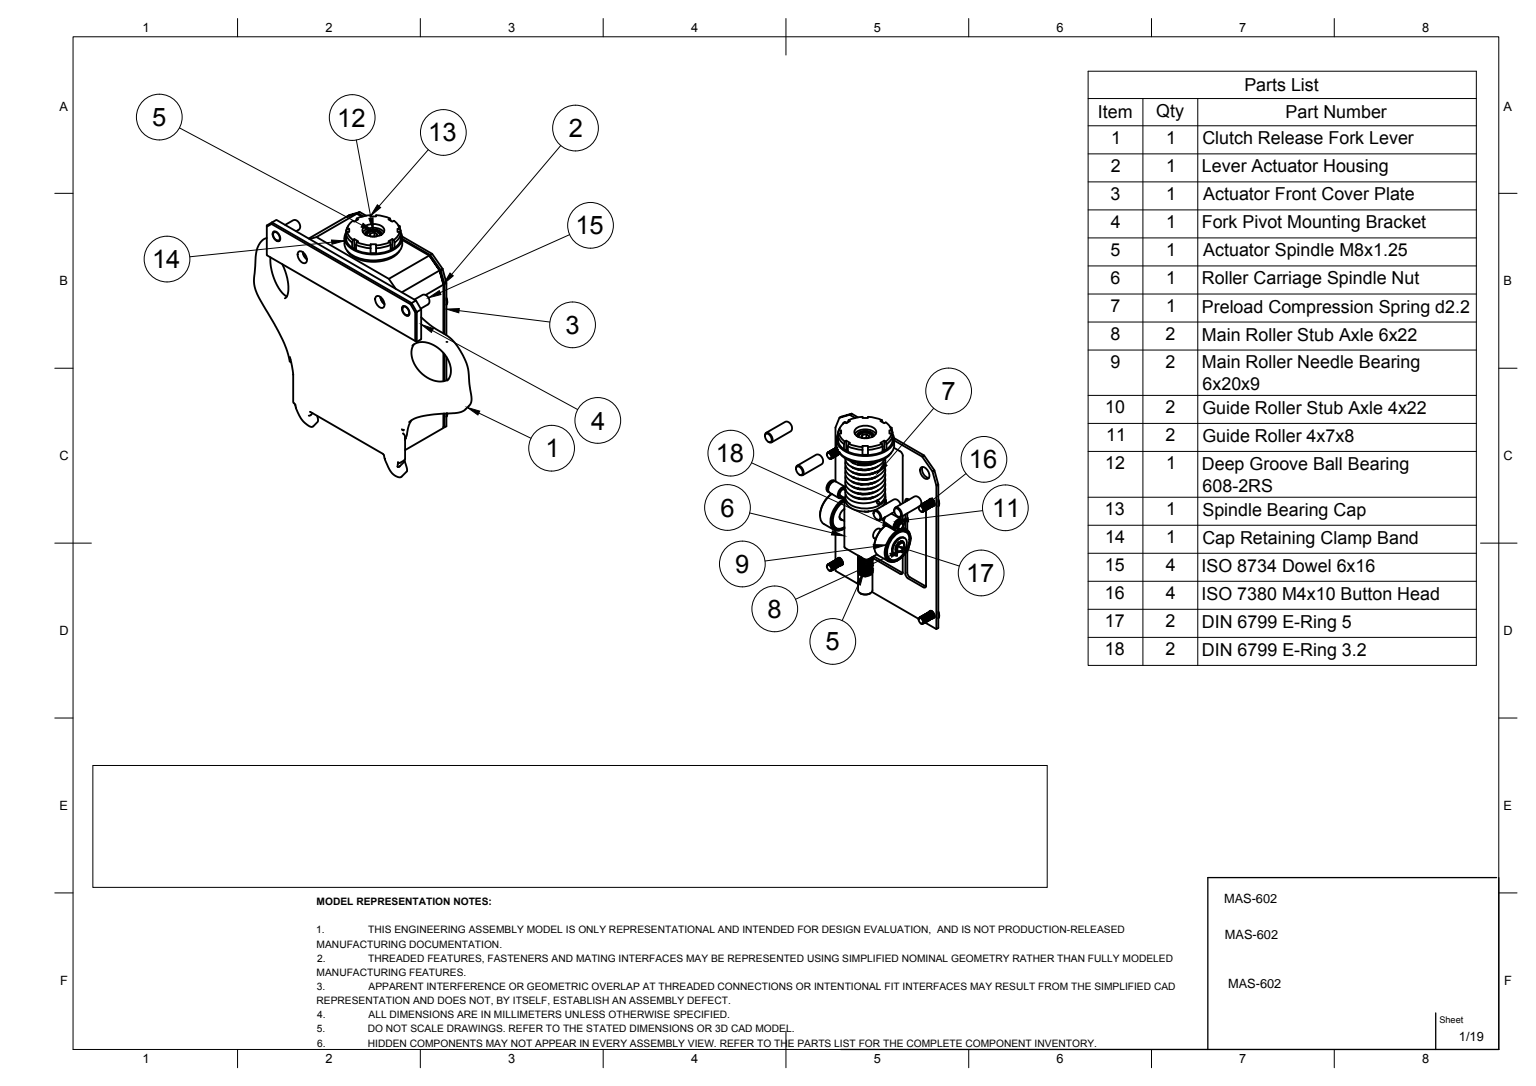
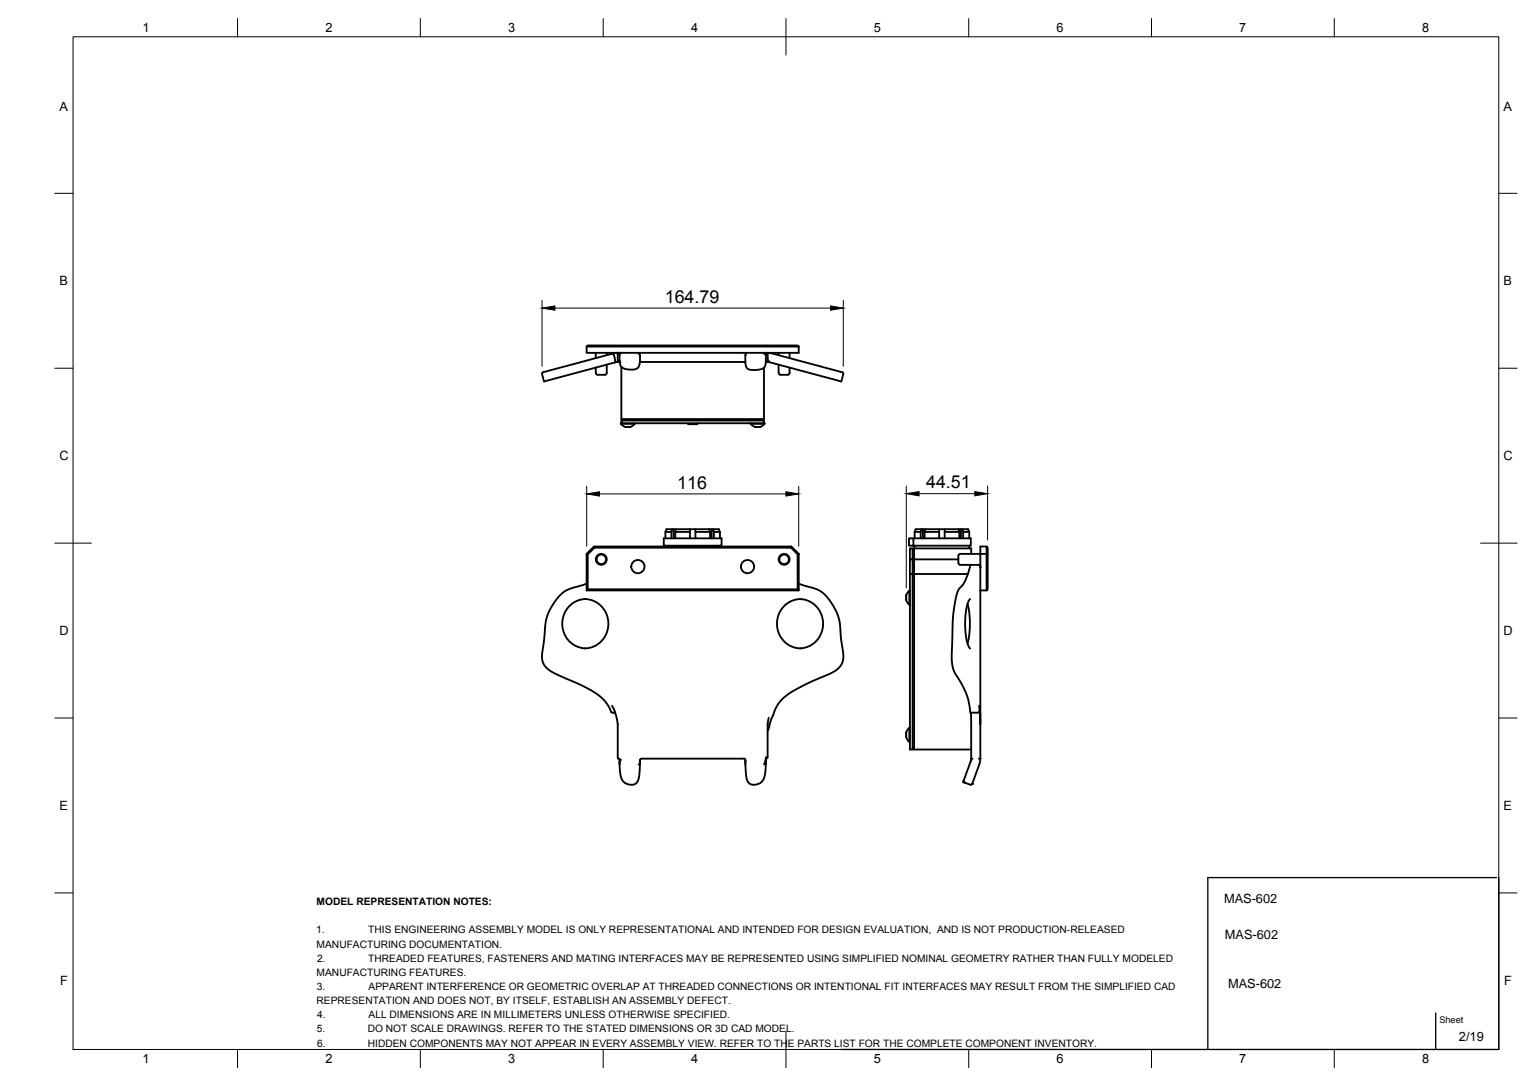
ISO-10303-21;
HEADER;
/* Generated by software containing ST-Developer
 * from STEP Tools, Inc. (www.steptools.com) 
 */

FILE_DESCRIPTION(
/* description */ (''),
/* implementation_level */ '2;1');

FILE_NAME(
/* name */ 'MAS-602',
/* time_stamp */ '2026-10-15T14:42:47-07:00',
/* author */ (''),
/* organization */ (''),
/* preprocessor_version */ 'ST-DEVELOPER v20.2',
/* originating_system */ 'Autodesk Translation Framework v15.15.0.0',
/* authorisation */ '');

FILE_SCHEMA (('AUTOMOTIVE_DESIGN { 1 0 10303 214 3 1 1 }'));
ENDSEC;

DATA;
#10=MECHANICAL_DESIGN_GEOMETRIC_PRESENTATION_REPRESENTATION('',(#234,#235,
#236,#237,#238,#239,#240,#241,#242,#243,#244,#245,#246,#247,#248,#249,#250,
#251),#85789);
#11=ITEM_DEFINED_TRANSFORMATION($,$,#10099,#10929);
#12=ITEM_DEFINED_TRANSFORMATION($,$,#10303,#10930);
#13=ITEM_DEFINED_TRANSFORMATION($,$,#10376,#10931);
#14=ITEM_DEFINED_TRANSFORMATION($,$,#10453,#10932);
#15=ITEM_DEFINED_TRANSFORMATION($,$,#10480,#10933);
#16=ITEM_DEFINED_TRANSFORMATION($,$,#10504,#10934);
#17=ITEM_DEFINED_TRANSFORMATION($,$,#10562,#10935);
#18=ITEM_DEFINED_TRANSFORMATION($,$,#10741,#10936);
#19=ITEM_DEFINED_TRANSFORMATION($,$,#10691,#10937);
#20=ITEM_DEFINED_TRANSFORMATION($,$,#10759,#10938);
#21=ITEM_DEFINED_TRANSFORMATION($,$,#10724,#10939);
#22=ITEM_DEFINED_TRANSFORMATION($,$,#10565,#10940);
#23=ITEM_DEFINED_TRANSFORMATION($,$,#10598,#10941);
#24=ITEM_DEFINED_TRANSFORMATION($,$,#10679,#10942);
#25=ITEM_DEFINED_TRANSFORMATION($,$,#10777,#10943);
#26=ITEM_DEFINED_TRANSFORMATION($,$,#10788,#10944);
#27=ITEM_DEFINED_TRANSFORMATION($,$,#10855,#10945);
#28=ITEM_DEFINED_TRANSFORMATION($,$,#10892,#10946);
#29=ITEM_DEFINED_TRANSFORMATION($,$,#10691,#10947);
#30=ITEM_DEFINED_TRANSFORMATION($,$,#10724,#10948);
#31=ITEM_DEFINED_TRANSFORMATION($,$,#10741,#10949);
#32=ITEM_DEFINED_TRANSFORMATION($,$,#10759,#10950);
#33=ITEM_DEFINED_TRANSFORMATION($,$,#10777,#10951);
#34=ITEM_DEFINED_TRANSFORMATION($,$,#10777,#10952);
#35=ITEM_DEFINED_TRANSFORMATION($,$,#10777,#10953);
#36=ITEM_DEFINED_TRANSFORMATION($,$,#10788,#10954);
#37=ITEM_DEFINED_TRANSFORMATION($,$,#10788,#10955);
#38=ITEM_DEFINED_TRANSFORMATION($,$,#10788,#10956);
#39=ITEM_DEFINED_TRANSFORMATION($,$,#10855,#10957);
#40=ITEM_DEFINED_TRANSFORMATION($,$,#10892,#10958);
#41=(
REPRESENTATION_RELATIONSHIP($,$,#85863,#85862)
REPRESENTATION_RELATIONSHIP_WITH_TRANSFORMATION(#11)
SHAPE_REPRESENTATION_RELATIONSHIP()
);
#42=(
REPRESENTATION_RELATIONSHIP($,$,#85864,#85862)
REPRESENTATION_RELATIONSHIP_WITH_TRANSFORMATION(#12)
SHAPE_REPRESENTATION_RELATIONSHIP()
);
#43=(
REPRESENTATION_RELATIONSHIP($,$,#85865,#85862)
REPRESENTATION_RELATIONSHIP_WITH_TRANSFORMATION(#13)
SHAPE_REPRESENTATION_RELATIONSHIP()
);
#44=(
REPRESENTATION_RELATIONSHIP($,$,#85866,#85862)
REPRESENTATION_RELATIONSHIP_WITH_TRANSFORMATION(#14)
SHAPE_REPRESENTATION_RELATIONSHIP()
);
#45=(
REPRESENTATION_RELATIONSHIP($,$,#85867,#85862)
REPRESENTATION_RELATIONSHIP_WITH_TRANSFORMATION(#15)
SHAPE_REPRESENTATION_RELATIONSHIP()
);
#46=(
REPRESENTATION_RELATIONSHIP($,$,#85868,#85862)
REPRESENTATION_RELATIONSHIP_WITH_TRANSFORMATION(#16)
SHAPE_REPRESENTATION_RELATIONSHIP()
);
#47=(
REPRESENTATION_RELATIONSHIP($,$,#85869,#85862)
REPRESENTATION_RELATIONSHIP_WITH_TRANSFORMATION(#17)
SHAPE_REPRESENTATION_RELATIONSHIP()
);
#48=(
REPRESENTATION_RELATIONSHIP($,$,#85875,#85862)
REPRESENTATION_RELATIONSHIP_WITH_TRANSFORMATION(#18)
SHAPE_REPRESENTATION_RELATIONSHIP()
);
#49=(
REPRESENTATION_RELATIONSHIP($,$,#85873,#85862)
REPRESENTATION_RELATIONSHIP_WITH_TRANSFORMATION(#19)
SHAPE_REPRESENTATION_RELATIONSHIP()
);
#50=(
REPRESENTATION_RELATIONSHIP($,$,#85876,#85862)
REPRESENTATION_RELATIONSHIP_WITH_TRANSFORMATION(#20)
SHAPE_REPRESENTATION_RELATIONSHIP()
);
#51=(
REPRESENTATION_RELATIONSHIP($,$,#85874,#85862)
REPRESENTATION_RELATIONSHIP_WITH_TRANSFORMATION(#21)
SHAPE_REPRESENTATION_RELATIONSHIP()
);
#52=(
REPRESENTATION_RELATIONSHIP($,$,#85870,#85862)
REPRESENTATION_RELATIONSHIP_WITH_TRANSFORMATION(#22)
SHAPE_REPRESENTATION_RELATIONSHIP()
);
#53=(
REPRESENTATION_RELATIONSHIP($,$,#85871,#85862)
REPRESENTATION_RELATIONSHIP_WITH_TRANSFORMATION(#23)
SHAPE_REPRESENTATION_RELATIONSHIP()
);
#54=(
REPRESENTATION_RELATIONSHIP($,$,#85872,#85862)
REPRESENTATION_RELATIONSHIP_WITH_TRANSFORMATION(#24)
SHAPE_REPRESENTATION_RELATIONSHIP()
);
#55=(
REPRESENTATION_RELATIONSHIP($,$,#85877,#85862)
REPRESENTATION_RELATIONSHIP_WITH_TRANSFORMATION(#25)
SHAPE_REPRESENTATION_RELATIONSHIP()
);
#56=(
REPRESENTATION_RELATIONSHIP($,$,#85878,#85862)
REPRESENTATION_RELATIONSHIP_WITH_TRANSFORMATION(#26)
SHAPE_REPRESENTATION_RELATIONSHIP()
);
#57=(
REPRESENTATION_RELATIONSHIP($,$,#85879,#85862)
REPRESENTATION_RELATIONSHIP_WITH_TRANSFORMATION(#27)
SHAPE_REPRESENTATION_RELATIONSHIP()
);
#58=(
REPRESENTATION_RELATIONSHIP($,$,#85880,#85862)
REPRESENTATION_RELATIONSHIP_WITH_TRANSFORMATION(#28)
SHAPE_REPRESENTATION_RELATIONSHIP()
);
#59=(
REPRESENTATION_RELATIONSHIP($,$,#85873,#85862)
REPRESENTATION_RELATIONSHIP_WITH_TRANSFORMATION(#29)
SHAPE_REPRESENTATION_RELATIONSHIP()
);
#60=(
REPRESENTATION_RELATIONSHIP($,$,#85874,#85862)
REPRESENTATION_RELATIONSHIP_WITH_TRANSFORMATION(#30)
SHAPE_REPRESENTATION_RELATIONSHIP()
);
#61=(
REPRESENTATION_RELATIONSHIP($,$,#85875,#85862)
REPRESENTATION_RELATIONSHIP_WITH_TRANSFORMATION(#31)
SHAPE_REPRESENTATION_RELATIONSHIP()
);
#62=(
REPRESENTATION_RELATIONSHIP($,$,#85876,#85862)
REPRESENTATION_RELATIONSHIP_WITH_TRANSFORMATION(#32)
SHAPE_REPRESENTATION_RELATIONSHIP()
);
#63=(
REPRESENTATION_RELATIONSHIP($,$,#85877,#85862)
REPRESENTATION_RELATIONSHIP_WITH_TRANSFORMATION(#33)
SHAPE_REPRESENTATION_RELATIONSHIP()
);
#64=(
REPRESENTATION_RELATIONSHIP($,$,#85877,#85862)
REPRESENTATION_RELATIONSHIP_WITH_TRANSFORMATION(#34)
SHAPE_REPRESENTATION_RELATIONSHIP()
);
#65=(
REPRESENTATION_RELATIONSHIP($,$,#85877,#85862)
REPRESENTATION_RELATIONSHIP_WITH_TRANSFORMATION(#35)
SHAPE_REPRESENTATION_RELATIONSHIP()
);
#66=(
REPRESENTATION_RELATIONSHIP($,$,#85878,#85862)
REPRESENTATION_RELATIONSHIP_WITH_TRANSFORMATION(#36)
SHAPE_REPRESENTATION_RELATIONSHIP()
);
#67=(
REPRESENTATION_RELATIONSHIP($,$,#85878,#85862)
REPRESENTATION_RELATIONSHIP_WITH_TRANSFORMATION(#37)
SHAPE_REPRESENTATION_RELATIONSHIP()
);
#68=(
REPRESENTATION_RELATIONSHIP($,$,#85878,#85862)
REPRESENTATION_RELATIONSHIP_WITH_TRANSFORMATION(#38)
SHAPE_REPRESENTATION_RELATIONSHIP()
);
#69=(
REPRESENTATION_RELATIONSHIP($,$,#85879,#85862)
REPRESENTATION_RELATIONSHIP_WITH_TRANSFORMATION(#39)
SHAPE_REPRESENTATION_RELATIONSHIP()
);
#70=(
REPRESENTATION_RELATIONSHIP($,$,#85880,#85862)
REPRESENTATION_RELATIONSHIP_WITH_TRANSFORMATION(#40)
SHAPE_REPRESENTATION_RELATIONSHIP()
);
#71=CONTEXT_DEPENDENT_SHAPE_REPRESENTATION(#41,#85832);
#72=CONTEXT_DEPENDENT_SHAPE_REPRESENTATION(#42,#85833);
#73=CONTEXT_DEPENDENT_SHAPE_REPRESENTATION(#43,#85834);
#74=CONTEXT_DEPENDENT_SHAPE_REPRESENTATION(#44,#85835);
#75=CONTEXT_DEPENDENT_SHAPE_REPRESENTATION(#45,#85836);
#76=CONTEXT_DEPENDENT_SHAPE_REPRESENTATION(#46,#85837);
#77=CONTEXT_DEPENDENT_SHAPE_REPRESENTATION(#47,#85838);
#78=CONTEXT_DEPENDENT_SHAPE_REPRESENTATION(#48,#85839);
#79=CONTEXT_DEPENDENT_SHAPE_REPRESENTATION(#49,#85840);
#80=CONTEXT_DEPENDENT_SHAPE_REPRESENTATION(#50,#85841);
#81=CONTEXT_DEPENDENT_SHAPE_REPRESENTATION(#51,#85842);
#82=CONTEXT_DEPENDENT_SHAPE_REPRESENTATION(#52,#85843);
#83=CONTEXT_DEPENDENT_SHAPE_REPRESENTATION(#53,#85844);
#84=CONTEXT_DEPENDENT_SHAPE_REPRESENTATION(#54,#85845);
#85=CONTEXT_DEPENDENT_SHAPE_REPRESENTATION(#55,#85846);
#86=CONTEXT_DEPENDENT_SHAPE_REPRESENTATION(#56,#85847);
#87=CONTEXT_DEPENDENT_SHAPE_REPRESENTATION(#57,#85848);
#88=CONTEXT_DEPENDENT_SHAPE_REPRESENTATION(#58,#85849);
#89=CONTEXT_DEPENDENT_SHAPE_REPRESENTATION(#59,#85850);
#90=CONTEXT_DEPENDENT_SHAPE_REPRESENTATION(#60,#85851);
#91=CONTEXT_DEPENDENT_SHAPE_REPRESENTATION(#61,#85852);
#92=CONTEXT_DEPENDENT_SHAPE_REPRESENTATION(#62,#85853);
#93=CONTEXT_DEPENDENT_SHAPE_REPRESENTATION(#63,#85854);
#94=CONTEXT_DEPENDENT_SHAPE_REPRESENTATION(#64,#85855);
#95=CONTEXT_DEPENDENT_SHAPE_REPRESENTATION(#65,#85856);
#96=CONTEXT_DEPENDENT_SHAPE_REPRESENTATION(#66,#85857);
#97=CONTEXT_DEPENDENT_SHAPE_REPRESENTATION(#67,#85858);
#98=CONTEXT_DEPENDENT_SHAPE_REPRESENTATION(#68,#85859);
#99=CONTEXT_DEPENDENT_SHAPE_REPRESENTATION(#69,#85860);
#100=CONTEXT_DEPENDENT_SHAPE_REPRESENTATION(#70,#85861);
#101=NEXT_ASSEMBLY_USAGE_OCCURRENCE('Clutch Release Fork Lever:1',
'Clutch Release Fork Lever:1','Clutch Release Fork Lever:1',#85882,#85883,
'Clutch Release Fork Lever:1');
#102=NEXT_ASSEMBLY_USAGE_OCCURRENCE('Lever Actuator Housing:1',
'Lever Actuator Housing:1','Lever Actuator Housing:1',#85882,#85884,
'Lever Actuator Housing:1');
#103=NEXT_ASSEMBLY_USAGE_OCCURRENCE('Actuator Front Cover Plate:1',
'Actuator Front Cover Plate:1','Actuator Front Cover Plate:1',#85882,#85885,
'Actuator Front Cover Plate:1');
#104=NEXT_ASSEMBLY_USAGE_OCCURRENCE('Fork Pivot Mounting Bracket:1',
'Fork Pivot Mounting Bracket:1','Fork Pivot Mounting Bracket:1',#85882,
#85886,'Fork Pivot Mounting Bracket:1');
#105=NEXT_ASSEMBLY_USAGE_OCCURRENCE('Actuator Spindle M8x1.25:1',
'Actuator Spindle M8x1.25:1','Actuator Spindle M8x1.25:1',#85882,#85887,
'Actuator Spindle M8x1.25:1');
#106=NEXT_ASSEMBLY_USAGE_OCCURRENCE('Roller Carriage Spindle Nut:1',
'Roller Carriage Spindle Nut:1','Roller Carriage Spindle Nut:1',#85882,
#85888,'Roller Carriage Spindle Nut:1');
#107=NEXT_ASSEMBLY_USAGE_OCCURRENCE('Preload Compression Spring d2.2:1',
'Preload Compression Spring d2.2:1','Preload Compression Spring d2.2:1',
#85882,#85889,'Preload Compression Spring d2.2:1');
#108=NEXT_ASSEMBLY_USAGE_OCCURRENCE('Main Roller Stub Axle 6x22:1',
'Main Roller Stub Axle 6x22:1','Main Roller Stub Axle 6x22:1',#85882,#85895,
'Main Roller Stub Axle 6x22:1');
#109=NEXT_ASSEMBLY_USAGE_OCCURRENCE(
'Main Roller Needle Bearing 6x20x9:1',
'Main Roller Needle Bearing 6x20x9:1',
'Main Roller Needle Bearing 6x20x9:1',#85882,#85893,
'Main Roller Needle Bearing 6x20x9:1');
#110=NEXT_ASSEMBLY_USAGE_OCCURRENCE('Guide Roller Stub Axle 4x22:1',
'Guide Roller Stub Axle 4x22:1','Guide Roller Stub Axle 4x22:1',#85882,
#85896,'Guide Roller Stub Axle 4x22:1');
#111=NEXT_ASSEMBLY_USAGE_OCCURRENCE('Guide Roller 4x7x8:1',
'Guide Roller 4x7x8:1','Guide Roller 4x7x8:1',#85882,#85894,
'Guide Roller 4x7x8:1');
#112=NEXT_ASSEMBLY_USAGE_OCCURRENCE(
'Deep Groove Ball Bearing 608-2RS:1',
'Deep Groove Ball Bearing 608-2RS:1',
'Deep Groove Ball Bearing 608-2RS:1',#85882,#85890,
'Deep Groove Ball Bearing 608-2RS:1');
#113=NEXT_ASSEMBLY_USAGE_OCCURRENCE('Spindle Bearing Cap:1',
'Spindle Bearing Cap:1','Spindle Bearing Cap:1',#85882,#85891,
'Spindle Bearing Cap:1');
#114=NEXT_ASSEMBLY_USAGE_OCCURRENCE('Cap Retaining Clamp Band:1',
'Cap Retaining Clamp Band:1','Cap Retaining Clamp Band:1',#85882,#85892,
'Cap Retaining Clamp Band:1');
#115=NEXT_ASSEMBLY_USAGE_OCCURRENCE('ISO 8734 Dowel 6x16:1',
'ISO 8734 Dowel 6x16:1','ISO 8734 Dowel 6x16:1',#85882,#85897,
'ISO 8734 Dowel 6x16:1');
#116=NEXT_ASSEMBLY_USAGE_OCCURRENCE('ISO 7380 M4x10 Button Head:1',
'ISO 7380 M4x10 Button Head:1','ISO 7380 M4x10 Button Head:1',#85882,#85898,
'ISO 7380 M4x10 Button Head:1');
#117=NEXT_ASSEMBLY_USAGE_OCCURRENCE('DIN 6799 E-Ring 5:1',
'DIN 6799 E-Ring 5:1','DIN 6799 E-Ring 5:1',#85882,#85899,
'DIN 6799 E-Ring 5:1');
#118=NEXT_ASSEMBLY_USAGE_OCCURRENCE('DIN 6799 E-Ring 3.2:1',
'DIN 6799 E-Ring 3.2:1','DIN 6799 E-Ring 3.2:1',#85882,#85900,
'DIN 6799 E-Ring 3.2:1');
#119=NEXT_ASSEMBLY_USAGE_OCCURRENCE(
'Main Roller Needle Bearing 6x20x9:2',
'Main Roller Needle Bearing 6x20x9:2',
'Main Roller Needle Bearing 6x20x9:2',#85882,#85893,
'Main Roller Needle Bearing 6x20x9:2');
#120=NEXT_ASSEMBLY_USAGE_OCCURRENCE('Guide Roller 4x7x8:2',
'Guide Roller 4x7x8:2','Guide Roller 4x7x8:2',#85882,#85894,
'Guide Roller 4x7x8:2');
#121=NEXT_ASSEMBLY_USAGE_OCCURRENCE('Main Roller Stub Axle 6x22:2',
'Main Roller Stub Axle 6x22:2','Main Roller Stub Axle 6x22:2',#85882,#85895,
'Main Roller Stub Axle 6x22:2');
#122=NEXT_ASSEMBLY_USAGE_OCCURRENCE('Guide Roller Stub Axle 4x22:2',
'Guide Roller Stub Axle 4x22:2','Guide Roller Stub Axle 4x22:2',#85882,
#85896,'Guide Roller Stub Axle 4x22:2');
#123=NEXT_ASSEMBLY_USAGE_OCCURRENCE('ISO 8734 Dowel 6x16:2',
'ISO 8734 Dowel 6x16:2','ISO 8734 Dowel 6x16:2',#85882,#85897,
'ISO 8734 Dowel 6x16:2');
#124=NEXT_ASSEMBLY_USAGE_OCCURRENCE('ISO 8734 Dowel 6x16:3',
'ISO 8734 Dowel 6x16:3','ISO 8734 Dowel 6x16:3',#85882,#85897,
'ISO 8734 Dowel 6x16:3');
#125=NEXT_ASSEMBLY_USAGE_OCCURRENCE('ISO 8734 Dowel 6x16:4',
'ISO 8734 Dowel 6x16:4','ISO 8734 Dowel 6x16:4',#85882,#85897,
'ISO 8734 Dowel 6x16:4');
#126=NEXT_ASSEMBLY_USAGE_OCCURRENCE('ISO 7380 M4x10 Button Head:2',
'ISO 7380 M4x10 Button Head:2','ISO 7380 M4x10 Button Head:2',#85882,#85898,
'ISO 7380 M4x10 Button Head:2');
#127=NEXT_ASSEMBLY_USAGE_OCCURRENCE('ISO 7380 M4x10 Button Head:3',
'ISO 7380 M4x10 Button Head:3','ISO 7380 M4x10 Button Head:3',#85882,#85898,
'ISO 7380 M4x10 Button Head:3');
#128=NEXT_ASSEMBLY_USAGE_OCCURRENCE('ISO 7380 M4x10 Button Head:4',
'ISO 7380 M4x10 Button Head:4','ISO 7380 M4x10 Button Head:4',#85882,#85898,
'ISO 7380 M4x10 Button Head:4');
#129=NEXT_ASSEMBLY_USAGE_OCCURRENCE('DIN 6799 E-Ring 5:2',
'DIN 6799 E-Ring 5:2','DIN 6799 E-Ring 5:2',#85882,#85899,
'DIN 6799 E-Ring 5:2');
#130=NEXT_ASSEMBLY_USAGE_OCCURRENCE('DIN 6799 E-Ring 3.2:2',
'DIN 6799 E-Ring 3.2:2','DIN 6799 E-Ring 3.2:2',#85882,#85900,
'DIN 6799 E-Ring 3.2:2');
#131=(
BOUNDED_CURVE()
B_SPLINE_CURVE(2,(#77398,#77399,#77400),.UNSPECIFIED.,.F.,.F.)
B_SPLINE_CURVE_WITH_KNOTS((3,3),(0.,0.161672183572005),.UNSPECIFIED.)
CURVE()
GEOMETRIC_REPRESENTATION_ITEM()
RATIONAL_B_SPLINE_CURVE((1.,1.00021050527521,1.))
REPRESENTATION_ITEM('')
);
#132=(
BOUNDED_CURVE()
B_SPLINE_CURVE(2,(#77406,#77407,#77408),.UNSPECIFIED.,.F.,.F.)
B_SPLINE_CURVE_WITH_KNOTS((3,3),(0.,0.161672183572005),.UNSPECIFIED.)
CURVE()
GEOMETRIC_REPRESENTATION_ITEM()
RATIONAL_B_SPLINE_CURVE((1.,1.00021050550154,1.))
REPRESENTATION_ITEM('')
);
#133=(
BOUNDED_CURVE()
B_SPLINE_CURVE(2,(#77482,#77483,#77484),.UNSPECIFIED.,.F.,.F.)
B_SPLINE_CURVE_WITH_KNOTS((3,3),(0.,0.161672183572003),.UNSPECIFIED.)
CURVE()
GEOMETRIC_REPRESENTATION_ITEM()
RATIONAL_B_SPLINE_CURVE((1.,1.00021050513902,1.))
REPRESENTATION_ITEM('')
);
#134=(
BOUNDED_CURVE()
B_SPLINE_CURVE(2,(#77487,#77488,#77489),.UNSPECIFIED.,.F.,.F.)
B_SPLINE_CURVE_WITH_KNOTS((3,3),(0.,0.161672183572005),.UNSPECIFIED.)
CURVE()
GEOMETRIC_REPRESENTATION_ITEM()
RATIONAL_B_SPLINE_CURVE((1.,1.00021050510688,1.))
REPRESENTATION_ITEM('')
);
#135=(
BOUNDED_CURVE()
B_SPLINE_CURVE(2,(#77498,#77499,#77500),.UNSPECIFIED.,.F.,.F.)
B_SPLINE_CURVE_WITH_KNOTS((3,3),(0.,0.161672183572005),.UNSPECIFIED.)
CURVE()
GEOMETRIC_REPRESENTATION_ITEM()
RATIONAL_B_SPLINE_CURVE((1.,1.00021050528206,1.))
REPRESENTATION_ITEM('')
);
#136=(
BOUNDED_CURVE()
B_SPLINE_CURVE(2,(#77513,#77514,#77515),.UNSPECIFIED.,.F.,.F.)
B_SPLINE_CURVE_WITH_KNOTS((3,3),(0.,0.161672183572005),.UNSPECIFIED.)
CURVE()
GEOMETRIC_REPRESENTATION_ITEM()
RATIONAL_B_SPLINE_CURVE((1.,1.00021050523753,1.))
REPRESENTATION_ITEM('')
);
#137=(
BOUNDED_CURVE()
B_SPLINE_CURVE(2,(#77524,#77525,#77526),.UNSPECIFIED.,.F.,.F.)
B_SPLINE_CURVE_WITH_KNOTS((3,3),(0.,0.161672183572005),.UNSPECIFIED.)
CURVE()
GEOMETRIC_REPRESENTATION_ITEM()
RATIONAL_B_SPLINE_CURVE((1.,1.00021050533942,1.))
REPRESENTATION_ITEM('')
);
#138=(
BOUNDED_CURVE()
B_SPLINE_CURVE(2,(#77539,#77540,#77541),.UNSPECIFIED.,.F.,.F.)
B_SPLINE_CURVE_WITH_KNOTS((3,3),(0.,0.161672183572005),.UNSPECIFIED.)
CURVE()
GEOMETRIC_REPRESENTATION_ITEM()
RATIONAL_B_SPLINE_CURVE((1.,1.00021050540546,1.))
REPRESENTATION_ITEM('')
);
#139=(
BOUNDED_CURVE()
B_SPLINE_CURVE(2,(#77550,#77551,#77552),.UNSPECIFIED.,.F.,.F.)
B_SPLINE_CURVE_WITH_KNOTS((3,3),(0.,0.161672183572005),.UNSPECIFIED.)
CURVE()
GEOMETRIC_REPRESENTATION_ITEM()
RATIONAL_B_SPLINE_CURVE((1.,1.00021050533233,1.))
REPRESENTATION_ITEM('')
);
#140=(
BOUNDED_CURVE()
B_SPLINE_CURVE(2,(#77567,#77568,#77569),.UNSPECIFIED.,.F.,.F.)
B_SPLINE_CURVE_WITH_KNOTS((3,3),(0.,0.161672183572005),.UNSPECIFIED.)
CURVE()
GEOMETRIC_REPRESENTATION_ITEM()
RATIONAL_B_SPLINE_CURVE((1.,1.00021050531619,1.))
REPRESENTATION_ITEM('')
);
#141=(
BOUNDED_CURVE()
B_SPLINE_CURVE(2,(#77578,#77579,#77580),.UNSPECIFIED.,.F.,.F.)
B_SPLINE_CURVE_WITH_KNOTS((3,3),(0.,0.161672183572005),.UNSPECIFIED.)
CURVE()
GEOMETRIC_REPRESENTATION_ITEM()
RATIONAL_B_SPLINE_CURVE((1.,1.00021050600963,1.))
REPRESENTATION_ITEM('')
);
#142=(
BOUNDED_CURVE()
B_SPLINE_CURVE(2,(#77593,#77594,#77595),.UNSPECIFIED.,.F.,.F.)
B_SPLINE_CURVE_WITH_KNOTS((3,3),(0.,0.161672183572005),.UNSPECIFIED.)
CURVE()
GEOMETRIC_REPRESENTATION_ITEM()
RATIONAL_B_SPLINE_CURVE((1.,1.00021050495933,1.))
REPRESENTATION_ITEM('')
);
#143=(
BOUNDED_CURVE()
B_SPLINE_CURVE(2,(#77604,#77605,#77606),.UNSPECIFIED.,.F.,.F.)
B_SPLINE_CURVE_WITH_KNOTS((3,3),(0.,0.161672183572005),.UNSPECIFIED.)
CURVE()
GEOMETRIC_REPRESENTATION_ITEM()
RATIONAL_B_SPLINE_CURVE((1.,1.00021050494585,1.))
REPRESENTATION_ITEM('')
);
#144=(
BOUNDED_CURVE()
B_SPLINE_CURVE(2,(#77619,#77620,#77621),.UNSPECIFIED.,.F.,.F.)
B_SPLINE_CURVE_WITH_KNOTS((3,3),(0.,0.161672183572003),.UNSPECIFIED.)
CURVE()
GEOMETRIC_REPRESENTATION_ITEM()
RATIONAL_B_SPLINE_CURVE((1.,1.00021050534925,1.))
REPRESENTATION_ITEM('')
);
#145=(
BOUNDED_CURVE()
B_SPLINE_CURVE(2,(#77631,#77632,#77633),.UNSPECIFIED.,.F.,.F.)
B_SPLINE_CURVE_WITH_KNOTS((3,3),(0.,0.161672183572003),.UNSPECIFIED.)
CURVE()
GEOMETRIC_REPRESENTATION_ITEM()
RATIONAL_B_SPLINE_CURVE((1.,1.00021050497678,1.))
REPRESENTATION_ITEM('')
);
#146=(
BOUNDED_CURVE()
B_SPLINE_CURVE(2,(#77645,#77646,#77647),.UNSPECIFIED.,.F.,.F.)
B_SPLINE_CURVE_WITH_KNOTS((3,3),(0.,0.161672183572003),.UNSPECIFIED.)
CURVE()
GEOMETRIC_REPRESENTATION_ITEM()
RATIONAL_B_SPLINE_CURVE((1.,1.00021050515309,1.))
REPRESENTATION_ITEM('')
);
#147=(
BOUNDED_CURVE()
B_SPLINE_CURVE(2,(#85443,#85444,#85445),.UNSPECIFIED.,.F.,.F.)
B_SPLINE_CURVE_WITH_KNOTS((3,3),(0.00911071066679689,0.0953350369275265),
 .UNSPECIFIED.)
CURVE()
GEOMETRIC_REPRESENTATION_ITEM()
RATIONAL_B_SPLINE_CURVE((1.01317087172823,1.0695397444443,1.01317087172823))
REPRESENTATION_ITEM('')
);
#148=(
BOUNDED_CURVE()
B_SPLINE_CURVE(2,(#85450,#85451,#85452),.UNSPECIFIED.,.F.,.F.)
B_SPLINE_CURVE_WITH_KNOTS((3,3),(0.00911071066679641,0.0953350369275264),
 .UNSPECIFIED.)
CURVE()
GEOMETRIC_REPRESENTATION_ITEM()
RATIONAL_B_SPLINE_CURVE((1.01317087172823,1.06953974444431,1.01317087172823))
REPRESENTATION_ITEM('')
);
#149=(
BOUNDED_CURVE()
B_SPLINE_CURVE(2,(#85457,#85458,#85459),.UNSPECIFIED.,.F.,.F.)
B_SPLINE_CURVE_WITH_KNOTS((3,3),(0.00911071066679675,0.0953350369275265),
 .UNSPECIFIED.)
CURVE()
GEOMETRIC_REPRESENTATION_ITEM()
RATIONAL_B_SPLINE_CURVE((1.01317087172823,1.0695397444443,1.01317087172823))
REPRESENTATION_ITEM('')
);
#150=(
BOUNDED_CURVE()
B_SPLINE_CURVE(2,(#85464,#85465,#85466),.UNSPECIFIED.,.F.,.F.)
B_SPLINE_CURVE_WITH_KNOTS((3,3),(0.00911071066679614,0.0953350369275257),
 .UNSPECIFIED.)
CURVE()
GEOMETRIC_REPRESENTATION_ITEM()
RATIONAL_B_SPLINE_CURVE((1.01317087172823,1.0695397444443,1.01317087172823))
REPRESENTATION_ITEM('')
);
#151=(
BOUNDED_CURVE()
B_SPLINE_CURVE(2,(#85471,#85472,#85473),.UNSPECIFIED.,.F.,.F.)
B_SPLINE_CURVE_WITH_KNOTS((3,3),(0.0091107106667967,0.0953350369275265),
 .UNSPECIFIED.)
CURVE()
GEOMETRIC_REPRESENTATION_ITEM()
RATIONAL_B_SPLINE_CURVE((1.01317087172823,1.0695397444443,1.01317087172823))
REPRESENTATION_ITEM('')
);
#152=(
BOUNDED_CURVE()
B_SPLINE_CURVE(2,(#85480,#85481,#85482),.UNSPECIFIED.,.F.,.F.)
B_SPLINE_CURVE_WITH_KNOTS((3,3),(0.00911071066679617,0.0953350369275259),
 .UNSPECIFIED.)
CURVE()
GEOMETRIC_REPRESENTATION_ITEM()
RATIONAL_B_SPLINE_CURVE((1.01317087172823,1.0695397444443,1.01317087172823))
REPRESENTATION_ITEM('')
);
#153=CONICAL_SURFACE('',#10323,0.1025,1.02974425867665);
#154=CONICAL_SURFACE('',#10327,0.255,0.785398163397446);
#155=CONICAL_SURFACE('',#10328,0.1025,1.02974425867665);
#156=CONICAL_SURFACE('',#10332,0.255,0.785398163397448);
#157=CONICAL_SURFACE('',#10333,0.1025,1.02974425867665);
#158=CONICAL_SURFACE('',#10337,0.255,0.785398163397446);
#159=CONICAL_SURFACE('',#10338,0.1025,1.02974425867665);
#160=CONICAL_SURFACE('',#10342,0.255,0.785398163397448);
#161=CONICAL_SURFACE('',#10343,0.15,1.02974425867665);
#162=CONICAL_SURFACE('',#10347,0.15,1.02974425867665);
#163=CONICAL_SURFACE('',#10500,0.375,0.785398163397451);
#164=CONICAL_SURFACE('',#10501,0.38,0.785398163397437);
#165=CONICAL_SURFACE('',#10569,0.415,0.785398163397448);
#166=CONICAL_SURFACE('',#10581,1.085,0.785398163397452);
#167=CONICAL_SURFACE('',#10585,1.085,0.785398163397454);
#168=CONICAL_SURFACE('',#10597,0.415,0.785398163397449);
#169=CONICAL_SURFACE('',#10614,1.47,0.380506377112364);
#170=CONICAL_SURFACE('',#10616,1.47,0.380506377112364);
#171=CONICAL_SURFACE('',#10623,1.47,0.380506377112364);
#172=CONICAL_SURFACE('',#10630,1.47,0.380506377112364);
#173=CONICAL_SURFACE('',#10638,1.47,0.380506377112364);
#174=CONICAL_SURFACE('',#10645,1.47,0.380506377112364);
#175=CONICAL_SURFACE('',#10652,1.47,0.380506377112364);
#176=CONICAL_SURFACE('',#10659,1.47,0.380506377112364);
#177=CONICAL_SURFACE('',#10695,0.322,0.785398163397448);
#178=CONICAL_SURFACE('',#10707,0.975,0.785398163397449);
#179=CONICAL_SURFACE('',#10711,0.975,0.785398163397448);
#180=CONICAL_SURFACE('',#10723,0.322,0.785398163397448);
#181=CONICAL_SURFACE('',#10728,0.217,0.785398163397448);
#182=CONICAL_SURFACE('',#10732,0.335,0.785398163397448);
#183=CONICAL_SURFACE('',#10736,0.335,0.785398163397447);
#184=CONICAL_SURFACE('',#10740,0.217,0.785398163397447);
#185=CONICAL_SURFACE('',#10744,0.285,0.785398163397449);
#186=CONICAL_SURFACE('',#10756,0.285,0.785398163397444);
#187=CONICAL_SURFACE('',#10762,0.185,0.78539816339745);
#188=CONICAL_SURFACE('',#10774,0.185,0.785398163397445);
#189=CONICAL_SURFACE('',#10787,0.28,0.785398163397448);
#190=CONICAL_SURFACE('',#10812,0.185470053837925,1.0471975511966);
#191=CONICAL_SURFACE('',#10814,0.185470053837925,1.0471975511966);
#192=CONICAL_SURFACE('',#10816,0.185470053837925,1.0471975511966);
#193=CONICAL_SURFACE('',#10818,0.185470053837925,1.0471975511966);
#194=CONICAL_SURFACE('',#10820,0.185470053837925,1.0471975511966);
#195=CONICAL_SURFACE('',#10823,0.185470053837925,1.0471975511966);
#196=CONICAL_SURFACE('',#10840,0.06125,1.02376802452586);
#197=CONICAL_SURFACE('',#10851,0.185,0.785398163397448);
#198=SHAPE_REPRESENTATION_RELATIONSHIP('SRR','None',#85863,#216);
#199=SHAPE_REPRESENTATION_RELATIONSHIP('SRR','None',#85864,#217);
#200=SHAPE_REPRESENTATION_RELATIONSHIP('SRR','None',#85865,#218);
#201=SHAPE_REPRESENTATION_RELATIONSHIP('SRR','None',#85866,#219);
#202=SHAPE_REPRESENTATION_RELATIONSHIP('SRR','None',#85867,#220);
#203=SHAPE_REPRESENTATION_RELATIONSHIP('SRR','None',#85868,#221);
#204=SHAPE_REPRESENTATION_RELATIONSHIP('SRR','None',#85869,#222);
#205=SHAPE_REPRESENTATION_RELATIONSHIP('SRR','None',#85870,#223);
#206=SHAPE_REPRESENTATION_RELATIONSHIP('SRR','None',#85871,#224);
#207=SHAPE_REPRESENTATION_RELATIONSHIP('SRR','None',#85872,#225);
#208=SHAPE_REPRESENTATION_RELATIONSHIP('SRR','None',#85873,#226);
#209=SHAPE_REPRESENTATION_RELATIONSHIP('SRR','None',#85874,#227);
#210=SHAPE_REPRESENTATION_RELATIONSHIP('SRR','None',#85875,#228);
#211=SHAPE_REPRESENTATION_RELATIONSHIP('SRR','None',#85876,#229);
#212=SHAPE_REPRESENTATION_RELATIONSHIP('SRR','None',#85877,#230);
#213=SHAPE_REPRESENTATION_RELATIONSHIP('SRR','None',#85878,#231);
#214=SHAPE_REPRESENTATION_RELATIONSHIP('SRR','None',#85879,#232);
#215=SHAPE_REPRESENTATION_RELATIONSHIP('SRR','None',#85880,#233);
#216=ADVANCED_BREP_SHAPE_REPRESENTATION('',(#252),#85771);
#217=ADVANCED_BREP_SHAPE_REPRESENTATION('',(#253),#85772);
#218=ADVANCED_BREP_SHAPE_REPRESENTATION('',(#254),#85773);
#219=ADVANCED_BREP_SHAPE_REPRESENTATION('',(#255),#85774);
#220=ADVANCED_BREP_SHAPE_REPRESENTATION('',(#256),#85775);
#221=ADVANCED_BREP_SHAPE_REPRESENTATION('',(#257),#85776);
#222=ADVANCED_BREP_SHAPE_REPRESENTATION('',(#258),#85777);
#223=ADVANCED_BREP_SHAPE_REPRESENTATION('',(#259),#85778);
#224=ADVANCED_BREP_SHAPE_REPRESENTATION('',(#260),#85779);
#225=ADVANCED_BREP_SHAPE_REPRESENTATION('',(#261),#85780);
#226=ADVANCED_BREP_SHAPE_REPRESENTATION('',(#262),#85781);
#227=ADVANCED_BREP_SHAPE_REPRESENTATION('',(#263),#85782);
#228=ADVANCED_BREP_SHAPE_REPRESENTATION('',(#264),#85783);
#229=ADVANCED_BREP_SHAPE_REPRESENTATION('',(#265),#85784);
#230=ADVANCED_BREP_SHAPE_REPRESENTATION('',(#266),#85785);
#231=ADVANCED_BREP_SHAPE_REPRESENTATION('',(#267),#85786);
#232=ADVANCED_BREP_SHAPE_REPRESENTATION('',(#268),#85787);
#233=ADVANCED_BREP_SHAPE_REPRESENTATION('',(#269),#85788);
#234=STYLED_ITEM('',(#85962),#252);
#235=STYLED_ITEM('',(#85963),#253);
#236=STYLED_ITEM('',(#85964),#254);
#237=STYLED_ITEM('',(#85965),#255);
#238=STYLED_ITEM('',(#85966),#256);
#239=STYLED_ITEM('',(#85967),#257);
#240=STYLED_ITEM('',(#85968),#258);
#241=STYLED_ITEM('',(#85969),#259);
#242=STYLED_ITEM('',(#85970),#260);
#243=STYLED_ITEM('',(#85971),#261);
#244=STYLED_ITEM('',(#85972),#262);
#245=STYLED_ITEM('',(#85973),#263);
#246=STYLED_ITEM('',(#85974),#264);
#247=STYLED_ITEM('',(#85975),#265);
#248=STYLED_ITEM('',(#85976),#266);
#249=STYLED_ITEM('',(#85977),#267);
#250=STYLED_ITEM('',(#85978),#268);
#251=STYLED_ITEM('',(#85978),#269);
#252=MANIFOLD_SOLID_BREP('Body1',#9881);
#253=MANIFOLD_SOLID_BREP('Body1',#9882);
#254=MANIFOLD_SOLID_BREP('Body1',#9883);
#255=MANIFOLD_SOLID_BREP('Body1',#9884);
#256=MANIFOLD_SOLID_BREP('Body1',#9885);
#257=MANIFOLD_SOLID_BREP('Body1',#9886);
#258=MANIFOLD_SOLID_BREP('Body1',#9887);
#259=MANIFOLD_SOLID_BREP('Body1',#9888);
#260=MANIFOLD_SOLID_BREP('Body1',#9889);
#261=MANIFOLD_SOLID_BREP('Body1',#9890);
#262=MANIFOLD_SOLID_BREP('Body1',#9891);
#263=MANIFOLD_SOLID_BREP('Body1',#9892);
#264=MANIFOLD_SOLID_BREP('Body1',#9893);
#265=MANIFOLD_SOLID_BREP('Body1',#9894);
#266=MANIFOLD_SOLID_BREP('Body1',#9895);
#267=MANIFOLD_SOLID_BREP('Body1',#9896);
#268=MANIFOLD_SOLID_BREP('Body1',#9897);
#269=MANIFOLD_SOLID_BREP('Body1',#9898);
#270=SPHERICAL_SURFACE('',#10130,0.08);
#271=SPHERICAL_SURFACE('',#10138,0.08);
#272=SPHERICAL_SURFACE('',#10178,0.08);
#273=SPHERICAL_SURFACE('',#10200,0.08);
#274=SPHERICAL_SURFACE('',#10239,0.08);
#275=SPHERICAL_SURFACE('',#10241,0.08);
#276=SPHERICAL_SURFACE('',#10260,0.08);
#277=SPHERICAL_SURFACE('',#10282,0.08);
#278=SPHERICAL_SURFACE('',#10292,0.08);
#279=SPHERICAL_SURFACE('',#10825,0.475);
#280=B_SPLINE_SURFACE_WITH_KNOTS('',3,1,((#13627,#13628),(#13629,#13630),
(#13631,#13632),(#13633,#13634),(#13635,#13636),(#13637,#13638),(#13639,
#13640)),.UNSPECIFIED.,.F.,.F.,.F.,(4,1,1,1,4),(2,2),(0.,0.285714285714286,
0.571428571428571,0.785714285714286,1.),(0.,0.504000000000458),
 .UNSPECIFIED.);
#281=B_SPLINE_SURFACE_WITH_KNOTS('',5,1,((#13700,#13701),(#13702,#13703),
(#13704,#13705),(#13706,#13707),(#13708,#13709),(#13710,#13711),(#13712,
#13713),(#13714,#13715),(#13716,#13717),(#13718,#13719),(#13720,#13721),
(#13722,#13723),(#13724,#13725),(#13726,#13727),(#13728,#13729),(#13730,
#13731),(#13732,#13733),(#13734,#13735),(#13736,#13737),(#13738,#13739),
(#13740,#13741),(#13742,#13743),(#13744,#13745),(#13746,#13747),(#13748,
#13749),(#13750,#13751),(#13752,#13753),(#13754,#13755),(#13756,#13757),
(#13758,#13759),(#13760,#13761),(#13762,#13763),(#13764,#13765),(#13766,
#13767),(#13768,#13769),(#13770,#13771),(#13772,#13773),(#13774,#13775),
(#13776,#13777),(#13778,#13779),(#13780,#13781),(#13782,#13783),(#13784,
#13785),(#13786,#13787),(#13788,#13789),(#13790,#13791),(#13792,#13793),
(#13794,#13795),(#13796,#13797),(#13798,#13799),(#13800,#13801),(#13802,
#13803),(#13804,#13805),(#13806,#13807),(#13808,#13809),(#13810,#13811),
(#13812,#13813),(#13814,#13815),(#13816,#13817),(#13818,#13819),(#13820,
#13821),(#13822,#13823),(#13824,#13825),(#13826,#13827),(#13828,#13829),
(#13830,#13831),(#13832,#13833),(#13834,#13835),(#13836,#13837),(#13838,
#13839),(#13840,#13841),(#13842,#13843),(#13844,#13845),(#13846,#13847),
(#13848,#13849),(#13850,#13851),(#13852,#13853),(#13854,#13855),(#13856,
#13857),(#13858,#13859),(#13860,#13861),(#13862,#13863),(#13864,#13865),
(#13866,#13867),(#13868,#13869),(#13870,#13871),(#13872,#13873),(#13874,
#13875),(#13876,#13877),(#13878,#13879),(#13880,#13881),(#13882,#13883),
(#13884,#13885),(#13886,#13887),(#13888,#13889),(#13890,#13891),(#13892,
#13893),(#13894,#13895),(#13896,#13897),(#13898,#13899),(#13900,#13901),
(#13902,#13903),(#13904,#13905),(#13906,#13907),(#13908,#13909),(#13910,
#13911),(#13912,#13913),(#13914,#13915),(#13916,#13917),(#13918,#13919),
(#13920,#13921),(#13922,#13923),(#13924,#13925),(#13926,#13927),(#13928,
#13929),(#13930,#13931),(#13932,#13933),(#13934,#13935),(#13936,#13937),
(#13938,#13939),(#13940,#13941),(#13942,#13943),(#13944,#13945),(#13946,
#13947),(#13948,#13949),(#13950,#13951),(#13952,#13953),(#13954,#13955),
(#13956,#13957),(#13958,#13959),(#13960,#13961),(#13962,#13963),(#13964,
#13965),(#13966,#13967),(#13968,#13969),(#13970,#13971),(#13972,#13973),
(#13974,#13975),(#13976,#13977),(#13978,#13979),(#13980,#13981),(#13982,
#13983),(#13984,#13985),(#13986,#13987),(#13988,#13989),(#13990,#13991),
(#13992,#13993),(#13994,#13995),(#13996,#13997),(#13998,#13999),(#14000,
#14001),(#14002,#14003),(#14004,#14005),(#14006,#14007),(#14008,#14009),
(#14010,#14011),(#14012,#14013),(#14014,#14015),(#14016,#14017),(#14018,
#14019),(#14020,#14021),(#14022,#14023),(#14024,#14025),(#14026,#14027),
(#14028,#14029),(#14030,#14031),(#14032,#14033),(#14034,#14035),(#14036,
#14037),(#14038,#14039),(#14040,#14041),(#14042,#14043),(#14044,#14045),
(#14046,#14047),(#14048,#14049),(#14050,#14051),(#14052,#14053),(#14054,
#14055),(#14056,#14057),(#14058,#14059),(#14060,#14061),(#14062,#14063),
(#14064,#14065),(#14066,#14067),(#14068,#14069),(#14070,#14071),(#14072,
#14073),(#14074,#14075),(#14076,#14077),(#14078,#14079),(#14080,#14081),
(#14082,#14083),(#14084,#14085),(#14086,#14087),(#14088,#14089),(#14090,
#14091),(#14092,#14093),(#14094,#14095),(#14096,#14097),(#14098,#14099),
(#14100,#14101),(#14102,#14103),(#14104,#14105),(#14106,#14107),(#14108,
#14109),(#14110,#14111),(#14112,#14113),(#14114,#14115),(#14116,#14117),
(#14118,#14119),(#14120,#14121),(#14122,#14123),(#14124,#14125),(#14126,
#14127),(#14128,#14129),(#14130,#14131),(#14132,#14133),(#14134,#14135),
(#14136,#14137),(#14138,#14139),(#14140,#14141),(#14142,#14143),(#14144,
#14145),(#14146,#14147),(#14148,#14149),(#14150,#14151),(#14152,#14153),
(#14154,#14155),(#14156,#14157),(#14158,#14159),(#14160,#14161),(#14162,
#14163),(#14164,#14165),(#14166,#14167),(#14168,#14169),(#14170,#14171),
(#14172,#14173),(#14174,#14175),(#14176,#14177),(#14178,#14179),(#14180,
#14181),(#14182,#14183),(#14184,#14185),(#14186,#14187),(#14188,#14189),
(#14190,#14191),(#14192,#14193),(#14194,#14195),(#14196,#14197),(#14198,
#14199),(#14200,#14201),(#14202,#14203),(#14204,#14205),(#14206,#14207),
(#14208,#14209),(#14210,#14211),(#14212,#14213),(#14214,#14215),(#14216,
#14217),(#14218,#14219)),.UNSPECIFIED.,.T.,.F.,.F.,(6,1,1,1,1,1,1,1,1,1,
1,1,1,1,1,1,1,1,1,1,1,1,1,1,1,1,1,1,1,1,1,1,1,1,1,1,1,1,1,1,1,1,1,1,1,1,
1,1,1,1,1,1,1,1,1,1,1,1,1,1,1,1,1,1,1,1,1,1,1,1,1,1,1,1,1,1,1,1,1,1,5,1,
1,1,1,1,1,1,1,1,1,1,1,1,1,1,1,1,1,1,1,1,1,1,1,1,1,1,1,1,1,1,1,1,1,1,1,1,
1,1,1,1,1,1,1,1,1,1,1,1,1,1,1,1,1,1,1,1,1,1,1,1,1,1,1,1,1,1,1,1,1,1,1,1,
1,1,1,1,1,1,1,1,1,1,1,1,1,1,1,1,1,1,1,1,1,1,1,1,1,1,1,1,1,1,1,1,1,1,1,1,
1,1,1,1,1,1,1,1,1,1,1,1,1,1,1,1,1,1,1,1,1,1,1,1,1,1,1,1,1,1,1,1,1,1,1,1,
1,1,1,1,1,1,1,1,1,1,1,1,1,1,1,1,1,1,1,1,1,1,1,1,1,6),(2,2),(-0.318438690804418,
-0.316,-0.312,-0.308,-0.304,-0.3,-0.296,-0.292,-0.288,-0.284,-0.28,-0.276,
-0.272,-0.268,-0.264,-0.26,-0.256,-0.252,-0.248,-0.244,-0.24,-0.236,-0.232,
-0.228,-0.224,-0.22,-0.216,-0.212,-0.208,-0.204,-0.2,-0.196,-0.192,-0.188,
-0.184,-0.18,-0.176,-0.172,-0.168,-0.164,-0.16,-0.156,-0.152,-0.148,-0.144,
-0.14,-0.136,-0.132,-0.128,-0.124,-0.12,-0.116,-0.112,-0.108,-0.104,-0.1,
-0.0960000000000001,-0.0920000000000001,-0.0880000000000001,-0.084,-0.08,
-0.076,-0.072,-0.068,-0.064,-0.06,-0.056,-0.052,-0.048,-0.044,-0.04,-0.036,
-0.032,-0.028,-0.024,-0.02,-0.016,-0.012,-0.008,-0.004,0.,0.00399999999999923,
0.00799999999999923,0.0119999999999992,0.0159999999999992,0.0199999999999992,
0.0239999999999992,0.0279999999999992,0.0319999999999993,0.0359999999999993,
0.0399999999999993,0.0439999999999993,0.0479999999999993,0.0519999999999993,
0.0559999999999993,0.0599999999999993,0.0639999999999993,0.0679999999999993,
0.0719999999999993,0.0759999999999993,0.0799999999999993,0.0839999999999993,
0.0879999999999993,0.0919999999999993,0.0959999999999993,0.0999999999999993,
0.103999999999999,0.107999999999999,0.111999999999999,0.115999999999999,
0.119999999999999,0.123999999999999,0.127999999999999,0.131999999999999,
0.135999999999999,0.139999999999999,0.143999999999999,0.147999999999999,
0.151999999999999,0.155999999999999,0.159999999999999,0.163999999999999,
0.167999999999999,0.171999999999999,0.175999999999999,0.179999999999999,
0.183999999999999,0.187999999999999,0.191999999999999,0.195999999999999,
0.199999999999999,0.203999999999999,0.207999999999999,0.211999999999999,
0.215999999999999,0.219999999999999,0.223999999999999,0.227999999999999,
0.231999999999999,0.235999999999999,0.239999999999999,0.243999999999999,
0.247999999999999,0.251999999999999,0.255999999999999,0.259999999999999,
0.263999999999999,0.267999999999999,0.271999999999999,0.275999999999999,
0.279999999999999,0.283999999999999,0.287999999999999,0.291999999999999,
0.295999999999999,0.299999999999999,0.303999999999999,0.307999999999999,
0.311999999999999,0.316,0.32,0.324,0.328,0.332,0.336,0.34,0.344,0.348,0.352,
0.356,0.36,0.364,0.368,0.372,0.376,0.38,0.384,0.388,0.392,0.396,0.4,0.404,
0.408,0.412,0.416,0.42,0.424,0.428,0.432,0.436,0.44,0.444,0.448,0.452,0.456,
0.46,0.464,0.468,0.472,0.476,0.48,0.484,0.488,0.492,0.496,0.5,0.504,0.508,
0.512,0.516,0.52,0.524,0.528,0.532,0.536,0.54,0.544,0.548,0.552,0.556,0.56,
0.564,0.568,0.572,0.576,0.58,0.584,0.588,0.592,0.596,0.6,0.604,0.608,0.612,
0.616,0.62,0.624,0.628,0.632,0.636,0.64,0.644,0.648,0.652,0.656,0.66,0.664,
0.668,0.672,0.676,0.68,0.681561309195582),(0.,2.17767906516806),
 .UNSPECIFIED.);
#282=B_SPLINE_SURFACE_WITH_KNOTS('',3,3,((#14275,#14276,#14277,#14278,#14279,
#14280,#14281,#14282,#14283,#14284,#14285,#14286,#14287,#14288,#14289,#14290,
#14291,#14292,#14293,#14294,#14295,#14296,#14297,#14298,#14299,#14300,#14301,
#14302,#14303,#14304,#14305,#14306,#14307,#14308,#14309),(#14310,#14311,
#14312,#14313,#14314,#14315,#14316,#14317,#14318,#14319,#14320,#14321,#14322,
#14323,#14324,#14325,#14326,#14327,#14328,#14329,#14330,#14331,#14332,#14333,
#14334,#14335,#14336,#14337,#14338,#14339,#14340,#14341,#14342,#14343,#14344),
(#14345,#14346,#14347,#14348,#14349,#14350,#14351,#14352,#14353,#14354,
#14355,#14356,#14357,#14358,#14359,#14360,#14361,#14362,#14363,#14364,#14365,
#14366,#14367,#14368,#14369,#14370,#14371,#14372,#14373,#14374,#14375,#14376,
#14377,#14378,#14379),(#14380,#14381,#14382,#14383,#14384,#14385,#14386,
#14387,#14388,#14389,#14390,#14391,#14392,#14393,#14394,#14395,#14396,#14397,
#14398,#14399,#14400,#14401,#14402,#14403,#14404,#14405,#14406,#14407,#14408,
#14409,#14410,#14411,#14412,#14413,#14414),(#14415,#14416,#14417,#14418,
#14419,#14420,#14421,#14422,#14423,#14424,#14425,#14426,#14427,#14428,#14429,
#14430,#14431,#14432,#14433,#14434,#14435,#14436,#14437,#14438,#14439,#14440,
#14441,#14442,#14443,#14444,#14445,#14446,#14447,#14448,#14449)),
 .UNSPECIFIED.,.F.,.F.,.F.,(4,1,4),(4,1,1,1,1,1,1,1,1,1,1,1,1,1,1,1,1,1,
1,1,1,1,1,1,1,1,1,1,1,1,1,1,4),(0.,0.571428571428571,1.),(0.,0.433353360299055,
0.866706720598111,1.30006008089717,1.73341344119622,2.16676680149528,2.49178182171957,
2.60012016179433,3.03347352209339,3.25015020224292,3.46682688239244,4.04463136279118,
4.62243584318992,4.91133808338929,5.20024032358866,5.77804480398741,6.06694704418677,
6.35584928438614,6.64475152458552,6.93365376478489,7.22255600498426,7.36700712508394,
7.51145824518363,7.65590936528331,7.800360485383,8.08926272558237,8.66706720598111,
9.24487168637985,9.82267616677859,10.4004806471773,11.2671873677754,11.7005407280745,
12.1338940883735),.UNSPECIFIED.);
#283=B_SPLINE_SURFACE_WITH_KNOTS('',3,3,((#14451,#14452,#14453,#14454,#14455,
#14456),(#14457,#14458,#14459,#14460,#14461,#14462),(#14463,#14464,#14465,
#14466,#14467,#14468),(#14469,#14470,#14471,#14472,#14473,#14474)),
 .UNSPECIFIED.,.F.,.F.,.F.,(4,4),(4,2,4),(-0.0537574666271907,1.),(-0.15340523472588,
-0.152867184867239,-0.0444303035234761),.UNSPECIFIED.);
#284=B_SPLINE_SURFACE_WITH_KNOTS('',3,3,((#14503,#14504,#14505,#14506),
(#14507,#14508,#14509,#14510),(#14511,#14512,#14513,#14514),(#14515,#14516,
#14517,#14518),(#14519,#14520,#14521,#14522)),.UNSPECIFIED.,.F.,.F.,.F.,
(4,1,4),(4,4),(0.,0.571428571428571,1.),(0.,0.0543233651499556),
 .UNSPECIFIED.);
#285=B_SPLINE_SURFACE_WITH_KNOTS('',3,3,((#14540,#14541,#14542,#14543,#14544,
#14545,#14546,#14547),(#14548,#14549,#14550,#14551,#14552,#14553,#14554,
#14555),(#14556,#14557,#14558,#14559,#14560,#14561,#14562,#14563),(#14564,
#14565,#14566,#14567,#14568,#14569,#14570,#14571),(#14572,#14573,#14574,
#14575,#14576,#14577,#14578,#14579),(#14580,#14581,#14582,#14583,#14584,
#14585,#14586,#14587)),.UNSPECIFIED.,.F.,.F.,.F.,(4,1,1,4),(4,1,1,1,1,4),
(0.,0.285714285714286,0.571428571428571,1.),(0.0937174606900304,0.104785099917186,
0.112163526068624,0.115852739144342,0.117697345682202,0.119541952220061),
 .UNSPECIFIED.);
#286=B_SPLINE_SURFACE_WITH_KNOTS('',3,3,((#14598,#14599,#14600,#14601,#14602,
#14603),(#14604,#14605,#14606,#14607,#14608,#14609),(#14610,#14611,#14612,
#14613,#14614,#14615),(#14616,#14617,#14618,#14619,#14620,#14621),(#14622,
#14623,#14624,#14625,#14626,#14627)),.UNSPECIFIED.,.F.,.F.,.F.,(4,1,4),
(4,1,1,4),(0.362133804475251,0.635505031128715,1.),(1.65498255800438E-15,
0.129082836972258,0.215138061620429,0.3011932862686),.UNSPECIFIED.);
#287=B_SPLINE_SURFACE_WITH_KNOTS('',3,3,((#14636,#14637,#14638,#14639),
(#14640,#14641,#14642,#14643),(#14644,#14645,#14646,#14647),(#14648,#14649,
#14650,#14651),(#14652,#14653,#14654,#14655)),.UNSPECIFIED.,.F.,.F.,.F.,
(4,1,4),(4,4),(-3.21642455285252E-5,0.5,1.),(-3.21642455285252E-5,0.22768259721804),
 .UNSPECIFIED.);
#288=B_SPLINE_SURFACE_WITH_KNOTS('',3,3,((#14667,#14668,#14669,#14670),
(#14671,#14672,#14673,#14674),(#14675,#14676,#14677,#14678),(#14679,#14680,
#14681,#14682),(#14683,#14684,#14685,#14686)),.UNSPECIFIED.,.F.,.F.,.F.,
(4,1,4),(4,4),(0.,0.5,1.),(6.03465648009666E-14,0.0429068684110201),
 .UNSPECIFIED.);
#289=B_SPLINE_SURFACE_WITH_KNOTS('',3,3,((#14693,#14694,#14695,#14696),
(#14697,#14698,#14699,#14700),(#14701,#14702,#14703,#14704),(#14705,#14706,
#14707,#14708),(#14709,#14710,#14711,#14712)),.UNSPECIFIED.,.F.,.F.,.F.,
(4,1,4),(4,4),(0.,0.571428571428571,1.),(0.,0.0979595230969147),
 .UNSPECIFIED.);
#290=B_SPLINE_SURFACE_WITH_KNOTS('',3,3,((#14714,#14715,#14716,#14717),
(#14718,#14719,#14720,#14721),(#14722,#14723,#14724,#14725),(#14726,#14727,
#14728,#14729),(#14730,#14731,#14732,#14733)),.UNSPECIFIED.,.F.,.F.,.F.,
(4,1,4),(4,4),(0.,0.5,1.),(0.101309492239901,0.150948832556605),
 .UNSPECIFIED.);
#291=B_SPLINE_SURFACE_WITH_KNOTS('',3,3,((#14774,#14775,#14776,#14777),
(#14778,#14779,#14780,#14781),(#14782,#14783,#14784,#14785),(#14786,#14787,
#14788,#14789),(#14790,#14791,#14792,#14793)),.UNSPECIFIED.,.F.,.F.,.F.,
(4,1,4),(4,4),(0.362133804475334,0.726628773346571,1.),(0.,0.0965340005117894),
 .UNSPECIFIED.);
#292=B_SPLINE_SURFACE_WITH_KNOTS('',3,3,((#14829,#14830,#14831,#14832),
(#14833,#14834,#14835,#14836),(#14837,#14838,#14839,#14840),(#14841,#14842,
#14843,#14844),(#14845,#14846,#14847,#14848)),.UNSPECIFIED.,.F.,.F.,.F.,
(4,1,4),(4,4),(0.40963181845835,0.704815909229175,1.),(0.,0.224615521635083),
 .UNSPECIFIED.);
#293=B_SPLINE_SURFACE_WITH_KNOTS('',3,3,((#14855,#14856,#14857,#14858),
(#14859,#14860,#14861,#14862),(#14863,#14864,#14865,#14866),(#14867,#14868,
#14869,#14870),(#14871,#14872,#14873,#14874)),.UNSPECIFIED.,.F.,.F.,.F.,
(4,1,4),(4,4),(0.,0.23767239441161,0.47534478882322),(0.0854459382956349,
0.127798241063314),.UNSPECIFIED.);
#294=B_SPLINE_SURFACE_WITH_KNOTS('',3,3,((#14881,#14882,#14883,#14884,#14885,
#14886,#14887),(#14888,#14889,#14890,#14891,#14892,#14893,#14894),(#14895,
#14896,#14897,#14898,#14899,#14900,#14901),(#14902,#14903,#14904,#14905,
#14906,#14907,#14908),(#14909,#14910,#14911,#14912,#14913,#14914,#14915),
(#14916,#14917,#14918,#14919,#14920,#14921,#14922)),.UNSPECIFIED.,.F.,.F.,
 .F.,(4,1,1,4),(4,1,1,1,4),(0.283162399774082,0.590378514156618,0.795189257078309,
1.),(0.,0.0328013253035665,0.065602650607133,0.109337751011888,0.153072851416644),
 .UNSPECIFIED.);
#295=B_SPLINE_SURFACE_WITH_KNOTS('',3,3,((#14931,#14932,#14933,#14934),
(#14935,#14936,#14937,#14938),(#14939,#14940,#14941,#14942),(#14943,#14944,
#14945,#14946),(#14947,#14948,#14949,#14950)),.UNSPECIFIED.,.F.,.F.,.F.,
(4,1,4),(4,4),(0.44925085787876,0.702584769501779,0.955918681124799),(0.,
0.0419417607304844),.UNSPECIFIED.);
#296=B_SPLINE_SURFACE_WITH_KNOTS('',3,3,((#14951,#14952,#14953,#14954),
(#14955,#14956,#14957,#14958),(#14959,#14960,#14961,#14962),(#14963,#14964,
#14965,#14966)),.UNSPECIFIED.,.F.,.F.,.F.,(4,4),(4,4),(0.,0.279727981322212),
(0.,0.17884239607127),.UNSPECIFIED.);
#297=B_SPLINE_SURFACE_WITH_KNOTS('',3,3,((#14973,#14974,#14975,#14976),
(#14977,#14978,#14979,#14980),(#14981,#14982,#14983,#14984),(#14985,#14986,
#14987,#14988)),.UNSPECIFIED.,.F.,.F.,.F.,(4,4),(4,4),(0.547578918945948,
1.),(0.,0.0801298062963358),.UNSPECIFIED.);
#298=B_SPLINE_SURFACE_WITH_KNOTS('',3,3,((#14995,#14996,#14997,#14998,#14999,
#15000,#15001,#15002,#15003,#15004,#15005,#15006,#15007,#15008,#15009,#15010,
#15011,#15012,#15013,#15014,#15015),(#15016,#15017,#15018,#15019,#15020,
#15021,#15022,#15023,#15024,#15025,#15026,#15027,#15028,#15029,#15030,#15031,
#15032,#15033,#15034,#15035,#15036),(#15037,#15038,#15039,#15040,#15041,
#15042,#15043,#15044,#15045,#15046,#15047,#15048,#15049,#15050,#15051,#15052,
#15053,#15054,#15055,#15056,#15057),(#15058,#15059,#15060,#15061,#15062,
#15063,#15064,#15065,#15066,#15067,#15068,#15069,#15070,#15071,#15072,#15073,
#15074,#15075,#15076,#15077,#15078),(#15079,#15080,#15081,#15082,#15083,
#15084,#15085,#15086,#15087,#15088,#15089,#15090,#15091,#15092,#15093,#15094,
#15095,#15096,#15097,#15098,#15099)),.UNSPECIFIED.,.F.,.F.,.F.,(4,1,4),
(4,1,1,1,1,1,1,1,1,1,1,1,1,1,1,1,1,1,4),(0.,0.571428571428571,1.),(0.,0.148302061038192,
0.296604122076384,0.444906183114576,0.593208244152767,0.889812366229151,
1.18641648830553,1.7796247324583,2.37283297661107,4.74566595322214,5.93208244152767,
6.52529068568044,7.11849892983321,7.41510305190959,7.71170717398598,7.86000923502417,
8.00831129606236,8.15661335710055,8.30491541813874),.UNSPECIFIED.);
#299=B_SPLINE_SURFACE_WITH_KNOTS('',5,1,((#15347,#15348),(#15349,#15350),
(#15351,#15352),(#15353,#15354),(#15355,#15356),(#15357,#15358),(#15359,
#15360),(#15361,#15362),(#15363,#15364),(#15365,#15366),(#15367,#15368),
(#15369,#15370),(#15371,#15372),(#15373,#15374),(#15375,#15376),(#15377,
#15378),(#15379,#15380),(#15381,#15382),(#15383,#15384),(#15385,#15386),
(#15387,#15388),(#15389,#15390),(#15391,#15392),(#15393,#15394),(#15395,
#15396),(#15397,#15398),(#15399,#15400),(#15401,#15402),(#15403,#15404),
(#15405,#15406),(#15407,#15408),(#15409,#15410),(#15411,#15412),(#15413,
#15414),(#15415,#15416),(#15417,#15418),(#15419,#15420),(#15421,#15422),
(#15423,#15424),(#15425,#15426),(#15427,#15428)),.UNSPECIFIED.,.F.,.F.,
 .F.,(6,1,1,1,1,1,1,1,1,1,1,1,1,1,1,1,5,1,1,1,1,1,1,1,1,1,1,1,1,1,1,1,6),
(2,2),(-1.06140995878253,-1.06,-1.056,-1.052,-1.048,-1.044,-1.04,-1.036,
-1.032,-1.028,-1.024,-1.02,-1.016,-1.012,-1.008,-1.004,-1.,-0.996000000000001,
-0.992000000000001,-0.988000000000001,-0.984000000000001,-0.980000000000001,
-0.976000000000001,-0.972000000000001,-0.968000000000001,-0.964000000000001,
-0.960000000000001,-0.956000000000001,-0.952000000000001,-0.948000000000001,
-0.944000000000001,-0.940000000000001,-0.938590041217474),(0.,0.6),
 .UNSPECIFIED.);
#300=B_SPLINE_SURFACE_WITH_KNOTS('',5,1,((#15656,#15657),(#15658,#15659),
(#15660,#15661),(#15662,#15663),(#15664,#15665),(#15666,#15667),(#15668,
#15669),(#15670,#15671),(#15672,#15673),(#15674,#15675),(#15676,#15677),
(#15678,#15679),(#15680,#15681),(#15682,#15683),(#15684,#15685),(#15686,
#15687),(#15688,#15689),(#15690,#15691),(#15692,#15693),(#15694,#15695),
(#15696,#15697),(#15698,#15699),(#15700,#15701),(#15702,#15703),(#15704,
#15705),(#15706,#15707),(#15708,#15709),(#15710,#15711),(#15712,#15713),
(#15714,#15715),(#15716,#15717),(#15718,#15719),(#15720,#15721),(#15722,
#15723),(#15724,#15725),(#15726,#15727),(#15728,#15729),(#15730,#15731),
(#15732,#15733),(#15734,#15735),(#15736,#15737),(#15738,#15739),(#15740,
#15741),(#15742,#15743),(#15744,#15745),(#15746,#15747),(#15748,#15749),
(#15750,#15751),(#15752,#15753),(#15754,#15755),(#15756,#15757),(#15758,
#15759),(#15760,#15761),(#15762,#15763),(#15764,#15765),(#15766,#15767),
(#15768,#15769),(#15770,#15771),(#15772,#15773),(#15774,#15775),(#15776,
#15777),(#15778,#15779),(#15780,#15781),(#15782,#15783),(#15784,#15785),
(#15786,#15787),(#15788,#15789),(#15790,#15791),(#15792,#15793),(#15794,
#15795)),.UNSPECIFIED.,.F.,.F.,.F.,(6,1,1,1,1,1,1,1,1,1,1,1,1,1,1,1,1,1,
1,1,1,1,1,1,1,1,1,1,1,1,1,1,1,1,1,1,1,1,1,1,1,1,1,1,1,1,1,1,1,1,1,1,1,1,
1,1,1,1,1,1,1,1,1,1,1,6),(2,2),(-0.318438690804418,-0.316,-0.312,-0.308,
-0.304,-0.3,-0.296,-0.292,-0.288,-0.284,-0.28,-0.276,-0.272,-0.268,-0.264,
-0.26,-0.256,-0.252,-0.248,-0.244,-0.24,-0.236,-0.232,-0.228,-0.224,-0.22,
-0.216,-0.212,-0.208,-0.204,-0.2,-0.196,-0.192,-0.188,-0.184,-0.18,-0.176,
-0.172,-0.168,-0.164,-0.16,-0.156,-0.152,-0.148,-0.144,-0.14,-0.136,-0.132,
-0.128,-0.124,-0.12,-0.116,-0.112,-0.108,-0.104,-0.1,-0.0960000000000001,
-0.0920000000000001,-0.0880000000000001,-0.084,-0.08,-0.076,-0.072,-0.068,
-0.064,-0.0614099587825327),(0.,7.2),.UNSPECIFIED.);
#301=B_SPLINE_SURFACE_WITH_KNOTS('',3,3,((#15802,#15803,#15804,#15805,#15806,
#15807),(#15808,#15809,#15810,#15811,#15812,#15813),(#15814,#15815,#15816,
#15817,#15818,#15819),(#15820,#15821,#15822,#15823,#15824,#15825)),
 .UNSPECIFIED.,.F.,.F.,.F.,(4,4),(4,1,1,4),(-4.4838175058205E-5,1.),(-0.140841580089521,
-0.0804552810939789,-0.0402276405469894,4.34253766641143E-5),
 .UNSPECIFIED.);
#302=B_SPLINE_SURFACE_WITH_KNOTS('',3,3,((#15860,#15861,#15862,#15863),
(#15864,#15865,#15866,#15867),(#15868,#15869,#15870,#15871),(#15872,#15873,
#15874,#15875)),.UNSPECIFIED.,.F.,.F.,.F.,(4,4),(4,4),(0.,1.),(-0.0800719510115295,
0.),.UNSPECIFIED.);
#303=B_SPLINE_SURFACE_WITH_KNOTS('',3,3,((#15884,#15885,#15886,#15887,#15888,
#15889),(#15890,#15891,#15892,#15893,#15894,#15895),(#15896,#15897,#15898,
#15899,#15900,#15901),(#15902,#15903,#15904,#15905,#15906,#15907)),
 .UNSPECIFIED.,.F.,.F.,.F.,(4,4),(4,2,4),(0.,1.),(0.148045073228805,0.168188087897107,
0.168704904027193),.UNSPECIFIED.);
#304=B_SPLINE_SURFACE_WITH_KNOTS('',3,3,((#15911,#15912,#15913,#15914),
(#15915,#15916,#15917,#15918),(#15919,#15920,#15921,#15922),(#15923,#15924,
#15925,#15926)),.UNSPECIFIED.,.F.,.F.,.F.,(4,4),(4,4),(0.,1.),(-0.0911290973321825,
-0.0858168351305703),.UNSPECIFIED.);
#305=B_SPLINE_SURFACE_WITH_KNOTS('',3,3,((#15932,#15933,#15934,#15935),
(#15936,#15937,#15938,#15939),(#15940,#15941,#15942,#15943),(#15944,#15945,
#15946,#15947)),.UNSPECIFIED.,.F.,.F.,.F.,(4,4),(4,4),(0.,1.),(0.00872869968615488,
0.428984955288124),.UNSPECIFIED.);
#306=B_SPLINE_SURFACE_WITH_KNOTS('',3,3,((#15962,#15963,#15964,#15965,#15966,
#15967,#15968,#15969),(#15970,#15971,#15972,#15973,#15974,#15975,#15976,
#15977),(#15978,#15979,#15980,#15981,#15982,#15983,#15984,#15985),(#15986,
#15987,#15988,#15989,#15990,#15991,#15992,#15993),(#15994,#15995,#15996,
#15997,#15998,#15999,#16000,#16001)),.UNSPECIFIED.,.F.,.F.,.F.,(4,1,4),
(4,1,1,1,1,4),(0.,0.5,1.),(-0.288406861392734,-0.268681894462045,-0.248956927531355,
-0.209506993669976,-0.170057059808597,-0.01225732436308),.UNSPECIFIED.);
#307=B_SPLINE_SURFACE_WITH_KNOTS('',5,1,((#16074,#16075),(#16076,#16077),
(#16078,#16079),(#16080,#16081),(#16082,#16083),(#16084,#16085),(#16086,
#16087),(#16088,#16089),(#16090,#16091),(#16092,#16093),(#16094,#16095),
(#16096,#16097),(#16098,#16099),(#16100,#16101),(#16102,#16103),(#16104,
#16105),(#16106,#16107),(#16108,#16109),(#16110,#16111),(#16112,#16113),
(#16114,#16115),(#16116,#16117),(#16118,#16119),(#16120,#16121),(#16122,
#16123),(#16124,#16125),(#16126,#16127),(#16128,#16129),(#16130,#16131),
(#16132,#16133),(#16134,#16135),(#16136,#16137),(#16138,#16139),(#16140,
#16141),(#16142,#16143),(#16144,#16145),(#16146,#16147),(#16148,#16149),
(#16150,#16151),(#16152,#16153),(#16154,#16155),(#16156,#16157),(#16158,
#16159),(#16160,#16161),(#16162,#16163),(#16164,#16165),(#16166,#16167),
(#16168,#16169),(#16170,#16171),(#16172,#16173),(#16174,#16175),(#16176,
#16177),(#16178,#16179),(#16180,#16181),(#16182,#16183),(#16184,#16185),
(#16186,#16187),(#16188,#16189),(#16190,#16191),(#16192,#16193),(#16194,
#16195),(#16196,#16197),(#16198,#16199),(#16200,#16201),(#16202,#16203),
(#16204,#16205),(#16206,#16207),(#16208,#16209),(#16210,#16211),(#16212,
#16213),(#16214,#16215),(#16216,#16217),(#16218,#16219),(#16220,#16221),
(#16222,#16223),(#16224,#16225),(#16226,#16227),(#16228,#16229),(#16230,
#16231),(#16232,#16233),(#16234,#16235),(#16236,#16237),(#16238,#16239),
(#16240,#16241),(#16242,#16243),(#16244,#16245),(#16246,#16247),(#16248,
#16249),(#16250,#16251),(#16252,#16253),(#16254,#16255),(#16256,#16257),
(#16258,#16259),(#16260,#16261),(#16262,#16263),(#16264,#16265),(#16266,
#16267),(#16268,#16269),(#16270,#16271),(#16272,#16273),(#16274,#16275),
(#16276,#16277),(#16278,#16279),(#16280,#16281),(#16282,#16283),(#16284,
#16285),(#16286,#16287),(#16288,#16289),(#16290,#16291),(#16292,#16293),
(#16294,#16295),(#16296,#16297),(#16298,#16299),(#16300,#16301),(#16302,
#16303),(#16304,#16305),(#16306,#16307),(#16308,#16309),(#16310,#16311),
(#16312,#16313),(#16314,#16315),(#16316,#16317),(#16318,#16319),(#16320,
#16321),(#16322,#16323),(#16324,#16325),(#16326,#16327),(#16328,#16329),
(#16330,#16331),(#16332,#16333),(#16334,#16335),(#16336,#16337),(#16338,
#16339),(#16340,#16341),(#16342,#16343),(#16344,#16345),(#16346,#16347),
(#16348,#16349),(#16350,#16351),(#16352,#16353),(#16354,#16355),(#16356,
#16357),(#16358,#16359),(#16360,#16361),(#16362,#16363),(#16364,#16365),
(#16366,#16367),(#16368,#16369),(#16370,#16371),(#16372,#16373),(#16374,
#16375),(#16376,#16377),(#16378,#16379),(#16380,#16381),(#16382,#16383),
(#16384,#16385),(#16386,#16387),(#16388,#16389),(#16390,#16391),(#16392,
#16393),(#16394,#16395),(#16396,#16397),(#16398,#16399),(#16400,#16401),
(#16402,#16403),(#16404,#16405),(#16406,#16407),(#16408,#16409),(#16410,
#16411),(#16412,#16413),(#16414,#16415),(#16416,#16417),(#16418,#16419),
(#16420,#16421),(#16422,#16423),(#16424,#16425),(#16426,#16427),(#16428,
#16429),(#16430,#16431),(#16432,#16433),(#16434,#16435),(#16436,#16437),
(#16438,#16439),(#16440,#16441),(#16442,#16443),(#16444,#16445),(#16446,
#16447),(#16448,#16449),(#16450,#16451),(#16452,#16453),(#16454,#16455),
(#16456,#16457),(#16458,#16459),(#16460,#16461),(#16462,#16463),(#16464,
#16465),(#16466,#16467),(#16468,#16469),(#16470,#16471),(#16472,#16473),
(#16474,#16475),(#16476,#16477),(#16478,#16479),(#16480,#16481),(#16482,
#16483),(#16484,#16485),(#16486,#16487),(#16488,#16489),(#16490,#16491),
(#16492,#16493),(#16494,#16495),(#16496,#16497),(#16498,#16499),(#16500,
#16501),(#16502,#16503),(#16504,#16505),(#16506,#16507),(#16508,#16509),
(#16510,#16511),(#16512,#16513),(#16514,#16515),(#16516,#16517),(#16518,
#16519),(#16520,#16521),(#16522,#16523),(#16524,#16525),(#16526,#16527),
(#16528,#16529),(#16530,#16531),(#16532,#16533),(#16534,#16535),(#16536,
#16537),(#16538,#16539),(#16540,#16541),(#16542,#16543),(#16544,#16545),
(#16546,#16547),(#16548,#16549),(#16550,#16551),(#16552,#16553),(#16554,
#16555),(#16556,#16557),(#16558,#16559),(#16560,#16561),(#16562,#16563),
(#16564,#16565),(#16566,#16567),(#16568,#16569),(#16570,#16571),(#16572,
#16573),(#16574,#16575),(#16576,#16577),(#16578,#16579),(#16580,#16581),
(#16582,#16583),(#16584,#16585),(#16586,#16587),(#16588,#16589),(#16590,
#16591),(#16592,#16593)),.UNSPECIFIED.,.T.,.F.,.F.,(6,1,1,1,1,1,1,1,1,1,
1,1,1,1,1,1,1,1,1,1,1,1,1,1,1,1,1,1,1,1,1,1,1,1,1,1,1,1,1,1,1,1,1,1,1,1,
1,1,1,1,1,1,1,1,1,1,1,1,1,1,1,1,1,1,1,1,1,1,1,1,1,1,1,1,1,1,1,1,1,1,1,1,
1,1,1,1,1,1,1,1,1,1,1,1,1,1,1,1,1,1,1,1,1,1,1,1,1,1,1,1,1,1,1,1,1,1,1,1,
1,1,1,1,1,1,1,1,1,1,1,1,1,1,1,1,1,1,1,1,1,1,1,1,1,1,1,1,1,1,1,1,1,1,1,1,
1,1,1,1,1,1,1,1,1,1,5,1,1,1,1,1,1,1,1,1,1,1,1,1,1,1,1,1,1,1,1,1,1,1,1,1,
1,1,1,1,1,1,1,1,1,1,1,1,1,1,1,1,1,1,1,1,1,1,1,1,1,1,1,1,1,1,1,1,1,1,1,1,
1,1,1,1,1,1,1,1,1,1,1,1,1,1,1,1,1,1,1,1,1,1,1,1,1,6),(2,2),(-0.652913544304935,
-0.652,-0.648,-0.644,-0.64,-0.636,-0.632,-0.628,-0.624,-0.62,-0.616,-0.612,
-0.608,-0.604,-0.6,-0.596,-0.592,-0.588,-0.584,-0.58,-0.576,-0.572,-0.568,
-0.564,-0.56,-0.556,-0.552,-0.548,-0.544,-0.54,-0.536,-0.532,-0.528,-0.524,
-0.52,-0.516,-0.512,-0.508,-0.504,-0.5,-0.496,-0.492,-0.488,-0.484,-0.48,
-0.476,-0.472,-0.468,-0.464,-0.46,-0.456,-0.452,-0.448,-0.444,-0.44,-0.436,
-0.432,-0.428,-0.424,-0.42,-0.416,-0.412,-0.408,-0.404,-0.4,-0.396,-0.392,
-0.388,-0.384,-0.38,-0.376,-0.372,-0.368,-0.364,-0.36,-0.356,-0.352,-0.348,
-0.344,-0.34,-0.336,-0.332,-0.328,-0.324,-0.32,-0.316,-0.312,-0.308,-0.304,
-0.3,-0.296,-0.292,-0.288,-0.284,-0.28,-0.276,-0.272,-0.268,-0.264,-0.26,
-0.256,-0.252,-0.248,-0.244,-0.24,-0.236,-0.232,-0.228,-0.224,-0.22,-0.216,
-0.212,-0.208,-0.204,-0.2,-0.196,-0.192,-0.188,-0.184,-0.18,-0.176,-0.172,
-0.168,-0.164,-0.16,-0.156,-0.152,-0.148,-0.144,-0.14,-0.136,-0.132,-0.128,
-0.124,-0.12,-0.116,-0.112,-0.108,-0.104,-0.1,-0.0960000000000001,-0.0920000000000001,
-0.0880000000000001,-0.084,-0.08,-0.076,-0.072,-0.068,-0.064,-0.06,-0.056,
-0.052,-0.048,-0.044,-0.04,-0.036,-0.032,-0.028,-0.024,-0.02,-0.016,-0.012,
-0.008,-0.004,0.,0.00399999999999923,0.00799999999999923,0.0119999999999992,
0.0159999999999992,0.0199999999999992,0.0239999999999992,0.0279999999999992,
0.0319999999999993,0.0359999999999993,0.0399999999999993,0.0439999999999993,
0.0479999999999993,0.0519999999999993,0.0559999999999993,0.0599999999999993,
0.0639999999999993,0.0679999999999993,0.0719999999999993,0.0759999999999993,
0.0799999999999993,0.0839999999999993,0.0879999999999993,0.0919999999999993,
0.0959999999999993,0.0999999999999993,0.103999999999999,0.107999999999999,
0.111999999999999,0.115999999999999,0.119999999999999,0.123999999999999,
0.127999999999999,0.131999999999999,0.135999999999999,0.139999999999999,
0.143999999999999,0.147999999999999,0.151999999999999,0.155999999999999,
0.159999999999999,0.163999999999999,0.167999999999999,0.171999999999999,
0.175999999999999,0.179999999999999,0.183999999999999,0.187999999999999,
0.191999999999999,0.195999999999999,0.199999999999999,0.203999999999999,
0.207999999999999,0.211999999999999,0.215999999999999,0.219999999999999,
0.223999999999999,0.227999999999999,0.231999999999999,0.235999999999999,
0.239999999999999,0.243999999999999,0.247999999999999,0.251999999999999,
0.255999999999999,0.259999999999999,0.263999999999999,0.267999999999999,
0.271999999999999,0.275999999999999,0.279999999999999,0.283999999999999,
0.287999999999999,0.291999999999999,0.295999999999999,0.299999999999999,
0.303999999999999,0.307999999999999,0.311999999999999,0.316,0.32,0.324,
0.328,0.332,0.336,0.34,0.344,0.347086455695065),(0.,1.0992),
 .UNSPECIFIED.);
#308=B_SPLINE_SURFACE_WITH_KNOTS('',3,3,((#16651,#16652,#16653,#16654,#16655,
#16656,#16657,#16658,#16659,#16660,#16661,#16662,#16663,#16664,#16665,#16666,
#16667,#16668,#16669),(#16670,#16671,#16672,#16673,#16674,#16675,#16676,
#16677,#16678,#16679,#16680,#16681,#16682,#16683,#16684,#16685,#16686,#16687,
#16688),(#16689,#16690,#16691,#16692,#16693,#16694,#16695,#16696,#16697,
#16698,#16699,#16700,#16701,#16702,#16703,#16704,#16705,#16706,#16707),
(#16708,#16709,#16710,#16711,#16712,#16713,#16714,#16715,#16716,#16717,
#16718,#16719,#16720,#16721,#16722,#16723,#16724,#16725,#16726),(#16727,
#16728,#16729,#16730,#16731,#16732,#16733,#16734,#16735,#16736,#16737,#16738,
#16739,#16740,#16741,#16742,#16743,#16744,#16745)),.UNSPECIFIED.,.F.,.F.,
 .F.,(4,1,4),(4,1,1,1,1,1,1,1,1,1,1,1,1,1,1,1,4),(0.,0.571428571428571,
1.),(0.,0.393620506063259,0.787241012126518,0.918447847480938,1.01685297399675,
1.04965468283536,1.11525810051257,1.18086151818978,1.3120683535442,1.44327518889862,
1.57448202425304,1.67288715076885,1.77129227728467,1.96810253031629,2.16491278334792,
2.36172303637955,2.75534354244281),.UNSPECIFIED.);
#309=B_SPLINE_SURFACE_WITH_KNOTS('',3,3,((#16940,#16941,#16942,#16943,#16944),
(#16945,#16946,#16947,#16948,#16949),(#16950,#16951,#16952,#16953,#16954),
(#16955,#16956,#16957,#16958,#16959),(#16960,#16961,#16962,#16963,#16964)),
 .UNSPECIFIED.,.F.,.F.,.F.,(4,1,4),(4,1,4),(0.,0.571428571428571,1.),(-0.166725339205234,
-0.0833626696026172,0.),.UNSPECIFIED.);
#310=B_SPLINE_SURFACE_WITH_KNOTS('',3,3,((#16977,#16978,#16979,#16980),
(#16981,#16982,#16983,#16984),(#16985,#16986,#16987,#16988),(#16989,#16990,
#16991,#16992),(#16993,#16994,#16995,#16996)),.UNSPECIFIED.,.F.,.F.,.F.,
(4,1,4),(4,4),(0.,0.571428571428571,1.),(0.,0.164730944371734),
 .UNSPECIFIED.);
#311=B_SPLINE_SURFACE_WITH_KNOTS('',3,3,((#17011,#17012,#17013,#17014),
(#17015,#17016,#17017,#17018),(#17019,#17020,#17021,#17022),(#17023,#17024,
#17025,#17026),(#17027,#17028,#17029,#17030)),.UNSPECIFIED.,.F.,.F.,.F.,
(4,1,4),(4,4),(0.,0.571428571428571,1.),(0.,0.0505769327849995),
 .UNSPECIFIED.);
#312=B_SPLINE_SURFACE_WITH_KNOTS('',3,3,((#17042,#17043,#17044,#17045),
(#17046,#17047,#17048,#17049),(#17050,#17051,#17052,#17053),(#17054,#17055,
#17056,#17057),(#17058,#17059,#17060,#17061)),.UNSPECIFIED.,.F.,.F.,.F.,
(4,1,4),(4,4),(0.,0.571428571428571,1.),(0.,0.075415368178403),
 .UNSPECIFIED.);
#313=B_SPLINE_SURFACE_WITH_KNOTS('',3,3,((#17070,#17071,#17072,#17073),
(#17074,#17075,#17076,#17077),(#17078,#17079,#17080,#17081),(#17082,#17083,
#17084,#17085),(#17086,#17087,#17088,#17089)),.UNSPECIFIED.,.F.,.F.,.F.,
(4,1,4),(4,4),(0.,0.571428571428571,1.),(0.,0.0172305871960441),
 .UNSPECIFIED.);
#314=B_SPLINE_SURFACE_WITH_KNOTS('',5,1,((#17098,#17099),(#17100,#17101),
(#17102,#17103),(#17104,#17105),(#17106,#17107),(#17108,#17109),(#17110,
#17111),(#17112,#17113),(#17114,#17115),(#17116,#17117),(#17118,#17119),
(#17120,#17121),(#17122,#17123),(#17124,#17125),(#17126,#17127),(#17128,
#17129),(#17130,#17131),(#17132,#17133),(#17134,#17135),(#17136,#17137),
(#17138,#17139),(#17140,#17141),(#17142,#17143),(#17144,#17145)),
 .UNSPECIFIED.,.F.,.F.,.F.,(6,1,1,1,1,1,1,1,1,1,1,1,1,1,1,1,1,1,1,6),(2,
2),(-0.648016352593037,-0.648,-0.644,-0.64,-0.636,-0.632,-0.628,-0.624,
-0.62,-0.616,-0.612,-0.608,-0.604,-0.6,-0.596,-0.592,-0.588,-0.584,-0.58,
-0.578213301303361),(0.,0.600000000000007),.UNSPECIFIED.);
#315=B_SPLINE_SURFACE_WITH_KNOTS('',3,3,((#17175,#17176,#17177,#17178),
(#17179,#17180,#17181,#17182),(#17183,#17184,#17185,#17186),(#17187,#17188,
#17189,#17190)),.UNSPECIFIED.,.F.,.F.,.F.,(4,4),(4,4),(0.,1.),(0.0795665830105256,
0.50017173665434),.UNSPECIFIED.);
#316=B_SPLINE_SURFACE_WITH_KNOTS('',3,3,((#17204,#17205,#17206,#17207),
(#17208,#17209,#17210,#17211),(#17212,#17213,#17214,#17215),(#17216,#17217,
#17218,#17219)),.UNSPECIFIED.,.F.,.F.,.F.,(4,4),(4,4),(0.301693544058951,
1.00002749346625),(0.119480684281991,0.541502145499565),.UNSPECIFIED.);
#317=B_SPLINE_SURFACE_WITH_KNOTS('',5,1,((#17232,#17233),(#17234,#17235),
(#17236,#17237),(#17238,#17239),(#17240,#17241),(#17242,#17243),(#17244,
#17245),(#17246,#17247),(#17248,#17249),(#17250,#17251),(#17252,#17253),
(#17254,#17255),(#17256,#17257),(#17258,#17259),(#17260,#17261),(#17262,
#17263),(#17264,#17265),(#17266,#17267),(#17268,#17269),(#17270,#17271),
(#17272,#17273),(#17274,#17275),(#17276,#17277),(#17278,#17279),(#17280,
#17281),(#17282,#17283),(#17284,#17285),(#17286,#17287),(#17288,#17289),
(#17290,#17291),(#17292,#17293),(#17294,#17295),(#17296,#17297),(#17298,
#17299),(#17300,#17301),(#17302,#17303),(#17304,#17305),(#17306,#17307),
(#17308,#17309),(#17310,#17311),(#17312,#17313),(#17314,#17315),(#17316,
#17317),(#17318,#17319),(#17320,#17321),(#17322,#17323),(#17324,#17325),
(#17326,#17327),(#17328,#17329),(#17330,#17331),(#17332,#17333),(#17334,
#17335),(#17336,#17337),(#17338,#17339),(#17340,#17341),(#17342,#17343),
(#17344,#17345),(#17346,#17347),(#17348,#17349),(#17350,#17351),(#17352,
#17353),(#17354,#17355),(#17356,#17357),(#17358,#17359),(#17360,#17361),
(#17362,#17363),(#17364,#17365),(#17366,#17367),(#17368,#17369),(#17370,
#17371),(#17372,#17373),(#17374,#17375),(#17376,#17377),(#17378,#17379),
(#17380,#17381),(#17382,#17383),(#17384,#17385),(#17386,#17387),(#17388,
#17389),(#17390,#17391),(#17392,#17393),(#17394,#17395),(#17396,#17397),
(#17398,#17399),(#17400,#17401),(#17402,#17403),(#17404,#17405),(#17406,
#17407),(#17408,#17409),(#17410,#17411),(#17412,#17413),(#17414,#17415),
(#17416,#17417),(#17418,#17419),(#17420,#17421),(#17422,#17423),(#17424,
#17425),(#17426,#17427),(#17428,#17429),(#17430,#17431),(#17432,#17433),
(#17434,#17435),(#17436,#17437),(#17438,#17439),(#17440,#17441),(#17442,
#17443),(#17444,#17445),(#17446,#17447),(#17448,#17449),(#17450,#17451),
(#17452,#17453),(#17454,#17455),(#17456,#17457),(#17458,#17459),(#17460,
#17461),(#17462,#17463),(#17464,#17465),(#17466,#17467),(#17468,#17469),
(#17470,#17471),(#17472,#17473),(#17474,#17475),(#17476,#17477),(#17478,
#17479),(#17480,#17481),(#17482,#17483),(#17484,#17485),(#17486,#17487),
(#17488,#17489),(#17490,#17491),(#17492,#17493),(#17494,#17495),(#17496,
#17497),(#17498,#17499),(#17500,#17501),(#17502,#17503),(#17504,#17505),
(#17506,#17507),(#17508,#17509),(#17510,#17511),(#17512,#17513),(#17514,
#17515),(#17516,#17517),(#17518,#17519),(#17520,#17521),(#17522,#17523),
(#17524,#17525),(#17526,#17527),(#17528,#17529),(#17530,#17531),(#17532,
#17533),(#17534,#17535),(#17536,#17537),(#17538,#17539),(#17540,#17541),
(#17542,#17543),(#17544,#17545),(#17546,#17547),(#17548,#17549),(#17550,
#17551),(#17552,#17553),(#17554,#17555),(#17556,#17557),(#17558,#17559),
(#17560,#17561),(#17562,#17563),(#17564,#17565),(#17566,#17567),(#17568,
#17569),(#17570,#17571),(#17572,#17573),(#17574,#17575),(#17576,#17577),
(#17578,#17579),(#17580,#17581),(#17582,#17583),(#17584,#17585),(#17586,
#17587),(#17588,#17589),(#17590,#17591),(#17592,#17593),(#17594,#17595),
(#17596,#17597),(#17598,#17599),(#17600,#17601),(#17602,#17603),(#17604,
#17605),(#17606,#17607),(#17608,#17609),(#17610,#17611),(#17612,#17613),
(#17614,#17615),(#17616,#17617),(#17618,#17619),(#17620,#17621),(#17622,
#17623),(#17624,#17625),(#17626,#17627),(#17628,#17629),(#17630,#17631),
(#17632,#17633),(#17634,#17635),(#17636,#17637),(#17638,#17639),(#17640,
#17641),(#17642,#17643),(#17644,#17645),(#17646,#17647),(#17648,#17649),
(#17650,#17651),(#17652,#17653),(#17654,#17655),(#17656,#17657),(#17658,
#17659),(#17660,#17661),(#17662,#17663),(#17664,#17665),(#17666,#17667),
(#17668,#17669),(#17670,#17671),(#17672,#17673),(#17674,#17675),(#17676,
#17677),(#17678,#17679),(#17680,#17681),(#17682,#17683),(#17684,#17685),
(#17686,#17687),(#17688,#17689),(#17690,#17691),(#17692,#17693),(#17694,
#17695),(#17696,#17697),(#17698,#17699),(#17700,#17701),(#17702,#17703),
(#17704,#17705),(#17706,#17707),(#17708,#17709),(#17710,#17711),(#17712,
#17713),(#17714,#17715),(#17716,#17717),(#17718,#17719),(#17720,#17721),
(#17722,#17723),(#17724,#17725),(#17726,#17727),(#17728,#17729),(#17730,
#17731),(#17732,#17733),(#17734,#17735),(#17736,#17737),(#17738,#17739),
(#17740,#17741),(#17742,#17743),(#17744,#17745),(#17746,#17747),(#17748,
#17749),(#17750,#17751)),.UNSPECIFIED.,.T.,.F.,.F.,(6,1,1,1,1,1,1,1,1,1,
1,1,1,1,1,1,1,1,1,1,1,1,1,1,1,1,1,1,1,1,1,1,1,1,1,1,1,1,1,1,1,1,1,1,1,1,
1,1,1,1,1,1,1,1,1,1,1,1,1,1,1,1,1,1,1,1,1,1,1,1,1,1,1,1,1,1,1,1,1,1,1,1,
1,1,1,1,1,1,1,1,1,1,1,1,1,1,1,1,1,1,1,1,1,1,1,1,1,1,1,1,1,1,1,1,1,1,1,1,
1,1,1,1,1,1,1,1,1,1,1,1,1,1,1,1,1,1,1,1,1,1,1,1,1,1,1,1,1,1,1,1,1,1,1,1,
1,1,1,1,1,1,1,1,1,5,1,1,1,1,1,1,1,1,1,1,1,1,1,1,1,1,1,1,1,1,1,1,1,1,1,1,
1,1,1,1,1,1,1,1,1,1,1,1,1,1,1,1,1,1,1,1,1,1,1,1,1,1,1,1,1,1,1,1,1,1,1,1,
1,1,1,1,1,1,1,1,1,1,1,1,1,1,1,1,1,1,1,1,1,1,1,1,1,6),(2,2),(-0.648016352593037,
-0.648,-0.644,-0.64,-0.636,-0.632,-0.628,-0.624,-0.62,-0.616,-0.612,-0.608,
-0.604,-0.6,-0.596,-0.592,-0.588,-0.584,-0.58,-0.576,-0.572,-0.568,-0.564,
-0.56,-0.556,-0.552,-0.548,-0.544,-0.54,-0.536,-0.532,-0.528,-0.524,-0.52,
-0.516,-0.512,-0.508,-0.504,-0.5,-0.496,-0.492,-0.488,-0.484,-0.48,-0.476,
-0.472,-0.468,-0.464,-0.46,-0.456,-0.452,-0.448,-0.444,-0.44,-0.436,-0.432,
-0.428,-0.424,-0.42,-0.416,-0.412,-0.408,-0.404,-0.4,-0.396,-0.392,-0.388,
-0.384,-0.38,-0.376,-0.372,-0.368,-0.364,-0.36,-0.356,-0.352,-0.348,-0.344,
-0.34,-0.336,-0.332,-0.328,-0.324,-0.32,-0.316,-0.312,-0.308,-0.304,-0.3,
-0.296,-0.292,-0.288,-0.284,-0.28,-0.276,-0.272,-0.268,-0.264,-0.26,-0.256,
-0.252,-0.248,-0.244,-0.24,-0.236,-0.232,-0.228,-0.224,-0.22,-0.216,-0.212,
-0.208,-0.204,-0.2,-0.196,-0.192,-0.188,-0.184,-0.18,-0.176,-0.172,-0.168,
-0.164,-0.16,-0.156,-0.152,-0.148,-0.144,-0.14,-0.136,-0.132,-0.128,-0.124,
-0.12,-0.116,-0.112,-0.108,-0.104,-0.1,-0.0960000000000001,-0.0920000000000001,
-0.0880000000000001,-0.084,-0.08,-0.076,-0.072,-0.068,-0.064,-0.06,-0.056,
-0.052,-0.048,-0.044,-0.04,-0.036,-0.032,-0.028,-0.024,-0.02,-0.016,-0.012,
-0.008,-0.004,0.,0.00399999999999923,0.00799999999999923,0.0119999999999992,
0.0159999999999992,0.0199999999999992,0.0239999999999992,0.0279999999999992,
0.0319999999999993,0.0359999999999993,0.0399999999999993,0.0439999999999993,
0.0479999999999993,0.0519999999999993,0.0559999999999993,0.0599999999999993,
0.0639999999999993,0.0679999999999993,0.0719999999999993,0.0759999999999993,
0.0799999999999993,0.0839999999999993,0.0879999999999993,0.0919999999999993,
0.0959999999999993,0.0999999999999993,0.103999999999999,0.107999999999999,
0.111999999999999,0.115999999999999,0.119999999999999,0.123999999999999,
0.127999999999999,0.131999999999999,0.135999999999999,0.139999999999999,
0.143999999999999,0.147999999999999,0.151999999999999,0.155999999999999,
0.159999999999999,0.163999999999999,0.167999999999999,0.171999999999999,
0.175999999999999,0.179999999999999,0.183999999999999,0.187999999999999,
0.191999999999999,0.195999999999999,0.199999999999999,0.203999999999999,
0.207999999999999,0.211999999999999,0.215999999999999,0.219999999999999,
0.223999999999999,0.227999999999999,0.231999999999999,0.235999999999999,
0.239999999999999,0.243999999999999,0.247999999999999,0.251999999999999,
0.255999999999999,0.259999999999999,0.263999999999999,0.267999999999999,
0.271999999999999,0.275999999999999,0.279999999999999,0.283999999999999,
0.287999999999999,0.291999999999999,0.295999999999999,0.299999999999999,
0.303999999999999,0.307999999999999,0.311999999999999,0.316,0.32,0.324,
0.328,0.332,0.336,0.34,0.344,0.348,0.351983647406963),(0.,0.878547542022766),
 .UNSPECIFIED.);
#318=B_SPLINE_SURFACE_WITH_KNOTS('',3,1,((#17757,#17758),(#17759,#17760),
(#17761,#17762),(#17763,#17764),(#17765,#17766)),.UNSPECIFIED.,.F.,.F.,
 .F.,(4,1,4),(2,2),(0.,0.571428571428571,1.),(0.,0.51269230976995),
 .UNSPECIFIED.);
#319=B_SPLINE_SURFACE_WITH_KNOTS('',5,1,((#17785,#17786),(#17787,#17788),
(#17789,#17790),(#17791,#17792),(#17793,#17794),(#17795,#17796),(#17797,
#17798),(#17799,#17800),(#17801,#17802),(#17803,#17804),(#17805,#17806),
(#17807,#17808),(#17809,#17810),(#17811,#17812),(#17813,#17814),(#17815,
#17816),(#17817,#17818),(#17819,#17820),(#17821,#17822),(#17823,#17824),
(#17825,#17826),(#17827,#17828),(#17829,#17830),(#17831,#17832),(#17833,
#17834),(#17835,#17836),(#17837,#17838),(#17839,#17840),(#17841,#17842),
(#17843,#17844),(#17845,#17846),(#17847,#17848),(#17849,#17850),(#17851,
#17852),(#17853,#17854),(#17855,#17856),(#17857,#17858),(#17859,#17860),
(#17861,#17862),(#17863,#17864),(#17865,#17866),(#17867,#17868),(#17869,
#17870),(#17871,#17872),(#17873,#17874),(#17875,#17876),(#17877,#17878),
(#17879,#17880),(#17881,#17882),(#17883,#17884),(#17885,#17886),(#17887,
#17888),(#17889,#17890),(#17891,#17892),(#17893,#17894),(#17895,#17896),
(#17897,#17898),(#17899,#17900),(#17901,#17902),(#17903,#17904),(#17905,
#17906),(#17907,#17908),(#17909,#17910),(#17911,#17912),(#17913,#17914),
(#17915,#17916),(#17917,#17918),(#17919,#17920),(#17921,#17922),(#17923,
#17924),(#17925,#17926),(#17927,#17928),(#17929,#17930),(#17931,#17932),
(#17933,#17934),(#17935,#17936),(#17937,#17938),(#17939,#17940),(#17941,
#17942),(#17943,#17944),(#17945,#17946),(#17947,#17948),(#17949,#17950),
(#17951,#17952),(#17953,#17954),(#17955,#17956),(#17957,#17958),(#17959,
#17960),(#17961,#17962),(#17963,#17964),(#17965,#17966),(#17967,#17968),
(#17969,#17970),(#17971,#17972),(#17973,#17974),(#17975,#17976),(#17977,
#17978),(#17979,#17980),(#17981,#17982),(#17983,#17984),(#17985,#17986),
(#17987,#17988),(#17989,#17990),(#17991,#17992),(#17993,#17994),(#17995,
#17996),(#17997,#17998),(#17999,#18000),(#18001,#18002),(#18003,#18004),
(#18005,#18006),(#18007,#18008),(#18009,#18010),(#18011,#18012),(#18013,
#18014),(#18015,#18016),(#18017,#18018),(#18019,#18020),(#18021,#18022),
(#18023,#18024),(#18025,#18026),(#18027,#18028),(#18029,#18030),(#18031,
#18032),(#18033,#18034),(#18035,#18036),(#18037,#18038),(#18039,#18040),
(#18041,#18042),(#18043,#18044),(#18045,#18046),(#18047,#18048),(#18049,
#18050),(#18051,#18052),(#18053,#18054),(#18055,#18056),(#18057,#18058),
(#18059,#18060),(#18061,#18062),(#18063,#18064),(#18065,#18066),(#18067,
#18068),(#18069,#18070),(#18071,#18072),(#18073,#18074),(#18075,#18076),
(#18077,#18078),(#18079,#18080),(#18081,#18082),(#18083,#18084),(#18085,
#18086),(#18087,#18088),(#18089,#18090),(#18091,#18092),(#18093,#18094),
(#18095,#18096),(#18097,#18098),(#18099,#18100),(#18101,#18102),(#18103,
#18104),(#18105,#18106),(#18107,#18108),(#18109,#18110),(#18111,#18112),
(#18113,#18114),(#18115,#18116),(#18117,#18118),(#18119,#18120),(#18121,
#18122),(#18123,#18124),(#18125,#18126),(#18127,#18128),(#18129,#18130),
(#18131,#18132),(#18133,#18134),(#18135,#18136),(#18137,#18138),(#18139,
#18140),(#18141,#18142),(#18143,#18144),(#18145,#18146),(#18147,#18148),
(#18149,#18150),(#18151,#18152),(#18153,#18154),(#18155,#18156),(#18157,
#18158),(#18159,#18160),(#18161,#18162),(#18163,#18164),(#18165,#18166),
(#18167,#18168),(#18169,#18170),(#18171,#18172),(#18173,#18174),(#18175,
#18176),(#18177,#18178),(#18179,#18180),(#18181,#18182),(#18183,#18184),
(#18185,#18186),(#18187,#18188),(#18189,#18190),(#18191,#18192),(#18193,
#18194),(#18195,#18196),(#18197,#18198),(#18199,#18200),(#18201,#18202),
(#18203,#18204),(#18205,#18206),(#18207,#18208),(#18209,#18210),(#18211,
#18212),(#18213,#18214),(#18215,#18216),(#18217,#18218),(#18219,#18220),
(#18221,#18222),(#18223,#18224),(#18225,#18226),(#18227,#18228),(#18229,
#18230),(#18231,#18232),(#18233,#18234),(#18235,#18236),(#18237,#18238),
(#18239,#18240),(#18241,#18242),(#18243,#18244),(#18245,#18246),(#18247,
#18248),(#18249,#18250),(#18251,#18252),(#18253,#18254),(#18255,#18256),
(#18257,#18258),(#18259,#18260),(#18261,#18262),(#18263,#18264),(#18265,
#18266),(#18267,#18268),(#18269,#18270),(#18271,#18272),(#18273,#18274),
(#18275,#18276),(#18277,#18278),(#18279,#18280),(#18281,#18282),(#18283,
#18284),(#18285,#18286),(#18287,#18288),(#18289,#18290),(#18291,#18292),
(#18293,#18294),(#18295,#18296),(#18297,#18298),(#18299,#18300),(#18301,
#18302),(#18303,#18304)),.UNSPECIFIED.,.T.,.F.,.F.,(6,1,1,1,1,1,1,1,1,1,
1,1,1,1,1,1,1,1,1,1,1,1,1,1,1,1,1,1,1,1,1,1,1,1,1,1,1,1,1,1,1,1,1,1,1,1,
1,1,1,1,1,1,1,1,1,1,1,1,1,1,1,1,1,1,1,1,1,1,1,1,1,1,1,1,1,1,1,1,1,1,1,5,
1,1,1,1,1,1,1,1,1,1,1,1,1,1,1,1,1,1,1,1,1,1,1,1,1,1,1,1,1,1,1,1,1,1,1,1,
1,1,1,1,1,1,1,1,1,1,1,1,1,1,1,1,1,1,1,1,1,1,1,1,1,1,1,1,1,1,1,1,1,1,1,1,
1,1,1,1,1,1,1,1,1,1,1,1,1,1,1,1,1,1,1,1,1,1,1,1,1,1,1,1,1,1,1,1,1,1,1,1,
1,1,1,1,1,1,1,1,1,1,1,1,1,1,1,1,1,1,1,1,1,1,1,1,1,1,1,1,1,1,1,1,1,1,1,1,
1,1,1,1,1,1,1,1,1,1,1,1,1,1,1,1,1,1,1,1,1,1,1,1,1,6),(2,2),(-0.322416215027029,
-0.32,-0.316,-0.312,-0.308,-0.304,-0.3,-0.296,-0.292,-0.288,-0.284,-0.28,
-0.276,-0.272,-0.268,-0.264,-0.26,-0.256,-0.252,-0.248,-0.244,-0.24,-0.236,
-0.232,-0.228,-0.224,-0.22,-0.216,-0.212,-0.208,-0.204,-0.2,-0.196,-0.192,
-0.188,-0.184,-0.18,-0.176,-0.172,-0.168,-0.164,-0.16,-0.156,-0.152,-0.148,
-0.144,-0.14,-0.136,-0.132,-0.128,-0.124,-0.12,-0.116,-0.112,-0.108,-0.104,
-0.1,-0.0960000000000001,-0.0920000000000001,-0.0880000000000001,-0.084,
-0.08,-0.076,-0.072,-0.068,-0.064,-0.06,-0.056,-0.052,-0.048,-0.044,-0.04,
-0.036,-0.032,-0.028,-0.024,-0.02,-0.016,-0.012,-0.008,-0.004,0.,0.00399999999999923,
0.00799999999999923,0.0119999999999992,0.0159999999999992,0.0199999999999992,
0.0239999999999992,0.0279999999999992,0.0319999999999993,0.0359999999999993,
0.0399999999999993,0.0439999999999993,0.0479999999999993,0.0519999999999993,
0.0559999999999993,0.0599999999999993,0.0639999999999993,0.0679999999999993,
0.0719999999999993,0.0759999999999993,0.0799999999999993,0.0839999999999993,
0.0879999999999993,0.0919999999999993,0.0959999999999993,0.0999999999999993,
0.103999999999999,0.107999999999999,0.111999999999999,0.115999999999999,
0.119999999999999,0.123999999999999,0.127999999999999,0.131999999999999,
0.135999999999999,0.139999999999999,0.143999999999999,0.147999999999999,
0.151999999999999,0.155999999999999,0.159999999999999,0.163999999999999,
0.167999999999999,0.171999999999999,0.175999999999999,0.179999999999999,
0.183999999999999,0.187999999999999,0.191999999999999,0.195999999999999,
0.199999999999999,0.203999999999999,0.207999999999999,0.211999999999999,
0.215999999999999,0.219999999999999,0.223999999999999,0.227999999999999,
0.231999999999999,0.235999999999999,0.239999999999999,0.243999999999999,
0.247999999999999,0.251999999999999,0.255999999999999,0.259999999999999,
0.263999999999999,0.267999999999999,0.271999999999999,0.275999999999999,
0.279999999999999,0.283999999999999,0.287999999999999,0.291999999999999,
0.295999999999999,0.299999999999999,0.303999999999999,0.307999999999999,
0.311999999999999,0.316,0.32,0.324,0.328,0.332,0.336,0.34,0.344,0.348,0.352,
0.356,0.36,0.364,0.368,0.372,0.376,0.38,0.384,0.388,0.392,0.396,0.4,0.404,
0.408,0.412,0.416,0.42,0.424,0.428,0.432,0.436,0.44,0.444,0.448,0.452,0.456,
0.46,0.464,0.468,0.472,0.476,0.48,0.484,0.488,0.492,0.496,0.5,0.504,0.508,
0.512,0.516,0.52,0.524,0.528,0.532,0.536,0.54,0.544,0.548,0.552,0.556,0.56,
0.564,0.568,0.572,0.576,0.58,0.584,0.588,0.592,0.596,0.6,0.604,0.608,0.612,
0.616,0.62,0.624,0.628,0.632,0.636,0.64,0.644,0.648,0.652,0.656,0.66,0.664,
0.668,0.672,0.676,0.677583784972971),(0.,7.2),.UNSPECIFIED.);
#320=B_SPLINE_SURFACE_WITH_KNOTS('',3,3,((#18315,#18316,#18317,#18318),
(#18319,#18320,#18321,#18322),(#18323,#18324,#18325,#18326),(#18327,#18328,
#18329,#18330)),.UNSPECIFIED.,.F.,.F.,.F.,(4,4),(4,4),(0.,1.),(0.214918350132049,
0.48911828449592),.UNSPECIFIED.);
#321=B_SPLINE_SURFACE_WITH_KNOTS('',3,3,((#18350,#18351,#18352,#18353),
(#18354,#18355,#18356,#18357),(#18358,#18359,#18360,#18361),(#18362,#18363,
#18364,#18365)),.UNSPECIFIED.,.F.,.F.,.F.,(4,4),(4,4),(0.,1.),(0.,0.197269104818139),
 .UNSPECIFIED.);
#322=B_SPLINE_SURFACE_WITH_KNOTS('',3,3,((#18377,#18378,#18379,#18380),
(#18381,#18382,#18383,#18384),(#18385,#18386,#18387,#18388),(#18389,#18390,
#18391,#18392)),.UNSPECIFIED.,.F.,.F.,.F.,(4,4),(4,4),(-0.0471135960368116,
1.),(-0.237658380445436,7.56806292790953E-5),.UNSPECIFIED.);
#323=B_SPLINE_SURFACE_WITH_KNOTS('',3,3,((#18408,#18409,#18410,#18411,#18412,
#18413),(#18414,#18415,#18416,#18417,#18418,#18419),(#18420,#18421,#18422,
#18423,#18424,#18425),(#18426,#18427,#18428,#18429,#18430,#18431)),
 .UNSPECIFIED.,.F.,.F.,.F.,(4,4),(4,2,4),(0.,1.),(0.,0.471468502883735,
0.473994966708672),.UNSPECIFIED.);
#324=B_SPLINE_SURFACE_WITH_KNOTS('',3,3,((#18452,#18453,#18454,#18455),
(#18456,#18457,#18458,#18459),(#18460,#18461,#18462,#18463),(#18464,#18465,
#18466,#18467)),.UNSPECIFIED.,.F.,.F.,.F.,(4,4),(4,4),(0.,1.),(1.89854339553983E-15,
0.0666641979607186),.UNSPECIFIED.);
#325=B_SPLINE_SURFACE_WITH_KNOTS('',3,3,((#18476,#18477,#18478,#18479),
(#18480,#18481,#18482,#18483),(#18484,#18485,#18486,#18487),(#18488,#18489,
#18490,#18491)),.UNSPECIFIED.,.F.,.F.,.F.,(4,4),(4,4),(0.186511816400127,
1.),(-1.01772858153936,-0.745004297261558),.UNSPECIFIED.);
#326=B_SPLINE_SURFACE_WITH_KNOTS('',3,3,((#18506,#18507,#18508,#18509),
(#18510,#18511,#18512,#18513),(#18514,#18515,#18516,#18517),(#18518,#18519,
#18520,#18521)),.UNSPECIFIED.,.F.,.F.,.F.,(4,4),(4,4),(0.165314557349038,
1.),(-0.195956842698031,-5.68173586430139E-15),.UNSPECIFIED.);
#327=B_SPLINE_SURFACE_WITH_KNOTS('',3,3,((#18523,#18524,#18525,#18526,#18527,
#18528),(#18529,#18530,#18531,#18532,#18533,#18534),(#18535,#18536,#18537,
#18538,#18539,#18540),(#18541,#18542,#18543,#18544,#18545,#18546)),
 .UNSPECIFIED.,.F.,.F.,.F.,(4,4),(4,2,4),(0.144606210418872,1.),(-0.531787427886525,
-0.530925715886322,0.),.UNSPECIFIED.);
#328=B_SPLINE_SURFACE_WITH_KNOTS('',3,3,((#18547,#18548,#18549,#18550,#18551,
#18552),(#18553,#18554,#18555,#18556,#18557,#18558),(#18559,#18560,#18561,
#18562,#18563,#18564),(#18565,#18566,#18567,#18568,#18569,#18570)),
 .UNSPECIFIED.,.F.,.F.,.F.,(4,4),(4,2,4),(0.,1.02106399261821),(-0.880320663133757,
0.,0.00551932282830541),.UNSPECIFIED.);
#329=B_SPLINE_SURFACE_WITH_KNOTS('',3,3,((#18652,#18653,#18654,#18655),
(#18656,#18657,#18658,#18659),(#18660,#18661,#18662,#18663),(#18664,#18665,
#18666,#18667),(#18668,#18669,#18670,#18671)),.UNSPECIFIED.,.F.,.F.,.F.,
(4,1,4),(4,4),(0.,0.571428571428571,1.00011302068706),(-0.000113020687060352,
0.32384869792086),.UNSPECIFIED.);
#330=B_SPLINE_SURFACE_WITH_KNOTS('',3,3,((#18692,#18693,#18694,#18695),
(#18696,#18697,#18698,#18699),(#18700,#18701,#18702,#18703),(#18704,#18705,
#18706,#18707),(#18708,#18709,#18710,#18711)),.UNSPECIFIED.,.F.,.F.,.F.,
(4,1,4),(4,4),(0.,0.5,1.),(0.,0.105411804182902),.UNSPECIFIED.);
#331=B_SPLINE_SURFACE_WITH_KNOTS('',3,3,((#18722,#18723,#18724,#18725),
(#18726,#18727,#18728,#18729),(#18730,#18731,#18732,#18733),(#18734,#18735,
#18736,#18737),(#18738,#18739,#18740,#18741)),.UNSPECIFIED.,.F.,.F.,.F.,
(4,1,4),(4,4),(0.,0.571428571428571,1.),(0.0597111975742865,0.0778887211231013),
 .UNSPECIFIED.);
#332=B_SPLINE_SURFACE_WITH_KNOTS('',3,3,((#18747,#18748,#18749,#18750,#18751,
#18752,#18753),(#18754,#18755,#18756,#18757,#18758,#18759,#18760),(#18761,
#18762,#18763,#18764,#18765,#18766,#18767),(#18768,#18769,#18770,#18771,
#18772,#18773,#18774),(#18775,#18776,#18777,#18778,#18779,#18780,#18781),
(#18782,#18783,#18784,#18785,#18786,#18787,#18788)),.UNSPECIFIED.,.F.,.F.,
 .F.,(4,1,1,4),(4,1,1,1,4),(0.,0.285714285714286,0.571428571428571,1.),
(-1.84302877518546E-14,0.0336059064221182,0.0672118128442549,0.11201968807377,
0.156827563303286),.UNSPECIFIED.);
#333=B_SPLINE_SURFACE_WITH_KNOTS('',3,3,((#18807,#18808,#18809,#18810,#18811),
(#18812,#18813,#18814,#18815,#18816),(#18817,#18818,#18819,#18820,#18821),
(#18822,#18823,#18824,#18825,#18826),(#18827,#18828,#18829,#18830,#18831)),
 .UNSPECIFIED.,.F.,.F.,.F.,(4,1,4),(4,1,4),(0.,0.571428571428571,1.),(4.07518504807266E-15,
0.0864360398355901,0.172872079671176),.UNSPECIFIED.);
#334=B_SPLINE_SURFACE_WITH_KNOTS('',3,3,((#18845,#18846,#18847,#18848),
(#18849,#18850,#18851,#18852),(#18853,#18854,#18855,#18856),(#18857,#18858,
#18859,#18860),(#18861,#18862,#18863,#18864)),.UNSPECIFIED.,.F.,.F.,.F.,
(4,1,4),(4,4),(0.,0.571428571428571,1.),(0.00704588444375797,0.110567549348147),
 .UNSPECIFIED.);
#335=B_SPLINE_SURFACE_WITH_KNOTS('',3,1,((#18892,#18893),(#18894,#18895),
(#18896,#18897),(#18898,#18899),(#18900,#18901)),.UNSPECIFIED.,.F.,.F.,
 .F.,(4,1,4),(2,2),(0.,0.367757184420533,0.643575072735933),(0.,0.504000000000047),
 .UNSPECIFIED.);
#336=B_SPLINE_SURFACE_WITH_KNOTS('',5,1,((#18910,#18911),(#18912,#18913),
(#18914,#18915),(#18916,#18917),(#18918,#18919),(#18920,#18921),(#18922,
#18923),(#18924,#18925),(#18926,#18927),(#18928,#18929),(#18930,#18931),
(#18932,#18933),(#18934,#18935),(#18936,#18937),(#18938,#18939),(#18940,
#18941),(#18942,#18943),(#18944,#18945),(#18946,#18947),(#18948,#18949),
(#18950,#18951),(#18952,#18953),(#18954,#18955),(#18956,#18957),(#18958,
#18959),(#18960,#18961),(#18962,#18963),(#18964,#18965),(#18966,#18967),
(#18968,#18969),(#18970,#18971),(#18972,#18973),(#18974,#18975),(#18976,
#18977),(#18978,#18979),(#18980,#18981),(#18982,#18983),(#18984,#18985),
(#18986,#18987),(#18988,#18989),(#18990,#18991),(#18992,#18993),(#18994,
#18995),(#18996,#18997),(#18998,#18999),(#19000,#19001),(#19002,#19003),
(#19004,#19005),(#19006,#19007),(#19008,#19009),(#19010,#19011),(#19012,
#19013),(#19014,#19015),(#19016,#19017),(#19018,#19019),(#19020,#19021),
(#19022,#19023),(#19024,#19025),(#19026,#19027),(#19028,#19029),(#19030,
#19031),(#19032,#19033),(#19034,#19035),(#19036,#19037),(#19038,#19039),
(#19040,#19041),(#19042,#19043),(#19044,#19045),(#19046,#19047),(#19048,
#19049),(#19050,#19051),(#19052,#19053),(#19054,#19055),(#19056,#19057),
(#19058,#19059),(#19060,#19061),(#19062,#19063),(#19064,#19065),(#19066,
#19067),(#19068,#19069),(#19070,#19071),(#19072,#19073),(#19074,#19075),
(#19076,#19077),(#19078,#19079),(#19080,#19081),(#19082,#19083),(#19084,
#19085),(#19086,#19087),(#19088,#19089),(#19090,#19091),(#19092,#19093),
(#19094,#19095),(#19096,#19097),(#19098,#19099),(#19100,#19101),(#19102,
#19103),(#19104,#19105),(#19106,#19107),(#19108,#19109),(#19110,#19111),
(#19112,#19113),(#19114,#19115),(#19116,#19117),(#19118,#19119),(#19120,
#19121),(#19122,#19123),(#19124,#19125),(#19126,#19127),(#19128,#19129),
(#19130,#19131),(#19132,#19133),(#19134,#19135),(#19136,#19137),(#19138,
#19139),(#19140,#19141),(#19142,#19143),(#19144,#19145),(#19146,#19147),
(#19148,#19149),(#19150,#19151),(#19152,#19153),(#19154,#19155),(#19156,
#19157),(#19158,#19159),(#19160,#19161),(#19162,#19163),(#19164,#19165),
(#19166,#19167),(#19168,#19169),(#19170,#19171),(#19172,#19173),(#19174,
#19175),(#19176,#19177),(#19178,#19179),(#19180,#19181),(#19182,#19183),
(#19184,#19185),(#19186,#19187),(#19188,#19189),(#19190,#19191),(#19192,
#19193),(#19194,#19195),(#19196,#19197),(#19198,#19199),(#19200,#19201),
(#19202,#19203),(#19204,#19205),(#19206,#19207),(#19208,#19209),(#19210,
#19211),(#19212,#19213),(#19214,#19215),(#19216,#19217),(#19218,#19219),
(#19220,#19221),(#19222,#19223),(#19224,#19225),(#19226,#19227),(#19228,
#19229),(#19230,#19231),(#19232,#19233),(#19234,#19235),(#19236,#19237),
(#19238,#19239),(#19240,#19241),(#19242,#19243),(#19244,#19245),(#19246,
#19247),(#19248,#19249),(#19250,#19251),(#19252,#19253),(#19254,#19255),
(#19256,#19257),(#19258,#19259),(#19260,#19261),(#19262,#19263),(#19264,
#19265),(#19266,#19267),(#19268,#19269),(#19270,#19271),(#19272,#19273),
(#19274,#19275),(#19276,#19277),(#19278,#19279),(#19280,#19281),(#19282,
#19283),(#19284,#19285),(#19286,#19287),(#19288,#19289),(#19290,#19291),
(#19292,#19293),(#19294,#19295),(#19296,#19297),(#19298,#19299),(#19300,
#19301),(#19302,#19303),(#19304,#19305),(#19306,#19307),(#19308,#19309),
(#19310,#19311),(#19312,#19313),(#19314,#19315),(#19316,#19317),(#19318,
#19319),(#19320,#19321),(#19322,#19323),(#19324,#19325),(#19326,#19327),
(#19328,#19329),(#19330,#19331),(#19332,#19333),(#19334,#19335),(#19336,
#19337),(#19338,#19339),(#19340,#19341),(#19342,#19343),(#19344,#19345),
(#19346,#19347),(#19348,#19349),(#19350,#19351),(#19352,#19353),(#19354,
#19355),(#19356,#19357),(#19358,#19359),(#19360,#19361),(#19362,#19363),
(#19364,#19365),(#19366,#19367),(#19368,#19369),(#19370,#19371),(#19372,
#19373),(#19374,#19375),(#19376,#19377),(#19378,#19379),(#19380,#19381),
(#19382,#19383),(#19384,#19385),(#19386,#19387),(#19388,#19389),(#19390,
#19391),(#19392,#19393),(#19394,#19395),(#19396,#19397),(#19398,#19399),
(#19400,#19401),(#19402,#19403),(#19404,#19405),(#19406,#19407),(#19408,
#19409),(#19410,#19411),(#19412,#19413),(#19414,#19415),(#19416,#19417),
(#19418,#19419),(#19420,#19421),(#19422,#19423),(#19424,#19425),(#19426,
#19427),(#19428,#19429)),.UNSPECIFIED.,.T.,.F.,.F.,(6,1,1,1,1,1,1,1,1,1,
1,1,1,1,1,1,1,1,1,1,1,1,1,1,1,1,1,1,1,1,1,1,1,1,1,1,1,1,1,1,1,1,1,1,1,1,
1,1,1,1,1,1,1,1,1,1,1,1,1,1,1,1,1,1,1,1,1,1,1,1,1,1,1,1,1,1,1,1,1,1,1,1,
1,1,1,1,1,1,1,1,1,1,1,1,1,1,1,1,1,1,1,1,1,1,1,1,1,1,1,1,1,1,1,1,1,1,1,1,
1,1,1,1,1,1,1,1,1,1,1,1,1,1,1,1,1,1,1,1,1,1,1,1,1,1,1,1,1,1,1,1,1,1,1,1,
1,1,1,1,1,1,1,1,1,1,1,1,1,1,1,1,1,1,1,1,1,1,1,1,1,1,1,1,1,1,1,1,1,1,1,1,
1,1,1,1,1,1,1,1,1,1,1,1,1,1,1,1,1,1,1,1,1,1,1,1,1,1,1,1,1,1,1,1,1,1,1,1,
1,1,1,1,1,1,1,1,1,5,1,1,1,1,1,1,1,1,1,1,1,1,1,1,1,6),(2,2),(-0.939015270874982,
-0.936000000000001,-0.932000000000001,-0.928000000000001,-0.924000000000001,
-0.920000000000001,-0.916000000000001,-0.912000000000001,-0.908000000000001,
-0.904000000000001,-0.900000000000001,-0.896000000000001,-0.892000000000001,
-0.888000000000001,-0.884000000000001,-0.880000000000001,-0.876000000000001,
-0.872000000000001,-0.868000000000001,-0.864000000000001,-0.860000000000001,
-0.856000000000001,-0.852000000000001,-0.848000000000001,-0.844000000000001,
-0.840000000000001,-0.836000000000001,-0.832000000000001,-0.828000000000001,
-0.824000000000001,-0.820000000000001,-0.816000000000001,-0.812000000000001,
-0.808000000000001,-0.804000000000001,-0.800000000000001,-0.796000000000001,
-0.792000000000001,-0.788000000000001,-0.784000000000001,-0.780000000000001,
-0.776000000000001,-0.772000000000001,-0.768000000000001,-0.764000000000001,
-0.760000000000001,-0.756000000000001,-0.752000000000001,-0.748000000000001,
-0.744000000000001,-0.740000000000001,-0.736000000000001,-0.732000000000001,
-0.728000000000001,-0.724000000000001,-0.720000000000001,-0.716000000000001,
-0.712000000000001,-0.708000000000001,-0.704000000000001,-0.700000000000001,
-0.696000000000001,-0.692000000000001,-0.688000000000001,-0.684,-0.68,-0.676,
-0.672,-0.668,-0.664,-0.66,-0.656,-0.652,-0.648,-0.644,-0.64,-0.636,-0.632,
-0.628,-0.624,-0.62,-0.616,-0.612,-0.608,-0.604,-0.6,-0.596,-0.592,-0.588,
-0.584,-0.58,-0.576,-0.572,-0.568,-0.564,-0.56,-0.556,-0.552,-0.548,-0.544,
-0.54,-0.536,-0.532,-0.528,-0.524,-0.52,-0.516,-0.512,-0.508,-0.504,-0.5,
-0.496,-0.492,-0.488,-0.484,-0.48,-0.476,-0.472,-0.468,-0.464,-0.46,-0.456,
-0.452,-0.448,-0.444,-0.44,-0.436,-0.432,-0.428,-0.424,-0.42,-0.416,-0.412,
-0.408,-0.404,-0.4,-0.396,-0.392,-0.388,-0.384,-0.38,-0.376,-0.372,-0.368,
-0.364,-0.36,-0.356,-0.352,-0.348,-0.344,-0.34,-0.336,-0.332,-0.328,-0.324,
-0.32,-0.316,-0.312,-0.308,-0.304,-0.3,-0.296,-0.292,-0.288,-0.284,-0.28,
-0.276,-0.272,-0.268,-0.264,-0.26,-0.256,-0.252,-0.248,-0.244,-0.24,-0.236,
-0.232,-0.228,-0.224,-0.22,-0.216,-0.212,-0.208,-0.204,-0.2,-0.196,-0.192,
-0.188,-0.184,-0.18,-0.176,-0.172,-0.168,-0.164,-0.16,-0.156,-0.152,-0.148,
-0.144,-0.14,-0.136,-0.132,-0.128,-0.124,-0.12,-0.116,-0.112,-0.108,-0.104,
-0.1,-0.0960000000000001,-0.0920000000000001,-0.0880000000000001,-0.084,
-0.08,-0.076,-0.072,-0.068,-0.064,-0.06,-0.056,-0.052,-0.048,-0.044,-0.04,
-0.036,-0.032,-0.028,-0.024,-0.02,-0.016,-0.012,-0.008,-0.004,0.,0.00399999999999923,
0.00799999999999923,0.0119999999999992,0.0159999999999992,0.0199999999999992,
0.0239999999999992,0.0279999999999992,0.0319999999999993,0.0359999999999993,
0.0399999999999993,0.0439999999999993,0.0479999999999993,0.0519999999999993,
0.0559999999999993,0.0599999999999993,0.0609847291250184),(0.,2.16728151094469),
 .UNSPECIFIED.);
#337=B_SPLINE_SURFACE_WITH_KNOTS('',5,1,((#19434,#19435),(#19436,#19437),
(#19438,#19439),(#19440,#19441),(#19442,#19443),(#19444,#19445),(#19446,
#19447),(#19448,#19449),(#19450,#19451),(#19452,#19453),(#19454,#19455),
(#19456,#19457),(#19458,#19459),(#19460,#19461),(#19462,#19463),(#19464,
#19465),(#19466,#19467),(#19468,#19469),(#19470,#19471),(#19472,#19473),
(#19474,#19475),(#19476,#19477),(#19478,#19479),(#19480,#19481),(#19482,
#19483),(#19484,#19485),(#19486,#19487),(#19488,#19489),(#19490,#19491),
(#19492,#19493),(#19494,#19495),(#19496,#19497),(#19498,#19499),(#19500,
#19501),(#19502,#19503),(#19504,#19505),(#19506,#19507),(#19508,#19509),
(#19510,#19511),(#19512,#19513),(#19514,#19515),(#19516,#19517),(#19518,
#19519),(#19520,#19521),(#19522,#19523),(#19524,#19525),(#19526,#19527),
(#19528,#19529),(#19530,#19531),(#19532,#19533),(#19534,#19535),(#19536,
#19537),(#19538,#19539),(#19540,#19541),(#19542,#19543),(#19544,#19545),
(#19546,#19547),(#19548,#19549),(#19550,#19551),(#19552,#19553),(#19554,
#19555),(#19556,#19557),(#19558,#19559),(#19560,#19561),(#19562,#19563),
(#19564,#19565),(#19566,#19567),(#19568,#19569),(#19570,#19571),(#19572,
#19573),(#19574,#19575),(#19576,#19577),(#19578,#19579),(#19580,#19581),
(#19582,#19583),(#19584,#19585),(#19586,#19587),(#19588,#19589),(#19590,
#19591),(#19592,#19593),(#19594,#19595),(#19596,#19597),(#19598,#19599),
(#19600,#19601),(#19602,#19603),(#19604,#19605),(#19606,#19607),(#19608,
#19609),(#19610,#19611),(#19612,#19613),(#19614,#19615),(#19616,#19617),
(#19618,#19619),(#19620,#19621),(#19622,#19623),(#19624,#19625),(#19626,
#19627),(#19628,#19629),(#19630,#19631),(#19632,#19633),(#19634,#19635),
(#19636,#19637),(#19638,#19639),(#19640,#19641),(#19642,#19643),(#19644,
#19645),(#19646,#19647),(#19648,#19649),(#19650,#19651),(#19652,#19653),
(#19654,#19655),(#19656,#19657),(#19658,#19659),(#19660,#19661),(#19662,
#19663),(#19664,#19665),(#19666,#19667),(#19668,#19669),(#19670,#19671),
(#19672,#19673),(#19674,#19675),(#19676,#19677),(#19678,#19679),(#19680,
#19681),(#19682,#19683),(#19684,#19685),(#19686,#19687),(#19688,#19689),
(#19690,#19691),(#19692,#19693),(#19694,#19695),(#19696,#19697),(#19698,
#19699),(#19700,#19701),(#19702,#19703),(#19704,#19705),(#19706,#19707),
(#19708,#19709),(#19710,#19711),(#19712,#19713),(#19714,#19715),(#19716,
#19717),(#19718,#19719),(#19720,#19721),(#19722,#19723),(#19724,#19725),
(#19726,#19727),(#19728,#19729),(#19730,#19731),(#19732,#19733),(#19734,
#19735),(#19736,#19737),(#19738,#19739),(#19740,#19741),(#19742,#19743),
(#19744,#19745),(#19746,#19747),(#19748,#19749),(#19750,#19751),(#19752,
#19753),(#19754,#19755),(#19756,#19757),(#19758,#19759),(#19760,#19761),
(#19762,#19763),(#19764,#19765),(#19766,#19767),(#19768,#19769),(#19770,
#19771),(#19772,#19773),(#19774,#19775),(#19776,#19777),(#19778,#19779),
(#19780,#19781),(#19782,#19783),(#19784,#19785),(#19786,#19787),(#19788,
#19789),(#19790,#19791),(#19792,#19793),(#19794,#19795),(#19796,#19797),
(#19798,#19799),(#19800,#19801),(#19802,#19803),(#19804,#19805),(#19806,
#19807),(#19808,#19809),(#19810,#19811),(#19812,#19813),(#19814,#19815),
(#19816,#19817),(#19818,#19819),(#19820,#19821),(#19822,#19823),(#19824,
#19825),(#19826,#19827),(#19828,#19829),(#19830,#19831),(#19832,#19833),
(#19834,#19835),(#19836,#19837),(#19838,#19839),(#19840,#19841),(#19842,
#19843),(#19844,#19845),(#19846,#19847),(#19848,#19849),(#19850,#19851),
(#19852,#19853),(#19854,#19855),(#19856,#19857),(#19858,#19859),(#19860,
#19861),(#19862,#19863),(#19864,#19865),(#19866,#19867),(#19868,#19869),
(#19870,#19871),(#19872,#19873),(#19874,#19875),(#19876,#19877),(#19878,
#19879),(#19880,#19881),(#19882,#19883),(#19884,#19885),(#19886,#19887),
(#19888,#19889),(#19890,#19891),(#19892,#19893),(#19894,#19895),(#19896,
#19897),(#19898,#19899),(#19900,#19901),(#19902,#19903),(#19904,#19905),
(#19906,#19907),(#19908,#19909),(#19910,#19911),(#19912,#19913),(#19914,
#19915),(#19916,#19917),(#19918,#19919),(#19920,#19921),(#19922,#19923),
(#19924,#19925),(#19926,#19927),(#19928,#19929),(#19930,#19931),(#19932,
#19933),(#19934,#19935),(#19936,#19937),(#19938,#19939),(#19940,#19941),
(#19942,#19943),(#19944,#19945),(#19946,#19947),(#19948,#19949),(#19950,
#19951),(#19952,#19953)),.UNSPECIFIED.,.T.,.F.,.F.,(6,1,1,1,1,1,1,1,1,1,
1,1,1,1,1,1,1,1,1,1,1,1,1,1,1,1,1,1,1,1,1,1,1,1,1,1,1,1,1,1,1,1,1,1,1,1,
1,1,1,1,1,1,1,1,1,1,1,1,1,1,1,1,1,1,1,1,1,1,1,1,1,1,1,1,1,1,1,1,1,1,1,1,
1,1,1,1,1,1,1,1,1,1,1,1,1,1,1,1,1,1,1,1,1,1,1,1,1,1,1,1,1,1,1,1,1,1,1,1,
1,1,1,1,1,1,1,1,1,1,1,1,1,1,1,1,1,1,1,1,1,1,1,1,1,1,1,1,1,1,1,1,1,1,1,1,
1,1,1,1,1,1,1,1,1,1,1,1,1,1,1,1,1,1,1,1,1,1,1,1,1,1,1,1,1,1,1,1,1,1,1,1,
1,1,1,1,1,1,1,1,1,1,1,1,1,1,1,1,1,1,1,1,1,1,1,1,1,1,1,1,1,1,1,1,1,1,1,1,
1,1,1,1,1,1,1,1,1,5,1,1,1,1,1,1,1,1,1,1,1,1,1,1,1,6),(2,2),(-0.938590041217468,
-0.936000000000001,-0.932000000000001,-0.928000000000001,-0.924000000000001,
-0.920000000000001,-0.916000000000001,-0.912000000000001,-0.908000000000001,
-0.904000000000001,-0.900000000000001,-0.896000000000001,-0.892000000000001,
-0.888000000000001,-0.884000000000001,-0.880000000000001,-0.876000000000001,
-0.872000000000001,-0.868000000000001,-0.864000000000001,-0.860000000000001,
-0.856000000000001,-0.852000000000001,-0.848000000000001,-0.844000000000001,
-0.840000000000001,-0.836000000000001,-0.832000000000001,-0.828000000000001,
-0.824000000000001,-0.820000000000001,-0.816000000000001,-0.812000000000001,
-0.808000000000001,-0.804000000000001,-0.800000000000001,-0.796000000000001,
-0.792000000000001,-0.788000000000001,-0.784000000000001,-0.780000000000001,
-0.776000000000001,-0.772000000000001,-0.768000000000001,-0.764000000000001,
-0.760000000000001,-0.756000000000001,-0.752000000000001,-0.748000000000001,
-0.744000000000001,-0.740000000000001,-0.736000000000001,-0.732000000000001,
-0.728000000000001,-0.724000000000001,-0.720000000000001,-0.716000000000001,
-0.712000000000001,-0.708000000000001,-0.704000000000001,-0.700000000000001,
-0.696000000000001,-0.692000000000001,-0.688000000000001,-0.684,-0.68,-0.676,
-0.672,-0.668,-0.664,-0.66,-0.656,-0.652,-0.648,-0.644,-0.64,-0.636,-0.632,
-0.628,-0.624,-0.62,-0.616,-0.612,-0.608,-0.604,-0.6,-0.596,-0.592,-0.588,
-0.584,-0.58,-0.576,-0.572,-0.568,-0.564,-0.56,-0.556,-0.552,-0.548,-0.544,
-0.54,-0.536,-0.532,-0.528,-0.524,-0.52,-0.516,-0.512,-0.508,-0.504,-0.5,
-0.496,-0.492,-0.488,-0.484,-0.48,-0.476,-0.472,-0.468,-0.464,-0.46,-0.456,
-0.452,-0.448,-0.444,-0.44,-0.436,-0.432,-0.428,-0.424,-0.42,-0.416,-0.412,
-0.408,-0.404,-0.4,-0.396,-0.392,-0.388,-0.384,-0.38,-0.376,-0.372,-0.368,
-0.364,-0.36,-0.356,-0.352,-0.348,-0.344,-0.34,-0.336,-0.332,-0.328,-0.324,
-0.32,-0.316,-0.312,-0.308,-0.304,-0.3,-0.296,-0.292,-0.288,-0.284,-0.28,
-0.276,-0.272,-0.268,-0.264,-0.26,-0.256,-0.252,-0.248,-0.244,-0.24,-0.236,
-0.232,-0.228,-0.224,-0.22,-0.216,-0.212,-0.208,-0.204,-0.2,-0.196,-0.192,
-0.188,-0.184,-0.18,-0.176,-0.172,-0.168,-0.164,-0.16,-0.156,-0.152,-0.148,
-0.144,-0.14,-0.136,-0.132,-0.128,-0.124,-0.12,-0.116,-0.112,-0.108,-0.104,
-0.1,-0.0960000000000001,-0.0920000000000001,-0.0880000000000001,-0.084,
-0.08,-0.076,-0.072,-0.068,-0.064,-0.06,-0.056,-0.052,-0.048,-0.044,-0.04,
-0.036,-0.032,-0.028,-0.024,-0.02,-0.016,-0.012,-0.008,-0.004,0.,0.00399999999999923,
0.00799999999999923,0.0119999999999992,0.0159999999999992,0.0199999999999992,
0.0239999999999992,0.0279999999999992,0.0319999999999993,0.0359999999999993,
0.0399999999999993,0.0439999999999993,0.0479999999999993,0.0519999999999993,
0.0559999999999993,0.0599999999999993,0.0614099587825321),(0.,0.936109769296308),
 .UNSPECIFIED.);
#338=B_SPLINE_SURFACE_WITH_KNOTS('',3,3,((#19994,#19995,#19996,#19997,#19998,
#19999,#20000,#20001,#20002,#20003,#20004,#20005,#20006,#20007,#20008,#20009,
#20010,#20011,#20012,#20013,#20014,#20015,#20016,#20017,#20018,#20019,#20020,
#20021,#20022,#20023,#20024,#20025,#20026,#20027),(#20028,#20029,#20030,
#20031,#20032,#20033,#20034,#20035,#20036,#20037,#20038,#20039,#20040,#20041,
#20042,#20043,#20044,#20045,#20046,#20047,#20048,#20049,#20050,#20051,#20052,
#20053,#20054,#20055,#20056,#20057,#20058,#20059,#20060,#20061),(#20062,
#20063,#20064,#20065,#20066,#20067,#20068,#20069,#20070,#20071,#20072,#20073,
#20074,#20075,#20076,#20077,#20078,#20079,#20080,#20081,#20082,#20083,#20084,
#20085,#20086,#20087,#20088,#20089,#20090,#20091,#20092,#20093,#20094,#20095),
(#20096,#20097,#20098,#20099,#20100,#20101,#20102,#20103,#20104,#20105,
#20106,#20107,#20108,#20109,#20110,#20111,#20112,#20113,#20114,#20115,#20116,
#20117,#20118,#20119,#20120,#20121,#20122,#20123,#20124,#20125,#20126,#20127,
#20128,#20129),(#20130,#20131,#20132,#20133,#20134,#20135,#20136,#20137,
#20138,#20139,#20140,#20141,#20142,#20143,#20144,#20145,#20146,#20147,#20148,
#20149,#20150,#20151,#20152,#20153,#20154,#20155,#20156,#20157,#20158,#20159,
#20160,#20161,#20162,#20163)),.UNSPECIFIED.,.F.,.F.,.F.,(4,1,4),(4,1,1,
1,1,1,1,1,1,1,1,1,1,1,1,1,1,1,1,1,1,1,1,1,1,1,1,1,1,1,1,4),(0.,0.571428571428571,
1.),(0.,0.438300757907035,0.876601515814069,1.3149022737211,1.75320303162814,
2.19150378953517,2.62980454744221,3.50640606325628,4.01775694748115,4.09080707379899,
4.6752080843417,4.96740858961306,5.11350884224874,5.25960909488442,5.55180960015577,
5.84401010542713,6.42841111596984,7.01281212651256,7.30501263178391,7.59721313705527,
8.18161414759798,8.76601515814069,9.05821566341205,9.35041616868341,9.64261667395476,
9.93481717922612,10.5192181897688,10.6287933792456,10.9575189476759,11.3958197055829,
11.8341204634899,12.272421221397),.UNSPECIFIED.);
#339=B_SPLINE_SURFACE_WITH_KNOTS('',3,3,((#20178,#20179,#20180,#20181),
(#20182,#20183,#20184,#20185),(#20186,#20187,#20188,#20189),(#20190,#20191,
#20192,#20193),(#20194,#20195,#20196,#20197)),.UNSPECIFIED.,.F.,.F.,.F.,
(4,1,4),(4,4),(0.,0.571428571428571,1.),(0.,0.164738445253465),
 .UNSPECIFIED.);
#340=B_SPLINE_SURFACE_WITH_KNOTS('',3,3,((#20212,#20213,#20214,#20215),
(#20216,#20217,#20218,#20219),(#20220,#20221,#20222,#20223),(#20224,#20225,
#20226,#20227),(#20228,#20229,#20230,#20231)),.UNSPECIFIED.,.F.,.F.,.F.,
(4,1,4),(4,4),(0.,0.571428571428571,1.),(0.,0.0754181362626584),
 .UNSPECIFIED.);
#341=B_SPLINE_SURFACE_WITH_KNOTS('',3,3,((#20243,#20244,#20245,#20246),
(#20247,#20248,#20249,#20250),(#20251,#20252,#20253,#20254),(#20255,#20256,
#20257,#20258),(#20259,#20260,#20261,#20262)),.UNSPECIFIED.,.F.,.F.,.F.,
(4,1,4),(4,4),(0.,0.571428571428571,1.),(0.,0.0505696713863416),
 .UNSPECIFIED.);
#342=B_SPLINE_SURFACE_WITH_KNOTS('',3,3,((#20274,#20275,#20276,#20277,#20278),
(#20279,#20280,#20281,#20282,#20283),(#20284,#20285,#20286,#20287,#20288),
(#20289,#20290,#20291,#20292,#20293),(#20294,#20295,#20296,#20297,#20298)),
 .UNSPECIFIED.,.F.,.F.,.F.,(4,1,4),(4,1,4),(0.,0.571428571428571,1.),(0.,
0.0837730396707311,0.167546079341462),.UNSPECIFIED.);
#343=B_SPLINE_SURFACE_WITH_KNOTS('',3,3,((#20309,#20310,#20311,#20312,#20313),
(#20314,#20315,#20316,#20317,#20318),(#20319,#20320,#20321,#20322,#20323),
(#20324,#20325,#20326,#20327,#20328),(#20329,#20330,#20331,#20332,#20333)),
 .UNSPECIFIED.,.F.,.F.,.F.,(4,1,4),(4,1,4),(-2.33603068056626E-9,0.571428571428571,
1.00000203313126),(-0.0971295855432269,-0.0737466502954258,-0.0503637127115938),
 .UNSPECIFIED.);
#344=B_SPLINE_SURFACE_WITH_KNOTS('',5,1,((#20382,#20383),(#20384,#20385),
(#20386,#20387),(#20388,#20389),(#20390,#20391),(#20392,#20393),(#20394,
#20395),(#20396,#20397),(#20398,#20399),(#20400,#20401),(#20402,#20403),
(#20404,#20405),(#20406,#20407),(#20408,#20409),(#20410,#20411),(#20412,
#20413),(#20414,#20415),(#20416,#20417),(#20418,#20419),(#20420,#20421),
(#20422,#20423),(#20424,#20425),(#20426,#20427),(#20428,#20429)),
 .UNSPECIFIED.,.F.,.F.,.F.,(6,1,1,1,1,1,1,1,1,1,1,1,1,1,1,1,1,1,1,6),(2,
2),(-0.421786698696643,-0.42,-0.416,-0.412,-0.408,-0.404,-0.4,-0.396,-0.392,
-0.388,-0.384,-0.38,-0.376,-0.372,-0.368,-0.364,-0.36,-0.356,-0.352,-0.351983647406963),
(0.,7.2),.UNSPECIFIED.);
#345=B_SPLINE_SURFACE_WITH_KNOTS('',3,3,((#20446,#20447,#20448,#20449),
(#20450,#20451,#20452,#20453),(#20454,#20455,#20456,#20457),(#20458,#20459,
#20460,#20461)),.UNSPECIFIED.,.F.,.F.,.F.,(4,4),(4,4),(-2.28168025676385E-5,
1.),(-0.0965691449411131,-0.0938109728066715),.UNSPECIFIED.);
#346=B_SPLINE_SURFACE_WITH_KNOTS('',3,3,((#20463,#20464,#20465,#20466,#20467,
#20468,#20469,#20470,#20471,#20472,#20473,#20474,#20475,#20476,#20477,#20478,
#20479,#20480,#20481,#20482),(#20483,#20484,#20485,#20486,#20487,#20488,
#20489,#20490,#20491,#20492,#20493,#20494,#20495,#20496,#20497,#20498,#20499,
#20500,#20501,#20502),(#20503,#20504,#20505,#20506,#20507,#20508,#20509,
#20510,#20511,#20512,#20513,#20514,#20515,#20516,#20517,#20518,#20519,#20520,
#20521,#20522),(#20523,#20524,#20525,#20526,#20527,#20528,#20529,#20530,
#20531,#20532,#20533,#20534,#20535,#20536,#20537,#20538,#20539,#20540,#20541,
#20542),(#20543,#20544,#20545,#20546,#20547,#20548,#20549,#20550,#20551,
#20552,#20553,#20554,#20555,#20556,#20557,#20558,#20559,#20560,#20561,#20562)),
 .UNSPECIFIED.,.F.,.F.,.F.,(4,1,4),(4,1,1,1,1,1,1,1,1,1,1,1,1,1,1,1,1,4),
(0.,0.571428571428571,1.),(0.,0.197097619692083,0.394195239384165,0.689841668922289,
0.78839047876833,0.886939288614372,0.985488098460413,1.08403690830645,1.1825857181525,
1.37968333784458,1.47823214769062,1.57678095753666,1.62605536245968,1.6753297673827,
1.77387857722874,1.97097619692083,2.36517143630499,2.75936667568916),
 .UNSPECIFIED.);
#347=B_SPLINE_SURFACE_WITH_KNOTS('',3,3,((#20785,#20786,#20787,#20788),
(#20789,#20790,#20791,#20792),(#20793,#20794,#20795,#20796),(#20797,#20798,
#20799,#20800),(#20801,#20802,#20803,#20804)),.UNSPECIFIED.,.F.,.F.,.F.,
(4,1,4),(4,4),(0.,0.571428571428571,1.),(0.,0.304037814733278),
 .UNSPECIFIED.);
#348=B_SPLINE_SURFACE_WITH_KNOTS('',3,3,((#20816,#20817,#20818,#20819,#20820,
#20821,#20822,#20823,#20824,#20825,#20826,#20827,#20828,#20829,#20830,#20831,
#20832,#20833,#20834,#20835,#20836),(#20837,#20838,#20839,#20840,#20841,
#20842,#20843,#20844,#20845,#20846,#20847,#20848,#20849,#20850,#20851,#20852,
#20853,#20854,#20855,#20856,#20857),(#20858,#20859,#20860,#20861,#20862,
#20863,#20864,#20865,#20866,#20867,#20868,#20869,#20870,#20871,#20872,#20873,
#20874,#20875,#20876,#20877,#20878),(#20879,#20880,#20881,#20882,#20883,
#20884,#20885,#20886,#20887,#20888,#20889,#20890,#20891,#20892,#20893,#20894,
#20895,#20896,#20897,#20898,#20899),(#20900,#20901,#20902,#20903,#20904,
#20905,#20906,#20907,#20908,#20909,#20910,#20911,#20912,#20913,#20914,#20915,
#20916,#20917,#20918,#20919,#20920)),.UNSPECIFIED.,.F.,.F.,.F.,(4,1,4),
(4,1,1,1,1,1,1,1,1,1,1,1,1,1,1,1,1,1,4),(0.,0.571428571428571,1.),(0.,0.148302061038192,
0.296604122076384,0.444906183114576,0.593208244152768,0.889812366229152,
1.18641648830554,1.7796247324583,2.37283297661107,4.74566595322215,5.93208244152768,
6.52529068568045,7.11849892983322,7.4151030519096,7.71170717398599,7.86000923502418,
8.00831129606237,8.15661335710056,8.30491541813876),.UNSPECIFIED.);
#349=B_SPLINE_SURFACE_WITH_KNOTS('',3,3,((#20946,#20947,#20948,#20949),
(#20950,#20951,#20952,#20953),(#20954,#20955,#20956,#20957),(#20958,#20959,
#20960,#20961),(#20962,#20963,#20964,#20965)),.UNSPECIFIED.,.F.,.F.,.F.,
(4,1,4),(4,4),(0.,0.571428571428571,1.),(0.,0.0801298062965183),
 .UNSPECIFIED.);
#350=B_SPLINE_SURFACE_WITH_KNOTS('',3,3,((#20974,#20975,#20976,#20977),
(#20978,#20979,#20980,#20981),(#20982,#20983,#20984,#20985),(#20986,#20987,
#20988,#20989),(#20990,#20991,#20992,#20993)),.UNSPECIFIED.,.F.,.F.,.F.,
(4,1,4),(4,4),(0.,0.571428571428571,1.),(0.0423193643606908,0.252933252504432),
 .UNSPECIFIED.);
#351=B_SPLINE_SURFACE_WITH_KNOTS('',3,3,((#20995,#20996,#20997,#20998),
(#20999,#21000,#21001,#21002),(#21003,#21004,#21005,#21006),(#21007,#21008,
#21009,#21010),(#21011,#21012,#21013,#21014)),.UNSPECIFIED.,.F.,.F.,.F.,
(4,1,4),(4,4),(0.,0.571428571428571,1.),(2.65444323739948E-13,0.080129806296636),
 .UNSPECIFIED.);
#352=B_SPLINE_SURFACE_WITH_KNOTS('',3,3,((#21199,#21200,#21201,#21202),
(#21203,#21204,#21205,#21206),(#21207,#21208,#21209,#21210),(#21211,#21212,
#21213,#21214),(#21215,#21216,#21217,#21218)),.UNSPECIFIED.,.F.,.F.,.F.,
(4,1,4),(4,4),(0.,0.571428571428571,1.),(0.,0.0200337106211744),
 .UNSPECIFIED.);
#353=B_SPLINE_SURFACE_WITH_KNOTS('',3,3,((#21222,#21223,#21224,#21225),
(#21226,#21227,#21228,#21229),(#21230,#21231,#21232,#21233),(#21234,#21235,
#21236,#21237),(#21238,#21239,#21240,#21241)),.UNSPECIFIED.,.F.,.F.,.F.,
(4,1,4),(4,4),(0.,0.571428571428571,1.),(0.,0.357185215222936),
 .UNSPECIFIED.);
#354=B_SPLINE_SURFACE_WITH_KNOTS('',3,3,((#21248,#21249,#21250,#21251,#21252,
#21253),(#21254,#21255,#21256,#21257,#21258,#21259),(#21260,#21261,#21262,
#21263,#21264,#21265),(#21266,#21267,#21268,#21269,#21270,#21271),(#21272,
#21273,#21274,#21275,#21276,#21277)),.UNSPECIFIED.,.F.,.F.,.F.,(4,1,4),
(4,1,1,4),(0.,0.5,1.),(0.0650388601395548,0.184879728366205,0.264773640517305,
0.344667552668405),.UNSPECIFIED.);
#355=B_SPLINE_SURFACE_WITH_KNOTS('',3,3,((#21288,#21289,#21290,#21291),
(#21292,#21293,#21294,#21295),(#21296,#21297,#21298,#21299),(#21300,#21301,
#21302,#21303),(#21304,#21305,#21306,#21307)),.UNSPECIFIED.,.F.,.F.,.F.,
(4,1,4),(4,4),(0.,0.571428571428571,1.),(0.,0.0647166470509305),
 .UNSPECIFIED.);
#356=B_SPLINE_SURFACE_WITH_KNOTS('',3,3,((#21309,#21310,#21311,#21312),
(#21313,#21314,#21315,#21316),(#21317,#21318,#21319,#21320),(#21321,#21322,
#21323,#21324)),.UNSPECIFIED.,.F.,.F.,.F.,(4,4),(4,4),(0.,1.),(0.,0.0229846076752987),
 .UNSPECIFIED.);
#357=B_SPLINE_SURFACE_WITH_KNOTS('',5,1,((#21330,#21331),(#21332,#21333),
(#21334,#21335),(#21336,#21337),(#21338,#21339),(#21340,#21341),(#21342,
#21343),(#21344,#21345),(#21346,#21347),(#21348,#21349),(#21350,#21351),
(#21352,#21353),(#21354,#21355),(#21356,#21357),(#21358,#21359),(#21360,
#21361),(#21362,#21363),(#21364,#21365),(#21366,#21367),(#21368,#21369),
(#21370,#21371),(#21372,#21373),(#21374,#21375),(#21376,#21377),(#21378,
#21379),(#21380,#21381),(#21382,#21383),(#21384,#21385),(#21386,#21387),
(#21388,#21389),(#21390,#21391),(#21392,#21393),(#21394,#21395),(#21396,
#21397),(#21398,#21399),(#21400,#21401),(#21402,#21403),(#21404,#21405),
(#21406,#21407),(#21408,#21409),(#21410,#21411),(#21412,#21413),(#21414,
#21415),(#21416,#21417),(#21418,#21419),(#21420,#21421),(#21422,#21423),
(#21424,#21425),(#21426,#21427),(#21428,#21429),(#21430,#21431),(#21432,
#21433),(#21434,#21435),(#21436,#21437),(#21438,#21439),(#21440,#21441),
(#21442,#21443),(#21444,#21445),(#21446,#21447),(#21448,#21449),(#21450,
#21451),(#21452,#21453),(#21454,#21455),(#21456,#21457),(#21458,#21459),
(#21460,#21461),(#21462,#21463),(#21464,#21465),(#21466,#21467),(#21468,
#21469),(#21470,#21471),(#21472,#21473),(#21474,#21475),(#21476,#21477),
(#21478,#21479),(#21480,#21481),(#21482,#21483),(#21484,#21485),(#21486,
#21487),(#21488,#21489),(#21490,#21491),(#21492,#21493),(#21494,#21495),
(#21496,#21497),(#21498,#21499),(#21500,#21501),(#21502,#21503),(#21504,
#21505),(#21506,#21507),(#21508,#21509),(#21510,#21511),(#21512,#21513),
(#21514,#21515),(#21516,#21517),(#21518,#21519),(#21520,#21521),(#21522,
#21523),(#21524,#21525),(#21526,#21527),(#21528,#21529),(#21530,#21531),
(#21532,#21533),(#21534,#21535),(#21536,#21537),(#21538,#21539),(#21540,
#21541),(#21542,#21543),(#21544,#21545),(#21546,#21547),(#21548,#21549),
(#21550,#21551),(#21552,#21553),(#21554,#21555),(#21556,#21557),(#21558,
#21559),(#21560,#21561),(#21562,#21563),(#21564,#21565),(#21566,#21567),
(#21568,#21569),(#21570,#21571),(#21572,#21573),(#21574,#21575),(#21576,
#21577),(#21578,#21579),(#21580,#21581),(#21582,#21583),(#21584,#21585),
(#21586,#21587),(#21588,#21589),(#21590,#21591),(#21592,#21593),(#21594,
#21595),(#21596,#21597),(#21598,#21599),(#21600,#21601),(#21602,#21603),
(#21604,#21605),(#21606,#21607),(#21608,#21609),(#21610,#21611),(#21612,
#21613),(#21614,#21615),(#21616,#21617),(#21618,#21619),(#21620,#21621),
(#21622,#21623),(#21624,#21625),(#21626,#21627),(#21628,#21629),(#21630,
#21631),(#21632,#21633),(#21634,#21635),(#21636,#21637),(#21638,#21639),
(#21640,#21641),(#21642,#21643),(#21644,#21645),(#21646,#21647),(#21648,
#21649),(#21650,#21651),(#21652,#21653),(#21654,#21655),(#21656,#21657),
(#21658,#21659),(#21660,#21661),(#21662,#21663),(#21664,#21665),(#21666,
#21667),(#21668,#21669),(#21670,#21671),(#21672,#21673),(#21674,#21675),
(#21676,#21677),(#21678,#21679),(#21680,#21681),(#21682,#21683),(#21684,
#21685),(#21686,#21687),(#21688,#21689),(#21690,#21691),(#21692,#21693),
(#21694,#21695),(#21696,#21697),(#21698,#21699),(#21700,#21701),(#21702,
#21703),(#21704,#21705),(#21706,#21707),(#21708,#21709),(#21710,#21711),
(#21712,#21713),(#21714,#21715),(#21716,#21717),(#21718,#21719),(#21720,
#21721),(#21722,#21723),(#21724,#21725),(#21726,#21727),(#21728,#21729),
(#21730,#21731),(#21732,#21733),(#21734,#21735),(#21736,#21737),(#21738,
#21739),(#21740,#21741),(#21742,#21743),(#21744,#21745),(#21746,#21747),
(#21748,#21749),(#21750,#21751),(#21752,#21753),(#21754,#21755),(#21756,
#21757),(#21758,#21759),(#21760,#21761),(#21762,#21763),(#21764,#21765),
(#21766,#21767),(#21768,#21769),(#21770,#21771),(#21772,#21773),(#21774,
#21775),(#21776,#21777),(#21778,#21779),(#21780,#21781),(#21782,#21783),
(#21784,#21785),(#21786,#21787),(#21788,#21789),(#21790,#21791),(#21792,
#21793),(#21794,#21795),(#21796,#21797),(#21798,#21799),(#21800,#21801),
(#21802,#21803),(#21804,#21805),(#21806,#21807),(#21808,#21809),(#21810,
#21811),(#21812,#21813),(#21814,#21815),(#21816,#21817),(#21818,#21819),
(#21820,#21821),(#21822,#21823),(#21824,#21825),(#21826,#21827),(#21828,
#21829),(#21830,#21831),(#21832,#21833),(#21834,#21835),(#21836,#21837),
(#21838,#21839),(#21840,#21841),(#21842,#21843),(#21844,#21845),(#21846,
#21847),(#21848,#21849)),.UNSPECIFIED.,.T.,.F.,.F.,(6,1,1,1,1,1,1,1,1,1,
1,1,1,1,1,1,1,1,1,1,1,1,1,1,1,1,1,1,1,1,1,1,1,1,1,1,1,1,1,1,1,1,1,1,1,1,
1,1,1,1,1,1,1,1,1,1,1,1,1,1,1,1,1,1,1,1,1,1,1,1,1,1,1,1,1,1,1,1,1,1,1,1,
1,1,1,1,1,1,1,1,1,1,1,1,1,1,1,1,1,1,1,1,1,1,1,1,1,1,1,1,1,1,1,1,1,1,1,1,
1,1,1,1,1,1,1,1,1,1,1,1,1,1,1,1,1,1,1,1,1,1,1,1,1,1,1,1,1,1,1,1,1,1,1,1,
1,1,1,1,1,1,1,1,1,1,1,1,1,1,1,1,1,1,1,1,1,1,1,1,1,1,1,1,1,1,1,1,1,1,1,1,
1,1,1,1,1,1,1,1,1,1,1,1,1,1,1,1,1,1,1,1,1,1,1,1,1,1,1,1,1,1,1,1,1,1,1,1,
1,1,1,1,1,1,1,1,1,5,1,1,1,1,1,1,1,1,1,1,1,1,1,1,1,6),(2,2),(-0.938590041217468,
-0.936000000000001,-0.932000000000001,-0.928000000000001,-0.924000000000001,
-0.920000000000001,-0.916000000000001,-0.912000000000001,-0.908000000000001,
-0.904000000000001,-0.900000000000001,-0.896000000000001,-0.892000000000001,
-0.888000000000001,-0.884000000000001,-0.880000000000001,-0.876000000000001,
-0.872000000000001,-0.868000000000001,-0.864000000000001,-0.860000000000001,
-0.856000000000001,-0.852000000000001,-0.848000000000001,-0.844000000000001,
-0.840000000000001,-0.836000000000001,-0.832000000000001,-0.828000000000001,
-0.824000000000001,-0.820000000000001,-0.816000000000001,-0.812000000000001,
-0.808000000000001,-0.804000000000001,-0.800000000000001,-0.796000000000001,
-0.792000000000001,-0.788000000000001,-0.784000000000001,-0.780000000000001,
-0.776000000000001,-0.772000000000001,-0.768000000000001,-0.764000000000001,
-0.760000000000001,-0.756000000000001,-0.752000000000001,-0.748000000000001,
-0.744000000000001,-0.740000000000001,-0.736000000000001,-0.732000000000001,
-0.728000000000001,-0.724000000000001,-0.720000000000001,-0.716000000000001,
-0.712000000000001,-0.708000000000001,-0.704000000000001,-0.700000000000001,
-0.696000000000001,-0.692000000000001,-0.688000000000001,-0.684,-0.68,-0.676,
-0.672,-0.668,-0.664,-0.66,-0.656,-0.652,-0.648,-0.644,-0.64,-0.636,-0.632,
-0.628,-0.624,-0.62,-0.616,-0.612,-0.608,-0.604,-0.6,-0.596,-0.592,-0.588,
-0.584,-0.58,-0.576,-0.572,-0.568,-0.564,-0.56,-0.556,-0.552,-0.548,-0.544,
-0.54,-0.536,-0.532,-0.528,-0.524,-0.52,-0.516,-0.512,-0.508,-0.504,-0.5,
-0.496,-0.492,-0.488,-0.484,-0.48,-0.476,-0.472,-0.468,-0.464,-0.46,-0.456,
-0.452,-0.448,-0.444,-0.44,-0.436,-0.432,-0.428,-0.424,-0.42,-0.416,-0.412,
-0.408,-0.404,-0.4,-0.396,-0.392,-0.388,-0.384,-0.38,-0.376,-0.372,-0.368,
-0.364,-0.36,-0.356,-0.352,-0.348,-0.344,-0.34,-0.336,-0.332,-0.328,-0.324,
-0.32,-0.316,-0.312,-0.308,-0.304,-0.3,-0.296,-0.292,-0.288,-0.284,-0.28,
-0.276,-0.272,-0.268,-0.264,-0.26,-0.256,-0.252,-0.248,-0.244,-0.24,-0.236,
-0.232,-0.228,-0.224,-0.22,-0.216,-0.212,-0.208,-0.204,-0.2,-0.196,-0.192,
-0.188,-0.184,-0.18,-0.176,-0.172,-0.168,-0.164,-0.16,-0.156,-0.152,-0.148,
-0.144,-0.14,-0.136,-0.132,-0.128,-0.124,-0.12,-0.116,-0.112,-0.108,-0.104,
-0.1,-0.0960000000000001,-0.0920000000000001,-0.0880000000000001,-0.084,
-0.08,-0.076,-0.072,-0.068,-0.064,-0.06,-0.056,-0.052,-0.048,-0.044,-0.04,
-0.036,-0.032,-0.028,-0.024,-0.02,-0.016,-0.012,-0.008,-0.004,0.,0.00399999999999923,
0.00799999999999923,0.0119999999999992,0.0159999999999992,0.0199999999999992,
0.0239999999999992,0.0279999999999992,0.0319999999999993,0.0359999999999993,
0.0399999999999993,0.0439999999999993,0.0479999999999993,0.0519999999999993,
0.0559999999999993,0.0599999999999993,0.0614099587825321),(0.,0.8496),
 .UNSPECIFIED.);
#358=B_SPLINE_SURFACE_WITH_KNOTS('',3,3,((#21860,#21861,#21862,#21863,#21864),
(#21865,#21866,#21867,#21868,#21869),(#21870,#21871,#21872,#21873,#21874),
(#21875,#21876,#21877,#21878,#21879),(#21880,#21881,#21882,#21883,#21884),
(#21885,#21886,#21887,#21888,#21889)),.UNSPECIFIED.,.F.,.F.,.F.,(4,1,1,
4),(4,1,4),(-6.44657208043772E-5,0.285714285714286,0.571428571428571,1.),
(0.0475827460273853,0.473360639981091,1.04097854429163),.UNSPECIFIED.);
#359=B_SPLINE_SURFACE_WITH_KNOTS('',3,3,((#21920,#21921,#21922,#21923,#21924,
#21925),(#21926,#21927,#21928,#21929,#21930,#21931),(#21932,#21933,#21934,
#21935,#21936,#21937),(#21938,#21939,#21940,#21941,#21942,#21943),(#21944,
#21945,#21946,#21947,#21948,#21949),(#21950,#21951,#21952,#21953,#21954,
#21955)),.UNSPECIFIED.,.F.,.F.,.F.,(4,1,1,4),(4,1,1,4),(0.331395853675239,
0.617940487814422,0.808970243907211,1.),(-0.0266531801543891,0.336302079828547,
0.698984668949978,1.24300855263212),.UNSPECIFIED.);
#360=B_SPLINE_SURFACE_WITH_KNOTS('',3,3,((#21956,#21957,#21958,#21959),
(#21960,#21961,#21962,#21963),(#21964,#21965,#21966,#21967),(#21968,#21969,
#21970,#21971),(#21972,#21973,#21974,#21975)),.UNSPECIFIED.,.F.,.F.,.F.,
(4,1,4),(4,4),(0.,0.571428571428571,1.),(0.19533758964745,0.254963272600067),
 .UNSPECIFIED.);
#361=B_SPLINE_SURFACE_WITH_KNOTS('',3,3,((#21983,#21984,#21985,#21986),
(#21987,#21988,#21989,#21990),(#21991,#21992,#21993,#21994),(#21995,#21996,
#21997,#21998),(#21999,#22000,#22001,#22002)),.UNSPECIFIED.,.F.,.F.,.F.,
(4,1,4),(4,4),(0.,0.571428571428571,1.),(2.63411853293822E-13,0.0801298062968181),
 .UNSPECIFIED.);
#362=B_SPLINE_SURFACE_WITH_KNOTS('',3,1,((#22009,#22010),(#22011,#22012),
(#22013,#22014),(#22015,#22016),(#22017,#22018)),.UNSPECIFIED.,.F.,.F.,
 .F.,(4,1,4),(2,2),(0.,0.5,1.),(0.,0.6),.UNSPECIFIED.);
#363=B_SPLINE_SURFACE_WITH_KNOTS('',3,3,((#22052,#22053,#22054,#22055,#22056),
(#22057,#22058,#22059,#22060,#22061),(#22062,#22063,#22064,#22065,#22066),
(#22067,#22068,#22069,#22070,#22071),(#22072,#22073,#22074,#22075,#22076),
(#22077,#22078,#22079,#22080,#22081)),.UNSPECIFIED.,.F.,.F.,.F.,(4,1,1,
4),(4,1,4),(-1.51321272498462E-5,0.285714285714286,0.571428571428571,1.),
(-6.52754885944507E-7,0.0874114081347553,0.17493857403387),
 .UNSPECIFIED.);
#364=B_SPLINE_SURFACE_WITH_KNOTS('',3,1,((#22105,#22106),(#22107,#22108),
(#22109,#22110),(#22111,#22112),(#22113,#22114)),.UNSPECIFIED.,.F.,.F.,
 .F.,(4,1,4),(2,2),(0.239075842950699,0.619537921475349,1.),(0.,0.410906527432635),
 .UNSPECIFIED.);
#365=B_SPLINE_SURFACE_WITH_KNOTS('',3,3,((#22118,#22119,#22120,#22121,#22122,
#22123),(#22124,#22125,#22126,#22127,#22128,#22129),(#22130,#22131,#22132,
#22133,#22134,#22135),(#22136,#22137,#22138,#22139,#22140,#22141),(#22142,
#22143,#22144,#22145,#22146,#22147)),.UNSPECIFIED.,.F.,.F.,.F.,(4,1,4),
(4,1,1,4),(0.,0.571428571428571,1.),(0.,0.107642143366443,0.179403572277406,
0.251165001188368),.UNSPECIFIED.);
#366=B_SPLINE_SURFACE_WITH_KNOTS('',3,3,((#22154,#22155,#22156,#22157),
(#22158,#22159,#22160,#22161),(#22162,#22163,#22164,#22165),(#22166,#22167,
#22168,#22169),(#22170,#22171,#22172,#22173)),.UNSPECIFIED.,.F.,.F.,.F.,
(4,1,4),(4,4),(0.,0.571428571428571,1.),(0.00243784671109485,0.137031673359032),
 .UNSPECIFIED.);
#367=B_SPLINE_SURFACE_WITH_KNOTS('',3,3,((#22182,#22183,#22184,#22185),
(#22186,#22187,#22188,#22189),(#22190,#22191,#22192,#22193),(#22194,#22195,
#22196,#22197),(#22198,#22199,#22200,#22201)),.UNSPECIFIED.,.F.,.F.,.F.,
(4,1,4),(4,4),(0.,0.571428571428571,1.),(0.,0.033167786256901),
 .UNSPECIFIED.);
#368=B_SPLINE_SURFACE_WITH_KNOTS('',3,3,((#22207,#22208,#22209,#22210,#22211,
#22212,#22213,#22214,#22215,#22216,#22217,#22218,#22219,#22220,#22221,#22222,
#22223,#22224,#22225,#22226),(#22227,#22228,#22229,#22230,#22231,#22232,
#22233,#22234,#22235,#22236,#22237,#22238,#22239,#22240,#22241,#22242,#22243,
#22244,#22245,#22246),(#22247,#22248,#22249,#22250,#22251,#22252,#22253,
#22254,#22255,#22256,#22257,#22258,#22259,#22260,#22261,#22262,#22263,#22264,
#22265,#22266),(#22267,#22268,#22269,#22270,#22271,#22272,#22273,#22274,
#22275,#22276,#22277,#22278,#22279,#22280,#22281,#22282,#22283,#22284,#22285,
#22286),(#22287,#22288,#22289,#22290,#22291,#22292,#22293,#22294,#22295,
#22296,#22297,#22298,#22299,#22300,#22301,#22302,#22303,#22304,#22305,#22306)),
 .UNSPECIFIED.,.F.,.F.,.F.,(4,1,4),(4,1,1,1,1,1,1,1,1,1,1,1,1,1,1,1,1,4),
(0.,0.571428571428571,1.),(0.00458897054204579,0.398834822329043,0.79308067411604,
0.990203600009539,1.02305742099179,1.05591124197404,1.12161888393854,1.18732652590304,
1.31874180983204,1.45015709376104,1.58157237769003,1.68013384063678,1.77869530358353,
1.97581822947703,2.07437969242378,2.17294115537053,2.37006408126403,2.76430993305103),
 .UNSPECIFIED.);
#369=B_SPLINE_SURFACE_WITH_KNOTS('',3,3,((#22503,#22504,#22505,#22506),
(#22507,#22508,#22509,#22510),(#22511,#22512,#22513,#22514),(#22515,#22516,
#22517,#22518)),.UNSPECIFIED.,.F.,.F.,.F.,(4,4),(4,4),(0.461946105359466,
1.),(-0.919615460485724,-0.751979757135207),.UNSPECIFIED.);
#370=B_SPLINE_SURFACE_WITH_KNOTS('',3,3,((#22527,#22528,#22529,#22530),
(#22531,#22532,#22533,#22534),(#22535,#22536,#22537,#22538),(#22539,#22540,
#22541,#22542),(#22543,#22544,#22545,#22546)),.UNSPECIFIED.,.F.,.F.,.F.,
(4,1,4),(4,4),(0.,0.571428571428571,1.),(0.0177382428884037,0.0280297096615123),
 .UNSPECIFIED.);
#371=B_SPLINE_SURFACE_WITH_KNOTS('',3,3,((#22549,#22550,#22551,#22552),
(#22553,#22554,#22555,#22556),(#22557,#22558,#22559,#22560),(#22561,#22562,
#22563,#22564)),.UNSPECIFIED.,.F.,.F.,.F.,(4,4),(4,4),(0.,1.),(0.0797065098565302,
0.419743206478425),.UNSPECIFIED.);
#372=B_SPLINE_SURFACE_WITH_KNOTS('',5,1,((#22575,#22576),(#22577,#22578),
(#22579,#22580),(#22581,#22582),(#22583,#22584),(#22585,#22586),(#22587,
#22588),(#22589,#22590),(#22591,#22592),(#22593,#22594),(#22595,#22596),
(#22597,#22598),(#22599,#22600),(#22601,#22602),(#22603,#22604),(#22605,
#22606),(#22607,#22608),(#22609,#22610),(#22611,#22612),(#22613,#22614),
(#22615,#22616),(#22617,#22618),(#22619,#22620),(#22621,#22622)),
 .UNSPECIFIED.,.F.,.F.,.F.,(6,1,1,1,1,1,1,1,1,1,1,1,1,1,1,1,1,1,1,6),(2,
2),(-0.421786698696643,-0.42,-0.416,-0.412,-0.408,-0.404,-0.4,-0.396,-0.392,
-0.388,-0.384,-0.38,-0.376,-0.372,-0.368,-0.364,-0.36,-0.356,-0.352,-0.351983647406963),
(0.,0.600000000000009),.UNSPECIFIED.);
#373=B_SPLINE_SURFACE_WITH_KNOTS('',3,3,((#22624,#22625,#22626,#22627),
(#22628,#22629,#22630,#22631),(#22632,#22633,#22634,#22635),(#22636,#22637,
#22638,#22639)),.UNSPECIFIED.,.F.,.F.,.F.,(4,4),(4,4),(0.,1.),(0.0253342885542915,
0.430969252801444),.UNSPECIFIED.);
#374=B_SPLINE_SURFACE_WITH_KNOTS('',3,1,((#22640,#22641),(#22642,#22643),
(#22644,#22645),(#22646,#22647),(#22648,#22649)),.UNSPECIFIED.,.F.,.F.,
 .F.,(4,1,4),(2,2),(0.,0.571428571428571,1.),(0.,0.504),.UNSPECIFIED.);
#375=B_SPLINE_SURFACE_WITH_KNOTS('',3,3,((#22651,#22652,#22653,#22654),
(#22655,#22656,#22657,#22658),(#22659,#22660,#22661,#22662),(#22663,#22664,
#22665,#22666),(#22667,#22668,#22669,#22670)),.UNSPECIFIED.,.F.,.F.,.F.,
(4,1,4),(4,4),(-0.000167747802972519,0.571428571428571,1.00016650641139),
(0.,0.17490202709838),.UNSPECIFIED.);
#376=B_SPLINE_SURFACE_WITH_KNOTS('',3,3,((#22677,#22678,#22679,#22680),
(#22681,#22682,#22683,#22684),(#22685,#22686,#22687,#22688),(#22689,#22690,
#22691,#22692),(#22693,#22694,#22695,#22696)),.UNSPECIFIED.,.F.,.F.,.F.,
(4,1,4),(4,4),(0.,0.571428571428571,1.),(0.,0.0459140586584383),
 .UNSPECIFIED.);
#377=B_SPLINE_SURFACE_WITH_KNOTS('',3,3,((#22703,#22704,#22705,#22706),
(#22707,#22708,#22709,#22710),(#22711,#22712,#22713,#22714),(#22715,#22716,
#22717,#22718),(#22719,#22720,#22721,#22722)),.UNSPECIFIED.,.F.,.F.,.F.,
(4,1,4),(4,4),(0.,0.571428571428571,1.),(0.0248279171959177,0.040552544467034),
 .UNSPECIFIED.);
#378=B_SPLINE_SURFACE_WITH_KNOTS('',3,3,((#22726,#22727,#22728,#22729),
(#22730,#22731,#22732,#22733),(#22734,#22735,#22736,#22737),(#22738,#22739,
#22740,#22741)),.UNSPECIFIED.,.F.,.F.,.F.,(4,4),(4,4),(0.287554629624749,
1.),(0.120808499840007,0.462316210796172),.UNSPECIFIED.);
#379=B_SPLINE_SURFACE_WITH_KNOTS('',5,1,((#22746,#22747),(#22748,#22749),
(#22750,#22751),(#22752,#22753),(#22754,#22755),(#22756,#22757),(#22758,
#22759),(#22760,#22761),(#22762,#22763),(#22764,#22765),(#22766,#22767),
(#22768,#22769),(#22770,#22771),(#22772,#22773),(#22774,#22775),(#22776,
#22777),(#22778,#22779),(#22780,#22781),(#22782,#22783),(#22784,#22785),
(#22786,#22787),(#22788,#22789),(#22790,#22791),(#22792,#22793)),
 .UNSPECIFIED.,.F.,.F.,.F.,(6,1,1,1,1,1,1,1,1,1,1,1,1,1,1,1,1,1,1,6),(2,
2),(-0.421786698696643,-0.42,-0.416,-0.412,-0.408,-0.404,-0.4,-0.396,-0.392,
-0.388,-0.384,-0.38,-0.376,-0.372,-0.368,-0.364,-0.36,-0.356,-0.352,-0.351983647406963),
(0.,7.2),.UNSPECIFIED.);
#380=B_SPLINE_SURFACE_WITH_KNOTS('',5,1,((#22799,#22800),(#22801,#22802),
(#22803,#22804),(#22805,#22806),(#22807,#22808),(#22809,#22810),(#22811,
#22812),(#22813,#22814),(#22815,#22816),(#22817,#22818),(#22819,#22820),
(#22821,#22822),(#22823,#22824),(#22825,#22826),(#22827,#22828),(#22829,
#22830),(#22831,#22832),(#22833,#22834),(#22835,#22836),(#22837,#22838),
(#22839,#22840),(#22841,#22842),(#22843,#22844),(#22845,#22846),(#22847,
#22848),(#22849,#22850),(#22851,#22852),(#22853,#22854),(#22855,#22856),
(#22857,#22858),(#22859,#22860),(#22861,#22862),(#22863,#22864),(#22865,
#22866),(#22867,#22868),(#22869,#22870),(#22871,#22872),(#22873,#22874),
(#22875,#22876),(#22877,#22878),(#22879,#22880),(#22881,#22882),(#22883,
#22884),(#22885,#22886),(#22887,#22888),(#22889,#22890),(#22891,#22892),
(#22893,#22894),(#22895,#22896),(#22897,#22898),(#22899,#22900),(#22901,
#22902),(#22903,#22904),(#22905,#22906),(#22907,#22908),(#22909,#22910),
(#22911,#22912),(#22913,#22914),(#22915,#22916),(#22917,#22918),(#22919,
#22920),(#22921,#22922),(#22923,#22924),(#22925,#22926),(#22927,#22928),
(#22929,#22930),(#22931,#22932),(#22933,#22934),(#22935,#22936),(#22937,
#22938),(#22939,#22940),(#22941,#22942),(#22943,#22944),(#22945,#22946),
(#22947,#22948),(#22949,#22950),(#22951,#22952),(#22953,#22954),(#22955,
#22956),(#22957,#22958),(#22959,#22960),(#22961,#22962),(#22963,#22964),
(#22965,#22966),(#22967,#22968),(#22969,#22970),(#22971,#22972),(#22973,
#22974),(#22975,#22976),(#22977,#22978),(#22979,#22980),(#22981,#22982),
(#22983,#22984),(#22985,#22986),(#22987,#22988),(#22989,#22990),(#22991,
#22992),(#22993,#22994),(#22995,#22996),(#22997,#22998),(#22999,#23000),
(#23001,#23002),(#23003,#23004),(#23005,#23006),(#23007,#23008),(#23009,
#23010),(#23011,#23012),(#23013,#23014),(#23015,#23016),(#23017,#23018),
(#23019,#23020),(#23021,#23022),(#23023,#23024),(#23025,#23026),(#23027,
#23028),(#23029,#23030),(#23031,#23032),(#23033,#23034),(#23035,#23036),
(#23037,#23038),(#23039,#23040),(#23041,#23042),(#23043,#23044),(#23045,
#23046),(#23047,#23048),(#23049,#23050),(#23051,#23052),(#23053,#23054),
(#23055,#23056),(#23057,#23058),(#23059,#23060),(#23061,#23062),(#23063,
#23064),(#23065,#23066),(#23067,#23068),(#23069,#23070),(#23071,#23072),
(#23073,#23074),(#23075,#23076),(#23077,#23078),(#23079,#23080),(#23081,
#23082),(#23083,#23084),(#23085,#23086),(#23087,#23088),(#23089,#23090),
(#23091,#23092),(#23093,#23094),(#23095,#23096),(#23097,#23098),(#23099,
#23100),(#23101,#23102),(#23103,#23104),(#23105,#23106),(#23107,#23108),
(#23109,#23110),(#23111,#23112),(#23113,#23114),(#23115,#23116),(#23117,
#23118),(#23119,#23120),(#23121,#23122),(#23123,#23124),(#23125,#23126),
(#23127,#23128),(#23129,#23130),(#23131,#23132),(#23133,#23134),(#23135,
#23136),(#23137,#23138),(#23139,#23140),(#23141,#23142),(#23143,#23144),
(#23145,#23146),(#23147,#23148),(#23149,#23150),(#23151,#23152),(#23153,
#23154),(#23155,#23156),(#23157,#23158),(#23159,#23160),(#23161,#23162),
(#23163,#23164),(#23165,#23166),(#23167,#23168),(#23169,#23170),(#23171,
#23172),(#23173,#23174),(#23175,#23176),(#23177,#23178),(#23179,#23180),
(#23181,#23182),(#23183,#23184),(#23185,#23186),(#23187,#23188),(#23189,
#23190),(#23191,#23192),(#23193,#23194),(#23195,#23196),(#23197,#23198),
(#23199,#23200),(#23201,#23202),(#23203,#23204),(#23205,#23206),(#23207,
#23208),(#23209,#23210),(#23211,#23212),(#23213,#23214),(#23215,#23216),
(#23217,#23218),(#23219,#23220),(#23221,#23222),(#23223,#23224),(#23225,
#23226),(#23227,#23228),(#23229,#23230),(#23231,#23232),(#23233,#23234),
(#23235,#23236),(#23237,#23238),(#23239,#23240),(#23241,#23242),(#23243,
#23244),(#23245,#23246),(#23247,#23248),(#23249,#23250),(#23251,#23252),
(#23253,#23254),(#23255,#23256),(#23257,#23258),(#23259,#23260),(#23261,
#23262),(#23263,#23264),(#23265,#23266),(#23267,#23268),(#23269,#23270),
(#23271,#23272),(#23273,#23274),(#23275,#23276),(#23277,#23278),(#23279,
#23280),(#23281,#23282),(#23283,#23284),(#23285,#23286),(#23287,#23288),
(#23289,#23290),(#23291,#23292),(#23293,#23294),(#23295,#23296),(#23297,
#23298),(#23299,#23300),(#23301,#23302),(#23303,#23304),(#23305,#23306),
(#23307,#23308),(#23309,#23310),(#23311,#23312),(#23313,#23314),(#23315,
#23316),(#23317,#23318)),.UNSPECIFIED.,.T.,.F.,.F.,(6,1,1,1,1,1,1,1,1,1,
1,1,1,1,1,1,1,1,1,1,1,1,1,1,1,1,1,1,1,1,1,1,1,1,1,1,1,1,1,1,1,1,1,1,1,1,
1,1,1,1,1,1,1,1,1,1,1,1,1,1,1,1,1,1,1,1,1,1,1,1,1,1,1,1,1,1,1,1,1,1,1,1,
1,1,1,1,1,1,1,1,1,1,1,1,1,1,1,1,1,1,1,1,1,1,1,1,1,1,1,1,1,1,1,1,1,1,1,1,
1,1,1,1,1,1,1,1,1,1,1,1,1,1,1,1,1,1,1,1,1,1,1,1,1,1,1,1,1,1,1,1,1,1,1,1,
1,1,1,1,1,1,1,1,1,1,1,1,1,1,1,1,1,1,1,1,1,1,1,1,1,1,1,1,1,1,1,1,1,1,1,1,
1,1,1,1,1,1,1,1,1,1,1,1,1,1,1,1,1,1,1,1,1,1,1,1,1,1,1,1,1,1,1,1,1,1,1,1,
1,1,1,1,1,1,1,1,1,5,1,1,1,1,1,1,1,1,1,1,1,1,1,1,1,6),(2,2),(-0.939015270874982,
-0.936000000000001,-0.932000000000001,-0.928000000000001,-0.924000000000001,
-0.920000000000001,-0.916000000000001,-0.912000000000001,-0.908000000000001,
-0.904000000000001,-0.900000000000001,-0.896000000000001,-0.892000000000001,
-0.888000000000001,-0.884000000000001,-0.880000000000001,-0.876000000000001,
-0.872000000000001,-0.868000000000001,-0.864000000000001,-0.860000000000001,
-0.856000000000001,-0.852000000000001,-0.848000000000001,-0.844000000000001,
-0.840000000000001,-0.836000000000001,-0.832000000000001,-0.828000000000001,
-0.824000000000001,-0.820000000000001,-0.816000000000001,-0.812000000000001,
-0.808000000000001,-0.804000000000001,-0.800000000000001,-0.796000000000001,
-0.792000000000001,-0.788000000000001,-0.784000000000001,-0.780000000000001,
-0.776000000000001,-0.772000000000001,-0.768000000000001,-0.764000000000001,
-0.760000000000001,-0.756000000000001,-0.752000000000001,-0.748000000000001,
-0.744000000000001,-0.740000000000001,-0.736000000000001,-0.732000000000001,
-0.728000000000001,-0.724000000000001,-0.720000000000001,-0.716000000000001,
-0.712000000000001,-0.708000000000001,-0.704000000000001,-0.700000000000001,
-0.696000000000001,-0.692000000000001,-0.688000000000001,-0.684,-0.68,-0.676,
-0.672,-0.668,-0.664,-0.66,-0.656,-0.652,-0.648,-0.644,-0.64,-0.636,-0.632,
-0.628,-0.624,-0.62,-0.616,-0.612,-0.608,-0.604,-0.6,-0.596,-0.592,-0.588,
-0.584,-0.58,-0.576,-0.572,-0.568,-0.564,-0.56,-0.556,-0.552,-0.548,-0.544,
-0.54,-0.536,-0.532,-0.528,-0.524,-0.52,-0.516,-0.512,-0.508,-0.504,-0.5,
-0.496,-0.492,-0.488,-0.484,-0.48,-0.476,-0.472,-0.468,-0.464,-0.46,-0.456,
-0.452,-0.448,-0.444,-0.44,-0.436,-0.432,-0.428,-0.424,-0.42,-0.416,-0.412,
-0.408,-0.404,-0.4,-0.396,-0.392,-0.388,-0.384,-0.38,-0.376,-0.372,-0.368,
-0.364,-0.36,-0.356,-0.352,-0.348,-0.344,-0.34,-0.336,-0.332,-0.328,-0.324,
-0.32,-0.316,-0.312,-0.308,-0.304,-0.3,-0.296,-0.292,-0.288,-0.284,-0.28,
-0.276,-0.272,-0.268,-0.264,-0.26,-0.256,-0.252,-0.248,-0.244,-0.24,-0.236,
-0.232,-0.228,-0.224,-0.22,-0.216,-0.212,-0.208,-0.204,-0.2,-0.196,-0.192,
-0.188,-0.184,-0.18,-0.176,-0.172,-0.168,-0.164,-0.16,-0.156,-0.152,-0.148,
-0.144,-0.14,-0.136,-0.132,-0.128,-0.124,-0.12,-0.116,-0.112,-0.108,-0.104,
-0.1,-0.0960000000000001,-0.0920000000000001,-0.0880000000000001,-0.084,
-0.08,-0.076,-0.072,-0.068,-0.064,-0.06,-0.056,-0.052,-0.048,-0.044,-0.04,
-0.036,-0.032,-0.028,-0.024,-0.02,-0.016,-0.012,-0.008,-0.004,0.,0.00399999999999923,
0.00799999999999923,0.0119999999999992,0.0159999999999992,0.0199999999999992,
0.0239999999999992,0.0279999999999992,0.0319999999999993,0.0359999999999993,
0.0399999999999993,0.0439999999999993,0.0479999999999993,0.0519999999999993,
0.0559999999999993,0.0599999999999993,0.0609847291250184),(0.,2.16728151094469),
 .UNSPECIFIED.);
#381=B_SPLINE_SURFACE_WITH_KNOTS('',3,3,((#71919,#71920,#71921,#71922,#71923,
#71924,#71925,#71926,#71927,#71928,#71929,#71930,#71931,#71932,#71933,#71934,
#71935,#71936,#71937,#71938,#71939,#71940,#71941,#71942,#71943,#71944,#71945,
#71946,#71947,#71948,#71949,#71950,#71951,#71952,#71953,#71954,#71955,#71956,
#71957,#71958,#71959,#71960,#71961,#71962,#71963,#71964,#71965,#71966,#71967,
#71968,#71969,#71970,#71971,#71972,#71973,#71974,#71975,#71976,#71977,#71978,
#71979,#71980,#71981,#71982,#71983,#71984,#71985,#71986,#71987,#71988,#71989,
#71990,#71991,#71992,#71993,#71994,#71995,#71996,#71997,#71998,#71999,#72000,
#72001,#72002,#72003,#72004,#72005,#72006,#72007,#72008,#72009,#72010,#72011,
#72012,#72013,#72014,#72015,#72016,#72017,#72018,#72019,#72020,#72021,#72022,
#72023,#72024,#72025,#72026,#72027,#72028,#72029,#72030,#72031,#72032,#72033,
#72034,#72035,#72036,#72037,#72038,#72039,#72040,#72041,#72042,#72043,#72044,
#72045,#72046,#72047,#72048,#72049,#72050,#72051,#72052,#72053,#72054,#72055,
#72056,#72057,#72058,#72059,#72060,#72061,#72062,#72063,#72064,#72065,#72066,
#72067,#72068,#72069,#72070,#72071,#72072,#72073,#72074,#72075,#72076,#72077,
#72078,#72079,#72080,#72081,#72082,#72083,#72084,#72085,#72086,#72087,#72088,
#72089,#72090,#72091,#72092,#72093,#72094,#72095,#72096,#72097,#72098,#72099,
#72100,#72101,#72102,#72103,#72104,#72105,#72106,#72107,#72108,#72109,#72110,
#72111,#72112,#72113,#72114,#72115,#72116,#72117,#72118,#72119,#72120,#72121,
#72122,#72123,#72124,#72125,#72126,#72127,#72128,#72129,#72130,#72131,#72132,
#72133,#72134,#72135,#72136,#72137,#72138,#72139,#72140,#72141,#72142,#72143,
#72144,#72145,#72146,#72147,#72148,#72149,#72150,#72151,#72152,#72153,#72154,
#72155,#72156,#72157,#72158,#72159,#72160,#72161,#72162,#72163,#72164,#72165,
#72166,#72167,#72168,#72169,#72170,#72171,#72172,#72173,#72174,#72175,#72176,
#72177,#72178,#72179,#72180,#72181,#72182,#72183,#72184,#72185,#72186,#72187,
#72188,#72189,#72190,#72191,#72192,#72193,#72194,#72195,#72196,#72197,#72198,
#72199,#72200,#72201,#72202,#72203,#72204,#72205,#72206,#72207,#72208,#72209,
#72210,#72211,#72212,#72213,#72214,#72215,#72216,#72217,#72218,#72219,#72220,
#72221,#72222,#72223,#72224,#72225,#72226,#72227,#72228,#72229,#72230,#72231,
#72232,#72233,#72234,#72235,#72236,#72237,#72238,#72239,#72240,#72241,#72242,
#72243,#72244,#72245,#72246,#72247,#72248,#72249,#72250,#72251,#72252,#72253,
#72254,#72255,#72256,#72257,#72258,#72259,#72260,#72261,#72262,#72263,#72264,
#72265,#72266,#72267,#72268,#72269,#72270,#72271,#72272,#72273,#72274,#72275,
#72276,#72277,#72278,#72279,#72280,#72281,#72282,#72283,#72284,#72285,#72286,
#72287,#72288,#72289,#72290,#72291,#72292,#72293,#72294,#72295,#72296,#72297,
#72298,#72299,#72300,#72301,#72302,#72303,#72304,#72305,#72306,#72307,#72308,
#72309,#72310,#72311,#72312,#72313,#72314,#72315,#72316,#72317,#72318,#72319,
#72320,#72321,#72322,#72323,#72324,#72325,#72326,#72327,#72328,#72329,#72330,
#72331,#72332,#72333,#72334,#72335,#72336,#72337,#72338,#72339,#72340,#72341,
#72342,#72343,#72344,#72345,#72346,#72347,#72348,#72349,#72350,#72351,#72352,
#72353,#72354,#72355,#72356,#72357,#72358,#72359,#72360,#72361,#72362,#72363,
#72364,#72365,#72366,#72367,#72368,#72369,#72370,#72371,#72372,#72373,#72374,
#72375,#72376),(#72377,#72378,#72379,#72380,#72381,#72382,#72383,#72384,
#72385,#72386,#72387,#72388,#72389,#72390,#72391,#72392,#72393,#72394,#72395,
#72396,#72397,#72398,#72399,#72400,#72401,#72402,#72403,#72404,#72405,#72406,
#72407,#72408,#72409,#72410,#72411,#72412,#72413,#72414,#72415,#72416,#72417,
#72418,#72419,#72420,#72421,#72422,#72423,#72424,#72425,#72426,#72427,#72428,
#72429,#72430,#72431,#72432,#72433,#72434,#72435,#72436,#72437,#72438,#72439,
#72440,#72441,#72442,#72443,#72444,#72445,#72446,#72447,#72448,#72449,#72450,
#72451,#72452,#72453,#72454,#72455,#72456,#72457,#72458,#72459,#72460,#72461,
#72462,#72463,#72464,#72465,#72466,#72467,#72468,#72469,#72470,#72471,#72472,
#72473,#72474,#72475,#72476,#72477,#72478,#72479,#72480,#72481,#72482,#72483,
#72484,#72485,#72486,#72487,#72488,#72489,#72490,#72491,#72492,#72493,#72494,
#72495,#72496,#72497,#72498,#72499,#72500,#72501,#72502,#72503,#72504,#72505,
#72506,#72507,#72508,#72509,#72510,#72511,#72512,#72513,#72514,#72515,#72516,
#72517,#72518,#72519,#72520,#72521,#72522,#72523,#72524,#72525,#72526,#72527,
#72528,#72529,#72530,#72531,#72532,#72533,#72534,#72535,#72536,#72537,#72538,
#72539,#72540,#72541,#72542,#72543,#72544,#72545,#72546,#72547,#72548,#72549,
#72550,#72551,#72552,#72553,#72554,#72555,#72556,#72557,#72558,#72559,#72560,
#72561,#72562,#72563,#72564,#72565,#72566,#72567,#72568,#72569,#72570,#72571,
#72572,#72573,#72574,#72575,#72576,#72577,#72578,#72579,#72580,#72581,#72582,
#72583,#72584,#72585,#72586,#72587,#72588,#72589,#72590,#72591,#72592,#72593,
#72594,#72595,#72596,#72597,#72598,#72599,#72600,#72601,#72602,#72603,#72604,
#72605,#72606,#72607,#72608,#72609,#72610,#72611,#72612,#72613,#72614,#72615,
#72616,#72617,#72618,#72619,#72620,#72621,#72622,#72623,#72624,#72625,#72626,
#72627,#72628,#72629,#72630,#72631,#72632,#72633,#72634,#72635,#72636,#72637,
#72638,#72639,#72640,#72641,#72642,#72643,#72644,#72645,#72646,#72647,#72648,
#72649,#72650,#72651,#72652,#72653,#72654,#72655,#72656,#72657,#72658,#72659,
#72660,#72661,#72662,#72663,#72664,#72665,#72666,#72667,#72668,#72669,#72670,
#72671,#72672,#72673,#72674,#72675,#72676,#72677,#72678,#72679,#72680,#72681,
#72682,#72683,#72684,#72685,#72686,#72687,#72688,#72689,#72690,#72691,#72692,
#72693,#72694,#72695,#72696,#72697,#72698,#72699,#72700,#72701,#72702,#72703,
#72704,#72705,#72706,#72707,#72708,#72709,#72710,#72711,#72712,#72713,#72714,
#72715,#72716,#72717,#72718,#72719,#72720,#72721,#72722,#72723,#72724,#72725,
#72726,#72727,#72728,#72729,#72730,#72731,#72732,#72733,#72734,#72735,#72736,
#72737,#72738,#72739,#72740,#72741,#72742,#72743,#72744,#72745,#72746,#72747,
#72748,#72749,#72750,#72751,#72752,#72753,#72754,#72755,#72756,#72757,#72758,
#72759,#72760,#72761,#72762,#72763,#72764,#72765,#72766,#72767,#72768,#72769,
#72770,#72771,#72772,#72773,#72774,#72775,#72776,#72777,#72778,#72779,#72780,
#72781,#72782,#72783,#72784,#72785,#72786,#72787,#72788,#72789,#72790,#72791,
#72792,#72793,#72794,#72795,#72796,#72797,#72798,#72799,#72800,#72801,#72802,
#72803,#72804,#72805,#72806,#72807,#72808,#72809,#72810,#72811,#72812,#72813,
#72814,#72815,#72816,#72817,#72818,#72819,#72820,#72821,#72822,#72823,#72824,
#72825,#72826,#72827,#72828,#72829,#72830,#72831,#72832,#72833,#72834),
(#72835,#72836,#72837,#72838,#72839,#72840,#72841,#72842,#72843,#72844,
#72845,#72846,#72847,#72848,#72849,#72850,#72851,#72852,#72853,#72854,#72855,
#72856,#72857,#72858,#72859,#72860,#72861,#72862,#72863,#72864,#72865,#72866,
#72867,#72868,#72869,#72870,#72871,#72872,#72873,#72874,#72875,#72876,#72877,
#72878,#72879,#72880,#72881,#72882,#72883,#72884,#72885,#72886,#72887,#72888,
#72889,#72890,#72891,#72892,#72893,#72894,#72895,#72896,#72897,#72898,#72899,
#72900,#72901,#72902,#72903,#72904,#72905,#72906,#72907,#72908,#72909,#72910,
#72911,#72912,#72913,#72914,#72915,#72916,#72917,#72918,#72919,#72920,#72921,
#72922,#72923,#72924,#72925,#72926,#72927,#72928,#72929,#72930,#72931,#72932,
#72933,#72934,#72935,#72936,#72937,#72938,#72939,#72940,#72941,#72942,#72943,
#72944,#72945,#72946,#72947,#72948,#72949,#72950,#72951,#72952,#72953,#72954,
#72955,#72956,#72957,#72958,#72959,#72960,#72961,#72962,#72963,#72964,#72965,
#72966,#72967,#72968,#72969,#72970,#72971,#72972,#72973,#72974,#72975,#72976,
#72977,#72978,#72979,#72980,#72981,#72982,#72983,#72984,#72985,#72986,#72987,
#72988,#72989,#72990,#72991,#72992,#72993,#72994,#72995,#72996,#72997,#72998,
#72999,#73000,#73001,#73002,#73003,#73004,#73005,#73006,#73007,#73008,#73009,
#73010,#73011,#73012,#73013,#73014,#73015,#73016,#73017,#73018,#73019,#73020,
#73021,#73022,#73023,#73024,#73025,#73026,#73027,#73028,#73029,#73030,#73031,
#73032,#73033,#73034,#73035,#73036,#73037,#73038,#73039,#73040,#73041,#73042,
#73043,#73044,#73045,#73046,#73047,#73048,#73049,#73050,#73051,#73052,#73053,
#73054,#73055,#73056,#73057,#73058,#73059,#73060,#73061,#73062,#73063,#73064,
#73065,#73066,#73067,#73068,#73069,#73070,#73071,#73072,#73073,#73074,#73075,
#73076,#73077,#73078,#73079,#73080,#73081,#73082,#73083,#73084,#73085,#73086,
#73087,#73088,#73089,#73090,#73091,#73092,#73093,#73094,#73095,#73096,#73097,
#73098,#73099,#73100,#73101,#73102,#73103,#73104,#73105,#73106,#73107,#73108,
#73109,#73110,#73111,#73112,#73113,#73114,#73115,#73116,#73117,#73118,#73119,
#73120,#73121,#73122,#73123,#73124,#73125,#73126,#73127,#73128,#73129,#73130,
#73131,#73132,#73133,#73134,#73135,#73136,#73137,#73138,#73139,#73140,#73141,
#73142,#73143,#73144,#73145,#73146,#73147,#73148,#73149,#73150,#73151,#73152,
#73153,#73154,#73155,#73156,#73157,#73158,#73159,#73160,#73161,#73162,#73163,
#73164,#73165,#73166,#73167,#73168,#73169,#73170,#73171,#73172,#73173,#73174,
#73175,#73176,#73177,#73178,#73179,#73180,#73181,#73182,#73183,#73184,#73185,
#73186,#73187,#73188,#73189,#73190,#73191,#73192,#73193,#73194,#73195,#73196,
#73197,#73198,#73199,#73200,#73201,#73202,#73203,#73204,#73205,#73206,#73207,
#73208,#73209,#73210,#73211,#73212,#73213,#73214,#73215,#73216,#73217,#73218,
#73219,#73220,#73221,#73222,#73223,#73224,#73225,#73226,#73227,#73228,#73229,
#73230,#73231,#73232,#73233,#73234,#73235,#73236,#73237,#73238,#73239,#73240,
#73241,#73242,#73243,#73244,#73245,#73246,#73247,#73248,#73249,#73250,#73251,
#73252,#73253,#73254,#73255,#73256,#73257,#73258,#73259,#73260,#73261,#73262,
#73263,#73264,#73265,#73266,#73267,#73268,#73269,#73270,#73271,#73272,#73273,
#73274,#73275,#73276,#73277,#73278,#73279,#73280,#73281,#73282,#73283,#73284,
#73285,#73286,#73287,#73288,#73289,#73290,#73291,#73292),(#73293,#73294,
#73295,#73296,#73297,#73298,#73299,#73300,#73301,#73302,#73303,#73304,#73305,
#73306,#73307,#73308,#73309,#73310,#73311,#73312,#73313,#73314,#73315,#73316,
#73317,#73318,#73319,#73320,#73321,#73322,#73323,#73324,#73325,#73326,#73327,
#73328,#73329,#73330,#73331,#73332,#73333,#73334,#73335,#73336,#73337,#73338,
#73339,#73340,#73341,#73342,#73343,#73344,#73345,#73346,#73347,#73348,#73349,
#73350,#73351,#73352,#73353,#73354,#73355,#73356,#73357,#73358,#73359,#73360,
#73361,#73362,#73363,#73364,#73365,#73366,#73367,#73368,#73369,#73370,#73371,
#73372,#73373,#73374,#73375,#73376,#73377,#73378,#73379,#73380,#73381,#73382,
#73383,#73384,#73385,#73386,#73387,#73388,#73389,#73390,#73391,#73392,#73393,
#73394,#73395,#73396,#73397,#73398,#73399,#73400,#73401,#73402,#73403,#73404,
#73405,#73406,#73407,#73408,#73409,#73410,#73411,#73412,#73413,#73414,#73415,
#73416,#73417,#73418,#73419,#73420,#73421,#73422,#73423,#73424,#73425,#73426,
#73427,#73428,#73429,#73430,#73431,#73432,#73433,#73434,#73435,#73436,#73437,
#73438,#73439,#73440,#73441,#73442,#73443,#73444,#73445,#73446,#73447,#73448,
#73449,#73450,#73451,#73452,#73453,#73454,#73455,#73456,#73457,#73458,#73459,
#73460,#73461,#73462,#73463,#73464,#73465,#73466,#73467,#73468,#73469,#73470,
#73471,#73472,#73473,#73474,#73475,#73476,#73477,#73478,#73479,#73480,#73481,
#73482,#73483,#73484,#73485,#73486,#73487,#73488,#73489,#73490,#73491,#73492,
#73493,#73494,#73495,#73496,#73497,#73498,#73499,#73500,#73501,#73502,#73503,
#73504,#73505,#73506,#73507,#73508,#73509,#73510,#73511,#73512,#73513,#73514,
#73515,#73516,#73517,#73518,#73519,#73520,#73521,#73522,#73523,#73524,#73525,
#73526,#73527,#73528,#73529,#73530,#73531,#73532,#73533,#73534,#73535,#73536,
#73537,#73538,#73539,#73540,#73541,#73542,#73543,#73544,#73545,#73546,#73547,
#73548,#73549,#73550,#73551,#73552,#73553,#73554,#73555,#73556,#73557,#73558,
#73559,#73560,#73561,#73562,#73563,#73564,#73565,#73566,#73567,#73568,#73569,
#73570,#73571,#73572,#73573,#73574,#73575,#73576,#73577,#73578,#73579,#73580,
#73581,#73582,#73583,#73584,#73585,#73586,#73587,#73588,#73589,#73590,#73591,
#73592,#73593,#73594,#73595,#73596,#73597,#73598,#73599,#73600,#73601,#73602,
#73603,#73604,#73605,#73606,#73607,#73608,#73609,#73610,#73611,#73612,#73613,
#73614,#73615,#73616,#73617,#73618,#73619,#73620,#73621,#73622,#73623,#73624,
#73625,#73626,#73627,#73628,#73629,#73630,#73631,#73632,#73633,#73634,#73635,
#73636,#73637,#73638,#73639,#73640,#73641,#73642,#73643,#73644,#73645,#73646,
#73647,#73648,#73649,#73650,#73651,#73652,#73653,#73654,#73655,#73656,#73657,
#73658,#73659,#73660,#73661,#73662,#73663,#73664,#73665,#73666,#73667,#73668,
#73669,#73670,#73671,#73672,#73673,#73674,#73675,#73676,#73677,#73678,#73679,
#73680,#73681,#73682,#73683,#73684,#73685,#73686,#73687,#73688,#73689,#73690,
#73691,#73692,#73693,#73694,#73695,#73696,#73697,#73698,#73699,#73700,#73701,
#73702,#73703,#73704,#73705,#73706,#73707,#73708,#73709,#73710,#73711,#73712,
#73713,#73714,#73715,#73716,#73717,#73718,#73719,#73720,#73721,#73722,#73723,
#73724,#73725,#73726,#73727,#73728,#73729,#73730,#73731,#73732,#73733,#73734,
#73735,#73736,#73737,#73738,#73739,#73740,#73741,#73742,#73743,#73744,#73745,
#73746,#73747,#73748,#73749,#73750)),.UNSPECIFIED.,.F.,.F.,.F.,(4,4),(4,
1,1,1,1,1,1,1,1,1,1,1,1,1,1,1,1,1,1,1,1,1,1,1,1,1,1,1,1,1,1,1,1,1,1,1,1,
1,1,1,1,1,1,1,1,1,1,1,1,1,1,1,1,1,1,1,1,1,1,1,1,1,1,1,1,1,1,1,1,1,1,1,1,
1,1,1,1,1,1,1,1,1,1,1,1,1,1,1,1,1,1,1,1,1,1,1,1,1,1,1,1,1,1,1,1,1,1,1,1,
1,1,1,1,1,1,1,1,1,1,1,1,1,1,1,1,1,1,1,1,1,1,1,1,1,1,1,1,1,1,1,1,1,1,1,1,
1,1,1,1,1,1,1,1,1,1,1,1,1,1,1,1,1,1,1,1,1,1,1,1,1,1,1,1,1,1,1,1,1,1,1,1,
1,1,1,1,1,1,1,1,1,1,1,1,1,1,1,1,1,1,1,1,1,1,1,1,1,1,1,1,1,1,1,1,1,1,1,1,
1,1,1,1,1,1,1,1,1,1,1,1,1,1,1,1,1,1,1,1,1,1,1,1,1,1,1,1,1,1,1,1,1,1,1,1,
1,1,1,1,1,1,1,1,1,1,1,1,1,1,1,1,1,1,1,1,1,1,1,1,1,1,1,1,1,1,1,1,1,1,1,1,
1,1,1,1,1,1,1,1,1,1,1,1,1,1,1,1,1,1,1,1,1,1,1,1,1,1,1,1,1,1,1,1,1,1,1,1,
1,1,1,1,1,1,1,1,1,1,1,1,1,1,1,1,1,1,1,1,1,1,1,1,1,1,1,1,1,1,1,1,1,1,1,1,
1,1,1,1,1,1,1,1,1,1,1,1,1,1,1,1,1,1,1,1,1,1,1,1,1,1,1,1,1,1,1,1,1,1,1,1,
1,1,1,1,1,1,1,1,1,1,1,1,1,1,1,1,1,1,1,1,1,1,1,1,1,1,1,1,1,1,1,1,1,1,1,1,
1,1,1,1,1,1,1,1,1,1,1,1,1,1,1,1,1,1,1,1,1,1,4),(-0.000668976878624835,0.0823370872655779),
(12.7582013990964,13.7569938028644,14.7557862066324,15.7545786104004,16.7533710141684,
17.7521634179365,18.7509558217045,19.7497482254725,20.7485406292405,21.7473330330085,
22.7461254367765,23.7449178405445,24.7437102443125,25.7425026480806,26.7412950518486,
27.7400874556166,28.7388798593846,29.7376722631526,30.7364646669206,31.7352570706886,
32.7340494744567,33.7328418782247,34.7316342819927,35.7304266857607,36.7292190895287,
37.7280114932967,38.7268038970647,39.7255963008328,40.7243887046008,41.7231811083688,
42.7219735121368,43.7207659159048,44.7195583196728,45.7183507234408,46.7171431272089,
47.7159355309769,48.7147279347449,49.7135203385129,50.7123127422809,51.7111051460489,
52.7098975498169,53.708689953585,54.707482357353,55.706274761121,56.705067164889,
57.703859568657,58.702651972425,59.701444376193,60.700236779961,61.6990291837291,
62.6978215874971,63.6966139912651,64.6954063950331,65.6941987988011,66.6929912025691,
67.6917836063371,68.6905760101052,69.6893684138732,70.6881608176412,71.6869532214092,
72.6857456251772,73.6845380289452,74.6833304327132,75.6821228364813,76.6809152402493,
77.6797076440173,78.6785000477853,79.6772924515533,80.6760848553213,81.6748772590893,
82.6736696628573,83.6724620666254,84.6712544703934,85.6700468741614,86.6688392779294,
87.6676316816974,88.6664240854654,89.6652164892334,90.6640088930015,91.6628012967695,
92.6615937005375,93.6603861043055,94.6591785080735,95.6579709118415,96.6567633156095,
97.6555557193776,98.6543481231456,99.6531405269136,100.651932930682,101.65072533445,
102.649517738218,103.648310141986,104.647102545754,105.645894949522,106.64468735329,
107.643479757058,108.642272160826,109.641064564594,110.639856968362,111.63864937213,
112.637441775898,113.636234179666,114.635026583434,115.633818987202,116.63261139097,
117.631403794738,118.630196198506,119.628988602274,120.627781006042,121.62657340981,
122.625365813578,123.624158217346,124.622950621114,125.621743024882,126.62053542865,
127.619327832418,128.618120236186,129.616912639954,130.615705043722,131.61449744749,
132.613289851258,133.612082255026,134.610874658794,135.609667062562,136.60845946633,
137.607251870098,138.606044273866,139.604836677634,140.603629081402,141.60242148517,
142.601213888938,143.600006292706,144.598798696474,145.597591100242,146.59638350401,
147.595175907778,148.593968311546,149.592760715314,150.591553119082,151.59034552285,
152.589137926618,153.587930330386,154.586722734154,155.585515137922,156.58430754169,
157.583099945458,158.581892349226,159.580684752994,160.579477156762,161.57826956053,
162.577061964298,163.575854368066,164.574646771834,165.573439175602,166.572231579371,
167.571023983139,168.569816386907,169.568608790675,170.567401194443,171.566193598211,
172.564986001979,173.563778405747,174.562570809515,175.561363213283,176.560155617051,
177.558948020819,178.557740424587,179.556532828355,180.555325232123,181.554117635891,
182.552910039659,183.551702443427,184.550494847195,185.549287250963,186.548079654731,
187.546872058499,188.545664462267,189.544456866035,190.543249269803,191.542041673571,
192.540834077339,193.539626481107,194.538418884875,195.537211288643,196.536003692411,
197.534796096179,198.533588499947,199.532380903715,200.531173307483,201.529965711251,
202.528758115019,203.527550518787,204.526342922555,205.525135326323,206.523927730091,
207.522720133859,208.521512537627,209.520304941395,210.519097345163,211.517889748931,
212.516682152699,213.515474556467,214.514266960235,215.513059364003,216.511851767771,
217.510644171539,218.509436575307,219.508228979075,220.507021382843,221.505813786611,
222.504606190379,223.503398594147,224.502190997915,225.500983401683,226.499775805451,
227.498568209219,228.497360612987,229.496153016755,230.494945420523,231.493737824291,
232.492530228059,233.491322631827,234.490115035595,235.488907439363,236.487699843131,
237.486492246899,238.485284650667,239.484077054436,240.482869458204,241.481661861972,
242.48045426574,243.479246669508,244.478039073276,245.476831477044,246.475623880812,
247.47441628458,248.473208688348,249.472001092116,250.470793495884,251.469585899652,
252.46837830342,253.467170707188,254.465963110956,255.464755514724,256.463547918492,
257.46234032226,258.461132726028,259.459925129796,260.458717533564,261.457509937332,
262.4563023411,263.455094744868,264.453887148636,265.452679552404,266.451471956172,
267.45026435994,268.449056763708,269.447849167476,270.446641571244,271.445433975012,
272.44422637878,273.443018782548,274.441811186316,275.440603590084,276.439395993852,
277.43818839762,278.436980801388,279.435773205156,280.434565608924,281.433358012692,
282.43215041646,283.430942820228,284.429735223996,285.428527627764,286.427320031532,
287.4261124353,288.424904839068,289.423697242836,290.422489646604,291.421282050372,
292.42007445414,293.418866857908,294.417659261676,295.416451665444,296.415244069212,
297.41403647298,298.412828876748,299.411621280516,300.410413684284,301.409206088052,
302.40799849182,303.406790895588,304.405583299356,305.404375703124,306.403168106892,
307.40196051066,308.400752914428,309.399545318196,310.398337721964,311.397130125733,
312.395922529501,313.394714933269,314.393507337037,315.392299740805,316.391092144573,
317.389884548341,318.388676952109,319.387469355877,320.386261759645,321.385054163413,
322.383846567181,323.382638970949,324.381431374717,325.380223778485,326.379016182253,
327.377808586021,328.376600989789,329.375393393557,330.374185797325,331.372978201093,
332.371770604861,333.370563008629,334.369355412397,335.368147816165,336.366940219933,
337.365732623701,338.364525027469,339.363317431237,340.362109835005,341.360902238773,
342.359694642541,343.358487046309,344.357279450077,345.356071853845,346.354864257613,
347.353656661381,348.352449065149,349.351241468917,350.350033872685,351.348826276453,
352.347618680221,353.346411083989,354.345203487757,355.343995891525,356.342788295293,
357.341580699061,358.340373102829,359.339165506597,360.337957910365,361.336750314133,
362.335542717901,363.334335121669,364.333127525437,365.331919929205,366.330712332973,
367.329504736741,368.328297140509,369.327089544277,370.325881948045,371.324674351813,
372.323466755581,373.322259159349,374.321051563117,375.319843966885,376.318636370653,
377.317428774421,378.316221178189,379.315013581957,380.313805985725,381.312598389493,
382.311390793261,383.31018319703,384.308975600798,385.307768004566,386.306560408334,
387.305352812102,388.30414521587,389.302937619638,390.301730023406,391.300522427174,
392.299314830942,393.29810723471,394.296899638478,395.295692042246,396.294484446014,
397.293276849782,398.29206925355,399.290861657318,400.289654061086,401.288446464854,
402.287238868622,403.28603127239,404.284823676158,405.283616079926,406.282408483694,
407.281200887462,408.27999329123,409.278785694998,410.277578098766,411.276370502534,
412.275162906302,413.27395531007,414.272747713838,415.271540117606,416.270332521374,
417.269124925142,418.26791732891,419.266709732678,420.265502136446,421.264294540214,
422.263086943982,423.26187934775,424.260671751518,425.259464155286,426.258256559054,
427.257048962822,428.25584136659,429.254633770358,430.253426174126,431.252218577894,
432.251010981662,433.24980338543,434.248595789198,435.247388192966,436.246180596734,
437.244973000502,438.24376540427,439.242557808038,440.241350211806,441.240142615574,
442.238935019342,443.23772742311,444.236519826878,445.235312230646,446.234104634414,
447.232897038182,448.23168944195,449.230481845718,450.229274249486,451.228066653254,
452.226859057022,453.22565146079,454.224443864559,455.223236268327,456.222028672094,
457.220821075863,458.219613479631,459.218405883399,460.217198287167,461.215990690935,
462.214783094703,463.213575498471,464.212367902239,465.211160306007,466.209952709775,
467.209414090422),.UNSPECIFIED.);
#382=B_SPLINE_SURFACE_WITH_KNOTS('',3,3,((#73883,#73884,#73885,#73886,#73887,
#73888,#73889,#73890,#73891,#73892,#73893,#73894,#73895,#73896,#73897,#73898,
#73899,#73900,#73901,#73902,#73903,#73904,#73905,#73906,#73907,#73908,#73909,
#73910,#73911,#73912,#73913,#73914,#73915,#73916,#73917,#73918,#73919,#73920,
#73921,#73922,#73923,#73924,#73925,#73926,#73927,#73928,#73929,#73930,#73931,
#73932,#73933,#73934,#73935,#73936,#73937,#73938,#73939,#73940,#73941,#73942,
#73943,#73944,#73945,#73946,#73947,#73948,#73949,#73950,#73951,#73952,#73953,
#73954,#73955,#73956,#73957,#73958,#73959,#73960,#73961,#73962,#73963,#73964,
#73965,#73966,#73967,#73968,#73969,#73970,#73971,#73972,#73973,#73974,#73975,
#73976,#73977,#73978,#73979,#73980,#73981,#73982,#73983,#73984,#73985,#73986,
#73987,#73988,#73989,#73990,#73991,#73992,#73993,#73994,#73995,#73996,#73997,
#73998,#73999,#74000,#74001,#74002,#74003,#74004,#74005,#74006,#74007,#74008,
#74009,#74010,#74011,#74012,#74013,#74014,#74015,#74016,#74017,#74018,#74019,
#74020,#74021,#74022,#74023,#74024,#74025,#74026,#74027,#74028,#74029,#74030,
#74031,#74032,#74033,#74034,#74035,#74036,#74037,#74038,#74039,#74040,#74041,
#74042,#74043,#74044,#74045,#74046,#74047,#74048,#74049,#74050,#74051,#74052,
#74053,#74054,#74055,#74056,#74057,#74058,#74059,#74060,#74061,#74062,#74063,
#74064,#74065,#74066,#74067,#74068,#74069,#74070,#74071,#74072,#74073,#74074,
#74075,#74076,#74077,#74078,#74079,#74080,#74081,#74082,#74083,#74084,#74085,
#74086,#74087,#74088,#74089,#74090,#74091,#74092,#74093,#74094,#74095,#74096,
#74097,#74098,#74099,#74100,#74101,#74102,#74103,#74104,#74105,#74106,#74107,
#74108,#74109,#74110,#74111,#74112,#74113,#74114,#74115,#74116,#74117,#74118,
#74119,#74120,#74121,#74122,#74123,#74124,#74125,#74126,#74127,#74128,#74129,
#74130,#74131,#74132,#74133,#74134,#74135,#74136,#74137,#74138,#74139,#74140,
#74141,#74142,#74143,#74144,#74145,#74146,#74147,#74148,#74149,#74150,#74151,
#74152,#74153,#74154,#74155,#74156,#74157,#74158,#74159,#74160,#74161,#74162,
#74163,#74164,#74165,#74166,#74167,#74168,#74169,#74170,#74171,#74172,#74173,
#74174,#74175,#74176,#74177,#74178,#74179,#74180,#74181,#74182,#74183,#74184,
#74185,#74186,#74187,#74188,#74189,#74190,#74191,#74192,#74193,#74194,#74195,
#74196,#74197,#74198,#74199,#74200,#74201,#74202,#74203,#74204,#74205,#74206,
#74207,#74208,#74209,#74210,#74211,#74212,#74213,#74214,#74215,#74216,#74217,
#74218,#74219,#74220,#74221,#74222,#74223,#74224,#74225,#74226,#74227,#74228,
#74229,#74230,#74231,#74232,#74233,#74234,#74235,#74236,#74237,#74238,#74239,
#74240,#74241,#74242,#74243,#74244,#74245,#74246,#74247,#74248,#74249,#74250,
#74251,#74252,#74253,#74254,#74255,#74256,#74257,#74258,#74259,#74260,#74261,
#74262,#74263,#74264,#74265,#74266,#74267,#74268,#74269,#74270,#74271,#74272,
#74273,#74274,#74275,#74276,#74277,#74278,#74279,#74280,#74281,#74282,#74283,
#74284,#74285,#74286,#74287,#74288,#74289,#74290,#74291,#74292,#74293,#74294,
#74295,#74296,#74297,#74298,#74299,#74300,#74301,#74302,#74303,#74304,#74305,
#74306,#74307,#74308,#74309,#74310,#74311,#74312,#74313,#74314,#74315,#74316,
#74317,#74318,#74319,#74320,#74321,#74322,#74323,#74324,#74325,#74326,#74327,
#74328,#74329,#74330,#74331,#74332,#74333,#74334,#74335,#74336,#74337,#74338,
#74339,#74340),(#74341,#74342,#74343,#74344,#74345,#74346,#74347,#74348,
#74349,#74350,#74351,#74352,#74353,#74354,#74355,#74356,#74357,#74358,#74359,
#74360,#74361,#74362,#74363,#74364,#74365,#74366,#74367,#74368,#74369,#74370,
#74371,#74372,#74373,#74374,#74375,#74376,#74377,#74378,#74379,#74380,#74381,
#74382,#74383,#74384,#74385,#74386,#74387,#74388,#74389,#74390,#74391,#74392,
#74393,#74394,#74395,#74396,#74397,#74398,#74399,#74400,#74401,#74402,#74403,
#74404,#74405,#74406,#74407,#74408,#74409,#74410,#74411,#74412,#74413,#74414,
#74415,#74416,#74417,#74418,#74419,#74420,#74421,#74422,#74423,#74424,#74425,
#74426,#74427,#74428,#74429,#74430,#74431,#74432,#74433,#74434,#74435,#74436,
#74437,#74438,#74439,#74440,#74441,#74442,#74443,#74444,#74445,#74446,#74447,
#74448,#74449,#74450,#74451,#74452,#74453,#74454,#74455,#74456,#74457,#74458,
#74459,#74460,#74461,#74462,#74463,#74464,#74465,#74466,#74467,#74468,#74469,
#74470,#74471,#74472,#74473,#74474,#74475,#74476,#74477,#74478,#74479,#74480,
#74481,#74482,#74483,#74484,#74485,#74486,#74487,#74488,#74489,#74490,#74491,
#74492,#74493,#74494,#74495,#74496,#74497,#74498,#74499,#74500,#74501,#74502,
#74503,#74504,#74505,#74506,#74507,#74508,#74509,#74510,#74511,#74512,#74513,
#74514,#74515,#74516,#74517,#74518,#74519,#74520,#74521,#74522,#74523,#74524,
#74525,#74526,#74527,#74528,#74529,#74530,#74531,#74532,#74533,#74534,#74535,
#74536,#74537,#74538,#74539,#74540,#74541,#74542,#74543,#74544,#74545,#74546,
#74547,#74548,#74549,#74550,#74551,#74552,#74553,#74554,#74555,#74556,#74557,
#74558,#74559,#74560,#74561,#74562,#74563,#74564,#74565,#74566,#74567,#74568,
#74569,#74570,#74571,#74572,#74573,#74574,#74575,#74576,#74577,#74578,#74579,
#74580,#74581,#74582,#74583,#74584,#74585,#74586,#74587,#74588,#74589,#74590,
#74591,#74592,#74593,#74594,#74595,#74596,#74597,#74598,#74599,#74600,#74601,
#74602,#74603,#74604,#74605,#74606,#74607,#74608,#74609,#74610,#74611,#74612,
#74613,#74614,#74615,#74616,#74617,#74618,#74619,#74620,#74621,#74622,#74623,
#74624,#74625,#74626,#74627,#74628,#74629,#74630,#74631,#74632,#74633,#74634,
#74635,#74636,#74637,#74638,#74639,#74640,#74641,#74642,#74643,#74644,#74645,
#74646,#74647,#74648,#74649,#74650,#74651,#74652,#74653,#74654,#74655,#74656,
#74657,#74658,#74659,#74660,#74661,#74662,#74663,#74664,#74665,#74666,#74667,
#74668,#74669,#74670,#74671,#74672,#74673,#74674,#74675,#74676,#74677,#74678,
#74679,#74680,#74681,#74682,#74683,#74684,#74685,#74686,#74687,#74688,#74689,
#74690,#74691,#74692,#74693,#74694,#74695,#74696,#74697,#74698,#74699,#74700,
#74701,#74702,#74703,#74704,#74705,#74706,#74707,#74708,#74709,#74710,#74711,
#74712,#74713,#74714,#74715,#74716,#74717,#74718,#74719,#74720,#74721,#74722,
#74723,#74724,#74725,#74726,#74727,#74728,#74729,#74730,#74731,#74732,#74733,
#74734,#74735,#74736,#74737,#74738,#74739,#74740,#74741,#74742,#74743,#74744,
#74745,#74746,#74747,#74748,#74749,#74750,#74751,#74752,#74753,#74754,#74755,
#74756,#74757,#74758,#74759,#74760,#74761,#74762,#74763,#74764,#74765,#74766,
#74767,#74768,#74769,#74770,#74771,#74772,#74773,#74774,#74775,#74776,#74777,
#74778,#74779,#74780,#74781,#74782,#74783,#74784,#74785,#74786,#74787,#74788,
#74789,#74790,#74791,#74792,#74793,#74794,#74795,#74796,#74797,#74798),
(#74799,#74800,#74801,#74802,#74803,#74804,#74805,#74806,#74807,#74808,
#74809,#74810,#74811,#74812,#74813,#74814,#74815,#74816,#74817,#74818,#74819,
#74820,#74821,#74822,#74823,#74824,#74825,#74826,#74827,#74828,#74829,#74830,
#74831,#74832,#74833,#74834,#74835,#74836,#74837,#74838,#74839,#74840,#74841,
#74842,#74843,#74844,#74845,#74846,#74847,#74848,#74849,#74850,#74851,#74852,
#74853,#74854,#74855,#74856,#74857,#74858,#74859,#74860,#74861,#74862,#74863,
#74864,#74865,#74866,#74867,#74868,#74869,#74870,#74871,#74872,#74873,#74874,
#74875,#74876,#74877,#74878,#74879,#74880,#74881,#74882,#74883,#74884,#74885,
#74886,#74887,#74888,#74889,#74890,#74891,#74892,#74893,#74894,#74895,#74896,
#74897,#74898,#74899,#74900,#74901,#74902,#74903,#74904,#74905,#74906,#74907,
#74908,#74909,#74910,#74911,#74912,#74913,#74914,#74915,#74916,#74917,#74918,
#74919,#74920,#74921,#74922,#74923,#74924,#74925,#74926,#74927,#74928,#74929,
#74930,#74931,#74932,#74933,#74934,#74935,#74936,#74937,#74938,#74939,#74940,
#74941,#74942,#74943,#74944,#74945,#74946,#74947,#74948,#74949,#74950,#74951,
#74952,#74953,#74954,#74955,#74956,#74957,#74958,#74959,#74960,#74961,#74962,
#74963,#74964,#74965,#74966,#74967,#74968,#74969,#74970,#74971,#74972,#74973,
#74974,#74975,#74976,#74977,#74978,#74979,#74980,#74981,#74982,#74983,#74984,
#74985,#74986,#74987,#74988,#74989,#74990,#74991,#74992,#74993,#74994,#74995,
#74996,#74997,#74998,#74999,#75000,#75001,#75002,#75003,#75004,#75005,#75006,
#75007,#75008,#75009,#75010,#75011,#75012,#75013,#75014,#75015,#75016,#75017,
#75018,#75019,#75020,#75021,#75022,#75023,#75024,#75025,#75026,#75027,#75028,
#75029,#75030,#75031,#75032,#75033,#75034,#75035,#75036,#75037,#75038,#75039,
#75040,#75041,#75042,#75043,#75044,#75045,#75046,#75047,#75048,#75049,#75050,
#75051,#75052,#75053,#75054,#75055,#75056,#75057,#75058,#75059,#75060,#75061,
#75062,#75063,#75064,#75065,#75066,#75067,#75068,#75069,#75070,#75071,#75072,
#75073,#75074,#75075,#75076,#75077,#75078,#75079,#75080,#75081,#75082,#75083,
#75084,#75085,#75086,#75087,#75088,#75089,#75090,#75091,#75092,#75093,#75094,
#75095,#75096,#75097,#75098,#75099,#75100,#75101,#75102,#75103,#75104,#75105,
#75106,#75107,#75108,#75109,#75110,#75111,#75112,#75113,#75114,#75115,#75116,
#75117,#75118,#75119,#75120,#75121,#75122,#75123,#75124,#75125,#75126,#75127,
#75128,#75129,#75130,#75131,#75132,#75133,#75134,#75135,#75136,#75137,#75138,
#75139,#75140,#75141,#75142,#75143,#75144,#75145,#75146,#75147,#75148,#75149,
#75150,#75151,#75152,#75153,#75154,#75155,#75156,#75157,#75158,#75159,#75160,
#75161,#75162,#75163,#75164,#75165,#75166,#75167,#75168,#75169,#75170,#75171,
#75172,#75173,#75174,#75175,#75176,#75177,#75178,#75179,#75180,#75181,#75182,
#75183,#75184,#75185,#75186,#75187,#75188,#75189,#75190,#75191,#75192,#75193,
#75194,#75195,#75196,#75197,#75198,#75199,#75200,#75201,#75202,#75203,#75204,
#75205,#75206,#75207,#75208,#75209,#75210,#75211,#75212,#75213,#75214,#75215,
#75216,#75217,#75218,#75219,#75220,#75221,#75222,#75223,#75224,#75225,#75226,
#75227,#75228,#75229,#75230,#75231,#75232,#75233,#75234,#75235,#75236,#75237,
#75238,#75239,#75240,#75241,#75242,#75243,#75244,#75245,#75246,#75247,#75248,
#75249,#75250,#75251,#75252,#75253,#75254,#75255,#75256),(#75257,#75258,
#75259,#75260,#75261,#75262,#75263,#75264,#75265,#75266,#75267,#75268,#75269,
#75270,#75271,#75272,#75273,#75274,#75275,#75276,#75277,#75278,#75279,#75280,
#75281,#75282,#75283,#75284,#75285,#75286,#75287,#75288,#75289,#75290,#75291,
#75292,#75293,#75294,#75295,#75296,#75297,#75298,#75299,#75300,#75301,#75302,
#75303,#75304,#75305,#75306,#75307,#75308,#75309,#75310,#75311,#75312,#75313,
#75314,#75315,#75316,#75317,#75318,#75319,#75320,#75321,#75322,#75323,#75324,
#75325,#75326,#75327,#75328,#75329,#75330,#75331,#75332,#75333,#75334,#75335,
#75336,#75337,#75338,#75339,#75340,#75341,#75342,#75343,#75344,#75345,#75346,
#75347,#75348,#75349,#75350,#75351,#75352,#75353,#75354,#75355,#75356,#75357,
#75358,#75359,#75360,#75361,#75362,#75363,#75364,#75365,#75366,#75367,#75368,
#75369,#75370,#75371,#75372,#75373,#75374,#75375,#75376,#75377,#75378,#75379,
#75380,#75381,#75382,#75383,#75384,#75385,#75386,#75387,#75388,#75389,#75390,
#75391,#75392,#75393,#75394,#75395,#75396,#75397,#75398,#75399,#75400,#75401,
#75402,#75403,#75404,#75405,#75406,#75407,#75408,#75409,#75410,#75411,#75412,
#75413,#75414,#75415,#75416,#75417,#75418,#75419,#75420,#75421,#75422,#75423,
#75424,#75425,#75426,#75427,#75428,#75429,#75430,#75431,#75432,#75433,#75434,
#75435,#75436,#75437,#75438,#75439,#75440,#75441,#75442,#75443,#75444,#75445,
#75446,#75447,#75448,#75449,#75450,#75451,#75452,#75453,#75454,#75455,#75456,
#75457,#75458,#75459,#75460,#75461,#75462,#75463,#75464,#75465,#75466,#75467,
#75468,#75469,#75470,#75471,#75472,#75473,#75474,#75475,#75476,#75477,#75478,
#75479,#75480,#75481,#75482,#75483,#75484,#75485,#75486,#75487,#75488,#75489,
#75490,#75491,#75492,#75493,#75494,#75495,#75496,#75497,#75498,#75499,#75500,
#75501,#75502,#75503,#75504,#75505,#75506,#75507,#75508,#75509,#75510,#75511,
#75512,#75513,#75514,#75515,#75516,#75517,#75518,#75519,#75520,#75521,#75522,
#75523,#75524,#75525,#75526,#75527,#75528,#75529,#75530,#75531,#75532,#75533,
#75534,#75535,#75536,#75537,#75538,#75539,#75540,#75541,#75542,#75543,#75544,
#75545,#75546,#75547,#75548,#75549,#75550,#75551,#75552,#75553,#75554,#75555,
#75556,#75557,#75558,#75559,#75560,#75561,#75562,#75563,#75564,#75565,#75566,
#75567,#75568,#75569,#75570,#75571,#75572,#75573,#75574,#75575,#75576,#75577,
#75578,#75579,#75580,#75581,#75582,#75583,#75584,#75585,#75586,#75587,#75588,
#75589,#75590,#75591,#75592,#75593,#75594,#75595,#75596,#75597,#75598,#75599,
#75600,#75601,#75602,#75603,#75604,#75605,#75606,#75607,#75608,#75609,#75610,
#75611,#75612,#75613,#75614,#75615,#75616,#75617,#75618,#75619,#75620,#75621,
#75622,#75623,#75624,#75625,#75626,#75627,#75628,#75629,#75630,#75631,#75632,
#75633,#75634,#75635,#75636,#75637,#75638,#75639,#75640,#75641,#75642,#75643,
#75644,#75645,#75646,#75647,#75648,#75649,#75650,#75651,#75652,#75653,#75654,
#75655,#75656,#75657,#75658,#75659,#75660,#75661,#75662,#75663,#75664,#75665,
#75666,#75667,#75668,#75669,#75670,#75671,#75672,#75673,#75674,#75675,#75676,
#75677,#75678,#75679,#75680,#75681,#75682,#75683,#75684,#75685,#75686,#75687,
#75688,#75689,#75690,#75691,#75692,#75693,#75694,#75695,#75696,#75697,#75698,
#75699,#75700,#75701,#75702,#75703,#75704,#75705,#75706,#75707,#75708,#75709,
#75710,#75711,#75712,#75713,#75714)),.UNSPECIFIED.,.F.,.F.,.F.,(4,4),(4,
1,1,1,1,1,1,1,1,1,1,1,1,1,1,1,1,1,1,1,1,1,1,1,1,1,1,1,1,1,1,1,1,1,1,1,1,
1,1,1,1,1,1,1,1,1,1,1,1,1,1,1,1,1,1,1,1,1,1,1,1,1,1,1,1,1,1,1,1,1,1,1,1,
1,1,1,1,1,1,1,1,1,1,1,1,1,1,1,1,1,1,1,1,1,1,1,1,1,1,1,1,1,1,1,1,1,1,1,1,
1,1,1,1,1,1,1,1,1,1,1,1,1,1,1,1,1,1,1,1,1,1,1,1,1,1,1,1,1,1,1,1,1,1,1,1,
1,1,1,1,1,1,1,1,1,1,1,1,1,1,1,1,1,1,1,1,1,1,1,1,1,1,1,1,1,1,1,1,1,1,1,1,
1,1,1,1,1,1,1,1,1,1,1,1,1,1,1,1,1,1,1,1,1,1,1,1,1,1,1,1,1,1,1,1,1,1,1,1,
1,1,1,1,1,1,1,1,1,1,1,1,1,1,1,1,1,1,1,1,1,1,1,1,1,1,1,1,1,1,1,1,1,1,1,1,
1,1,1,1,1,1,1,1,1,1,1,1,1,1,1,1,1,1,1,1,1,1,1,1,1,1,1,1,1,1,1,1,1,1,1,1,
1,1,1,1,1,1,1,1,1,1,1,1,1,1,1,1,1,1,1,1,1,1,1,1,1,1,1,1,1,1,1,1,1,1,1,1,
1,1,1,1,1,1,1,1,1,1,1,1,1,1,1,1,1,1,1,1,1,1,1,1,1,1,1,1,1,1,1,1,1,1,1,1,
1,1,1,1,1,1,1,1,1,1,1,1,1,1,1,1,1,1,1,1,1,1,1,1,1,1,1,1,1,1,1,1,1,1,1,1,
1,1,1,1,1,1,1,1,1,1,1,1,1,1,1,1,1,1,1,1,1,1,1,1,1,1,1,1,1,1,1,1,1,1,1,1,
1,1,1,1,1,1,1,1,1,1,1,1,1,1,1,1,1,1,1,1,1,1,4),(-0.000353810282139617,0.0826815503419868),
(16.0580139323897,17.0574752807613,18.0562676845293,19.0550600882973,20.0538524920653,
21.0526448958333,22.0514372996014,23.0502297033694,24.0490221071374,25.0478145109054,
26.0466069146734,27.0453993184414,28.0441917222094,29.0429841259775,30.0417765297455,
31.0405689335135,32.0393613372815,33.0381537410495,34.0369461448175,35.0357385485855,
36.0345309523535,37.0333233561216,38.0321157598896,39.0309081636576,40.0297005674256,
41.0284929711936,42.0272853749616,43.0260777787296,44.0248701824977,45.0236625862657,
46.0224549900337,47.0212473938017,48.0200397975697,49.0188322013377,50.0176246051057,
51.0164170088737,52.0152094126418,53.0140018164098,54.0127942201778,55.0115866239458,
56.0103790277138,57.0091714314818,58.0079638352498,59.0067562390179,60.0055486427859,
61.0043410465539,62.0031334503219,63.0019258540899,64.0007182578579,64.9995106616259,
65.9983030653939,66.997095469162,67.99588787293,68.994680276698,69.993472680466,
70.992265084234,71.991057488002,72.98984989177,73.9886422955381,74.9874346993061,
75.9862271030741,76.9850195068421,77.9838119106101,78.9826043143781,79.9813967181461,
80.9801891219142,81.9789815256821,82.9777739294502,83.9765663332182,84.9753587369862,
85.9741511407542,86.9729435445222,87.9717359482902,88.9705283520582,89.9693207558263,
90.9681131595943,91.9669055633623,92.9656979671303,93.9644903708983,94.9632827746663,
95.9620751784343,96.9608675822024,97.9596599859704,98.9584523897384,99.9572447935064,
100.956037197274,101.954829601042,102.95362200481,103.952414408578,104.951206812346,
105.949999216114,106.948791619882,107.947584023651,108.946376427419,109.945168831187,
110.943961234955,111.942753638723,112.941546042491,113.940338446259,114.939130850027,
115.937923253795,116.936715657563,117.935508061331,118.934300465099,119.933092868867,
120.931885272635,121.930677676403,122.929470080171,123.928262483939,124.927054887707,
125.925847291475,126.924639695243,127.923432099011,128.922224502779,129.921016906547,
130.919809310315,131.918601714083,132.917394117851,133.916186521619,134.914978925387,
135.913771329155,136.912563732923,137.911356136691,138.910148540459,139.908940944227,
140.907733347995,141.906525751763,142.905318155531,143.904110559299,144.902902963067,
145.901695366835,146.900487770603,147.899280174371,148.898072578139,149.896864981907,
150.895657385675,151.894449789443,152.893242193211,153.892034596979,154.890827000747,
155.889619404515,156.888411808283,157.887204212051,158.885996615819,159.884789019587,
160.883581423355,161.882373827123,162.881166230891,163.879958634659,164.878751038427,
165.877543442195,166.876335845963,167.875128249731,168.873920653499,169.872713057267,
170.871505461035,171.870297864803,172.869090268571,173.867882672339,174.866675076107,
175.865467479875,176.864259883643,177.863052287411,178.861844691179,179.860637094947,
180.859429498715,181.858221902483,182.857014306252,183.85580671002,184.854599113788,
185.853391517556,186.852183921324,187.850976325092,188.84976872886,189.848561132628,
190.847353536396,191.846145940164,192.844938343932,193.8437307477,194.842523151468,
195.841315555236,196.840107959004,197.838900362772,198.83769276654,199.836485170308,
200.835277574076,201.834069977844,202.832862381612,203.83165478538,204.830447189148,
205.829239592916,206.828031996684,207.826824400452,208.82561680422,209.824409207988,
210.823201611756,211.821994015524,212.820786419292,213.81957882306,214.818371226828,
215.817163630596,216.815956034364,217.814748438132,218.8135408419,219.812333245668,
220.811125649436,221.809918053204,222.808710456972,223.80750286074,224.806295264508,
225.805087668276,226.803880072044,227.802672475812,228.80146487958,229.800257283348,
230.799049687116,231.797842090884,232.796634494652,233.79542689842,234.794219302188,
235.793011705956,236.791804109724,237.790596513492,238.78938891726,239.788181321028,
240.786973724796,241.785766128564,242.784558532332,243.7833509361,244.782143339868,
245.780935743636,246.779728147404,247.778520551172,248.77731295494,249.776105358708,
250.774897762476,251.773690166244,252.772482570012,253.77127497378,254.770067377548,
255.768859781316,256.767652185084,257.766444588852,258.76523699262,259.764029396389,
260.762821800157,261.761614203925,262.760406607693,263.759199011461,264.757991415229,
265.756783818997,266.755576222765,267.754368626533,268.753161030301,269.751953434069,
270.750745837837,271.749538241605,272.748330645373,273.747123049141,274.745915452909,
275.744707856677,276.743500260445,277.742292664213,278.741085067981,279.739877471749,
280.738669875517,281.737462279285,282.736254683053,283.735047086821,284.733839490589,
285.732631894357,286.731424298125,287.730216701893,288.729009105661,289.727801509429,
290.726593913197,291.725386316965,292.724178720733,293.722971124501,294.721763528269,
295.720555932037,296.719348335805,297.718140739573,298.716933143341,299.715725547109,
300.714517950877,301.713310354645,302.712102758413,303.710895162181,304.709687565949,
305.708479969717,306.707272373485,307.706064777253,308.704857181021,309.703649584789,
310.702441988557,311.701234392325,312.700026796093,313.698819199861,314.697611603629,
315.696404007397,316.695196411165,317.693988814933,318.692781218701,319.691573622469,
320.690366026237,321.689158430005,322.687950833773,323.686743237541,324.685535641309,
325.684328045077,326.683120448845,327.681912852613,328.680705256381,329.679497660149,
330.678290063917,331.677082467685,332.675874871453,333.674667275221,334.67345967899,
335.672252082757,336.671044486525,337.669836890294,338.668629294062,339.66742169783,
340.666214101598,341.665006505366,342.663798909134,343.662591312902,344.66138371667,
345.660176120438,346.658968524206,347.657760927974,348.656553331742,349.65534573551,
350.654138139278,351.652930543046,352.651722946814,353.650515350582,354.64930775435,
355.648100158118,356.646892561886,357.645684965654,358.644477369422,359.64326977319,
360.642062176958,361.640854580726,362.639646984494,363.638439388262,364.63723179203,
365.636024195798,366.634816599566,367.633609003334,368.632401407102,369.63119381087,
370.629986214638,371.628778618406,372.627571022174,373.626363425942,374.62515582971,
375.623948233478,376.622740637246,377.621533041014,378.620325444782,379.61911784855,
380.617910252318,381.616702656086,382.615495059854,383.614287463622,384.61307986739,
385.611872271158,386.610664674926,387.609457078694,388.608249482462,389.60704188623,
390.605834289998,391.604626693766,392.603419097534,393.602211501302,394.60100390507,
395.599796308838,396.598588712606,397.597381116374,398.596173520142,399.59496592391,
400.593758327678,401.592550731446,402.591343135214,403.590135538982,404.58892794275,
405.587720346518,406.586512750286,407.585305154054,408.584097557822,409.58288996159,
410.581682365359,411.580474769127,412.579267172895,413.578059576663,414.576851980431,
415.575644384199,416.574436787967,417.573229191735,418.572021595503,419.570813999271,
420.569606403039,421.568398806807,422.567191210575,423.565983614343,424.564776018111,
425.563568421879,426.562360825647,427.561153229415,428.559945633183,429.558738036951,
430.557530440719,431.556322844487,432.555115248255,433.553907652023,434.552700055791,
435.551492459559,436.550284863327,437.549077267095,438.547869670863,439.546662074631,
440.545454478399,441.544246882167,442.543039285935,443.541831689703,444.540624093471,
445.539416497239,446.538208901007,447.537001304775,448.535793708543,449.534586112311,
450.533378516079,451.532170919847,452.530963323615,453.529755727383,454.528548131151,
455.527340534919,456.526132938687,457.524925342455,458.523717746223,459.522510149991,
460.521302553759,461.520094957527,462.518887361295,463.517679765063,464.516472168831,
465.515264572599,466.514056976367,467.512849380135,468.511641783903,469.510434187671,
470.509226591439),.UNSPECIFIED.);
#383=B_SPLINE_SURFACE_WITH_KNOTS('',3,3,((#76038,#76039,#76040,#76041,#76042,
#76043,#76044,#76045,#76046,#76047,#76048,#76049,#76050,#76051,#76052,#76053,
#76054,#76055,#76056,#76057,#76058,#76059,#76060,#76061,#76062,#76063,#76064,
#76065,#76066,#76067,#76068,#76069,#76070,#76071,#76072,#76073,#76074,#76075,
#76076,#76077,#76078,#76079,#76080,#76081,#76082,#76083,#76084,#76085,#76086,
#76087,#76088,#76089,#76090,#76091,#76092,#76093,#76094,#76095,#76096,#76097,
#76098,#76099,#76100,#76101,#76102,#76103,#76104,#76105,#76106,#76107,#76108,
#76109,#76110,#76111,#76112,#76113,#76114,#76115,#76116,#76117,#76118,#76119,
#76120,#76121,#76122,#76123,#76124,#76125,#76126,#76127,#76128,#76129,#76130,
#76131,#76132,#76133,#76134,#76135,#76136,#76137,#76138,#76139,#76140,#76141,
#76142,#76143,#76144,#76145,#76146,#76147),(#76148,#76149,#76150,#76151,
#76152,#76153,#76154,#76155,#76156,#76157,#76158,#76159,#76160,#76161,#76162,
#76163,#76164,#76165,#76166,#76167,#76168,#76169,#76170,#76171,#76172,#76173,
#76174,#76175,#76176,#76177,#76178,#76179,#76180,#76181,#76182,#76183,#76184,
#76185,#76186,#76187,#76188,#76189,#76190,#76191,#76192,#76193,#76194,#76195,
#76196,#76197,#76198,#76199,#76200,#76201,#76202,#76203,#76204,#76205,#76206,
#76207,#76208,#76209,#76210,#76211,#76212,#76213,#76214,#76215,#76216,#76217,
#76218,#76219,#76220,#76221,#76222,#76223,#76224,#76225,#76226,#76227,#76228,
#76229,#76230,#76231,#76232,#76233,#76234,#76235,#76236,#76237,#76238,#76239,
#76240,#76241,#76242,#76243,#76244,#76245,#76246,#76247,#76248,#76249,#76250,
#76251,#76252,#76253,#76254,#76255,#76256,#76257),(#76258,#76259,#76260,
#76261,#76262,#76263,#76264,#76265,#76266,#76267,#76268,#76269,#76270,#76271,
#76272,#76273,#76274,#76275,#76276,#76277,#76278,#76279,#76280,#76281,#76282,
#76283,#76284,#76285,#76286,#76287,#76288,#76289,#76290,#76291,#76292,#76293,
#76294,#76295,#76296,#76297,#76298,#76299,#76300,#76301,#76302,#76303,#76304,
#76305,#76306,#76307,#76308,#76309,#76310,#76311,#76312,#76313,#76314,#76315,
#76316,#76317,#76318,#76319,#76320,#76321,#76322,#76323,#76324,#76325,#76326,
#76327,#76328,#76329,#76330,#76331,#76332,#76333,#76334,#76335,#76336,#76337,
#76338,#76339,#76340,#76341,#76342,#76343,#76344,#76345,#76346,#76347,#76348,
#76349,#76350,#76351,#76352,#76353,#76354,#76355,#76356,#76357,#76358,#76359,
#76360,#76361,#76362,#76363,#76364,#76365,#76366,#76367),(#76368,#76369,
#76370,#76371,#76372,#76373,#76374,#76375,#76376,#76377,#76378,#76379,#76380,
#76381,#76382,#76383,#76384,#76385,#76386,#76387,#76388,#76389,#76390,#76391,
#76392,#76393,#76394,#76395,#76396,#76397,#76398,#76399,#76400,#76401,#76402,
#76403,#76404,#76405,#76406,#76407,#76408,#76409,#76410,#76411,#76412,#76413,
#76414,#76415,#76416,#76417,#76418,#76419,#76420,#76421,#76422,#76423,#76424,
#76425,#76426,#76427,#76428,#76429,#76430,#76431,#76432,#76433,#76434,#76435,
#76436,#76437,#76438,#76439,#76440,#76441,#76442,#76443,#76444,#76445,#76446,
#76447,#76448,#76449,#76450,#76451,#76452,#76453,#76454,#76455,#76456,#76457,
#76458,#76459,#76460,#76461,#76462,#76463,#76464,#76465,#76466,#76467,#76468,
#76469,#76470,#76471,#76472,#76473,#76474,#76475,#76476,#76477),(#76478,
#76479,#76480,#76481,#76482,#76483,#76484,#76485,#76486,#76487,#76488,#76489,
#76490,#76491,#76492,#76493,#76494,#76495,#76496,#76497,#76498,#76499,#76500,
#76501,#76502,#76503,#76504,#76505,#76506,#76507,#76508,#76509,#76510,#76511,
#76512,#76513,#76514,#76515,#76516,#76517,#76518,#76519,#76520,#76521,#76522,
#76523,#76524,#76525,#76526,#76527,#76528,#76529,#76530,#76531,#76532,#76533,
#76534,#76535,#76536,#76537,#76538,#76539,#76540,#76541,#76542,#76543,#76544,
#76545,#76546,#76547,#76548,#76549,#76550,#76551,#76552,#76553,#76554,#76555,
#76556,#76557,#76558,#76559,#76560,#76561,#76562,#76563,#76564,#76565,#76566,
#76567,#76568,#76569,#76570,#76571,#76572,#76573,#76574,#76575,#76576,#76577,
#76578,#76579,#76580,#76581,#76582,#76583,#76584,#76585,#76586,#76587),
(#76588,#76589,#76590,#76591,#76592,#76593,#76594,#76595,#76596,#76597,
#76598,#76599,#76600,#76601,#76602,#76603,#76604,#76605,#76606,#76607,#76608,
#76609,#76610,#76611,#76612,#76613,#76614,#76615,#76616,#76617,#76618,#76619,
#76620,#76621,#76622,#76623,#76624,#76625,#76626,#76627,#76628,#76629,#76630,
#76631,#76632,#76633,#76634,#76635,#76636,#76637,#76638,#76639,#76640,#76641,
#76642,#76643,#76644,#76645,#76646,#76647,#76648,#76649,#76650,#76651,#76652,
#76653,#76654,#76655,#76656,#76657,#76658,#76659,#76660,#76661,#76662,#76663,
#76664,#76665,#76666,#76667,#76668,#76669,#76670,#76671,#76672,#76673,#76674,
#76675,#76676,#76677,#76678,#76679,#76680,#76681,#76682,#76683,#76684,#76685,
#76686,#76687,#76688,#76689,#76690,#76691,#76692,#76693,#76694,#76695,#76696,
#76697),(#76698,#76699,#76700,#76701,#76702,#76703,#76704,#76705,#76706,
#76707,#76708,#76709,#76710,#76711,#76712,#76713,#76714,#76715,#76716,#76717,
#76718,#76719,#76720,#76721,#76722,#76723,#76724,#76725,#76726,#76727,#76728,
#76729,#76730,#76731,#76732,#76733,#76734,#76735,#76736,#76737,#76738,#76739,
#76740,#76741,#76742,#76743,#76744,#76745,#76746,#76747,#76748,#76749,#76750,
#76751,#76752,#76753,#76754,#76755,#76756,#76757,#76758,#76759,#76760,#76761,
#76762,#76763,#76764,#76765,#76766,#76767,#76768,#76769,#76770,#76771,#76772,
#76773,#76774,#76775,#76776,#76777,#76778,#76779,#76780,#76781,#76782,#76783,
#76784,#76785,#76786,#76787,#76788,#76789,#76790,#76791,#76792,#76793,#76794,
#76795,#76796,#76797,#76798,#76799,#76800,#76801,#76802,#76803,#76804,#76805,
#76806,#76807),(#76808,#76809,#76810,#76811,#76812,#76813,#76814,#76815,
#76816,#76817,#76818,#76819,#76820,#76821,#76822,#76823,#76824,#76825,#76826,
#76827,#76828,#76829,#76830,#76831,#76832,#76833,#76834,#76835,#76836,#76837,
#76838,#76839,#76840,#76841,#76842,#76843,#76844,#76845,#76846,#76847,#76848,
#76849,#76850,#76851,#76852,#76853,#76854,#76855,#76856,#76857,#76858,#76859,
#76860,#76861,#76862,#76863,#76864,#76865,#76866,#76867,#76868,#76869,#76870,
#76871,#76872,#76873,#76874,#76875,#76876,#76877,#76878,#76879,#76880,#76881,
#76882,#76883,#76884,#76885,#76886,#76887,#76888,#76889,#76890,#76891,#76892,
#76893,#76894,#76895,#76896,#76897,#76898,#76899,#76900,#76901,#76902,#76903,
#76904,#76905,#76906,#76907,#76908,#76909,#76910,#76911,#76912,#76913,#76914,
#76915,#76916,#76917),(#76918,#76919,#76920,#76921,#76922,#76923,#76924,
#76925,#76926,#76927,#76928,#76929,#76930,#76931,#76932,#76933,#76934,#76935,
#76936,#76937,#76938,#76939,#76940,#76941,#76942,#76943,#76944,#76945,#76946,
#76947,#76948,#76949,#76950,#76951,#76952,#76953,#76954,#76955,#76956,#76957,
#76958,#76959,#76960,#76961,#76962,#76963,#76964,#76965,#76966,#76967,#76968,
#76969,#76970,#76971,#76972,#76973,#76974,#76975,#76976,#76977,#76978,#76979,
#76980,#76981,#76982,#76983,#76984,#76985,#76986,#76987,#76988,#76989,#76990,
#76991,#76992,#76993,#76994,#76995,#76996,#76997,#76998,#76999,#77000,#77001,
#77002,#77003,#77004,#77005,#77006,#77007,#77008,#77009,#77010,#77011,#77012,
#77013,#77014,#77015,#77016,#77017,#77018,#77019,#77020,#77021,#77022,#77023,
#77024,#77025,#77026,#77027),(#77028,#77029,#77030,#77031,#77032,#77033,
#77034,#77035,#77036,#77037,#77038,#77039,#77040,#77041,#77042,#77043,#77044,
#77045,#77046,#77047,#77048,#77049,#77050,#77051,#77052,#77053,#77054,#77055,
#77056,#77057,#77058,#77059,#77060,#77061,#77062,#77063,#77064,#77065,#77066,
#77067,#77068,#77069,#77070,#77071,#77072,#77073,#77074,#77075,#77076,#77077,
#77078,#77079,#77080,#77081,#77082,#77083,#77084,#77085,#77086,#77087,#77088,
#77089,#77090,#77091,#77092,#77093,#77094,#77095,#77096,#77097,#77098,#77099,
#77100,#77101,#77102,#77103,#77104,#77105,#77106,#77107,#77108,#77109,#77110,
#77111,#77112,#77113,#77114,#77115,#77116,#77117,#77118,#77119,#77120,#77121,
#77122,#77123,#77124,#77125,#77126,#77127,#77128,#77129,#77130,#77131,#77132,
#77133,#77134,#77135,#77136,#77137)),.UNSPECIFIED.,.T.,.F.,.F.,(4,1,1,1,
1,1,1,4),(4,1,1,1,1,1,1,1,1,1,1,1,1,1,1,1,1,1,1,1,1,1,1,1,1,1,1,1,1,1,1,
1,1,1,1,1,1,1,1,1,1,1,1,1,1,1,1,1,1,1,1,1,1,1,1,1,1,1,1,1,1,1,1,1,1,1,1,
1,1,1,1,1,1,1,1,1,1,1,1,1,1,1,1,1,1,1,1,1,1,1,1,1,1,1,1,1,1,1,1,1,1,1,1,
1,1,1,1,4),(-3.14159265358979,-2.24399475256414,-1.34639685153848,-0.448798950512828,
0.448798950512828,1.34639685153848,2.24399475256414,3.14159265358979),(0.,
0.00446428571428571,0.00892857142857143,0.0178571428571429,0.0267857142857143,
0.0357142857142857,0.0446428571428571,0.0535714285714286,0.0625,0.0714285714285714,
0.0803571428571428,0.0892857142857143,0.0982142857142857,0.107142857142857,
0.116071428571429,0.125,0.133928571428571,0.142857142857143,0.154761904761905,
0.166666666666667,0.178571428571429,0.18452380952381,0.19047619047619,0.196428571428571,
0.202380952380952,0.214285714285714,0.222222222222222,0.23015873015873,
0.238095238095238,0.244047619047619,0.25,0.261904761904762,0.273809523809524,
0.285714285714286,0.297619047619048,0.30952380952381,0.321428571428571,
0.333333333333333,0.341269841269841,0.349206349206349,0.357142857142857,
0.365079365079365,0.373015873015873,0.380952380952381,0.392857142857143,
0.404761904761905,0.416666666666667,0.428571428571429,0.44047619047619,
0.452380952380952,0.46031746031746,0.468253968253968,0.472222222222222,
0.476190476190476,0.486772486772487,0.492063492063492,0.5,0.507936507936508,
0.515873015873016,0.523809523809524,0.535714285714286,0.547619047619048,
0.55952380952381,0.571428571428571,0.583333333333333,0.595238095238095,
0.607142857142857,0.619047619047619,0.626984126984127,0.634920634920635,
0.642857142857143,0.650793650793651,0.658730158730159,0.666666666666667,
0.674603174603175,0.682539682539683,0.69047619047619,0.702380952380952,
0.714285714285714,0.726190476190476,0.738095238095238,0.75,0.761904761904762,
0.773809523809524,0.785714285714286,0.797619047619047,0.809523809523809,
0.821428571428571,0.833333333333333,0.845238095238095,0.857142857142857,
0.866071428571429,0.875,0.883928571428571,0.892857142857143,0.901785714285714,
0.910714285714286,0.919642857142857,0.928571428571429,0.9375,0.946428571428571,
0.955357142857143,0.964285714285714,0.973214285714286,0.982142857142857,
0.991071428571429,0.995535714285714,1.),.UNSPECIFIED.);
#384=B_SPLINE_SURFACE_WITH_KNOTS('',3,3,((#84473,#84474,#84475,#84476,#84477,
#84478,#84479,#84480,#84481,#84482,#84483,#84484,#84485,#84486,#84487,#84488,
#84489,#84490,#84491,#84492,#84493,#84494,#84495,#84496,#84497,#84498,#84499,
#84500,#84501,#84502,#84503,#84504,#84505,#84506,#84507,#84508,#84509,#84510,
#84511,#84512,#84513,#84514,#84515,#84516,#84517,#84518,#84519,#84520,#84521,
#84522,#84523,#84524,#84525,#84526,#84527,#84528,#84529,#84530,#84531,#84532,
#84533,#84534,#84535,#84536,#84537,#84538,#84539,#84540,#84541,#84542,#84543,
#84544,#84545,#84546,#84547,#84548,#84549,#84550,#84551,#84552,#84553,#84554,
#84555,#84556,#84557,#84558,#84559,#84560,#84561,#84562,#84563,#84564,#84565),
(#84566,#84567,#84568,#84569,#84570,#84571,#84572,#84573,#84574,#84575,
#84576,#84577,#84578,#84579,#84580,#84581,#84582,#84583,#84584,#84585,#84586,
#84587,#84588,#84589,#84590,#84591,#84592,#84593,#84594,#84595,#84596,#84597,
#84598,#84599,#84600,#84601,#84602,#84603,#84604,#84605,#84606,#84607,#84608,
#84609,#84610,#84611,#84612,#84613,#84614,#84615,#84616,#84617,#84618,#84619,
#84620,#84621,#84622,#84623,#84624,#84625,#84626,#84627,#84628,#84629,#84630,
#84631,#84632,#84633,#84634,#84635,#84636,#84637,#84638,#84639,#84640,#84641,
#84642,#84643,#84644,#84645,#84646,#84647,#84648,#84649,#84650,#84651,#84652,
#84653,#84654,#84655,#84656,#84657,#84658),(#84659,#84660,#84661,#84662,
#84663,#84664,#84665,#84666,#84667,#84668,#84669,#84670,#84671,#84672,#84673,
#84674,#84675,#84676,#84677,#84678,#84679,#84680,#84681,#84682,#84683,#84684,
#84685,#84686,#84687,#84688,#84689,#84690,#84691,#84692,#84693,#84694,#84695,
#84696,#84697,#84698,#84699,#84700,#84701,#84702,#84703,#84704,#84705,#84706,
#84707,#84708,#84709,#84710,#84711,#84712,#84713,#84714,#84715,#84716,#84717,
#84718,#84719,#84720,#84721,#84722,#84723,#84724,#84725,#84726,#84727,#84728,
#84729,#84730,#84731,#84732,#84733,#84734,#84735,#84736,#84737,#84738,#84739,
#84740,#84741,#84742,#84743,#84744,#84745,#84746,#84747,#84748,#84749,#84750,
#84751),(#84752,#84753,#84754,#84755,#84756,#84757,#84758,#84759,#84760,
#84761,#84762,#84763,#84764,#84765,#84766,#84767,#84768,#84769,#84770,#84771,
#84772,#84773,#84774,#84775,#84776,#84777,#84778,#84779,#84780,#84781,#84782,
#84783,#84784,#84785,#84786,#84787,#84788,#84789,#84790,#84791,#84792,#84793,
#84794,#84795,#84796,#84797,#84798,#84799,#84800,#84801,#84802,#84803,#84804,
#84805,#84806,#84807,#84808,#84809,#84810,#84811,#84812,#84813,#84814,#84815,
#84816,#84817,#84818,#84819,#84820,#84821,#84822,#84823,#84824,#84825,#84826,
#84827,#84828,#84829,#84830,#84831,#84832,#84833,#84834,#84835,#84836,#84837,
#84838,#84839,#84840,#84841,#84842,#84843,#84844)),.UNSPECIFIED.,.F.,.F.,
 .F.,(4,4),(4,1,1,1,1,1,1,1,1,1,1,1,1,1,1,1,1,1,1,1,1,1,1,1,1,1,1,1,1,1,
1,1,1,1,1,1,1,1,1,1,1,1,1,1,1,1,1,1,1,1,1,1,1,1,1,1,1,1,1,1,1,1,1,1,1,1,
1,1,1,1,1,1,1,1,1,1,1,1,1,1,1,1,1,1,1,1,1,1,1,1,4),(-0.000253204253161567,
0.04630431131317),(8.3105869227397,9.30553171793124,10.3004765131228,11.2954213083143,
12.2903661035059,13.2853108986974,14.2802556938889,15.2752004890805,16.270145284272,
17.2650900794635,18.2600348746551,19.2549796698466,20.2499244650382,21.2448692602297,
22.2398140554212,23.2347588506128,24.2297036458043,25.2246484409959,26.2195932361874,
27.2145380313789,28.2094828265705,29.204427621762,30.1993724169535,31.1943172121451,
32.1892620073366,33.1842068025282,34.1791515977197,35.1740963929112,36.1690411881028,
37.1639859832943,38.1589307784859,39.1538755736774,40.1488203688689,41.1437651640605,
42.138709959252,43.1336547544436,44.1285995496351,45.1235443448266,46.1184891400182,
47.1134339352097,48.1083787304012,49.1033235255928,50.0982683207843,51.0932131159759,
52.0881579111674,53.0831027063589,54.0780475015505,55.072992296742,56.0679370919336,
57.0628818871251,58.0578266823166,59.0527714775082,60.0477162726997,61.0426610678912,
62.0376058630828,63.0325506582743,64.0274954534659,65.0224402486574,66.0173850438489,
67.0123298390405,68.007274634232,69.0022194294236,69.9971642246151,70.9921090198066,
71.9870538149982,72.9819986101897,73.9769434053812,74.9718882005728,75.9668329957643,
76.9617777909559,77.9567225861474,78.951667381339,79.9466121765305,80.941556971722,
81.9365017669136,82.9314465621051,83.9263913572966,84.9213361524882,85.9162809476797,
86.9112257428713,87.9061705380628,88.9011153332543,89.8960601284459,90.8910049236374,
91.885949718829,92.8808945140205,93.875839309212,94.8707841044036,95.8657288995951,
96.8606736947866,97.8556184899782),.UNSPECIFIED.);
#385=B_SPLINE_SURFACE_WITH_KNOTS('',3,3,((#85012,#85013,#85014,#85015,#85016,
#85017,#85018,#85019,#85020,#85021,#85022,#85023,#85024,#85025,#85026,#85027,
#85028,#85029,#85030,#85031,#85032,#85033,#85034,#85035,#85036,#85037,#85038,
#85039,#85040,#85041,#85042,#85043,#85044,#85045,#85046,#85047,#85048,#85049,
#85050,#85051,#85052,#85053,#85054,#85055,#85056,#85057,#85058,#85059,#85060,
#85061,#85062,#85063,#85064,#85065,#85066,#85067,#85068,#85069,#85070,#85071,
#85072,#85073,#85074,#85075,#85076,#85077,#85078,#85079,#85080,#85081,#85082,
#85083,#85084,#85085,#85086,#85087,#85088,#85089,#85090,#85091,#85092,#85093,
#85094,#85095,#85096,#85097,#85098,#85099,#85100,#85101,#85102,#85103,#85104),
(#85105,#85106,#85107,#85108,#85109,#85110,#85111,#85112,#85113,#85114,
#85115,#85116,#85117,#85118,#85119,#85120,#85121,#85122,#85123,#85124,#85125,
#85126,#85127,#85128,#85129,#85130,#85131,#85132,#85133,#85134,#85135,#85136,
#85137,#85138,#85139,#85140,#85141,#85142,#85143,#85144,#85145,#85146,#85147,
#85148,#85149,#85150,#85151,#85152,#85153,#85154,#85155,#85156,#85157,#85158,
#85159,#85160,#85161,#85162,#85163,#85164,#85165,#85166,#85167,#85168,#85169,
#85170,#85171,#85172,#85173,#85174,#85175,#85176,#85177,#85178,#85179,#85180,
#85181,#85182,#85183,#85184,#85185,#85186,#85187,#85188,#85189,#85190,#85191,
#85192,#85193,#85194,#85195,#85196,#85197),(#85198,#85199,#85200,#85201,
#85202,#85203,#85204,#85205,#85206,#85207,#85208,#85209,#85210,#85211,#85212,
#85213,#85214,#85215,#85216,#85217,#85218,#85219,#85220,#85221,#85222,#85223,
#85224,#85225,#85226,#85227,#85228,#85229,#85230,#85231,#85232,#85233,#85234,
#85235,#85236,#85237,#85238,#85239,#85240,#85241,#85242,#85243,#85244,#85245,
#85246,#85247,#85248,#85249,#85250,#85251,#85252,#85253,#85254,#85255,#85256,
#85257,#85258,#85259,#85260,#85261,#85262,#85263,#85264,#85265,#85266,#85267,
#85268,#85269,#85270,#85271,#85272,#85273,#85274,#85275,#85276,#85277,#85278,
#85279,#85280,#85281,#85282,#85283,#85284,#85285,#85286,#85287,#85288,#85289,
#85290),(#85291,#85292,#85293,#85294,#85295,#85296,#85297,#85298,#85299,
#85300,#85301,#85302,#85303,#85304,#85305,#85306,#85307,#85308,#85309,#85310,
#85311,#85312,#85313,#85314,#85315,#85316,#85317,#85318,#85319,#85320,#85321,
#85322,#85323,#85324,#85325,#85326,#85327,#85328,#85329,#85330,#85331,#85332,
#85333,#85334,#85335,#85336,#85337,#85338,#85339,#85340,#85341,#85342,#85343,
#85344,#85345,#85346,#85347,#85348,#85349,#85350,#85351,#85352,#85353,#85354,
#85355,#85356,#85357,#85358,#85359,#85360,#85361,#85362,#85363,#85364,#85365,
#85366,#85367,#85368,#85369,#85370,#85371,#85372,#85373,#85374,#85375,#85376,
#85377,#85378,#85379,#85380,#85381,#85382,#85383)),.UNSPECIFIED.,.F.,.F.,
 .F.,(4,4),(4,1,1,1,1,1,1,1,1,1,1,1,1,1,1,1,1,1,1,1,1,1,1,1,1,1,1,1,1,1,
1,1,1,1,1,1,1,1,1,1,1,1,1,1,1,1,1,1,1,1,1,1,1,1,1,1,1,1,1,1,1,1,1,1,1,1,
1,1,1,1,1,1,1,1,1,1,1,1,1,1,1,1,1,1,1,1,1,1,1,1,4),(-0.000274284936597264,
0.0463311323873803),(11.6151052031776,12.6103663143021,13.6053111094936,
14.6002559046852,15.5952006998767,16.5901454950682,17.5850902902598,18.5800350854513,
19.5749798806429,20.5699246758344,21.5648694710259,22.5598142662175,23.554759061409,
24.5497038566006,25.5446486517921,26.5395934469836,27.5345382421752,28.5294830373667,
29.5244278325583,30.5193726277498,31.5143174229413,32.5092622181329,33.5042070133244,
34.4991518085159,35.4940966037075,36.489041398899,37.4839861940906,38.4789309892821,
39.4738757844736,40.4688205796652,41.4637653748567,42.4587101700483,43.4536549652398,
44.4485997604313,45.4435445556229,46.4384893508144,47.433434146006,48.4283789411975,
49.423323736389,50.4182685315806,51.4132133267721,52.4081581219637,53.4031029171552,
54.3980477123467,55.3929925075383,56.3879373027298,57.3828820979213,58.3778268931129,
59.3727716883044,60.367716483496,61.3626612786875,62.357606073879,63.3525508690706,
64.3474956642621,65.3424404594537,66.3373852546452,67.3323300498367,68.3272748450283,
69.3222196402198,70.3171644354113,71.3121092306029,72.3070540257944,73.301998820986,
74.2969436161775,75.291888411369,76.2868332065606,77.2817780017521,78.2767227969437,
79.2716675921352,80.2666123873267,81.2615571825183,82.2565019777098,83.2514467729014,
84.2463915680929,85.2413363632844,86.236281158476,87.2312259536675,88.226170748859,
89.2211155440506,90.2160603392421,91.2110051344337,92.2059499296252,93.2008947248167,
94.1958395200083,95.1907843151998,96.1857291103914,97.1806739055829,98.1756187007744,
99.170563495966,100.165508291158,101.160453086349),.UNSPECIFIED.);
#386=FACE_BOUND('',#2906,.T.);
#387=FACE_BOUND('',#2909,.T.);
#388=FACE_BOUND('',#2913,.T.);
#389=FACE_BOUND('',#2916,.T.);
#390=FACE_BOUND('',#3005,.T.);
#391=FACE_BOUND('',#3006,.T.);
#392=FACE_BOUND('',#3007,.T.);
#393=FACE_BOUND('',#3008,.T.);
#394=FACE_BOUND('',#3018,.T.);
#395=FACE_BOUND('',#3019,.T.);
#396=FACE_BOUND('',#3020,.T.);
#397=FACE_BOUND('',#3021,.T.);
#398=FACE_BOUND('',#3084,.T.);
#399=FACE_BOUND('',#3085,.T.);
#400=FACE_BOUND('',#3086,.T.);
#401=FACE_BOUND('',#3087,.T.);
#402=FACE_BOUND('',#3088,.T.);
#403=FACE_BOUND('',#3089,.T.);
#404=FACE_BOUND('',#3090,.T.);
#405=FACE_BOUND('',#3114,.T.);
#406=FACE_BOUND('',#3126,.T.);
#407=FACE_BOUND('',#3130,.T.);
#408=FACE_BOUND('',#3131,.T.);
#409=FACE_BOUND('',#3132,.T.);
#410=FACE_BOUND('',#3133,.T.);
#411=FACE_BOUND('',#3173,.T.);
#412=FACE_BOUND('',#3174,.T.);
#413=FACE_BOUND('',#3175,.T.);
#414=FACE_BOUND('',#3176,.T.);
#415=FACE_BOUND('',#3177,.T.);
#416=FACE_BOUND('',#3178,.T.);
#417=FACE_BOUND('',#3179,.T.);
#418=FACE_BOUND('',#3180,.T.);
#419=FACE_BOUND('',#3181,.T.);
#420=FACE_BOUND('',#3183,.T.);
#421=FACE_BOUND('',#3184,.T.);
#422=FACE_BOUND('',#3185,.T.);
#423=FACE_BOUND('',#3186,.T.);
#424=FACE_BOUND('',#3187,.T.);
#425=FACE_BOUND('',#3188,.T.);
#426=FACE_BOUND('',#3189,.T.);
#427=FACE_BOUND('',#3190,.T.);
#428=FACE_BOUND('',#3191,.T.);
#429=FACE_BOUND('',#3202,.T.);
#430=FACE_BOUND('',#3203,.T.);
#431=FACE_BOUND('',#3204,.T.);
#432=FACE_BOUND('',#3205,.T.);
#433=FACE_BOUND('',#3214,.T.);
#434=FACE_BOUND('',#3215,.T.);
#435=FACE_BOUND('',#3216,.T.);
#436=FACE_BOUND('',#3217,.T.);
#437=FACE_BOUND('',#3219,.T.);
#438=FACE_BOUND('',#3220,.T.);
#439=FACE_BOUND('',#3237,.T.);
#440=FACE_BOUND('',#3246,.T.);
#441=FACE_BOUND('',#3257,.T.);
#442=FACE_BOUND('',#3258,.T.);
#443=FACE_BOUND('',#3265,.T.);
#444=FACE_BOUND('',#3269,.T.);
#445=FACE_BOUND('',#3270,.T.);
#446=FACE_BOUND('',#3272,.T.);
#447=FACE_BOUND('',#3273,.T.);
#448=FACE_BOUND('',#3275,.T.);
#449=FACE_BOUND('',#3282,.T.);
#450=FACE_BOUND('',#3285,.T.);
#451=FACE_BOUND('',#3288,.T.);
#452=FACE_BOUND('',#3293,.T.);
#453=FACE_BOUND('',#3296,.T.);
#454=FACE_BOUND('',#3299,.T.);
#455=FACE_BOUND('',#3306,.T.);
#456=FACE_BOUND('',#3345,.T.);
#457=FACE_BOUND('',#3348,.T.);
#458=FACE_BOUND('',#3352,.T.);
#459=FACE_BOUND('',#3357,.T.);
#460=FACE_BOUND('',#3361,.T.);
#461=FACE_BOUND('',#3365,.T.);
#462=FACE_BOUND('',#3368,.T.);
#463=FACE_BOUND('',#3371,.T.);
#464=FACE_BOUND('',#3376,.T.);
#465=FACE_BOUND('',#3379,.T.);
#466=FACE_BOUND('',#3382,.T.);
#467=FACE_BOUND('',#3387,.T.);
#468=FACE_BOUND('',#3392,.T.);
#469=FACE_BOUND('',#3398,.T.);
#470=FACE_BOUND('',#3401,.T.);
#471=FACE_BOUND('',#3409,.T.);
#472=FACE_BOUND('',#3412,.T.);
#473=FACE_BOUND('',#3455,.T.);
#474=FACE_BOUND('',#3459,.T.);
#475=ELLIPSE('',#10109,0.179163796285099,0.132134456811432);
#476=ELLIPSE('',#10160,0.0711578408474482,0.0609612663807345);
#477=ELLIPSE('',#10161,0.643183425815913,0.414173412397355);
#478=ELLIPSE('',#10163,0.0804815181446777,0.0720771207638654);
#479=ELLIPSE('',#10165,0.062158381280911,0.0435390307992324);
#480=ELLIPSE('',#10177,0.0691697767700365,0.0595893379399011);
#481=ELLIPSE('',#10204,0.111726638420037,0.0803736621029293);
#482=ELLIPSE('',#10214,0.0704571051122974,0.0497299141222001);
#483=ELLIPSE('',#10227,0.417631904706076,0.321033921213905);
#484=ELLIPSE('',#10257,0.224701868798773,0.0973759172030223);
#485=ELLIPSE('',#10259,0.14551373866235,0.0747733658362826);
#486=ELLIPSE('',#10277,0.11254060849194,0.108742931573845);
#487=ELLIPSE('',#10285,0.0694099985395438,0.0599094462298757);
#488=ELLIPSE('',#10286,0.138556662637378,0.119815564117158);
#489=ELLIPSE('',#10291,0.0693000182697834,0.0597453527106058);
#490=B_SPLINE_CURVE_WITH_KNOTS('',3,(#13238,#13239,#13240,#13241),
 .UNSPECIFIED.,.F.,.F.,(4,4),(0.394864882524291,0.484810313459459),
 .UNSPECIFIED.);
#491=B_SPLINE_CURVE_WITH_KNOTS('',3,(#13248,#13249,#13250,#13251,#13252,
#13253,#13254,#13255,#13256,#13257,#13258,#13259,#13260,#13261,#13262,#13263,
#13264,#13265,#13266,#13267,#13268,#13269,#13270,#13271,#13272,#13273,#13274,
#13275,#13276,#13277,#13278,#13279,#13280,#13281),.UNSPECIFIED.,.F.,.F.,
(4,1,1,1,1,1,1,1,1,1,1,1,1,1,1,1,1,1,1,1,1,1,1,1,1,1,1,1,1,1,1,4),(-12.272421221397,
-11.8341204634899,-11.3958197055829,-10.9575189476759,-10.6287933792456,
-10.5192181897688,-9.93481717922612,-9.64261667395476,-9.35041616868341,
-9.05821566341205,-8.76601515814069,-8.18161414759798,-7.59721313705527,
-7.30501263178391,-7.01281212651256,-6.42841111596984,-5.84401010542713,
-5.55180960015577,-5.25960909488442,-5.11350884224874,-4.96740858961306,
-4.6752080843417,-4.09080707379899,-4.01775694748115,-3.50640606325628,
-2.62980454744221,-2.19150378953517,-1.75320303162814,-1.3149022737211,
-0.876601515814069,-0.438300757907035,0.),.UNSPECIFIED.);
#492=B_SPLINE_CURVE_WITH_KNOTS('',3,(#13289,#13290,#13291,#13292),
 .UNSPECIFIED.,.F.,.F.,(4,4),(-1.01772858153936,-0.900201355715508),
 .UNSPECIFIED.);
#493=B_SPLINE_CURVE_WITH_KNOTS('',3,(#13294,#13295,#13296,#13297),
 .UNSPECIFIED.,.F.,.F.,(4,4),(-0.195956842698031,-5.68173586430139E-15),
 .UNSPECIFIED.);
#494=B_SPLINE_CURVE_WITH_KNOTS('',3,(#13299,#13300,#13301,#13302,#13303,
#13304),.UNSPECIFIED.,.F.,.F.,(4,2,4),(-0.531787427886525,-0.530925715886322,
0.),.UNSPECIFIED.);
#495=B_SPLINE_CURVE_WITH_KNOTS('',3,(#13308,#13309,#13310,#13311,#13312,
#13313),.UNSPECIFIED.,.F.,.F.,(4,2,4),(0.,0.0240503814822642,0.0482649912255638),
 .UNSPECIFIED.);
#496=B_SPLINE_CURVE_WITH_KNOTS('',3,(#13315,#13316,#13317,#13318,#13319),
 .UNSPECIFIED.,.F.,.F.,(4,1,4),(0.,0.0699088059566157,0.0984547839530403),
 .UNSPECIFIED.);
#497=B_SPLINE_CURVE_WITH_KNOTS('',5,(#13321,#13322,#13323,#13324,#13325,
#13326,#13327,#13328,#13329,#13330,#13331,#13332,#13333,#13334,#13335,#13336,
#13337,#13338,#13339,#13340,#13341,#13342,#13343,#13344,#13345,#13346,#13347,
#13348,#13349,#13350,#13351,#13352,#13353,#13354,#13355,#13356,#13357,#13358,
#13359,#13360,#13361,#13362,#13363,#13364,#13365,#13366,#13367,#13368,#13369,
#13370,#13371,#13372,#13373,#13374,#13375,#13376,#13377,#13378,#13379,#13380,
#13381,#13382,#13383,#13384,#13385,#13386,#13387,#13388,#13389),
 .UNSPECIFIED.,.F.,.F.,(6,1,1,1,1,1,1,1,1,1,1,1,1,1,1,1,1,1,1,1,1,1,1,1,
1,1,1,1,1,1,1,1,1,1,1,1,1,1,1,1,1,1,1,1,1,1,1,1,1,1,1,1,1,1,1,1,1,1,1,1,
1,1,1,1,6),(-0.934439937517936,-0.932000000000001,-0.928000000000001,-0.924000000000001,
-0.920000000000001,-0.916000000000001,-0.912000000000001,-0.908000000000001,
-0.904000000000001,-0.900000000000001,-0.896000000000001,-0.892000000000001,
-0.888000000000001,-0.884000000000001,-0.880000000000001,-0.876000000000001,
-0.872000000000001,-0.868000000000001,-0.864000000000001,-0.860000000000001,
-0.856000000000001,-0.852000000000001,-0.848000000000001,-0.844000000000001,
-0.840000000000001,-0.836000000000001,-0.832000000000001,-0.828000000000001,
-0.824000000000001,-0.820000000000001,-0.816000000000001,-0.812000000000001,
-0.808000000000001,-0.804000000000001,-0.800000000000001,-0.796000000000001,
-0.792000000000001,-0.788000000000001,-0.784000000000001,-0.780000000000001,
-0.776000000000001,-0.772000000000001,-0.768000000000001,-0.764000000000001,
-0.760000000000001,-0.756000000000001,-0.752000000000001,-0.748000000000001,
-0.744000000000001,-0.740000000000001,-0.736000000000001,-0.732000000000001,
-0.728000000000001,-0.724000000000001,-0.720000000000001,-0.716000000000001,
-0.712000000000001,-0.708000000000001,-0.704000000000001,-0.700000000000001,
-0.696000000000001,-0.692000000000001,-0.688000000000001,-0.684,-0.681561309195619),
 .UNSPECIFIED.);
#498=B_SPLINE_CURVE_WITH_KNOTS('',5,(#13391,#13392,#13393,#13394,#13395,
#13396,#13397),.UNSPECIFIED.,.F.,.F.,(6,1,6),(-0.681561309195566,-0.68,
-0.679861520205026),.UNSPECIFIED.);
#499=B_SPLINE_CURVE_WITH_KNOTS('',3,(#13398,#13399,#13400,#13401,#13402,
#13403),.UNSPECIFIED.,.F.,.F.,(4,2,4),(-0.260568044992996,-0.115264054870948,
0.),.UNSPECIFIED.);
#500=B_SPLINE_CURVE_WITH_KNOTS('',3,(#13423,#13424,#13425,#13426,#13427,
#13428,#13429),.UNSPECIFIED.,.F.,.F.,(4,3,4),(0.584503639029328,0.623122512964242,
0.74773332064937),.UNSPECIFIED.);
#501=B_SPLINE_CURVE_WITH_KNOTS('',3,(#13433,#13434,#13435,#13436),
 .UNSPECIFIED.,.F.,.F.,(4,4),(-0.0543233651499556,0.),.UNSPECIFIED.);
#502=B_SPLINE_CURVE_WITH_KNOTS('',3,(#13437,#13438,#13439,#13440,#13441,
#13442,#13443,#13444,#13445,#13446,#13447,#13448,#13449,#13450,#13451,#13452,
#13453,#13454,#13455,#13456,#13457,#13458,#13459,#13460,#13461,#13462,#13463,
#13464,#13465,#13466,#13467,#13468,#13469,#13470,#13471),.UNSPECIFIED.,
 .F.,.F.,(4,1,1,1,1,1,1,1,1,1,1,1,1,1,1,1,1,1,1,1,1,1,1,1,1,1,1,1,1,1,1,
1,4),(-12.1338940883735,-11.7005407280745,-11.2671873677754,-10.4004806471773,
-9.82267616677859,-9.24487168637985,-8.66706720598111,-8.08926272558237,
-7.800360485383,-7.65590936528331,-7.51145824518363,-7.36700712508394,-7.22255600498426,
-6.93365376478489,-6.64475152458552,-6.35584928438614,-6.06694704418677,
-5.77804480398741,-5.20024032358866,-4.91133808338929,-4.62243584318992,
-4.04463136279118,-3.46682688239244,-3.25015020224292,-3.03347352209339,
-2.60012016179433,-2.49178182171957,-2.16676680149528,-1.73341344119622,
-1.30006008089717,-0.866706720598111,-0.433353360299055,0.),
 .UNSPECIFIED.);
#503=B_SPLINE_CURVE_WITH_KNOTS('',3,(#13479,#13480,#13481,#13482,#13483,
#13484,#13485),.UNSPECIFIED.,.F.,.F.,(4,3,4),(0.489041562207919,0.588820757539051,
0.610492150702822),.UNSPECIFIED.);
#504=B_SPLINE_CURVE_WITH_KNOTS('',3,(#13487,#13488,#13489,#13490,#13491,
#13492),.UNSPECIFIED.,.F.,.F.,(4,1,1,4),(0.,0.0638374291107252,0.12767485822145,
0.141538528407714),.UNSPECIFIED.);
#505=B_SPLINE_CURVE_WITH_KNOTS('',5,(#13494,#13495,#13496,#13497,#13498,
#13499,#13500,#13501,#13502,#13503,#13504,#13505,#13506,#13507,#13508,#13509,
#13510,#13511,#13512,#13513,#13514,#13515,#13516,#13517,#13518,#13519,#13520,
#13521,#13522,#13523,#13524,#13525,#13526,#13527,#13528,#13529,#13530,#13531,
#13532,#13533,#13534,#13535,#13536,#13537,#13538,#13539,#13540,#13541,#13542,
#13543,#13544,#13545,#13546,#13547,#13548,#13549,#13550,#13551,#13552,#13553,
#13554,#13555,#13556,#13557,#13558,#13559,#13560),.UNSPECIFIED.,.F.,.F.,
(6,1,1,1,1,1,1,1,1,1,1,1,1,1,1,1,1,1,1,1,1,1,1,1,1,1,1,1,1,1,1,1,1,1,1,
1,1,1,1,1,1,1,1,1,1,1,1,1,1,1,1,1,1,1,1,1,1,1,1,1,1,1,6),(-0.304944691462234,
-0.304,-0.3,-0.296,-0.292,-0.288,-0.284,-0.28,-0.276,-0.272,-0.268,-0.264,
-0.26,-0.256,-0.252,-0.248,-0.244,-0.24,-0.236,-0.232,-0.228,-0.224,-0.22,
-0.216,-0.212,-0.208,-0.204,-0.2,-0.196,-0.192,-0.188,-0.184,-0.18,-0.176,
-0.172,-0.168,-0.164,-0.16,-0.156,-0.152,-0.148,-0.144,-0.14,-0.136,-0.132,
-0.128,-0.124,-0.12,-0.116,-0.112,-0.108,-0.104,-0.1,-0.0960000000000001,
-0.0920000000000001,-0.0880000000000001,-0.084,-0.08,-0.076,-0.072,-0.068,
-0.064,-0.0619278530721094),.UNSPECIFIED.);
#506=B_SPLINE_CURVE_WITH_KNOTS('',3,(#13562,#13563,#13564,#13565,#13566,
#13567),.UNSPECIFIED.,.F.,.F.,(4,2,4),(-0.0398334813165403,-0.0199277813067177,
-9.94871254822449E-10),.UNSPECIFIED.);
#507=B_SPLINE_CURVE_WITH_KNOTS('',3,(#13569,#13570,#13571,#13572,#13573,
#13574),.UNSPECIFIED.,.F.,.F.,(4,2,4),(2.70147232916989E-5,0.0170939199782327,
0.035271687213346),.UNSPECIFIED.);
#508=B_SPLINE_CURVE_WITH_KNOTS('',3,(#13576,#13577,#13578,#13579,#13580,
#13581,#13582,#13583,#13584,#13585,#13586,#13587,#13588,#13589,#13590,#13591,
#13592,#13593,#13594,#13595),.UNSPECIFIED.,.F.,.F.,(4,2,2,2,2,2,2,2,2,4),
(1.63651820619147E-6,0.010862670932703,0.0337514199363196,0.0421677436560315,
0.0461502331381883,0.0493656606269703,0.0531827874377784,0.0608034042333055,
0.0815457243745407,0.0967454812796038),.UNSPECIFIED.);
#509=B_SPLINE_CURVE_WITH_KNOTS('',3,(#13597,#13598,#13599,#13600,#13601,
#13602),.UNSPECIFIED.,.F.,.F.,(4,2,4),(8.18815340054483E-6,0.00711074921072509,
0.0142181038164433),.UNSPECIFIED.);
#510=B_SPLINE_CURVE_WITH_KNOTS('',3,(#13604,#13605,#13606,#13607,#13608,
#13609),.UNSPECIFIED.,.F.,.F.,(4,2,4),(1.21976025657623E-6,0.00359236891011489,
0.00724827734012079),.UNSPECIFIED.);
#511=B_SPLINE_CURVE_WITH_KNOTS('',3,(#13611,#13612,#13613,#13614,#13615,
#13616),.UNSPECIFIED.,.F.,.F.,(4,2,4),(1.24265944092431E-5,0.0394422622090392,
0.0830428857918921),.UNSPECIFIED.);
#512=B_SPLINE_CURVE_WITH_KNOTS('',3,(#13618,#13619,#13620,#13621,#13622,
#13623,#13624,#13625),.UNSPECIFIED.,.F.,.F.,(4,2,2,4),(-0.000597804895778801,
0.,0.0849714808180455,0.169669487930669),.UNSPECIFIED.);
#513=B_SPLINE_CURVE_WITH_KNOTS('',3,(#13642,#13643,#13644,#13645,#13646,
#13647,#13648,#13649,#13650,#13651,#13652,#13653,#13654,#13655,#13656,#13657,
#13658,#13659,#13660),.UNSPECIFIED.,.F.,.F.,(4,3,3,3,3,3,4),(0.,0.057820470339356,
0.0749307800866031,0.0860134923791381,0.116509264080236,0.148377898752131,
0.154536834355727),.UNSPECIFIED.);
#514=B_SPLINE_CURVE_WITH_KNOTS('',3,(#13668,#13669,#13670,#13671,#13672,
#13673,#13674,#13675,#13676,#13677,#13678,#13679,#13680,#13681,#13682,#13683,
#13684,#13685,#13686,#13687,#13688,#13689,#13690,#13691,#13692,#13693,#13694,
#13695),.UNSPECIFIED.,.F.,.F.,(4,3,3,3,3,3,3,3,3,4),(-0.221165784147146,
-0.203605965934998,-0.1863734624514,-0.168207576681715,-0.143931298953183,
-0.100603143960458,-0.064904744585576,-0.048733613964838,-0.0209494131580949,
-9.99999236175762E-7),.UNSPECIFIED.);
#515=B_SPLINE_CURVE_WITH_KNOTS('',3,(#14221,#14222,#14223,#14224,#14225,
#14226,#14227,#14228,#14229,#14230,#14231,#14232,#14233,#14234,#14235,#14236,
#14237,#14238,#14239,#14240,#14241,#14242,#14243,#14244,#14245,#14246,#14247,
#14248,#14249,#14250,#14251,#14252,#14253,#14254,#14255),.UNSPECIFIED.,
 .F.,.F.,(4,1,1,1,1,1,1,1,1,1,1,1,1,1,1,1,1,1,1,1,1,1,1,1,1,1,1,1,1,1,1,
1,4),(0.,0.433353360299055,0.866706720598111,1.30006008089717,1.73341344119622,
2.16676680149528,2.49178182171957,2.60012016179433,3.03347352209339,3.25015020224292,
3.46682688239244,4.04463136279118,4.62243584318992,4.91133808338929,5.20024032358866,
5.77804480398741,6.06694704418677,6.35584928438614,6.64475152458552,6.93365376478489,
7.22255600498426,7.36700712508394,7.51145824518363,7.65590936528331,7.800360485383,
8.08926272558237,8.66706720598111,9.24487168637985,9.82267616677859,10.4004806471773,
11.2671873677754,11.7005407280745,12.1338940883735),.UNSPECIFIED.);
#516=B_SPLINE_CURVE_WITH_KNOTS('',3,(#14257,#14258,#14259,#14260,#14261,
#14262,#14263,#14264),.UNSPECIFIED.,.F.,.F.,(4,1,1,1,1,4),(-0.119541952220061,
-0.117697345682202,-0.115852739144342,-0.112163526068624,-0.104785099917186,
-0.0937174606900304),.UNSPECIFIED.);
#517=B_SPLINE_CURVE_WITH_KNOTS('',3,(#14268,#14269,#14270,#14271),
 .UNSPECIFIED.,.F.,.F.,(4,4),(-0.227650451044217,0.),.UNSPECIFIED.);
#518=B_SPLINE_CURVE_WITH_KNOTS('',3,(#14478,#14479,#14480,#14481,#14482,
#14483),.UNSPECIFIED.,.F.,.F.,(4,2,4),(0.0543371154509674,0.152867184867239,
0.15340523472588),.UNSPECIFIED.);
#519=B_SPLINE_CURVE_WITH_KNOTS('',3,(#14484,#14485,#14486,#14487,#14488,
#14489,#14490,#14491,#14492,#14493,#14494,#14495,#14496,#14497,#14498,#14499,
#14500,#14501,#14502),.UNSPECIFIED.,.F.,.F.,(4,3,3,3,3,3,4),(-0.15340523472588,
-0.152867184867239,-0.121542670578485,-0.0960576486891604,-0.0776465306498218,
-0.0660266035836145,-0.05433711858811),.UNSPECIFIED.);
#520=B_SPLINE_CURVE_WITH_KNOTS('',3,(#14525,#14526,#14527,#14528,#14529,
#14530,#14531,#14532,#14533,#14534,#14535,#14536,#14537),.UNSPECIFIED.,
 .F.,.F.,(4,3,3,3,4),(0.,0.0223793464434253,0.0433077332578928,0.0522216264092524,
0.0543233530776371),.UNSPECIFIED.);
#521=B_SPLINE_CURVE_WITH_KNOTS('',3,(#14589,#14590,#14591,#14592,#14593,
#14594,#14595,#14596),.UNSPECIFIED.,.F.,.F.,(4,1,1,1,1,4),(0.0937174606900304,
0.104785099917186,0.112163526068624,0.115852739144342,0.117697345682202,
0.119541952220061),.UNSPECIFIED.);
#522=B_SPLINE_CURVE_WITH_KNOTS('',3,(#14629,#14630,#14631,#14632,#14633,
#14634),.UNSPECIFIED.,.F.,.F.,(4,1,1,4),(1.65498255800438E-15,0.129082836972258,
0.215138061620429,0.301190240731281),.UNSPECIFIED.);
#523=B_SPLINE_CURVE_WITH_KNOTS('',3,(#14660,#14661,#14662,#14663,#14664,
#14665,#14666),.UNSPECIFIED.,.F.,.F.,(4,3,4),(0.,0.150132901020185,0.227650451044083),
 .UNSPECIFIED.);
#524=B_SPLINE_CURVE_WITH_KNOTS('',3,(#14689,#14690,#14691,#14692),
 .UNSPECIFIED.,.F.,.F.,(4,4),(6.03465648009666E-14,0.0429068684110201),
 .UNSPECIFIED.);
#525=B_SPLINE_CURVE_WITH_KNOTS('',3,(#14734,#14735,#14736,#14737,#14738,
#14739,#14740,#14741,#14742,#14743,#14744,#14745,#14746,#14747,#14748,#14749,
#14750,#14751,#14752,#14753,#14754,#14755,#14756,#14757,#14758,#14759,#14760,
#14761,#14762,#14763,#14764,#14765,#14766,#14767,#14768,#14769,#14770,#14771,
#14772,#14773),.UNSPECIFIED.,.F.,.F.,(4,3,3,3,3,3,3,3,3,3,3,3,3,4),(-0.000426969481637764,
-5.70290342727375E-17,0.0136974853077621,0.0169318002365105,0.0215321188993139,
0.030659423657535,0.0358425712401134,0.0361428073033054,0.0487839324257399,
0.0601713945215638,0.0711682787397989,0.071687262555713,0.075441369769445,
0.0785208370583627),.UNSPECIFIED.);
#526=B_SPLINE_CURVE_WITH_KNOTS('',3,(#14799,#14800,#14801,#14802,#14803,
#14804,#14805,#14806,#14807,#14808,#14809,#14810,#14811,#14812,#14813,#14814,
#14815,#14816,#14817,#14818,#14819,#14820),.UNSPECIFIED.,.F.,.F.,(4,3,3,
3,3,3,3,4),(9.99999753309056E-7,0.212329740918838,0.392771135232247,0.447248810346286,
0.622477441204398,0.70601051205627,0.853321790119657,0.891484214299584),
 .UNSPECIFIED.);
#527=B_SPLINE_CURVE_WITH_KNOTS('',3,(#14825,#14826,#14827,#14828),
 .UNSPECIFIED.,.F.,.F.,(4,4),(0.0423193643606908,0.252933252504432),
 .UNSPECIFIED.);
#528=B_SPLINE_CURVE_WITH_KNOTS('',3,(#14850,#14851,#14852,#14853),
 .UNSPECIFIED.,.F.,.F.,(4,4),(0.,0.224615521635083),.UNSPECIFIED.);
#529=B_SPLINE_CURVE_WITH_KNOTS('',3,(#14876,#14877,#14878,#14879),
 .UNSPECIFIED.,.F.,.F.,(4,4),(-0.127798241063314,-0.0854459382956349),
 .UNSPECIFIED.);
#530=B_SPLINE_CURVE_WITH_KNOTS('',3,(#14923,#14924,#14925,#14926,#14927,
#14928,#14929),.UNSPECIFIED.,.F.,.F.,(4,1,1,1,4),(0.,0.0328013253035665,
0.065602650607133,0.109337751011888,0.137794282289288),.UNSPECIFIED.);
#531=B_SPLINE_CURVE_WITH_KNOTS('',3,(#14969,#14970,#14971,#14972),
 .UNSPECIFIED.,.F.,.F.,(4,4),(0.,0.17884239607127),.UNSPECIFIED.);
#532=B_SPLINE_CURVE_WITH_KNOTS('',3,(#14991,#14992,#14993,#14994),
 .UNSPECIFIED.,.F.,.F.,(4,4),(-0.0801298062963358,0.),.UNSPECIFIED.);
#533=B_SPLINE_CURVE_WITH_KNOTS('',3,(#15101,#15102,#15103,#15104,#15105,
#15106,#15107,#15108,#15109,#15110,#15111,#15112,#15113,#15114,#15115,#15116,
#15117,#15118,#15119,#15120,#15121,#15122,#15123,#15124,#15125,#15126,#15127,
#15128,#15129,#15130,#15131,#15132,#15133,#15134,#15135,#15136,#15137,#15138,
#15139,#15140,#15141,#15142,#15143,#15144,#15145,#15146,#15147,#15148,#15149,
#15150,#15151,#15152,#15153,#15154,#15155,#15156,#15157,#15158,#15159,#15160,
#15161,#15162,#15163,#15164,#15165,#15166,#15167,#15168,#15169,#15170,#15171,
#15172,#15173,#15174,#15175,#15176,#15177,#15178,#15179,#15180,#15181,#15182,
#15183,#15184,#15185,#15186,#15187,#15188,#15189,#15190,#15191,#15192,#15193,
#15194,#15195,#15196,#15197,#15198,#15199,#15200,#15201,#15202,#15203,#15204,
#15205,#15206,#15207,#15208,#15209,#15210,#15211,#15212,#15213,#15214,#15215,
#15216,#15217,#15218,#15219,#15220,#15221,#15222,#15223,#15224,#15225,#15226,
#15227,#15228,#15229,#15230,#15231,#15232,#15233,#15234,#15235,#15236,#15237,
#15238,#15239,#15240,#15241,#15242,#15243,#15244,#15245,#15246,#15247,#15248,
#15249,#15250,#15251,#15252,#15253,#15254,#15255,#15256,#15257,#15258,#15259,
#15260,#15261,#15262,#15263,#15264,#15265,#15266,#15267,#15268,#15269,#15270,
#15271,#15272,#15273,#15274,#15275,#15276,#15277,#15278,#15279,#15280,#15281,
#15282,#15283,#15284,#15285,#15286,#15287,#15288,#15289,#15290,#15291,#15292,
#15293,#15294,#15295,#15296,#15297,#15298,#15299,#15300,#15301,#15302,#15303,
#15304,#15305,#15306,#15307,#15308,#15309,#15310,#15311,#15312,#15313,#15314,
#15315,#15316,#15317,#15318,#15319,#15320,#15321,#15322,#15323),
 .UNSPECIFIED.,.F.,.F.,(4,3,3,3,3,3,3,3,3,3,3,3,3,3,3,3,3,3,3,3,3,3,3,3,
3,3,3,3,3,3,3,3,3,3,3,3,3,3,3,3,3,3,3,3,3,3,3,3,3,3,3,3,3,3,3,3,3,3,3,3,
3,3,3,3,3,3,3,3,3,3,3,3,3,3,4),(0.0143556209070032,0.0918173375013859,0.137368681256099,
0.164850487143807,0.236118654939979,0.29915612965247,0.361701124093769,
0.423757485765995,0.463705909920997,0.516706771668045,0.570541124923225,
0.604256389891492,0.685039858234251,0.766114259399882,0.848927080753196,
0.893877183497122,0.978785410078009,1.06778327179008,1.16126984103901,1.21538171189569,
1.333822502657,1.45799045338518,1.58635211001713,1.69368579518043,1.76887432285106,
1.82502584109974,1.99446359366836,2.1682652962319,2.34746509975619,2.40944331829074,
2.63945041210237,2.87599055478919,3.12224465593178,3.38274453001889,3.66483085961975,
4.00177577901762,4.34319730999942,4.59080469175813,4.73545737518022,4.788086707876,
5.04860488829482,5.29050385726843,5.52038017836126,5.74206280076628,5.90224108935206,
6.08765479241645,6.25857458098853,6.42517545732593,6.52288884673658,6.57920791189009,
6.70933184189355,6.83569015966474,6.95707192851147,7.05644314801653,7.12291710476878,
7.21605540565365,7.30472824136214,7.38580967032176,7.44201203358028,7.52405452487865,
7.60444481353644,7.68453791087736,7.71803570888323,7.77141664614894,7.82397351603657,
7.87085605861451,7.92952553290749,7.9764492685614,8.00862146467435,8.0699558254521,
8.12869572362376,8.15667568402911,8.21796501853068,8.28865197779449,8.30491541813874),
 .UNSPECIFIED.);
#534=B_SPLINE_CURVE_WITH_KNOTS('',3,(#15326,#15327,#15328,#15329,#15330,
#15331,#15332,#15333,#15334,#15335,#15336,#15337,#15338,#15339,#15340,#15341,
#15342,#15343,#15344,#15345,#15346),.UNSPECIFIED.,.F.,.F.,(4,1,1,1,1,1,
1,1,1,1,1,1,1,1,1,1,1,1,4),(-8.30491541813874,-8.15661335710055,-8.00831129606236,
-7.86000923502417,-7.71170717398598,-7.41510305190959,-7.11849892983321,
-6.52529068568044,-5.93208244152767,-4.74566595322214,-2.37283297661107,
-1.7796247324583,-1.18641648830553,-0.889812366229151,-0.593208244152767,
-0.444906183114576,-0.296604122076384,-0.148302061038192,0.),
 .UNSPECIFIED.);
#535=B_SPLINE_CURVE_WITH_KNOTS('',3,(#15432,#15433,#15434,#15435,#15436,
#15437,#15438,#15439,#15440,#15441,#15442,#15443,#15444,#15445,#15446,#15447,
#15448,#15449,#15450,#15451,#15452,#15453,#15454,#15455,#15456,#15457,#15458,
#15459,#15460,#15461,#15462,#15463,#15464,#15465,#15466,#15467,#15468,#15469,
#15470,#15471,#15472,#15473,#15474,#15475,#15476,#15477,#15478,#15479,#15480,
#15481,#15482,#15483,#15484,#15485,#15486,#15487,#15488,#15489,#15490,#15491,
#15492,#15493,#15494,#15495,#15496,#15497,#15498,#15499,#15500,#15501,#15502,
#15503,#15504,#15505,#15506,#15507,#15508,#15509,#15510,#15511,#15512,#15513,
#15514,#15515,#15516,#15517,#15518,#15519,#15520,#15521,#15522,#15523,#15524,
#15525,#15526,#15527,#15528,#15529,#15530,#15531,#15532,#15533,#15534,#15535,
#15536,#15537,#15538,#15539,#15540,#15541,#15542,#15543,#15544,#15545,#15546,
#15547,#15548,#15549,#15550,#15551,#15552,#15553,#15554,#15555,#15556,#15557,
#15558,#15559,#15560,#15561,#15562,#15563,#15564,#15565,#15566,#15567,#15568,
#15569,#15570,#15571,#15572,#15573,#15574,#15575,#15576,#15577,#15578,#15579,
#15580,#15581,#15582,#15583,#15584,#15585,#15586,#15587,#15588,#15589,#15590,
#15591,#15592,#15593,#15594,#15595,#15596,#15597,#15598,#15599,#15600,#15601,
#15602,#15603,#15604,#15605,#15606,#15607,#15608,#15609,#15610,#15611,#15612,
#15613,#15614,#15615,#15616,#15617,#15618,#15619,#15620,#15621,#15622,#15623,
#15624,#15625,#15626,#15627,#15628,#15629,#15630,#15631,#15632,#15633,#15634,
#15635,#15636,#15637,#15638,#15639,#15640,#15641,#15642,#15643,#15644,#15645,
#15646,#15647,#15648,#15649,#15650,#15651,#15652,#15653,#15654),
 .UNSPECIFIED.,.F.,.F.,(4,3,3,3,3,3,3,3,3,3,3,3,3,3,3,3,3,3,3,3,3,3,3,3,
3,3,3,3,3,3,3,3,3,3,3,3,3,3,3,3,3,3,3,3,3,3,3,3,3,3,3,3,3,3,3,3,3,3,3,3,
3,3,3,3,3,3,3,3,3,3,3,3,3,3,4),(0.,0.0796002531402428,0.143860527866794,
0.179459274819612,0.242939400939292,0.289836237203638,0.325717441475301,
0.388054925667984,0.442922087934823,0.495706533831402,0.549137052626795,
0.589808904685002,0.633776280374242,0.714472650605738,0.796031244337957,
0.863874470471167,0.933235621193325,1.02001599391656,1.11110468536068,1.19249198525964,
1.30962863517608,1.43279082776966,1.56039482576159,1.69164843617825,1.76643789090045,
1.82645895882964,1.99593365718847,2.16977738887537,2.34903131982582,2.41009920440689,
2.64012149822895,2.87668451600587,3.12297220656693,3.38352156197452,3.66568523716309,
4.00272734179774,4.34406360830132,4.59161684641616,4.73716379055164,4.78741151509335,
5.04798742679384,5.28992117381758,5.51982022830723,5.74151786718094,5.9017302141158,
6.08789567836694,6.25881116250794,6.42540866186584,6.52355479195162,6.57973305697088,
6.70984225463914,6.83618333626226,6.95754104745397,7.05650826390725,7.12298174141615,
7.21611710010299,7.30478715182435,7.38589019760746,7.44197485199613,7.52401831132503,
7.6044090168049,7.68450183493196,7.71800683849413,7.77138849884627,7.82394576594535,
7.87083250800939,7.92950086544489,7.97642768453163,8.00860889412839,8.06994218027327,
8.12868548973964,8.15666640215728,8.21795386255756,8.28863888262294,8.30491541813876),
 .UNSPECIFIED.);
#536=B_SPLINE_CURVE_WITH_KNOTS('',3,(#15798,#15799,#15800,#15801),
 .UNSPECIFIED.,.F.,.F.,(4,4),(2.65444323739948E-13,0.080129806296636),
 .UNSPECIFIED.);
#537=B_SPLINE_CURVE_WITH_KNOTS('',3,(#15830,#15831,#15832,#15833,#15834,
#15835),.UNSPECIFIED.,.F.,.F.,(4,1,1,4),(-0.140796741914463,-0.0804552810939789,
-0.0402276405469894,0.),.UNSPECIFIED.);
#538=B_SPLINE_CURVE_WITH_KNOTS('',3,(#15838,#15839,#15840,#15841,#15842,
#15843,#15844,#15845,#15846,#15847,#15848,#15849,#15850,#15851,#15852,#15853,
#15854,#15855,#15856,#15857,#15858,#15859),.UNSPECIFIED.,.F.,.F.,(4,3,3,
3,3,3,3,4),(-0.116549789703214,-0.104681178539138,-0.0961709462162922,-0.0773146819780265,
-0.0757921027293709,-0.0712796665105129,-0.0536565317120064,-0.0452352637954112),
 .UNSPECIFIED.);
#539=B_SPLINE_CURVE_WITH_KNOTS('',3,(#15879,#15880,#15881,#15882),
 .UNSPECIFIED.,.F.,.F.,(4,4),(-0.0800719510115295,0.),.UNSPECIFIED.);
#540=B_SPLINE_CURVE_WITH_KNOTS('',3,(#15950,#15951,#15952,#15953,#15954,
#15955,#15956),.UNSPECIFIED.,.F.,.F.,(4,3,4),(0.,0.0137497525298979,0.0275089565102414),
 .UNSPECIFIED.);
#541=B_SPLINE_CURVE_WITH_KNOTS('',3,(#15957,#15958,#15959,#15960),
 .UNSPECIFIED.,.F.,.F.,(4,4),(0.00882828078135349,0.428984955288124),
 .UNSPECIFIED.);
#542=B_SPLINE_CURVE_WITH_KNOTS('',3,(#16003,#16004,#16005,#16006,#16007,
#16008,#16009,#16010),.UNSPECIFIED.,.F.,.F.,(4,1,1,1,1,4),(0.0418199835477882,
0.170057059808597,0.209506993669976,0.248956927531355,0.268681894462045,
0.288323933546714),.UNSPECIFIED.);
#543=B_SPLINE_CURVE_WITH_KNOTS('',3,(#16013,#16014,#16015,#16016,#16017,
#16018,#16019,#16020,#16021,#16022,#16023,#16024,#16025,#16026,#16027,#16028,
#16029,#16030,#16031,#16032,#16033,#16034,#16035,#16036,#16037,#16038,#16039,
#16040,#16041,#16042,#16043,#16044,#16045,#16046,#16047,#16048,#16049,#16050,
#16051,#16052,#16053,#16054,#16055,#16056,#16057,#16058,#16059,#16060,#16061,
#16062,#16063,#16064,#16065,#16066,#16067,#16068,#16069,#16070,#16071,#16072,
#16073),.UNSPECIFIED.,.F.,.F.,(4,3,3,3,3,3,3,3,3,3,3,3,3,3,3,3,3,3,3,3,
4),(-0.0442526796497479,-0.0442281707822011,-0.0442036619146543,-0.0441546441795607,
-0.0440566087093734,-0.0438605377689989,-0.0431195460395093,-0.0422129105337495,
-0.0415351353283317,-0.0398096658242585,-0.0373324461243466,-0.0332891307954845,
-0.0254070365801755,-0.0151992737645416,-0.00246712194872464,0.00377091893863574,
0.0240422992970927,0.064119853096241,0.133396539450971,0.205795596167866,
0.226989045266928),.UNSPECIFIED.);
#544=B_SPLINE_CURVE_WITH_KNOTS('',3,(#16595,#16596,#16597,#16598,#16599,
#16600,#16601),.UNSPECIFIED.,.F.,.F.,(4,3,4),(0.0271515251943673,0.0836066639604027,
0.140061802726436),.UNSPECIFIED.);
#545=B_SPLINE_CURVE_WITH_KNOTS('',5,(#16603,#16604,#16605,#16606,#16607,
#16608),.UNSPECIFIED.,.F.,.F.,(6,6),(0.648016352593037,0.649373679600467),
 .UNSPECIFIED.);
#546=B_SPLINE_CURVE_WITH_KNOTS('',3,(#16610,#16611,#16612,#16613,#16614,
#16615,#16616,#16617,#16618,#16619,#16620,#16621,#16622,#16623),
 .UNSPECIFIED.,.F.,.F.,(4,2,2,2,2,2,4),(-0.300128297810014,-0.297956747127101,
-0.285522099406917,-0.254881013502635,-0.225735659999153,-0.194244463145828,
-0.1740900876335),.UNSPECIFIED.);
#547=B_SPLINE_CURVE_WITH_KNOTS('',3,(#16627,#16628,#16629,#16630,#16631,
#16632,#16633,#16634,#16635,#16636,#16637,#16638,#16639,#16640,#16641,#16642),
 .UNSPECIFIED.,.F.,.F.,(4,2,2,2,2,2,2,4),(-0.334017896162169,-0.307673650184263,
-0.27974268303834,-0.254256084112274,-0.232306890768372,-0.212897818769103,
-0.209691850469659,-0.208062418892068),.UNSPECIFIED.);
#548=B_SPLINE_CURVE_WITH_KNOTS('',5,(#16644,#16645,#16646,#16647,#16648,
#16649),.UNSPECIFIED.,.F.,.F.,(6,6),(-0.649373679600467,-0.648016352593037),
 .UNSPECIFIED.);
#549=B_SPLINE_CURVE_WITH_KNOTS('',3,(#16747,#16748,#16749,#16750,#16751,
#16752,#16753,#16754,#16755,#16756,#16757,#16758,#16759,#16760,#16761,#16762,
#16763,#16764,#16765),.UNSPECIFIED.,.F.,.F.,(4,1,1,1,1,1,1,1,1,1,1,1,1,
1,1,1,4),(-2.75290571088706,-2.36172303637955,-2.16491278334792,-1.96810253031629,
-1.77129227728466,-1.67288715076885,-1.57448202425304,-1.44327518889862,
-1.3120683535442,-1.18086151818978,-1.11525810051257,-1.04965468283536,
-1.01685297399675,-0.918447847480937,-0.787241012126518,-0.393620506063259,
0.),.UNSPECIFIED.);
#550=B_SPLINE_CURVE_WITH_KNOTS('',3,(#16768,#16769,#16770,#16771,#16772,
#16773,#16774,#16775,#16776,#16777,#16778,#16779,#16780,#16781,#16782,#16783,
#16784,#16785,#16786,#16787,#16788,#16789,#16790,#16791,#16792,#16793,#16794,
#16795,#16796,#16797,#16798,#16799,#16800,#16801,#16802,#16803,#16804,#16805,
#16806,#16807,#16808,#16809,#16810,#16811,#16812,#16813,#16814,#16815,#16816,
#16817,#16818,#16819,#16820,#16821,#16822,#16823,#16824,#16825,#16826,#16827,
#16828,#16829,#16830,#16831,#16832,#16833,#16834,#16835,#16836,#16837,#16838,
#16839,#16840,#16841,#16842,#16843,#16844,#16845,#16846,#16847,#16848,#16849,
#16850,#16851,#16852,#16853,#16854,#16855,#16856,#16857,#16858,#16859,#16860,
#16861,#16862,#16863,#16864,#16865,#16866,#16867,#16868,#16869,#16870,#16871,
#16872,#16873,#16874,#16875,#16876,#16877,#16878,#16879,#16880,#16881,#16882,
#16883,#16884,#16885,#16886,#16887,#16888,#16889,#16890,#16891,#16892,#16893,
#16894,#16895,#16896,#16897,#16898,#16899,#16900,#16901,#16902,#16903,#16904,
#16905,#16906,#16907,#16908,#16909,#16910,#16911,#16912,#16913,#16914,#16915,
#16916,#16917,#16918,#16919,#16920,#16921,#16922,#16923,#16924,#16925,#16926,
#16927,#16928,#16929,#16930,#16931,#16932,#16933,#16934,#16935,#16936,#16937,
#16938,#16939),.UNSPECIFIED.,.F.,.F.,(4,3,3,3,3,3,3,3,3,3,3,3,3,3,3,3,3,
3,3,3,3,3,3,3,3,3,3,3,3,3,3,3,3,3,3,3,3,3,3,3,3,3,3,3,3,3,3,3,3,3,3,3,3,
3,3,3,3,4),(0.,0.124369445529287,0.240030100192546,0.341233173022898,0.386674939404266,
0.411251254648982,0.491051683172279,0.563259965633032,0.630860010468553,
0.694792605008278,0.755770367876227,0.786749499491396,0.817139299607178,
0.861736210910445,0.904274509743171,0.933198720069145,0.967921430487703,
1.00176688673899,1.03365991619405,1.04965468283536,1.07830325879074,1.1039428236405,
1.123230742087,1.14569030213385,1.16906027640734,1.18086151818978,1.21528836919337,
1.25037899156894,1.28678619044467,1.30975642476343,1.3319781812234,1.37090028685257,
1.41175418522684,1.44539431955843,1.4917123985274,1.53781361798719,1.57586142812643,
1.62639986626241,1.66167935614305,1.68488494942284,1.71866494451513,1.75106115070037,
1.77418615895868,1.83844826443971,1.89630279494469,1.94999284166332,1.99684076151575,
2.05216246141503,2.10981892955224,2.1576446865864,2.20199668451076,2.28010760411423,
2.35258768188503,2.41850715945014,2.51795162746106,2.62227620558227,2.73424605476883,
2.75534354244281),.UNSPECIFIED.);
#551=B_SPLINE_CURVE_WITH_KNOTS('',3,(#16972,#16973,#16974,#16975,#16976),
 .UNSPECIFIED.,.F.,.F.,(4,1,4),(0.,0.0833626696026172,0.166725339205234),
 .UNSPECIFIED.);
#552=B_SPLINE_CURVE_WITH_KNOTS('',3,(#17001,#17002,#17003,#17004),
 .UNSPECIFIED.,.F.,.F.,(4,4),(-0.164730944371734,0.),.UNSPECIFIED.);
#553=B_SPLINE_CURVE_WITH_KNOTS('',3,(#17007,#17008,#17009,#17010),
 .UNSPECIFIED.,.F.,.F.,(4,4),(0.,0.164730944371734),.UNSPECIFIED.);
#554=B_SPLINE_CURVE_WITH_KNOTS('',3,(#17034,#17035,#17036,#17037),
 .UNSPECIFIED.,.F.,.F.,(4,4),(-0.0505768769923026,0.),.UNSPECIFIED.);
#555=B_SPLINE_CURVE_WITH_KNOTS('',3,(#17038,#17039,#17040,#17041),
 .UNSPECIFIED.,.F.,.F.,(4,4),(0.,0.0505769320975467),.UNSPECIFIED.);
#556=B_SPLINE_CURVE_WITH_KNOTS('',3,(#17062,#17063,#17064,#17065),
 .UNSPECIFIED.,.F.,.F.,(4,4),(-0.075415368178403,0.),.UNSPECIFIED.);
#557=B_SPLINE_CURVE_WITH_KNOTS('',3,(#17066,#17067,#17068,#17069),
 .UNSPECIFIED.,.F.,.F.,(4,4),(0.,0.075415368178403),.UNSPECIFIED.);
#558=B_SPLINE_CURVE_WITH_KNOTS('',3,(#17147,#17148,#17149,#17150),
 .UNSPECIFIED.,.F.,.F.,(4,4),(-0.499612937204198,-0.0795665830105256),
 .UNSPECIFIED.);
#559=B_SPLINE_CURVE_WITH_KNOTS('',5,(#17151,#17152,#17153,#17154,#17155,
#17156,#17157,#17158,#17159,#17160,#17161,#17162,#17163,#17164,#17165,#17166,
#17167,#17168,#17169,#17170,#17171,#17172,#17173,#17174),.UNSPECIFIED.,
 .F.,.F.,(6,1,1,1,1,1,1,1,1,1,1,1,1,1,1,1,1,1,1,6),(-0.648016352593037,
-0.648,-0.644,-0.64,-0.636,-0.632,-0.628,-0.624,-0.62,-0.616,-0.612,-0.608,
-0.604,-0.6,-0.596,-0.592,-0.588,-0.584,-0.58,-0.578475706653789),
 .UNSPECIFIED.);
#560=B_SPLINE_CURVE_WITH_KNOTS('',3,(#17192,#17193,#17194,#17195),
 .UNSPECIFIED.,.F.,.F.,(4,4),(0.0795665875934902,0.50017173665434),
 .UNSPECIFIED.);
#561=B_SPLINE_CURVE_WITH_KNOTS('',3,(#17198,#17199,#17200,#17201,#17202,
#17203),.UNSPECIFIED.,.F.,.F.,(4,2,4),(-0.0146609285082182,-0.00733041182656413,
0.),.UNSPECIFIED.);
#562=B_SPLINE_CURVE_WITH_KNOTS('',3,(#17221,#17222,#17223,#17224),
 .UNSPECIFIED.,.F.,.F.,(4,4),(0.120092046373885,0.541502145499565),
 .UNSPECIFIED.);
#563=B_SPLINE_CURVE_WITH_KNOTS('',3,(#17225,#17226,#17227,#17228,#17229,
#17230,#17231),.UNSPECIFIED.,.F.,.F.,(4,3,4),(0.,0.0172799395456661,0.0241280202161043),
 .UNSPECIFIED.);
#564=B_SPLINE_CURVE_WITH_KNOTS('',3,(#17769,#17770,#17771,#17772,#17773,
#17774,#17775,#17776,#17777,#17778),.UNSPECIFIED.,.F.,.F.,(4,2,2,2,4),(-0.100432637091733,
-0.0783128365433848,-0.0562142474116246,-0.0304582357928518,0.),
 .UNSPECIFIED.);
#565=B_SPLINE_CURVE_WITH_KNOTS('',3,(#18305,#18306,#18307,#18308),
 .UNSPECIFIED.,.F.,.F.,(4,4),(0.302038178795817,0.512484404778385),
 .UNSPECIFIED.);
#566=B_SPLINE_CURVE_WITH_KNOTS('',3,(#18309,#18310,#18311,#18312,#18313,
#18314),.UNSPECIFIED.,.F.,.F.,(4,2,4),(-0.531120307157959,-0.238218417429911,
-9.99999644757388E-7),.UNSPECIFIED.);
#567=B_SPLINE_CURVE_WITH_KNOTS('',3,(#18335,#18336,#18337,#18338),
 .UNSPECIFIED.,.F.,.F.,(4,4),(0.214918350132049,0.48911828449592),
 .UNSPECIFIED.);
#568=B_SPLINE_CURVE_WITH_KNOTS('',3,(#18342,#18343,#18344,#18345),
 .UNSPECIFIED.,.F.,.F.,(4,4),(-0.48911828449592,-0.216907151819261),
 .UNSPECIFIED.);
#569=B_SPLINE_CURVE_WITH_KNOTS('',3,(#18346,#18347,#18348,#18349),
 .UNSPECIFIED.,.F.,.F.,(4,4),(-0.00307307886366898,0.),.UNSPECIFIED.);
#570=B_SPLINE_CURVE_WITH_KNOTS('',3,(#18369,#18370,#18371,#18372),
 .UNSPECIFIED.,.F.,.F.,(4,4),(-0.197269104818139,0.),.UNSPECIFIED.);
#571=B_SPLINE_CURVE_WITH_KNOTS('',3,(#18373,#18374,#18375,#18376),
 .UNSPECIFIED.,.F.,.F.,(4,4),(0.,0.197269104818139),.UNSPECIFIED.);
#572=B_SPLINE_CURVE_WITH_KNOTS('',3,(#18394,#18395,#18396,#18397,#18398,
#18399,#18400,#18401,#18402,#18403),.UNSPECIFIED.,.F.,.F.,(4,3,3,4),(-0.221056240648656,
-0.141998498310432,-0.0700174415183823,-7.01203975429252E-6),
 .UNSPECIFIED.);
#573=B_SPLINE_CURVE_WITH_KNOTS('',3,(#18404,#18405,#18406,#18407),
 .UNSPECIFIED.,.F.,.F.,(4,4),(-6.0267045889705E-5,0.216046193075007),
 .UNSPECIFIED.);
#574=B_SPLINE_CURVE_WITH_KNOTS('',3,(#18433,#18434,#18435,#18436,#18437,
#18438),.UNSPECIFIED.,.F.,.F.,(4,2,4),(0.,0.471468502883735,0.473994966708672),
 .UNSPECIFIED.);
#575=B_SPLINE_CURVE_WITH_KNOTS('',3,(#18440,#18441,#18442,#18443,#18444,
#18445),.UNSPECIFIED.,.F.,.F.,(4,2,4),(-0.473994966708672,-0.471468502883735,
-0.468943296379571),.UNSPECIFIED.);
#576=B_SPLINE_CURVE_WITH_KNOTS('',3,(#18447,#18448,#18449,#18450),
 .UNSPECIFIED.,.F.,.F.,(4,4),(-0.468943296379571,0.),.UNSPECIFIED.);
#577=B_SPLINE_CURVE_WITH_KNOTS('',3,(#18468,#18469,#18470,#18471),
 .UNSPECIFIED.,.F.,.F.,(4,4),(-0.0666641938434966,-1.89854339553983E-15),
 .UNSPECIFIED.);
#578=B_SPLINE_CURVE_WITH_KNOTS('',3,(#18472,#18473,#18474,#18475),
 .UNSPECIFIED.,.F.,.F.,(4,4),(1.89854339553983E-15,0.0666641979607186),
 .UNSPECIFIED.);
#579=B_SPLINE_CURVE_WITH_KNOTS('',3,(#18493,#18494,#18495,#18496,#18497,
#18498),.UNSPECIFIED.,.F.,.F.,(4,2,4),(-0.124627466599506,-0.0741353398935927,
-0.00200197401216558),.UNSPECIFIED.);
#580=B_SPLINE_CURVE_WITH_KNOTS('',3,(#18500,#18501,#18502,#18503,#18504,
#18505),.UNSPECIFIED.,.F.,.F.,(4,2,4),(0.,0.0142795390469111,0.0283526878042237),
 .UNSPECIFIED.);
#581=B_SPLINE_CURVE_WITH_KNOTS('',3,(#18572,#18573,#18574,#18575,#18576,
#18577,#18578,#18579,#18580,#18581,#18582,#18583,#18584,#18585,#18586,#18587,
#18588,#18589,#18590,#18591,#18592,#18593,#18594,#18595,#18596),
 .UNSPECIFIED.,.F.,.F.,(4,3,3,3,3,3,3,3,4),(-0.328233327143732,-0.31988827792317,
-0.309570168667151,-0.283899379158957,-0.217011923344775,-0.143922571576324,
-0.117316316451159,-0.0546021126575079,-0.0454417463122694),
 .UNSPECIFIED.);
#582=B_SPLINE_CURVE_WITH_KNOTS('',3,(#18598,#18599,#18600,#18601,#18602,
#18603),.UNSPECIFIED.,.F.,.F.,(4,2,4),(-0.0454927189511385,-0.0227385236174852,
0.),.UNSPECIFIED.);
#583=B_SPLINE_CURVE_WITH_KNOTS('',3,(#18605,#18606,#18607,#18608,#18609,
#18610,#18611,#18612,#18613,#18614,#18615,#18616,#18617,#18618,#18619,#18620,
#18621,#18622,#18623),.UNSPECIFIED.,.F.,.F.,(4,3,3,3,3,3,4),(-0.859256670515544,
-0.689904013970006,-0.517379897379589,-0.342422169251531,-0.159325101934034,
0.,0.00551932282830541),.UNSPECIFIED.);
#584=B_SPLINE_CURVE_WITH_KNOTS('',3,(#18624,#18625,#18626,#18627,#18628,
#18629,#18630,#18631,#18632,#18633,#18634,#18635,#18636,#18637,#18638,#18639,
#18640,#18641,#18642,#18643,#18644,#18645,#18646,#18647,#18648,#18649,#18650,
#18651),.UNSPECIFIED.,.F.,.F.,(4,3,3,3,3,3,3,3,3,4),(0.494993241232899,
0.496085380942586,0.497177520652273,0.49806747763899,0.499361800071647,
0.503730358910395,0.512467476587892,0.612356912997924,0.702921203547389,
0.782344701900257),.UNSPECIFIED.);
#585=B_SPLINE_CURVE_WITH_KNOTS('',3,(#18676,#18677,#18678,#18679),
 .UNSPECIFIED.,.F.,.F.,(4,4),(-0.3237356772338,0.),.UNSPECIFIED.);
#586=B_SPLINE_CURVE_WITH_KNOTS('',3,(#18682,#18683,#18684,#18685,#18686,
#18687,#18688,#18689,#18690,#18691),.UNSPECIFIED.,.F.,.F.,(4,3,3,4),(0.,
0.140915294581484,0.27533410968208,0.3237356772338),.UNSPECIFIED.);
#587=B_SPLINE_CURVE_WITH_KNOTS('',3,(#18712,#18713,#18714,#18715),
 .UNSPECIFIED.,.F.,.F.,(4,4),(-0.105411802493843,-2.2267163093265E-6),
 .UNSPECIFIED.);
#588=B_SPLINE_CURVE_WITH_KNOTS('',3,(#18718,#18719,#18720,#18721),
 .UNSPECIFIED.,.F.,.F.,(4,4),(0.,0.105411804182902),.UNSPECIFIED.);
#589=B_SPLINE_CURVE_WITH_KNOTS('',3,(#18790,#18791,#18792,#18793,#18794,
#18795,#18796,#18797,#18798,#18799),.UNSPECIFIED.,.F.,.F.,(4,2,2,2,4),(-0.092999678223845,
-0.054767181661459,-0.027983845416742,-8.71951452430242E-8,0.000452064458421415),
 .UNSPECIFIED.);
#590=B_SPLINE_CURVE_WITH_KNOTS('',3,(#18800,#18801,#18802,#18803,#18804,
#18805,#18806),.UNSPECIFIED.,.F.,.F.,(4,1,1,1,4),(9.50220145082506E-8,0.0336059064221182,
0.0672118128442549,0.11201968807377,0.156827563303286),.UNSPECIFIED.);
#591=B_SPLINE_CURVE_WITH_KNOTS('',3,(#18835,#18836,#18837,#18838,#18839),
 .UNSPECIFIED.,.F.,.F.,(4,1,4),(-0.172872079671176,-0.0864360398355901,
-4.07518504807266E-15),.UNSPECIFIED.);
#592=B_SPLINE_CURVE_WITH_KNOTS('',3,(#18840,#18841,#18842,#18843,#18844),
 .UNSPECIFIED.,.F.,.F.,(4,1,4),(4.10788875408049E-5,0.0864360398355901,
0.172872079671176),.UNSPECIFIED.);
#593=B_SPLINE_CURVE_WITH_KNOTS('',3,(#18867,#18868,#18869,#18870,#18871,
#18872,#18873,#18874,#18875,#18876),.UNSPECIFIED.,.F.,.F.,(4,3,3,4),(-0.082403918867489,
-0.0430009988442003,-0.0288947220991941,-3.17406135744279E-5),
 .UNSPECIFIED.);
#594=B_SPLINE_CURVE_WITH_KNOTS('',3,(#18877,#18878,#18879,#18880),
 .UNSPECIFIED.,.F.,.F.,(4,4),(0.00704588444375797,0.110567549348147),
 .UNSPECIFIED.);
#595=B_SPLINE_CURVE_WITH_KNOTS('',3,(#18882,#18883,#18884,#18885),
 .UNSPECIFIED.,.F.,.F.,(4,4),(-0.110567549348147,-0.0322193451720294),
 .UNSPECIFIED.);
#596=B_SPLINE_CURVE_WITH_KNOTS('',3,(#18886,#18887,#18888,#18889,#18890,
#18891),.UNSPECIFIED.,.F.,.F.,(4,2,4),(3.38858789424881E-5,0.0291642218697387,
0.058248786360198),.UNSPECIFIED.);
#597=B_SPLINE_CURVE_WITH_KNOTS('',3,(#19430,#19431,#19432,#19433),
 .UNSPECIFIED.,.F.,.F.,(4,4),(0.365433236291192,0.388387607255886),
 .UNSPECIFIED.);
#598=B_SPLINE_CURVE_WITH_KNOTS('',3,(#19955,#19956,#19957,#19958,#19959,
#19960,#19961,#19962,#19963,#19964,#19965,#19966,#19967,#19968,#19969,#19970,
#19971,#19972,#19973,#19974,#19975,#19976,#19977,#19978,#19979,#19980,#19981,
#19982,#19983,#19984,#19985,#19986,#19987,#19988),.UNSPECIFIED.,.F.,.F.,
(4,1,1,1,1,1,1,1,1,1,1,1,1,1,1,1,1,1,1,1,1,1,1,1,1,1,1,1,1,1,1,4),(0.,0.438300757907035,
0.876601515814069,1.3149022737211,1.75320303162814,2.19150378953517,2.62980454744221,
3.50640606325628,4.01775694748115,4.09080707379899,4.6752080843417,4.96740858961306,
5.11350884224874,5.25960909488442,5.55180960015577,5.84401010542713,6.42841111596984,
7.01281212651256,7.30501263178391,7.59721313705527,8.18161414759798,8.76601515814069,
9.05821566341205,9.35041616868341,9.64261667395476,9.93481717922612,10.5192181897688,
10.6287933792456,10.9575189476759,11.3958197055829,11.8341204634899,12.272421221397),
 .UNSPECIFIED.);
#599=B_SPLINE_CURVE_WITH_KNOTS('',3,(#19989,#19990,#19991,#19992,#19993),
 .UNSPECIFIED.,.F.,.F.,(4,1,4),(-0.792076380669774,-0.473360640006854,-0.0476472117508909),
 .UNSPECIFIED.);
#600=B_SPLINE_CURVE_WITH_KNOTS('',3,(#20166,#20167,#20168,#20169,#20170,
#20171),.UNSPECIFIED.,.F.,.F.,(4,2,4),(-0.0417560322026806,-0.0208857221654478,
0.),.UNSPECIFIED.);
#601=B_SPLINE_CURVE_WITH_KNOTS('',3,(#20202,#20203,#20204,#20205),
 .UNSPECIFIED.,.F.,.F.,(4,4),(-0.164738445253465,0.),.UNSPECIFIED.);
#602=B_SPLINE_CURVE_WITH_KNOTS('',3,(#20208,#20209,#20210,#20211),
 .UNSPECIFIED.,.F.,.F.,(4,4),(0.,0.164738445253465),.UNSPECIFIED.);
#603=B_SPLINE_CURVE_WITH_KNOTS('',3,(#20233,#20234,#20235,#20236),
 .UNSPECIFIED.,.F.,.F.,(4,4),(-0.0754181362626584,0.),.UNSPECIFIED.);
#604=B_SPLINE_CURVE_WITH_KNOTS('',3,(#20239,#20240,#20241,#20242),
 .UNSPECIFIED.,.F.,.F.,(4,4),(0.,0.0754181362626584),.UNSPECIFIED.);
#605=B_SPLINE_CURVE_WITH_KNOTS('',3,(#20266,#20267,#20268,#20269),
 .UNSPECIFIED.,.F.,.F.,(4,4),(-0.0505696713863416,0.),.UNSPECIFIED.);
#606=B_SPLINE_CURVE_WITH_KNOTS('',3,(#20270,#20271,#20272,#20273),
 .UNSPECIFIED.,.F.,.F.,(4,4),(0.,0.0505696713863416),.UNSPECIFIED.);
#607=B_SPLINE_CURVE_WITH_KNOTS('',3,(#20299,#20300,#20301,#20302,#20303),
 .UNSPECIFIED.,.F.,.F.,(4,1,4),(-0.167546057491724,-0.0837730396707311,
0.),.UNSPECIFIED.);
#608=B_SPLINE_CURVE_WITH_KNOTS('',3,(#20304,#20305,#20306,#20307,#20308),
 .UNSPECIFIED.,.F.,.F.,(4,1,4),(0.,0.0837730396707311,0.167546079341462),
 .UNSPECIFIED.);
#609=B_SPLINE_CURVE_WITH_KNOTS('',3,(#20336,#20337,#20338,#20339,#20340,
#20341,#20342,#20343,#20344,#20345,#20346,#20347,#20348,#20349,#20350,#20351,
#20352,#20353,#20354,#20355,#20356,#20357,#20358,#20359,#20360,#20361,#20362,
#20363,#20364,#20365,#20366,#20367,#20368,#20369,#20370,#20371,#20372,#20373,
#20374,#20375),.UNSPECIFIED.,.F.,.F.,(4,2,2,2,2,2,2,2,2,2,2,2,2,2,2,2,2,
2,2,4),(-0.143338394766602,-0.143331321978003,-0.143321921751135,-0.143310773562853,
-0.143294817451188,-0.143273441019733,-0.143239462197249,-0.143157800746622,
-0.142979467545553,-0.14264046123677,-0.141964852019619,-0.140613536202353,
-0.137910059169606,-0.132499723273395,-0.121667756807207,-0.0999966720102727,
-0.0636768389896232,-0.0323614893999653,-0.0161529766319166,0.),
 .UNSPECIFIED.);
#610=B_SPLINE_CURVE_WITH_KNOTS('',3,(#20376,#20377,#20378,#20379,#20380),
 .UNSPECIFIED.,.F.,.F.,(4,1,4),(-0.0971295855432269,-0.0737466502954258,
-0.0503637150476246),.UNSPECIFIED.);
#611=B_SPLINE_CURVE_WITH_KNOTS('',3,(#20433,#20434,#20435,#20436),
 .UNSPECIFIED.,.F.,.F.,(4,4),(0.0253342885542915,0.430969252801444),
 .UNSPECIFIED.);
#612=B_SPLINE_CURVE_WITH_KNOTS('',5,(#20438,#20439,#20440,#20441,#20442,
#20443,#20444),.UNSPECIFIED.,.F.,.F.,(6,1,6),(-0.420429130898424,-0.42,
-0.419832797309863),.UNSPECIFIED.);
#613=B_SPLINE_CURVE_WITH_KNOTS('',3,(#20564,#20565,#20566,#20567,#20568,
#20569,#20570,#20571,#20572,#20573,#20574,#20575,#20576,#20577,#20578,#20579,
#20580,#20581,#20582,#20583),.UNSPECIFIED.,.F.,.F.,(4,1,1,1,1,1,1,1,1,1,
1,1,1,1,1,1,1,4),(-2.73841348611599,-2.36517143630499,-1.97097619692083,
-1.77387857722874,-1.6753297673827,-1.62605536245968,-1.57678095753666,
-1.47823214769062,-1.37968333784458,-1.1825857181525,-1.08403690830645,
-0.985488098460413,-0.886939288614372,-0.78839047876833,-0.689841668922289,
-0.394195239384165,-0.197097619692083,0.),.UNSPECIFIED.);
#614=B_SPLINE_CURVE_WITH_KNOTS('',3,(#20586,#20587,#20588,#20589,#20590,
#20591,#20592,#20593,#20594,#20595,#20596,#20597,#20598,#20599,#20600,#20601,
#20602,#20603,#20604,#20605,#20606,#20607,#20608,#20609,#20610,#20611,#20612,
#20613,#20614,#20615,#20616,#20617,#20618,#20619,#20620,#20621,#20622,#20623,
#20624,#20625,#20626,#20627,#20628,#20629,#20630,#20631,#20632,#20633,#20634,
#20635,#20636,#20637,#20638,#20639,#20640,#20641,#20642,#20643,#20644,#20645,
#20646,#20647,#20648,#20649,#20650,#20651,#20652,#20653,#20654,#20655,#20656,
#20657,#20658,#20659,#20660,#20661,#20662,#20663,#20664,#20665,#20666,#20667,
#20668,#20669,#20670,#20671,#20672,#20673,#20674,#20675,#20676,#20677,#20678,
#20679,#20680,#20681,#20682,#20683,#20684,#20685,#20686,#20687,#20688,#20689,
#20690,#20691,#20692,#20693,#20694,#20695,#20696,#20697,#20698,#20699,#20700,
#20701,#20702,#20703,#20704,#20705,#20706,#20707,#20708,#20709,#20710,#20711,
#20712,#20713,#20714,#20715,#20716,#20717,#20718,#20719,#20720,#20721,#20722,
#20723,#20724,#20725,#20726,#20727,#20728,#20729,#20730,#20731,#20732,#20733,
#20734,#20735,#20736,#20737,#20738,#20739,#20740,#20741,#20742,#20743,#20744,
#20745,#20746,#20747,#20748,#20749,#20750,#20751,#20752,#20753,#20754,#20755,
#20756,#20757),.UNSPECIFIED.,.F.,.F.,(4,3,3,3,3,3,3,3,3,3,3,3,3,3,3,3,3,
3,3,3,3,3,3,3,3,3,3,3,3,3,3,3,3,3,3,3,3,3,3,3,3,3,3,3,3,3,3,3,3,3,3,3,3,
3,3,3,3,4),(0.,0.11697816486161,0.199552805824971,0.29207922439174,0.379904425280162,
0.414491531816278,0.487768880062305,0.558756311175645,0.627525385066692,
0.674261606492045,0.716485480031171,0.771587302682763,0.818558905154333,
0.86735829475901,0.896793608968199,0.946203496056523,0.978061410992569,
1.00230666564603,1.0367677818061,1.06943217583647,1.09199787333064,1.14810717859007,
1.17935190443171,1.20496993722993,1.24928688584476,1.29365824383217,1.3394616323277,
1.37582359152284,1.40705262279406,1.44237449278729,1.47192259312313,1.49540819182661,
1.54265747358181,1.56746644655096,1.58208267476035,1.6042054561175,1.62520599234938,
1.65028459177019,1.67022579977173,1.69055676674289,1.72445360136606,1.75960930850324,
1.78944132262637,1.82876432801193,1.86987036112636,1.913227937659,1.95926954326023,
2.00171332991122,2.06665546647158,2.13507849354725,2.20786196528303,2.28965040690062,
2.34836494049919,2.38778597604317,2.49002389242042,2.59973840902036,2.72326481917138,
2.75936667568916),.UNSPECIFIED.);
#615=B_SPLINE_CURVE_WITH_KNOTS('',3,(#20766,#20767,#20768,#20769,#20770,
#20771,#20772,#20773,#20774,#20775),.UNSPECIFIED.,.F.,.F.,(4,2,2,2,4),(-0.000388876996940957,
4.56612658924702E-11,0.0575621541740994,0.0822985038873295,0.0906504752664335),
 .UNSPECIFIED.);
#616=B_SPLINE_CURVE_WITH_KNOTS('',3,(#20777,#20778,#20779,#20780),
 .UNSPECIFIED.,.F.,.F.,(4,4),(0.,0.173814018518568),.UNSPECIFIED.);
#617=B_SPLINE_CURVE_WITH_KNOTS('',3,(#20781,#20782,#20783,#20784),
 .UNSPECIFIED.,.F.,.F.,(4,4),(-0.0459140586584383,0.),.UNSPECIFIED.);
#618=B_SPLINE_CURVE_WITH_KNOTS('',3,(#20806,#20807,#20808,#20809),
 .UNSPECIFIED.,.F.,.F.,(4,4),(-0.107690415926182,0.),.UNSPECIFIED.);
#619=B_SPLINE_CURVE_WITH_KNOTS('',3,(#20812,#20813,#20814,#20815),
 .UNSPECIFIED.,.F.,.F.,(4,4),(0.,0.304037814733278),.UNSPECIFIED.);
#620=B_SPLINE_CURVE_WITH_KNOTS('',3,(#20924,#20925,#20926,#20927,#20928,
#20929,#20930,#20931,#20932,#20933,#20934,#20935,#20936,#20937,#20938,#20939,
#20940,#20941,#20942,#20943,#20944),.UNSPECIFIED.,.F.,.F.,(4,1,1,1,1,1,
1,1,1,1,1,1,1,1,1,1,1,1,4),(-8.30491541813876,-8.15661335710056,-8.00831129606237,
-7.86000923502418,-7.71170717398599,-7.4151030519096,-7.11849892983322,
-6.52529068568045,-5.93208244152768,-4.74566595322215,-2.37283297661107,
-1.7796247324583,-1.18641648830554,-0.889812366229152,-0.593208244152768,
-0.444906183114576,-0.296604122076384,-0.148302061038192,0.),
 .UNSPECIFIED.);
#621=B_SPLINE_CURVE_WITH_KNOTS('',3,(#20966,#20967,#20968,#20969),
 .UNSPECIFIED.,.F.,.F.,(4,4),(-0.0801298062965183,0.),.UNSPECIFIED.);
#622=B_SPLINE_CURVE_WITH_KNOTS('',3,(#20970,#20971,#20972,#20973),
 .UNSPECIFIED.,.F.,.F.,(4,4),(0.,0.0801298062965183),.UNSPECIFIED.);
#623=B_SPLINE_CURVE_WITH_KNOTS('',3,(#21015,#21016,#21017,#21018),
 .UNSPECIFIED.,.F.,.F.,(4,4),(-0.080129806296636,-2.65444323739948E-13),
 .UNSPECIFIED.);
#624=B_SPLINE_CURVE_WITH_KNOTS('',3,(#21022,#21023,#21024,#21025,#21026,
#21027),.UNSPECIFIED.,.F.,.F.,(4,1,1,4),(-0.344667552668405,-0.264773640517305,
-0.184879728366205,-0.0650388601395548),.UNSPECIFIED.);
#625=B_SPLINE_CURVE_WITH_KNOTS('',3,(#21036,#21037,#21038,#21039),
 .UNSPECIFIED.,.F.,.F.,(4,4),(-0.357185215222936,0.),.UNSPECIFIED.);
#626=B_SPLINE_CURVE_WITH_KNOTS('',3,(#21044,#21045,#21046,#21047,#21048),
 .UNSPECIFIED.,.F.,.F.,(4,1,4),(0.0124441963939058,0.048258887840249,0.0965121156546766),
 .UNSPECIFIED.);
#627=B_SPLINE_CURVE_WITH_KNOTS('',3,(#21087,#21088,#21089,#21090,#21091,
#21092,#21093,#21094),.UNSPECIFIED.,.F.,.F.,(4,2,2,4),(0.000388650349350716,
0.116108579564429,0.168099156279993,0.196635243830291),.UNSPECIFIED.);
#628=B_SPLINE_CURVE_WITH_KNOTS('',3,(#21098,#21099,#21100,#21101,#21102,
#21103,#21104,#21105,#21106,#21107,#21108,#21109,#21110,#21111),
 .UNSPECIFIED.,.F.,.F.,(4,2,2,2,2,2,4),(0.000179524113000012,0.0103957521563598,
0.0961675209313773,0.135083973905907,0.163219630081561,0.178069326504183,
0.19211441705983),.UNSPECIFIED.);
#629=B_SPLINE_CURVE_WITH_KNOTS('',3,(#21115,#21116,#21117,#21118),
 .UNSPECIFIED.,.F.,.F.,(4,4),(-0.921184518536775,-0.83453843347903),
 .UNSPECIFIED.);
#630=B_SPLINE_CURVE_WITH_KNOTS('',3,(#21120,#21121,#21122,#21123,#21124,
#21125),.UNSPECIFIED.,.F.,.F.,(4,2,4),(-0.150027473993582,-0.0719000872483259,
-1.60162876488653E-5),.UNSPECIFIED.);
#631=B_SPLINE_CURVE_WITH_KNOTS('',3,(#21127,#21128,#21129,#21130,#21131,
#21132,#21133,#21134),.UNSPECIFIED.,.F.,.F.,(4,2,2,4),(-0.159862307608192,
-0.0802383050665597,0.,0.000515045900834663),.UNSPECIFIED.);
#632=B_SPLINE_CURVE_WITH_KNOTS('',3,(#21138,#21139,#21140,#21141,#21142,
#21143,#21144,#21145),.UNSPECIFIED.,.F.,.F.,(4,2,2,4),(0.000127650722345724,
0.0504964849387841,0.100554030953333,0.101083886401504),.UNSPECIFIED.);
#633=B_SPLINE_CURVE_WITH_KNOTS('',3,(#21147,#21148,#21149,#21150,#21151,
#21152,#21153,#21154,#21155,#21156,#21157,#21158,#21159,#21160),
 .UNSPECIFIED.,.F.,.F.,(4,2,2,2,2,2,4),(0.,0.0370101874890961,0.0864161496254977,
0.117374893296465,0.141975914212591,0.160694465086184,0.18074188497048),
 .UNSPECIFIED.);
#634=B_SPLINE_CURVE_WITH_KNOTS('',3,(#21164,#21165,#21166,#21167,#21168),
 .UNSPECIFIED.,.F.,.F.,(4,1,4),(0.,0.0482654156519333,0.0840891532006709),
 .UNSPECIFIED.);
#635=B_SPLINE_CURVE_WITH_KNOTS('',3,(#21172,#21173,#21174,#21175),
 .UNSPECIFIED.,.F.,.F.,(4,4),(-0.0801298062968181,-2.63411853293822E-13),
 .UNSPECIFIED.);
#636=B_SPLINE_CURVE_WITH_KNOTS('',3,(#21180,#21181,#21182,#21183,#21184),
 .UNSPECIFIED.,.F.,.F.,(4,1,4),(-0.121804337225533,-0.0522018588109426,
0.),.UNSPECIFIED.);
#637=B_SPLINE_CURVE_WITH_KNOTS('',3,(#21185,#21186,#21187,#21188,#21189,
#21190),.UNSPECIFIED.,.F.,.F.,(4,2,4),(-0.0372063908700252,-0.0185630077537129,
0.),.UNSPECIFIED.);
#638=B_SPLINE_CURVE_WITH_KNOTS('',3,(#21244,#21245,#21246,#21247),
 .UNSPECIFIED.,.F.,.F.,(4,4),(0.,0.35717455535325),.UNSPECIFIED.);
#639=B_SPLINE_CURVE_WITH_KNOTS('',3,(#21281,#21282,#21283,#21284,#21285,
#21286),.UNSPECIFIED.,.F.,.F.,(4,1,1,4),(0.0650388601395548,0.184879728366205,
0.264773640517305,0.344667552668405),.UNSPECIFIED.);
#640=B_SPLINE_CURVE_WITH_KNOTS('',3,(#21852,#21853,#21854,#21855,#21856),
 .UNSPECIFIED.,.F.,.F.,(4,1,4),(0.122333686396133,0.336302079828547,0.52623217118239),
 .UNSPECIFIED.);
#641=B_SPLINE_CURVE_WITH_KNOTS('',3,(#21891,#21892,#21893,#21894,#21895,
#21896,#21897,#21898,#21899,#21900,#21901,#21902,#21903,#21904,#21905,#21906,
#21907,#21908,#21909,#21910,#21911,#21912,#21913,#21914,#21915),
 .UNSPECIFIED.,.F.,.F.,(4,3,3,3,3,3,3,3,4),(0.0476472117481897,0.176707628536091,
0.309197145860186,0.421180594715224,0.473360639981091,0.629106032564461,
0.80736131459052,0.81926637292792,1.03517553998266),.UNSPECIFIED.);
#642=B_SPLINE_CURVE_WITH_KNOTS('',3,(#21916,#21917,#21918,#21919),
 .UNSPECIFIED.,.F.,.F.,(4,4),(1.03517572369524,1.04062713634001),
 .UNSPECIFIED.);
#643=B_SPLINE_CURVE_WITH_KNOTS('',3,(#21979,#21980,#21981,#21982),
 .UNSPECIFIED.,.F.,.F.,(4,4),(-0.254963272600067,-0.19533758964745),
 .UNSPECIFIED.);
#644=B_SPLINE_CURVE_WITH_KNOTS('',3,(#22003,#22004,#22005,#22006),
 .UNSPECIFIED.,.F.,.F.,(4,4),(2.63411853293822E-13,0.0801298062968181),
 .UNSPECIFIED.);
#645=B_SPLINE_CURVE_WITH_KNOTS('',3,(#22021,#22022,#22023,#22024,#22025,
#22026),.UNSPECIFIED.,.F.,.F.,(4,2,4),(-0.0739729607057787,0.,0.00065196825529525),
 .UNSPECIFIED.);
#646=B_SPLINE_CURVE_WITH_KNOTS('',3,(#22030,#22031,#22032,#22033,#22034,
#22035,#22036,#22037,#22038,#22039,#22040,#22041,#22042),.UNSPECIFIED.,
 .F.,.F.,(4,3,3,3,4),(-0.0741141580594659,-0.0733119809727613,-0.0421649270605065,
-0.0161079664769414,-3.24706403037789E-5),.UNSPECIFIED.);
#647=B_SPLINE_CURVE_WITH_KNOTS('',1,(#22043,#22044),.UNSPECIFIED.,.F.,.F.,
(2,2),(-0.0103667322106565,0.),.UNSPECIFIED.);
#648=B_SPLINE_CURVE_WITH_KNOTS('',3,(#22046,#22047,#22048,#22049,#22050,
#22051),.UNSPECIFIED.,.F.,.F.,(4,2,4),(-0.000271009268404639,-0.000152937970284206,
-1.02670240187253E-5),.UNSPECIFIED.);
#649=B_SPLINE_CURVE_WITH_KNOTS('',3,(#22084,#22085,#22086,#22087,#22088,
#22089,#22090,#22091,#22092,#22093,#22094,#22095,#22096,#22097,#22098,#22099),
 .UNSPECIFIED.,.F.,.F.,(4,3,3,3,3,4),(-0.170468208410896,-0.121851917489685,
-0.109877931374803,-0.0874114081347553,-0.0402533150305619,0.),
 .UNSPECIFIED.);
#650=B_SPLINE_CURVE_WITH_KNOTS('',3,(#22148,#22149,#22150,#22151,#22152,
#22153),.UNSPECIFIED.,.F.,.F.,(4,1,1,4),(-0.251165001188368,-0.179403572277406,
-0.107642143366443,0.),.UNSPECIFIED.);
#651=B_SPLINE_CURVE_WITH_KNOTS('',3,(#22175,#22176,#22177,#22178),
 .UNSPECIFIED.,.F.,.F.,(4,4),(0.00243784671109485,0.137031673359032),
 .UNSPECIFIED.);
#652=B_SPLINE_CURVE_WITH_KNOTS('',3,(#22308,#22309,#22310,#22311),
 .UNSPECIFIED.,.F.,.F.,(4,4),(0.,0.0029947073568665),.UNSPECIFIED.);
#653=B_SPLINE_CURVE_WITH_KNOTS('',3,(#22313,#22314,#22315,#22316,#22317,
#22318,#22319,#22320,#22321,#22322,#22323,#22324,#22325,#22326,#22327,#22328,
#22329,#22330,#22331,#22332,#22333,#22334,#22335,#22336,#22337,#22338,#22339,
#22340,#22341,#22342,#22343,#22344,#22345,#22346,#22347,#22348,#22349,#22350,
#22351,#22352,#22353,#22354,#22355,#22356,#22357,#22358,#22359,#22360,#22361,
#22362,#22363,#22364,#22365,#22366,#22367,#22368,#22369,#22370,#22371,#22372,
#22373,#22374,#22375,#22376,#22377,#22378,#22379,#22380,#22381,#22382,#22383,
#22384,#22385,#22386,#22387,#22388,#22389,#22390,#22391,#22392,#22393,#22394,
#22395,#22396,#22397,#22398,#22399,#22400,#22401,#22402,#22403,#22404,#22405,
#22406,#22407,#22408,#22409,#22410,#22411,#22412,#22413,#22414,#22415,#22416,
#22417,#22418,#22419,#22420,#22421,#22422,#22423,#22424,#22425,#22426,#22427,
#22428,#22429,#22430,#22431,#22432,#22433,#22434,#22435,#22436,#22437,#22438,
#22439,#22440,#22441,#22442,#22443,#22444,#22445,#22446,#22447,#22448,#22449,
#22450,#22451,#22452,#22453,#22454,#22455,#22456,#22457,#22458,#22459,#22460,
#22461,#22462,#22463,#22464,#22465,#22466,#22467,#22468,#22469,#22470,#22471,
#22472,#22473,#22474,#22475,#22476,#22477,#22478),.UNSPECIFIED.,.F.,.F.,
(4,3,3,3,3,3,3,3,3,3,3,3,3,3,3,3,3,3,3,3,3,3,3,3,3,3,3,3,3,3,3,3,3,3,3,
3,3,3,3,3,3,3,3,3,3,3,3,3,3,3,3,3,3,3,3,4),(0.150051581338353,0.256863936659208,
0.335221624046453,0.385884192471485,0.415095529930595,0.496109926387356,
0.569942607877855,0.638650952641705,0.705077795779496,0.769428800069232,
0.804505228482622,0.849643463003826,0.892080534823519,0.932340746449873,
0.971002669683063,0.990292699500749,1.02414419558244,1.05133428523039,1.07725069503007,
1.10382298151386,1.12328365106401,1.14494121098181,1.1667241512046,1.18428652869351,
1.20604733438692,1.24354147974281,1.28115827676027,1.31547262018988,1.33594212716517,
1.37354010313882,1.4132592349251,1.44718380388559,1.48803315339709,1.53384225960426,
1.57229437439947,1.60642722308793,1.66117380917141,1.68727241905653,1.72119555000744,
1.75379287447755,1.77871300744534,1.8485007475128,1.91500567133357,1.96808718769091,
2.00382424755494,2.05135460289845,2.08266994362526,2.15070750358199,2.21528666185066,
2.28827074173757,2.35567498677221,2.40419094803851,2.50311616375164,2.60679823955146,
2.71856348129842,2.76430993305103),.UNSPECIFIED.);
#654=B_SPLINE_CURVE_WITH_KNOTS('',3,(#22482,#22483,#22484,#22485,#22486,
#22487,#22488,#22489,#22490,#22491,#22492,#22493,#22494,#22495,#22496,#22497,
#22498,#22499,#22500,#22501),.UNSPECIFIED.,.F.,.F.,(4,1,1,1,1,1,1,1,1,1,
1,1,1,1,1,1,1,4),(-2.76430993305103,-2.37006408126403,-2.17294115537053,
-2.07437969242378,-1.97581822947703,-1.77869530358353,-1.68013384063678,
-1.58157237769003,-1.45015709376104,-1.31874180983204,-1.18732652590304,
-1.12161888393854,-1.05591124197404,-1.02305742099179,-0.990203600009539,
-0.79308067411604,-0.398834822329043,-0.00458897054204579),
 .UNSPECIFIED.);
#655=B_SPLINE_CURVE_WITH_KNOTS('',3,(#22519,#22520,#22521,#22522),
 .UNSPECIFIED.,.F.,.F.,(4,4),(0.7519797577463,0.919615460485724),
 .UNSPECIFIED.);
#656=B_SPLINE_CURVE_WITH_KNOTS('',3,(#22565,#22566,#22567,#22568),
 .UNSPECIFIED.,.F.,.F.,(4,4),(-0.419743206478425,-0.0797065098565302),
 .UNSPECIFIED.);
#657=B_SPLINE_CURVE_WITH_KNOTS('',3,(#22571,#22572,#22573,#22574),
 .UNSPECIFIED.,.F.,.F.,(4,4),(0.0797065098565302,0.419743206478425),
 .UNSPECIFIED.);
#658=B_SPLINE_CURVE_WITH_KNOTS('',3,(#22672,#22673,#22674,#22675),
 .UNSPECIFIED.,.F.,.F.,(4,4),(-0.166269642083837,0.),.UNSPECIFIED.);
#659=B_SPLINE_CURVE_WITH_KNOTS('',3,(#22699,#22700,#22701,#22702),
 .UNSPECIFIED.,.F.,.F.,(4,4),(0.,0.0459140586584383),.UNSPECIFIED.);
#660=B_SPLINE_CURVE_WITH_KNOTS('',3,(#22742,#22743,#22744,#22745),
 .UNSPECIFIED.,.F.,.F.,(4,4),(0.121211854500864,0.461940930144229),
 .UNSPECIFIED.);
#661=B_SPLINE_CURVE_WITH_KNOTS('',3,(#23900,#23901,#23902,#23903,#23904,
#23905),.UNSPECIFIED.,.F.,.F.,(4,1,1,4),(-454.450543714446,-453.451751310678,
-452.45295890691,-452.038622507886),.UNSPECIFIED.);
#662=B_SPLINE_CURVE_WITH_KNOTS('',3,(#23907,#23908,#23909,#23910,#23911,
#23912,#23913,#23914,#23915,#23916),.UNSPECIFIED.,.F.,.F.,(4,1,1,1,1,1,
1,4),(-452.038622507886,-451.454166503142,-450.455374099374,-449.456581695606,
-448.457789291838,-447.45899688807,-446.460204484302,-445.755437200706),
 .UNSPECIFIED.);
#663=B_SPLINE_CURVE_WITH_KNOTS('',3,(#23918,#23919,#23920,#23921,#23922,
#23923,#23924,#23925,#23926,#23927,#23928,#23929,#23930,#23931,#23932,#23933,
#23934,#23935,#23936,#23937,#23938,#23939,#23940,#23941,#23942,#23943,#23944,
#23945,#23946,#23947,#23948,#23949,#23950,#23951,#23952,#23953,#23954,#23955,
#23956,#23957,#23958,#23959,#23960,#23961,#23962,#23963,#23964,#23965,#23966,
#23967,#23968,#23969,#23970,#23971,#23972,#23973,#23974,#23975,#23976,#23977,
#23978,#23979,#23980,#23981,#23982,#23983,#23984,#23985,#23986,#23987,#23988,
#23989,#23990,#23991,#23992,#23993,#23994,#23995,#23996,#23997,#23998,#23999,
#24000,#24001,#24002,#24003,#24004,#24005,#24006,#24007,#24008,#24009,#24010,
#24011,#24012,#24013,#24014,#24015,#24016,#24017,#24018,#24019,#24020,#24021,
#24022,#24023,#24024,#24025,#24026,#24027,#24028,#24029,#24030,#24031,#24032,
#24033,#24034,#24035,#24036,#24037,#24038,#24039,#24040,#24041,#24042,#24043,
#24044,#24045,#24046,#24047,#24048,#24049,#24050),.UNSPECIFIED.,.F.,.F.,
(4,3,3,3,3,3,3,3,3,3,3,3,3,3,3,3,3,3,3,3,3,3,3,3,3,3,3,3,3,3,3,3,3,3,3,
3,3,3,3,3,3,3,3,3,4),(-445.755437031918,-445.563647569504,-445.461412080534,
-445.303982702834,-445.146842808848,-444.989871571425,-444.832819606925,
-444.675719587285,-444.51827995468,-444.462619676766,-444.305197863777,
-444.148065737253,-443.991102442813,-443.834058588833,-443.676966786957,
-443.519535409268,-443.463827272998,-443.306400089056,-443.149262491187,
-442.992293644092,-442.835244182094,-442.678146733064,-442.520709734799,
-442.46503486923,-442.307608665139,-442.150472048908,-441.993504181851,
-441.836455685854,-441.679359195915,-441.521923131783,-441.466242465462,
-441.308817158692,-441.151681465853,-440.994714545015,-440.837667018058,
-440.680571511596,-440.523136437804,-440.467450061694,-440.31012564541,
-440.153090641361,-439.996223862719,-439.839276201223,-439.682279418494,
-439.524944479556,-439.472251893657),.UNSPECIFIED.);
#664=B_SPLINE_CURVE_WITH_KNOTS('',3,(#24052,#24053,#24054,#24055,#24056,
#24057,#24058,#24059,#24060,#24061,#24062,#24063,#24064,#24065,#24066,#24067,
#24068,#24069,#24070,#24071,#24072,#24073,#24074,#24075,#24076,#24077,#24078,
#24079,#24080,#24081,#24082,#24083,#24084,#24085,#24086,#24087,#24088,#24089,
#24090,#24091,#24092,#24093,#24094,#24095,#24096,#24097,#24098,#24099,#24100,
#24101,#24102,#24103,#24104,#24105,#24106,#24107,#24108,#24109,#24110,#24111,
#24112,#24113,#24114,#24115,#24116,#24117,#24118,#24119,#24120,#24121,#24122,
#24123,#24124,#24125,#24126,#24127,#24128,#24129,#24130,#24131,#24132,#24133,
#24134,#24135,#24136,#24137,#24138,#24139,#24140,#24141,#24142,#24143,#24144,
#24145,#24146,#24147,#24148,#24149,#24150,#24151,#24152,#24153,#24154,#24155,
#24156,#24157,#24158,#24159,#24160,#24161,#24162,#24163,#24164,#24165,#24166,
#24167,#24168,#24169,#24170,#24171,#24172,#24173,#24174,#24175,#24176,#24177,
#24178,#24179,#24180,#24181,#24182,#24183,#24184,#24185,#24186,#24187),
 .UNSPECIFIED.,.F.,.F.,(4,3,3,3,3,3,3,3,3,3,3,3,3,3,3,3,3,3,3,3,3,3,3,3,
3,3,3,3,3,3,3,3,3,3,3,3,3,3,3,3,3,3,3,3,3,4),(-439.472251893527,-439.468657657926,
-439.311231772696,-439.15409548774,-438.997127963201,-438.840079822431,
-438.682983695525,-438.525548000696,-438.469865254158,-438.312439469266,
-438.155303287897,-437.998335869829,-437.841287838569,-437.684191823072,
-437.526756240826,-437.47107285039,-437.313646957827,-437.156510666562,
-436.999543136757,-436.842494992339,-436.685398862719,-436.527963166623,
-436.472280446622,-436.314854587534,-436.157718330119,-436.000750834421,
-435.84370272409,-435.686606628587,-435.529170966138,-435.473488042854,
-435.316062193978,-435.158925947163,-435.001958462417,-434.844910363434,
-434.687814279521,-434.530378628852,-434.474695639086,-434.317269775444,
-434.160133513544,-434.003166013446,-433.846117898893,-433.689021799266,
-433.531586132904,-433.475903235318,-433.282382207345,-433.189066586492),
 .UNSPECIFIED.);
#665=B_SPLINE_CURVE_WITH_KNOTS('',3,(#24189,#24190,#24191,#24192,#24193,
#24194,#24195,#24196,#24197,#24198,#24199,#24200,#24201,#24202,#24203,#24204,
#24205,#24206,#24207,#24208,#24209,#24210,#24211,#24212,#24213,#24214,#24215,
#24216,#24217,#24218,#24219,#24220,#24221,#24222,#24223,#24224,#24225,#24226,
#24227,#24228,#24229,#24230,#24231,#24232,#24233,#24234,#24235,#24236,#24237,
#24238,#24239,#24240,#24241,#24242,#24243,#24244,#24245,#24246,#24247,#24248,
#24249,#24250,#24251,#24252,#24253,#24254,#24255,#24256,#24257,#24258,#24259,
#24260,#24261,#24262,#24263,#24264,#24265,#24266,#24267,#24268,#24269,#24270,
#24271,#24272,#24273,#24274,#24275,#24276,#24277,#24278,#24279,#24280,#24281,
#24282,#24283,#24284,#24285,#24286,#24287,#24288,#24289,#24290,#24291,#24292,
#24293,#24294,#24295,#24296,#24297,#24298,#24299,#24300,#24301,#24302,#24303,
#24304,#24305,#24306,#24307,#24308,#24309,#24310,#24311,#24312,#24313,#24314,
#24315,#24316,#24317,#24318,#24319,#24320,#24321),.UNSPECIFIED.,.F.,.F.,
(4,3,3,3,3,3,3,3,3,3,3,3,3,3,3,3,3,3,3,3,3,3,3,3,3,3,3,3,3,3,3,3,3,3,3,
3,3,3,3,3,3,3,3,3,4),(-433.189066586347,-433.033254193185,-432.877394202068,
-432.721515030693,-432.565286838749,-432.47711083155,-432.319684974318,
-432.162548718947,-432.005581225473,-431.848533117611,-431.69143702472,
-431.534001365061,-431.478318427782,-431.320892568569,-431.163756311173,
-431.006788815636,-430.849740705678,-430.69264461067,-430.535208948895,
-430.479526024014,-430.322100165682,-430.16496390918,-430.007996414548,
-429.850948305499,-429.693852211404,-429.536416550533,-429.480733620246,
-429.323307761953,-429.166171505494,-429.00920401091,-428.852155901915,
-428.695059807878,-428.537624147069,-428.481941216478,-428.324515357926,
-428.167379101201,-428.010411606347,-427.853363497076,-427.696267402761,
-427.538831741673,-427.48314881271,-427.322417720406,-427.162039311243,
-427.001921757567,-426.905881279168),.UNSPECIFIED.);
#666=B_SPLINE_CURVE_WITH_KNOTS('',3,(#24323,#24324,#24325,#24326,#24327,
#24328,#24329,#24330,#24331,#24332,#24333,#24334,#24335,#24336,#24337,#24338,
#24339,#24340,#24341,#24342,#24343,#24344,#24345,#24346,#24347,#24348,#24349,
#24350,#24351,#24352,#24353,#24354,#24355,#24356,#24357,#24358,#24359,#24360,
#24361,#24362,#24363,#24364,#24365,#24366,#24367,#24368,#24369,#24370,#24371,
#24372,#24373,#24374,#24375,#24376,#24377,#24378,#24379,#24380,#24381,#24382,
#24383,#24384,#24385,#24386,#24387,#24388,#24389,#24390,#24391,#24392,#24393,
#24394,#24395,#24396,#24397,#24398,#24399,#24400,#24401,#24402,#24403,#24404,
#24405,#24406,#24407,#24408,#24409,#24410,#24411,#24412,#24413,#24414,#24415,
#24416,#24417,#24418,#24419,#24420,#24421,#24422,#24423,#24424,#24425,#24426,
#24427,#24428,#24429,#24430,#24431,#24432,#24433,#24434,#24435,#24436,#24437,
#24438,#24439,#24440,#24441,#24442,#24443,#24444,#24445,#24446,#24447,#24448,
#24449,#24450,#24451,#24452,#24453,#24454,#24455),.UNSPECIFIED.,.F.,.F.,
(4,3,3,3,3,3,3,3,3,3,3,3,3,3,3,3,3,3,3,3,3,3,3,3,3,3,3,3,3,3,3,3,3,3,3,
3,3,3,3,3,3,3,3,3,4),(-426.905881278986,-426.734684431719,-426.562354361466,
-426.484356408942,-426.326930550519,-426.169794293926,-426.012826799205,
-425.85577869007,-425.698682595891,-425.54124693494,-425.485564005174,-425.328138146718,
-425.171001890091,-425.014034395336,-424.856986286166,-424.699890191952,
-424.542454530965,-424.486771601406,-424.32934574297,-424.172209486364,
-424.015241991629,-423.85819388248,-423.701097788287,-423.543662127321,
-423.487979197638,-423.330553339199,-423.173417082591,-423.016449587854,
-422.859401478702,-422.702305384507,-422.544869723539,-422.48918679387,
-422.331760935427,-422.174624678815,-422.017657184074,-421.860609074918,
-421.703512980719,-421.546077319746,-421.490394390102,-421.335204760125,
-421.180302064992,-421.025459880721,-420.870661563784,-420.715596582732,
-420.622695971988),.UNSPECIFIED.);
#667=B_SPLINE_CURVE_WITH_KNOTS('',3,(#24457,#24458,#24459,#24460,#24461,
#24462,#24463,#24464,#24465,#24466,#24467),.UNSPECIFIED.,.F.,.F.,(4,1,1,
1,1,1,1,1,4),(-420.622695971988,-420.491601986334,-419.492809582566,-418.494017178798,
-417.49522477503,-416.496432371262,-415.497639967494,-414.498847563725,
-414.339510664809),.UNSPECIFIED.);
#668=B_SPLINE_CURVE_WITH_KNOTS('',3,(#24469,#24470,#24471,#24472,#24473,
#24474,#24475,#24476,#24477,#24478,#24479,#24480,#24481,#24482,#24483,#24484,
#24485,#24486,#24487,#24488,#24489,#24490,#24491,#24492,#24493,#24494,#24495,
#24496,#24497,#24498,#24499,#24500,#24501,#24502,#24503,#24504,#24505,#24506,
#24507,#24508,#24509,#24510,#24511,#24512,#24513,#24514,#24515,#24516,#24517,
#24518,#24519,#24520,#24521,#24522,#24523,#24524,#24525,#24526,#24527,#24528,
#24529,#24530,#24531,#24532,#24533,#24534,#24535,#24536,#24537,#24538,#24539,
#24540,#24541,#24542,#24543,#24544,#24545,#24546,#24547,#24548,#24549,#24550,
#24551,#24552,#24553,#24554,#24555,#24556,#24557,#24558,#24559,#24560,#24561,
#24562,#24563,#24564,#24565,#24566,#24567,#24568,#24569,#24570,#24571,#24572,
#24573,#24574,#24575,#24576,#24577,#24578,#24579,#24580,#24581,#24582,#24583,
#24584,#24585,#24586,#24587,#24588,#24589,#24590,#24591,#24592,#24593,#24594,
#24595,#24596,#24597,#24598,#24599,#24600,#24601),.UNSPECIFIED.,.F.,.F.,
(4,3,3,3,3,3,3,3,3,3,3,3,3,3,3,3,3,3,3,3,3,3,3,3,3,3,3,3,3,3,3,3,3,3,3,
3,3,3,3,3,3,3,3,3,4),(-414.339510664809,-414.18459996589,-414.02990276154,
-413.875168508411,-413.720414365598,-413.565333554294,-413.500055159957,
-413.342629301517,-413.185493044907,-413.028525550168,-412.871477441014,
-412.714381346817,-412.556945685847,-412.501262756189,-412.343836897749,
-412.186700641139,-412.0297331464,-411.872685037246,-411.715588943049,-411.558153282079,
-411.502470352421,-411.34504449398,-411.18790823737,-411.030940742631,-410.873892633478,
-410.71679653928,-410.55936087831,-410.503677948653,-410.346252090213,-410.189115833602,
-410.032148338863,-409.87510022971,-409.718004135513,-409.560568474542,
-409.504885544885,-409.347459686444,-409.190323429834,-409.033355935095,
-408.876307825941,-408.719211731744,-408.561776070773,-408.506093141117,
-408.336537608055,-408.167873380534,-408.056325619396),.UNSPECIFIED.);
#669=B_SPLINE_CURVE_WITH_KNOTS('',3,(#24603,#24604,#24605,#24606,#24607,
#24608,#24609,#24610,#24611,#24612),.UNSPECIFIED.,.F.,.F.,(4,1,1,1,1,1,
1,4),(-408.056325357629,-407.507300737349,-406.508508333581,-405.509715929813,
-404.510923526045,-403.512131122277,-402.513338718509,-401.773140050449),
 .UNSPECIFIED.);
#670=B_SPLINE_CURVE_WITH_KNOTS('',3,(#24614,#24615,#24616,#24617,#24618,
#24619,#24620,#24621,#24622,#24623,#24624,#24625,#24626,#24627,#24628,#24629,
#24630,#24631,#24632,#24633,#24634,#24635,#24636,#24637,#24638,#24639,#24640,
#24641,#24642,#24643,#24644,#24645,#24646,#24647,#24648,#24649,#24650,#24651,
#24652,#24653,#24654,#24655,#24656,#24657,#24658,#24659,#24660,#24661,#24662,
#24663,#24664,#24665,#24666,#24667,#24668,#24669,#24670,#24671,#24672,#24673,
#24674,#24675,#24676,#24677,#24678,#24679,#24680,#24681,#24682,#24683,#24684,
#24685,#24686,#24687,#24688,#24689,#24690,#24691,#24692,#24693,#24694,#24695,
#24696,#24697,#24698,#24699,#24700,#24701,#24702,#24703,#24704,#24705,#24706,
#24707,#24708,#24709,#24710,#24711,#24712,#24713,#24714,#24715,#24716,#24717,
#24718,#24719,#24720,#24721,#24722,#24723,#24724,#24725,#24726,#24727,#24728,
#24729,#24730,#24731,#24732,#24733,#24734,#24735,#24736,#24737,#24738,#24739,
#24740,#24741,#24742,#24743,#24744,#24745,#24746,#24747,#24748,#24749),
 .UNSPECIFIED.,.F.,.F.,(4,3,3,3,3,3,3,3,3,3,3,3,3,3,3,3,3,3,3,3,3,3,3,3,
3,3,3,3,3,3,3,3,3,3,3,3,3,3,3,3,3,3,3,3,3,4),(-401.773139972096,-401.571895517567,
-401.514546314741,-401.3571204563,-401.19998419969,-401.04301670495,-400.885968595796,
-400.728872501598,-400.571436840628,-400.515753910973,-400.358328052533,
-400.201191795923,-400.044224301183,-399.88717619203,-399.730080097833,
-399.572644436863,-399.516961507205,-399.359535648765,-399.202399392154,
-399.045431897415,-398.888383788262,-398.731287694065,-398.573852033095,
-398.518169103437,-398.360743244997,-398.203606988386,-398.046639493647,
-397.889591384493,-397.732495290296,-397.575059629326,-397.519376699669,
-397.361950841229,-397.204814584618,-397.047847089879,-396.890798980726,
-396.733702886529,-396.576267225559,-396.520584295901,-396.36315843746,
-396.20602218085,-396.049054686111,-395.892006576957,-395.73491048276,-395.577474821789,
-395.521791892133,-395.48995474327),.UNSPECIFIED.);
#671=B_SPLINE_CURVE_WITH_KNOTS('',3,(#24751,#24752,#24753,#24754,#24755,
#24756,#24757,#24758,#24759,#24760,#24761,#24762,#24763,#24764,#24765,#24766,
#24767,#24768,#24769,#24770,#24771,#24772,#24773,#24774,#24775,#24776,#24777,
#24778,#24779,#24780,#24781,#24782,#24783,#24784,#24785,#24786,#24787,#24788,
#24789,#24790,#24791,#24792,#24793,#24794,#24795,#24796,#24797,#24798,#24799,
#24800,#24801,#24802,#24803,#24804,#24805,#24806,#24807,#24808,#24809,#24810,
#24811,#24812,#24813,#24814,#24815,#24816,#24817,#24818,#24819,#24820,#24821,
#24822,#24823,#24824,#24825,#24826,#24827,#24828,#24829,#24830,#24831,#24832,
#24833,#24834,#24835,#24836,#24837,#24838,#24839,#24840,#24841,#24842,#24843,
#24844,#24845,#24846,#24847,#24848,#24849,#24850,#24851,#24852,#24853,#24854,
#24855,#24856,#24857,#24858,#24859,#24860,#24861,#24862,#24863,#24864,#24865,
#24866,#24867,#24868,#24869,#24870,#24871,#24872,#24873,#24874,#24875,#24876,
#24877,#24878,#24879,#24880,#24881,#24882,#24883),.UNSPECIFIED.,.F.,.F.,
(4,3,3,3,3,3,3,3,3,3,3,3,3,3,3,3,3,3,3,3,3,3,3,3,3,3,3,3,3,3,3,3,3,3,3,
3,3,3,3,3,3,3,3,3,4),(-395.489954743044,-395.333356255252,-395.177042096409,
-395.013531444398,-394.857291860972,-394.700987210959,-394.544356112011,
-394.522999488365,-394.365573629925,-394.208437373314,-394.051469878575,
-393.894421769422,-393.737325675225,-393.579890014255,-393.524207084597,
-393.366781226157,-393.209644969546,-393.052677474807,-392.895629365654,
-392.738533271457,-392.581097610486,-392.525414680829,-392.367988822388,
-392.210852565778,-392.053885071039,-391.896836961886,-391.739740867688,
-391.582305206718,-391.526622277061,-391.369196418621,-391.21206016201,
-391.055092667271,-390.898044558118,-390.740948463921,-390.583512802951,
-390.527829873293,-390.370404014853,-390.213267758243,-390.056300263504,
-389.89925215435,-389.742156060153,-389.584720399183,-389.529037469525,
-389.343111524021,-389.206769436297),.UNSPECIFIED.);
#672=B_SPLINE_CURVE_WITH_KNOTS('',3,(#24885,#24886,#24887,#24888,#24889,
#24890,#24891,#24892,#24893,#24894,#24895,#24896,#24897,#24898,#24899,#24900,
#24901,#24902,#24903,#24904,#24905,#24906,#24907,#24908,#24909,#24910,#24911,
#24912,#24913,#24914,#24915,#24916,#24917,#24918,#24919,#24920,#24921,#24922,
#24923,#24924,#24925,#24926,#24927,#24928,#24929,#24930,#24931,#24932,#24933,
#24934,#24935,#24936,#24937,#24938,#24939,#24940,#24941,#24942,#24943,#24944,
#24945,#24946,#24947,#24948,#24949,#24950,#24951,#24952,#24953,#24954,#24955,
#24956,#24957,#24958,#24959,#24960,#24961,#24962,#24963,#24964,#24965,#24966,
#24967,#24968,#24969,#24970,#24971,#24972,#24973,#24974,#24975,#24976,#24977,
#24978,#24979,#24980,#24981,#24982,#24983,#24984,#24985,#24986,#24987,#24988,
#24989,#24990,#24991,#24992,#24993,#24994,#24995,#24996,#24997,#24998,#24999,
#25000,#25001,#25002,#25003,#25004,#25005,#25006,#25007,#25008,#25009,#25010,
#25011,#25012,#25013,#25014,#25015,#25016,#25017),.UNSPECIFIED.,.F.,.F.,
(4,3,3,3,3,3,3,3,3,3,3,3,3,3,3,3,3,3,3,3,3,3,3,3,3,3,3,3,3,3,3,3,3,3,3,
3,3,3,3,3,3,3,3,3,4),(-389.20676943609,-389.050212150193,-388.893556938872,
-388.736841628448,-388.57977489144,-388.530245065757,-388.372819207317,
-388.215682950706,-388.058715455967,-387.901667346814,-387.744571252616,
-387.587135591646,-387.531452661989,-387.374026803549,-387.216890546938,
-387.059923052199,-386.902874943046,-386.745778848848,-386.588343187878,
-386.532660258221,-386.375234399781,-386.21809814317,-386.061130648431,
-385.904082539278,-385.746986445081,-385.589550784111,-385.533867854453,
-385.376441996013,-385.219305739402,-385.062338244663,-384.90529013551,
-384.748194041312,-384.590758380342,-384.535075450685,-384.377649592244,
-384.220513335634,-384.063545840895,-383.906497731741,-383.749401637544,
-383.591965976573,-383.536283046917,-383.377122321744,-383.218286232242,
-383.059621574311,-382.923584128911),.UNSPECIFIED.);
#673=B_SPLINE_CURVE_WITH_KNOTS('',3,(#25019,#25020,#25021,#25022,#25023,
#25024,#25025,#25026,#25027,#25028),.UNSPECIFIED.,.F.,.F.,(4,1,1,1,1,1,
1,4),(-382.923576795181,-382.537490643149,-381.538698239381,-380.539905835613,
-379.541113431845,-378.542321028077,-377.543528624309,-376.64040770302),
 .UNSPECIFIED.);
#674=B_SPLINE_CURVE_WITH_KNOTS('',3,(#25030,#25031,#25032,#25033,#25034,
#25035,#25036,#25037,#25038,#25039,#25040,#25041,#25042,#25043,#25044,#25045,
#25046,#25047,#25048,#25049,#25050,#25051,#25052,#25053,#25054,#25055,#25056,
#25057,#25058,#25059,#25060,#25061,#25062,#25063,#25064,#25065,#25066,#25067,
#25068,#25069,#25070,#25071,#25072,#25073,#25074,#25075,#25076,#25077,#25078,
#25079,#25080,#25081,#25082,#25083,#25084,#25085,#25086,#25087,#25088,#25089,
#25090,#25091,#25092,#25093,#25094,#25095,#25096,#25097,#25098,#25099,#25100,
#25101,#25102,#25103,#25104,#25105,#25106,#25107,#25108,#25109,#25110,#25111,
#25112,#25113,#25114,#25115,#25116,#25117,#25118,#25119,#25120,#25121,#25122,
#25123,#25124,#25125,#25126,#25127,#25128,#25129,#25130,#25131,#25132,#25133,
#25134,#25135,#25136,#25137,#25138,#25139,#25140,#25141,#25142,#25143,#25144,
#25145,#25146,#25147,#25148,#25149,#25150,#25151,#25152,#25153,#25154,#25155,
#25156,#25157,#25158,#25159,#25160,#25161,#25162),.UNSPECIFIED.,.F.,.F.,
(4,3,3,3,3,3,3,3,3,3,3,3,3,3,3,3,3,3,3,3,3,3,3,3,3,3,3,3,3,3,3,3,3,3,3,
3,3,3,3,3,3,3,3,3,4),(-376.640398821731,-376.544736220541,-376.3873103621,
-376.23017410549,-376.073206610751,-375.916158501597,-375.7590624074,-375.60162674643,
-375.545943816773,-375.388517958333,-375.231381701722,-375.074414206983,
-374.91736609783,-374.760270003632,-374.602834342662,-374.547151413005,
-374.389725554565,-374.232589297955,-374.075621803215,-373.918573694062,
-373.761477599865,-373.604041938895,-373.548359009237,-373.390933150797,
-373.233796894186,-373.076829399447,-372.919781290294,-372.762685196096,
-372.605249535126,-372.549566605469,-372.392140747029,-372.235004490418,
-372.078036995679,-371.920988886525,-371.763892792328,-371.606457131358,
-371.550774201701,-371.393348343261,-371.23621208665,-371.079244591911,
-370.922196482758,-370.76510038856,-370.60766472759,-370.551981797933,-370.357213514552),
 .UNSPECIFIED.);
#675=B_SPLINE_CURVE_WITH_KNOTS('',3,(#25164,#25165,#25166,#25167,#25168,
#25169,#25170,#25171,#25172,#25173),.UNSPECIFIED.,.F.,.F.,(4,1,1,1,1,1,
1,4),(-370.357209727041,-369.553189394165,-368.554396990397,-367.555604586629,
-366.556812182861,-365.558019779093,-364.559227375325,-364.074029310628),
 .UNSPECIFIED.);
#676=B_SPLINE_CURVE_WITH_KNOTS('',3,(#25175,#25176,#25177,#25178,#25179,
#25180,#25181,#25182,#25183,#25184,#25185,#25186,#25187,#25188,#25189,#25190,
#25191,#25192,#25193,#25194,#25195,#25196,#25197,#25198,#25199,#25200,#25201,
#25202,#25203,#25204,#25205,#25206,#25207,#25208,#25209,#25210,#25211,#25212,
#25213,#25214,#25215,#25216,#25217,#25218,#25219,#25220,#25221,#25222,#25223,
#25224,#25225,#25226,#25227,#25228,#25229,#25230,#25231,#25232,#25233,#25234,
#25235,#25236,#25237,#25238,#25239,#25240,#25241,#25242,#25243,#25244,#25245,
#25246,#25247,#25248,#25249,#25250,#25251,#25252,#25253,#25254,#25255,#25256,
#25257,#25258,#25259,#25260,#25261,#25262,#25263,#25264,#25265,#25266,#25267,
#25268,#25269,#25270,#25271,#25272,#25273,#25274,#25275,#25276,#25277,#25278,
#25279,#25280,#25281,#25282,#25283,#25284,#25285,#25286,#25287,#25288,#25289,
#25290,#25291,#25292,#25293,#25294,#25295,#25296,#25297,#25298,#25299,#25300,
#25301,#25302,#25303,#25304,#25305,#25306,#25307),.UNSPECIFIED.,.F.,.F.,
(4,3,3,3,3,3,3,3,3,3,3,3,3,3,3,3,3,3,3,3,3,3,3,3,3,3,3,3,3,3,3,3,3,3,3,
3,3,3,3,3,3,3,3,3,4),(-364.074028207372,-363.910363618122,-363.746409744268,
-363.581908190044,-363.560434971557,-363.403009113117,-363.245872856506,
-363.088905361767,-362.931857252614,-362.774761158417,-362.617325497447,
-362.561642567789,-362.404216709349,-362.247080452738,-362.090112957999,
-361.933064848846,-361.775968754648,-361.618533093678,-361.562850164021,
-361.40542430558,-361.24828804897,-361.091320554231,-360.934272445078,-360.77717635088,
-360.61974068991,-360.564057760253,-360.406631901813,-360.249495645202,
-360.092528150463,-359.93548004131,-359.778383947113,-359.620948286143,
-359.565265356485,-359.407839498044,-359.250703241434,-359.093735746695,
-358.936687637542,-358.779591543344,-358.622155882374,-358.566472952717,
-358.411148615583,-358.256067606148,-358.101147748962,-357.945995324577,
-357.790842900193),.UNSPECIFIED.);
#677=B_SPLINE_CURVE_WITH_KNOTS('',3,(#25309,#25310,#25311,#25312,#25313,
#25314,#25315,#25316,#25317,#25318,#25319),.UNSPECIFIED.,.F.,.F.,(4,1,1,
1,1,1,1,1,4),(-357.790842900193,-357.567680548949,-356.568888145181,-355.570095741413,
-354.571303337645,-353.572510933877,-352.573718530109,-351.574926126341,
-351.507657593013),.UNSPECIFIED.);
#678=B_SPLINE_CURVE_WITH_KNOTS('',3,(#25321,#25322,#25323,#25324,#25325,
#25326,#25327,#25328,#25329,#25330,#25331,#25332,#25333,#25334,#25335,#25336,
#25337,#25338,#25339,#25340,#25341,#25342,#25343,#25344,#25345,#25346,#25347,
#25348,#25349,#25350,#25351,#25352,#25353,#25354,#25355,#25356,#25357,#25358,
#25359,#25360,#25361,#25362,#25363,#25364,#25365,#25366,#25367,#25368,#25369,
#25370,#25371,#25372,#25373,#25374,#25375,#25376,#25377,#25378,#25379,#25380,
#25381,#25382,#25383,#25384,#25385,#25386,#25387,#25388,#25389,#25390,#25391,
#25392,#25393,#25394,#25395,#25396,#25397,#25398,#25399,#25400,#25401,#25402,
#25403,#25404,#25405,#25406,#25407,#25408,#25409,#25410,#25411,#25412,#25413,
#25414,#25415,#25416,#25417,#25418,#25419,#25420,#25421,#25422,#25423,#25424,
#25425,#25426,#25427,#25428,#25429,#25430,#25431,#25432,#25433,#25434,#25435,
#25436,#25437,#25438,#25439,#25440,#25441,#25442,#25443,#25444,#25445,#25446,
#25447,#25448,#25449,#25450),.UNSPECIFIED.,.F.,.F.,(4,3,3,3,3,3,3,3,3,3,
3,3,3,3,3,3,3,3,3,3,3,3,3,3,3,3,3,3,3,3,3,3,3,3,3,3,3,3,3,3,3,3,3,4),(-351.507657593013,
-351.351786036364,-351.19618592939,-351.040599679445,-350.885048669655,
-350.72913646519,-350.576133722573,-350.418707864133,-350.261571607522,
-350.104604112783,-349.94755600363,-349.790459909432,-349.633024248462,
-349.577341318805,-349.419915460365,-349.262779203754,-349.105811709015,
-348.948763599862,-348.791667505664,-348.634231844694,-348.578548915037,
-348.421123056597,-348.263986799986,-348.107019305247,-347.949971196094,
-347.792875101896,-347.635439440926,-347.579756511269,-347.422330652829,
-347.265194396218,-347.108226901479,-346.951178792326,-346.794082698128,
-346.636647037158,-346.580964107501,-346.423538249061,-346.266401992451,
-346.109434497712,-345.952386388559,-345.795290294362,-345.637854633392,
-345.582171703733,-345.402219924872,-345.224472530763),.UNSPECIFIED.);
#679=B_SPLINE_CURVE_WITH_KNOTS('',3,(#25452,#25453,#25454,#25455,#25456,
#25457,#25458,#25459,#25460,#25461),.UNSPECIFIED.,.F.,.F.,(4,1,1,1,1,1,
1,4),(-345.224472285833,-344.583379299965,-343.584586896197,-342.585794492429,
-341.587002088661,-340.588209684893,-339.589417281125,-338.941286978654),
 .UNSPECIFIED.);
#680=B_SPLINE_CURVE_WITH_KNOTS('',3,(#25463,#25464,#25465,#25466,#25467,
#25468,#25469,#25470,#25471,#25472,#25473,#25474,#25475,#25476,#25477,#25478,
#25479,#25480,#25481,#25482,#25483,#25484,#25485,#25486,#25487,#25488,#25489,
#25490,#25491,#25492,#25493,#25494,#25495,#25496,#25497,#25498,#25499,#25500,
#25501,#25502,#25503,#25504,#25505,#25506,#25507,#25508,#25509,#25510,#25511,
#25512,#25513,#25514,#25515,#25516,#25517,#25518,#25519,#25520,#25521,#25522,
#25523,#25524,#25525,#25526,#25527,#25528,#25529,#25530,#25531,#25532,#25533,
#25534,#25535,#25536,#25537,#25538,#25539,#25540,#25541,#25542,#25543,#25544,
#25545,#25546,#25547,#25548,#25549,#25550,#25551,#25552,#25553,#25554,#25555,
#25556,#25557,#25558,#25559,#25560,#25561,#25562,#25563,#25564,#25565,#25566,
#25567,#25568,#25569,#25570,#25571,#25572,#25573,#25574,#25575,#25576,#25577,
#25578,#25579,#25580,#25581,#25582,#25583,#25584,#25585,#25586,#25587,#25588,
#25589,#25590,#25591,#25592),.UNSPECIFIED.,.F.,.F.,(4,3,3,3,3,3,3,3,3,3,
3,3,3,3,3,3,3,3,3,3,3,3,3,3,3,3,3,3,3,3,3,3,3,3,3,3,3,3,3,3,3,3,3,4),(-338.941286736142,
-338.760252301847,-338.590624877357,-338.433199018916,-338.276062762304,
-338.119095267564,-337.962047158409,-337.804951064211,-337.64751540324,
-337.591832473588,-337.434406615148,-337.277270358537,-337.120302863798,
-336.963254754645,-336.806158660448,-336.648722999478,-336.59304006982,
-336.43561421138,-336.27847795477,-336.121510460031,-335.964462350878,-335.807366256681,
-335.649930595711,-335.594247666052,-335.436821807611,-335.279685551001,
-335.122718056262,-334.965669947108,-334.808573852911,-334.651138191941,
-334.595455262284,-334.438029403844,-334.280893147233,-334.123925652494,
-333.966877543341,-333.809781449143,-333.652345788173,-333.596662858516,
-333.440630649672,-333.284885507811,-333.128189548727,-332.972529747918,
-332.815315709696,-332.658101671474),.UNSPECIFIED.);
#681=B_SPLINE_CURVE_WITH_KNOTS('',3,(#25594,#25595,#25596,#25597,#25598,
#25599,#25600,#25601,#25602,#25603,#25604,#25605),.UNSPECIFIED.,.F.,.F.,
(4,2,1,1,1,1,1,1,4),(-332.658101671474,-332.597870454748,-331.59907805098,
-330.600285647212,-329.601493243444,-328.602700839676,-327.603908435908,
-326.60511603214,-326.374916364295),.UNSPECIFIED.);
#682=B_SPLINE_CURVE_WITH_KNOTS('',3,(#25607,#25608,#25609,#25610,#25611,
#25612,#25613,#25614,#25615,#25616,#25617,#25618,#25619,#25620,#25621,#25622,
#25623,#25624,#25625,#25626,#25627,#25628,#25629,#25630,#25631,#25632,#25633,
#25634,#25635,#25636,#25637,#25638,#25639,#25640,#25641,#25642,#25643,#25644,
#25645,#25646,#25647,#25648,#25649,#25650,#25651,#25652,#25653,#25654,#25655,
#25656,#25657,#25658,#25659,#25660,#25661,#25662,#25663,#25664,#25665,#25666,
#25667,#25668,#25669,#25670,#25671,#25672,#25673,#25674,#25675,#25676,#25677,
#25678,#25679,#25680,#25681,#25682,#25683,#25684,#25685,#25686,#25687,#25688,
#25689,#25690,#25691,#25692,#25693,#25694,#25695,#25696,#25697,#25698,#25699,
#25700,#25701,#25702,#25703,#25704,#25705,#25706,#25707,#25708,#25709,#25710,
#25711,#25712,#25713,#25714,#25715,#25716,#25717,#25718,#25719,#25720,#25721,
#25722,#25723,#25724,#25725,#25726,#25727,#25728,#25729,#25730,#25731,#25732,
#25733,#25734,#25735,#25736,#25737,#25738,#25739),.UNSPECIFIED.,.F.,.F.,
(4,3,3,3,3,3,3,3,3,3,3,3,3,3,3,3,3,3,3,3,3,3,3,3,3,3,3,3,3,3,3,3,3,3,3,
3,3,3,3,3,3,3,3,3,4),(-326.374916364295,-326.21983494529,-326.064772095614,
-325.909746049644,-325.754364066725,-325.606323628372,-325.448897769932,
-325.291761513322,-325.134794018582,-324.977745909429,-324.820649815232,
-324.663214154262,-324.607531224604,-324.450105366164,-324.292969109553,
-324.136001614814,-323.978953505661,-323.821857411464,-323.664421750494,
-323.608738820836,-323.451312962395,-323.294176705785,-323.137209211046,
-322.980161101892,-322.823065007695,-322.665629346725,-322.609946417068,
-322.452520558628,-322.295384302017,-322.138416807278,-321.981368698125,
-321.824272603927,-321.666836942957,-321.6111540133,-321.45372815486,-321.296591898249,
-321.13962440351,-320.982576294357,-320.825480200159,-320.668044539189,
-320.612361609532,-320.448407729625,-320.284879993641,-320.121782250729,
-320.091731057115),.UNSPECIFIED.);
#683=B_SPLINE_CURVE_WITH_KNOTS('',3,(#25741,#25742,#25743,#25744,#25745,
#25746,#25747,#25748,#25749,#25750),.UNSPECIFIED.,.F.,.F.,(4,1,1,1,1,1,
1,4),(-320.091729415284,-319.613569205764,-318.614776801996,-317.615984398228,
-316.61719199446,-315.618399590692,-314.619607186924,-313.808550197804),
 .UNSPECIFIED.);
#684=B_SPLINE_CURVE_WITH_KNOTS('',3,(#25752,#25753,#25754,#25755,#25756,
#25757,#25758,#25759,#25760,#25761,#25762,#25763,#25764,#25765,#25766,#25767,
#25768,#25769,#25770,#25771,#25772,#25773,#25774,#25775,#25776,#25777,#25778,
#25779,#25780,#25781,#25782,#25783,#25784,#25785,#25786,#25787,#25788,#25789,
#25790,#25791,#25792,#25793,#25794,#25795,#25796,#25797,#25798,#25799,#25800,
#25801,#25802,#25803,#25804,#25805,#25806,#25807,#25808,#25809,#25810,#25811,
#25812,#25813,#25814,#25815,#25816,#25817,#25818,#25819,#25820,#25821,#25822,
#25823,#25824,#25825,#25826,#25827,#25828,#25829,#25830,#25831,#25832,#25833,
#25834,#25835,#25836,#25837,#25838,#25839,#25840,#25841,#25842,#25843,#25844,
#25845,#25846,#25847,#25848,#25849,#25850,#25851,#25852,#25853,#25854,#25855,
#25856,#25857,#25858,#25859,#25860,#25861,#25862,#25863,#25864,#25865,#25866,
#25867,#25868,#25869,#25870,#25871,#25872,#25873,#25874,#25875,#25876,#25877,
#25878,#25879,#25880,#25881,#25882,#25883,#25884),.UNSPECIFIED.,.F.,.F.,
(4,3,3,3,3,3,3,3,3,3,3,3,3,3,3,3,3,3,3,3,3,3,3,3,3,3,3,3,3,3,3,3,3,3,3,
3,3,3,3,3,3,3,3,3,4),(-313.808545749936,-313.620814783156,-313.463388924717,
-313.306252668109,-313.149285173372,-312.992237064221,-312.835140970025,
-312.677705309057,-312.622022379388,-312.464596520947,-312.307460264337,
-312.150492769598,-311.993444660444,-311.836348566246,-311.678912905276,
-311.62322997562,-311.465804117179,-311.308667860569,-311.151700365829,
-310.994652256676,-310.837556162478,-310.680120501508,-310.624437571852,
-310.467011713412,-310.309875456802,-310.152907962063,-309.995859852909,
-309.838763758712,-309.681328097742,-309.625645168084,-309.468219309644,
-309.311083053033,-309.154115558294,-308.997067449141,-308.839971354943,
-308.682535693973,-308.626852764316,-308.469426905875,-308.312290649265,
-308.155323154526,-307.998275045372,-307.841178951175,-307.683743290205,
-307.628060360548,-307.525360442756),.UNSPECIFIED.);
#685=B_SPLINE_CURVE_WITH_KNOTS('',3,(#25886,#25887,#25888,#25889,#25890,
#25891,#25892,#25893,#25894,#25895,#25896,#25897,#25898,#25899,#25900,#25901,
#25902,#25903,#25904,#25905,#25906,#25907,#25908,#25909,#25910,#25911,#25912,
#25913,#25914,#25915,#25916,#25917,#25918,#25919,#25920,#25921,#25922,#25923,
#25924,#25925,#25926,#25927,#25928,#25929,#25930,#25931,#25932,#25933,#25934,
#25935,#25936,#25937,#25938,#25939,#25940,#25941,#25942,#25943,#25944,#25945,
#25946,#25947,#25948,#25949,#25950,#25951,#25952,#25953,#25954,#25955,#25956,
#25957,#25958,#25959,#25960,#25961,#25962,#25963,#25964,#25965,#25966,#25967,
#25968,#25969,#25970,#25971,#25972,#25973,#25974,#25975,#25976,#25977,#25978,
#25979,#25980,#25981,#25982,#25983,#25984,#25985,#25986,#25987,#25988,#25989,
#25990,#25991,#25992,#25993,#25994,#25995,#25996,#25997,#25998,#25999,#26000,
#26001,#26002,#26003,#26004,#26005,#26006,#26007,#26008,#26009,#26010,#26011,
#26012,#26013,#26014,#26015,#26016,#26017,#26018),.UNSPECIFIED.,.F.,.F.,
(4,3,3,3,3,3,3,3,3,3,3,3,3,3,3,3,3,3,3,3,3,3,3,3,3,3,3,3,3,3,3,3,3,3,3,
3,3,3,3,3,3,3,3,3,4),(-307.52536044253,-307.37001604778,-307.214924493805,
-307.05983056049,-306.904753186811,-306.749329999325,-306.62926795678,-306.47184209834,
-306.314705841729,-306.15773834699,-306.000690237837,-305.84359414364,-305.686158482669,
-305.630475553012,-305.473049694572,-305.315913437961,-305.158945943222,
-305.001897834069,-304.844801739871,-304.687366078901,-304.631683149244,
-304.474257290804,-304.317121034193,-304.160153539454,-304.003105430301,
-303.846009336103,-303.688573675134,-303.632890745476,-303.475464887036,
-303.318328630425,-303.161361135686,-303.004313026533,-302.847216932335,
-302.689781271365,-302.634098341708,-302.476672483268,-302.319536226657,
-302.162568731918,-302.005520622765,-301.848424528568,-301.690988867598,
-301.63530593794,-301.459521411222,-301.285103403596,-301.242175365152),
 .UNSPECIFIED.);
#686=B_SPLINE_CURVE_WITH_KNOTS('',3,(#26020,#26021,#26022,#26023,#26024,
#26025,#26026,#26027,#26028,#26029),.UNSPECIFIED.,.F.,.F.,(4,1,1,1,1,1,
1,4),(-301.242175135576,-300.636513534172,-299.637721130404,-298.638928726636,
-297.640136322868,-296.6413439191,-295.642551515332,-294.958989828397),
 .UNSPECIFIED.);
#687=B_SPLINE_CURVE_WITH_KNOTS('',3,(#26031,#26032,#26033,#26034,#26035,
#26036,#26037,#26038,#26039,#26040,#26041,#26042,#26043,#26044,#26045,#26046,
#26047,#26048,#26049,#26050,#26051,#26052,#26053,#26054,#26055,#26056,#26057,
#26058,#26059,#26060,#26061,#26062,#26063,#26064,#26065,#26066,#26067,#26068,
#26069,#26070,#26071,#26072,#26073,#26074,#26075,#26076,#26077,#26078,#26079,
#26080,#26081,#26082,#26083,#26084,#26085,#26086,#26087,#26088,#26089,#26090,
#26091,#26092,#26093,#26094,#26095,#26096,#26097,#26098,#26099,#26100,#26101,
#26102,#26103,#26104,#26105,#26106,#26107,#26108,#26109,#26110,#26111,#26112,
#26113,#26114,#26115,#26116,#26117,#26118,#26119,#26120,#26121,#26122,#26123,
#26124,#26125,#26126,#26127,#26128,#26129,#26130,#26131,#26132,#26133,#26134,
#26135,#26136,#26137,#26138,#26139,#26140,#26141,#26142,#26143,#26144,#26145,
#26146,#26147,#26148,#26149,#26150,#26151,#26152,#26153,#26154,#26155,#26156,
#26157,#26158,#26159,#26160,#26161,#26162,#26163),.UNSPECIFIED.,.F.,.F.,
(4,3,3,3,3,3,3,3,3,3,3,3,3,3,3,3,3,3,3,3,3,3,3,3,3,3,3,3,3,3,3,3,3,3,3,
3,3,3,3,3,3,3,3,3,4),(-294.958989620074,-294.771703088725,-294.643759111564,
-294.486333253124,-294.329196996514,-294.172229501775,-294.015181392622,
-293.858085298424,-293.700649637455,-293.644966707796,-293.487540849356,
-293.330404592745,-293.173437098006,-293.016388988853,-292.859292894655,
-292.701857233685,-292.646174304028,-292.488748445588,-292.331612188977,
-292.174644694238,-292.017596585085,-291.860500490887,-291.703064829917,
-291.64738190026,-291.48995604182,-291.332819785209,-291.17585229047,-291.018804181317,
-290.861708087119,-290.704272426149,-290.648589496492,-290.491163638052,
-290.334027381441,-290.177059886702,-290.020011777549,-289.862915683352,
-289.705480022382,-289.649797092724,-289.493023928706,-289.336539147324,
-289.180219794627,-289.023819424796,-288.867364041646,-288.710580833308,
-288.675804521405),.UNSPECIFIED.);
#688=B_SPLINE_CURVE_WITH_KNOTS('',3,(#26165,#26166,#26167,#26168,#26169,
#26170,#26171,#26172,#26173,#26174,#26175,#26176,#26177,#26178,#26179,#26180,
#26181,#26182,#26183,#26184,#26185,#26186,#26187,#26188,#26189,#26190,#26191,
#26192,#26193,#26194,#26195,#26196,#26197,#26198,#26199,#26200,#26201,#26202,
#26203,#26204,#26205,#26206,#26207,#26208,#26209,#26210,#26211,#26212,#26213,
#26214,#26215,#26216,#26217,#26218,#26219,#26220,#26221,#26222,#26223,#26224,
#26225,#26226,#26227,#26228,#26229,#26230,#26231,#26232,#26233,#26234,#26235,
#26236,#26237,#26238,#26239,#26240,#26241,#26242,#26243,#26244,#26245,#26246,
#26247,#26248,#26249,#26250,#26251,#26252,#26253,#26254,#26255,#26256,#26257,
#26258,#26259,#26260,#26261,#26262,#26263,#26264,#26265,#26266,#26267,#26268,
#26269,#26270,#26271,#26272,#26273,#26274,#26275,#26276,#26277,#26278,#26279,
#26280,#26281,#26282,#26283,#26284,#26285,#26286,#26287,#26288,#26289,#26290,
#26291,#26292,#26293,#26294,#26295,#26296,#26297,#26298,#26299,#26300),
 .UNSPECIFIED.,.F.,.F.,(4,3,3,3,3,3,3,3,3,3,3,3,3,3,3,3,3,3,3,3,3,3,3,3,
3,3,3,3,3,3,3,3,3,3,3,3,3,3,3,3,3,3,3,3,3,4),(-288.675804521217,-288.651004688956,
-288.493578830515,-288.336442573905,-288.179475079166,-288.022426970012,
-287.865330875815,-287.707895214845,-287.652212285188,-287.494786426748,
-287.337650170137,-287.180682675398,-287.023634566245,-286.866538472047,
-286.709102811077,-286.65341988142,-286.49599402298,-286.338857766369,-286.18189027163,
-286.024842162477,-285.867746068279,-285.710310407309,-285.654627477652,
-285.497201619212,-285.340065362601,-285.183097867862,-285.026049758709,
-284.868953664511,-284.711518003541,-284.655835073884,-284.498409215444,
-284.341272958833,-284.184305464094,-284.027257354941,-283.870161260743,
-283.712725599773,-283.657042670116,-283.499616811676,-283.342480555065,
-283.185513060326,-283.028464951173,-282.871368856975,-282.713933196005,
-282.658250266348,-282.459103445106,-282.392619214225),.UNSPECIFIED.);
#689=B_SPLINE_CURVE_WITH_KNOTS('',3,(#26302,#26303,#26304,#26305,#26306,
#26307,#26308,#26309,#26310,#26311,#26312,#26313,#26314,#26315,#26316,#26317,
#26318,#26319,#26320,#26321,#26322,#26323,#26324,#26325,#26326,#26327,#26328,
#26329,#26330,#26331,#26332,#26333,#26334,#26335,#26336,#26337,#26338,#26339,
#26340,#26341,#26342,#26343,#26344,#26345,#26346,#26347,#26348,#26349,#26350,
#26351,#26352,#26353,#26354,#26355,#26356,#26357,#26358,#26359,#26360,#26361,
#26362,#26363,#26364,#26365,#26366,#26367,#26368,#26369,#26370,#26371,#26372,
#26373,#26374,#26375,#26376,#26377,#26378,#26379,#26380,#26381,#26382,#26383,
#26384,#26385,#26386,#26387,#26388,#26389,#26390,#26391,#26392,#26393,#26394,
#26395,#26396,#26397,#26398,#26399,#26400,#26401,#26402,#26403,#26404,#26405,
#26406,#26407,#26408,#26409,#26410,#26411,#26412,#26413,#26414,#26415,#26416,
#26417,#26418,#26419,#26420,#26421,#26422,#26423,#26424,#26425,#26426,#26427,
#26428,#26429,#26430,#26431,#26432,#26433,#26434),.UNSPECIFIED.,.F.,.F.,
(4,3,3,3,3,3,3,3,3,3,3,3,3,3,3,3,3,3,3,3,3,3,3,3,3,3,3,3,3,3,3,3,3,3,3,
3,3,3,3,3,3,3,3,3,4),(-282.392619214038,-282.237144823419,-282.08164941839,
-281.926157026577,-281.770314486552,-281.65945786258,-281.50203200414,-281.344895747529,
-281.18792825279,-281.030880143637,-280.873784049439,-280.716348388469,
-280.660665458812,-280.503239600372,-280.346103343761,-280.189135849022,
-280.032087739869,-279.874991645671,-279.717555984701,-279.661873055044,
-279.504447196604,-279.347310939993,-279.190343445254,-279.033295336101,
-278.876199241903,-278.718763580933,-278.663080651276,-278.505654792836,
-278.348518536225,-278.191551041486,-278.034502932333,-277.877406838136,
-277.719971177166,-277.664288247508,-277.506862389068,-277.349726132458,
-277.192758637719,-277.035710528565,-276.878614434368,-276.721178773398,
-276.66549584374,-276.50366837988,-276.342216082717,-276.181083091226,-276.109433906858),
 .UNSPECIFIED.);
#690=B_SPLINE_CURVE_WITH_KNOTS('',3,(#26436,#26437,#26438,#26439,#26440,
#26441,#26442,#26443,#26444,#26445),.UNSPECIFIED.,.F.,.F.,(4,1,1,1,1,1,
1,4),(-276.109429479534,-275.666703439972,-274.667911036204,-273.669118632436,
-272.670326228668,-271.6715338249,-270.672741421132,-269.8262558826),
 .UNSPECIFIED.);
#691=B_SPLINE_CURVE_WITH_KNOTS('',3,(#26447,#26448,#26449,#26450,#26451,
#26452,#26453,#26454,#26455,#26456,#26457,#26458,#26459,#26460,#26461,#26462,
#26463,#26464,#26465,#26466,#26467,#26468,#26469,#26470,#26471,#26472,#26473,
#26474,#26475,#26476,#26477,#26478,#26479,#26480,#26481,#26482,#26483,#26484,
#26485,#26486,#26487,#26488,#26489,#26490,#26491,#26492,#26493,#26494,#26495,
#26496,#26497,#26498,#26499,#26500,#26501,#26502,#26503,#26504,#26505,#26506,
#26507,#26508,#26509,#26510,#26511,#26512,#26513,#26514,#26515,#26516,#26517,
#26518,#26519,#26520,#26521,#26522,#26523,#26524,#26525,#26526,#26527,#26528,
#26529,#26530,#26531,#26532,#26533,#26534,#26535,#26536,#26537,#26538,#26539,
#26540,#26541,#26542,#26543,#26544,#26545,#26546,#26547,#26548,#26549,#26550,
#26551,#26552,#26553,#26554,#26555,#26556,#26557,#26558,#26559,#26560,#26561,
#26562,#26563,#26564,#26565,#26566,#26567,#26568,#26569,#26570,#26571,#26572,
#26573,#26574,#26575,#26576,#26577,#26578,#26579),.UNSPECIFIED.,.F.,.F.,
(4,3,3,3,3,3,3,3,3,3,3,3,3,3,3,3,3,3,3,3,3,3,3,3,3,3,3,3,3,3,3,3,3,3,3,
3,3,3,3,3,3,3,3,3,4),(-269.826248599679,-269.673949017364,-269.516523158924,
-269.359386902313,-269.202419407574,-269.04537129842,-268.888275204223,
-268.730839543253,-268.675156613596,-268.517730755156,-268.360594498545,
-268.203627003806,-268.046578894653,-267.889482800455,-267.732047139485,
-267.676364209828,-267.518938351388,-267.361802094777,-267.204834600038,
-267.047786490885,-266.890690396687,-266.733254735717,-266.67757180606,
-266.52014594762,-266.363009691009,-266.20604219627,-266.048994087117,-265.891897992919,
-265.734462331949,-265.678779402292,-265.521353543852,-265.364217287242,
-265.207249792503,-265.050201683349,-264.893105589152,-264.735669928182,
-264.679986998524,-264.522561140083,-264.365424883473,-264.208457388733,
-264.051409279579,-263.894313185381,-263.736877524411,-263.681194594755,
-263.543063292499),.UNSPECIFIED.);
#692=B_SPLINE_CURVE_WITH_KNOTS('',3,(#26581,#26582,#26583,#26584,#26585,
#26586,#26587,#26588,#26589,#26590),.UNSPECIFIED.,.F.,.F.,(4,1,1,1,1,1,
1,4),(-263.543055204836,-262.682402190987,-261.683609787219,-260.684817383451,
-259.686024979683,-258.687232575916,-257.688440172147,-257.259883482651),
 .UNSPECIFIED.);
#693=B_SPLINE_CURVE_WITH_KNOTS('',3,(#26592,#26593,#26594,#26595,#26596,
#26597,#26598,#26599,#26600,#26601,#26602,#26603,#26604,#26605,#26606,#26607,
#26608,#26609,#26610,#26611,#26612,#26613,#26614,#26615,#26616,#26617,#26618,
#26619,#26620,#26621,#26622,#26623,#26624,#26625,#26626,#26627,#26628,#26629,
#26630,#26631,#26632,#26633,#26634,#26635,#26636,#26637,#26638,#26639,#26640,
#26641,#26642,#26643,#26644,#26645,#26646,#26647,#26648,#26649,#26650,#26651,
#26652,#26653,#26654,#26655,#26656,#26657,#26658,#26659,#26660,#26661,#26662,
#26663,#26664,#26665,#26666,#26667,#26668,#26669,#26670,#26671,#26672,#26673,
#26674,#26675,#26676,#26677,#26678,#26679,#26680,#26681,#26682,#26683,#26684,
#26685,#26686,#26687,#26688,#26689,#26690,#26691,#26692,#26693,#26694,#26695,
#26696,#26697,#26698,#26699,#26700,#26701,#26702,#26703,#26704,#26705,#26706,
#26707,#26708,#26709,#26710,#26711,#26712,#26713,#26714,#26715,#26716,#26717,
#26718,#26719,#26720,#26721,#26722,#26723,#26724),.UNSPECIFIED.,.F.,.F.,
(4,3,3,3,3,3,3,3,3,3,3,3,3,3,3,3,3,3,3,3,3,3,3,3,3,3,3,3,3,3,3,3,3,3,3,
3,3,3,3,3,3,3,3,3,4),(-257.259877985319,-257.09937952014,-256.93874742661,
-256.777648047078,-256.689647768379,-256.532221909939,-256.375085653328,
-256.218118158589,-256.061070049436,-255.903973955238,-255.746538294268,
-255.690855364611,-255.533429506171,-255.37629324956,-255.219325754821,
-255.062277645668,-254.905181551471,-254.7477458905,-254.692062960843,-254.534637102403,
-254.377500845792,-254.220533351053,-254.0634852419,-253.906389147702,-253.748953486732,
-253.693270557075,-253.535844698635,-253.378708442024,-253.221740947285,
-253.064692838132,-252.907596743934,-252.750161082964,-252.694478153307,
-252.537052294866,-252.379916038256,-252.222948543517,-252.065900434364,
-251.908804340166,-251.751368679196,-251.695685749539,-251.539571791047,
-251.383743775657,-251.228086863493,-251.072362179131,-250.97669267814),
 .UNSPECIFIED.);
#694=B_SPLINE_CURVE_WITH_KNOTS('',3,(#26726,#26727,#26728,#26729,#26730,
#26731,#26732,#26733,#26734,#26735,#26736,#26737,#26738,#26739,#26740,#26741,
#26742,#26743,#26744,#26745,#26746,#26747,#26748,#26749,#26750,#26751,#26752,
#26753,#26754,#26755,#26756,#26757,#26758,#26759,#26760,#26761,#26762,#26763,
#26764,#26765,#26766,#26767,#26768,#26769,#26770,#26771,#26772,#26773,#26774,
#26775,#26776,#26777,#26778,#26779,#26780,#26781,#26782,#26783,#26784,#26785,
#26786,#26787,#26788,#26789,#26790,#26791,#26792,#26793,#26794,#26795,#26796,
#26797,#26798,#26799,#26800,#26801,#26802,#26803,#26804,#26805,#26806,#26807,
#26808,#26809,#26810,#26811,#26812,#26813,#26814,#26815,#26816,#26817,#26818,
#26819,#26820,#26821,#26822,#26823,#26824,#26825,#26826,#26827,#26828,#26829,
#26830,#26831,#26832,#26833,#26834,#26835,#26836,#26837,#26838,#26839,#26840,
#26841,#26842,#26843,#26844,#26845,#26846,#26847,#26848,#26849,#26850,#26851,
#26852,#26853,#26854,#26855,#26856,#26857,#26858,#26859,#26860,#26861),
 .UNSPECIFIED.,.F.,.F.,(4,3,3,3,3,3,3,3,3,3,3,3,3,3,3,3,3,3,3,3,3,3,3,3,
3,3,3,3,3,3,3,3,3,3,3,3,3,3,3,3,3,3,3,3,3,4),(-250.976692678011,-250.781410048543,
-250.696893345771,-250.539467487331,-250.382331230722,-250.225363735984,
-250.068315626831,-249.911219532634,-249.753783871665,-249.698100942003,
-249.540675083563,-249.383538826952,-249.226571332213,-249.06952322306,
-248.912427128862,-248.754991467892,-248.699308538235,-248.541882679794,
-248.384746423184,-248.227778928445,-248.070730819291,-247.913634725094,
-247.756199064124,-247.700516134467,-247.543090276027,-247.385954019416,
-247.228986524677,-247.071938415524,-246.914842321327,-246.757406660357,
-246.701723730699,-246.544297872259,-246.387161615648,-246.230194120909,
-246.073146011756,-245.916049917558,-245.758614256588,-245.702931326931,
-245.545505468491,-245.388369211881,-245.231401717141,-245.074353607988,
-244.917257513791,-244.759821852821,-244.704138923163,-244.69350737096),
 .UNSPECIFIED.);
#695=B_SPLINE_CURVE_WITH_KNOTS('',3,(#26863,#26864,#26865,#26866,#26867,
#26868,#26869,#26870,#26871,#26872,#26873,#26874,#26875,#26876,#26877,#26878,
#26879,#26880,#26881,#26882,#26883,#26884,#26885,#26886,#26887,#26888,#26889,
#26890,#26891,#26892,#26893,#26894,#26895,#26896,#26897,#26898,#26899,#26900,
#26901,#26902,#26903,#26904,#26905,#26906,#26907,#26908,#26909,#26910,#26911,
#26912,#26913,#26914,#26915,#26916,#26917,#26918,#26919,#26920,#26921,#26922,
#26923,#26924,#26925,#26926,#26927,#26928,#26929,#26930,#26931,#26932,#26933,
#26934,#26935,#26936,#26937,#26938,#26939,#26940,#26941,#26942,#26943,#26944,
#26945,#26946,#26947,#26948,#26949,#26950,#26951,#26952,#26953,#26954,#26955,
#26956,#26957,#26958,#26959,#26960,#26961,#26962,#26963,#26964,#26965,#26966,
#26967,#26968,#26969,#26970,#26971,#26972,#26973,#26974,#26975,#26976,#26977,
#26978,#26979,#26980,#26981,#26982,#26983,#26984,#26985,#26986,#26987,#26988,
#26989,#26990,#26991,#26992,#26993,#26994,#26995),.UNSPECIFIED.,.F.,.F.,
(4,3,3,3,3,3,3,3,3,3,3,3,3,3,3,3,3,3,3,3,3,3,3,3,3,3,3,3,3,3,3,3,3,3,3,
3,3,3,3,3,3,3,3,3,4),(-244.693507370801,-244.536376405573,-244.379534057459,
-244.222858503389,-244.066101113119,-243.909292124089,-243.752147502817,
-243.705346519395,-243.547920660955,-243.390784404344,-243.233816909605,
-243.076768800452,-242.919672706254,-242.762237045284,-242.706554115627,
-242.549128257187,-242.391992000576,-242.235024505837,-242.077976396684,
-241.920880302486,-241.763444641516,-241.707761711859,-241.550335853419,
-241.393199596808,-241.236232102069,-241.079183992916,-240.922087898719,
-240.764652237749,-240.708969308091,-240.551543449651,-240.39440719304,
-240.237439698301,-240.080391589148,-239.92329549495,-239.76585983398,-239.710176904323,
-239.552751045882,-239.395614789272,-239.238647294533,-239.081599185379,
-238.924503091182,-238.767067430211,-238.711384500555,-238.521147976858,
-238.410322247389),.UNSPECIFIED.);
#696=B_SPLINE_CURVE_WITH_KNOTS('',3,(#26997,#26998,#26999,#27000,#27001,
#27002,#27003,#27004,#27005,#27006),.UNSPECIFIED.,.F.,.F.,(4,1,1,1,1,1,
1,4),(-238.410322063781,-237.712592096787,-236.713799693019,-235.715007289251,
-234.716214885483,-233.717422481715,-232.718630077947,-232.127136756601),
 .UNSPECIFIED.);
#697=B_SPLINE_CURVE_WITH_KNOTS('',3,(#27008,#27009,#27010,#27011,#27012,
#27013,#27014,#27015,#27016,#27017,#27018,#27019,#27020,#27021,#27022,#27023,
#27024,#27025,#27026,#27027,#27028,#27029,#27030,#27031,#27032,#27033,#27034,
#27035,#27036,#27037,#27038,#27039,#27040,#27041,#27042,#27043,#27044,#27045,
#27046,#27047,#27048,#27049,#27050,#27051,#27052,#27053,#27054,#27055,#27056,
#27057,#27058,#27059,#27060,#27061,#27062,#27063,#27064,#27065,#27066,#27067,
#27068,#27069,#27070,#27071,#27072,#27073,#27074,#27075,#27076,#27077,#27078,
#27079,#27080,#27081,#27082,#27083,#27084,#27085,#27086,#27087,#27088,#27089,
#27090,#27091,#27092,#27093,#27094,#27095,#27096,#27097,#27098,#27099,#27100,
#27101,#27102,#27103,#27104,#27105,#27106,#27107,#27108,#27109,#27110,#27111,
#27112,#27113,#27114,#27115,#27116,#27117,#27118,#27119,#27120,#27121,#27122,
#27123,#27124,#27125,#27126,#27127,#27128,#27129,#27130,#27131,#27132,#27133,
#27134,#27135,#27136,#27137,#27138,#27139,#27140),.UNSPECIFIED.,.F.,.F.,
(4,3,3,3,3,3,3,3,3,3,3,3,3,3,3,3,3,3,3,3,3,3,3,3,3,3,3,3,3,3,3,3,3,3,3,
3,3,3,3,3,3,3,3,3,4),(-232.127136544053,-231.954428880424,-231.780471113885,
-231.719837674179,-231.562411815739,-231.405275559128,-231.248308064389,
-231.091259955236,-230.934163861038,-230.776728200068,-230.721045270411,
-230.563619411971,-230.40648315536,-230.249515660621,-230.092467551468,
-229.93537145727,-229.7779357963,-229.722252866643,-229.564827008203,-229.407690751592,
-229.250723256853,-229.0936751477,-228.936579053502,-228.779143392532,-228.723460462875,
-228.566034604435,-228.408898347824,-228.251930853085,-228.094882743932,
-227.937786649734,-227.780350988764,-227.724668059107,-227.567242200666,
-227.410105944056,-227.253138449317,-227.096090340163,-226.938994245966,
-226.781558584996,-226.725875655339,-226.570583424025,-226.415577817779,
-226.260626803486,-226.105720181143,-225.950529992756,-225.843951449422),
 .UNSPECIFIED.);
#698=B_SPLINE_CURVE_WITH_KNOTS('',3,(#27142,#27143,#27144,#27145,#27146,
#27147,#27148,#27149,#27150,#27151,#27152),.UNSPECIFIED.,.F.,.F.,(4,1,1,
1,1,1,1,1,4),(-225.843951449422,-225.727083251571,-224.728290847803,-223.729498444035,
-222.730706040267,-221.731913636499,-220.733121232731,-219.734328828963,
-219.560766142242),.UNSPECIFIED.);
#699=B_SPLINE_CURVE_WITH_KNOTS('',3,(#27154,#27155,#27156,#27157,#27158,
#27159,#27160,#27161,#27162,#27163,#27164,#27165,#27166,#27167,#27168,#27169,
#27170,#27171,#27172,#27173,#27174,#27175,#27176,#27177,#27178,#27179,#27180,
#27181,#27182,#27183,#27184,#27185,#27186,#27187,#27188,#27189,#27190,#27191,
#27192,#27193,#27194,#27195,#27196,#27197,#27198,#27199,#27200,#27201,#27202,
#27203,#27204,#27205,#27206,#27207,#27208,#27209,#27210,#27211,#27212,#27213,
#27214,#27215,#27216,#27217,#27218,#27219,#27220,#27221,#27222,#27223,#27224,
#27225,#27226,#27227,#27228,#27229,#27230,#27231,#27232,#27233,#27234,#27235,
#27236,#27237,#27238,#27239,#27240,#27241,#27242,#27243,#27244,#27245,#27246,
#27247,#27248,#27249,#27250,#27251,#27252,#27253,#27254,#27255,#27256,#27257,
#27258,#27259,#27260,#27261,#27262,#27263,#27264,#27265,#27266,#27267,#27268,
#27269,#27270,#27271,#27272,#27273,#27274,#27275,#27276,#27277,#27278,#27279,
#27280,#27281,#27282,#27283,#27284,#27285,#27286),.UNSPECIFIED.,.F.,.F.,
(4,3,3,3,3,3,3,3,3,3,3,3,3,3,3,3,3,3,3,3,3,3,3,3,3,3,3,3,3,3,3,3,3,3,3,
3,3,3,3,3,3,3,3,3,4),(-219.560766142242,-219.405885364159,-219.251206515928,
-219.096480412599,-218.941724077899,-218.786644708032,-218.735536425195,
-218.578110566755,-218.420974310144,-218.264006815405,-218.106958706252,
-217.949862612054,-217.792426951084,-217.736744021427,-217.579318162987,
-217.422181906376,-217.265214411637,-217.108166302484,-216.951070208286,
-216.793634547316,-216.737951617659,-216.580525759219,-216.423389502608,
-216.266422007869,-216.109373898716,-215.952277804518,-215.794842143548,
-215.739159213891,-215.581733355451,-215.42459709884,-215.267629604101,
-215.110581494948,-214.95348540075,-214.79604973978,-214.740366810123,-214.582940951683,
-214.425804695073,-214.268837200334,-214.111789091181,-213.954692996983,
-213.797257336014,-213.741574406355,-213.573311654301,-213.405853618667,
-213.277581026691),.UNSPECIFIED.);
#700=B_SPLINE_CURVE_WITH_KNOTS('',3,(#27288,#27289,#27290,#27291,#27292,
#27293,#27294,#27295,#27296,#27297),.UNSPECIFIED.,.F.,.F.,(4,1,1,1,1,1,
1,4),(-213.277580835062,-212.742782002587,-211.743989598819,-210.745197195051,
-209.746404791283,-208.747612387515,-207.748819983747,-206.994395527883),
 .UNSPECIFIED.);
#701=B_SPLINE_CURVE_WITH_KNOTS('',3,(#27299,#27300,#27301,#27302,#27303,
#27304,#27305,#27306,#27307,#27308,#27309,#27310,#27311,#27312,#27313,#27314,
#27315,#27316,#27317,#27318,#27319,#27320,#27321,#27322,#27323,#27324,#27325,
#27326,#27327,#27328,#27329,#27330,#27331,#27332,#27333,#27334,#27335,#27336,
#27337,#27338,#27339,#27340,#27341,#27342,#27343,#27344,#27345,#27346,#27347,
#27348,#27349,#27350,#27351,#27352,#27353,#27354,#27355,#27356,#27357,#27358,
#27359,#27360,#27361,#27362,#27363,#27364,#27365,#27366,#27367,#27368,#27369,
#27370,#27371,#27372,#27373,#27374,#27375,#27376,#27377,#27378,#27379,#27380,
#27381,#27382,#27383,#27384,#27385,#27386,#27387,#27388,#27389,#27390,#27391,
#27392,#27393,#27394,#27395,#27396,#27397,#27398,#27399,#27400,#27401,#27402,
#27403,#27404,#27405,#27406,#27407,#27408,#27409,#27410,#27411,#27412,#27413,
#27414,#27415,#27416,#27417,#27418,#27419,#27420,#27421,#27422,#27423,#27424,
#27425,#27426,#27427,#27428,#27429,#27430,#27431,#27432,#27433,#27434),
 .UNSPECIFIED.,.F.,.F.,(4,3,3,3,3,3,3,3,3,3,3,3,3,3,3,3,3,3,3,3,3,3,3,3,
3,3,3,3,3,3,3,3,3,3,3,3,3,3,3,3,3,3,3,3,3,4),(-206.994395456771,-206.788485113507,
-206.750027579979,-206.592601721539,-206.435465464928,-206.278497970189,
-206.121449861036,-205.964353766838,-205.806918105868,-205.751235176211,
-205.593809317771,-205.43667306116,-205.279705566421,-205.122657457268,
-204.96556136307,-204.8081257021,-204.752442772443,-204.595016914003,-204.437880657392,
-204.280913162653,-204.1238650535,-203.966768959303,-203.809333298333,-203.753650368675,
-203.596224510235,-203.439088253624,-203.282120758885,-203.125072649732,
-202.967976555534,-202.810540894564,-202.754857964907,-202.597432106467,
-202.440295849856,-202.283328355117,-202.126280245964,-201.969184151766,
-201.811748490796,-201.756065561139,-201.598639702699,-201.441503446089,
-201.28453595135,-201.127487842197,-200.970391748,-200.81295608703,-200.757273157371,
-200.711210220703),.UNSPECIFIED.);
#702=B_SPLINE_CURVE_WITH_KNOTS('',3,(#27436,#27437,#27438,#27439,#27440,
#27441,#27442,#27443,#27444,#27445,#27446,#27447,#27448,#27449,#27450,#27451,
#27452,#27453,#27454,#27455,#27456,#27457,#27458,#27459,#27460,#27461,#27462,
#27463,#27464,#27465,#27466,#27467,#27468,#27469,#27470,#27471,#27472,#27473,
#27474,#27475,#27476,#27477,#27478,#27479,#27480,#27481,#27482,#27483,#27484,
#27485,#27486,#27487,#27488,#27489,#27490,#27491,#27492,#27493,#27494,#27495,
#27496,#27497,#27498,#27499,#27500,#27501,#27502,#27503,#27504,#27505,#27506,
#27507,#27508,#27509,#27510,#27511,#27512,#27513,#27514,#27515,#27516,#27517,
#27518,#27519,#27520,#27521,#27522,#27523,#27524,#27525,#27526,#27527,#27528,
#27529,#27530,#27531,#27532,#27533,#27534,#27535,#27536,#27537,#27538,#27539,
#27540,#27541,#27542,#27543,#27544,#27545,#27546,#27547,#27548,#27549,#27550,
#27551,#27552,#27553,#27554,#27555,#27556,#27557,#27558,#27559,#27560,#27561,
#27562,#27563,#27564,#27565),.UNSPECIFIED.,.F.,.F.,(4,3,3,3,3,3,3,3,3,3,
3,3,3,3,3,3,3,3,3,3,3,3,3,3,3,3,3,3,3,3,3,3,3,3,3,3,3,3,3,3,3,3,3,4),(-200.71121022055,
-200.554927857576,-200.39892543186,-200.238814262296,-200.08287729828,-199.920679025941,
-199.758480753603,-199.601054895162,-199.443918638552,-199.286951143813,
-199.129903034659,-198.972806940462,-198.815371279492,-198.759688349835,
-198.602262491394,-198.445126234784,-198.288158740045,-198.131110630891,
-197.974014536694,-197.816578875724,-197.760895946067,-197.603470087627,
-197.446333831017,-197.289366336277,-197.132318227124,-196.975222132927,
-196.817786471957,-196.762103542299,-196.604677683859,-196.447541427248,
-196.290573932509,-196.133525823356,-195.976429729158,-195.818994068188,
-195.763311138531,-195.605885280091,-195.44874902348,-195.291781528741,
-195.134733419588,-194.97763732539,-194.82020166442,-194.764518734763,-194.581155261081,
-194.428024913746),.UNSPECIFIED.);
#703=B_SPLINE_CURVE_WITH_KNOTS('',3,(#27567,#27568,#27569,#27570,#27571,
#27572,#27573,#27574,#27575,#27576,#27577,#27578,#27579,#27580,#27581,#27582,
#27583,#27584,#27585,#27586,#27587,#27588,#27589,#27590,#27591,#27592,#27593,
#27594,#27595,#27596,#27597,#27598,#27599,#27600,#27601,#27602,#27603,#27604,
#27605,#27606,#27607,#27608,#27609,#27610,#27611,#27612,#27613,#27614,#27615,
#27616,#27617,#27618,#27619,#27620,#27621,#27622,#27623,#27624,#27625,#27626,
#27627,#27628,#27629,#27630,#27631,#27632,#27633,#27634,#27635,#27636,#27637,
#27638,#27639,#27640,#27641,#27642,#27643,#27644,#27645,#27646,#27647,#27648,
#27649,#27650,#27651,#27652,#27653,#27654,#27655,#27656,#27657,#27658,#27659,
#27660,#27661,#27662,#27663,#27664,#27665,#27666,#27667,#27668,#27669,#27670,
#27671,#27672,#27673,#27674,#27675,#27676,#27677,#27678,#27679,#27680,#27681,
#27682,#27683,#27684,#27685,#27686,#27687,#27688,#27689,#27690,#27691,#27692,
#27693,#27694,#27695,#27696,#27697,#27698,#27699),.UNSPECIFIED.,.F.,.F.,
(4,3,3,3,3,3,3,3,3,3,3,3,3,3,3,3,3,3,3,3,3,3,3,3,3,3,3,3,3,3,3,3,3,3,3,
3,3,3,3,3,3,3,3,3,4),(-194.428024913524,-194.271102313192,-194.114059104038,
-193.956937816817,-193.799462526794,-193.765726330995,-193.608300472555,
-193.451164215944,-193.294196721205,-193.137148612052,-192.980052517854,
-192.822616856884,-192.766933927227,-192.609508068787,-192.452371812176,
-192.295404317437,-192.138356208284,-191.981260114086,-191.823824453116,
-191.768141523459,-191.610715665019,-191.453579408408,-191.296611913669,
-191.139563804516,-190.982467710318,-190.825032049348,-190.769349119691,
-190.611923261251,-190.45478700464,-190.297819509901,-190.140771400748,
-189.98367530655,-189.82623964558,-189.770556715923,-189.613130857483,-189.455994600873,
-189.299027106134,-189.14197899698,-188.984882902783,-188.827447241813,
-188.771764312155,-188.613149272119,-188.454850209973,-188.296688673262,
-188.144839606344),.UNSPECIFIED.);
#704=B_SPLINE_CURVE_WITH_KNOTS('',3,(#27701,#27702,#27703,#27704,#27705,
#27706,#27707,#27708,#27709,#27710),.UNSPECIFIED.,.F.,.F.,(4,1,1,1,1,1,
1,4),(-188.144832027655,-187.772971908386,-186.774179504619,-185.775387100851,
-184.776594697082,-183.777802293314,-182.779009889546,-181.861662808607),
 .UNSPECIFIED.);
#705=B_SPLINE_CURVE_WITH_KNOTS('',3,(#27712,#27713,#27714,#27715,#27716,
#27717,#27718,#27719,#27720,#27721,#27722,#27723,#27724,#27725,#27726,#27727,
#27728,#27729,#27730,#27731,#27732,#27733,#27734,#27735,#27736,#27737,#27738,
#27739,#27740,#27741,#27742,#27743,#27744,#27745,#27746,#27747,#27748,#27749,
#27750,#27751,#27752,#27753,#27754,#27755,#27756,#27757,#27758,#27759,#27760,
#27761,#27762,#27763,#27764,#27765,#27766,#27767,#27768,#27769,#27770,#27771,
#27772,#27773,#27774,#27775,#27776,#27777,#27778,#27779,#27780,#27781,#27782,
#27783,#27784,#27785,#27786,#27787,#27788,#27789,#27790,#27791,#27792,#27793,
#27794,#27795,#27796,#27797,#27798,#27799,#27800,#27801,#27802,#27803,#27804,
#27805,#27806,#27807,#27808,#27809,#27810,#27811,#27812,#27813,#27814,#27815,
#27816,#27817,#27818,#27819,#27820,#27821,#27822,#27823,#27824,#27825,#27826,
#27827,#27828,#27829,#27830,#27831,#27832,#27833,#27834,#27835,#27836,#27837,
#27838,#27839,#27840,#27841,#27842,#27843,#27844),.UNSPECIFIED.,.F.,.F.,
(4,3,3,3,3,3,3,3,3,3,3,3,3,3,3,3,3,3,3,3,3,3,3,3,3,3,3,3,3,3,3,3,3,3,3,
3,3,3,3,3,3,3,3,3,4),(-181.861654299165,-181.780217485778,-181.622791627338,
-181.465655370728,-181.308687875988,-181.151639766835,-180.994543672638,
-180.837108011668,-180.78142508201,-180.62399922357,-180.466862966959,-180.30989547222,
-180.152847363067,-179.995751268869,-179.838315607899,-179.782632678242,
-179.625206819802,-179.468070563191,-179.311103068452,-179.154054959299,
-178.996958865101,-178.839523204131,-178.783840274474,-178.626414416034,
-178.469278159423,-178.312310664684,-178.155262555531,-177.998166461333,
-177.840730800363,-177.785047870706,-177.627622012266,-177.470485755655,
-177.313518260916,-177.156470151763,-176.999374057565,-176.841938396595,
-176.786255466938,-176.628829608497,-176.471693351887,-176.314725857148,
-176.157677747994,-176.000581653797,-175.843145992827,-175.78746306317,
-175.578468991985),.UNSPECIFIED.);
#706=B_SPLINE_CURVE_WITH_KNOTS('',3,(#27846,#27847,#27848,#27849,#27850,
#27851,#27852,#27853,#27854,#27855),.UNSPECIFIED.,.F.,.F.,(4,1,1,1,1,1,
1,4),(-175.578466593548,-174.788670659402,-173.789878255634,-172.791085851866,
-171.792293448098,-170.79350104433,-169.794708640562,-169.295283684806),
 .UNSPECIFIED.);
#707=B_SPLINE_CURVE_WITH_KNOTS('',3,(#27857,#27858,#27859,#27860,#27861,
#27862,#27863,#27864,#27865,#27866),.UNSPECIFIED.,.F.,.F.,(4,1,1,1,1,1,
1,4),(-169.295283684806,-168.795916236794,-167.797123833026,-166.798331429258,
-165.79953902549,-164.800746621722,-163.801954217954,-163.012100781783),
 .UNSPECIFIED.);
#708=B_SPLINE_CURVE_WITH_KNOTS('',3,(#27868,#27869,#27870,#27871,#27872,
#27873,#27874,#27875,#27876,#27877,#27878,#27879,#27880,#27881,#27882,#27883,
#27884,#27885,#27886,#27887,#27888,#27889,#27890,#27891,#27892,#27893,#27894,
#27895,#27896,#27897,#27898,#27899,#27900,#27901,#27902,#27903,#27904,#27905,
#27906,#27907,#27908,#27909,#27910,#27911,#27912,#27913,#27914,#27915,#27916,
#27917,#27918,#27919,#27920,#27921,#27922,#27923,#27924,#27925,#27926,#27927,
#27928,#27929,#27930,#27931,#27932,#27933,#27934,#27935,#27936,#27937,#27938,
#27939,#27940,#27941,#27942,#27943,#27944,#27945,#27946,#27947,#27948,#27949,
#27950,#27951,#27952,#27953,#27954,#27955,#27956,#27957,#27958,#27959,#27960,
#27961,#27962,#27963,#27964,#27965,#27966,#27967,#27968,#27969,#27970,#27971,
#27972,#27973,#27974,#27975,#27976,#27977,#27978,#27979,#27980,#27981,#27982,
#27983,#27984,#27985,#27986,#27987,#27988,#27989,#27990,#27991,#27992,#27993,
#27994,#27995,#27996,#27997,#27998,#27999,#28000),.UNSPECIFIED.,.F.,.F.,
(4,3,3,3,3,3,3,3,3,3,3,3,3,3,3,3,3,3,3,3,3,3,3,3,3,3,3,3,3,3,3,3,3,3,3,
3,3,3,3,3,3,3,3,3,4),(-163.012098377626,-162.803161814186,-162.645735955746,
-162.488599699136,-162.331632204397,-162.174584095244,-162.017488001047,
-161.860052340077,-161.804369410418,-161.646943551978,-161.489807295367,
-161.332839800628,-161.175791691475,-161.018695597277,-160.861259936307,
-160.80557700665,-160.64815114821,-160.491014891599,-160.33404739686,-160.176999287707,
-160.019903193509,-159.862467532539,-159.806784602882,-159.649358744442,
-159.492222487831,-159.335254993092,-159.178206883939,-159.021110789741,
-158.863675128771,-158.807992199114,-158.650566340674,-158.493430084063,
-158.336462589324,-158.179414480171,-158.022318385973,-157.864882725003,
-157.809199795346,-157.651773936906,-157.494637680296,-157.337670185556,
-157.180622076403,-157.023525982206,-156.866090321236,-156.810407391578,
-156.728913070446),.UNSPECIFIED.);
#709=B_SPLINE_CURVE_WITH_KNOTS('',3,(#28002,#28003,#28004,#28005,#28006,
#28007,#28008,#28009,#28010,#28011),.UNSPECIFIED.,.F.,.F.,(4,1,1,1,1,1,
1,4),(-156.728904558766,-155.81161498781,-154.812822584042,-153.814030180274,
-152.815237776506,-151.816445372738,-150.81765296897,-150.445735341375),
 .UNSPECIFIED.);
#710=B_SPLINE_CURVE_WITH_KNOTS('',3,(#28013,#28014,#28015,#28016,#28017,
#28018,#28019,#28020,#28021,#28022,#28023,#28024,#28025,#28026,#28027,#28028,
#28029,#28030,#28031,#28032,#28033,#28034,#28035,#28036,#28037,#28038,#28039,
#28040,#28041,#28042,#28043,#28044,#28045,#28046,#28047,#28048,#28049,#28050,
#28051,#28052,#28053,#28054,#28055,#28056,#28057,#28058,#28059,#28060,#28061,
#28062,#28063,#28064,#28065,#28066,#28067,#28068,#28069,#28070,#28071,#28072,
#28073,#28074,#28075,#28076,#28077,#28078,#28079,#28080,#28081,#28082,#28083,
#28084,#28085,#28086,#28087,#28088,#28089,#28090,#28091,#28092,#28093,#28094,
#28095,#28096,#28097,#28098,#28099,#28100,#28101,#28102,#28103,#28104,#28105,
#28106,#28107,#28108,#28109,#28110,#28111,#28112,#28113,#28114,#28115,#28116,
#28117,#28118,#28119,#28120,#28121,#28122,#28123,#28124,#28125,#28126,#28127,
#28128,#28129,#28130,#28131,#28132,#28133,#28134,#28135,#28136,#28137,#28138,
#28139,#28140,#28141,#28142,#28143,#28144,#28145),.UNSPECIFIED.,.F.,.F.,
(4,3,3,3,3,3,3,3,3,3,3,3,3,3,3,3,3,3,3,3,3,3,3,3,3,3,3,3,3,3,3,3,3,3,3,
3,3,3,3,3,3,3,3,3,4),(-150.445727763267,-150.287559345543,-150.12936657424,
-149.970749373709,-149.818860565202,-149.661434706762,-149.504298450152,
-149.347330955412,-149.190282846259,-149.033186752062,-148.875751091092,
-148.820068161434,-148.662642302994,-148.505506046383,-148.348538551644,
-148.191490442491,-148.034394348293,-147.876958687323,-147.821275757666,
-147.663849899226,-147.506713642615,-147.349746147876,-147.192698038723,
-147.035601944525,-146.878166283555,-146.822483353898,-146.665057495458,
-146.507921238847,-146.350953744108,-146.193905634955,-146.036809540757,
-145.879373879787,-145.82369095013,-145.66626509169,-145.50912883508,-145.35216134034,
-145.195113231187,-145.03801713699,-144.88058147602,-144.824898546362,-144.659309523793,
-144.502171753509,-144.345219652649,-144.188289944736,-144.162542456087),
 .UNSPECIFIED.);
#711=B_SPLINE_CURVE_WITH_KNOTS('',3,(#28147,#28148,#28149,#28150,#28151,
#28152,#28153,#28154,#28155,#28156,#28157,#28158,#28159,#28160,#28161,#28162,
#28163,#28164,#28165,#28166,#28167,#28168,#28169,#28170,#28171,#28172,#28173,
#28174,#28175,#28176,#28177,#28178,#28179,#28180,#28181,#28182,#28183,#28184,
#28185,#28186,#28187,#28188,#28189,#28190,#28191,#28192,#28193,#28194,#28195,
#28196,#28197,#28198,#28199,#28200,#28201,#28202,#28203,#28204,#28205,#28206,
#28207,#28208,#28209,#28210,#28211,#28212,#28213,#28214,#28215,#28216,#28217,
#28218,#28219,#28220,#28221,#28222,#28223,#28224,#28225,#28226,#28227,#28228,
#28229,#28230,#28231,#28232,#28233,#28234,#28235,#28236,#28237,#28238,#28239,
#28240,#28241,#28242,#28243,#28244,#28245,#28246,#28247,#28248,#28249,#28250,
#28251,#28252,#28253,#28254,#28255,#28256,#28257,#28258,#28259,#28260,#28261,
#28262,#28263,#28264,#28265,#28266,#28267,#28268,#28269,#28270,#28271,#28272,
#28273,#28274,#28275,#28276),.UNSPECIFIED.,.F.,.F.,(4,3,3,3,3,3,3,3,3,3,
3,3,3,3,3,3,3,3,3,3,3,3,3,3,3,3,3,3,3,3,3,3,3,3,3,3,3,3,3,3,3,3,3,4),(-144.162542455865,
-143.979169095402,-143.826106142594,-143.668680284153,-143.511544027543,
-143.354576532803,-143.197528423649,-143.040432329451,-142.882996668481,
-142.827313738826,-142.669887880386,-142.512751623775,-142.355784129036,
-142.198736019883,-142.041639925685,-141.884204264715,-141.828521335058,
-141.671095476618,-141.513959220008,-141.356991725268,-141.199943616115,
-141.042847521918,-140.885411860948,-140.82972893129,-140.67230307285,-140.515166816239,
-140.3581993215,-140.201151212347,-140.044055118149,-139.886619457179,-139.830936527522,
-139.673510669082,-139.516374412471,-139.359406917732,-139.202358808579,
-139.045262714381,-138.887827053411,-138.832144123754,-138.675840847802,
-138.519825091293,-138.359708105736,-138.203776393364,-138.041566771214,
-137.879357149064),.UNSPECIFIED.);
#712=B_SPLINE_CURVE_WITH_KNOTS('',3,(#28278,#28279,#28280,#28281,#28282,
#28283,#28284,#28285,#28286,#28287,#28288,#28289,#28290,#28291,#28292,#28293,
#28294,#28295,#28296,#28297,#28298,#28299,#28300,#28301,#28302,#28303,#28304,
#28305,#28306,#28307,#28308,#28309,#28310,#28311,#28312,#28313,#28314,#28315,
#28316,#28317,#28318,#28319,#28320,#28321,#28322,#28323,#28324,#28325,#28326,
#28327,#28328,#28329,#28330,#28331,#28332,#28333,#28334,#28335,#28336,#28337,
#28338,#28339,#28340,#28341,#28342,#28343,#28344,#28345,#28346,#28347,#28348,
#28349,#28350,#28351,#28352,#28353,#28354,#28355,#28356,#28357,#28358,#28359,
#28360,#28361,#28362,#28363,#28364,#28365,#28366,#28367,#28368,#28369,#28370,
#28371,#28372,#28373,#28374,#28375,#28376,#28377,#28378,#28379,#28380,#28381,
#28382,#28383,#28384,#28385,#28386,#28387,#28388,#28389,#28390,#28391,#28392,
#28393,#28394,#28395,#28396,#28397,#28398,#28399,#28400,#28401,#28402,#28403,
#28404,#28405,#28406,#28407,#28408,#28409,#28410,#28411,#28412,#28413),
 .UNSPECIFIED.,.F.,.F.,(4,3,3,3,3,3,3,3,3,3,3,3,3,3,3,3,3,3,3,3,3,3,3,3,
3,3,3,3,3,3,3,3,3,3,3,3,3,3,3,3,3,3,3,3,3,4),(-137.879357148908,-137.833351719986,
-137.675925861546,-137.518789604935,-137.361822110196,-137.204774001043,
-137.047677906846,-136.890242245876,-136.834559316218,-136.677133457778,
-136.519997201167,-136.363029706428,-136.205981597275,-136.048885503077,
-135.891449842107,-135.83576691245,-135.67834105401,-135.521204797399,-135.36423730266,
-135.207189193507,-135.050093099309,-134.892657438339,-134.836974508682,
-134.679548650242,-134.522412393631,-134.365444898892,-134.208396789739,
-134.051300695541,-133.893865034571,-133.838182104914,-133.680756246474,
-133.523619989863,-133.366652495124,-133.209604385971,-133.052508291773,
-132.895072630803,-132.839389701146,-132.681963842706,-132.524827586096,
-132.367860091357,-132.210811982203,-132.053715888006,-131.896280227036,
-131.840597297378,-131.634707085204,-131.596171913192),.UNSPECIFIED.);
#713=B_SPLINE_CURVE_WITH_KNOTS('',3,(#28415,#28416,#28417,#28418,#28419,
#28420,#28421,#28422,#28423,#28424),.UNSPECIFIED.,.F.,.F.,(4,1,1,1,1,1,
1,4),(-131.596171841728,-130.84180489361,-129.843012489842,-128.844220086074,
-127.845427682306,-126.846635278538,-125.84784287477,-125.312986534549),
 .UNSPECIFIED.);
#714=B_SPLINE_CURVE_WITH_KNOTS('',3,(#28426,#28427,#28428,#28429,#28430,
#28431,#28432,#28433,#28434,#28435,#28436,#28437,#28438,#28439,#28440,#28441,
#28442,#28443,#28444,#28445,#28446,#28447,#28448,#28449,#28450,#28451,#28452,
#28453,#28454,#28455,#28456,#28457,#28458,#28459,#28460,#28461,#28462,#28463,
#28464,#28465,#28466,#28467,#28468,#28469,#28470,#28471,#28472,#28473,#28474,
#28475,#28476,#28477,#28478,#28479,#28480,#28481,#28482,#28483,#28484,#28485,
#28486,#28487,#28488,#28489,#28490,#28491,#28492,#28493,#28494,#28495,#28496,
#28497,#28498,#28499,#28500,#28501,#28502,#28503,#28504,#28505,#28506,#28507,
#28508,#28509,#28510,#28511,#28512,#28513,#28514,#28515,#28516,#28517,#28518,
#28519,#28520,#28521,#28522,#28523,#28524,#28525,#28526,#28527,#28528,#28529,
#28530,#28531,#28532,#28533,#28534,#28535,#28536,#28537,#28538,#28539,#28540,
#28541,#28542,#28543,#28544,#28545,#28546,#28547,#28548,#28549,#28550,#28551,
#28552,#28553,#28554,#28555,#28556,#28557,#28558),.UNSPECIFIED.,.F.,.F.,
(4,3,3,3,3,3,3,3,3,3,3,3,3,3,3,3,3,3,3,3,3,3,3,3,3,3,3,3,3,3,3,3,3,3,3,
3,3,3,3,3,3,3,3,3,4),(-125.312986342626,-125.145692167388,-124.977524770016,
-124.849050471002,-124.691624612562,-124.534488355952,-124.377520861213,
-124.220472752059,-124.063376657862,-123.905940996892,-123.850258067234,
-123.692832208794,-123.535695952183,-123.378728457444,-123.221680348291,
-123.064584254093,-122.907148593123,-122.851465663466,-122.694039805026,
-122.536903548415,-122.379936053676,-122.222887944523,-122.065791850325,
-121.908356189355,-121.852673259698,-121.695247401258,-121.538111144647,
-121.381143649908,-121.224095540755,-121.066999446557,-120.909563785587,
-120.85388085593,-120.69645499749,-120.539318740879,-120.38235124614,-120.225303136987,
-120.06820704279,-119.91077138182,-119.855088452162,-119.70000916941,-119.545219027811,
-119.390509726915,-119.235844442665,-119.080963609224,-119.029801227369),
 .UNSPECIFIED.);
#715=B_SPLINE_CURVE_WITH_KNOTS('',3,(#28560,#28561,#28562,#28563,#28564,
#28565,#28566,#28567,#28568,#28569,#28570),.UNSPECIFIED.,.F.,.F.,(4,1,1,
1,1,1,1,1,4),(-119.029801227369,-118.856296048394,-117.857503644626,-116.858711240858,
-115.85991883709,-114.861126433322,-113.862334029554,-112.863541625786,
-112.746615920189),.UNSPECIFIED.);
#716=B_SPLINE_CURVE_WITH_KNOTS('',3,(#28572,#28573,#28574,#28575,#28576,
#28577,#28578,#28579,#28580,#28581,#28582,#28583,#28584,#28585,#28586,#28587,
#28588,#28589,#28590,#28591,#28592,#28593,#28594,#28595,#28596,#28597,#28598,
#28599,#28600,#28601,#28602,#28603,#28604,#28605,#28606,#28607,#28608,#28609,
#28610,#28611,#28612,#28613,#28614,#28615,#28616,#28617,#28618,#28619,#28620,
#28621,#28622,#28623,#28624,#28625,#28626,#28627,#28628,#28629,#28630,#28631,
#28632,#28633,#28634,#28635,#28636,#28637,#28638,#28639,#28640,#28641,#28642,
#28643,#28644,#28645,#28646,#28647,#28648,#28649,#28650,#28651,#28652,#28653,
#28654,#28655,#28656,#28657,#28658,#28659,#28660,#28661,#28662,#28663,#28664,
#28665,#28666,#28667,#28668,#28669,#28670,#28671,#28672,#28673,#28674,#28675,
#28676,#28677,#28678,#28679,#28680,#28681,#28682,#28683,#28684,#28685,#28686,
#28687,#28688,#28689,#28690,#28691,#28692,#28693,#28694,#28695,#28696,#28697,
#28698,#28699,#28700,#28701,#28702,#28703,#28704),.UNSPECIFIED.,.F.,.F.,
(4,3,3,3,3,3,3,3,3,3,3,3,3,3,3,3,3,3,3,3,3,3,3,3,3,3,3,3,3,3,3,3,3,3,3,
3,3,3,3,3,3,3,3,3,4),(-112.746615920189,-112.591427658643,-112.436483398331,
-112.281528987221,-112.126582709523,-111.971296091352,-111.864749222017,
-111.707323363577,-111.550187106966,-111.393219612227,-111.236171503074,
-111.079075408876,-110.921639747906,-110.865956818249,-110.708530959809,
-110.551394703198,-110.394427208459,-110.237379099306,-110.080283005108,
-109.922847344138,-109.867164414481,-109.709738556041,-109.55260229943,
-109.395634804691,-109.238586695538,-109.08149060134,-108.92405494037,-108.868372010713,
-108.710946152273,-108.553809895662,-108.396842400923,-108.23979429177,
-108.082698197572,-107.925262536602,-107.869579606945,-107.712153748504,
-107.555017491894,-107.398049997155,-107.241001888001,-107.083905793803,
-106.926470132833,-106.870787203177,-106.696751389778,-106.523937038518,
-106.463430825477),.UNSPECIFIED.);
#717=B_SPLINE_CURVE_WITH_KNOTS('',3,(#28706,#28707,#28708,#28709,#28710,
#28711,#28712,#28713,#28714,#28715),.UNSPECIFIED.,.F.,.F.,(4,1,1,1,1,1,
1,4),(-106.46343061301,-105.871994799409,-104.873202395641,-103.874409991873,
-102.875617588105,-101.876825184337,-100.878032780569,-100.18024530583),
 .UNSPECIFIED.);
#718=B_SPLINE_CURVE_WITH_KNOTS('',3,(#28717,#28718,#28719,#28720,#28721,
#28722,#28723,#28724,#28725,#28726,#28727,#28728,#28729,#28730,#28731,#28732,
#28733,#28734,#28735,#28736,#28737,#28738,#28739,#28740,#28741,#28742,#28743,
#28744,#28745,#28746,#28747,#28748,#28749,#28750,#28751,#28752,#28753,#28754,
#28755,#28756,#28757,#28758,#28759,#28760,#28761,#28762,#28763,#28764,#28765,
#28766,#28767,#28768,#28769,#28770,#28771,#28772,#28773,#28774,#28775,#28776,
#28777,#28778,#28779,#28780,#28781,#28782,#28783,#28784,#28785,#28786,#28787,
#28788,#28789,#28790,#28791,#28792,#28793,#28794,#28795,#28796,#28797,#28798,
#28799,#28800,#28801,#28802,#28803,#28804,#28805,#28806,#28807,#28808,#28809,
#28810,#28811,#28812,#28813,#28814,#28815,#28816,#28817,#28818,#28819,#28820,
#28821,#28822,#28823,#28824,#28825,#28826,#28827,#28828,#28829,#28830,#28831,
#28832,#28833,#28834,#28835,#28836,#28837,#28838,#28839,#28840,#28841,#28842,
#28843,#28844,#28845,#28846,#28847,#28848,#28849),.UNSPECIFIED.,.F.,.F.,
(4,3,3,3,3,3,3,3,3,3,3,3,3,3,3,3,3,3,3,3,3,3,3,3,3,3,3,3,3,3,3,3,3,3,3,
3,3,3,3,3,3,3,3,3,4),(-100.180245122334,-99.9899960061537,-99.8792403768013,
-99.7218145183607,-99.5646782617502,-99.4077107670109,-99.2506626578573,
-99.0935665636596,-98.9361309026894,-98.8804479730333,-98.7230221145929,
-98.5658858579827,-98.4089183632435,-98.2518702540902,-98.0947741598927,
-97.9373384989227,-97.8816555692653,-97.7242297108249,-97.5670934542147,
-97.4101259594756,-97.2530778503222,-97.0959817561248,-96.9385460951547,
-96.8828631654973,-96.7254373070569,-96.5683010504466,-96.4113335557074,
-96.254285446554,-96.0971893523565,-95.9397536913864,-95.8840707617293,
-95.7266449032889,-95.5695086466786,-95.4125411519395,-95.2554930427861,
-95.0983969485886,-94.9409612876185,-94.8852783579613,-94.728144675395,
-94.571300053841,-94.4146226728758,-94.2578641017484,-94.1010543235121,
-93.9439094261303,-93.8970599988234),.UNSPECIFIED.);
#719=B_SPLINE_CURVE_WITH_KNOTS('',3,(#28851,#28852,#28853,#28854,#28855,
#28856,#28857,#28858,#28859,#28860,#28861,#28862,#28863,#28864,#28865,#28866,
#28867,#28868,#28869,#28870,#28871,#28872,#28873,#28874,#28875,#28876,#28877,
#28878,#28879,#28880,#28881,#28882,#28883,#28884,#28885,#28886,#28887,#28888,
#28889,#28890,#28891,#28892,#28893,#28894,#28895,#28896,#28897,#28898,#28899,
#28900,#28901,#28902,#28903,#28904,#28905,#28906,#28907,#28908,#28909,#28910,
#28911,#28912,#28913,#28914,#28915,#28916,#28917,#28918,#28919,#28920,#28921,
#28922,#28923,#28924,#28925,#28926,#28927,#28928,#28929,#28930,#28931,#28932,
#28933,#28934,#28935,#28936,#28937,#28938,#28939,#28940,#28941,#28942,#28943,
#28944,#28945,#28946,#28947,#28948,#28949,#28950,#28951,#28952,#28953,#28954,
#28955,#28956,#28957,#28958,#28959,#28960,#28961,#28962,#28963,#28964,#28965,
#28966,#28967,#28968,#28969,#28970,#28971,#28972,#28973,#28974,#28975,#28976,
#28977,#28978,#28979,#28980,#28981,#28982,#28983,#28984,#28985,#28986),
 .UNSPECIFIED.,.F.,.F.,(4,3,3,3,3,3,3,3,3,3,3,3,3,3,3,3,3,3,3,3,3,3,3,3,
3,3,3,3,3,3,3,3,3,3,3,3,3,3,3,3,3,3,3,3,3,4),(-93.8970599986506,-93.8864859541932,
-93.7290600957528,-93.5719238391426,-93.4149563444034,-93.25790823525,-93.1008121410525,
-92.9433764800825,-92.8876935504252,-92.7302676919848,-92.5731314353745,
-92.4161639406354,-92.259115831482,-92.1020197372846,-91.9445840763145,
-91.8889011466572,-91.7314752882168,-91.5743390316065,-91.4173715368674,
-91.260323427714,-91.1032273335165,-90.9457916725464,-90.8901087428892,
-90.7326828844488,-90.5755466278386,-90.4185791330994,-90.261531023946,
-90.1044349297486,-89.9469992687786,-89.8913163391212,-89.7338904806808,
-89.5767542240706,-89.4197867293314,-89.262738620178,-89.1056425259805,
-88.9482068650105,-88.8925239353532,-88.7350980769127,-88.5779618203025,
-88.4209943255633,-88.2639462164099,-88.1068501222124,-87.9494144612423,
-87.8937315315851,-87.6984636965869,-87.6138746916003),.UNSPECIFIED.);
#720=B_SPLINE_CURVE_WITH_KNOTS('',3,(#28988,#28989,#28990,#28991,#28992,
#28993,#28994,#28995,#28996,#28997,#28998,#28999,#29000,#29001,#29002,#29003,
#29004,#29005,#29006,#29007,#29008,#29009,#29010,#29011,#29012,#29013,#29014,
#29015,#29016,#29017,#29018,#29019,#29020,#29021,#29022,#29023,#29024,#29025,
#29026,#29027,#29028,#29029,#29030,#29031,#29032,#29033,#29034,#29035,#29036,
#29037,#29038,#29039,#29040,#29041,#29042,#29043,#29044,#29045,#29046,#29047,
#29048,#29049,#29050,#29051,#29052,#29053,#29054,#29055,#29056,#29057,#29058,
#29059,#29060,#29061,#29062,#29063,#29064,#29065,#29066,#29067,#29068,#29069,
#29070,#29071,#29072,#29073,#29074,#29075,#29076,#29077,#29078,#29079,#29080,
#29081,#29082,#29083,#29084,#29085,#29086,#29087,#29088,#29089,#29090,#29091,
#29092,#29093,#29094,#29095,#29096,#29097,#29098,#29099,#29100,#29101,#29102,
#29103,#29104,#29105,#29106,#29107,#29108,#29109,#29110,#29111,#29112,#29113,
#29114,#29115,#29116,#29117,#29118,#29119,#29120),.UNSPECIFIED.,.F.,.F.,
(4,3,3,3,3,3,3,3,3,3,3,3,3,3,3,3,3,3,3,3,3,3,3,3,3,3,3,3,3,3,3,3,3,3,3,
3,3,3,3,3,3,3,3,3,4),(-87.613874691471,-87.4581822547,-87.3024512341524,
-87.1467085139083,-86.9906166055535,-86.8949391278171,-86.7375132693767,
-86.5803770127665,-86.4234095180274,-86.2663614088741,-86.1092653146766,
-85.9518296537067,-85.8961467240491,-85.7387208656087,-85.5815846089985,
-85.4246171142593,-85.2675690051059,-85.1104729109085,-84.9530372499385,
-84.8973543202811,-84.7399284618406,-84.5827922052304,-84.4258247104913,
-84.2687766013378,-84.1116805071403,-83.9542448461704,-83.8985619165131,
-83.7411360580727,-83.5839998014625,-83.4270323067233,-83.2699841975699,
-83.1128881033725,-82.9554524424025,-82.8997695127451,-82.7423436543047,
-82.5852073976945,-82.4282399029553,-82.2711917938019,-82.1140956996044,
-81.9566600386343,-81.9009771089771,-81.7398987646841,-81.5791799583681,
-81.4187407475093,-81.3306893842914),.UNSPECIFIED.);
#721=B_SPLINE_CURVE_WITH_KNOTS('',3,(#29122,#29123,#29124,#29125,#29126,
#29127,#29128,#29129,#29130,#29131),.UNSPECIFIED.,.F.,.F.,(4,1,1,1,1,1,
1,4),(-81.3306838834889,-80.9021847052091,-79.9033923014411,-78.9045998976731,
-77.905807493905,-76.907015090137,-75.908222686369,-75.0475121675532),
 .UNSPECIFIED.);
#722=B_SPLINE_CURVE_WITH_KNOTS('',3,(#29133,#29134,#29135,#29136,#29137,
#29138,#29139,#29140,#29141,#29142,#29143,#29144,#29145,#29146,#29147,#29148,
#29149,#29150,#29151,#29152,#29153,#29154,#29155,#29156,#29157,#29158,#29159,
#29160,#29161,#29162,#29163,#29164,#29165,#29166,#29167,#29168,#29169,#29170,
#29171,#29172,#29173,#29174,#29175,#29176,#29177,#29178,#29179,#29180,#29181,
#29182,#29183,#29184,#29185,#29186,#29187,#29188,#29189,#29190,#29191,#29192,
#29193,#29194,#29195,#29196,#29197,#29198,#29199,#29200,#29201,#29202,#29203,
#29204,#29205,#29206,#29207,#29208,#29209,#29210,#29211,#29212,#29213,#29214,
#29215,#29216,#29217,#29218,#29219,#29220,#29221,#29222,#29223,#29224,#29225,
#29226,#29227,#29228,#29229,#29230,#29231,#29232,#29233,#29234,#29235,#29236,
#29237,#29238,#29239,#29240,#29241,#29242,#29243,#29244,#29245,#29246,#29247,
#29248,#29249,#29250,#29251,#29252,#29253,#29254,#29255,#29256,#29257,#29258,
#29259,#29260,#29261,#29262,#29263,#29264,#29265),.UNSPECIFIED.,.F.,.F.,
(4,3,3,3,3,3,3,3,3,3,3,3,3,3,3,3,3,3,3,3,3,3,3,3,3,3,3,3,3,3,3,3,3,3,3,
3,3,3,3,3,3,3,3,3,4),(-75.0475040771118,-74.909430282601,-74.7520044241609,
-74.5948681675511,-74.4379006728122,-74.2808525636592,-74.1237564694621,
-73.9663208084924,-73.910637878833,-73.7532120203925,-73.5960757637822,
-73.439108269043,-73.2820601598895,-73.124964065692,-72.9675284047219,-72.911845475065,
-72.7544196166245,-72.5972833600143,-72.4403158652751,-72.2832677561216,
-72.1261716619241,-71.968736000954,-71.913053071297,-71.7556272128566,-71.5984909562464,
-71.4415234615072,-71.2844753523538,-71.1273792581563,-70.9699435971863,
-70.9142606675289,-70.7568348090885,-70.5996985524782,-70.4427310577391,
-70.2856829485857,-70.1285868543882,-69.9711511934181,-69.9154682637609,
-69.7580424053205,-69.6009061487103,-69.4439386539711,-69.2868905448178,
-69.1297944506203,-68.9723587896503,-68.9166758599929,-68.7643187699322),
 .UNSPECIFIED.);
#723=B_SPLINE_CURVE_WITH_KNOTS('',3,(#29267,#29268,#29269,#29270,#29271,
#29272,#29273,#29274,#29275,#29276),.UNSPECIFIED.,.F.,.F.,(4,1,1,1,1,1,
1,4),(-68.7643114907279,-67.9178834562249,-66.9190910524569,-65.9202986486889,
-64.9215062449209,-63.9227138411528,-62.9239214373848,-62.4811378862089),
 .UNSPECIFIED.);
#724=B_SPLINE_CURVE_WITH_KNOTS('',3,(#29278,#29279,#29280,#29281,#29282,
#29283,#29284,#29285,#29286,#29287,#29288,#29289,#29290,#29291,#29292,#29293,
#29294,#29295,#29296,#29297,#29298,#29299,#29300,#29301,#29302,#29303,#29304,
#29305,#29306,#29307,#29308,#29309,#29310,#29311,#29312,#29313,#29314,#29315,
#29316,#29317,#29318,#29319,#29320,#29321,#29322,#29323,#29324,#29325,#29326,
#29327,#29328,#29329,#29330,#29331,#29332,#29333,#29334,#29335,#29336,#29337,
#29338,#29339,#29340,#29341,#29342,#29343,#29344,#29345,#29346,#29347,#29348,
#29349,#29350,#29351,#29352,#29353,#29354,#29355,#29356,#29357,#29358,#29359,
#29360,#29361,#29362,#29363,#29364,#29365,#29366,#29367,#29368,#29369,#29370,
#29371,#29372,#29373,#29374,#29375,#29376,#29377,#29378,#29379,#29380,#29381,
#29382,#29383,#29384,#29385,#29386,#29387,#29388,#29389,#29390,#29391,#29392,
#29393,#29394,#29395,#29396,#29397,#29398,#29399,#29400,#29401,#29402,#29403,
#29404,#29405,#29406,#29407,#29408,#29409,#29410),.UNSPECIFIED.,.F.,.F.,
(4,3,3,3,3,3,3,3,3,3,3,3,3,3,3,3,3,3,3,3,3,3,3,3,3,3,3,3,3,3,3,3,3,3,3,
3,3,3,3,3,3,3,3,3,4),(-62.4811334627526,-62.3199251441198,-62.1585495109481,
-61.9966903768796,-61.9251290336168,-61.7677031751763,-61.6105669185661,
-61.4535994238269,-61.2965513146734,-61.1394552204759,-60.9820195595058,
-60.9263366298488,-60.7689107714084,-60.6117745147981,-60.454807020059,
-60.2977589109056,-60.1406628167082,-59.9832271557382,-59.9275442260808,
-59.7701183676404,-59.6129821110303,-59.456014616291,-59.2989665071376,
-59.1418704129402,-58.9844347519701,-58.9287518223128,-58.7713259638724,
-58.6141897072622,-58.457222212523,-58.3001741033696,-58.1430780091721,
-57.9856423482021,-57.9299594185448,-57.7725335601044,-57.6153973034943,
-57.4584298087551,-57.3013816996017,-57.1442856054042,-56.9868499444341,
-56.9311670147768,-56.7753043145904,-56.6197160121704,-56.4642955554139,
-56.3087841197039,-56.1979481555731),.UNSPECIFIED.);
#725=B_SPLINE_CURVE_WITH_KNOTS('',3,(#29412,#29413,#29414,#29415,#29416,
#29417,#29418,#29419,#29420,#29421,#29422,#29423,#29424,#29425,#29426,#29427,
#29428,#29429,#29430,#29431,#29432,#29433,#29434,#29435,#29436,#29437,#29438,
#29439,#29440,#29441,#29442,#29443,#29444,#29445,#29446,#29447,#29448,#29449,
#29450,#29451,#29452,#29453,#29454,#29455,#29456,#29457,#29458,#29459,#29460,
#29461,#29462,#29463,#29464,#29465,#29466,#29467,#29468,#29469,#29470,#29471,
#29472,#29473,#29474,#29475,#29476,#29477,#29478,#29479,#29480,#29481,#29482,
#29483,#29484,#29485,#29486,#29487,#29488,#29489,#29490,#29491,#29492,#29493,
#29494,#29495,#29496,#29497,#29498,#29499,#29500,#29501,#29502,#29503,#29504,
#29505,#29506,#29507,#29508,#29509,#29510,#29511,#29512,#29513,#29514,#29515,
#29516,#29517,#29518,#29519,#29520,#29521,#29522,#29523,#29524,#29525,#29526,
#29527,#29528,#29529,#29530,#29531,#29532,#29533,#29534,#29535,#29536,#29537,
#29538,#29539,#29540,#29541,#29542,#29543,#29544,#29545,#29546,#29547),
 .UNSPECIFIED.,.F.,.F.,(4,3,3,3,3,3,3,3,3,3,3,3,3,3,3,3,3,3,3,3,3,3,3,3,
3,3,3,3,3,3,3,3,3,3,3,3,3,3,3,3,3,3,3,3,3,4),(-56.1979481553862,-55.9987847029591,
-55.9323746110087,-55.7749487525684,-55.6178124959584,-55.4608450012194,
-55.3037968920661,-55.1467007978688,-54.9892651368989,-54.9335822072407,
-54.7761563488003,-54.61902009219,-54.4620525974508,-54.3050044882974,-54.1479083941,
-53.9904727331299,-53.9347898034727,-53.7773639450323,-53.620227688422,
-53.4632601936828,-53.3062120845294,-53.1491159903319,-52.9916803293619,
-52.9359973997047,-52.7785715412643,-52.6214352846541,-52.4644677899149,
-52.3074196807615,-52.1503235865641,-51.9928879255941,-51.9372049959367,
-51.7797791374963,-51.622642880886,-51.4656753861469,-51.3086272769935,
-51.151531182796,-50.9940955218259,-50.9384125921687,-50.7809867337283,
-50.6238504771181,-50.466882982379,-50.3098348732256,-50.1527387790282,
-49.9953031180581,-49.9396201884007,-49.9147628483934),.UNSPECIFIED.);
#726=B_SPLINE_CURVE_WITH_KNOTS('',3,(#29549,#29550,#29551,#29552,#29553,
#29554,#29555,#29556,#29557,#29558,#29559,#29560,#29561,#29562,#29563,#29564,
#29565,#29566,#29567,#29568,#29569,#29570,#29571,#29572,#29573,#29574,#29575,
#29576,#29577,#29578,#29579,#29580,#29581,#29582,#29583,#29584,#29585,#29586,
#29587,#29588,#29589,#29590,#29591,#29592,#29593,#29594,#29595,#29596,#29597,
#29598,#29599,#29600,#29601,#29602,#29603,#29604,#29605,#29606,#29607,#29608,
#29609,#29610,#29611,#29612,#29613,#29614,#29615,#29616,#29617,#29618,#29619,
#29620,#29621,#29622,#29623,#29624,#29625,#29626,#29627,#29628,#29629,#29630,
#29631,#29632,#29633,#29634,#29635,#29636,#29637,#29638,#29639,#29640,#29641,
#29642,#29643,#29644,#29645,#29646,#29647,#29648,#29649,#29650,#29651,#29652,
#29653,#29654,#29655,#29656,#29657,#29658,#29659,#29660,#29661,#29662,#29663,
#29664,#29665,#29666,#29667,#29668,#29669,#29670,#29671,#29672,#29673,#29674,
#29675,#29676,#29677,#29678,#29679,#29680,#29681),.UNSPECIFIED.,.F.,.F.,
(4,3,3,3,3,3,3,3,3,3,3,3,3,3,3,3,3,3,3,3,3,3,3,3,3,3,3,3,3,3,3,3,3,3,3,
3,3,3,3,3,3,3,3,3,4),(-49.9147628482126,-49.7579972342683,-49.601517677362,
-49.4452012318009,-49.2888004018216,-49.1323425683609,-48.9755541490261,
-48.9408277846327,-48.7834019261923,-48.6262656695821,-48.4692981748429,
-48.3122500656895,-48.1551539714921,-47.9977183105221,-47.9420353808647,
-47.7846095224242,-47.627473265814,-47.4705057710747,-47.3134576619212,
-47.1563615677237,-46.9989259067536,-46.9432429770966,-46.7858171186562,
-46.6286808620461,-46.4717133673068,-46.3146652581534,-46.157569163956,
-46.000133502986,-45.9444505733286,-45.7870247148882,-45.629888458278,-45.4729209635388,
-45.3158728543854,-45.1587767601879,-45.0013410992178,-44.9456581695606,
-44.7882323111202,-44.6310960545101,-44.474128559771,-44.3170804506176,
-44.1599843564201,-44.0025486954501,-43.9468657657926,-43.7595906204688,
-43.6315777496244),.UNSPECIFIED.);
#727=B_SPLINE_CURVE_WITH_KNOTS('',3,(#29683,#29684,#29685,#29686,#29687,
#29688,#29689,#29690,#29691,#29692),.UNSPECIFIED.,.F.,.F.,(4,1,1,1,1,1,
1,4),(-43.6315775412138,-42.9480733620246,-41.9492809582566,-40.9504885544885,
-39.9516961507205,-38.9529037469525,-37.9541113431845,-37.3483922340342),
 .UNSPECIFIED.);
#728=B_SPLINE_CURVE_WITH_KNOTS('',3,(#29694,#29695,#29696,#29697,#29698,
#29699,#29700,#29701,#29702,#29703,#29704,#29705,#29706,#29707,#29708,#29709,
#29710,#29711,#29712,#29713,#29714,#29715,#29716,#29717,#29718,#29719,#29720,
#29721,#29722,#29723,#29724,#29725,#29726,#29727,#29728,#29729,#29730,#29731,
#29732,#29733,#29734,#29735,#29736,#29737,#29738,#29739,#29740,#29741,#29742,
#29743,#29744,#29745,#29746,#29747,#29748,#29749,#29750,#29751,#29752,#29753,
#29754,#29755,#29756,#29757,#29758,#29759,#29760,#29761,#29762,#29763,#29764,
#29765,#29766,#29767,#29768,#29769,#29770,#29771,#29772,#29773,#29774,#29775,
#29776,#29777,#29778,#29779,#29780,#29781,#29782,#29783,#29784,#29785,#29786,
#29787,#29788,#29789,#29790,#29791,#29792,#29793,#29794,#29795,#29796,#29797,
#29798,#29799,#29800,#29801,#29802,#29803,#29804,#29805,#29806,#29807,#29808,
#29809,#29810,#29811,#29812,#29813,#29814,#29815,#29816,#29817,#29818,#29819,
#29820,#29821,#29822,#29823,#29824,#29825,#29826),.UNSPECIFIED.,.F.,.F.,
(4,3,3,3,3,3,3,3,3,3,3,3,3,3,3,3,3,3,3,3,3,3,3,3,3,3,3,3,3,3,3,3,3,3,3,
3,3,3,3,3,3,3,3,3,4),(-37.3483920044007,-37.1740560776412,-36.9983336164258,
-36.9553189394165,-36.7978930809762,-36.6407568243661,-36.483789329627,
-36.3267412204737,-36.1696451262764,-36.0122094653064,-35.9565265356485,
-35.7991006772078,-35.6419644205973,-35.4849969258578,-35.3279488167041,
-35.1708527225064,-35.013417061536,-34.9577341318805,-34.8003082734402,
-34.6431720168302,-34.4862045220911,-34.3291564129379,-34.1720603187406,
-34.0146246577706,-33.9589417281124,-33.8015158696727,-33.6443796130633,
-33.4874121183249,-33.3303640091722,-33.1732679149755,-33.0158322540062,
-32.9601493243444,-32.8027234659016,-32.6455872092891,-32.4886197145476,
-32.3315716053919,-32.1744755111921,-32.0170398502199,-31.9613569205764,
-31.8059289511626,-31.6507874821997,-31.495695171176,-31.3406480503224,
-31.1853007557434,-31.0652069270835),.UNSPECIFIED.);
#729=B_SPLINE_CURVE_WITH_KNOTS('',3,(#29828,#29829,#29830,#29831,#29832,
#29833,#29834,#29835,#29836,#29837,#29838,#29839,#29840,#29841,#29842,#29843,
#29844,#29845,#29846,#29847,#29848,#29849,#29850,#29851,#29852,#29853,#29854,
#29855,#29856,#29857,#29858,#29859,#29860,#29861,#29862,#29863,#29864,#29865,
#29866,#29867,#29868,#29869,#29870,#29871,#29872,#29873,#29874,#29875,#29876,
#29877,#29878,#29879,#29880,#29881,#29882,#29883,#29884,#29885,#29886,#29887,
#29888,#29889,#29890,#29891,#29892,#29893,#29894,#29895,#29896,#29897,#29898,
#29899,#29900,#29901,#29902,#29903,#29904,#29905,#29906,#29907,#29908,#29909,
#29910,#29911,#29912,#29913,#29914,#29915,#29916,#29917,#29918,#29919,#29920,
#29921,#29922,#29923,#29924,#29925,#29926,#29927,#29928,#29929,#29930,#29931,
#29932,#29933,#29934,#29935,#29936,#29937,#29938,#29939,#29940,#29941,#29942,
#29943,#29944,#29945,#29946,#29947,#29948,#29949,#29950,#29951,#29952,#29953,
#29954,#29955,#29956,#29957,#29958,#29959,#29960),.UNSPECIFIED.,.F.,.F.,
(4,3,3,3,3,3,3,3,3,3,3,3,3,3,3,3,3,3,3,3,3,3,3,3,3,3,3,3,3,3,3,3,3,3,3,
3,3,3,3,3,3,3,3,3,4),(-31.0652069268547,-30.9625645168084,-30.8051386583722,
-30.6480024017662,-30.4910349070314,-30.3339867978823,-30.1768907036891,
-30.0194550427234,-29.9637721130404,-29.8063462545833,-29.6492099979563,
-29.4922425032005,-29.3351943940307,-29.1780982998169,-29.020662638831,
-28.9649797092724,-28.8075538508509,-28.6504175942594,-28.4934500995388,
-28.3364019904035,-28.1793058962238,-28.0218702352708,-27.9661873055044,
-27.8087614470865,-27.6516251904992,-27.4946576957833,-27.3376095866533,
-27.1805134924793,-27.0230778315326,-26.9673949017364,-26.8099690431787,
-26.652832786451,-26.4958652915946,-26.3388171823254,-26.181721088013,-26.0242854269309,
-25.9686024979683,-25.8111766396887,-25.6540403832383,-25.4970728886576,
-25.3400247796587,-25.1829286856137,-25.0254930247908,-24.9698100942003,
-24.7820216196751),.UNSPECIFIED.);
#730=B_SPLINE_CURVE_WITH_KNOTS('',3,(#29962,#29963,#29964,#29965,#29966,
#29967,#29968,#29969,#29970,#29971),.UNSPECIFIED.,.F.,.F.,(4,1,1,1,1,1,
1,4),(-24.7820171771123,-23.9710176904323,-22.9722252866643,-21.9734328828963,
-20.9746404791283,-19.9758480753603,-18.9770556715922,-18.4988379499898),
 .UNSPECIFIED.);
#731=B_SPLINE_CURVE_WITH_KNOTS('',3,(#29973,#29974,#29975,#29976,#29977,
#29978,#29979,#29980,#29981,#29982,#29983,#29984,#29985,#29986,#29987,#29988,
#29989,#29990,#29991,#29992,#29993,#29994,#29995,#29996,#29997,#29998,#29999,
#30000,#30001,#30002,#30003,#30004,#30005,#30006,#30007,#30008,#30009,#30010,
#30011,#30012,#30013,#30014,#30015,#30016,#30017,#30018,#30019,#30020,#30021,
#30022,#30023,#30024,#30025,#30026,#30027,#30028,#30029,#30030,#30031,#30032,
#30033,#30034,#30035,#30036,#30037,#30038,#30039,#30040,#30041,#30042,#30043,
#30044,#30045,#30046,#30047,#30048,#30049,#30050,#30051,#30052,#30053,#30054,
#30055,#30056,#30057,#30058,#30059,#30060,#30061,#30062,#30063,#30064,#30065,
#30066,#30067,#30068,#30069,#30070,#30071,#30072,#30073,#30074,#30075,#30076,
#30077,#30078,#30079,#30080,#30081,#30082,#30083,#30084,#30085,#30086,#30087,
#30088,#30089,#30090,#30091,#30092,#30093,#30094,#30095,#30096,#30097,#30098,
#30099,#30100,#30101,#30102,#30103,#30104,#30105),.UNSPECIFIED.,.F.,.F.,
(4,3,3,3,3,3,3,3,3,3,3,3,3,3,3,3,3,3,3,3,3,3,3,3,3,3,3,3,3,3,3,3,3,3,3,
3,3,3,3,3,3,3,3,3,4),(-18.4988363124955,-18.3356133666513,-18.1721238367137,
-18.0080989678902,-17.9782632678242,-17.8208373743237,-17.6637010824669,
-17.5067335524134,-17.3496854082564,-17.1925892791905,-17.035153584078,
-16.9794708640562,-16.8220450841236,-16.6649089058851,-16.5079414891278,
-16.3508934564909,-16.1937974380605,-16.0363618506131,-15.9806784602882,
-15.8232525681947,-15.6661162789071,-15.5091487525538,-15.3521006136902,
-15.1950044908435,-15.0375688032116,-14.9818860565202,-14.8244599770603,
-14.6673234979013,-14.5103557798413,-14.3533074488336,-14.196211133349,
-14.0387752552734,-13.9830936527522,-13.8256683799556,-13.668532708559,
-13.5115657966989,-13.3545182603062,-13.1974227337522,-13.0399876243365,
-12.9843012489842,-12.8289087549843,-12.6737644033177,-12.5187820442914,
-12.3636506841468,-12.2156510053159),.UNSPECIFIED.);
#732=B_SPLINE_CURVE_WITH_KNOTS('',3,(#30107,#30108,#30109,#30110,#30111,
#30112,#30113,#30114,#30115,#30116,#30117),.UNSPECIFIED.,.F.,.F.,(4,1,1,
1,1,1,1,1,4),(-12.2156510053159,-11.9855088452162,-10.9867164414481,-9.98792403768013,
-8.98913163391212,-7.99033923014411,-6.99154682637609,-5.99275442260808,
-5.93246569813632),.UNSPECIFIED.);
#733=B_SPLINE_CURVE_WITH_KNOTS('',3,(#30119,#30120,#30121,#30122,#30123,
#30124,#30125,#30126,#30127,#30128,#30129,#30130,#30131,#30132,#30133,#30134,
#30135,#30136,#30137,#30138,#30139,#30140,#30141,#30142,#30143,#30144,#30145,
#30146,#30147,#30148,#30149,#30150,#30151,#30152,#30153,#30154,#30155,#30156,
#30157,#30158,#30159,#30160,#30161,#30162,#30163,#30164,#30165,#30166,#30167,
#30168,#30169,#30170,#30171,#30172,#30173,#30174,#30175,#30176,#30177,#30178,
#30179,#30180,#30181,#30182,#30183,#30184,#30185,#30186,#30187,#30188,#30189,
#30190,#30191,#30192,#30193,#30194,#30195,#30196,#30197),.UNSPECIFIED.,
 .F.,.F.,(4,3,3,3,3,3,3,3,3,3,3,3,3,3,3,3,3,3,3,3,3,3,3,3,3,3,4),(-5.93246569813632,
-5.77641800085584,-5.62064407302824,-5.4639735594812,-5.30825355217736,
-5.15110778550871,-4.99396201884007,-4.8367491311759,-4.67982626504034,
-4.52307188923757,-4.36623406611058,-4.20934690291075,-4.05211503034409,
-3.99516961507205,-3.83744358884951,-3.68000888850026,-3.52274564504591,
-3.36540915336445,-3.20802859481956,-3.05031852022946,-2.99637721130404,
-2.8403043537898,-2.68451357335128,-2.52868632450517,-2.3729713138078,-2.21690906463917,
-2.06120457796682),.UNSPECIFIED.);
#734=B_SPLINE_CURVE_WITH_KNOTS('',3,(#30199,#30200,#30201,#30202),
 .UNSPECIFIED.,.F.,.F.,(4,4),(-0.00791600890681302,0.),.UNSPECIFIED.);
#735=B_SPLINE_CURVE_WITH_KNOTS('',3,(#30206,#30207,#30208,#30209,#30210,
#30211),.UNSPECIFIED.,.F.,.F.,(4,1,1,4),(0.,0.998792403768015,1.99758480753603,
2.94976186885485),.UNSPECIFIED.);
#736=B_SPLINE_CURVE_WITH_KNOTS('',3,(#30213,#30214,#30215,#30216,#30217,
#30218,#30219,#30220,#30221,#30222,#30223),.UNSPECIFIED.,.F.,.F.,(4,1,1,
1,1,1,1,1,4),(2.94976186885485,2.99637721130404,3.99516961507206,4.99396201884008,
5.9927544226081,6.99154682637612,7.99033923014414,8.98913163391216,9.23294717603444),
 .UNSPECIFIED.);
#737=B_SPLINE_CURVE_WITH_KNOTS('',3,(#30225,#30226,#30227,#30228,#30229,
#30230,#30231,#30232,#30233,#30234),.UNSPECIFIED.,.F.,.F.,(4,1,1,1,1,1,
1,4),(9.23294717603444,9.98792403768017,10.9867164414482,11.9855088452162,
12.9843012489842,13.9830936527522,14.9818860565202,15.516132483214),
 .UNSPECIFIED.);
#738=B_SPLINE_CURVE_WITH_KNOTS('',3,(#30236,#30237,#30238,#30239,#30240,
#30241,#30242,#30243,#30244,#30245,#30246,#30247,#30248,#30249,#30250,#30251,
#30252,#30253,#30254,#30255,#30256,#30257,#30258,#30259,#30260,#30261,#30262,
#30263,#30264,#30265,#30266,#30267,#30268,#30269,#30270,#30271,#30272,#30273,
#30274,#30275,#30276,#30277,#30278,#30279,#30280,#30281,#30282,#30283,#30284,
#30285,#30286,#30287,#30288,#30289,#30290,#30291,#30292,#30293,#30294,#30295,
#30296,#30297,#30298,#30299,#30300,#30301,#30302,#30303,#30304,#30305,#30306,
#30307,#30308,#30309,#30310,#30311,#30312,#30313,#30314,#30315,#30316,#30317,
#30318,#30319,#30320,#30321,#30322,#30323,#30324,#30325,#30326,#30327,#30328,
#30329,#30330,#30331,#30332,#30333,#30334,#30335,#30336,#30337,#30338,#30339,
#30340,#30341,#30342,#30343,#30344,#30345,#30346,#30347,#30348,#30349,#30350,
#30351,#30352,#30353,#30354,#30355,#30356,#30357,#30358,#30359,#30360,#30361,
#30362,#30363,#30364,#30365,#30366,#30367,#30368),.UNSPECIFIED.,.F.,.F.,
(4,3,3,3,3,3,3,3,3,3,3,3,3,3,3,3,3,3,3,3,3,3,3,3,3,3,3,3,3,3,3,3,3,3,3,
3,3,3,3,3,3,3,3,3,4),(15.5161326720168,15.6833768003707,15.8514912044741,
15.9806784602882,16.1381042453226,16.295240426837,16.4522078450532,16.6092558764632,
16.7663518921126,16.9237874745117,16.9794708640563,17.1368967565385,17.2940330477215,
17.4510005774442,17.6080487217782,17.7651448513149,17.9225805473274,17.9782632678243,
18.1356891269169,18.2928253843364,18.4497928800386,18.6068409903732,18.7639370858797,
18.9213727483317,18.9770556715923,19.1344815204902,19.2916177673265,19.4485852520946,
19.6056333511011,19.7627294350371,19.9201650857285,19.9758480753603,20.1332739389886,
20.2904102008745,20.4473777009587,20.6044258154971,20.7615219151095,20.9189575814576,
20.9746404791283,21.1297203095798,21.2845109513251,21.4392204316573,21.5938858731285,
21.7487661283071,21.7993177903936),.UNSPECIFIED.);
#739=B_SPLINE_CURVE_WITH_KNOTS('',3,(#30370,#30371,#30372,#30373,#30374,
#30375,#30376,#30377,#30378,#30379,#30380),.UNSPECIFIED.,.F.,.F.,(4,1,1,
1,1,1,1,1,4),(21.7993177903936,21.9734328828963,22.9722252866643,23.9710176904323,
24.9698100942003,25.9686024979684,26.9673949017364,27.9661873055044,28.0825030975732),
 .UNSPECIFIED.);
#740=B_SPLINE_CURVE_WITH_KNOTS('',3,(#30382,#30383,#30384,#30385,#30386,
#30387,#30388,#30389,#30390,#30391,#30392,#30393,#30394,#30395,#30396,#30397,
#30398,#30399,#30400,#30401,#30402,#30403,#30404,#30405,#30406,#30407,#30408,
#30409,#30410,#30411,#30412,#30413,#30414,#30415,#30416,#30417,#30418,#30419,
#30420,#30421,#30422,#30423,#30424,#30425,#30426,#30427,#30428,#30429,#30430,
#30431,#30432,#30433,#30434,#30435,#30436,#30437,#30438,#30439,#30440,#30441,
#30442,#30443,#30444,#30445,#30446,#30447,#30448,#30449,#30450,#30451,#30452,
#30453,#30454,#30455,#30456,#30457,#30458,#30459,#30460,#30461,#30462,#30463,
#30464,#30465,#30466,#30467,#30468,#30469,#30470,#30471,#30472,#30473,#30474,
#30475,#30476,#30477,#30478,#30479,#30480,#30481,#30482,#30483,#30484,#30485,
#30486,#30487,#30488,#30489,#30490,#30491,#30492,#30493,#30494,#30495,#30496,
#30497,#30498,#30499,#30500,#30501,#30502,#30503,#30504,#30505,#30506,#30507,
#30508,#30509,#30510,#30511,#30512,#30513,#30514),.UNSPECIFIED.,.F.,.F.,
(4,3,3,3,3,3,3,3,3,3,3,3,3,3,3,3,3,3,3,3,3,3,3,3,3,3,3,3,3,3,3,3,3,3,3,
3,3,3,3,3,3,3,3,3,4),(28.0825030975732,28.2376974030802,28.3926473134147,
28.5476070278282,28.7025582372351,28.8578500130469,28.9649797092724,29.1224055677287,
29.2795418243551,29.4365093191107,29.5935574282807,29.7506535224949,29.9080891834816,
29.9637721130404,30.1211979714765,30.2783342280825,30.4353017228172,30.5923498319662,
30.7494459261594,30.9068815871251,30.9625645168084,31.119990375247,31.2771266318553,
31.4340941265926,31.5911422357439,31.7482383299393,31.9056739909073,31.9613569205764,
32.118782779019,32.2759190356316,32.4328865303731,32.5899346395289,32.7470307337286,
32.904466394701,32.9601493243444,33.1175751827841,33.2747114393934,33.4316789341318,
33.5887270432845,33.7458231374812,33.9032587984505,33.9589417281124,34.1330497198208,
34.3059304641482,34.3656881914393),.UNSPECIFIED.);
#741=B_SPLINE_CURVE_WITH_KNOTS('',3,(#30516,#30517,#30518,#30519,#30520,
#30521,#30522,#30523,#30524,#30525),.UNSPECIFIED.,.F.,.F.,(4,1,1,1,1,1,
1,4),(34.3656884047528,34.9577341318804,35.9565265356485,36.9553189394165,
37.9541113431845,38.9529037469526,39.9516961507206,40.6488737119324),
 .UNSPECIFIED.);
#742=B_SPLINE_CURVE_WITH_KNOTS('',3,(#30527,#30528,#30529,#30530,#30531,
#30532,#30533,#30534,#30535,#30536,#30537,#30538,#30539,#30540,#30541,#30542,
#30543,#30544,#30545,#30546,#30547,#30548,#30549,#30550,#30551,#30552,#30553,
#30554,#30555,#30556,#30557,#30558,#30559,#30560,#30561,#30562,#30563,#30564,
#30565,#30566,#30567,#30568,#30569,#30570,#30571,#30572,#30573,#30574,#30575,
#30576,#30577,#30578,#30579,#30580,#30581,#30582,#30583,#30584,#30585,#30586,
#30587,#30588,#30589,#30590,#30591,#30592,#30593,#30594,#30595,#30596,#30597,
#30598,#30599,#30600,#30601,#30602,#30603,#30604,#30605,#30606,#30607,#30608,
#30609,#30610,#30611,#30612,#30613,#30614,#30615,#30616,#30617,#30618,#30619,
#30620,#30621,#30622,#30623,#30624,#30625,#30626,#30627,#30628,#30629,#30630,
#30631,#30632,#30633,#30634,#30635,#30636,#30637,#30638,#30639,#30640,#30641,
#30642,#30643,#30644,#30645,#30646,#30647,#30648,#30649,#30650,#30651,#30652,
#30653,#30654,#30655,#30656,#30657,#30658,#30659),.UNSPECIFIED.,.F.,.F.,
(4,3,3,3,3,3,3,3,3,3,3,3,3,3,3,3,3,3,3,3,3,3,3,3,3,3,3,3,3,3,3,3,3,3,3,
3,3,3,3,3,3,3,3,3,4),(40.6488738966027,40.8389897275225,40.9504885544886,
41.107914412929,41.2650506695392,41.4220181642784,41.5790662734318,41.7361623676293,
41.8935980285994,41.9492809582566,42.106706816697,42.2638430733072,42.4208105680465,
42.5778586771999,42.7349547713973,42.8923904323674,42.9480733620246,43.105499220465,
43.2626354770752,43.4196029718143,43.5766510809677,43.7337471751652,43.8911828361352,
43.9468657657926,44.1042916242331,44.2614278808433,44.4183953755826,44.575443484736,
44.7325395789335,44.8899752399036,44.9456581695607,45.1030840280011,45.2602202846113,
45.4171877793505,45.5742358885039,45.7313319827014,45.8887676436714,45.9444505733287,
46.1015680379833,46.2583964719956,46.4150577485581,46.5718002293858,46.7285940925013,
46.8857227911254,46.93205901893),.UNSPECIFIED.);
#743=B_SPLINE_CURVE_WITH_KNOTS('',3,(#30661,#30662,#30663,#30664,#30665,
#30666,#30667,#30668,#30669,#30670,#30671,#30672,#30673,#30674,#30675,#30676,
#30677,#30678,#30679,#30680,#30681,#30682,#30683,#30684,#30685,#30686,#30687,
#30688,#30689,#30690,#30691,#30692,#30693,#30694,#30695,#30696,#30697,#30698,
#30699,#30700,#30701,#30702,#30703,#30704,#30705,#30706,#30707,#30708,#30709,
#30710,#30711,#30712,#30713,#30714,#30715,#30716,#30717,#30718,#30719,#30720,
#30721,#30722,#30723,#30724,#30725,#30726,#30727,#30728,#30729,#30730,#30731,
#30732,#30733,#30734,#30735,#30736,#30737,#30738,#30739,#30740,#30741,#30742,
#30743,#30744,#30745,#30746,#30747,#30748,#30749,#30750,#30751,#30752,#30753,
#30754,#30755,#30756,#30757,#30758,#30759,#30760,#30761,#30762,#30763,#30764,
#30765,#30766,#30767,#30768,#30769,#30770,#30771,#30772,#30773,#30774,#30775,
#30776,#30777,#30778,#30779,#30780,#30781,#30782,#30783,#30784,#30785,#30786,
#30787,#30788,#30789,#30790,#30791,#30792,#30793,#30794,#30795,#30796),
 .UNSPECIFIED.,.F.,.F.,(4,3,3,3,3,3,3,3,3,3,3,3,3,3,3,3,3,3,3,3,3,3,3,3,
3,3,3,3,3,3,3,3,3,3,3,3,3,3,3,3,3,3,3,3,3,4),(46.932059019112,46.9432429770967,
47.1006688355372,47.2578050921474,47.4147725868865,47.57182069604,47.7289167902374,
47.8863524512075,47.9420353808647,48.0994612393051,48.2565974959154,48.4135649906546,
48.570613099808,48.7277091940054,48.8851448549755,48.9408277846327,49.0982536430731,
49.2553898996833,49.4123573944225,49.5694055035759,49.7265015977733,49.8839372587433,
49.9396201884007,50.0970460468411,50.2541823034514,50.4111497981906,50.568197907344,
50.7252940015415,50.8827296625115,50.9384125921687,51.0958384506091,51.2529747072194,
51.4099422019585,51.5669903111119,51.7240864053094,51.8815220662794,51.9372049959367,
52.0946308543771,52.2517671109873,52.4087346057264,52.5657827148798,52.7228788090773,
52.8803144700473,52.9359973997047,53.1314224868731,53.2152443261636),
 .UNSPECIFIED.);
#744=B_SPLINE_CURVE_WITH_KNOTS('',3,(#30798,#30799,#30800,#30801,#30802,
#30803,#30804,#30805,#30806,#30807,#30808,#30809,#30810,#30811,#30812,#30813,
#30814,#30815,#30816,#30817,#30818,#30819,#30820,#30821,#30822,#30823,#30824,
#30825,#30826,#30827,#30828,#30829,#30830,#30831,#30832,#30833,#30834,#30835,
#30836,#30837,#30838,#30839,#30840,#30841,#30842,#30843,#30844,#30845,#30846,
#30847,#30848,#30849,#30850,#30851,#30852,#30853,#30854,#30855,#30856,#30857,
#30858,#30859,#30860,#30861,#30862,#30863,#30864,#30865,#30866,#30867,#30868,
#30869,#30870,#30871,#30872,#30873,#30874,#30875,#30876,#30877,#30878,#30879,
#30880,#30881,#30882,#30883,#30884,#30885,#30886,#30887,#30888,#30889,#30890,
#30891,#30892,#30893,#30894,#30895,#30896,#30897,#30898,#30899,#30900,#30901,
#30902,#30903,#30904,#30905,#30906,#30907,#30908,#30909,#30910,#30911,#30912,
#30913,#30914,#30915,#30916,#30917,#30918,#30919,#30920,#30921,#30922,#30923,
#30924,#30925,#30926,#30927,#30928,#30929,#30930),.UNSPECIFIED.,.F.,.F.,
(4,3,3,3,3,3,3,3,3,3,3,3,3,3,3,3,3,3,3,3,3,3,3,3,3,3,3,3,3,3,3,3,3,3,3,
3,3,3,3,3,3,3,3,3,4),(53.2152443262915,53.370926689653,53.5266468618019,
53.6823780883531,53.8384585272822,53.9347898034727,54.0922156619131,54.2493519185232,
54.4063194132625,54.5633675224159,54.7204636166133,54.8778992775833,54.9335822072407,
55.0910080656812,55.2481443222914,55.4051118170306,55.562159926184,55.7192560203815,
55.8766916813516,55.9323746110088,56.0898004694492,56.2469367260595,56.4039042207987,
56.5609523299522,56.7180484241497,56.8754840851197,56.9311670147768,57.0885928732172,
57.2457291298273,57.4026966245663,57.5597447337196,57.7168408279169,57.8742764888869,
57.9299594185448,58.0873852769852,58.2445215335953,58.4014890283344,58.5585371374879,
58.7156332316853,58.8730688926553,58.9287518223128,59.0898611342064,59.250610284966,
59.4110781810322,59.4984296334711),.UNSPECIFIED.);
#745=B_SPLINE_CURVE_WITH_KNOTS('',3,(#30932,#30933,#30934,#30935,#30936,
#30937,#30938,#30939,#30940,#30941),.UNSPECIFIED.,.F.,.F.,(4,1,1,1,1,1,
1,4),(59.4984349204034,59.9275442260809,60.9263366298489,61.9251290336169,
62.9239214373849,63.9227138411529,64.9215062449209,65.7816068796228),
 .UNSPECIFIED.);
#746=B_SPLINE_CURVE_WITH_KNOTS('',3,(#30943,#30944,#30945,#30946,#30947,
#30948,#30949,#30950,#30951,#30952,#30953,#30954,#30955,#30956,#30957,#30958,
#30959,#30960,#30961,#30962,#30963,#30964,#30965,#30966,#30967,#30968,#30969,
#30970,#30971,#30972,#30973,#30974,#30975,#30976,#30977,#30978,#30979,#30980,
#30981,#30982,#30983,#30984,#30985,#30986,#30987,#30988,#30989,#30990,#30991,
#30992,#30993,#30994,#30995,#30996,#30997,#30998,#30999,#31000,#31001,#31002,
#31003,#31004,#31005,#31006,#31007,#31008,#31009,#31010,#31011,#31012,#31013,
#31014,#31015,#31016,#31017,#31018,#31019,#31020,#31021,#31022,#31023,#31024,
#31025,#31026,#31027,#31028,#31029,#31030,#31031,#31032,#31033,#31034,#31035,
#31036,#31037,#31038,#31039,#31040,#31041,#31042,#31043,#31044,#31045,#31046,
#31047,#31048,#31049,#31050,#31051,#31052,#31053,#31054,#31055,#31056,#31057,
#31058,#31059,#31060,#31061,#31062,#31063,#31064,#31065,#31066,#31067,#31068,
#31069,#31070,#31071,#31072,#31073,#31074,#31075),.UNSPECIFIED.,.F.,.F.,
(4,3,3,3,3,3,3,3,3,3,3,3,3,3,3,3,3,3,3,3,3,3,3,3,3,3,3,3,3,3,3,3,3,3,3,
3,3,3,3,3,3,3,3,3,4),(65.7816149406508,65.9202986486889,66.0777245071298,
66.2348607637404,66.39182825848,66.5488763676339,66.7059724618319,66.8634081228024,
66.9190910524569,67.0765169108973,67.2336531675074,67.3906206622465,67.5476687713999,
67.7047648655973,67.8622005265673,67.9178834562249,68.0753093146652,68.2324455712754,
68.3894130660145,68.5464611751678,68.7035572693652,68.8609929303351,68.9166758599929,
69.0741017184334,69.2312379750437,69.3882054697829,69.5452535789364,69.702349673134,
69.8597853341041,69.915468263761,70.0728941222014,70.2300303788117,70.3869978735509,
70.5440459827043,70.7011420769017,70.8585777378718,70.914260667529,71.0716865259694,
71.2288227825796,71.3857902773188,71.5428383864722,71.6999344806696,71.8573701416396,
71.913053071297,72.0648002478303),.UNSPECIFIED.);
#747=B_SPLINE_CURVE_WITH_KNOTS('',3,(#31077,#31078,#31079,#31080,#31081,
#31082,#31083,#31084,#31085,#31086),.UNSPECIFIED.,.F.,.F.,(4,1,1,1,1,1,
1,4),(72.0648075666675,72.911845475065,73.910637878833,74.909430282601,
75.908222686369,76.9070150901371,77.9058074939051,78.3479810907392),
 .UNSPECIFIED.);
#748=B_SPLINE_CURVE_WITH_KNOTS('',3,(#31088,#31089,#31090,#31091,#31092,
#31093,#31094,#31095,#31096,#31097,#31098,#31099,#31100,#31101,#31102,#31103,
#31104,#31105,#31106,#31107,#31108,#31109,#31110,#31111,#31112,#31113,#31114,
#31115,#31116,#31117,#31118,#31119,#31120,#31121,#31122,#31123,#31124,#31125,
#31126,#31127,#31128,#31129,#31130,#31131,#31132,#31133,#31134,#31135,#31136,
#31137,#31138,#31139,#31140,#31141,#31142,#31143,#31144,#31145,#31146,#31147,
#31148,#31149,#31150,#31151,#31152,#31153,#31154,#31155,#31156,#31157,#31158,
#31159,#31160,#31161,#31162,#31163,#31164,#31165,#31166,#31167,#31168,#31169,
#31170,#31171,#31172,#31173,#31174,#31175,#31176,#31177,#31178,#31179,#31180,
#31181,#31182,#31183,#31184,#31185,#31186,#31187,#31188,#31189,#31190,#31191,
#31192,#31193,#31194,#31195,#31196,#31197,#31198,#31199,#31200,#31201,#31202,
#31203,#31204,#31205,#31206,#31207,#31208,#31209,#31210,#31211,#31212,#31213,
#31214,#31215,#31216,#31217,#31218,#31219,#31220),.UNSPECIFIED.,.F.,.F.,
(4,3,3,3,3,3,3,3,3,3,3,3,3,3,3,3,3,3,3,3,3,3,3,3,3,3,3,3,3,3,3,3,3,3,3,
3,3,3,3,3,3,3,3,3,4),(78.3479855550099,78.5091623284623,78.6705049083517,
78.8323302432885,78.9045998976731,79.0620257561135,79.2191620127237,79.3761295074628,
79.5331776166161,79.6902737108135,79.8477093717835,79.9033923014411,80.0608181598815,
80.2179544164917,80.3749219112309,80.5319700203843,80.6890661145817,80.8465017755518,
80.9021847052091,81.0596105636496,81.2167468202599,81.3737143149991,81.5307624241525,
81.6878585183501,81.8452941793201,81.9009771089771,82.0584029674175,82.2155392240278,
82.3725067187669,82.5295548279203,82.6866509221178,82.8440865830878,82.8997695127452,
83.0571953711857,83.214331627796,83.371299122535,83.5283472316885,83.685443325886,
83.8428789868561,83.8985619165132,84.0544346455478,84.2100324943769,84.3654623696513,
84.5209822278603,84.6311708621895),.UNSPECIFIED.);
#749=B_SPLINE_CURVE_WITH_KNOTS('',3,(#31222,#31223,#31224,#31225,#31226,
#31227,#31228,#31229,#31230,#31231,#31232,#31233,#31234,#31235,#31236,#31237,
#31238,#31239,#31240,#31241,#31242,#31243,#31244,#31245,#31246,#31247,#31248,
#31249,#31250,#31251,#31252,#31253,#31254,#31255,#31256,#31257,#31258,#31259,
#31260,#31261,#31262,#31263,#31264,#31265,#31266,#31267,#31268,#31269,#31270,
#31271,#31272,#31273,#31274,#31275,#31276,#31277,#31278,#31279,#31280,#31281,
#31282,#31283,#31284,#31285,#31286,#31287,#31288,#31289,#31290,#31291,#31292,
#31293,#31294,#31295,#31296,#31297,#31298,#31299,#31300,#31301,#31302,#31303,
#31304,#31305,#31306,#31307,#31308,#31309,#31310,#31311,#31312,#31313,#31314,
#31315,#31316,#31317,#31318,#31319,#31320,#31321,#31322,#31323,#31324,#31325,
#31326,#31327,#31328,#31329,#31330,#31331,#31332,#31333,#31334,#31335,#31336,
#31337,#31338,#31339,#31340,#31341,#31342,#31343,#31344,#31345,#31346,#31347,
#31348,#31349,#31350,#31351,#31352,#31353,#31354,#31355,#31356,#31357),
 .UNSPECIFIED.,.F.,.F.,(4,3,3,3,3,3,3,3,3,3,3,3,3,3,3,3,3,3,3,3,3,3,3,3,
3,3,3,3,3,3,3,3,3,3,3,3,3,3,3,3,3,3,3,3,3,4),(84.6311708623796,84.8301583421363,
84.8973543202812,85.0547801787217,85.211916435332,85.3688839300712,85.5259320392247,
85.6830281334222,85.8404637943923,85.8961467240492,86.0535725824896,86.2107088390998,
86.367676333839,86.5247244429924,86.6818205371899,86.8392561981599,86.8949391278172,
87.0523649862576,87.2095012428678,87.366468737607,87.5235168467604,87.6806129409579,
87.8380486019279,87.8937315315852,88.0511573900256,88.2082936466359,88.365261141375,
88.5223092505284,88.6794053447259,88.8368410056959,88.8925239353532,89.0499497937936,
89.2070860504038,89.364053545143,89.5211016542964,89.6781977484939,89.8356334094639,
89.8913163391212,90.0487421975616,90.2058784541718,90.362845948911,90.5198940580644,
90.6769901522618,90.8344258132319,90.8901087428892,90.9143561693691),
 .UNSPECIFIED.);
#750=B_SPLINE_CURVE_WITH_KNOTS('',3,(#31359,#31360,#31361,#31362,#31363,
#31364,#31365,#31366,#31367,#31368,#31369,#31370,#31371,#31372,#31373,#31374,
#31375,#31376,#31377,#31378,#31379,#31380,#31381,#31382,#31383,#31384,#31385,
#31386,#31387,#31388,#31389,#31390,#31391,#31392,#31393,#31394,#31395,#31396,
#31397,#31398,#31399,#31400,#31401,#31402,#31403,#31404,#31405,#31406,#31407,
#31408,#31409,#31410,#31411,#31412,#31413,#31414,#31415,#31416,#31417,#31418,
#31419,#31420,#31421,#31422,#31423,#31424,#31425,#31426,#31427,#31428,#31429,
#31430,#31431,#31432,#31433,#31434,#31435,#31436,#31437,#31438,#31439,#31440,
#31441,#31442,#31443,#31444,#31445,#31446,#31447,#31448,#31449,#31450,#31451,
#31452,#31453,#31454,#31455,#31456,#31457,#31458,#31459,#31460,#31461,#31462,
#31463,#31464,#31465,#31466,#31467,#31468,#31469,#31470,#31471,#31472,#31473,
#31474,#31475,#31476,#31477,#31478,#31479,#31480,#31481,#31482,#31483,#31484,
#31485,#31486,#31487,#31488,#31489,#31490,#31491),.UNSPECIFIED.,.F.,.F.,
(4,3,3,3,3,3,3,3,3,3,3,3,3,3,3,3,3,3,3,3,3,3,3,3,3,3,3,3,3,3,3,3,3,3,3,
3,3,3,3,3,3,3,3,3,4),(90.9143561695458,91.071136765442,91.2276311674691,
91.3839622773045,91.540377642471,91.696849766663,91.8536526876333,91.8889011466572,
92.0463270050976,92.2034632617077,92.3604307564468,92.5174788656002,92.6745749597977,
92.8320106207677,92.8876935504252,93.0451194088657,93.202255665476,93.3592231602152,
93.5162712693686,93.6733673635661,93.8308030245362,93.8864859541933,94.0439118126337,
94.2010480692439,94.358015563983,94.5150636731364,94.6721597673337,94.8295954283037,
94.8852783579613,95.0427042164017,95.1998404730119,95.3568079677511,95.5138560769045,
95.6709521711019,95.8283878320719,95.8840707617293,96.0414966201698,96.19863287678,
96.3556003715192,96.5126484806726,96.6697445748702,96.8271802358402,96.8828631654974,
97.0702592987996,97.1975412690878),.UNSPECIFIED.);
#751=B_SPLINE_CURVE_WITH_KNOTS('',3,(#31493,#31494,#31495,#31496,#31497,
#31498,#31499,#31500,#31501,#31502),.UNSPECIFIED.,.F.,.F.,(4,1,1,1,1,1,
1,4),(97.1975414765487,97.8816555692654,98.8804479730334,99.8792403768014,
100.878032780569,101.876825184337,102.875617588105,103.480726783728),
 .UNSPECIFIED.);
#752=B_SPLINE_CURVE_WITH_KNOTS('',3,(#31504,#31505,#31506,#31507,#31508,
#31509,#31510,#31511,#31512,#31513,#31514,#31515,#31516,#31517,#31518,#31519,
#31520,#31521,#31522,#31523,#31524,#31525,#31526,#31527,#31528,#31529,#31530,
#31531,#31532,#31533,#31534,#31535,#31536,#31537,#31538,#31539,#31540,#31541,
#31542,#31543,#31544,#31545,#31546,#31547,#31548,#31549,#31550,#31551,#31552,
#31553,#31554,#31555,#31556,#31557,#31558,#31559,#31560,#31561,#31562,#31563,
#31564,#31565,#31566,#31567,#31568,#31569,#31570,#31571,#31572,#31573,#31574,
#31575,#31576,#31577,#31578,#31579,#31580,#31581,#31582,#31583,#31584,#31585,
#31586,#31587,#31588,#31589,#31590,#31591,#31592,#31593,#31594,#31595,#31596,
#31597,#31598,#31599,#31600,#31601,#31602,#31603,#31604,#31605,#31606,#31607,
#31608,#31609,#31610,#31611,#31612,#31613,#31614,#31615,#31616,#31617,#31618,
#31619,#31620,#31621,#31622,#31623,#31624,#31625,#31626,#31627,#31628,#31629,
#31630,#31631,#31632,#31633,#31634,#31635,#31636),.UNSPECIFIED.,.F.,.F.,
(4,3,3,3,3,3,3,3,3,3,3,3,3,3,3,3,3,3,3,3,3,3,3,3,3,3,3,3,3,3,3,3,3,3,3,
3,3,3,3,3,3,3,3,3,4),(103.480727012744,103.654990565238,103.830634353272,
103.874409991873,104.031835850313,104.188972106924,104.345939601663,104.502987710817,
104.660083805014,104.817519465984,104.873202395641,105.030628254081,105.187764510692,
105.344732005431,105.501780114584,105.658876208782,105.816311869752,105.871994799409,
106.029420657849,106.186556914459,106.343524409198,106.500572518352,106.657668612549,
106.815104273519,106.870787203177,107.028213061618,107.185349318228,107.342316812968,
107.499364922122,107.65646101632,107.81389667729,107.869579606946,108.027005465387,
108.184141721997,108.341109216736,108.49815732589,108.655253420087,108.812689081058,
108.868372010714,109.023793477623,109.178928442311,109.334014026415,109.48905446015,
109.644394363258,109.763912090679),.UNSPECIFIED.);
#753=B_SPLINE_CURVE_WITH_KNOTS('',3,(#31638,#31639,#31640,#31641,#31642,
#31643,#31644,#31645,#31646,#31647,#31648,#31649,#31650,#31651,#31652,#31653,
#31654,#31655,#31656,#31657,#31658,#31659,#31660,#31661,#31662,#31663,#31664,
#31665,#31666,#31667,#31668,#31669,#31670,#31671,#31672,#31673,#31674,#31675,
#31676,#31677,#31678,#31679,#31680,#31681,#31682,#31683,#31684,#31685,#31686,
#31687,#31688,#31689,#31690,#31691,#31692,#31693,#31694,#31695,#31696,#31697,
#31698,#31699,#31700,#31701,#31702,#31703,#31704,#31705,#31706,#31707,#31708,
#31709,#31710,#31711,#31712,#31713,#31714,#31715,#31716,#31717,#31718,#31719,
#31720,#31721,#31722,#31723,#31724,#31725,#31726,#31727,#31728,#31729,#31730,
#31731,#31732,#31733,#31734,#31735,#31736,#31737,#31738,#31739,#31740,#31741,
#31742,#31743,#31744,#31745,#31746,#31747,#31748,#31749,#31750,#31751,#31752,
#31753,#31754,#31755,#31756,#31757,#31758,#31759,#31760,#31761,#31762,#31763,
#31764,#31765,#31766,#31767,#31768,#31769,#31770),.UNSPECIFIED.,.F.,.F.,
(4,3,3,3,3,3,3,3,3,3,3,3,3,3,3,3,3,3,3,3,3,3,3,3,3,3,3,3,3,3,3,3,3,3,3,
3,3,3,3,3,3,3,3,3,4),(109.763912090908,109.867164414482,110.02459027292,
110.181726529529,110.338694024266,110.495742133417,110.652838227612,110.81027388858,
110.86595681825,111.023382676691,111.180518933301,111.337486428041,111.494534537194,
111.651630631392,111.809066292363,111.864749222018,112.022175080459,112.179311337069,
112.336278831809,112.493326940962,112.65042303516,112.80785869613,112.863541625786,
113.020967484226,113.178103740836,113.335071235575,113.492119344728,113.649215438926,
113.806651099895,113.862334029554,114.019759887994,114.176896144605,114.333863639344,
114.490911748497,114.648007842695,114.805443503665,114.861126433322,115.018552291763,
115.175688548373,115.332656043113,115.489704152267,115.646800246464,115.804235907435,
115.85991883709,116.047097398087),.UNSPECIFIED.);
#754=B_SPLINE_CURVE_WITH_KNOTS('',3,(#31772,#31773,#31774,#31775,#31776,
#31777,#31778,#31779,#31780,#31781),.UNSPECIFIED.,.F.,.F.,(4,1,1,1,1,1,
1,4),(116.047101897182,116.858711240858,117.857503644626,118.856296048394,
119.855088452162,120.85388085593,121.852673259698,122.330281021608),
 .UNSPECIFIED.);
#755=B_SPLINE_CURVE_WITH_KNOTS('',3,(#31783,#31784,#31785,#31786,#31787,
#31788,#31789,#31790,#31791,#31792,#31793,#31794,#31795,#31796,#31797,#31798,
#31799,#31800,#31801,#31802,#31803,#31804,#31805,#31806,#31807,#31808,#31809,
#31810,#31811,#31812,#31813,#31814,#31815,#31816,#31817,#31818,#31819,#31820,
#31821,#31822,#31823,#31824,#31825,#31826,#31827,#31828,#31829,#31830,#31831,
#31832,#31833,#31834,#31835,#31836,#31837,#31838,#31839,#31840,#31841,#31842,
#31843,#31844,#31845,#31846,#31847,#31848,#31849,#31850,#31851,#31852,#31853,
#31854,#31855,#31856,#31857,#31858,#31859,#31860,#31861,#31862,#31863,#31864,
#31865,#31866,#31867,#31868,#31869,#31870,#31871,#31872,#31873,#31874,#31875,
#31876,#31877,#31878,#31879,#31880,#31881,#31882,#31883,#31884,#31885,#31886,
#31887,#31888,#31889,#31890,#31891,#31892,#31893,#31894,#31895,#31896,#31897,
#31898,#31899,#31900,#31901,#31902,#31903,#31904,#31905,#31906,#31907,#31908,
#31909,#31910,#31911,#31912,#31913,#31914,#31915),.UNSPECIFIED.,.F.,.F.,
(4,3,3,3,3,3,3,3,3,3,3,3,3,3,3,3,3,3,3,3,3,3,3,3,3,3,3,3,3,3,3,3,3,3,3,
3,3,3,3,3,3,3,3,3,4),(122.330282705267,122.493467815871,122.656917583374,
122.820901647644,122.851465663466,123.008891521906,123.166027778516,123.322995273255,
123.480043382409,123.637139476606,123.794575137576,123.850258067234,124.007683925674,
124.164820182285,124.321787677024,124.478835786177,124.635931880375,124.793367541345,
124.849050471002,125.006476329442,125.163612586053,125.320580080792,125.477628189945,
125.634724284143,125.792159945113,125.84784287477,126.00526873321,126.162404989821,
126.31937248456,126.476420593713,126.633516687911,126.790952348881,126.846635278538,
127.004061136978,127.161197393589,127.318164888328,127.475212997481,127.632309091679,
127.789744752649,127.845427682306,128.000825675512,128.155975118574,128.310962499579,
128.466097903113,128.613468012447),.UNSPECIFIED.);
#756=B_SPLINE_CURVE_WITH_KNOTS('',3,(#31917,#31918,#31919,#31920,#31921,
#31922,#31923,#31924,#31925,#31926,#31927),.UNSPECIFIED.,.F.,.F.,(4,1,1,
1,1,1,1,1,4),(128.613468012447,128.844220086074,129.843012489842,130.84180489361,
131.840597297378,132.839389701146,133.838182104914,134.836974508682,134.896653319626),
 .UNSPECIFIED.);
#757=B_SPLINE_CURVE_WITH_KNOTS('',3,(#31929,#31930,#31931,#31932,#31933,
#31934,#31935,#31936,#31937,#31938,#31939,#31940,#31941,#31942,#31943,#31944,
#31945,#31946,#31947,#31948,#31949,#31950,#31951,#31952,#31953,#31954,#31955,
#31956,#31957,#31958,#31959,#31960,#31961,#31962,#31963,#31964,#31965,#31966,
#31967,#31968,#31969,#31970,#31971,#31972,#31973,#31974,#31975,#31976,#31977,
#31978,#31979,#31980,#31981,#31982,#31983,#31984,#31985,#31986,#31987,#31988,
#31989,#31990,#31991,#31992,#31993,#31994,#31995,#31996,#31997,#31998,#31999,
#32000,#32001,#32002,#32003,#32004,#32005,#32006,#32007,#32008,#32009,#32010,
#32011,#32012,#32013,#32014,#32015,#32016,#32017,#32018,#32019,#32020,#32021,
#32022,#32023,#32024,#32025,#32026,#32027,#32028,#32029,#32030,#32031,#32032,
#32033,#32034,#32035,#32036,#32037,#32038,#32039,#32040,#32041,#32042,#32043,
#32044,#32045,#32046,#32047,#32048,#32049,#32050,#32051,#32052,#32053,#32054,
#32055,#32056,#32057,#32058),.UNSPECIFIED.,.F.,.F.,(4,3,3,3,3,3,3,3,3,3,
3,3,3,3,3,3,3,3,3,3,3,3,3,3,3,3,3,3,3,3,3,3,3,3,3,3,3,3,3,3,3,3,3,4),(134.896653319626,
135.05266364742,135.208399238582,135.365241157049,135.520921408202,135.678344160326,
135.83576691245,135.99319277089,136.150329027501,136.30729652224,136.464344631393,
136.621440725591,136.778876386561,136.834559316218,136.991985174658,137.149121431269,
137.306088926008,137.463137035161,137.620233129359,137.777668790329,137.833351719986,
137.990777578426,138.147913835037,138.304881329776,138.461929438929,138.619025533127,
138.776461194097,138.832144123754,138.989569982194,139.146706238805,139.303673733544,
139.460721842697,139.617817936895,139.775253597865,139.830936527522,139.988362385962,
140.145498642573,140.302466137312,140.459514246465,140.616610340663,140.774046001633,
140.82972893129,141.010850350131,141.179838384518),.UNSPECIFIED.);
#758=B_SPLINE_CURVE_WITH_KNOTS('',3,(#32060,#32061,#32062,#32063,#32064,
#32065,#32066,#32067,#32068,#32069),.UNSPECIFIED.,.F.,.F.,(4,1,1,1,1,1,
1,4),(141.179838626806,141.828521335058,142.827313738826,143.826106142594,
144.824898546362,145.82369095013,146.822483353898,147.463023933985),
 .UNSPECIFIED.);
#759=B_SPLINE_CURVE_WITH_KNOTS('',3,(#32071,#32072,#32073,#32074,#32075,
#32076,#32077,#32078,#32079,#32080,#32081,#32082,#32083,#32084,#32085,#32086,
#32087,#32088,#32089,#32090,#32091,#32092,#32093,#32094,#32095,#32096,#32097,
#32098,#32099,#32100,#32101,#32102,#32103,#32104,#32105,#32106,#32107,#32108,
#32109,#32110,#32111,#32112,#32113,#32114,#32115,#32116,#32117,#32118,#32119,
#32120,#32121,#32122,#32123,#32124,#32125,#32126,#32127,#32128,#32129,#32130,
#32131,#32132,#32133,#32134,#32135,#32136,#32137,#32138,#32139,#32140,#32141,
#32142,#32143,#32144,#32145,#32146,#32147,#32148,#32149,#32150,#32151,#32152,
#32153,#32154,#32155,#32156,#32157,#32158,#32159,#32160,#32161,#32162,#32163,
#32164,#32165,#32166,#32167,#32168,#32169,#32170,#32171,#32172,#32173,#32174,
#32175,#32176,#32177,#32178,#32179,#32180,#32181,#32182,#32183,#32184,#32185,
#32186,#32187,#32188,#32189,#32190,#32191,#32192,#32193,#32194,#32195,#32196,
#32197,#32198,#32199,#32200),.UNSPECIFIED.,.F.,.F.,(4,3,3,3,3,3,3,3,3,3,
3,3,3,3,3,3,3,3,3,3,3,3,3,3,3,3,3,3,3,3,3,3,3,3,3,3,3,3,3,3,3,3,3,4),(147.463024178982,
147.642892926041,147.821275757666,147.978701616106,148.135837872716,148.292805367455,
148.449853476608,148.606949570805,148.764385231775,148.820068161434,148.977494019874,
149.134630276485,149.291597771224,149.448645880377,149.605741974574,149.763177635544,
149.818860565202,149.976286423642,150.133422680253,150.290390174992,150.447438284145,
150.604534378343,150.761970039313,150.81765296897,150.97507882741,151.132215084021,
151.28918257876,151.446230687913,151.603326782111,151.760762443081,151.816445372738,
151.973871231178,152.131007487789,152.287974982528,152.445023091681,152.602119185878,
152.759554846848,152.815237776506,152.971139595369,153.126754540017,153.282331372718,
153.437859901489,153.593727172196,153.746209241165),.UNSPECIFIED.);
#760=B_SPLINE_CURVE_WITH_KNOTS('',3,(#32202,#32203,#32204,#32205,#32206,
#32207,#32208,#32209,#32210,#32211,#32212),.UNSPECIFIED.,.F.,.F.,(4,1,1,
1,1,1,1,1,4),(153.746209241165,153.814030180274,154.812822584042,155.81161498781,
156.810407391578,157.809199795346,158.807992199114,159.806784602882,160.029394548344),
 .UNSPECIFIED.);
#761=B_SPLINE_CURVE_WITH_KNOTS('',3,(#32214,#32215,#32216,#32217,#32218,
#32219,#32220,#32221,#32222,#32223,#32224,#32225,#32226,#32227,#32228,#32229,
#32230,#32231,#32232,#32233,#32234,#32235,#32236,#32237,#32238,#32239,#32240,
#32241,#32242,#32243,#32244,#32245,#32246,#32247,#32248,#32249,#32250,#32251,
#32252,#32253,#32254,#32255,#32256,#32257,#32258,#32259,#32260,#32261,#32262,
#32263,#32264,#32265,#32266,#32267,#32268,#32269,#32270,#32271,#32272,#32273,
#32274,#32275,#32276,#32277,#32278,#32279,#32280,#32281,#32282,#32283,#32284,
#32285,#32286,#32287,#32288,#32289,#32290,#32291,#32292,#32293,#32294,#32295,
#32296,#32297,#32298,#32299,#32300,#32301,#32302,#32303,#32304,#32305,#32306,
#32307,#32308,#32309,#32310,#32311,#32312,#32313,#32314,#32315,#32316,#32317,
#32318,#32319,#32320,#32321,#32322,#32323,#32324,#32325,#32326,#32327,#32328,
#32329,#32330,#32331,#32332,#32333,#32334,#32335,#32336,#32337,#32338,#32339,
#32340,#32341,#32342,#32343,#32344,#32345,#32346),.UNSPECIFIED.,.F.,.F.,
(4,3,3,3,3,3,3,3,3,3,3,3,3,3,3,3,3,3,3,3,3,3,3,3,3,3,3,3,3,3,3,3,3,3,3,
3,3,3,3,3,3,3,3,3,4),(160.029394548344,160.184418985519,160.339708490802,
160.494663051404,160.650120029027,160.80557700665,160.96300286509,161.1201391217,
161.27710661644,161.434154725593,161.59125081979,161.74868648076,161.804369410418,
161.961795268858,162.118931525469,162.275899020208,162.432947129361,162.590043223559,
162.747478884529,162.803161814186,162.960587672626,163.117723929237,163.274691423976,
163.431739533129,163.588835627327,163.746271288297,163.801954217954,163.959380076394,
164.116516333005,164.273483827744,164.430531936897,164.587628031094,164.745063692064,
164.800746621722,164.958172480162,165.115308736773,165.272276231512,165.429324340665,
165.586420434863,165.743856095833,165.79953902549,165.96400090799,166.12802293368,
166.291588382925,166.312579855524),.UNSPECIFIED.);
#762=B_SPLINE_CURVE_WITH_KNOTS('',3,(#32348,#32349,#32350,#32351,#32352,
#32353,#32354,#32355,#32356,#32357),.UNSPECIFIED.,.F.,.F.,(4,1,1,1,1,1,
1,4),(166.31258091617,166.798331429258,167.797123833026,168.795916236794,
169.794708640562,170.79350104433,171.792293448098,172.595761427539),
 .UNSPECIFIED.);
#763=B_SPLINE_CURVE_WITH_KNOTS('',3,(#32359,#32360,#32361,#32362,#32363,
#32364,#32365,#32366,#32367,#32368,#32369,#32370,#32371,#32372,#32373,#32374,
#32375,#32376,#32377,#32378,#32379,#32380,#32381,#32382,#32383,#32384,#32385,
#32386,#32387,#32388,#32389,#32390,#32391,#32392,#32393,#32394,#32395,#32396,
#32397,#32398,#32399,#32400,#32401,#32402,#32403,#32404,#32405,#32406,#32407,
#32408,#32409,#32410,#32411,#32412,#32413,#32414,#32415,#32416,#32417,#32418,
#32419,#32420,#32421,#32422,#32423,#32424,#32425,#32426,#32427,#32428,#32429,
#32430,#32431,#32432,#32433,#32434,#32435,#32436,#32437,#32438,#32439,#32440,
#32441,#32442,#32443,#32444,#32445,#32446,#32447,#32448,#32449,#32450,#32451,
#32452,#32453,#32454,#32455,#32456,#32457,#32458,#32459,#32460,#32461,#32462,
#32463,#32464,#32465,#32466,#32467,#32468,#32469,#32470,#32471,#32472,#32473,
#32474,#32475,#32476,#32477,#32478,#32479,#32480,#32481,#32482,#32483,#32484,
#32485,#32486,#32487,#32488,#32489,#32490,#32491),.UNSPECIFIED.,.F.,.F.,
(4,3,3,3,3,3,3,3,3,3,3,3,3,3,3,3,3,3,3,3,3,3,3,3,3,3,3,3,3,3,3,3,3,3,3,
3,3,3,3,3,3,3,3,3,4),(172.595765162704,172.791085851866,172.948511710308,
173.105647966921,173.262615461662,173.419663570818,173.576759665017,173.734195325989,
173.789878255634,173.947304114074,174.104440370684,174.261407865423,174.418455974576,
174.575552068773,174.732987729743,174.788670659402,174.946096517842,175.103232774452,
175.260200269191,175.417248378344,175.574344472541,175.731780133511,175.78746306317,
175.944888921611,176.102025178221,176.25899267296,176.416040782114,176.573136876312,
176.730572537282,176.786255466938,176.943681325378,177.100817581989,177.257785076728,
177.414833185881,177.571929280079,177.729364941049,177.785047870706,177.942473729146,
178.099609985756,178.256577480495,178.413625589649,178.570721683846,178.728157344816,
178.783840274474,178.878950469883),.UNSPECIFIED.);
#764=B_SPLINE_CURVE_WITH_KNOTS('',3,(#32493,#32494,#32495,#32496,#32497,
#32498,#32499,#32500,#32501,#32502),.UNSPECIFIED.,.F.,.F.,(4,1,1,1,1,1,
1,4),(178.878959343412,179.782632678242,180.781425082011,181.780217485779,
182.779009889547,183.777802293315,184.776594697083,185.162128430314),
 .UNSPECIFIED.);
#765=B_SPLINE_CURVE_WITH_KNOTS('',3,(#32504,#32505,#32506,#32507,#32508,
#32509,#32510,#32511,#32512,#32513,#32514,#32515,#32516,#32517,#32518,#32519,
#32520,#32521,#32522,#32523,#32524,#32525,#32526,#32527,#32528,#32529,#32530,
#32531,#32532,#32533,#32534,#32535,#32536,#32537,#32538,#32539,#32540,#32541,
#32542,#32543,#32544,#32545,#32546,#32547,#32548,#32549,#32550,#32551,#32552,
#32553,#32554,#32555,#32556,#32557,#32558,#32559,#32560,#32561,#32562,#32563,
#32564,#32565,#32566,#32567,#32568,#32569,#32570,#32571,#32572,#32573,#32574,
#32575,#32576,#32577,#32578,#32579,#32580,#32581,#32582,#32583,#32584,#32585,
#32586,#32587,#32588,#32589,#32590,#32591,#32592,#32593,#32594,#32595,#32596,
#32597,#32598,#32599,#32600,#32601,#32602,#32603,#32604,#32605,#32606,#32607,
#32608,#32609,#32610,#32611,#32612,#32613,#32614,#32615,#32616,#32617,#32618,
#32619,#32620,#32621,#32622,#32623,#32624,#32625,#32626,#32627,#32628,#32629,
#32630,#32631,#32632,#32633,#32634,#32635,#32636),.UNSPECIFIED.,.F.,.F.,
(4,3,3,3,3,3,3,3,3,3,3,3,3,3,3,3,3,3,3,3,3,3,3,3,3,3,3,3,3,3,3,3,3,3,3,
3,3,3,3,3,3,3,3,3,4),(185.162135777063,185.320796314776,185.479504458316,
185.638644472916,185.775387100851,185.932812959291,186.089949215902,186.246916710641,
186.403964819794,186.561060913992,186.718496574962,186.774179504619,186.931605363059,
187.08874161967,187.245709114409,187.402757223562,187.559853317759,187.717288978729,
187.772971908387,187.930397766827,188.087534023438,188.244501518177,188.401549627331,
188.558645721528,188.716081382498,188.771764312155,188.929190170595,189.086326427206,
189.243293921945,189.400342031098,189.557438125296,189.714873786266,189.770556715923,
189.927982574364,190.085118830974,190.242086325713,190.399134434867,190.556230529064,
190.713666190034,190.769349119691,190.926450963375,191.083227689836,191.239819279954,
191.396408525495,191.445321084242),.UNSPECIFIED.);
#766=B_SPLINE_CURVE_WITH_KNOTS('',3,(#32638,#32639,#32640,#32641,#32642,
#32643,#32644,#32645,#32646,#32647,#32648,#32649,#32650,#32651,#32652,#32653,
#32654,#32655,#32656,#32657,#32658,#32659,#32660,#32661,#32662,#32663,#32664,
#32665,#32666,#32667,#32668,#32669,#32670,#32671,#32672,#32673,#32674,#32675,
#32676,#32677,#32678,#32679,#32680,#32681,#32682,#32683,#32684,#32685,#32686,
#32687,#32688,#32689,#32690,#32691,#32692,#32693,#32694,#32695,#32696,#32697,
#32698,#32699,#32700,#32701,#32702,#32703,#32704,#32705,#32706,#32707,#32708,
#32709,#32710,#32711,#32712,#32713,#32714,#32715,#32716,#32717,#32718,#32719,
#32720,#32721,#32722,#32723,#32724,#32725,#32726,#32727,#32728,#32729,#32730,
#32731,#32732,#32733,#32734,#32735,#32736,#32737,#32738,#32739,#32740,#32741,
#32742,#32743,#32744,#32745,#32746,#32747,#32748,#32749,#32750,#32751,#32752,
#32753,#32754,#32755,#32756,#32757,#32758,#32759,#32760,#32761,#32762,#32763,
#32764,#32765,#32766,#32767,#32768,#32769,#32770),.UNSPECIFIED.,.F.,.F.,
(4,3,3,3,3,3,3,3,3,3,3,3,3,3,3,3,3,3,3,3,3,3,3,3,3,3,3,3,3,3,3,3,3,3,3,
3,3,3,3,3,3,3,3,3,4),(191.44532108445,191.631142952482,191.768141523459,
191.925567381899,192.082703638508,192.239671133246,192.396719242399,192.553815336595,
192.711250997564,192.766933927227,192.924359785667,193.081496042278,193.238463537017,
193.39551164617,193.552607740368,193.710043401338,193.765726330995,193.923152189436,
194.080288446046,194.237255940785,194.394304049939,194.551400144136,194.708835805107,
194.764518734763,194.921944593203,195.079080849813,195.236048344553,195.393096453706,
195.550192547903,195.707628208873,195.763311138531,195.920736996971,196.077873253582,
196.234840748321,196.391888857474,196.548984951672,196.706420612642,196.762103542299,
196.918699351543,197.075007110055,197.238381930338,197.39460584084,197.550891671694,
197.70749924213,197.728506391186),.UNSPECIFIED.);
#767=B_SPLINE_CURVE_WITH_KNOTS('',3,(#32772,#32773,#32774,#32775,#32776,
#32777,#32778,#32779,#32780,#32781,#32782,#32783,#32784,#32785,#32786,#32787,
#32788,#32789,#32790,#32791,#32792,#32793,#32794,#32795,#32796,#32797,#32798,
#32799,#32800,#32801,#32802,#32803,#32804,#32805,#32806,#32807,#32808,#32809,
#32810,#32811,#32812,#32813,#32814,#32815,#32816,#32817,#32818,#32819,#32820,
#32821,#32822,#32823,#32824,#32825,#32826,#32827,#32828,#32829,#32830,#32831,
#32832,#32833,#32834,#32835,#32836,#32837,#32838,#32839,#32840,#32841,#32842,
#32843,#32844,#32845,#32846,#32847,#32848,#32849,#32850,#32851,#32852,#32853,
#32854,#32855,#32856,#32857,#32858,#32859,#32860,#32861,#32862,#32863,#32864,
#32865,#32866,#32867,#32868,#32869,#32870,#32871,#32872,#32873,#32874,#32875,
#32876,#32877,#32878,#32879,#32880,#32881,#32882,#32883,#32884,#32885,#32886,
#32887,#32888,#32889,#32890,#32891,#32892,#32893,#32894,#32895,#32896,#32897,
#32898,#32899,#32900,#32901,#32902,#32903,#32904,#32905,#32906,#32907),
 .UNSPECIFIED.,.F.,.F.,(4,3,3,3,3,3,3,3,3,3,3,3,3,3,3,3,3,3,3,3,3,3,3,3,
3,3,3,3,3,3,3,3,3,3,3,3,3,3,3,3,3,3,3,3,3,4),(197.728506391422,197.760895946067,
197.918321804507,198.075458061117,198.232425555857,198.38947366501,198.546569759207,
198.704005420177,198.759688349835,198.917114208275,199.074250464886,199.231217959625,
199.388266068778,199.545362162976,199.702797823946,199.758480753603,199.915906612043,
200.073042868654,200.230010363393,200.387058472546,200.544154566744,200.701590227714,
200.757273157371,200.914699015811,201.071835272422,201.228802767161,201.385850876314,
201.542946970511,201.700382631481,201.756065561139,201.913491419579,202.07062767619,
202.227595170929,202.384643280082,202.54173937428,202.69917503525,202.754857964907,
202.912283823348,203.069420079958,203.226387574697,203.383435683851,203.540531778049,
203.697967439019,203.753650368675,203.955064998701,204.011691621862),
 .UNSPECIFIED.);
#768=B_SPLINE_CURVE_WITH_KNOTS('',3,(#32909,#32910,#32911,#32912,#32913,
#32914,#32915,#32916,#32917,#32918),.UNSPECIFIED.,.F.,.F.,(4,1,1,1,1,1,
1,4),(204.011691698601,204.752442772443,205.751235176211,206.750027579979,
207.748819983747,208.747612387515,209.746404791283,210.294877005781),
 .UNSPECIFIED.);
#769=B_SPLINE_CURVE_WITH_KNOTS('',3,(#32920,#32921,#32922,#32923,#32924,
#32925,#32926,#32927,#32928,#32929,#32930,#32931,#32932,#32933,#32934,#32935,
#32936,#32937,#32938,#32939,#32940,#32941,#32942,#32943,#32944,#32945,#32946,
#32947,#32948,#32949,#32950,#32951,#32952,#32953,#32954,#32955,#32956,#32957,
#32958,#32959,#32960,#32961,#32962,#32963,#32964,#32965,#32966,#32967,#32968,
#32969,#32970,#32971,#32972,#32973,#32974,#32975,#32976,#32977,#32978,#32979,
#32980,#32981,#32982,#32983,#32984,#32985,#32986,#32987,#32988,#32989,#32990,
#32991,#32992,#32993,#32994,#32995,#32996,#32997,#32998,#32999,#33000,#33001,
#33002,#33003,#33004,#33005,#33006,#33007,#33008,#33009,#33010,#33011,#33012,
#33013,#33014,#33015,#33016,#33017,#33018,#33019,#33020,#33021,#33022,#33023,
#33024,#33025,#33026,#33027,#33028,#33029,#33030,#33031,#33032,#33033,#33034,
#33035,#33036,#33037,#33038,#33039,#33040,#33041,#33042,#33043,#33044,#33045,
#33046,#33047,#33048,#33049,#33050,#33051,#33052),.UNSPECIFIED.,.F.,.F.,
(4,3,3,3,3,3,3,3,3,3,3,3,3,3,3,3,3,3,3,3,3,3,3,3,3,3,3,3,3,3,3,3,3,3,3,
3,3,3,3,3,3,3,3,3,4),(210.294877264932,210.46333437215,210.632735937725,
210.745197195051,210.902623053491,211.059759310102,211.216726804841,211.373774913994,
211.530871008192,211.688306669162,211.743989598819,211.901415457259,212.05855171387,
212.215519208609,212.372567317762,212.52966341196,212.68709907293,212.742782002587,
212.900207861027,213.057344117638,213.214311612377,213.37135972153,213.528455815728,
213.685891476698,213.741574406355,213.899000264795,214.056136521406,214.213104016145,
214.370152125298,214.527248219496,214.684683880466,214.740366810123,214.897792668563,
215.054928925173,215.211896419913,215.368944529066,215.526040623263,215.683476284233,
215.739159213891,215.894242030097,216.04903664284,216.203757367494,216.358434417139,
216.513343457364,216.578062312961),.UNSPECIFIED.);
#770=B_SPLINE_CURVE_WITH_KNOTS('',3,(#33054,#33055,#33056,#33057,#33058,
#33059,#33060,#33061,#33062,#33063,#33064),.UNSPECIFIED.,.F.,.F.,(4,1,1,
1,1,1,1,1,4),(216.578062312961,216.737951617659,217.736744021427,218.735536425195,
219.734328828963,220.733121232731,221.731913636499,222.730706040267,222.86124762014),
 .UNSPECIFIED.);
#771=B_SPLINE_CURVE_WITH_KNOTS('',3,(#33066,#33067,#33068,#33069,#33070,
#33071,#33072,#33073,#33074,#33075,#33076,#33077,#33078,#33079,#33080,#33081,
#33082,#33083,#33084,#33085,#33086,#33087,#33088,#33089,#33090,#33091,#33092,
#33093,#33094,#33095,#33096,#33097,#33098,#33099,#33100,#33101,#33102,#33103,
#33104,#33105,#33106,#33107,#33108,#33109,#33110,#33111,#33112,#33113,#33114,
#33115,#33116,#33117,#33118,#33119,#33120,#33121,#33122,#33123,#33124,#33125,
#33126,#33127,#33128,#33129,#33130,#33131,#33132,#33133,#33134,#33135,#33136,
#33137,#33138,#33139,#33140,#33141,#33142,#33143,#33144,#33145,#33146,#33147,
#33148,#33149,#33150,#33151,#33152,#33153,#33154,#33155,#33156,#33157,#33158,
#33159,#33160,#33161,#33162,#33163,#33164,#33165,#33166,#33167,#33168,#33169,
#33170,#33171,#33172,#33173,#33174,#33175,#33176,#33177,#33178,#33179,#33180,
#33181,#33182,#33183,#33184,#33185,#33186,#33187,#33188,#33189,#33190,#33191,
#33192,#33193,#33194,#33195,#33196,#33197,#33198),.UNSPECIFIED.,.F.,.F.,
(4,3,3,3,3,3,3,3,3,3,3,3,3,3,3,3,3,3,3,3,3,3,3,3,3,3,3,3,3,3,3,3,3,3,3,
3,3,3,3,3,3,3,3,3,4),(222.86124762014,223.016316100705,223.171149712576,
223.326001519616,223.480853724508,223.636041436024,223.729498444035,223.886924302475,
224.044060559086,224.201028053825,224.358076162978,224.515172257176,224.672607918146,
224.728290847803,224.885716706243,225.042852962854,225.199820457593,225.356868566746,
225.513964660944,225.671400321914,225.727083251571,225.884509110011,226.041645366622,
226.198612861361,226.355660970514,226.512757064712,226.670192725682,226.725875655339,
226.883301513779,227.04043777039,227.197405265129,227.354453374282,227.51154946848,
227.66898512945,227.724668059107,227.882093917547,228.039230174158,228.196197668897,
228.35324577805,228.510341872248,228.667777533218,228.723460462875,228.895945905797,
229.067330276234,229.144432927137),.UNSPECIFIED.);
#772=B_SPLINE_CURVE_WITH_KNOTS('',3,(#33200,#33201,#33202,#33203,#33204,
#33205,#33206,#33207,#33208,#33209,#33210,#33211,#33212,#33213,#33214,#33215,
#33216,#33217,#33218,#33219,#33220,#33221,#33222,#33223,#33224,#33225,#33226,
#33227,#33228,#33229,#33230,#33231,#33232,#33233,#33234,#33235,#33236,#33237,
#33238,#33239,#33240,#33241,#33242,#33243,#33244,#33245,#33246,#33247,#33248,
#33249,#33250,#33251,#33252,#33253,#33254,#33255,#33256,#33257,#33258,#33259,
#33260,#33261,#33262,#33263,#33264,#33265,#33266,#33267,#33268,#33269,#33270,
#33271,#33272,#33273,#33274,#33275,#33276,#33277,#33278,#33279,#33280,#33281,
#33282,#33283,#33284,#33285,#33286,#33287,#33288,#33289,#33290,#33291,#33292,
#33293,#33294,#33295,#33296,#33297,#33298,#33299,#33300,#33301,#33302,#33303,
#33304,#33305,#33306,#33307,#33308,#33309,#33310,#33311,#33312,#33313,#33314,
#33315,#33316,#33317,#33318,#33319,#33320,#33321,#33322,#33323,#33324,#33325,
#33326,#33327,#33328,#33329,#33330,#33331,#33332),.UNSPECIFIED.,.F.,.F.,
(4,3,3,3,3,3,3,3,3,3,3,3,3,3,3,3,3,3,3,3,3,3,3,3,3,3,3,3,3,3,3,3,3,3,3,
3,3,3,3,3,3,3,3,3,4),(229.14443292732,229.304574268111,229.464832452386,
229.625550244693,229.722252866643,229.879678725084,230.036814981694,230.193782476433,
230.350830585587,230.507926679784,230.665362340755,230.721045270411,230.878471128851,
231.035607385462,231.192574880201,231.349622989354,231.506719083552,231.664154744522,
231.719837674179,231.877263532619,232.03439978923,232.191367283969,232.348415393122,
232.50551148732,232.66294714829,232.718630077947,232.876055936387,233.033192192998,
233.190159687737,233.34720779689,233.504303891088,233.661739552058,233.717422481715,
233.874848340155,234.031984596766,234.188952091505,234.346000200658,234.503096294856,
234.660531955826,234.716214885483,234.872477893564,235.028448536676,235.184246088232,
235.34009904764,235.427618234499),.UNSPECIFIED.);
#773=B_SPLINE_CURVE_WITH_KNOTS('',3,(#33334,#33335,#33336,#33337,#33338,
#33339,#33340,#33341,#33342,#33343,#33344,#33345,#33346,#33347,#33348,#33349,
#33350,#33351,#33352,#33353,#33354,#33355,#33356,#33357,#33358,#33359,#33360,
#33361,#33362,#33363,#33364,#33365,#33366,#33367,#33368,#33369,#33370,#33371,
#33372,#33373,#33374,#33375,#33376,#33377,#33378,#33379,#33380,#33381,#33382,
#33383,#33384,#33385,#33386,#33387,#33388,#33389,#33390,#33391,#33392,#33393,
#33394,#33395,#33396,#33397,#33398,#33399,#33400,#33401,#33402,#33403,#33404,
#33405,#33406,#33407,#33408,#33409,#33410,#33411,#33412,#33413,#33414,#33415,
#33416,#33417,#33418,#33419,#33420,#33421,#33422,#33423,#33424,#33425,#33426,
#33427,#33428,#33429,#33430,#33431,#33432,#33433,#33434,#33435,#33436,#33437,
#33438,#33439,#33440,#33441,#33442,#33443,#33444,#33445,#33446,#33447,#33448,
#33449,#33450,#33451,#33452,#33453,#33454,#33455,#33456,#33457,#33458,#33459,
#33460,#33461,#33462,#33463,#33464,#33465,#33466,#33467,#33468,#33469),
 .UNSPECIFIED.,.F.,.F.,(4,3,3,3,3,3,3,3,3,3,3,3,3,3,3,3,3,3,3,3,3,3,3,3,
3,3,3,3,3,3,3,3,3,3,3,3,3,3,3,3,3,3,3,3,3,4),(235.427618234645,235.621005037013,
235.715007289251,235.872433147691,236.029569404302,236.186536899041,236.343585008195,
236.500681102392,236.658116763362,236.713799693019,236.871225551459,237.02836180807,
237.185329302809,237.342377411962,237.49947350616,237.65690916713,237.712592096787,
237.870017955227,238.027154211838,238.184121706577,238.34116981573,238.498265909927,
238.655701570897,238.711384500555,238.868810358995,239.025946615606,239.182914110345,
239.339962219498,239.497058313696,239.654493974666,239.710176904323,239.867602762763,
240.024739019374,240.181706514113,240.338754623266,240.495850717464,240.653286378434,
240.708969308091,240.866395166531,241.023531423141,241.18049891788,241.337547027033,
241.49464312123,241.6520787822,241.707761711859,241.710803541679),
 .UNSPECIFIED.);
#774=B_SPLINE_CURVE_WITH_KNOTS('',3,(#33471,#33472,#33473,#33474,#33475,
#33476,#33477,#33478,#33479,#33480,#33481,#33482,#33483,#33484,#33485,#33486,
#33487,#33488,#33489,#33490,#33491,#33492,#33493,#33494,#33495,#33496,#33497,
#33498,#33499,#33500,#33501,#33502,#33503,#33504,#33505,#33506,#33507,#33508,
#33509,#33510,#33511,#33512,#33513,#33514,#33515,#33516,#33517,#33518,#33519,
#33520,#33521,#33522,#33523,#33524,#33525,#33526,#33527,#33528,#33529,#33530,
#33531,#33532,#33533,#33534,#33535,#33536,#33537,#33538,#33539,#33540,#33541,
#33542,#33543,#33544,#33545,#33546,#33547,#33548,#33549,#33550,#33551,#33552,
#33553,#33554,#33555,#33556,#33557,#33558,#33559,#33560,#33561,#33562,#33563,
#33564,#33565,#33566,#33567,#33568,#33569,#33570,#33571,#33572,#33573,#33574,
#33575,#33576,#33577,#33578,#33579,#33580,#33581,#33582,#33583,#33584,#33585,
#33586,#33587,#33588,#33589,#33590,#33591,#33592,#33593,#33594,#33595,#33596,
#33597,#33598,#33599,#33600,#33601,#33602,#33603),.UNSPECIFIED.,.F.,.F.,
(4,3,3,3,3,3,3,3,3,3,3,3,3,3,3,3,3,3,3,3,3,3,3,3,3,3,3,3,3,3,3,3,3,3,3,
3,3,3,3,3,3,3,3,3,4),(241.710803541844,241.868143106838,242.02519326494,
242.1820751511,242.339037937249,242.496049703508,242.653399897405,242.706554115627,
242.863979974067,243.021116230678,243.178083725417,243.33513183457,243.492227928768,
243.649663589738,243.705346519395,243.862772377836,244.019908634446,244.176876129185,
244.333924238339,244.491020332536,244.648455993506,244.704138923163,244.861564781603,
245.018701038214,245.175668532953,245.332716642106,245.489812736304,245.647248397274,
245.702931326931,245.860357185371,246.017493441982,246.174460936721,246.331509045874,
246.488605140071,246.646040801041,246.701723730699,246.859149589139,247.01628584575,
247.173253340489,247.330301449642,247.48739754384,247.64483320481,247.700516134467,
247.89246141975,247.993988848699),.UNSPECIFIED.);
#775=B_SPLINE_CURVE_WITH_KNOTS('',3,(#33605,#33606,#33607,#33608,#33609,
#33610,#33611,#33612,#33613,#33614,#33615,#33616,#33617,#33618,#33619,#33620,
#33621,#33622,#33623,#33624,#33625,#33626,#33627,#33628,#33629,#33630,#33631,
#33632,#33633,#33634,#33635,#33636,#33637,#33638,#33639,#33640,#33641,#33642,
#33643,#33644,#33645,#33646,#33647,#33648,#33649,#33650,#33651,#33652,#33653,
#33654,#33655,#33656,#33657,#33658,#33659,#33660,#33661,#33662,#33663,#33664,
#33665,#33666,#33667,#33668,#33669,#33670,#33671,#33672,#33673,#33674,#33675,
#33676,#33677,#33678,#33679,#33680,#33681,#33682,#33683,#33684,#33685,#33686,
#33687,#33688,#33689,#33690,#33691,#33692,#33693,#33694,#33695,#33696,#33697,
#33698,#33699,#33700,#33701,#33702,#33703,#33704,#33705,#33706,#33707,#33708,
#33709,#33710,#33711,#33712,#33713,#33714,#33715,#33716,#33717,#33718,#33719,
#33720,#33721,#33722,#33723,#33724,#33725,#33726,#33727,#33728,#33729,#33730,
#33731,#33732,#33733,#33734,#33735,#33736,#33737),.UNSPECIFIED.,.F.,.F.,
(4,3,3,3,3,3,3,3,3,3,3,3,3,3,3,3,3,3,3,3,3,3,3,3,3,3,3,3,3,3,3,3,3,3,3,
3,3,3,3,3,3,3,3,3,4),(247.993988848858,248.149923326116,248.305914227325,
248.461931588476,248.618298001352,248.699308538235,248.856734396675,249.013870653285,
249.170838148025,249.327886257178,249.484982351375,249.642418012345,249.698100942003,
249.855526800444,250.012663057055,250.169630551794,250.326678660948,250.483774755146,
250.641210416116,250.696893345772,250.854319204212,251.011455460823,251.168422955562,
251.325471064715,251.482567158913,251.640002819883,251.69568574954,251.85311160798,
252.01024786459,252.167215359329,252.324263468482,252.48135956268,252.63879522365,
252.694478153308,252.851904011749,253.009040268359,253.166007763098,253.323055872252,
253.480151966449,253.637587627419,253.693270557076,253.853683463077,254.013749755245,
254.173572614727,254.277174156038),.UNSPECIFIED.);
#776=B_SPLINE_CURVE_WITH_KNOTS('',3,(#33739,#33740,#33741,#33742,#33743,
#33744,#33745,#33746,#33747,#33748,#33749,#33750,#33751,#33752,#33753,#33754,
#33755,#33756,#33757,#33758,#33759,#33760,#33761,#33762,#33763,#33764,#33765,
#33766,#33767,#33768,#33769,#33770,#33771,#33772,#33773,#33774,#33775,#33776,
#33777,#33778,#33779,#33780,#33781,#33782,#33783,#33784,#33785,#33786,#33787,
#33788,#33789,#33790,#33791,#33792,#33793,#33794,#33795,#33796,#33797,#33798,
#33799,#33800,#33801,#33802,#33803,#33804,#33805,#33806,#33807,#33808,#33809,
#33810,#33811,#33812,#33813,#33814,#33815,#33816,#33817,#33818,#33819,#33820,
#33821,#33822,#33823,#33824,#33825,#33826,#33827,#33828,#33829,#33830,#33831,
#33832,#33833,#33834,#33835,#33836,#33837,#33838,#33839,#33840,#33841,#33842,
#33843,#33844,#33845,#33846,#33847,#33848,#33849,#33850,#33851,#33852,#33853,
#33854,#33855,#33856,#33857,#33858,#33859,#33860,#33861,#33862,#33863,#33864,
#33865,#33866,#33867,#33868,#33869,#33870,#33871),.UNSPECIFIED.,.F.,.F.,
(4,3,3,3,3,3,3,3,3,3,3,3,3,3,3,3,3,3,3,3,3,3,3,3,3,3,3,3,3,3,3,3,3,3,3,
3,3,3,3,3,3,3,3,3,4),(254.27717415623,254.449061850417,254.622135068757,
254.692062960844,254.849488819284,255.006625075894,255.163592570633,255.320640679786,
255.477736773983,255.635172434953,255.690855364612,255.848281223052,256.005417479663,
256.162384974402,256.319433083555,256.476529177753,256.633964838723,256.68964776838,
256.84707362682,257.004209883431,257.16117737817,257.318225487324,257.475321581521,
257.632757242491,257.688440172148,257.845866030588,258.003002287199,258.159969781938,
258.317017891091,258.474113985288,258.631549646258,258.687232575916,258.844658434356,
259.001794690967,259.158762185706,259.315810294859,259.472906389057,259.630342050027,
259.686024979684,259.841258359922,259.996204973962,260.151093896897,260.305938742112,
260.461058165079,260.560359463218),.UNSPECIFIED.);
#777=B_SPLINE_CURVE_WITH_KNOTS('',3,(#33873,#33874,#33875,#33876,#33877,
#33878,#33879,#33880,#33881,#33882,#33883),.UNSPECIFIED.,.F.,.F.,(4,1,1,
1,1,1,1,1,4),(260.560359463218,260.684817383452,261.68360978722,262.682402190988,
263.681194594756,264.679986998524,265.678779402292,266.67757180606,266.843544770397),
 .UNSPECIFIED.);
#778=B_SPLINE_CURVE_WITH_KNOTS('',3,(#33885,#33886,#33887,#33888,#33889,
#33890,#33891,#33892,#33893,#33894,#33895,#33896,#33897,#33898,#33899,#33900,
#33901,#33902,#33903,#33904,#33905,#33906,#33907,#33908,#33909,#33910,#33911,
#33912,#33913,#33914,#33915,#33916,#33917,#33918,#33919,#33920,#33921,#33922,
#33923,#33924,#33925,#33926,#33927,#33928,#33929,#33930,#33931,#33932,#33933,
#33934,#33935,#33936,#33937,#33938,#33939,#33940,#33941,#33942,#33943,#33944,
#33945,#33946,#33947,#33948,#33949,#33950,#33951,#33952,#33953,#33954,#33955,
#33956,#33957,#33958,#33959,#33960,#33961,#33962,#33963,#33964,#33965,#33966,
#33967,#33968,#33969,#33970,#33971,#33972,#33973,#33974,#33975,#33976,#33977,
#33978,#33979,#33980,#33981,#33982,#33983,#33984,#33985,#33986,#33987,#33988,
#33989,#33990,#33991,#33992,#33993,#33994,#33995,#33996,#33997,#33998,#33999,
#34000,#34001,#34002,#34003,#34004,#34005,#34006,#34007,#34008,#34009,#34010,
#34011,#34012,#34013,#34014,#34015,#34016,#34017),.UNSPECIFIED.,.F.,.F.,
(4,3,3,3,3,3,3,3,3,3,3,3,3,3,3,3,3,3,3,3,3,3,3,3,3,3,3,3,3,3,3,3,3,3,3,
3,3,3,3,3,3,3,3,3,4),(266.843544770397,266.998437545715,267.153122139019,
267.3078484695,267.4625994556,267.617675353046,267.676364209828,267.833790068268,
267.990926324879,268.147893819617,268.304941928771,268.462038022968,268.619473683938,
268.675156613596,268.832582472036,268.989718728646,269.146686223386,269.303734332539,
269.460830426736,269.618266087706,269.673949017364,269.831374875804,269.988511132415,
270.145478627154,270.302526736308,270.459622830505,270.617058491475,270.672741421132,
270.830167279572,270.987303536183,271.144271030922,271.301319140075,271.458415234273,
271.615850895243,271.6715338249,271.82895968334,271.986095939951,272.14306343469,
272.300111543843,272.457207638041,272.614643299011,272.670326228668,272.839266884683,
273.007357802531,273.126729847806),.UNSPECIFIED.);
#779=B_SPLINE_CURVE_WITH_KNOTS('',3,(#34019,#34020,#34021,#34022,#34023,
#34024,#34025,#34026,#34027,#34028),.UNSPECIFIED.,.F.,.F.,(4,1,1,1,1,1,
1,4),(273.126730077577,273.669118632436,274.667911036204,275.666703439972,
276.66549584374,277.664288247508,278.663080651276,279.409915384756),
 .UNSPECIFIED.);
#780=B_SPLINE_CURVE_WITH_KNOTS('',3,(#34030,#34031,#34032,#34033,#34034,
#34035,#34036,#34037,#34038,#34039,#34040,#34041,#34042,#34043,#34044,#34045,
#34046,#34047,#34048,#34049,#34050,#34051,#34052,#34053,#34054,#34055,#34056,
#34057,#34058,#34059,#34060,#34061,#34062,#34063,#34064,#34065,#34066,#34067,
#34068,#34069,#34070,#34071,#34072,#34073,#34074,#34075,#34076,#34077,#34078,
#34079,#34080,#34081,#34082,#34083,#34084,#34085,#34086,#34087,#34088,#34089,
#34090,#34091,#34092,#34093,#34094,#34095,#34096,#34097,#34098,#34099,#34100,
#34101,#34102,#34103,#34104,#34105,#34106,#34107,#34108,#34109,#34110,#34111,
#34112,#34113,#34114,#34115,#34116,#34117,#34118,#34119,#34120,#34121,#34122,
#34123,#34124,#34125,#34126,#34127,#34128,#34129,#34130,#34131,#34132,#34133,
#34134,#34135,#34136,#34137,#34138,#34139,#34140,#34141,#34142,#34143,#34144,
#34145,#34146,#34147,#34148,#34149,#34150,#34151,#34152,#34153,#34154,#34155,
#34156,#34157,#34158,#34159,#34160,#34161,#34162,#34163,#34164,#34165),
 .UNSPECIFIED.,.F.,.F.,(4,3,3,3,3,3,3,3,3,3,3,3,3,3,3,3,3,3,3,3,3,3,3,3,
3,3,3,3,3,3,3,3,3,3,3,3,3,3,3,3,3,3,3,3,3,4),(279.409915502333,279.613260937759,
279.661873055044,279.819298913484,279.976435170093,280.133402664831,280.290450773984,
280.447546868181,280.60498252915,280.660665458812,280.818091317252,280.975227573863,
281.132195068602,281.289243177756,281.446339271953,281.603774932923,281.65945786258,
281.816883721021,281.974019977631,282.13098747237,282.288035581524,282.445131675721,
282.602567336692,282.658250266348,282.815676124788,282.972812381398,283.129779876137,
283.286827985291,283.443924079488,283.601359740458,283.657042670116,283.814468528556,
283.971604785167,284.128572279906,284.285620389059,284.442716483257,284.600152144227,
284.655835073884,284.813260932324,284.970397188935,285.127364683674,285.284412792827,
285.441508887025,285.598944547995,285.654627477652,285.693100691936),
 .UNSPECIFIED.);
#781=B_SPLINE_CURVE_WITH_KNOTS('',3,(#34167,#34168,#34169,#34170,#34171,
#34172,#34173,#34174,#34175,#34176),.UNSPECIFIED.,.F.,.F.,(4,1,1,1,1,1,
1,4),(285.69310580607,286.65341988142,287.652212285188,288.651004688956,
289.649797092724,290.648589496492,291.64738190026,291.976278941454),
 .UNSPECIFIED.);
#782=B_SPLINE_CURVE_WITH_KNOTS('',3,(#34178,#34179,#34180,#34181,#34182,
#34183,#34184,#34185,#34186,#34187,#34188,#34189,#34190,#34191,#34192,#34193,
#34194,#34195,#34196,#34197,#34198,#34199,#34200,#34201,#34202,#34203,#34204,
#34205,#34206,#34207,#34208,#34209,#34210,#34211,#34212,#34213,#34214,#34215,
#34216,#34217,#34218,#34219,#34220,#34221,#34222,#34223,#34224,#34225,#34226,
#34227,#34228,#34229,#34230,#34231,#34232,#34233,#34234,#34235,#34236,#34237,
#34238,#34239,#34240,#34241,#34242,#34243,#34244,#34245,#34246,#34247,#34248,
#34249,#34250,#34251,#34252,#34253,#34254,#34255,#34256,#34257,#34258,#34259,
#34260,#34261,#34262,#34263,#34264,#34265,#34266,#34267,#34268,#34269,#34270,
#34271,#34272,#34273,#34274,#34275,#34276,#34277,#34278,#34279,#34280,#34281,
#34282,#34283,#34284,#34285,#34286,#34287,#34288,#34289,#34290,#34291,#34292,
#34293,#34294,#34295,#34296,#34297,#34298,#34299,#34300,#34301,#34302,#34303,
#34304,#34305,#34306,#34307,#34308,#34309,#34310),.UNSPECIFIED.,.F.,.F.,
(4,3,3,3,3,3,3,3,3,3,3,3,3,3,3,3,3,3,3,3,3,3,3,3,3,3,3,3,3,3,3,3,3,3,3,
3,3,3,3,3,3,3,3,3,4),(291.976285999115,292.133008839732,292.289839990702,
292.446739507181,292.603991533183,292.646174304028,292.803600162468,292.960736419079,
293.117703913818,293.274752022971,293.431848117168,293.589283778138,293.644966707796,
293.802392566236,293.959528822847,294.116496317586,294.273544426739,294.430640520936,
294.588076181906,294.643759111564,294.801184970004,294.958321226615,295.115288721354,
295.272336830507,295.429432924705,295.586868585675,295.642551515332,295.799977373772,
295.957113630383,296.114081125122,296.271129234275,296.428225328473,296.585660989443,
296.6413439191,296.79876977754,296.95590603415,297.112873528889,297.269921638043,
297.42701773224,297.58445339321,297.640136322868,297.799036718426,297.957616676704,
298.116041131907,298.259471306295),.UNSPECIFIED.);
#783=B_SPLINE_CURVE_WITH_KNOTS('',3,(#34312,#34313,#34314,#34315,#34316,
#34317,#34318,#34319,#34320,#34321),.UNSPECIFIED.,.F.,.F.,(4,1,1,1,1,1,
1,4),(298.259478779105,298.638928726636,299.637721130404,300.636513534172,
301.63530593794,302.634098341708,303.632890745476,304.542647862618),
 .UNSPECIFIED.);
#784=B_SPLINE_CURVE_WITH_KNOTS('',3,(#34323,#34324,#34325,#34326,#34327,
#34328,#34329,#34330,#34331,#34332,#34333,#34334,#34335,#34336,#34337,#34338,
#34339,#34340,#34341,#34342,#34343,#34344,#34345,#34346,#34347,#34348,#34349,
#34350,#34351,#34352,#34353,#34354,#34355,#34356,#34357,#34358,#34359,#34360,
#34361,#34362,#34363,#34364,#34365,#34366,#34367,#34368,#34369,#34370,#34371,
#34372,#34373,#34374,#34375,#34376,#34377,#34378,#34379,#34380,#34381,#34382,
#34383,#34384,#34385,#34386,#34387,#34388,#34389,#34390,#34391,#34392,#34393,
#34394,#34395,#34396,#34397,#34398,#34399,#34400,#34401,#34402,#34403,#34404,
#34405,#34406,#34407,#34408,#34409,#34410,#34411,#34412,#34413,#34414,#34415,
#34416,#34417,#34418,#34419,#34420,#34421,#34422,#34423,#34424,#34425,#34426,
#34427,#34428,#34429,#34430,#34431,#34432,#34433,#34434,#34435,#34436,#34437,
#34438,#34439,#34440,#34441,#34442,#34443,#34444,#34445,#34446,#34447,#34448,
#34449,#34450,#34451,#34452,#34453,#34454,#34455),.UNSPECIFIED.,.F.,.F.,
(4,3,3,3,3,3,3,3,3,3,3,3,3,3,3,3,3,3,3,3,3,3,3,3,3,3,3,3,3,3,3,3,3,3,3,
3,3,3,3,3,3,3,3,3,4),(304.542656613474,304.631683149244,304.789109007684,
304.946245264295,305.103212759034,305.260260868187,305.417356962385,305.574792623355,
305.630475553012,305.787901411452,305.945037668063,306.102005162802,306.259053271955,
306.416149366152,306.573585027122,306.62926795678,306.78669381522,306.943830071831,
307.10079756657,307.257845675723,307.414941769921,307.572377430891,307.628060360548,
307.785486218988,307.942622475599,308.099589970338,308.256638079491,308.413734173689,
308.571169834659,308.626852764316,308.784278622756,308.941414879367,309.098382374106,
309.255430483259,309.412526577457,309.569962238427,309.625645168084,309.783071026524,
309.940207283134,310.097174777873,310.254222887027,310.411318981224,310.568754642194,
310.624437571852,310.825841920654),.UNSPECIFIED.);
#785=B_SPLINE_CURVE_WITH_KNOTS('',3,(#34457,#34458,#34459,#34460,#34461,
#34462,#34463,#34464,#34465,#34466,#34467,#34468,#34469,#34470,#34471,#34472,
#34473,#34474,#34475,#34476,#34477,#34478,#34479,#34480,#34481,#34482,#34483,
#34484,#34485,#34486,#34487,#34488,#34489,#34490,#34491,#34492,#34493,#34494,
#34495,#34496,#34497,#34498,#34499,#34500,#34501,#34502,#34503,#34504,#34505,
#34506,#34507,#34508,#34509,#34510,#34511,#34512,#34513,#34514,#34515,#34516,
#34517,#34518,#34519,#34520,#34521,#34522,#34523,#34524,#34525,#34526,#34527,
#34528,#34529,#34530,#34531,#34532,#34533,#34534,#34535,#34536,#34537,#34538,
#34539,#34540,#34541,#34542,#34543,#34544,#34545,#34546,#34547,#34548,#34549,
#34550,#34551,#34552,#34553,#34554,#34555,#34556,#34557,#34558,#34559,#34560,
#34561,#34562,#34563,#34564,#34565,#34566,#34567,#34568,#34569,#34570,#34571,
#34572,#34573,#34574,#34575,#34576,#34577,#34578,#34579,#34580,#34581,#34582,
#34583,#34584,#34585,#34586,#34587,#34588,#34589),.UNSPECIFIED.,.F.,.F.,
(4,3,3,3,3,3,3,3,3,3,3,3,3,3,3,3,3,3,3,3,3,3,3,3,3,3,3,3,3,3,3,3,3,3,3,
3,3,3,3,3,3,3,3,3,4),(310.825841920814,310.98075688353,311.141375156553,
311.296181572029,311.451044128878,311.606222849238,311.62322997562,311.78065583406,
311.937792090671,312.09475958541,312.251807694563,312.408903788761,312.566339449731,
312.622022379388,312.779448237828,312.936584494439,313.093551989178,313.250600098331,
313.407696192529,313.565131853499,313.620814783156,313.778240641596,313.935376898207,
314.092344392946,314.249392502099,314.406488596297,314.563924257267,314.619607186924,
314.777033045364,314.934169301975,315.091136796714,315.248184905867,315.405281000065,
315.562716661035,315.618399590692,315.775825449132,315.932961705742,316.089929200481,
316.246977309634,316.404073403831,316.561509064801,316.61719199446,316.78318166121,
316.948512755425,317.109027227671),.UNSPECIFIED.);
#786=B_SPLINE_CURVE_WITH_KNOTS('',3,(#34591,#34592,#34593,#34594,#34595,
#34596,#34597,#34598,#34599,#34600,#34601,#34602,#34603,#34604,#34605,#34606,
#34607,#34608,#34609,#34610,#34611,#34612,#34613,#34614,#34615,#34616,#34617,
#34618,#34619,#34620,#34621,#34622,#34623,#34624,#34625,#34626,#34627,#34628,
#34629,#34630,#34631,#34632,#34633,#34634,#34635,#34636,#34637,#34638,#34639,
#34640,#34641,#34642,#34643,#34644,#34645,#34646,#34647,#34648,#34649,#34650,
#34651,#34652,#34653,#34654,#34655,#34656,#34657,#34658,#34659,#34660,#34661,
#34662,#34663,#34664,#34665,#34666,#34667,#34668,#34669,#34670,#34671,#34672,
#34673,#34674,#34675,#34676,#34677,#34678,#34679,#34680,#34681,#34682,#34683,
#34684,#34685,#34686,#34687,#34688,#34689,#34690,#34691,#34692,#34693,#34694,
#34695,#34696,#34697,#34698,#34699,#34700,#34701,#34702,#34703,#34704,#34705,
#34706,#34707,#34708,#34709,#34710,#34711,#34712,#34713,#34714,#34715,#34716,
#34717,#34718,#34719,#34720),.UNSPECIFIED.,.F.,.F.,(4,3,3,3,3,3,3,3,3,3,
3,3,3,3,3,3,3,3,3,3,3,3,3,3,3,3,3,3,3,3,3,3,3,3,3,3,3,3,3,3,3,3,3,4),(317.109027227834,
317.273126322695,317.444555360461,317.615984398228,317.773410256669,317.93054651328,
318.087514008019,318.244562117173,318.401658211371,318.559093872342,318.614776801996,
318.772202660437,318.929338917047,319.086306411786,319.243354520939,319.400450615137,
319.557886276107,319.613569205764,319.770995064204,319.928131320814,320.085098815553,
320.242146924706,320.399243018903,320.556678679873,320.612361609532,320.769787467973,
320.926923724584,321.083891219324,321.240939328478,321.398035422676,321.555471083646,
321.611154013301,321.768579871741,321.925716128351,322.08268362309,322.239731732243,
322.39682782644,322.554263487409,322.609946417068,322.76521431044,322.921963866583,
323.076831294499,323.234521914756,323.392212535013),.UNSPECIFIED.);
#787=B_SPLINE_CURVE_WITH_KNOTS('',3,(#34722,#34723,#34724,#34725,#34726,
#34727,#34728,#34729,#34730,#34731,#34732),.UNSPECIFIED.,.F.,.F.,(4,1,1,
1,1,1,1,1,4),(323.392212535013,323.608738820837,324.607531224605,325.606323628372,
326.605116032141,327.603908435909,328.602700839677,329.601493243445,329.675397842193),
 .UNSPECIFIED.);
#788=B_SPLINE_CURVE_WITH_KNOTS('',3,(#34734,#34735,#34736,#34737,#34738,
#34739,#34740,#34741,#34742,#34743,#34744,#34745,#34746,#34747,#34748,#34749,
#34750,#34751,#34752,#34753,#34754,#34755,#34756,#34757,#34758,#34759,#34760,
#34761,#34762,#34763,#34764,#34765,#34766,#34767,#34768,#34769,#34770,#34771,
#34772,#34773,#34774,#34775,#34776,#34777,#34778,#34779,#34780,#34781,#34782,
#34783,#34784,#34785,#34786,#34787,#34788,#34789,#34790,#34791,#34792,#34793,
#34794,#34795,#34796,#34797,#34798,#34799,#34800,#34801,#34802,#34803,#34804,
#34805,#34806,#34807,#34808,#34809,#34810,#34811,#34812,#34813,#34814,#34815,
#34816,#34817,#34818,#34819,#34820,#34821,#34822,#34823,#34824,#34825,#34826,
#34827,#34828,#34829,#34830,#34831,#34832,#34833,#34834,#34835,#34836,#34837,
#34838,#34839,#34840,#34841,#34842,#34843,#34844,#34845,#34846,#34847,#34848,
#34849,#34850,#34851,#34852,#34853,#34854,#34855,#34856,#34857,#34858,#34859,
#34860,#34861,#34862,#34863),.UNSPECIFIED.,.F.,.F.,(4,3,3,3,3,3,3,3,3,3,
3,3,3,3,3,3,3,3,3,3,3,3,3,3,3,3,3,3,3,3,3,3,3,3,3,3,3,3,3,3,3,3,3,4),(329.675397842193,
329.831155571038,329.986644937876,330.142123120359,330.297569297493,330.453373608074,
330.600285647213,330.757711505653,330.914847762264,331.071815257003,331.228863366156,
331.385959460353,331.543395121324,331.599078050981,331.756503909421,331.913640166032,
332.070607660771,332.227655769924,332.384751864121,332.542187525091,332.597870454749,
332.755296313189,332.9124325698,333.069400064539,333.226448173692,333.38354426789,
333.54097992886,333.596662858517,333.754088716957,333.911224973568,334.068192468307,
334.22524057746,334.382336671657,334.539772332627,334.595455262285,334.752881120726,
334.910017377336,335.066984872075,335.224032981229,335.381129075426,335.538564736397,
335.594247666053,335.776415407595,335.958583149137),.UNSPECIFIED.);
#789=B_SPLINE_CURVE_WITH_KNOTS('',3,(#34865,#34866,#34867,#34868,#34869,
#34870,#34871,#34872,#34873,#34874,#34875,#34876,#34877,#34878,#34879,#34880,
#34881,#34882,#34883,#34884,#34885,#34886,#34887,#34888,#34889,#34890,#34891,
#34892,#34893,#34894,#34895,#34896,#34897,#34898,#34899,#34900,#34901,#34902,
#34903,#34904,#34905,#34906,#34907,#34908,#34909,#34910,#34911,#34912,#34913,
#34914,#34915,#34916,#34917,#34918,#34919,#34920,#34921,#34922,#34923,#34924,
#34925,#34926,#34927,#34928,#34929,#34930,#34931,#34932,#34933,#34934,#34935,
#34936,#34937,#34938,#34939,#34940,#34941,#34942,#34943,#34944,#34945,#34946,
#34947,#34948,#34949,#34950,#34951,#34952,#34953,#34954,#34955,#34956,#34957,
#34958,#34959,#34960,#34961,#34962,#34963,#34964,#34965,#34966,#34967,#34968,
#34969,#34970,#34971,#34972,#34973,#34974,#34975,#34976,#34977,#34978,#34979,
#34980,#34981,#34982,#34983,#34984,#34985,#34986,#34987,#34988,#34989,#34990,
#34991,#34992,#34993,#34994,#34995,#34996,#34997),.UNSPECIFIED.,.F.,.F.,
(4,3,3,3,3,3,3,3,3,3,3,3,3,3,3,3,3,3,3,3,3,3,3,3,3,3,3,3,3,3,3,3,3,3,3,
3,3,3,3,3,3,3,3,3,4),(335.958583149372,336.117197379484,336.275121374349,
336.434080722085,336.593040069821,336.750465928261,336.907602184871,337.06456967961,
337.221617788763,337.37871388296,337.53614954393,337.591832473589,337.749258332029,
337.90639458864,338.063362083379,338.220410192532,338.377506286729,338.534941947699,
338.590624877357,338.748050735798,338.905186992408,339.062154487147,339.219202596301,
339.376298690498,339.533734351468,339.589417281125,339.746843139565,339.903979396176,
340.060946890915,340.217995000068,340.375091094266,340.532526755236,340.588209684893,
340.745635543333,340.902771799944,341.059739294683,341.216787403836,341.373883498034,
341.531319159004,341.587002088661,341.750693680634,341.908058796137,342.065232937769,
342.222371717184,342.241768456552),.UNSPECIFIED.);
#790=B_SPLINE_CURVE_WITH_KNOTS('',3,(#34999,#35000,#35001,#35002,#35003,
#35004,#35005,#35006,#35007,#35008,#35009,#35010,#35011,#35012,#35013,#35014,
#35015,#35016,#35017,#35018,#35019,#35020,#35021,#35022,#35023,#35024,#35025,
#35026,#35027,#35028,#35029,#35030,#35031,#35032,#35033,#35034,#35035,#35036,
#35037,#35038,#35039,#35040,#35041,#35042,#35043,#35044,#35045,#35046,#35047,
#35048,#35049,#35050,#35051,#35052,#35053,#35054,#35055,#35056,#35057,#35058,
#35059,#35060,#35061,#35062,#35063,#35064,#35065,#35066,#35067,#35068,#35069,
#35070,#35071,#35072,#35073,#35074,#35075,#35076,#35077,#35078,#35079,#35080,
#35081,#35082,#35083,#35084,#35085,#35086,#35087,#35088,#35089,#35090,#35091,
#35092,#35093,#35094,#35095,#35096,#35097,#35098,#35099,#35100,#35101,#35102,
#35103,#35104,#35105,#35106,#35107,#35108,#35109,#35110,#35111,#35112,#35113,
#35114,#35115,#35116,#35117,#35118,#35119,#35120,#35121,#35122,#35123,#35124,
#35125,#35126,#35127,#35128),.UNSPECIFIED.,.F.,.F.,(4,3,3,3,3,3,3,3,3,3,
3,3,3,3,3,3,3,3,3,3,3,3,3,3,3,3,3,3,3,3,3,3,3,3,3,3,3,3,3,3,3,3,3,4),(342.241768456779,
342.423867884614,342.585794492429,342.743220350869,342.900356607479,343.057324102218,
343.214372211372,343.371468305569,343.528903966539,343.584586896197,343.742012754637,
343.899149011248,344.056116505987,344.21316461514,344.370260709338,344.527696370308,
344.583379299965,344.740805158405,344.897941415016,345.054908909755,345.211957018908,
345.369053113106,345.526488774076,345.582171703733,345.739597562173,345.896733818784,
346.053701313523,346.210749422676,346.367845516874,346.525281177844,346.580964107501,
346.738389965942,346.895526222552,347.052493717291,347.209541826445,347.366637920642,
347.524073581612,347.579756511269,347.735910813974,347.891777852744,348.050071830491,
348.205854264497,348.365404014114,348.524953763731),.UNSPECIFIED.);
#791=B_SPLINE_CURVE_WITH_KNOTS('',3,(#35130,#35131,#35132,#35133,#35134,
#35135,#35136,#35137,#35138,#35139,#35140,#35141),.UNSPECIFIED.,.F.,.F.,
(4,2,1,1,1,1,1,1,4),(348.524953763731,348.578548915037,349.577341318805,
350.576133722573,351.574926126341,352.573718530109,353.572510933877,354.571303337645,
354.808138699911),.UNSPECIFIED.);
#792=B_SPLINE_CURVE_WITH_KNOTS('',3,(#35143,#35144,#35145,#35146,#35147,
#35148,#35149,#35150,#35151,#35152,#35153,#35154,#35155,#35156,#35157,#35158,
#35159,#35160,#35161,#35162,#35163,#35164,#35165,#35166,#35167,#35168,#35169,
#35170,#35171,#35172,#35173,#35174,#35175,#35176,#35177,#35178,#35179,#35180,
#35181,#35182,#35183,#35184,#35185,#35186,#35187,#35188,#35189,#35190,#35191,
#35192,#35193,#35194,#35195,#35196,#35197,#35198,#35199,#35200,#35201,#35202,
#35203,#35204,#35205,#35206,#35207,#35208,#35209,#35210,#35211,#35212,#35213,
#35214,#35215,#35216,#35217,#35218,#35219,#35220,#35221,#35222,#35223,#35224,
#35225,#35226,#35227,#35228,#35229,#35230,#35231,#35232,#35233,#35234,#35235,
#35236,#35237,#35238,#35239,#35240,#35241,#35242,#35243,#35244,#35245,#35246,
#35247,#35248,#35249,#35250,#35251,#35252,#35253,#35254,#35255,#35256,#35257,
#35258,#35259,#35260,#35261,#35262,#35263,#35264,#35265,#35266,#35267,#35268,
#35269,#35270,#35271,#35272,#35273,#35274,#35275),.UNSPECIFIED.,.F.,.F.,
(4,3,3,3,3,3,3,3,3,3,3,3,3,3,3,3,3,3,3,3,3,3,3,3,3,3,3,3,3,3,3,3,3,3,3,
3,3,3,3,3,3,3,3,3,4),(354.808139070911,354.963278088943,355.118405533254,
355.273502210574,355.428953389041,355.570095741413,355.727521599853,355.884657856464,
356.041625351203,356.198673460356,356.355769554553,356.513205215523,356.568888145181,
356.726314003621,356.883450260232,357.040417754971,357.197465864124,357.354561958322,
357.511997619292,357.567680548949,357.725106407389,357.882242664,358.039210158739,
358.196258267892,358.35335436209,358.51079002306,358.566472952717,358.723898811157,
358.881035067768,359.038002562507,359.19505067166,359.352146765858,359.509582426828,
359.565265356485,359.722691214925,359.879827471535,360.036794966274,360.193843075428,
360.350939169625,360.508374830595,360.564057760253,360.727583305717,360.890693796198,
361.053396591264,361.091324378091),.UNSPECIFIED.);
#793=B_SPLINE_CURVE_WITH_KNOTS('',3,(#35277,#35278,#35279,#35280,#35281,
#35282,#35283,#35284,#35285,#35286),.UNSPECIFIED.,.F.,.F.,(4,1,1,1,1,1,
1,4),(361.091326518203,361.562850164021,362.561642567789,363.560434971557,
364.559227375325,365.558019779093,366.556812182861,367.37450968527),
 .UNSPECIFIED.);
#794=B_SPLINE_CURVE_WITH_KNOTS('',3,(#35288,#35289,#35290,#35291,#35292,
#35293,#35294,#35295,#35296,#35297,#35298),.UNSPECIFIED.,.F.,.F.,(4,1,1,
1,1,1,1,1,4),(367.37450968527,367.555604586629,368.554396990397,369.553189394165,
370.551981797933,371.550774201701,372.549566605469,373.548359009237,373.65769499245),
 .UNSPECIFIED.);
#795=B_SPLINE_CURVE_WITH_KNOTS('',3,(#35300,#35301,#35302,#35303,#35304,
#35305,#35306,#35307,#35308,#35309,#35310,#35311,#35312,#35313,#35314,#35315,
#35316,#35317,#35318,#35319,#35320,#35321,#35322,#35323,#35324,#35325,#35326,
#35327,#35328,#35329,#35330,#35331,#35332,#35333,#35334,#35335,#35336,#35337,
#35338,#35339,#35340,#35341,#35342,#35343,#35344,#35345,#35346,#35347,#35348,
#35349,#35350,#35351,#35352,#35353,#35354,#35355,#35356,#35357,#35358,#35359,
#35360,#35361,#35362,#35363,#35364,#35365,#35366,#35367,#35368,#35369,#35370,
#35371,#35372,#35373,#35374,#35375,#35376,#35377,#35378,#35379,#35380,#35381,
#35382,#35383,#35384,#35385,#35386,#35387,#35388,#35389,#35390,#35391,#35392,
#35393,#35394,#35395,#35396,#35397,#35398,#35399,#35400,#35401,#35402,#35403,
#35404,#35405,#35406,#35407,#35408,#35409,#35410,#35411,#35412,#35413,#35414,
#35415,#35416,#35417,#35418,#35419,#35420,#35421,#35422,#35423,#35424,#35425,
#35426,#35427,#35428,#35429,#35430,#35431,#35432),.UNSPECIFIED.,.F.,.F.,
(4,3,3,3,3,3,3,3,3,3,3,3,3,3,3,3,3,3,3,3,3,3,3,3,3,3,3,3,3,3,3,3,3,3,3,
3,3,3,3,3,3,3,3,3,4),(373.65769499245,373.812962610095,373.967981418969,
374.123006149566,374.278018188158,374.43337343482,374.547151413005,374.704577271445,
374.861713528056,375.018681022795,375.175729131948,375.332825226146,375.490260887116,
375.545943816773,375.703369675213,375.860505931824,376.017473426563,376.174521535716,
376.331617629914,376.489053290884,376.544736220541,376.702162078981,376.859298335592,
377.016265830331,377.173313939484,377.330410033682,377.487845694652,377.543528624309,
377.700954482749,377.85809073936,378.015058234099,378.172106343252,378.32920243745,
378.48663809842,378.542321028077,378.699746886517,378.856883143128,379.013850637867,
379.17089874702,379.327994841218,379.485430502188,379.541113431845,379.716064966872,
379.889720377981,379.94088007731),.UNSPECIFIED.);
#796=B_SPLINE_CURVE_WITH_KNOTS('',3,(#35434,#35435,#35436,#35437,#35438,
#35439,#35440,#35441,#35442,#35443),.UNSPECIFIED.,.F.,.F.,(4,1,1,1,1,1,
1,4),(379.940880299629,380.539905835613,381.538698239381,382.537490643149,
383.536283046917,384.535075450685,385.533867854453,386.224065606809),
 .UNSPECIFIED.);
#797=B_SPLINE_CURVE_WITH_KNOTS('',3,(#35445,#35446,#35447,#35448,#35449,
#35450,#35451,#35452,#35453,#35454,#35455,#35456,#35457,#35458,#35459,#35460,
#35461,#35462,#35463,#35464,#35465,#35466,#35467,#35468,#35469,#35470,#35471,
#35472,#35473,#35474,#35475,#35476,#35477,#35478,#35479,#35480,#35481,#35482,
#35483,#35484,#35485,#35486,#35487,#35488,#35489,#35490,#35491,#35492,#35493,
#35494,#35495,#35496,#35497,#35498,#35499,#35500,#35501,#35502,#35503,#35504,
#35505,#35506,#35507,#35508,#35509,#35510,#35511,#35512,#35513,#35514,#35515,
#35516,#35517,#35518,#35519,#35520,#35521,#35522,#35523,#35524,#35525,#35526,
#35527,#35528,#35529,#35530,#35531,#35532,#35533,#35534,#35535,#35536,#35537,
#35538,#35539,#35540,#35541,#35542,#35543,#35544,#35545,#35546,#35547,#35548,
#35549,#35550,#35551,#35552,#35553,#35554,#35555,#35556,#35557,#35558,#35559,
#35560,#35561,#35562,#35563,#35564,#35565,#35566,#35567,#35568,#35569,#35570,
#35571,#35572,#35573,#35574,#35575,#35576,#35577),.UNSPECIFIED.,.F.,.F.,
(4,3,3,3,3,3,3,3,3,3,3,3,3,3,3,3,3,3,3,3,3,3,3,3,3,3,3,3,3,3,3,3,3,3,3,
3,3,3,3,3,3,3,3,3,4),(386.224065804283,386.412697267132,386.532660258221,
386.690086116662,386.847222373273,387.004189868013,387.161237977167,387.318334071365,
387.475769732336,387.531452661989,387.688878520429,387.84601477704,388.002982271779,
388.160030380932,388.317126475129,388.4745621361,388.530245065757,388.687670924197,
388.844807180807,389.001774675546,389.1588227847,389.315918878897,389.473354539867,
389.529037469525,389.686463327965,389.843599584576,390.000567079315,390.157615188469,
390.314711282666,390.472146943636,390.527829873293,390.685255731733,390.842391988344,
390.999359483083,391.156407592236,391.313503686434,391.470939347404,391.526622277061,
391.683559019512,391.840207071128,391.996688881692,392.15325191782,392.30986826289,
392.466816005711,392.507250913988),.UNSPECIFIED.);
#798=B_SPLINE_CURVE_WITH_KNOTS('',3,(#35579,#35580,#35581,#35582,#35583,
#35584,#35585,#35586,#35587,#35588,#35589,#35590),.UNSPECIFIED.,.F.,.F.,
(4,2,1,1,1,1,1,1,4),(392.507250913988,392.525414680829,393.524207084597,
394.522999488365,395.521791892133,396.520584295901,397.51937669967,398.518169103438,
398.790432579651),.UNSPECIFIED.);
#799=B_SPLINE_CURVE_WITH_KNOTS('',3,(#35592,#35593,#35594,#35595,#35596,
#35597,#35598,#35599,#35600,#35601,#35602,#35603,#35604,#35605,#35606,#35607,
#35608,#35609,#35610,#35611,#35612,#35613,#35614,#35615,#35616,#35617,#35618,
#35619,#35620,#35621,#35622,#35623,#35624,#35625,#35626,#35627,#35628,#35629,
#35630,#35631,#35632,#35633,#35634,#35635,#35636,#35637,#35638,#35639,#35640,
#35641,#35642,#35643,#35644,#35645,#35646,#35647,#35648,#35649,#35650,#35651,
#35652,#35653,#35654,#35655,#35656,#35657,#35658,#35659,#35660,#35661,#35662,
#35663,#35664,#35665,#35666,#35667,#35668,#35669,#35670,#35671,#35672,#35673,
#35674,#35675,#35676,#35677,#35678,#35679,#35680,#35681,#35682,#35683,#35684,
#35685,#35686,#35687,#35688,#35689,#35690,#35691,#35692,#35693,#35694,#35695,
#35696,#35697,#35698,#35699,#35700,#35701,#35702,#35703,#35704,#35705,#35706,
#35707,#35708,#35709,#35710,#35711,#35712,#35713,#35714,#35715,#35716,#35717,
#35718,#35719,#35720,#35721,#35722,#35723,#35724),.UNSPECIFIED.,.F.,.F.,
(4,3,3,3,3,3,3,3,3,3,3,3,3,3,3,3,3,3,3,3,3,3,3,3,3,3,3,3,3,3,3,3,3,3,3,
3,3,3,3,3,3,3,3,3,4),(398.790436221168,398.946007945138,399.101608749528,
399.257213317091,399.413167483264,399.516961507206,399.674387365646,399.831523622256,
399.988491116995,400.145539226149,400.302635320346,400.460070981316,400.515753910974,
400.673179769414,400.830316026025,400.987283520764,401.144331629917,401.301427724115,
401.458863385085,401.514546314742,401.671972173182,401.829108429793,401.986075924532,
402.143124033685,402.300220127883,402.457655788853,402.51333871851,402.67076457695,
402.827900833561,402.9848683283,403.141916437453,403.299012531651,403.456448192621,
403.512131122278,403.669556980718,403.826693237329,403.983660732068,404.140708841221,
404.297804935419,404.455240596389,404.510923526046,404.672394501581,404.833497892842,
404.994300774243,405.073621528348),.UNSPECIFIED.);
#800=B_SPLINE_CURVE_WITH_KNOTS('',3,(#35726,#35727,#35728,#35729,#35730,
#35731,#35732,#35733,#35734,#35735),.UNSPECIFIED.,.F.,.F.,(4,1,1,1,1,1,
1,4),(405.073626388949,405.509715929814,406.508508333582,407.50730073735,
408.506093141118,409.504885544886,410.503677948654,411.356799146851),
 .UNSPECIFIED.);
#801=B_SPLINE_CURVE_WITH_KNOTS('',3,(#35737,#35738,#35739,#35740,#35741,
#35742,#35743,#35744,#35745,#35746,#35747,#35748,#35749,#35750,#35751,#35752,
#35753,#35754,#35755,#35756,#35757,#35758,#35759,#35760,#35761,#35762,#35763,
#35764,#35765,#35766,#35767,#35768,#35769,#35770,#35771,#35772,#35773,#35774,
#35775,#35776,#35777,#35778,#35779,#35780,#35781,#35782,#35783,#35784,#35785,
#35786,#35787,#35788,#35789,#35790,#35791,#35792,#35793,#35794,#35795,#35796,
#35797,#35798,#35799,#35800,#35801,#35802,#35803,#35804,#35805,#35806,#35807,
#35808,#35809,#35810,#35811,#35812,#35813,#35814,#35815,#35816,#35817,#35818,
#35819,#35820,#35821,#35822,#35823,#35824,#35825,#35826,#35827,#35828,#35829,
#35830,#35831,#35832,#35833,#35834,#35835,#35836,#35837,#35838,#35839,#35840,
#35841,#35842,#35843,#35844,#35845,#35846,#35847,#35848,#35849,#35850,#35851,
#35852,#35853,#35854,#35855,#35856,#35857,#35858,#35859,#35860,#35861,#35862,
#35863,#35864,#35865,#35866,#35867,#35868,#35869),.UNSPECIFIED.,.F.,.F.,
(4,3,3,3,3,3,3,3,3,3,3,3,3,3,3,3,3,3,3,3,3,3,3,3,3,3,3,3,3,3,3,3,3,3,3,
3,3,3,3,3,3,3,3,3,4),(411.356806835527,411.502470352422,411.659896210861,
411.81703246747,411.973999962208,412.13104807136,412.288144165556,412.445579826525,
412.50126275619,412.658688614631,412.815824871241,412.97279236598,413.129840475134,
413.286936569332,413.444372230302,413.500055159958,413.657481018399,413.814617275009,
413.971584769748,414.128632878902,414.285728973099,414.443164634069,414.498847563726,
414.656273422166,414.813409678776,414.970377173515,415.127425282669,415.284521376866,
415.441957037836,415.497639967494,415.655065825935,415.812202082545,415.969169577284,
416.126217686438,416.283313780635,416.440749441605,416.496432371262,416.653858229702,
416.810994486313,416.967961981052,417.125010090205,417.282106184402,417.439541845373,
417.49522477503,417.639992142707),.UNSPECIFIED.);
#802=B_SPLINE_CURVE_WITH_KNOTS('',3,(#35871,#35872,#35873,#35874,#35875,
#35876,#35877,#35878,#35879,#35880),.UNSPECIFIED.,.F.,.F.,(4,1,1,1,1,1,
1,4),(417.63999988239,418.494017178798,419.492809582566,420.491601986334,
421.490394390102,422.48918679387,423.487979197638,423.923172532797),
 .UNSPECIFIED.);
#803=B_SPLINE_CURVE_WITH_KNOTS('',3,(#35882,#35883,#35884,#35885,#35886,
#35887,#35888,#35889,#35890,#35891,#35892,#35893,#35894,#35895,#35896,#35897,
#35898,#35899,#35900,#35901,#35902,#35903,#35904,#35905,#35906,#35907,#35908,
#35909,#35910,#35911,#35912,#35913,#35914,#35915,#35916,#35917,#35918,#35919,
#35920,#35921,#35922,#35923,#35924,#35925,#35926,#35927,#35928,#35929,#35930,
#35931,#35932,#35933,#35934,#35935,#35936,#35937,#35938,#35939,#35940,#35941,
#35942,#35943,#35944,#35945,#35946,#35947,#35948,#35949,#35950,#35951,#35952,
#35953,#35954,#35955,#35956,#35957,#35958,#35959,#35960,#35961,#35962,#35963,
#35964,#35965,#35966,#35967,#35968,#35969,#35970,#35971,#35972,#35973,#35974,
#35975,#35976,#35977,#35978,#35979,#35980,#35981,#35982,#35983,#35984,#35985,
#35986,#35987,#35988,#35989,#35990,#35991,#35992,#35993,#35994,#35995,#35996,
#35997,#35998,#35999,#36000,#36001,#36002,#36003,#36004,#36005,#36006,#36007,
#36008,#36009,#36010,#36011,#36012,#36013,#36014),.UNSPECIFIED.,.F.,.F.,
(4,3,3,3,3,3,3,3,3,3,3,3,3,3,3,3,3,3,3,3,3,3,3,3,3,3,3,3,3,3,3,3,3,3,3,
3,3,3,3,3,3,3,3,3,4),(423.923177449886,424.08400036725,424.244972248657,
424.406418676567,424.486771601406,424.644197459863,424.80133371649,424.958301211245,
425.115349320415,425.272445414628,425.429881075614,425.485564005174,425.642989863596,
425.800126120187,425.957093614907,426.114141724043,426.271237818222,426.428673479175,
426.484356408942,426.64178226736,426.798918523948,426.955886018664,427.112934127794,
427.270030221968,427.427465882915,427.48314881271,427.640574671267,427.797710927994,
427.95467842285,428.111726532119,428.268822626431,428.426258287513,428.481941216478,
428.639367074758,428.796503331209,428.95347082579,429.110518934789,429.267615028834,
429.425050689657,429.480733620246,429.636725845168,429.792437589937,429.947979823974,
430.103600649651,430.206362757066),.UNSPECIFIED.);
#804=B_SPLINE_CURVE_WITH_KNOTS('',3,(#36016,#36017,#36018,#36019,#36020,
#36021,#36022,#36023,#36024,#36025,#36026),.UNSPECIFIED.,.F.,.F.,(4,1,1,
1,1,1,1,1,4),(430.206366472598,430.479526024014,431.478318427782,432.47711083155,
433.475903235318,434.474695639086,435.473488042854,436.472280446622,436.489548064245),
 .UNSPECIFIED.);
#805=B_SPLINE_CURVE_WITH_KNOTS('',3,(#36028,#36029,#36030,#36031,#36032,
#36033,#36034,#36035,#36036,#36037,#36038,#36039,#36040,#36041,#36042,#36043,
#36044,#36045,#36046,#36047,#36048,#36049,#36050,#36051,#36052,#36053,#36054,
#36055,#36056,#36057,#36058,#36059,#36060,#36061,#36062,#36063,#36064,#36065,
#36066,#36067,#36068,#36069,#36070,#36071,#36072,#36073,#36074,#36075,#36076,
#36077,#36078,#36079,#36080,#36081,#36082,#36083,#36084,#36085,#36086,#36087,
#36088,#36089,#36090,#36091,#36092,#36093,#36094,#36095,#36096,#36097,#36098,
#36099,#36100,#36101,#36102,#36103,#36104,#36105,#36106,#36107,#36108,#36109,
#36110,#36111,#36112,#36113,#36114,#36115,#36116,#36117,#36118,#36119,#36120,
#36121,#36122,#36123,#36124,#36125,#36126,#36127,#36128,#36129,#36130,#36131,
#36132,#36133,#36134,#36135,#36136,#36137,#36138,#36139,#36140,#36141,#36142,
#36143,#36144,#36145,#36146,#36147,#36148,#36149,#36150,#36151,#36152,#36153,
#36154,#36155,#36156,#36157,#36158,#36159,#36160),.UNSPECIFIED.,.F.,.F.,
(4,3,3,3,3,3,3,3,3,3,3,3,3,3,3,3,3,3,3,3,3,3,3,3,3,3,3,3,3,3,3,3,3,3,3,
3,3,3,3,3,3,3,3,3,4),(436.489548064245,436.646504491129,436.803173327651,
436.959676946089,437.11626346617,437.272904027796,437.429877834427,437.47107285039,
437.628498630474,437.785634808864,437.942602225772,438.099650258557,438.256746277134,
438.414181864723,438.469865254158,438.627291146232,438.784427435501,438.941394961838,
439.098443100689,439.255539223524,439.412974911147,439.468657657926,439.626083736926,
439.783220215622,439.940187933218,440.097236263765,440.254332578791,440.411768456417,
440.467450061694,440.624875335439,440.782011007782,440.938977920586,441.096025457905,
441.253120985378,441.410556095686,441.466242465462,441.623668724918,441.780805375985,
441.93777325746,442.094821737711,442.251918194449,442.409354199941,442.46503486923,
442.653850055278,442.772733175584),.UNSPECIFIED.);
#806=B_SPLINE_CURVE_WITH_KNOTS('',3,(#36162,#36163,#36164,#36165,#36166,
#36167,#36168,#36169,#36170,#36171),.UNSPECIFIED.,.F.,.F.,(4,1,1,1,1,1,
1,4),(442.772733371425,443.463827272998,444.462619676766,445.461412080534,
446.460204484302,447.45899688807,448.457789291838,449.055918678604),
 .UNSPECIFIED.);
#807=B_SPLINE_CURVE_WITH_KNOTS('',3,(#36173,#36174,#36175,#36176,#36177,
#36178,#36179,#36180,#36181,#36182,#36183,#36184,#36185,#36186,#36187,#36188,
#36189,#36190,#36191,#36192,#36193,#36194,#36195,#36196,#36197,#36198,#36199,
#36200,#36201,#36202,#36203,#36204,#36205,#36206,#36207,#36208,#36209,#36210,
#36211,#36212,#36213,#36214,#36215,#36216,#36217,#36218,#36219,#36220,#36221,
#36222,#36223,#36224,#36225,#36226,#36227,#36228,#36229,#36230,#36231,#36232,
#36233,#36234,#36235,#36236,#36237,#36238,#36239,#36240,#36241,#36242),
 .UNSPECIFIED.,.F.,.F.,(4,3,3,3,3,3,3,3,3,3,3,3,3,3,3,3,3,3,3,3,3,3,3,4),
(449.055918897709,449.229610385918,449.404629850206,449.456581695606,449.613794725139,
449.770717733325,449.92747225092,450.084310213884,450.241197515991,450.398429524026,
450.455374099374,450.613100063877,450.770534703474,450.927797887324,451.085134321733,
451.242514824289,451.400224845591,451.454166503142,451.6102390889,451.766029595577,
451.921856980043,452.07757171625,452.233633694466,452.389339133442),
 .UNSPECIFIED.);
#808=B_SPLINE_CURVE_WITH_KNOTS('',3,(#36243,#36244,#36245,#36246),
 .UNSPECIFIED.,.F.,.F.,(4,4),(-0.00791586410721434,0.),.UNSPECIFIED.);
#809=B_SPLINE_CURVE_WITH_KNOTS('',3,(#36252,#36253,#36254,#36255,#36256,
#36257,#36258,#36259,#36260,#36261,#36262,#36263,#36264,#36265,#36266,#36267,
#36268,#36269,#36270,#36271,#36272,#36273,#36274,#36275,#36276,#36277,#36278,
#36279,#36280,#36281,#36282,#36283,#36284,#36285,#36286,#36287,#36288,#36289,
#36290,#36291,#36292,#36293,#36294,#36295,#36296,#36297,#36298,#36299,#36300,
#36301,#36302,#36303,#36304,#36305,#36306,#36307,#36308,#36309,#36310,#36311,
#36312,#36313,#36314,#36315,#36316,#36317,#36318,#36319,#36320,#36321,#36322,
#36323,#36324,#36325,#36326,#36327,#36328,#36329,#36330,#36331,#36332,#36333,
#36334,#36335,#36336,#36337,#36338,#36339,#36340,#36341,#36342,#36343,#36344,
#36345,#36346,#36347,#36348,#36349,#36350,#36351,#36352,#36353,#36354,#36355,
#36356,#36357,#36358,#36359,#36360,#36361,#36362,#36363,#36364,#36365,#36366,
#36367,#36368,#36369,#36370,#36371,#36372,#36373,#36374,#36375,#36376,#36377,
#36378,#36379,#36380,#36381,#36382,#36383,#36384,#36385,#36386,#36387,#36388,
#36389,#36390,#36391,#36392,#36393,#36394,#36395,#36396,#36397,#36398,#36399,
#36400,#36401,#36402,#36403,#36404,#36405,#36406,#36407,#36408,#36409,#36410,
#36411,#36412,#36413,#36414,#36415,#36416,#36417,#36418,#36419,#36420,#36421,
#36422,#36423,#36424,#36425,#36426,#36427,#36428,#36429,#36430,#36431,#36432,
#36433,#36434,#36435,#36436,#36437,#36438,#36439,#36440,#36441,#36442,#36443,
#36444,#36445,#36446,#36447,#36448,#36449,#36450,#36451,#36452,#36453,#36454,
#36455,#36456,#36457,#36458,#36459,#36460,#36461,#36462,#36463,#36464,#36465,
#36466,#36467,#36468,#36469,#36470,#36471,#36472,#36473,#36474,#36475,#36476,
#36477,#36478,#36479,#36480,#36481,#36482,#36483,#36484,#36485,#36486,#36487,
#36488,#36489,#36490,#36491,#36492,#36493,#36494,#36495,#36496,#36497,#36498,
#36499,#36500,#36501,#36502,#36503,#36504,#36505,#36506,#36507,#36508,#36509,
#36510,#36511,#36512,#36513,#36514,#36515,#36516,#36517,#36518,#36519,#36520,
#36521,#36522,#36523,#36524,#36525,#36526,#36527,#36528,#36529,#36530,#36531,
#36532,#36533,#36534,#36535,#36536,#36537,#36538,#36539,#36540,#36541,#36542,
#36543,#36544,#36545,#36546,#36547,#36548,#36549,#36550,#36551,#36552,#36553,
#36554,#36555,#36556,#36557,#36558,#36559,#36560,#36561,#36562,#36563,#36564,
#36565,#36566,#36567,#36568,#36569,#36570,#36571,#36572,#36573,#36574,#36575,
#36576,#36577,#36578,#36579,#36580,#36581,#36582,#36583,#36584,#36585,#36586,
#36587,#36588,#36589,#36590,#36591,#36592,#36593,#36594,#36595,#36596,#36597,
#36598,#36599,#36600,#36601,#36602,#36603,#36604,#36605,#36606,#36607,#36608,
#36609,#36610,#36611,#36612,#36613,#36614,#36615,#36616,#36617,#36618,#36619,
#36620,#36621,#36622,#36623,#36624,#36625,#36626,#36627,#36628,#36629,#36630,
#36631,#36632,#36633,#36634,#36635,#36636,#36637,#36638,#36639,#36640,#36641,
#36642,#36643,#36644,#36645,#36646,#36647,#36648,#36649,#36650,#36651,#36652,
#36653,#36654,#36655,#36656,#36657,#36658,#36659,#36660,#36661,#36662,#36663,
#36664,#36665,#36666,#36667,#36668,#36669,#36670,#36671,#36672,#36673,#36674,
#36675,#36676,#36677,#36678,#36679,#36680,#36681,#36682,#36683,#36684,#36685,
#36686,#36687,#36688,#36689,#36690,#36691,#36692,#36693,#36694,#36695,#36696,
#36697,#36698,#36699,#36700,#36701,#36702,#36703,#36704,#36705,#36706,#36707,
#36708,#36709,#36710,#36711,#36712,#36713,#36714,#36715,#36716,#36717,#36718,
#36719,#36720,#36721,#36722,#36723,#36724,#36725,#36726,#36727,#36728,#36729,
#36730,#36731,#36732,#36733,#36734,#36735,#36736,#36737,#36738,#36739,#36740,
#36741,#36742,#36743,#36744,#36745,#36746,#36747,#36748,#36749,#36750,#36751,
#36752,#36753,#36754,#36755,#36756,#36757),.UNSPECIFIED.,.F.,.F.,(4,2,2,
2,2,2,2,2,2,2,2,2,2,2,2,2,2,2,2,2,2,2,2,2,2,2,2,2,2,2,2,2,2,2,2,2,2,2,2,
2,2,2,2,2,2,2,2,2,2,2,2,2,2,2,2,2,2,2,2,2,2,2,2,2,2,2,2,2,2,2,2,2,2,2,2,
2,2,2,2,2,2,2,2,2,2,2,2,2,2,2,2,2,2,2,2,2,2,2,2,2,2,2,2,2,2,2,2,2,2,2,2,
2,2,2,2,2,2,2,2,2,2,2,2,2,2,2,2,2,2,2,2,2,2,2,2,2,2,2,2,2,2,2,2,2,2,2,2,
2,2,2,2,2,2,2,2,2,2,2,2,2,2,2,2,2,2,2,2,2,2,2,2,2,2,2,2,2,2,2,2,2,2,2,2,
2,2,2,2,2,2,2,2,2,2,2,2,2,2,2,2,2,2,2,2,2,2,2,2,2,2,2,2,2,2,2,2,2,2,2,2,
2,2,2,2,2,2,2,2,2,2,2,2,2,2,2,2,2,2,2,2,2,2,2,2,2,2,2,2,2,2,2,2,2,4),(-4.17452195813823,
-4.17439487871219,-4.17304371703842,-4.16751898071022,-4.07124317834127,
-4.02097805912889,-4.01701665778691,-4.01534436649435,-4.01413689822972,
-4.01303804791001,-4.01157109034297,-4.00799980412009,-3.97328510288968,
-3.96118187303754,-3.9582040937554,-3.89038190714491,-3.87738595554472,
-3.85814999858147,-3.85480064281765,-3.85370197759768,-3.85308691584411,
-3.85245796441397,-3.85164581171374,-3.85007115774084,-3.84152283536915,
-3.77306526540815,-3.69755844438976,-3.69408939869832,-3.69250543612561,
-3.69131332219653,-3.69019345986971,-3.68864403344617,-3.68552149338136,
-3.65627889517135,-3.56912341648603,-3.55046426996838,-3.5348819440858,
-3.53192697001401,-3.5308802384808,-3.5302665262556,-3.5296160239285,-3.52876217519765,
-3.52699267942285,-3.51447063710142,-3.4256357067731,-3.37485758225468,
-3.37133073336013,-3.36973597872587,-3.3685421000649,-3.3674252013535,-3.36588714975239,
-3.36198324460933,-3.29990085229795,-3.21557943783811,-3.20968778140487,
-3.20834675534203,-3.20771412400482,-3.2070622900077,-3.20632719290959,
-3.20508990975243,-3.20076038784155,-3.11858442813876,-3.05192537786328,
-3.04847706608442,-3.04689684025256,-3.04570516431406,-3.04458397065106,
-3.04302993385378,-3.03903110229173,-2.9736797987165,-2.92623538023344,
-2.89150516915689,-2.88837953755055,-2.88611908469317,-2.8851899209631,
-2.88457346685516,-2.88390536838238,-2.88295809372591,-2.88070618432958,
-2.846599585726,-2.82902895629226,-2.77999802358922,-2.72939691692005,-2.72587105570796,
-2.72427652294097,-2.72308271924257,-2.72196582464215,-2.72042767521092,
-2.71652297644831,-2.6541488213404,-2.64041511211457,-2.59287158752175,
-2.57370876219136,-2.56462291761118,-2.56310018676764,-2.5622999809912,
-2.56170844946875,-2.56096241590814,-2.55968830753537,-2.55525276888979,
-2.45753641714127,-2.41157754200579,-2.40425448525077,-2.40213215900515,
-2.40082880405687,-2.39964586996712,-2.39812641827048,-2.39499263315095,
-2.37482154214041,-2.36901236391043,-2.29320657331557,-2.26810504573274,
-2.24489949690437,-2.24115118541617,-2.24000487821059,-2.23928736561258,
-2.2386225564605,-2.23775013322241,-2.23627684319443,-2.22724976920248,
-2.12312025780303,-2.08757228391103,-2.08143573950935,-2.07937077994688,
-2.07820909670758,-2.07714875883562,-2.0757300491835,-2.07308560424089,
-2.05858157330693,-2.02958123014083,-1.97997480343435,-1.92993335560801,
-1.9194627325079,-1.91774992846371,-1.91691055448302,-1.91625274508118,
-1.91551208466408,-1.91425954678137,-1.90944716770033,-1.87364533974832,
-1.77763326522993,-1.76032089329098,-1.75736695874268,-1.75586440948753,
-1.75468473501134,-1.75337481351886,-1.75121865243197,-1.74354918289198,
-1.71778119473499,-1.67436127825297,-1.59993326204173,-1.59587681081144,
-1.59464687167504,-1.59398463612504,-1.5933295392782,-1.59252085711016,
-1.59095721723457,-1.58088363471824,-1.55707818709128,-1.46645659202487,
-1.43821329232126,-1.43477389122103,-1.43321229954982,-1.43201914392537,
-1.43074664416405,-1.42876366757775,-1.42266901134504,-1.38863668929722,
-1.29214239504961,-1.28788675215526,-1.28676987080638,-1.27406106364352,
-1.27228294938027,-1.27142652550335,-1.27077572626754,-1.27007213124424,
-1.26894548662688,-1.26539033076042,-1.21319444198684,-1.14094231228655,
-1.13310940677126,-1.11547537849553,-1.11249762009222,-1.11098684629006,
-1.10980260227608,-1.10848954203071,-1.10633262823352,-1.09870476246025,
-1.07304168430524,-1.02985381806037,-0.962252279246089,-0.9516570962742,
-0.949972117162118,-0.949136321961259,-0.948489038628986,-0.947784741284802,
-0.946630355721876,-0.942753838349444,-0.918104484049999,-0.871376559550471,
-0.822886524110304,-0.814246672214374,-0.812483583562317,-0.806669877582027,
-0.791872501432713,-0.789320986427135,-0.787787048264001,-0.786605308780887,
-0.785335469360111,-0.783336799056528,-0.777037574735127,-0.740984582715386,
-0.687841760955233,-0.669496699765245,-0.629806478653441,-0.627297823410744,
-0.62630856066437,-0.625633113403179,-0.624970056093921,-0.624298559150293,
-0.622583053997668,-0.607486838643412,-0.579308217741458,-0.56048587428884,
-0.490617654251995,-0.469131099911989,-0.465927403096475,-0.464405844367376,
-0.463213996302834,-0.461913463564495,-0.459823609433707,-0.452868693162849,
-0.410757858894963,-0.363208647058619,-0.337648196126533,-0.306577047628254,
-0.304350317573486,-0.303399891016416,-0.302721331596898,-0.302028285969172,
-0.301001549021682,-0.298306739488092,-0.240705848798112,-0.177330690865758,
-0.151226259779667,-0.147821601327506,-0.146251722472837,-0.145042059850584,
-0.143741943667973,-0.141694963979227,-0.135236843584198,-0.0982832532670226,
-0.00581586883394552),.UNSPECIFIED.);
#810=B_SPLINE_CURVE_WITH_KNOTS('',3,(#36761,#36762,#36763,#36764,#36765,
#36766,#36767,#36768,#36769,#36770,#36771,#36772,#36773,#36774,#36775,#36776,
#36777,#36778,#36779,#36780,#36781,#36782,#36783,#36784,#36785,#36786,#36787,
#36788,#36789,#36790,#36791,#36792,#36793,#36794,#36795,#36796,#36797,#36798,
#36799,#36800,#36801,#36802,#36803,#36804,#36805,#36806,#36807,#36808,#36809,
#36810,#36811,#36812,#36813,#36814,#36815,#36816,#36817,#36818,#36819,#36820,
#36821,#36822,#36823,#36824,#36825,#36826,#36827,#36828,#36829,#36830,#36831,
#36832,#36833,#36834,#36835,#36836,#36837,#36838,#36839,#36840,#36841,#36842,
#36843,#36844,#36845,#36846,#36847,#36848,#36849,#36850,#36851,#36852,#36853,
#36854,#36855,#36856,#36857,#36858,#36859,#36860),.UNSPECIFIED.,.F.,.F.,
(4,3,3,3,3,3,3,3,3,3,3,3,3,3,3,3,3,3,3,3,3,3,3,3,3,3,3,3,3,3,3,3,3,4),(461.814120077872,
461.996678916982,462.180661142849,462.214783094703,462.380022213048,462.544944361337,
462.712102145621,462.876947800157,463.045261649314,463.213575498471,463.379353738302,
463.544813520999,463.711702116309,463.877070819623,464.044719360931,464.212367902239,
464.378036200707,464.543393437582,464.710335154688,464.8756207972,465.043390551604,
465.211160306007,465.37487731671,465.538278868406,465.706197328749,465.869554386492,
466.039753548133,466.209952709775,466.379993374218,466.54965327262,466.719100095224,
466.888395573125,467.05782179669,467.208745113543),.UNSPECIFIED.);
#811=B_SPLINE_CURVE_WITH_KNOTS('',3,(#36862,#36863,#36864,#36865,#36866,
#36867,#36868,#36869,#36870,#36871,#36872,#36873,#36874,#36875,#36876,#36877,
#36878,#36879,#36880,#36881,#36882,#36883,#36884,#36885,#36886,#36887,#36888,
#36889,#36890,#36891,#36892,#36893,#36894,#36895,#36896,#36897,#36898,#36899,
#36900,#36901,#36902,#36903,#36904,#36905,#36906,#36907,#36908,#36909,#36910,
#36911,#36912,#36913,#36914,#36915,#36916,#36917,#36918,#36919,#36920,#36921,
#36922,#36923,#36924,#36925,#36926,#36927,#36928,#36929,#36930,#36931,#36932,
#36933,#36934,#36935,#36936,#36937,#36938,#36939,#36940,#36941,#36942,#36943,
#36944,#36945,#36946,#36947,#36948,#36949,#36950,#36951,#36952,#36953,#36954,
#36955,#36956,#36957,#36958,#36959,#36960,#36961,#36962,#36963,#36964,#36965,
#36966,#36967,#36968,#36969,#36970,#36971,#36972,#36973,#36974,#36975,#36976,
#36977,#36978,#36979,#36980,#36981,#36982,#36983,#36984,#36985,#36986,#36987,
#36988,#36989,#36990,#36991,#36992,#36993,#36994,#36995,#36996,#36997,#36998,
#36999,#37000,#37001,#37002,#37003,#37004,#37005,#37006,#37007,#37008,#37009,
#37010,#37011,#37012,#37013,#37014,#37015,#37016,#37017,#37018,#37019,#37020,
#37021,#37022,#37023,#37024,#37025,#37026,#37027,#37028,#37029,#37030,#37031,
#37032,#37033,#37034,#37035,#37036,#37037,#37038,#37039,#37040,#37041,#37042,
#37043,#37044,#37045,#37046,#37047,#37048,#37049,#37050,#37051,#37052,#37053,
#37054,#37055,#37056,#37057,#37058,#37059,#37060,#37061,#37062,#37063,#37064,
#37065,#37066,#37067,#37068,#37069,#37070,#37071,#37072,#37073,#37074,#37075,
#37076,#37077,#37078,#37079,#37080,#37081,#37082,#37083,#37084,#37085,#37086,
#37087,#37088,#37089,#37090,#37091,#37092,#37093,#37094,#37095,#37096,#37097,
#37098,#37099,#37100,#37101,#37102,#37103,#37104,#37105,#37106,#37107,#37108,
#37109,#37110,#37111,#37112,#37113,#37114,#37115,#37116,#37117,#37118,#37119,
#37120,#37121,#37122,#37123,#37124,#37125,#37126,#37127,#37128,#37129,#37130,
#37131,#37132,#37133,#37134,#37135,#37136,#37137,#37138,#37139,#37140,#37141,
#37142,#37143,#37144,#37145,#37146,#37147,#37148,#37149,#37150,#37151,#37152,
#37153,#37154,#37155,#37156,#37157,#37158,#37159,#37160,#37161,#37162,#37163,
#37164,#37165,#37166,#37167,#37168,#37169,#37170,#37171,#37172,#37173,#37174,
#37175,#37176,#37177,#37178,#37179,#37180,#37181,#37182,#37183,#37184,#37185,
#37186,#37187,#37188,#37189,#37190,#37191,#37192,#37193,#37194,#37195,#37196,
#37197,#37198,#37199,#37200,#37201,#37202,#37203,#37204,#37205,#37206,#37207,
#37208,#37209,#37210,#37211,#37212,#37213,#37214,#37215,#37216,#37217,#37218,
#37219,#37220,#37221,#37222,#37223,#37224,#37225,#37226,#37227,#37228,#37229,
#37230,#37231,#37232,#37233,#37234,#37235,#37236,#37237,#37238,#37239,#37240,
#37241,#37242,#37243,#37244,#37245,#37246,#37247,#37248,#37249,#37250,#37251,
#37252,#37253,#37254,#37255,#37256,#37257,#37258,#37259,#37260,#37261,#37262,
#37263,#37264,#37265,#37266,#37267,#37268,#37269,#37270,#37271,#37272,#37273,
#37274,#37275,#37276,#37277,#37278,#37279,#37280,#37281,#37282,#37283,#37284,
#37285,#37286,#37287,#37288,#37289,#37290,#37291,#37292,#37293,#37294,#37295,
#37296,#37297,#37298,#37299,#37300,#37301,#37302,#37303,#37304,#37305,#37306,
#37307,#37308,#37309,#37310,#37311,#37312,#37313,#37314,#37315,#37316,#37317,
#37318,#37319,#37320,#37321,#37322,#37323,#37324,#37325,#37326,#37327,#37328,
#37329,#37330,#37331,#37332,#37333,#37334,#37335,#37336,#37337,#37338,#37339,
#37340,#37341,#37342,#37343,#37344,#37345,#37346,#37347,#37348,#37349,#37350,
#37351,#37352,#37353,#37354,#37355,#37356,#37357,#37358,#37359,#37360,#37361,
#37362,#37363,#37364,#37365,#37366,#37367,#37368,#37369,#37370,#37371,#37372,
#37373,#37374,#37375,#37376,#37377,#37378,#37379,#37380,#37381,#37382,#37383,
#37384,#37385,#37386,#37387,#37388,#37389,#37390,#37391,#37392,#37393,#37394,
#37395,#37396,#37397,#37398,#37399,#37400,#37401,#37402,#37403,#37404,#37405,
#37406,#37407),.UNSPECIFIED.,.F.,.F.,(4,2,2,2,2,2,2,2,2,2,2,2,2,2,2,2,2,
2,2,2,2,2,2,2,2,2,2,2,2,2,2,2,2,2,2,2,2,2,2,2,2,2,2,2,2,2,2,2,2,2,2,2,2,
2,2,2,2,2,2,2,2,2,2,2,2,2,2,2,2,2,2,2,2,2,2,2,2,2,2,2,2,2,2,2,2,2,2,2,2,
2,2,2,2,2,2,2,2,2,2,2,2,2,2,2,2,2,2,2,2,2,2,2,2,2,2,2,2,2,2,2,2,2,2,2,2,
2,2,2,2,2,2,2,2,2,2,2,2,2,2,2,2,2,2,2,2,2,2,2,2,2,2,2,2,2,2,2,2,2,2,2,2,
2,2,2,2,2,2,2,2,2,2,2,2,2,2,2,2,2,2,2,2,2,2,2,2,2,2,2,2,2,2,2,2,2,2,2,2,
2,2,2,2,2,2,2,2,2,2,2,2,2,2,2,2,2,2,2,2,2,2,2,2,2,2,2,2,2,2,2,2,2,2,2,2,
2,2,2,2,2,2,2,2,2,2,2,2,2,2,2,2,2,2,2,2,2,2,2,2,2,2,2,2,2,2,2,2,2,2,2,2,
2,2,2,4),(-4.0609209577756,-4.03439321587138,-4.03202807571868,-4.03052003469874,
-4.02935948148285,-4.02822854629725,-4.02710794456281,-4.02556121498386,
-4.0216162442498,-4.01215908496159,-4.00388370548196,-4.00093305540347,
-3.99428904551967,-3.91873599607122,-3.87220276864995,-3.86938848356587,
-3.86835932384938,-3.86766582874838,-3.86699358753679,-3.86618053102651,
-3.8642152986347,-3.84635442487326,-3.83486398267195,-3.74760157037942,
-3.7234393793014,-3.71524001563234,-3.70974579616973,-3.70784583793269,
-3.70674393341832,-3.70556180449928,-3.70404874302576,-3.70094705356752,
-3.68147362314665,-3.61903469940853,-3.61262187825567,-3.60527147043571,
-3.58079108255082,-3.56407050344909,-3.54798380771523,-3.54624993420277,
-3.54540667860522,-3.54481003896041,-3.54417970546147,-3.54310804563247,
-3.54022069661968,-3.53952156374914,-3.48257860387633,-3.43265590626405,
-3.40325216161727,-3.39353828947865,-3.38936163390965,-3.38711944361243,
-3.38519418901268,-3.38394694089309,-3.38275686070036,-3.38120416118785,
-3.37780404584238,-3.3506621669407,-3.34773906234186,-3.26554351356637,
-3.25161369395554,-3.23434213896093,-3.22499747588465,-3.2234650725166,
-3.22266352656457,-3.22207235386216,-3.22142335000057,-3.22026045340737,
-3.21674254182672,-3.15757669428901,-3.10841311809563,-3.07103655670531,
-3.06675776042096,-3.06447505468622,-3.06300280933877,-3.06162833065377,
-3.06047769156413,-3.05910398508388,-3.0567299255297,-3.04765934519056,
-3.04405390035487,-3.04140484031206,-3.03667589549175,-2.94284246935056,
-2.90670832928653,-2.90187060822497,-2.90061455799448,-2.89987241325827,
-2.89921440724647,-2.89837570211009,-2.89672209553241,-2.8869985567319,
-2.78348914037489,-2.74800551641451,-2.74385673988027,-2.74162474667482,
-2.73970543804909,-2.73845927642587,-2.73726706900813,-2.73570746443624,
-2.73227548412224,-2.70421493127265,-2.68405882127573,-2.61733468972596,
-2.58372331487403,-2.58065226290383,-2.5784234476627,-2.57748879271198,
-2.57681643961353,-2.57619983968093,-2.57536179578987,-2.57371799905378,
-2.56069484014506,-2.47137188838082,-2.42649443838459,-2.42173191388313,
-2.41814775891608,-2.41654305129541,-2.4153481323626,-2.41423488022111,
-2.41270905730336,-2.40887383573535,-2.35682755459862,-2.32103693855499,
-2.2852853276149,-2.26020966070372,-2.25628431377604,-2.25511895574868,
-2.25439757655385,-2.25373506052437,-2.25287353623011,-2.25106556977928,
-2.23790071218223,-2.2373472829386,-2.23493750603952,-2.23404679642131,
-2.14624863249812,-2.09906537571398,-2.09550871743851,-2.09390897257151,
-2.09271478742372,-2.09160008133662,-2.09006892886611,-2.0862028946839,
-2.03072694426372,-1.95510369053103,-1.9537167130423,-1.9350259399944,-1.93301371475446,
-1.93220672578147,-1.93153694824017,-1.93084478355361,-1.9298122889228,
-1.92695601908714,-1.90795003050569,-1.87171203057028,-1.79704687752457,
-1.79559057131351,-1.77578747397896,-1.77267171358367,-1.77115635367021,
-1.76997450057847,-1.76867019849177,-1.76654151457586,-1.75915004078413,
-1.71243495772883,-1.61562634520975,-1.6111292899295,-1.60984875534357,
-1.60910147516649,-1.60851036405338,-1.60771254222833,-1.6062002744661,
-1.59733729142129,-1.57840112291465,-1.53177633150656,-1.48324703370828,
-1.45365517357835,-1.45052395126507,-1.44897260408948,-1.44785247230227,
-1.44666111040255,-1.44507991820199,-1.44162400375511,-1.37189982512988,
-1.29991349191457,-1.2892206701147,-1.28749709406024,-1.28665570221722,
-1.28601254744694,-1.28529232581667,-1.28453511863891,-1.28341150400969,
-1.2813973641174,-1.2653768742639,-1.24558351684465,-1.16119822249368,-1.15358879321061,
-1.13056623712461,-1.12763702464534,-1.12613690667462,-1.12503003572176,
-1.12383008227053,-1.12219758857568,-1.11846145279996,-1.11344638931789,
-1.08779003937515,-1.0445925519493,-0.977297545623666,-0.966541711980067,
-0.964815020125381,-0.963973006930939,-0.963330382181621,-0.962610803367827,
-0.961854416453928,-0.960732749519643,-0.958723488056508,-0.942771741214701,
-0.923152353188501,-0.83686818747535,-0.808177203438175,-0.804770117859193,
-0.803332640447792,-0.802131979067573,-0.800898253959374,-0.79909223911427,
-0.794294574676434,-0.734845483977622,-0.647556156406522,-0.643014023176239,
-0.641743547849181,-0.640991097522692,-0.640348640109639,-0.63954966544356,
-0.638681977310649,-0.637294631095284,-0.634595557617483,-0.607894259800219,
-0.558522785536575,-0.524607542742761,-0.522661135807599,-0.507119234441697,
-0.504636140169383,-0.484956702527465,-0.481845869628993,-0.480331171432535,
-0.479149046927936,-0.477843643597691,-0.475711351835398,-0.468289728454649,
-0.421261761948019,-0.3788988760285,-0.334917217031607,-0.321347113347151,
-0.319499460976579,-0.318643031633751,-0.317996770370094,-0.317291566010471,
-0.316556003234873,-0.315484609900675,-0.31360124079712,-0.30950414220205,
-0.223780335750519,-0.163513190743061,-0.159616851340557,-0.158080336353971,
-0.156964049035915,-0.155770351035245,-0.154175025343039,-0.150643605247865,
-0.0987622606105739,-0.057506443010482,-0.000958348145723925),
 .UNSPECIFIED.);
#812=B_SPLINE_CURVE_WITH_KNOTS('',3,(#37409,#37410,#37411,#37412,#37413,
#37414,#37415,#37416,#37417,#37418,#37419,#37420,#37421,#37422,#37423,#37424,
#37425,#37426,#37427,#37428,#37429,#37430,#37431,#37432,#37433,#37434,#37435,
#37436,#37437,#37438,#37439,#37440,#37441,#37442,#37443,#37444,#37445,#37446,
#37447,#37448,#37449,#37450,#37451,#37452,#37453,#37454,#37455,#37456,#37457,
#37458,#37459,#37460,#37461,#37462,#37463,#37464,#37465,#37466,#37467,#37468,
#37469,#37470,#37471,#37472,#37473,#37474,#37475,#37476,#37477,#37478,#37479,
#37480,#37481,#37482,#37483,#37484,#37485,#37486,#37487,#37488,#37489,#37490,
#37491,#37492,#37493,#37494,#37495,#37496,#37497,#37498,#37499,#37500,#37501,
#37502,#37503,#37504,#37505,#37506,#37507,#37508,#37509,#37510,#37511,#37512,
#37513,#37514,#37515,#37516,#37517,#37518,#37519,#37520,#37521,#37522,#37523,
#37524,#37525,#37526),.UNSPECIFIED.,.F.,.F.,(4,3,3,3,3,3,3,3,3,3,3,3,3,
3,3,3,3,3,3,3,3,3,3,3,3,3,3,3,3,3,3,3,3,3,3,3,3,3,3,4),(442.964564156351,
443.171659902652,443.23772742311,443.403190236612,443.568336524023,443.735382349737,
443.900448657001,444.068484241939,444.236519826878,444.401982638167,444.56712892337,
444.734174750189,444.899241055297,445.067276642971,445.235312230646,445.400775043039,
445.565921329316,445.73296715559,445.898033461685,446.06606904805,446.234104634414,
446.399567452715,446.564713744946,446.731759568255,446.896825880289,447.064861459235,
447.232897038182,447.398359840069,447.563506115897,447.73055194741,447.895618243399,
448.063653842675,448.23168944195,448.397152256145,448.562298544091,448.729344369498,
448.894410676911,449.062446261315,449.230481845718,449.24774946334),
 .UNSPECIFIED.);
#813=B_SPLINE_CURVE_WITH_KNOTS('',3,(#37528,#37529,#37530,#37531,#37532,
#37533,#37534,#37535,#37536,#37537,#37538,#37539,#37540,#37541,#37542,#37543,
#37544,#37545,#37546,#37547,#37548,#37549,#37550,#37551,#37552,#37553,#37554,
#37555,#37556,#37557,#37558,#37559,#37560,#37561,#37562,#37563,#37564,#37565,
#37566,#37567,#37568,#37569,#37570,#37571,#37572,#37573,#37574,#37575,#37576,
#37577,#37578,#37579,#37580,#37581,#37582,#37583,#37584,#37585,#37586,#37587,
#37588,#37589,#37590,#37591,#37592,#37593,#37594,#37595,#37596,#37597,#37598,
#37599,#37600,#37601,#37602,#37603,#37604,#37605,#37606,#37607,#37608,#37609,
#37610,#37611,#37612,#37613,#37614,#37615,#37616,#37617,#37618,#37619,#37620,
#37621,#37622,#37623,#37624,#37625,#37626,#37627,#37628,#37629,#37630,#37631,
#37632,#37633,#37634,#37635,#37636,#37637,#37638,#37639,#37640,#37641,#37642,
#37643,#37644,#37645,#37646,#37647,#37648,#37649,#37650,#37651,#37652,#37653,
#37654,#37655,#37656,#37657,#37658,#37659,#37660,#37661,#37662,#37663,#37664,
#37665,#37666,#37667,#37668,#37669,#37670,#37671,#37672,#37673,#37674,#37675,
#37676,#37677,#37678,#37679,#37680,#37681,#37682,#37683,#37684,#37685,#37686,
#37687,#37688,#37689,#37690,#37691,#37692,#37693,#37694,#37695,#37696,#37697,
#37698,#37699,#37700,#37701,#37702,#37703,#37704,#37705,#37706,#37707,#37708,
#37709,#37710,#37711,#37712,#37713,#37714,#37715,#37716,#37717,#37718,#37719,
#37720,#37721,#37722,#37723,#37724,#37725,#37726,#37727,#37728,#37729,#37730,
#37731,#37732,#37733,#37734,#37735,#37736,#37737,#37738,#37739,#37740,#37741,
#37742,#37743,#37744,#37745,#37746,#37747,#37748,#37749,#37750,#37751,#37752,
#37753,#37754,#37755,#37756,#37757,#37758,#37759,#37760,#37761,#37762,#37763,
#37764,#37765,#37766,#37767,#37768,#37769,#37770,#37771,#37772,#37773,#37774,
#37775,#37776,#37777,#37778,#37779,#37780,#37781,#37782,#37783,#37784,#37785,
#37786,#37787,#37788,#37789,#37790,#37791,#37792,#37793,#37794,#37795,#37796,
#37797,#37798,#37799,#37800,#37801,#37802,#37803,#37804,#37805,#37806,#37807,
#37808,#37809,#37810,#37811,#37812,#37813,#37814,#37815,#37816,#37817,#37818,
#37819,#37820,#37821,#37822,#37823,#37824,#37825,#37826,#37827,#37828,#37829,
#37830,#37831,#37832,#37833,#37834,#37835,#37836,#37837,#37838,#37839,#37840,
#37841,#37842,#37843,#37844,#37845,#37846,#37847,#37848,#37849,#37850,#37851,
#37852,#37853,#37854,#37855,#37856,#37857,#37858,#37859,#37860,#37861,#37862,
#37863,#37864,#37865,#37866,#37867,#37868,#37869,#37870,#37871,#37872,#37873,
#37874,#37875,#37876,#37877,#37878,#37879,#37880,#37881,#37882,#37883,#37884,
#37885,#37886,#37887,#37888,#37889,#37890,#37891,#37892,#37893,#37894,#37895,
#37896,#37897,#37898,#37899,#37900,#37901,#37902,#37903,#37904,#37905,#37906,
#37907,#37908,#37909,#37910,#37911,#37912,#37913,#37914,#37915,#37916,#37917,
#37918,#37919,#37920,#37921,#37922,#37923,#37924,#37925,#37926,#37927,#37928,
#37929,#37930,#37931,#37932,#37933,#37934,#37935,#37936,#37937,#37938,#37939,
#37940,#37941,#37942,#37943,#37944,#37945,#37946,#37947,#37948,#37949,#37950,
#37951,#37952,#37953,#37954,#37955,#37956,#37957,#37958,#37959,#37960,#37961,
#37962,#37963,#37964,#37965,#37966,#37967,#37968,#37969,#37970,#37971,#37972,
#37973,#37974,#37975,#37976,#37977,#37978,#37979,#37980,#37981,#37982,#37983,
#37984,#37985,#37986,#37987,#37988,#37989,#37990,#37991,#37992,#37993,#37994,
#37995,#37996,#37997,#37998,#37999,#38000,#38001,#38002,#38003,#38004,#38005,
#38006,#38007,#38008,#38009,#38010,#38011,#38012,#38013,#38014,#38015,#38016,
#38017,#38018,#38019,#38020,#38021,#38022,#38023,#38024,#38025,#38026,#38027,
#38028,#38029,#38030,#38031,#38032,#38033,#38034,#38035,#38036,#38037,#38038,
#38039,#38040,#38041,#38042,#38043,#38044,#38045,#38046,#38047,#38048,#38049,
#38050,#38051,#38052,#38053,#38054,#38055,#38056,#38057),.UNSPECIFIED.,
 .F.,.F.,(4,2,2,2,2,2,2,2,2,2,2,2,2,2,2,2,2,2,2,2,2,2,2,2,2,2,2,2,2,2,2,
2,2,2,2,2,2,2,2,2,2,2,2,2,2,2,2,2,2,2,2,2,2,2,2,2,2,2,2,2,2,2,2,2,2,2,2,
2,2,2,2,2,2,2,2,2,2,2,2,2,2,2,2,2,2,2,2,2,2,2,2,2,2,2,2,2,2,2,2,2,2,2,2,
2,2,2,2,2,2,2,2,2,2,2,2,2,2,2,2,2,2,2,2,2,2,2,2,2,2,2,2,2,2,2,2,2,2,2,2,
2,2,2,2,2,2,2,2,2,2,2,2,2,2,2,2,2,2,2,2,2,2,2,2,2,2,2,2,2,2,2,2,2,2,2,2,
2,2,2,2,2,2,2,2,2,2,2,2,2,2,2,2,2,2,2,2,2,2,2,2,2,2,2,2,2,2,2,2,2,2,2,2,
2,2,2,2,2,2,2,2,2,2,2,2,2,2,2,2,2,2,2,2,2,2,2,2,2,2,2,2,2,2,2,2,2,2,2,2,
2,2,2,2,2,2,2,2,2,2,2,2,2,2,2,2,2,4),(-4.06054070524022,-3.99326051522267,
-3.99084428973821,-3.98931615075845,-3.98815039828341,-3.9869598316091,
-3.98583955478882,-3.98428658768096,-3.98028941894997,-3.91492271730446,
-3.89784305425163,-3.88168222377462,-3.8380713848695,-3.82863919750129,
-3.82709453356329,-3.8262900523961,-3.82563527152188,-3.82497056070661,
-3.82372888627286,-3.81957427593269,-3.74572513344288,-3.71937329977857,
-3.6862450786394,-3.67528013525912,-3.66839009918962,-3.66684849532081,
-3.66567798593909,-3.66448493392157,-3.66336908462542,-3.66183291190795,
-3.65793606789556,-3.59717372685146,-3.54276346777064,-3.51528145248087,
-3.50611532054715,-3.50458209341171,-3.50378001734271,-3.50318868262822,
-3.50253991045274,-3.50137728144466,-3.49785946278574,-3.43882426589436,
-3.40366292571612,-3.36436568411959,-3.34715033410808,-3.34439294550577,
-3.34321876996622,-3.34202373463892,-3.34091099648772,-3.33938684556923,
-3.33556085018345,-3.28432065404834,-3.21647747064557,-3.19358693672542,
-3.18369494262758,-3.18211699045145,-3.18130551124483,-3.18071312094093,
-3.18006904065185,-3.17912903492342,-3.17641828224889,-3.12853473407145,
-3.07577633330864,-3.03068256462879,-3.02590696022578,-3.02234437803812,
-3.02074693341714,-3.01954774819364,-3.01844087030313,-3.01693965210507,
-3.01400506094663,-2.99081508337822,-2.9763909121661,-2.89394559692313,
-2.86478218931693,-2.86051073143986,-2.85929602441597,-2.8585635696021,
-2.85790416305989,-2.85705019405579,-2.85526214381779,-2.84314230454785,
-2.84059228620198,-2.83282051251006,-2.817411616467,-2.74375975325612,-2.70705827826076,
-2.70282637917681,-2.69959266466719,-2.69806013403569,-2.69687168889515,
-2.69574679483467,-2.69417681033429,-2.69007707858343,-2.62117099375599,
-2.57691919067398,-2.55016405954213,-2.53865515159709,-2.5370404052921,
-2.53622126402496,-2.53556546133188,-2.53481137501156,-2.53353312678784,
-2.52891455966321,-2.44162726308138,-2.38043945137047,-2.37701431828801,
-2.37543923089102,-2.37424914701846,-2.37312777059087,-2.37157080257494,
-2.36754980656784,-2.31785008679071,-2.2927495632976,-2.24442945571271,
-2.21920637061212,-2.21526738715837,-2.2141005949072,-2.2133789238333,-2.21271663834819,
-2.21185601493605,-2.21005196114373,-2.19698443919665,-2.19383724275246,
-2.09593000097063,-2.06151341737643,-2.05537760401702,-2.05339089919288,
-2.05211847979351,-2.05092715038737,-2.04937046576136,-2.04675857594624,
-2.03104681987095,-2.00018903714906,-1.89649175050529,-1.89259974624666,
-1.89138933387924,-1.89073085713579,-1.89007530094762,-1.88925972897669,
-1.88766232294627,-1.87666583152726,-1.84848841454193,-1.80430877568617,
-1.76243080427412,-1.73519416476745,-1.73178888311709,-1.7302343950116,
-1.72904317930188,-1.72776935545361,-1.72577729684793,-1.71960036080034,
-1.68480867900998,-1.58511244918773,-1.58466726188599,-1.58400038227583,
-1.57099684002269,-1.56935353426866,-1.56851554481753,-1.56789888880882,
-1.56722640704725,-1.56629139935074,-1.56406090175465,-1.56098713675671,
-1.52732831510471,-1.44443562120157,-1.41263262841465,-1.40909090643026,
-1.40765350960922,-1.40645291839276,-1.40521926831581,-1.40341336871755,
-1.39861604174526,-1.33917040317465,-1.25186972236286,-1.24734225255723,
-1.24607338656308,-1.24532133852643,-1.24467130491806,-1.24386825644434,
-1.2423103831265,-1.24032727550266,-1.22474461305183,-1.20607691229983,
-1.14438025761629,-1.09048239542283,-1.08662903660657,-1.08509983565135,
-1.08398546816295,-1.08279062542378,-1.08118823267201,-1.07761840113263,
-1.02466724597505,-0.941159406369667,-0.938807059458008,-0.936068876591834,
-0.925373720310044,-0.923649920493063,-0.92280843870987,-0.922150272100306,
-0.921425238248575,-0.920293060536237,-0.918900933774189,-0.916189100617598,
-0.889269126479808,-0.842096112473254,-0.768651788895451,-0.764147673727876,
-0.762513352248259,-0.761370684610278,-0.760306743782586,-0.758851318376796,
-0.756031252266613,-0.737463917338268,-0.721333257226002,-0.676176616696737,
-0.627001089408738,-0.622974664504605,-0.603192450440141,-0.601354113354206,
-0.6004672624776,-0.599837660986247,-0.599240023440999,-0.598598800769223,
-0.597195423405945,-0.590329047383933,-0.576735512846013,-0.537794237235253,
-0.466422934081607,-0.444043731308734,-0.441138033208306,-0.439643913526779,
-0.438538502051963,-0.437337258003372,-0.435697867853547,-0.431923422307785,
-0.372418154913922,-0.345927432654378,-0.316207596183532,-0.303440638885575,
-0.301491700462127,-0.29572331895682,-0.292460426386885,-0.280178858544415,
-0.27856171791013,-0.277730409380508,-0.277115405793912,-0.276493627558292,
-0.275834062359139,-0.274954698785619,-0.270835113653864,-0.244989287461306,
-0.225911490542072,-0.159529503985296,-0.146375748866441,-0.140912668496702,
-0.121244625231708,-0.118134463827853,-0.116619957686544,-0.11543792180178,
-0.114132553933041,-0.112000179080363,-0.104576891054096,-0.0575288054657179,
-0.000958222783552507),.UNSPECIFIED.);
#814=B_SPLINE_CURVE_WITH_KNOTS('',3,(#38059,#38060,#38061,#38062,#38063,
#38064,#38065,#38066,#38067,#38068,#38069),.UNSPECIFIED.,.F.,.F.,(4,1,1,
1,1,1,1,1,4),(424.115008234622,424.260671751518,425.259464155286,426.258256559054,
427.257048962822,428.25584136659,429.254633770358,430.253426174126,430.398193541802),
 .UNSPECIFIED.);
#815=B_SPLINE_CURVE_WITH_KNOTS('',3,(#38071,#38072,#38073,#38074,#38075,
#38076,#38077,#38078,#38079,#38080,#38081,#38082,#38083,#38084,#38085,#38086,
#38087,#38088,#38089,#38090,#38091,#38092,#38093,#38094,#38095,#38096,#38097,
#38098,#38099,#38100,#38101,#38102,#38103,#38104,#38105,#38106,#38107,#38108,
#38109,#38110,#38111,#38112,#38113,#38114,#38115,#38116,#38117,#38118,#38119,
#38120,#38121,#38122,#38123,#38124,#38125,#38126,#38127,#38128,#38129,#38130,
#38131,#38132,#38133,#38134,#38135,#38136,#38137,#38138,#38139,#38140,#38141,
#38142,#38143,#38144,#38145,#38146,#38147,#38148,#38149,#38150,#38151,#38152,
#38153,#38154,#38155,#38156,#38157,#38158,#38159,#38160,#38161,#38162,#38163,
#38164,#38165,#38166,#38167,#38168,#38169,#38170,#38171,#38172,#38173,#38174,
#38175,#38176,#38177,#38178,#38179,#38180,#38181,#38182,#38183,#38184,#38185,
#38186,#38187,#38188,#38189,#38190,#38191,#38192,#38193,#38194,#38195,#38196,
#38197,#38198,#38199,#38200,#38201,#38202,#38203,#38204,#38205,#38206,#38207,
#38208,#38209,#38210,#38211,#38212,#38213,#38214,#38215,#38216,#38217,#38218,
#38219,#38220,#38221,#38222,#38223,#38224,#38225,#38226,#38227,#38228,#38229,
#38230,#38231,#38232,#38233,#38234,#38235,#38236,#38237,#38238,#38239,#38240,
#38241,#38242,#38243,#38244,#38245,#38246,#38247,#38248,#38249,#38250,#38251,
#38252,#38253,#38254,#38255,#38256,#38257,#38258,#38259,#38260,#38261,#38262,
#38263,#38264,#38265,#38266,#38267,#38268,#38269,#38270,#38271,#38272,#38273,
#38274,#38275,#38276,#38277,#38278,#38279,#38280,#38281,#38282,#38283,#38284,
#38285,#38286,#38287,#38288,#38289,#38290,#38291,#38292,#38293,#38294,#38295,
#38296,#38297,#38298,#38299,#38300,#38301,#38302,#38303,#38304,#38305,#38306,
#38307,#38308,#38309,#38310,#38311,#38312,#38313,#38314,#38315,#38316,#38317,
#38318,#38319,#38320,#38321,#38322,#38323,#38324,#38325,#38326,#38327,#38328,
#38329,#38330,#38331,#38332,#38333,#38334,#38335,#38336,#38337,#38338,#38339,
#38340,#38341,#38342,#38343,#38344,#38345,#38346,#38347,#38348,#38349,#38350,
#38351,#38352,#38353,#38354,#38355,#38356,#38357,#38358,#38359,#38360,#38361,
#38362,#38363,#38364,#38365,#38366,#38367,#38368,#38369,#38370,#38371,#38372,
#38373,#38374,#38375,#38376,#38377,#38378,#38379,#38380,#38381,#38382,#38383,
#38384,#38385,#38386,#38387,#38388,#38389,#38390,#38391,#38392,#38393,#38394,
#38395,#38396,#38397,#38398,#38399,#38400,#38401,#38402,#38403,#38404,#38405,
#38406,#38407,#38408,#38409,#38410,#38411,#38412,#38413,#38414,#38415,#38416,
#38417,#38418,#38419,#38420,#38421,#38422,#38423,#38424,#38425,#38426,#38427,
#38428,#38429,#38430,#38431,#38432,#38433,#38434,#38435,#38436,#38437,#38438,
#38439,#38440,#38441,#38442,#38443,#38444,#38445,#38446,#38447,#38448,#38449,
#38450,#38451,#38452,#38453,#38454,#38455,#38456,#38457,#38458,#38459,#38460,
#38461,#38462,#38463,#38464,#38465,#38466,#38467,#38468,#38469,#38470,#38471,
#38472,#38473,#38474,#38475,#38476,#38477,#38478,#38479,#38480,#38481,#38482,
#38483,#38484,#38485,#38486,#38487,#38488,#38489,#38490,#38491,#38492,#38493,
#38494,#38495,#38496,#38497,#38498,#38499,#38500,#38501,#38502,#38503,#38504,
#38505,#38506,#38507,#38508,#38509,#38510,#38511,#38512,#38513,#38514,#38515,
#38516,#38517,#38518,#38519,#38520,#38521,#38522,#38523,#38524,#38525,#38526,
#38527,#38528,#38529,#38530,#38531,#38532,#38533,#38534,#38535,#38536,#38537,
#38538,#38539,#38540,#38541,#38542,#38543,#38544,#38545,#38546,#38547,#38548,
#38549,#38550,#38551,#38552,#38553,#38554,#38555,#38556,#38557,#38558,#38559,
#38560,#38561,#38562,#38563,#38564,#38565,#38566,#38567,#38568,#38569,#38570,
#38571,#38572,#38573,#38574,#38575,#38576,#38577,#38578,#38579,#38580,#38581,
#38582,#38583,#38584,#38585,#38586,#38587,#38588,#38589,#38590,#38591,#38592,
#38593,#38594,#38595,#38596,#38597,#38598,#38599,#38600,#38601,#38602,#38603,
#38604),.UNSPECIFIED.,.F.,.F.,(4,2,2,2,2,2,2,2,2,2,2,2,2,2,2,2,2,2,2,2,
2,2,2,2,2,2,2,2,2,2,2,2,2,2,2,2,2,2,2,2,2,2,2,2,2,2,2,2,2,2,2,2,2,2,2,2,
2,2,2,2,2,2,2,2,2,2,2,2,2,2,2,2,2,2,2,2,2,2,2,2,2,2,2,2,2,2,2,2,2,2,2,2,
2,2,2,2,2,2,2,2,2,2,2,2,2,2,2,2,2,2,2,2,2,2,2,2,2,2,2,2,2,2,2,2,2,2,2,2,
2,2,2,2,2,2,2,2,2,2,2,2,2,2,2,2,2,2,2,2,2,2,2,2,2,2,2,2,2,2,2,2,2,2,2,2,
2,2,2,2,2,2,2,2,2,2,2,2,2,2,2,2,2,2,2,2,2,2,2,2,2,2,2,2,2,2,2,2,2,2,2,2,
2,2,2,2,2,2,2,2,2,2,2,2,2,2,2,2,2,2,2,2,2,2,2,2,2,2,2,2,2,2,2,2,2,2,2,2,
2,2,2,2,2,2,2,2,2,2,2,2,2,2,2,2,2,2,2,2,2,2,2,2,2,2,2,2,2,2,4),(-4.06128115076983,
-4.00337659414285,-3.95352302031363,-3.94957161734353,-3.94790154736699,
-3.94669494696125,-3.9455963828194,-3.94412906224133,-3.94055326902321,
-3.90559299010059,-3.8368217081903,-3.81768545738403,-3.79159930410022,
-3.78755815697234,-3.78668393196703,-3.78602630358188,-3.78540356010347,
-3.78478696598889,-3.78394907758219,-3.78230602442402,-3.76930673038337,
-3.76863966891963,-3.76819168911594,-3.75999889310883,-3.74441486304274,
-3.70533616580739,-3.66160033400585,-3.63578804248566,-3.6307197329802,
-3.62695177247449,-3.62531371958506,-3.62411288752704,-3.6230074560461,
-3.62151270429965,-3.6186039949592,-3.59613200008761,-3.52500687123347,
-3.48608234689981,-3.47507879755007,-3.46882499231493,-3.4662541052831,
-3.4643704359761,-3.46348018927821,-3.46281245739004,-3.46218948636098,
-3.46132714418981,-3.45912151703814,-3.42855538280345,-3.35907064735365,
-3.30773731462055,-3.30420911024686,-3.30261452431006,-3.30142109014958,
-3.30030483839994,-3.2987680409429,-3.29486923924047,-3.23392552169708,
-3.14880966393129,-3.14473376851407,-3.14196324095807,-3.14094514444701,
-3.14033173564655,-3.13966607051309,-3.13878578942747,-3.13680953610409,
-3.11941123736714,-3.03329993736812,-2.98501206607016,-2.98144836068129,
-2.97984716754302,-2.97865259497721,-2.97753802799056,-2.97600784860362,
-2.9721483542671,-2.91753651599664,-2.86807179042429,-2.8220572752161,-2.82017292792062,
-2.81867839614772,-2.81788893339083,-2.81729702038061,-2.81664971294239,
-2.81549516423628,-2.81204450935921,-2.75356883955704,-2.70437714124751,
-2.66271084634879,-2.65893443580827,-2.65729481503383,-2.65609364060156,
-2.65498845929144,-2.65349490229749,-2.6505910268777,-2.62825383294246,
-2.61606463596482,-2.53348155342824,-2.49863139135094,-2.49639056203132,
-2.49545374118098,-2.49478087569752,-2.49416453650912,-2.49332793739305,
-2.4916902107832,-2.47884728178292,-2.47806462670788,-2.47769236150409,
-2.47504493173271,-2.39790274120544,-2.36139330307826,-2.33875490108667,
-2.33580258184672,-2.33431993345178,-2.33325240956193,-2.33212112374322,
-2.33052823529818,-2.32628713884829,-2.25466613807874,-2.2093451006254,
-2.18508298235749,-2.17492628945015,-2.17335939963952,-2.1725500318806,
-2.17189469691472,-2.17123236148917,-2.17000344137782,-2.16596020381263,
-2.09676533278558,-2.05116792033457,-2.03140263621282,-2.01598204196407,
-2.01338474614578,-2.01183193430983,-2.0106407342294,-2.00936568881703,
-2.00736914768313,-2.00115816462975,-1.96606095971846,-1.86481930244715,
-1.85250218388215,-1.85088350930598,-1.85005173062519,-1.84943653542393,
-1.84876241531573,-1.84781942465291,-1.84554278641683,-1.80695006036606,
-1.71343611487381,-1.6934499114707,-1.69032494587288,-1.68880742949498,
-1.687624944379,-1.68632101109549,-1.68419533076884,-1.67683751282148,-1.63049373803252,
-1.57868466808116,-1.53109496508983,-1.52838549505615,-1.52744538764341,
-1.52680107799704,-1.52620834710958,-1.52539620912519,-1.52381631789719,
-1.51332027859801,-1.48741257196877,-1.37919231130839,-1.37721715169979,
-1.36919970601454,-1.36693359164968,-1.36558531054388,-1.36441002992956,
-1.36299285283188,-1.36032092503336,-1.35697180176389,-1.33244220570106,
-1.30905353004349,-1.23891413147441,-1.20758216523041,-1.20536578365824,
-1.20450157852215,-1.20387808014675,-1.20321059344723,-1.20230376136192,
-1.20032258346949,-1.17594256282558,-1.15235604387838,-1.07786204735764,
-1.04849551262255,-1.04537029860268,-1.04382044329179,-1.04270069403241,
-1.04150909383619,-1.03995816966256,-1.0366441828275,-1.03227559272862,
-0.993545917142618,-0.936759736440181,-0.900595964710359,-0.897359591211616,
-0.884318026493944,-0.882514669170517,-0.88165400466934,-0.880991517306588,
-0.880269449090748,-0.879101641326377,-0.875479742595385,-0.855345527380135,
-0.833722679499318,-0.77513345553407,-0.759604049652812,-0.749048769023668,
-0.743696504220069,-0.742457047935872,-0.741444596131449,-0.725098798543921,
-0.722452903789449,-0.720885835671027,-0.719692308580539,-0.718423090326915,
-0.716492130495393,-0.710770547526889,-0.702131962488849,-0.676242052192464,
-0.629271359365302,-0.573991840740875,-0.561699969203501,-0.5600825111822,
-0.559251144753252,-0.55863614999014,-0.557962140697752,-0.557019112314918,
-0.555965932379833,-0.547989704585828,-0.519751055138522,-0.465130511749062,
-0.404051412908648,-0.400151822098393,-0.398614797756203,-0.39749841033699,
-0.396304858474342,-0.395133871924719,-0.393591707124422,-0.386700638707445,
-0.375734121714229,-0.342562064166752,-0.315967694274086,-0.242234264453372,
-0.238109900227528,-0.236871385224489,-0.236207106160641,-0.235551937691001,
-0.234745804418132,-0.233194404707153,-0.223614723738133,-0.18027538427235,
-0.164193136826247,-0.147201617351755,-0.134960680961682,-0.0813583254433141,
-0.0775075171895236,-0.0759787046126711,-0.0748644000197485,-0.0736694170058863,
-0.0724958425958789,-0.0709465811315708,-0.0684807738006665,-0.000956977264331218),
 .UNSPECIFIED.);
#816=B_SPLINE_CURVE_WITH_KNOTS('',3,(#38606,#38607,#38608,#38609,#38610,
#38611,#38612,#38613,#38614,#38615,#38616,#38617,#38618,#38619,#38620,#38621,
#38622,#38623,#38624,#38625,#38626,#38627,#38628,#38629,#38630,#38631,#38632,
#38633,#38634,#38635,#38636,#38637,#38638,#38639,#38640,#38641,#38642,#38643,
#38644,#38645,#38646,#38647,#38648,#38649,#38650,#38651,#38652,#38653,#38654,
#38655,#38656,#38657,#38658,#38659,#38660,#38661,#38662,#38663,#38664,#38665,
#38666,#38667,#38668,#38669,#38670,#38671,#38672,#38673,#38674,#38675,#38676,
#38677,#38678,#38679,#38680,#38681,#38682,#38683,#38684,#38685,#38686,#38687,
#38688,#38689,#38690,#38691,#38692,#38693,#38694,#38695,#38696,#38697,#38698,
#38699,#38700,#38701,#38702,#38703,#38704,#38705,#38706,#38707,#38708,#38709,
#38710,#38711,#38712,#38713,#38714,#38715,#38716,#38717,#38718,#38719,#38720,
#38721,#38722,#38723,#38724,#38725,#38726,#38727,#38728,#38729,#38730,#38731,
#38732,#38733,#38734,#38735,#38736,#38737,#38738,#38739,#38740,#38741,#38742,
#38743,#38744,#38745,#38746,#38747,#38748,#38749,#38750,#38751,#38752,#38753,
#38754,#38755,#38756,#38757,#38758,#38759,#38760,#38761,#38762,#38763,#38764,
#38765,#38766,#38767,#38768,#38769,#38770,#38771,#38772,#38773,#38774,#38775,
#38776,#38777,#38778,#38779,#38780,#38781,#38782,#38783,#38784,#38785,#38786,
#38787,#38788,#38789,#38790,#38791,#38792,#38793,#38794,#38795,#38796,#38797,
#38798,#38799,#38800,#38801,#38802,#38803,#38804,#38805,#38806,#38807,#38808,
#38809,#38810,#38811,#38812,#38813,#38814,#38815,#38816,#38817,#38818,#38819,
#38820,#38821,#38822,#38823,#38824,#38825,#38826,#38827,#38828,#38829,#38830,
#38831,#38832,#38833,#38834,#38835,#38836,#38837,#38838,#38839,#38840,#38841,
#38842,#38843,#38844,#38845,#38846,#38847,#38848,#38849,#38850,#38851,#38852,
#38853,#38854,#38855,#38856,#38857,#38858,#38859,#38860,#38861,#38862,#38863,
#38864,#38865,#38866,#38867,#38868,#38869,#38870,#38871,#38872,#38873,#38874,
#38875,#38876,#38877,#38878,#38879,#38880,#38881,#38882,#38883,#38884,#38885,
#38886,#38887,#38888,#38889,#38890,#38891,#38892,#38893,#38894,#38895,#38896,
#38897,#38898,#38899,#38900,#38901,#38902,#38903,#38904,#38905,#38906,#38907,
#38908,#38909,#38910,#38911,#38912,#38913,#38914,#38915,#38916,#38917,#38918,
#38919,#38920,#38921,#38922,#38923,#38924,#38925,#38926,#38927,#38928,#38929,
#38930,#38931,#38932,#38933,#38934,#38935,#38936,#38937,#38938,#38939,#38940,
#38941,#38942,#38943,#38944,#38945,#38946,#38947,#38948,#38949,#38950,#38951,
#38952,#38953,#38954,#38955,#38956,#38957,#38958,#38959,#38960,#38961,#38962,
#38963,#38964,#38965,#38966,#38967,#38968,#38969,#38970,#38971,#38972,#38973,
#38974,#38975,#38976,#38977,#38978,#38979,#38980,#38981,#38982,#38983,#38984,
#38985,#38986,#38987,#38988,#38989,#38990,#38991,#38992,#38993,#38994,#38995,
#38996,#38997,#38998,#38999,#39000,#39001,#39002,#39003,#39004,#39005,#39006,
#39007,#39008,#39009,#39010,#39011,#39012,#39013,#39014,#39015,#39016,#39017,
#39018,#39019,#39020,#39021,#39022,#39023,#39024,#39025,#39026,#39027,#39028,
#39029,#39030,#39031,#39032,#39033,#39034,#39035,#39036,#39037,#39038,#39039,
#39040,#39041,#39042,#39043,#39044,#39045,#39046,#39047,#39048,#39049,#39050,
#39051,#39052,#39053,#39054,#39055,#39056,#39057,#39058,#39059,#39060,#39061,
#39062,#39063,#39064,#39065,#39066,#39067,#39068,#39069,#39070,#39071,#39072,
#39073,#39074,#39075,#39076,#39077,#39078,#39079,#39080,#39081,#39082,#39083,
#39084,#39085,#39086,#39087,#39088,#39089,#39090,#39091,#39092,#39093,#39094,
#39095,#39096,#39097,#39098,#39099,#39100,#39101,#39102,#39103,#39104,#39105,
#39106,#39107,#39108,#39109,#39110,#39111,#39112,#39113,#39114,#39115,#39116,
#39117,#39118,#39119,#39120,#39121,#39122,#39123,#39124,#39125,#39126,#39127,
#39128,#39129,#39130,#39131,#39132,#39133,#39134,#39135,#39136,#39137,#39138,
#39139,#39140,#39141,#39142,#39143,#39144,#39145,#39146,#39147,#39148,#39149,
#39150,#39151,#39152,#39153,#39154,#39155,#39156,#39157,#39158,#39159),
 .UNSPECIFIED.,.F.,.F.,(4,2,2,2,2,2,2,2,2,2,2,2,2,2,2,2,2,2,2,2,2,2,2,2,
2,2,2,2,2,2,2,2,2,2,2,2,2,2,2,2,2,2,2,2,2,2,2,2,2,2,2,2,2,2,2,2,2,2,2,2,
2,2,2,2,2,2,2,2,2,2,2,2,2,2,2,2,2,2,2,2,2,2,2,2,2,2,2,2,2,2,2,2,2,2,2,2,
2,2,2,2,2,2,2,2,2,2,2,2,2,2,2,2,2,2,2,2,2,2,2,2,2,2,2,2,2,2,2,2,2,2,2,2,
2,2,2,2,2,2,2,2,2,2,2,2,2,2,2,2,2,2,2,2,2,2,2,2,2,2,2,2,2,2,2,2,2,2,2,2,
2,2,2,2,2,2,2,2,2,2,2,2,2,2,2,2,2,2,2,2,2,2,2,2,2,2,2,2,2,2,2,2,2,2,2,2,
2,2,2,2,2,2,2,2,2,2,2,2,2,2,2,2,2,2,2,2,2,2,2,2,2,2,2,2,2,2,2,2,2,2,2,2,
2,2,2,2,2,2,2,2,2,2,2,2,2,2,2,2,2,2,2,2,2,2,2,2,2,2,2,2,2,2,2,2,2,2,2,2,
4),(-4.05985743828913,-3.98106395518661,-3.97680103017906,-3.97486204276291,
-3.97332002043937,-3.97251595153039,-3.9718610068192,-3.97119569804348,
-3.96995167127704,-3.9657787694658,-3.88585078515522,-3.86156563159282,
-3.82145877603785,-3.81454745049971,-3.81300456299151,-3.81183342341244,
-3.81063987760159,-3.80952398859958,-3.80798842330925,-3.80409660868656,
-3.74463547220707,-3.71789674876764,-3.69343816938377,-3.6637093792152,
-3.65616423834442,-3.65171328125454,-3.65048402520685,-3.64974826673558,
-3.64908951364081,-3.64824133078364,-3.64648296426891,-3.63504026937692,
-3.63169376695359,-3.57314380418947,-3.53617855770479,-3.50740527140734,
-3.49303723778487,-3.49049128560377,-3.48931798295473,-3.48812328122201,
-3.48700928408048,-3.48548096369386,-3.48163176439891,-3.42811659408292,
-3.37055317819946,-3.34110133333759,-3.32983839807071,-3.32822471360337,
-3.32740572167076,-3.32681231171474,-3.32617151466645,-3.32504913309249,
-3.3218238451119,-3.2668501478598,-3.22121042548354,-3.19142570765562,-3.17175828935828,
-3.16840941546383,-3.16681013853851,-3.16561041803425,-3.16450363120402,
-3.16300342809437,-3.16007345325645,-3.13702141581217,-3.12169001243361,
-3.12059699685356,-3.05160505551728,-3.01851110288221,-3.00906417778853,
-3.00622573654037,-3.00518367675347,-3.00448942659501,-3.00382110778999,
-3.00301977642636,-3.00104176527535,-2.9835754275094,-2.98258362100267,
-2.96169349755182,-2.90110354445804,-2.8543562195395,-2.84698763269912,
-2.84486545126362,-2.84355282047403,-2.84237259512579,-2.84087192920865,
-2.83792982668611,-2.82086845005743,-2.72774275613119,-2.69977444870512,
-2.68481544954595,-2.68306703983701,-2.68222073105265,-2.68162336705582,
-2.68099335091522,-2.68010482418368,-2.67825944683945,-2.65817256352403,
-2.57653368260059,-2.53141716864186,-2.52663953363931,-2.52304606603765,
-2.52143941812909,-2.52024394585335,-2.51913081867179,-2.51760616259377,
-2.51377904289108,-2.46261765454206,-2.41120234152801,-2.38668470816203,
-2.36471386623158,-2.36108729843683,-2.35995542605194,-2.35924140515383,
-2.35857605299654,-2.35769737667367,-2.35572968591057,-2.3386122673445,
-2.30475007271722,-2.27176024030886,-2.20383193979933,-2.20038124661493,
-2.19880105498407,-2.19760987191412,-2.19648948516118,-2.19493711269822,
-2.1918017124163,-2.16204976718353,-2.15533292734962,-2.15275649463431,
-2.07765511115172,-2.05105530133829,-2.03933454567053,-2.03771254873463,
-2.03689177143429,-2.03624166189933,-2.0355873184034,-2.03439792951514,
-2.0306758647374,-2.00696098453929,-1.98169586986702,-1.90736841965064,
-1.90030844786412,-1.88066125606198,-1.87755227542641,-1.87603809151406,
-1.87485619231357,-1.8735508584449,-1.87141827480954,-1.86399168064906,
-1.81690468959429,-1.73053643092043,-1.7296787087585,-1.7169314927229,-1.71529718085327,
-1.71446144291625,-1.71384530708451,-1.71317221686676,-1.71223429750922,
-1.70998713566387,-1.70688451499964,-1.67263436164602,-1.59667365656093,
-1.58012220228514,-1.57730250298544,-1.5579116062293,-1.55481437597069,
-1.55330244804808,-1.55212073037944,-1.55081398492712,-1.54867544280821,
-1.54119225270003,-1.49349391160159,-1.41226623373603,-1.41137044057747,
-1.40810797810299,-1.40771070033884,-1.40654210682658,-1.39418190137152,
-1.39256172677024,-1.39172959774865,-1.39111434957101,-1.39044038598459,
-1.38949799400813,-1.38722461899358,-1.3508423790782,-1.25468698857249,
-1.23510004256043,-1.23199369686486,-1.23047997103966,-1.22929805428327,
-1.22801882442329,-1.22601249914877,-1.22361457160696,-1.21903537545228,
-1.17708311059049,-1.11623759507788,-1.07280239378291,-1.07007881361724,
-1.06913670367478,-1.06849186704026,-1.06789932858539,-1.06708846882598,
-1.06551450329995,-1.05517373512465,-1.02999223416893,-0.942734046483729,
-0.912974669409553,-0.909838954291059,-0.908286468547347,-0.907166022319952,
-0.905974796722467,-0.904426378215918,-0.901116681102006,-0.896759600139733,
-0.886479685882287,-0.877946982304953,-0.8477495815758,-0.805027311266354,
-0.764761127191685,-0.764375447447097,-0.761909822788837,-0.748807362816994,
-0.747001668251853,-0.746140539198567,-0.745477990564899,-0.744756162913993,
-0.743589392958526,-0.739652996946715,-0.714468018027886,-0.634921719703111,
-0.617202650393045,-0.590239216616583,-0.587181911668168,-0.585649195014072,
-0.584533991959473,-0.583339878398973,-0.582167749984219,-0.579618215288261,
-0.565297903938635,-0.53661582355207,-0.504538023011802,-0.429480439559194,
-0.425194615601626,-0.423937544995388,-0.423269560418945,-0.422620992515017,
-0.421823837010682,-0.420314780187632,-0.411522214186124,-0.392719808588656,
-0.355169878331043,-0.317400746147991,-0.306945402869458,-0.306369479989895,
-0.299572074835488,-0.290155004601213,-0.267426832381596,-0.264508421846414,
-0.263011075402667,-0.261904898166456,-0.26070439083222,-0.259520738794475,
-0.257943610873731,-0.250507995535723,-0.218273638583761,-0.196668849510435,
-0.116468794268212,-0.103532088314514,-0.101890955606238,-0.101053461440696,
-0.100436872281089,-0.0997641562184845,-0.0988282840761091,-0.0965932001016937,
-0.0935115890801095,-0.0596963921842725,-0.000958062901417849),
 .UNSPECIFIED.);
#817=B_SPLINE_CURVE_WITH_KNOTS('',3,(#39161,#39162,#39163,#39164,#39165,
#39166,#39167,#39168,#39169,#39170,#39171,#39172,#39173,#39174,#39175,#39176,
#39177,#39178,#39179,#39180,#39181,#39182,#39183,#39184,#39185,#39186,#39187,
#39188,#39189,#39190,#39191,#39192,#39193,#39194,#39195,#39196,#39197,#39198,
#39199,#39200,#39201,#39202,#39203,#39204,#39205,#39206,#39207,#39208,#39209,
#39210,#39211,#39212,#39213,#39214,#39215,#39216,#39217,#39218,#39219,#39220,
#39221,#39222,#39223,#39224,#39225,#39226,#39227,#39228,#39229,#39230,#39231,
#39232,#39233,#39234,#39235,#39236,#39237,#39238,#39239,#39240,#39241,#39242,
#39243,#39244,#39245,#39246,#39247,#39248,#39249,#39250,#39251,#39252,#39253,
#39254,#39255,#39256,#39257,#39258,#39259,#39260,#39261,#39262,#39263,#39264,
#39265,#39266,#39267,#39268,#39269,#39270,#39271,#39272,#39273,#39274,#39275,
#39276,#39277,#39278,#39279,#39280,#39281,#39282,#39283,#39284,#39285,#39286,
#39287,#39288,#39289,#39290,#39291,#39292,#39293,#39294,#39295,#39296,#39297,
#39298,#39299,#39300,#39301,#39302,#39303,#39304,#39305,#39306,#39307,#39308,
#39309,#39310,#39311,#39312,#39313,#39314,#39315,#39316,#39317,#39318,#39319,
#39320,#39321,#39322,#39323,#39324,#39325,#39326,#39327,#39328,#39329,#39330,
#39331,#39332,#39333,#39334,#39335,#39336,#39337,#39338,#39339,#39340,#39341,
#39342,#39343,#39344,#39345,#39346,#39347,#39348,#39349,#39350,#39351,#39352,
#39353,#39354,#39355,#39356,#39357,#39358,#39359,#39360,#39361,#39362,#39363,
#39364,#39365,#39366,#39367,#39368,#39369,#39370,#39371,#39372,#39373,#39374,
#39375,#39376,#39377,#39378,#39379,#39380,#39381,#39382,#39383,#39384,#39385,
#39386,#39387,#39388,#39389,#39390,#39391,#39392,#39393,#39394,#39395,#39396,
#39397,#39398,#39399,#39400,#39401,#39402,#39403,#39404,#39405,#39406,#39407,
#39408,#39409,#39410,#39411,#39412,#39413,#39414,#39415,#39416,#39417,#39418,
#39419,#39420,#39421,#39422,#39423,#39424,#39425,#39426,#39427,#39428,#39429,
#39430,#39431,#39432,#39433,#39434,#39435,#39436,#39437,#39438,#39439,#39440,
#39441,#39442,#39443,#39444,#39445,#39446,#39447,#39448,#39449,#39450,#39451,
#39452,#39453,#39454,#39455,#39456,#39457,#39458,#39459,#39460,#39461,#39462,
#39463,#39464,#39465,#39466,#39467,#39468,#39469,#39470,#39471,#39472,#39473,
#39474,#39475,#39476,#39477,#39478,#39479,#39480,#39481,#39482,#39483,#39484,
#39485,#39486,#39487,#39488,#39489,#39490,#39491,#39492,#39493,#39494,#39495,
#39496,#39497,#39498,#39499,#39500,#39501,#39502,#39503,#39504,#39505,#39506,
#39507,#39508,#39509,#39510,#39511,#39512,#39513,#39514,#39515,#39516,#39517,
#39518,#39519,#39520,#39521,#39522,#39523,#39524,#39525,#39526,#39527,#39528,
#39529,#39530,#39531,#39532,#39533,#39534,#39535,#39536,#39537,#39538,#39539,
#39540,#39541,#39542,#39543,#39544,#39545,#39546,#39547,#39548,#39549,#39550,
#39551,#39552,#39553,#39554,#39555,#39556,#39557,#39558,#39559,#39560,#39561,
#39562,#39563,#39564,#39565,#39566,#39567,#39568,#39569,#39570,#39571,#39572,
#39573,#39574,#39575,#39576,#39577,#39578,#39579,#39580,#39581,#39582,#39583,
#39584,#39585,#39586,#39587,#39588,#39589,#39590,#39591,#39592,#39593,#39594,
#39595,#39596,#39597,#39598,#39599,#39600,#39601,#39602,#39603,#39604,#39605,
#39606,#39607,#39608,#39609,#39610,#39611,#39612,#39613,#39614,#39615,#39616,
#39617,#39618,#39619,#39620,#39621,#39622,#39623,#39624,#39625,#39626,#39627,
#39628,#39629,#39630,#39631,#39632,#39633,#39634,#39635,#39636,#39637,#39638,
#39639,#39640,#39641,#39642,#39643,#39644,#39645,#39646,#39647,#39648,#39649,
#39650,#39651,#39652,#39653,#39654,#39655,#39656,#39657,#39658,#39659,#39660,
#39661,#39662,#39663,#39664,#39665,#39666,#39667,#39668,#39669,#39670,#39671,
#39672,#39673,#39674,#39675,#39676,#39677,#39678,#39679,#39680,#39681,#39682,
#39683,#39684,#39685,#39686,#39687,#39688,#39689,#39690),.UNSPECIFIED.,
 .F.,.F.,(4,2,2,2,2,2,2,2,2,2,2,2,2,2,2,2,2,2,2,2,2,2,2,2,2,2,2,2,2,2,2,
2,2,2,2,2,2,2,2,2,2,2,2,2,2,2,2,2,2,2,2,2,2,2,2,2,2,2,2,2,2,2,2,2,2,2,2,
2,2,2,2,2,2,2,2,2,2,2,2,2,2,2,2,2,2,2,2,2,2,2,2,2,2,2,2,2,2,2,2,2,2,2,2,
2,2,2,2,2,2,2,2,2,2,2,2,2,2,2,2,2,2,2,2,2,2,2,2,2,2,2,2,2,2,2,2,2,2,2,2,
2,2,2,2,2,2,2,2,2,2,2,2,2,2,2,2,2,2,2,2,2,2,2,2,2,2,2,2,2,2,2,2,2,2,2,2,
2,2,2,2,2,2,2,2,2,2,2,2,2,2,2,2,2,2,2,2,2,2,2,2,2,2,2,2,2,2,2,2,2,2,2,2,
2,2,2,2,2,2,2,2,2,2,2,2,2,2,2,2,2,2,2,2,2,2,2,2,2,2,2,2,2,2,2,2,2,2,2,2,
2,2,2,2,2,2,2,2,2,2,2,2,2,2,2,2,2,4),(-4.06149043156728,-4.00581837979675,
-4.00334052717035,-4.00178628162882,-4.00061102447297,-3.99941522130083,
-3.99830270846965,-3.99678032563153,-3.9929663227205,-3.94283496208982,
-3.93559399747636,-3.87968837448941,-3.84519178415838,-3.84047227863743,
-3.83922752365697,-3.83848824736919,-3.83783011075537,-3.83698779698057,
-3.83531667968692,-3.82524707161149,-3.74956953807414,-3.72705312271508,
-3.70183475903954,-3.68877618215616,-3.68357298393008,-3.67975352803847,
-3.67846556257491,-3.67736342681777,-3.67618331263081,-3.6746837860935,
-3.67174704957063,-3.65478633014764,-3.6497991264112,-3.64080269878064,
-3.62963927160084,-3.62119804548356,-3.56915981071388,-3.56226667259324,
-3.55375611423414,-3.52996644183405,-3.51854339461683,-3.51693125579535,
-3.51611256109848,-3.51545668146772,-3.51479972799191,-3.5135971869704,
-3.50976983199108,-3.4438120568791,-3.40895540672335,-3.37551292595806,
-3.36485612104462,-3.36038094796908,-3.35701000241388,-3.35544335312315,
-3.35424924112962,-3.35313409756134,-3.3516015533835,-3.34854486019619,
-3.3216003522927,-3.30781712735768,-3.23425926036023,-3.20760663529798,
-3.19595596739138,-3.1943362950531,-3.19351602136316,-3.1928599871863,-3.19210638615152,
-3.19083068630761,-3.18623814228809,-3.09927251374508,-3.06419745889802,
-3.0398873146221,-3.03495246253299,-3.03313056723441,-3.03203058020372,
-3.03084154274146,-3.02930145570258,-3.02674681264277,-3.01209429340659,
-2.92550237231264,-2.87597029708654,-2.87234064557186,-2.87120838025185,
-2.87049425032792,-2.86982889785374,-2.86895036320901,-2.86698358020463,
-2.84988436079185,-2.84610545088336,-2.8339040425937,-2.76707668920941,
-2.74317764024306,-2.71744032039752,-2.7139981239142,-2.71126457943566,
-2.70983467542399,-2.70877036626216,-2.70762957077994,-2.70600174033468,
-2.70153932156986,-2.62636815547472,-2.57848969904921,-2.55497182236745,
-2.54996177484238,-2.54869112691636,-2.54794601922052,-2.54728880331071,
-2.54645577824458,-2.54514290787178,-2.53874260340388,-2.53753068473454,
-2.43187177127406,-2.39608482198018,-2.38979856009269,-2.38779313408404,
-2.38651625470472,-2.38532603246938,-2.3837783271904,-2.38119788586569,
-2.36608168458047,-2.32868683484901,-2.30734968855432,-2.26884607016408,
-2.23915095658938,-2.2278257226389,-2.22621691611165,-2.22539893422557,
-2.22474313903802,-2.22398803317378,-2.22270568490794,-2.21804897784234,
-2.1224969681484,-2.07489168827986,-2.06741711229514,-2.06527989616845,
-2.06397371394796,-2.06279234437239,-2.06128063840442,-2.05818307814034,
-2.03876978304821,-2.03128645458859,-2.00806069687948,-1.91679494318129,
-1.90531267034533,-1.90355244270604,-1.90270386033932,-1.90204502495239,
-1.90130941352252,-1.9000809464414,-1.89553587648808,-1.86332732056405,
-1.77640356362562,-1.74694669602831,-1.74381948038043,-1.74226926418756,
-1.74114954963591,-1.73995826071737,-1.7383765341345,-1.73491693651275,
-1.66348636388095,-1.59378958334992,-1.5825878482876,-1.58084044382942,
-1.57999439925936,-1.57933586474762,-1.57859881715422,-1.57736392762368,
-1.57275065278929,-1.5396694464484,-1.45177421040225,-1.42415310459325,
-1.42073536778248,-1.41917852633211,-1.41798689147565,-1.41671396585027,
-1.41472609853827,-1.40858381501322,-1.37410887584643,-1.2758921062224,
-1.27551632601284,-1.27306129249557,-1.25994681084638,-1.25814062957277,
-1.25727939546349,-1.25661682381564,-1.25590959008994,-1.25478076286552,
-1.25344606864184,-1.2508869384759,-1.22653272970793,-1.16286503555609,
-1.10223416078169,-1.09833655796127,-1.09679991229468,-1.09568365846267,
-1.0944901167414,-1.09289520753166,-1.08936555611704,-1.03779243771172,
-0.954186998239568,-0.952818853464944,-0.950404095374525,-0.937242366165131,
-0.935434237443029,-0.934572568802144,-0.93390988750529,-0.933202848443735,
-0.93207816308745,-0.930746999402649,-0.928197281272552,-0.843264101451716,
-0.779452437028871,-0.775546063270499,-0.774007904665031,-0.772891230327678,
-0.771697874907397,-0.770104309525041,-0.766582089573682,-0.71652326986269,
-0.632559474657294,-0.614681095467125,-0.612889293889667,-0.612013881822162,
-0.611387364557665,-0.610758022268843,-0.60990144278341,-0.608095843627627,
-0.605707421512541,-0.600049862069215,-0.581766784428509,-0.54946158457254,
-0.477931658881291,-0.455610072691515,-0.452706520684026,-0.451212959758374,
-0.450107693983158,-0.44890634864501,-0.447266354709601,-0.443488469021795,
-0.400776041374453,-0.360042451484228,-0.317073704317198,-0.310223492392585,
-0.308061028469674,-0.304857846820642,-0.291805659796358,-0.290001525663102,
-0.289140664167135,-0.288478104317273,-0.287864276067738,-0.286820424401417,
-0.283894010626118,-0.279512944889678,-0.266531095712988,-0.245716058379996,
-0.149910075152829,-0.132532027916332,-0.129573024619506,-0.128068681687065,
-0.126887980762742,-0.125577311835715,-0.123420817605302,-0.115759217333069,
-0.0900082820838625,-0.000958367751892826),.UNSPECIFIED.);
#818=B_SPLINE_CURVE_WITH_KNOTS('',3,(#39692,#39693,#39694,#39695,#39696,
#39697,#39698,#39699,#39700,#39701,#39702,#39703,#39704,#39705,#39706,#39707,
#39708,#39709,#39710,#39711,#39712,#39713,#39714,#39715,#39716,#39717,#39718,
#39719,#39720,#39721,#39722,#39723,#39724,#39725,#39726,#39727,#39728,#39729,
#39730,#39731,#39732,#39733,#39734,#39735,#39736,#39737,#39738,#39739,#39740,
#39741,#39742,#39743,#39744,#39745,#39746,#39747,#39748,#39749,#39750,#39751,
#39752,#39753,#39754,#39755,#39756,#39757,#39758,#39759,#39760,#39761,#39762,
#39763,#39764,#39765,#39766,#39767,#39768,#39769,#39770,#39771,#39772,#39773,
#39774,#39775,#39776,#39777,#39778,#39779,#39780,#39781,#39782,#39783,#39784,
#39785,#39786,#39787,#39788,#39789,#39790,#39791,#39792,#39793,#39794,#39795,
#39796,#39797,#39798,#39799,#39800,#39801,#39802,#39803,#39804,#39805,#39806,
#39807,#39808,#39809,#39810,#39811,#39812,#39813,#39814,#39815,#39816,#39817,
#39818,#39819,#39820,#39821,#39822,#39823,#39824,#39825,#39826,#39827,#39828,
#39829,#39830,#39831,#39832,#39833,#39834,#39835,#39836,#39837,#39838,#39839,
#39840,#39841,#39842,#39843,#39844,#39845,#39846,#39847,#39848,#39849,#39850,
#39851,#39852,#39853,#39854,#39855,#39856,#39857,#39858,#39859,#39860,#39861,
#39862,#39863,#39864,#39865,#39866,#39867,#39868,#39869,#39870,#39871,#39872,
#39873,#39874,#39875,#39876,#39877,#39878,#39879,#39880,#39881,#39882,#39883,
#39884,#39885,#39886,#39887,#39888,#39889,#39890,#39891,#39892,#39893,#39894,
#39895,#39896,#39897,#39898,#39899,#39900,#39901,#39902,#39903,#39904,#39905,
#39906,#39907,#39908,#39909,#39910,#39911,#39912,#39913,#39914,#39915,#39916,
#39917,#39918,#39919,#39920,#39921,#39922,#39923,#39924,#39925,#39926,#39927,
#39928,#39929,#39930,#39931,#39932,#39933,#39934,#39935,#39936,#39937,#39938,
#39939,#39940,#39941,#39942,#39943,#39944,#39945,#39946,#39947,#39948,#39949,
#39950,#39951,#39952,#39953,#39954,#39955,#39956,#39957,#39958,#39959,#39960,
#39961,#39962,#39963,#39964,#39965,#39966,#39967,#39968,#39969,#39970,#39971,
#39972,#39973,#39974,#39975,#39976,#39977,#39978,#39979,#39980,#39981,#39982,
#39983,#39984,#39985,#39986,#39987,#39988,#39989,#39990,#39991,#39992,#39993,
#39994,#39995,#39996,#39997,#39998,#39999,#40000,#40001,#40002,#40003,#40004,
#40005,#40006,#40007,#40008,#40009,#40010,#40011,#40012,#40013,#40014,#40015,
#40016,#40017,#40018,#40019,#40020,#40021,#40022,#40023,#40024,#40025,#40026,
#40027,#40028,#40029,#40030,#40031,#40032,#40033,#40034,#40035,#40036,#40037,
#40038,#40039,#40040,#40041,#40042,#40043,#40044,#40045,#40046,#40047,#40048,
#40049,#40050,#40051,#40052,#40053,#40054,#40055,#40056,#40057,#40058,#40059,
#40060,#40061,#40062,#40063,#40064,#40065,#40066,#40067,#40068,#40069,#40070,
#40071,#40072,#40073,#40074,#40075,#40076,#40077,#40078,#40079,#40080,#40081,
#40082,#40083,#40084,#40085,#40086,#40087,#40088,#40089,#40090,#40091,#40092,
#40093,#40094,#40095,#40096,#40097,#40098,#40099,#40100,#40101,#40102,#40103,
#40104,#40105,#40106,#40107,#40108,#40109,#40110,#40111,#40112,#40113,#40114,
#40115,#40116,#40117,#40118,#40119,#40120,#40121,#40122,#40123,#40124,#40125,
#40126,#40127,#40128,#40129,#40130,#40131,#40132,#40133,#40134,#40135,#40136,
#40137,#40138,#40139,#40140,#40141,#40142,#40143,#40144,#40145,#40146,#40147,
#40148,#40149,#40150,#40151,#40152,#40153,#40154,#40155,#40156,#40157,#40158,
#40159,#40160,#40161,#40162,#40163,#40164,#40165,#40166,#40167,#40168,#40169,
#40170,#40171,#40172,#40173,#40174,#40175,#40176,#40177,#40178,#40179,#40180,
#40181,#40182,#40183,#40184,#40185,#40186,#40187,#40188,#40189,#40190,#40191,
#40192,#40193,#40194,#40195,#40196,#40197,#40198,#40199,#40200,#40201,#40202,
#40203,#40204,#40205,#40206,#40207,#40208,#40209,#40210,#40211,#40212,#40213,
#40214,#40215,#40216,#40217,#40218,#40219,#40220,#40221,#40222,#40223,#40224,
#40225,#40226,#40227,#40228,#40229),.UNSPECIFIED.,.F.,.F.,(4,2,2,2,2,2,
2,2,2,2,2,2,2,2,2,2,2,2,2,2,2,2,2,2,2,2,2,2,2,2,2,2,2,2,2,2,2,2,2,2,2,2,
2,2,2,2,2,2,2,2,2,2,2,2,2,2,2,2,2,2,2,2,2,2,2,2,2,2,2,2,2,2,2,2,2,2,2,2,
2,2,2,2,2,2,2,2,2,2,2,2,2,2,2,2,2,2,2,2,2,2,2,2,2,2,2,2,2,2,2,2,2,2,2,2,
2,2,2,2,2,2,2,2,2,2,2,2,2,2,2,2,2,2,2,2,2,2,2,2,2,2,2,2,2,2,2,2,2,2,2,2,
2,2,2,2,2,2,2,2,2,2,2,2,2,2,2,2,2,2,2,2,2,2,2,2,2,2,2,2,2,2,2,2,2,2,2,2,
2,2,2,2,2,2,2,2,2,2,2,2,2,2,2,2,2,2,2,2,2,2,2,2,2,2,2,2,2,2,2,2,2,2,2,2,
2,2,2,2,2,2,2,2,2,2,2,2,2,2,2,2,2,2,2,2,2,2,2,2,2,2,2,2,2,2,2,2,2,2,2,2,
2,2,2,2,2,2,2,2,2,2,4),(-4.05959170843589,-4.02798711726565,-4.02657574666584,
-4.02569821081773,-4.02503952340485,-4.02441785342737,-4.02380279807382,
-4.02297028217099,-4.02134745348974,-4.0088930553482,-4.00781230425048,
-4.00480247029707,-4.00114129986191,-3.99233246825957,-3.98763530297311,
-3.9434148687593,-3.86927957203281,-3.86581573957689,-3.86423358099403,
-3.86304258753128,-3.86192360430866,-3.86037511972845,-3.85725362582928,
-3.82797508100751,-3.74835191021271,-3.72072764495734,-3.71415512390831,
-3.70470467091717,-3.70317176642285,-3.70251732366205,-3.70189290390233,
-3.70127357243822,-3.70042444524356,-3.69829465712175,-3.67238030116506,
-3.62040322323536,-3.61386687090801,-3.60607360222308,-3.57809194091337,
-3.55232520402001,-3.54464998508198,-3.54249273969563,-3.54118226876108,
-3.54000216914384,-3.53849917290203,-3.53554465022416,-3.5182343440434,
-3.51716278962261,-3.44842864192744,-3.41466763944054,-3.39216925670531,
-3.38562606821739,-3.38296857253047,-3.38099666855917,-3.38011091194923,
-3.37948878097006,-3.37887302211558,-3.37803784867234,-3.37640480201369,
-3.36367387713198,-3.36281187431033,-3.36071597296969,-3.35921473934554,
-3.27710713547334,-3.2295566911765,-3.22208803118854,-3.21995181281495,
-3.21864608964093,-3.21746503683688,-3.21595359983778,-3.21285611134719,
-3.1934310514034,-3.19164298126378,-3.11651102403723,-3.06491849121795,
-3.06124173862927,-3.05950275761514,-3.05848997089653,-3.0575870177305,
-3.05692949007532,-3.05631226864745,-3.05547136787374,-3.05338928383838,
-3.02995432911439,-2.93804353213902,-2.90513156133943,-2.89916269867738,
-2.89719680546365,-2.89592905286439,-2.8947359090102,-2.89316789906629,
-2.89051719910072,-2.87405772839289,-2.86864187383323,-2.79501023455936,
-2.73883219948443,-2.73701457363469,-2.73556391599424,-2.73478390243403,
-2.73413569056969,-2.73346759948526,-2.73220895436189,-2.7279057944492,
-2.64578563096422,-2.57912436625523,-2.57567932553791,-2.57410069523568,
-2.57291026331147,-2.571790270368,-2.5702379465274,-2.56710109160943,-2.53724638501829,
-2.45240391603141,-2.41867513926482,-2.41559887887888,-2.41336722508491,
-2.41243227407602,-2.41176003166997,-2.41114373973155,-2.41030645342166,
-2.40866515011107,-2.39570330269601,-2.39501330388163,-2.39461986295685,
-2.35709791092524,-2.32507368568797,-2.28800103281986,-2.26219999296711,
-2.25450712227595,-2.25234806647501,-2.25103716404954,-2.24985710736786,
-2.2483547576235,-2.24540337338364,-2.22815376632442,-2.22710952100059,
-2.13180547075541,-2.09629386730067,-2.09150163144771,-2.09025047514336,
-2.08950988168835,-2.08885218442694,-2.08801259258559,-2.08629709132287,
-2.07575758475101,-2.03111979608886,-1.96202548950655,-1.93401694556256,
-1.93058726062162,-1.92902832378566,-1.92783647108931,-1.9265646579175,
-1.92458130412699,-1.91847439723487,-1.84860619257299,-1.773215877696,-1.76890874629722,
-1.76764943626648,-1.76698109419472,-1.76633270332482,-1.76553651031646,
-1.76403148021447,-1.75532006576985,-1.736692212934,-1.69376311188224,-1.61347885469631,
-1.60864071011227,-1.60676991358382,-1.6056473715245,-1.60445772764382,
-1.60288605630931,-1.59947947694814,-1.54223161526436,-1.45742577332668,
-1.44700629233833,-1.44529663457791,-1.44445813270749,-1.44380046163443,
-1.4430590051924,-1.44180432220659,-1.43697426621603,-1.40093573483828,
-1.30514423660583,-1.28793023346886,-1.28498034768431,-1.28347816113017,
-1.28232213462967,-1.28104467696072,-1.27971133456328,-1.2777586111607,
-1.27431441707586,-1.24854296775392,-1.22462062232874,-1.12803431070674,
-1.12351111501504,-1.12222777887664,-1.12147989787315,-1.12088889653328,
-1.12009196880907,-1.11858380023822,-1.10980843781875,-1.09104153112899,
-1.04549286747864,-0.967707292849795,-0.9630985500505,-0.961448635164033,
-0.960301833748963,-0.95914578438976,-0.957684738309002,-0.956095222590293,
-0.953533309485896,-0.948519761545539,-0.922869431236602,-0.879683448242287,
-0.805052043420515,-0.800803387252043,-0.799550588532969,-0.798883484985961,
-0.798234893918666,-0.797436457537563,-0.795921249659214,-0.786993428910357,
-0.767954563458636,-0.714399064015869,-0.64441466213088,-0.640272145304883,
-0.638694996162758,-0.637568032008948,-0.636403942213641,-0.634889982478615,
-0.633227355967408,-0.630490671408316,-0.625005403129887,-0.610980677314018,
-0.579014859223885,-0.482701703188247,-0.478134850864779,-0.476861754824126,
-0.476108695900897,-0.475452491655252,-0.474631177215927,-0.473006793268334,
-0.46121491224806,-0.434680390385411,-0.389734046836864,-0.363625549918173,
-0.321079887567511,-0.3173748532572,-0.315871108856177,-0.314763235660489,
-0.313587787999309,-0.312006293674183,-0.310250194492015,-0.307288458700993,
-0.301182403455599,-0.284969422389137,-0.267066104057562,-0.217777237427747,
-0.158675528990929,-0.155256064423844,-0.154106105485343,-0.153459647922484,
-0.15286742197733,-0.152059677053076,-0.150500785779767,-0.140551006233259,
-0.117516965148734,-0.0706498920877946,-0.000957648626825045),
 .UNSPECIFIED.);
#819=B_SPLINE_CURVE_WITH_KNOTS('',3,(#40231,#40232,#40233,#40234,#40235,
#40236,#40237,#40238,#40239,#40240,#40241,#40242,#40243,#40244,#40245,#40246,
#40247,#40248,#40249,#40250,#40251,#40252,#40253,#40254,#40255,#40256,#40257,
#40258,#40259,#40260,#40261,#40262,#40263,#40264,#40265,#40266,#40267,#40268,
#40269,#40270,#40271,#40272,#40273,#40274,#40275,#40276,#40277,#40278,#40279,
#40280,#40281,#40282,#40283,#40284,#40285,#40286,#40287,#40288,#40289,#40290,
#40291,#40292,#40293,#40294,#40295,#40296,#40297,#40298,#40299,#40300,#40301,
#40302,#40303,#40304,#40305,#40306,#40307,#40308,#40309,#40310,#40311,#40312,
#40313,#40314,#40315,#40316,#40317,#40318,#40319,#40320,#40321,#40322,#40323,
#40324,#40325,#40326,#40327,#40328,#40329,#40330,#40331,#40332,#40333,#40334,
#40335,#40336,#40337,#40338,#40339,#40340,#40341,#40342,#40343,#40344,#40345,
#40346,#40347,#40348,#40349,#40350,#40351,#40352,#40353,#40354,#40355,#40356,
#40357,#40358,#40359,#40360,#40361,#40362,#40363,#40364,#40365,#40366,#40367,
#40368,#40369,#40370,#40371,#40372,#40373,#40374,#40375,#40376,#40377,#40378,
#40379,#40380,#40381,#40382,#40383,#40384,#40385,#40386,#40387,#40388,#40389,
#40390,#40391,#40392,#40393,#40394,#40395,#40396,#40397,#40398,#40399,#40400,
#40401,#40402,#40403,#40404,#40405,#40406,#40407,#40408,#40409,#40410,#40411,
#40412,#40413,#40414,#40415,#40416,#40417,#40418,#40419,#40420,#40421,#40422,
#40423,#40424,#40425,#40426,#40427,#40428,#40429,#40430,#40431,#40432,#40433,
#40434,#40435,#40436,#40437,#40438,#40439,#40440,#40441,#40442,#40443,#40444,
#40445,#40446,#40447,#40448,#40449,#40450,#40451,#40452,#40453,#40454,#40455,
#40456,#40457,#40458,#40459,#40460,#40461,#40462,#40463,#40464,#40465,#40466,
#40467,#40468,#40469,#40470,#40471,#40472,#40473,#40474,#40475,#40476,#40477,
#40478,#40479,#40480,#40481,#40482,#40483,#40484,#40485,#40486,#40487,#40488,
#40489,#40490,#40491,#40492,#40493,#40494,#40495,#40496,#40497,#40498,#40499,
#40500,#40501,#40502,#40503,#40504,#40505,#40506,#40507,#40508,#40509,#40510,
#40511,#40512,#40513,#40514,#40515,#40516,#40517,#40518,#40519,#40520,#40521,
#40522,#40523,#40524,#40525,#40526,#40527,#40528,#40529,#40530,#40531,#40532,
#40533,#40534,#40535,#40536,#40537,#40538,#40539,#40540,#40541,#40542,#40543,
#40544,#40545,#40546,#40547,#40548,#40549,#40550,#40551,#40552,#40553,#40554,
#40555,#40556,#40557,#40558,#40559,#40560,#40561,#40562,#40563,#40564,#40565,
#40566,#40567,#40568,#40569,#40570,#40571,#40572,#40573,#40574,#40575,#40576,
#40577,#40578,#40579,#40580,#40581,#40582,#40583,#40584,#40585,#40586,#40587,
#40588,#40589,#40590,#40591,#40592,#40593,#40594,#40595,#40596,#40597,#40598,
#40599,#40600,#40601,#40602,#40603,#40604,#40605,#40606,#40607,#40608,#40609,
#40610,#40611,#40612,#40613,#40614,#40615,#40616,#40617,#40618,#40619,#40620,
#40621,#40622,#40623,#40624,#40625,#40626,#40627,#40628,#40629,#40630,#40631,
#40632,#40633,#40634,#40635,#40636,#40637,#40638,#40639,#40640,#40641,#40642,
#40643,#40644,#40645,#40646,#40647,#40648,#40649,#40650,#40651,#40652,#40653,
#40654,#40655,#40656,#40657,#40658,#40659,#40660,#40661,#40662,#40663,#40664,
#40665,#40666,#40667,#40668,#40669,#40670,#40671,#40672,#40673,#40674,#40675,
#40676,#40677,#40678,#40679,#40680,#40681,#40682,#40683,#40684,#40685,#40686,
#40687,#40688,#40689,#40690,#40691,#40692,#40693,#40694,#40695,#40696,#40697,
#40698,#40699,#40700,#40701,#40702,#40703,#40704,#40705,#40706,#40707,#40708,
#40709,#40710,#40711,#40712,#40713,#40714,#40715,#40716,#40717,#40718,#40719,
#40720,#40721,#40722,#40723,#40724,#40725,#40726,#40727,#40728,#40729,#40730,
#40731,#40732,#40733,#40734,#40735,#40736,#40737,#40738,#40739,#40740,#40741,
#40742,#40743,#40744,#40745,#40746,#40747,#40748,#40749,#40750,#40751,#40752,
#40753,#40754,#40755,#40756,#40757,#40758,#40759,#40760,#40761,#40762,#40763,
#40764,#40765,#40766,#40767,#40768),.UNSPECIFIED.,.F.,.F.,(4,2,2,2,2,2,
2,2,2,2,2,2,2,2,2,2,2,2,2,2,2,2,2,2,2,2,2,2,2,2,2,2,2,2,2,2,2,2,2,2,2,2,
2,2,2,2,2,2,2,2,2,2,2,2,2,2,2,2,2,2,2,2,2,2,2,2,2,2,2,2,2,2,2,2,2,2,2,2,
2,2,2,2,2,2,2,2,2,2,2,2,2,2,2,2,2,2,2,2,2,2,2,2,2,2,2,2,2,2,2,2,2,2,2,2,
2,2,2,2,2,2,2,2,2,2,2,2,2,2,2,2,2,2,2,2,2,2,2,2,2,2,2,2,2,2,2,2,2,2,2,2,
2,2,2,2,2,2,2,2,2,2,2,2,2,2,2,2,2,2,2,2,2,2,2,2,2,2,2,2,2,2,2,2,2,2,2,2,
2,2,2,2,2,2,2,2,2,2,2,2,2,2,2,2,2,2,2,2,2,2,2,2,2,2,2,2,2,2,2,2,2,2,2,2,
2,2,2,2,2,2,2,2,2,2,2,2,2,2,2,2,2,2,2,2,2,2,2,2,2,2,2,2,2,2,2,2,2,2,2,2,
2,2,2,2,2,2,2,2,2,2,4),(-4.06107074159402,-4.05792311628498,-4.05505650757302,
-4.05370667619582,-4.05259411403693,-4.05153489084243,-4.05017190820217,
-4.04784210490371,-4.0400948612384,-3.93199530309746,-3.89746054387593,
-3.89273812527517,-3.89149306368082,-3.89075369604527,-3.89009553725701,
-3.88925327460879,-3.88758250956353,-3.87752097976065,-3.8329010998466,
-3.74206956993004,-3.73625782372181,-3.73340214139118,-3.73169003707714,
-3.7301406158905,-3.72897086964434,-3.72785500279065,-3.72631964798947,
-3.72242931441017,-3.66334154064967,-3.63357801875161,-3.6095968340008,
-3.57480694936298,-3.57167926388291,-3.56941789073379,-3.5684776896975,
-3.56780428551313,-3.56718881993942,-3.56635535935952,-3.56472954220267,
-3.55220740780105,-3.45124318580869,-3.42216011295069,-3.41476286397144,
-3.41134991418941,-3.40940977234448,-3.40769653027833,-3.40649592577635,
-3.40530301910232,-3.40384782014859,-3.40034032993913,-3.36812601629823,
-3.30885430922902,-3.29670936875526,-3.28408722341385,-3.25190585175597,
-3.24736375079728,-3.24613568924646,-3.2454002408586,-3.24474149748169,
-3.24389296294816,-3.2421325801564,-3.23064271199369,-3.22889460598271,
-3.13766056856445,-3.11518768505876,-3.0978575536199,-3.09144417073204,
-3.08837338372757,-3.08657262658688,-3.08496109143267,-3.08422957136854,
-3.08307422431332,-3.08157287593419,-3.07862660602756,-3.06147774582934,
-2.96760109378171,-2.9263314851616,-2.92405188672545,-2.92310866049859,
-2.92243472855039,-2.92181996208877,-2.92098912924519,-2.91937337264755,
-2.90711995962076,-2.90383673018631,-2.90348884890933,-2.90216993680237,
-2.82659539722198,-2.77308276103603,-2.76783062472699,-2.76517994034335,
-2.76355330198508,-2.76206548727548,-2.76090529718656,-2.75976937624903,
-2.75815870001489,-2.75380551969949,-2.68523113948357,-2.63071785528902,
-2.61158196328927,-2.6025657961901,-2.60104678115628,-2.60024761945674,
-2.59959910054777,-2.59893265756538,-2.59768278639568,-2.59345855794327,
-2.51561258175736,-2.44455929077339,-2.44110104609599,-2.43951967186602,
-2.43832853823853,-2.4372088878825,-2.43535300003718,-2.430606158018,-2.35644157996629,
-2.32154146527208,-2.29147218849282,-2.28006957227897,-2.27845833559954,
-2.27763991479335,-2.27698416316504,-2.27622954893315,-2.27494905409372,
-2.27030910629864,-2.17460824598838,-2.12176670714617,-2.11838631518486,
-2.11681970664643,-2.11563093859031,-2.11450702992522,-2.11262875425422,
-2.10774354659412,-2.03074199268243,-1.96056778899028,-1.95664786367709,
-1.95543405589394,-1.95477490662266,-1.95411945766315,-1.95330516073203,
-1.95171383258012,-1.94088853168741,-1.91348114940625,-1.83555327327358,
-1.81902461912921,-1.81385186794283,-1.79837384614871,-1.79577411452154,
-1.794220875633,-1.79302995314925,-1.79175579531467,-1.78976187043001,-1.78356863919322,
-1.74862592498321,-1.6481671615945,-1.63500535769052,-1.63319747792301,
-1.6323359560139,-1.63167340033351,-1.63095187098498,-1.62978622831091,
-1.62585952717989,-1.60077650712587,-1.55311615216838,-1.47805206329176,
-1.47362265767696,-1.47200005079682,-1.47086079708855,-1.46979624400581,
-1.46833410814099,-1.46548062513414,-1.44596870537084,-1.42667819134169,
-1.3293843991285,-1.32837123575537,-1.32705135095524,-1.31236557973351,
-1.31066505810144,-1.30981248943284,-1.30919204807235,-1.30853602327453,
-1.30764469821822,-1.30664796874454,-1.30494874151072,-1.25941885562339,
-1.17012498809876,-1.15299958690595,-1.15005397843829,-1.14855252708944,
-1.14737217627416,-1.14605991459967,-1.14389624544586,-1.13616262978701,
-1.11110702888269,-1.06866311766076,-1.00288118907866,-1.00077557592566,
-0.989457363641942,-0.98770449530953,-0.986857327793933,-0.986213632432669,
-0.985540233875388,-0.984414129577513,-0.983082568101587,-0.980531701875951,
-0.895536280521014,-0.831804152416426,-0.827898274939483,-0.826360288186352,
-0.825243730393034,-0.824050491819685,-0.822457069219483,-0.81893511095283,
-0.768863694892824,-0.757168978242177,-0.670295445749342,-0.665869313808614,
-0.664596510676812,-0.663850925036437,-0.663206762745967,-0.662398481959153,
-0.661517129204842,-0.660097023996654,-0.657309889348625,-0.650329849046117,
-0.635813018063733,-0.61119151185388,-0.536618651195705,-0.508303071883821,
-0.504862921997067,-0.503301738897064,-0.502109205807514,-0.50083767116124,
-0.498856820316133,-0.492773497165741,-0.3994197498584,-0.385142560644,
-0.360855134446266,-0.34424935647815,-0.342491366236673,-0.341624353986918,
-0.34100008658254,-0.340346422548127,-0.33945549313304,-0.338471074793271,
-0.336801977663959,-0.333325827066347,-0.323885484307112,-0.300378522497625,
-0.214977475826035,-0.185568068886635,-0.182441649627592,-0.180891475629612,
-0.179771626636407,-0.178580041525473,-0.17699766082912,-0.173535592333841,
-0.101309985512579,-0.0368048490202745,-0.0326796191665078,-0.0212083070452828,
-0.0194483451149031,-0.0185997227515182,-0.0179648019798001,-0.0173504645605992,
-0.0166340895606322,-0.0156094238509372,-0.0138416644030553,-0.0009566108525659),
 .UNSPECIFIED.);
#820=B_SPLINE_CURVE_WITH_KNOTS('',3,(#40770,#40771,#40772,#40773,#40774,
#40775,#40776,#40777,#40778,#40779,#40780,#40781,#40782,#40783,#40784,#40785,
#40786,#40787,#40788,#40789,#40790,#40791,#40792,#40793,#40794,#40795,#40796,
#40797,#40798,#40799,#40800,#40801,#40802,#40803,#40804,#40805,#40806,#40807,
#40808,#40809,#40810,#40811,#40812,#40813,#40814,#40815,#40816,#40817,#40818,
#40819,#40820,#40821,#40822,#40823,#40824,#40825,#40826,#40827,#40828,#40829,
#40830,#40831,#40832,#40833,#40834,#40835,#40836,#40837,#40838,#40839,#40840,
#40841,#40842,#40843,#40844,#40845,#40846,#40847,#40848,#40849,#40850,#40851,
#40852,#40853,#40854,#40855,#40856,#40857,#40858,#40859,#40860,#40861,#40862,
#40863,#40864,#40865,#40866,#40867,#40868,#40869,#40870,#40871,#40872,#40873,
#40874,#40875,#40876,#40877,#40878,#40879,#40880,#40881,#40882,#40883,#40884,
#40885,#40886,#40887,#40888,#40889,#40890,#40891,#40892,#40893,#40894,#40895,
#40896,#40897,#40898,#40899,#40900,#40901,#40902,#40903,#40904,#40905,#40906,
#40907,#40908,#40909,#40910,#40911,#40912,#40913,#40914,#40915,#40916,#40917,
#40918,#40919,#40920,#40921,#40922,#40923,#40924,#40925,#40926,#40927,#40928,
#40929,#40930,#40931,#40932,#40933,#40934,#40935,#40936,#40937,#40938,#40939,
#40940,#40941,#40942,#40943,#40944,#40945,#40946,#40947,#40948,#40949,#40950,
#40951,#40952,#40953,#40954,#40955,#40956,#40957,#40958,#40959,#40960,#40961,
#40962,#40963,#40964,#40965,#40966,#40967,#40968,#40969,#40970,#40971,#40972,
#40973,#40974,#40975,#40976,#40977,#40978,#40979,#40980,#40981,#40982,#40983,
#40984,#40985,#40986,#40987,#40988,#40989,#40990,#40991,#40992,#40993,#40994,
#40995,#40996,#40997,#40998,#40999,#41000,#41001,#41002,#41003,#41004,#41005,
#41006,#41007,#41008,#41009,#41010,#41011,#41012,#41013,#41014,#41015,#41016,
#41017,#41018,#41019,#41020,#41021,#41022,#41023,#41024,#41025,#41026,#41027,
#41028,#41029,#41030,#41031,#41032,#41033,#41034,#41035,#41036,#41037,#41038,
#41039,#41040,#41041,#41042,#41043,#41044,#41045,#41046,#41047,#41048,#41049,
#41050,#41051,#41052,#41053,#41054,#41055,#41056,#41057,#41058,#41059,#41060,
#41061,#41062,#41063,#41064,#41065,#41066,#41067,#41068,#41069,#41070,#41071,
#41072,#41073,#41074,#41075,#41076,#41077,#41078,#41079,#41080,#41081,#41082,
#41083,#41084,#41085,#41086,#41087,#41088,#41089,#41090,#41091,#41092,#41093,
#41094,#41095,#41096,#41097,#41098,#41099,#41100,#41101,#41102,#41103,#41104,
#41105,#41106,#41107,#41108,#41109,#41110,#41111,#41112,#41113,#41114,#41115,
#41116,#41117,#41118,#41119,#41120,#41121,#41122,#41123,#41124,#41125,#41126,
#41127,#41128,#41129,#41130,#41131,#41132,#41133,#41134,#41135,#41136,#41137,
#41138,#41139,#41140,#41141,#41142,#41143,#41144,#41145,#41146,#41147,#41148,
#41149,#41150,#41151,#41152,#41153,#41154,#41155,#41156,#41157,#41158,#41159,
#41160,#41161,#41162,#41163,#41164,#41165,#41166,#41167,#41168,#41169,#41170,
#41171,#41172,#41173,#41174,#41175,#41176,#41177,#41178,#41179,#41180,#41181,
#41182,#41183,#41184,#41185,#41186,#41187,#41188,#41189,#41190,#41191,#41192,
#41193,#41194,#41195,#41196,#41197,#41198,#41199,#41200,#41201,#41202,#41203,
#41204,#41205,#41206,#41207,#41208,#41209,#41210,#41211,#41212,#41213,#41214,
#41215,#41216,#41217,#41218,#41219,#41220,#41221,#41222,#41223,#41224,#41225,
#41226,#41227,#41228,#41229,#41230,#41231,#41232,#41233,#41234,#41235,#41236,
#41237,#41238,#41239,#41240,#41241,#41242,#41243,#41244,#41245,#41246,#41247,
#41248,#41249,#41250,#41251,#41252,#41253,#41254,#41255,#41256,#41257,#41258,
#41259,#41260,#41261,#41262,#41263,#41264,#41265,#41266,#41267,#41268,#41269,
#41270,#41271,#41272,#41273,#41274,#41275,#41276,#41277,#41278,#41279,#41280,
#41281,#41282,#41283,#41284,#41285,#41286,#41287,#41288,#41289,#41290,#41291,
#41292,#41293,#41294,#41295,#41296,#41297,#41298,#41299,#41300,#41301,#41302,
#41303,#41304,#41305,#41306,#41307,#41308,#41309,#41310,#41311,#41312,#41313),
 .UNSPECIFIED.,.F.,.F.,(4,2,2,2,2,2,2,2,2,2,2,2,2,2,2,2,2,2,2,2,2,2,2,2,
2,2,2,2,2,2,2,2,2,2,2,2,2,2,2,2,2,2,2,2,2,2,2,2,2,2,2,2,2,2,2,2,2,2,2,2,
2,2,2,2,2,2,2,2,2,2,2,2,2,2,2,2,2,2,2,2,2,2,2,2,2,2,2,2,2,2,2,2,2,2,2,2,
2,2,2,2,2,2,2,2,2,2,2,2,2,2,2,2,2,2,2,2,2,2,2,2,2,2,2,2,2,2,2,2,2,2,2,2,
2,2,2,2,2,2,2,2,2,2,2,2,2,2,2,2,2,2,2,2,2,2,2,2,2,2,2,2,2,2,2,2,2,2,2,2,
2,2,2,2,2,2,2,2,2,2,2,2,2,2,2,2,2,2,2,2,2,2,2,2,2,2,2,2,2,2,2,2,2,2,2,2,
2,2,2,2,2,2,2,2,2,2,2,2,2,2,2,2,2,2,2,2,2,2,2,2,2,2,2,2,2,2,2,2,2,2,2,2,
2,2,2,2,2,2,2,2,2,2,2,2,2,2,2,2,2,2,2,2,2,2,2,2,2,2,2,2,2,2,2,4),(-4.05989992915858,
-3.97542443936791,-3.93765455717652,-3.92075434847969,-3.91800229329291,
-3.91656200837748,-3.91550079003599,-3.9143529952597,-3.91269759599141,
-3.90804737278844,-3.90631984662432,-3.80199691578861,-3.77276469656581,
-3.7624611628741,-3.75875738490944,-3.75700914207113,-3.75599266351523,
-3.75508712065577,-3.75442878185482,-3.75381229442994,-3.75297385899741,
-3.7509052150137,-3.72808158417878,-3.70106738734646,-3.67010396306551,
-3.59933306399446,-3.59587696631157,-3.59429641058669,-3.59310582598412,
-3.59198664222436,-3.59043695264855,-3.58731013996494,-3.55781949030078,
-3.50926534502195,-3.46260451063372,-3.44410441135709,-3.43797090977061,
-3.43543693431227,-3.43411204714131,-3.4329901408467,-3.43228475338396,
-3.43163940778628,-3.43078546161704,-3.42894856062762,-3.4156186331254,
-3.41336492226598,-3.37186293663109,-3.32767837629357,-3.27709402895805,
-3.27357159087048,-3.27197866744232,-3.27078609390776,-3.26967036873029,
-3.26813385911199,-3.26423347986733,-3.20212173215203,-3.1178012262114,
-3.11400200536771,-3.11222071053332,-3.11119076549668,-3.11027612591858,
-3.10961580166741,-3.10900141840892,-3.10817148144552,-3.10655857385836,
-3.09435390097841,-3.02852226239184,-2.98547801671621,-2.9598898293343,
-2.95489291930771,-2.95116798346484,-2.94953809268848,-2.94833916501601,
-2.94723261366667,-2.94573197376895,-2.94279891321758,-2.91963642512135,
-2.90924047069381,-2.82808197429416,-2.80811523523283,-2.79203145273174,
-2.79001350443487,-2.78888858665651,-2.78813101468013,-2.7874106617429,
-2.78676854826433,-2.78592895750131,-2.78421292656896,-2.77365769947996,
-2.70263332844547,-2.66325605466512,-2.63750362485612,-2.62983551501849,
-2.62767905344853,-2.6263688005181,-2.62518873038106,-2.62368554267905,
-2.6207299201731,-2.60339672062262,-2.59988350424946,-2.50659162148337,
-2.47160765921039,-2.46847128889202,-2.46620507044399,-2.46526420928015,
-2.46459082196739,-2.46397572556954,-2.46314326925843,-2.46152089551297,
-2.44908318904217,-2.44798724320224,-2.44719932912115,-2.35930037503475,
-2.31433114387829,-2.30956342873598,-2.30597627554167,-2.30437120860514,
-2.30317641546634,-2.30206356321773,-2.30053872793626,-2.29670827133356,
-2.24497720441269,-2.18356750964765,-2.15778809962833,-2.14500176960697,
-2.14334811708189,-2.14252109110296,-2.14192678431162,-2.14128980403439,
-2.14018583739283,-2.13709092590166,-2.08189503917666,-2.03127542672754,
-2.01340219610737,-2.00541130457527,-1.98633703691398,-1.98325594197837,
-1.98174770766263,-1.98056696349491,-1.97925933553833,-1.97711489369088,
-1.96956686947523,-1.94404662555513,-1.90115540616016,-1.82611898482838,
-1.82183424126883,-1.82057758765004,-1.81990984550191,-1.81926152612959,
-1.81846469480406,-1.81695630714273,-1.80816910186986,-1.78937795610727,
-1.74357943140737,-1.66624566491097,-1.6615519351191,-1.65988960276889,
-1.65873956150045,-1.65767825263551,-1.65624084775174,-1.65350433614937,
-1.63699137157467,-1.60130056304688,-1.50365757092414,-1.49921723976541,
-1.49794307209154,-1.49719730067033,-1.4966061252213,-1.49580660541988,
-1.49428589520743,-1.48523174864873,-1.46608681513765,-1.41865485452393,
-1.34325277039749,-1.33879352171768,-1.33716642457734,-1.33602601164056,
-1.3348673659768,-1.33339313369555,-1.33178343321872,-1.32917319361608,
-1.32402987412637,-1.27256836805075,-1.18764356064116,-1.17730115115038,
-1.17559538295946,-1.17475765623421,-1.17410006170739,-1.17335811896915,
-1.17210128045753,-1.16724715466541,-1.14410806064156,-1.09852152421232,
-1.06305474521822,-1.01959415314777,-1.01587383840937,-1.01436765133685,
-1.01325933700123,-1.01208498608285,-1.01050489176729,-1.0087524102339,
-1.00579911276715,-0.999716081230722,-0.909180692343531,-0.86463435908407,
-0.854630615426017,-0.852962805667472,-0.852121178630782,-0.851463096720103,
-0.850723363950881,-0.849476650676588,-0.844736036962455,-0.809959015231754,
-0.716801035759007,-0.713222103223423,-0.695616152401385,-0.692645460919935,
-0.691138689759898,-0.689957793804983,-0.688674980095775,-0.686599911262268,
-0.684141212044954,-0.679401829828679,-0.667887674497593,-0.645236433402913,
-0.542631233300566,-0.531856118149043,-0.530128443210877,-0.529286221068031,
-0.528628009626192,-0.527888490519846,-0.526642964388592,-0.521916366951134,
-0.487334555192299,-0.477630447403251,-0.469693261699333,-0.462940795973436,
-0.404264453894064,-0.398833268763276,-0.393157078777552,-0.373071154468099,
-0.369941760184237,-0.368423412135481,-0.367240874792499,-0.366139496366874,
-0.364248863128718,-0.358827964164018,-0.350763826460689,-0.327132169738837,
-0.305848227375618,-0.222471394104182,-0.209343778077339,-0.20753681575816,
-0.206675320794779,-0.206012599221801,-0.205290695751057,-0.204124040741387,
-0.200190203975901,-0.175036332214692,-0.0902231898238672,-0.0835047851764577,
-0.0757971263120287,-0.0702444836189663,-0.0502993545465698,-0.047176311950564,
-0.0456591956395599,-0.0444767807691945,-0.0433753113320354,-0.042096307549911,
-0.0402758606323557,-0.0371576634159707,-0.000956516702297368),
 .UNSPECIFIED.);
#821=B_SPLINE_CURVE_WITH_KNOTS('',3,(#41315,#41316,#41317,#41318,#41319,
#41320,#41321,#41322,#41323,#41324,#41325,#41326,#41327,#41328,#41329,#41330,
#41331,#41332,#41333,#41334,#41335,#41336,#41337,#41338,#41339,#41340,#41341,
#41342,#41343,#41344,#41345,#41346,#41347,#41348,#41349,#41350,#41351,#41352,
#41353,#41354,#41355,#41356,#41357,#41358,#41359,#41360,#41361,#41362,#41363,
#41364,#41365,#41366,#41367,#41368,#41369,#41370,#41371,#41372,#41373,#41374,
#41375,#41376,#41377,#41378,#41379,#41380,#41381,#41382,#41383,#41384,#41385,
#41386,#41387,#41388,#41389,#41390,#41391,#41392,#41393,#41394,#41395,#41396,
#41397,#41398,#41399,#41400,#41401,#41402,#41403,#41404,#41405,#41406,#41407,
#41408,#41409,#41410,#41411,#41412,#41413,#41414,#41415,#41416,#41417,#41418,
#41419,#41420,#41421,#41422,#41423,#41424,#41425,#41426,#41427,#41428,#41429,
#41430,#41431,#41432,#41433,#41434,#41435,#41436,#41437,#41438,#41439,#41440,
#41441,#41442,#41443,#41444,#41445,#41446,#41447,#41448,#41449,#41450,#41451,
#41452,#41453,#41454,#41455,#41456,#41457,#41458,#41459,#41460,#41461,#41462,
#41463,#41464,#41465,#41466,#41467,#41468,#41469,#41470,#41471,#41472,#41473,
#41474,#41475,#41476,#41477,#41478,#41479,#41480,#41481,#41482,#41483,#41484,
#41485,#41486,#41487,#41488,#41489,#41490,#41491,#41492,#41493,#41494,#41495,
#41496,#41497,#41498,#41499,#41500,#41501,#41502,#41503,#41504,#41505,#41506,
#41507,#41508,#41509,#41510,#41511,#41512,#41513,#41514,#41515,#41516,#41517,
#41518,#41519,#41520,#41521,#41522,#41523,#41524,#41525,#41526,#41527,#41528,
#41529,#41530,#41531,#41532,#41533,#41534,#41535,#41536,#41537,#41538,#41539,
#41540,#41541,#41542,#41543,#41544,#41545,#41546,#41547,#41548,#41549,#41550,
#41551,#41552,#41553,#41554,#41555,#41556,#41557,#41558,#41559,#41560,#41561,
#41562,#41563,#41564,#41565,#41566,#41567,#41568,#41569,#41570,#41571,#41572,
#41573,#41574,#41575,#41576,#41577,#41578,#41579,#41580,#41581,#41582,#41583,
#41584,#41585,#41586,#41587,#41588,#41589,#41590,#41591,#41592,#41593,#41594,
#41595,#41596,#41597,#41598,#41599,#41600,#41601,#41602,#41603,#41604,#41605,
#41606,#41607,#41608,#41609,#41610,#41611,#41612,#41613,#41614,#41615,#41616,
#41617,#41618,#41619,#41620,#41621,#41622,#41623,#41624,#41625,#41626,#41627,
#41628,#41629,#41630,#41631,#41632,#41633,#41634,#41635,#41636,#41637,#41638,
#41639,#41640,#41641,#41642,#41643,#41644,#41645,#41646,#41647,#41648,#41649,
#41650,#41651,#41652,#41653,#41654,#41655,#41656,#41657,#41658,#41659,#41660,
#41661,#41662,#41663,#41664,#41665,#41666,#41667,#41668,#41669,#41670,#41671,
#41672,#41673,#41674,#41675,#41676,#41677,#41678,#41679,#41680,#41681,#41682,
#41683,#41684,#41685,#41686,#41687,#41688,#41689,#41690,#41691,#41692,#41693,
#41694,#41695,#41696,#41697,#41698,#41699,#41700,#41701,#41702,#41703,#41704,
#41705,#41706,#41707,#41708,#41709,#41710,#41711,#41712,#41713,#41714,#41715,
#41716,#41717,#41718,#41719,#41720,#41721,#41722,#41723,#41724,#41725,#41726,
#41727,#41728,#41729,#41730,#41731,#41732,#41733,#41734,#41735,#41736,#41737,
#41738,#41739,#41740,#41741,#41742,#41743,#41744,#41745,#41746,#41747,#41748,
#41749,#41750,#41751,#41752,#41753,#41754,#41755,#41756,#41757,#41758,#41759,
#41760,#41761,#41762,#41763,#41764,#41765,#41766,#41767,#41768,#41769,#41770,
#41771,#41772,#41773,#41774,#41775,#41776,#41777,#41778,#41779,#41780,#41781,
#41782,#41783,#41784,#41785,#41786,#41787,#41788,#41789,#41790,#41791,#41792,
#41793,#41794,#41795,#41796,#41797,#41798,#41799,#41800,#41801,#41802,#41803,
#41804,#41805,#41806,#41807,#41808,#41809,#41810,#41811,#41812,#41813,#41814,
#41815,#41816,#41817,#41818,#41819,#41820,#41821,#41822,#41823,#41824,#41825,
#41826,#41827,#41828,#41829,#41830,#41831,#41832,#41833,#41834,#41835,#41836,
#41837,#41838,#41839,#41840,#41841,#41842,#41843,#41844,#41845,#41846,#41847,
#41848,#41849,#41850,#41851,#41852,#41853,#41854,#41855,#41856,#41857,#41858,
#41859,#41860,#41861,#41862),.UNSPECIFIED.,.F.,.F.,(4,2,2,2,2,2,2,2,2,2,
2,2,2,2,2,2,2,2,2,2,2,2,2,2,2,2,2,2,2,2,2,2,2,2,2,2,2,2,2,2,2,2,2,2,2,2,
2,2,2,2,2,2,2,2,2,2,2,2,2,2,2,2,2,2,2,2,2,2,2,2,2,2,2,2,2,2,2,2,2,2,2,2,
2,2,2,2,2,2,2,2,2,2,2,2,2,2,2,2,2,2,2,2,2,2,2,2,2,2,2,2,2,2,2,2,2,2,2,2,
2,2,2,2,2,2,2,2,2,2,2,2,2,2,2,2,2,2,2,2,2,2,2,2,2,2,2,2,2,2,2,2,2,2,2,2,
2,2,2,2,2,2,2,2,2,2,2,2,2,2,2,2,2,2,2,2,2,2,2,2,2,2,2,2,2,2,2,2,2,2,2,2,
2,2,2,2,2,2,2,2,2,2,2,2,2,2,2,2,2,2,2,2,2,2,2,2,2,2,2,2,2,2,2,2,2,2,2,2,
2,2,2,2,2,2,2,2,2,2,2,2,2,2,2,2,2,2,2,2,2,2,2,2,2,2,2,2,2,2,2,2,2,2,2,2,
2,2,2,2,2,2,2,2,2,2,2,4),(-4.06041562041457,-3.97343373173595,-3.95442637936347,
-3.94552365114943,-3.9440094887776,-3.943211233984,-3.94262004933636,-3.9418730039183,
-3.94059365560091,-3.93610794809912,-3.83922561225848,-3.82378937695582,
-3.79883945183429,-3.7904400024817,-3.78484711605959,-3.78293070092868,
-3.78182868750865,-3.78064830464436,-3.77914651357275,-3.77619929512866,
-3.75904312305322,-3.75541945648697,-3.7453832706041,-3.69732964688064,
-3.65701679974696,-3.62669353702674,-3.62230232341125,-3.6210886746521,
-3.62035636985202,-3.61969677087007,-3.61885619033214,-3.61709054005959,
-3.60548840513624,-3.51441887903404,-3.48000390925606,-3.46927265032198,
-3.46477437144957,-3.46240747593738,-3.46046666904196,-3.45918231783831,
-3.45800178343789,-3.45649788911251,-3.45354051305316,-3.43618873919216,
-3.43267368496004,-3.34938925944133,-3.30125482638702,-3.29899089305309,
-3.29805022928541,-3.29737671144118,-3.29676129938635,-3.29592813578425,
-3.29430355912873,-3.28181680640983,-3.28075703227766,-3.28037076031094,
-3.18055889701578,-3.1513675222654,-3.144181290362,-3.14084068950504,-3.13817341164928,
-3.13675796465361,-3.13559024372659,-3.13424376827514,-3.13198473102816,
-3.12403044560653,-3.12208368966232,-3.11903957250021,-3.11780884970613,
-3.11727654513758,-3.01779313833982,-2.9816575315634,-2.97682098244964,
-2.97556562844794,-2.97482397204346,-2.97416624943387,-2.97332785229426,
-2.97161898594325,-2.96121786679749,-2.87640807894311,-2.82493709196789,
-2.81979239873427,-2.81718149568649,-2.81557142903982,-2.81409538474537,
-2.81293664330545,-2.8117957851141,-2.81016745872443,-2.80570115155815,
-2.73039280987081,-2.68284351026427,-2.66372927624845,-2.65459362421853,
-2.65306911543051,-2.65226871850029,-2.65167737901053,-2.65093204250992,
-2.64966014263574,-2.64524146220511,-2.54740940156743,-2.49724161640787,
-2.49328380176823,-2.49161267734301,-2.49040592455061,-2.48930763870141,
-2.48784130693746,-2.48427092634136,-2.44953359574334,-2.38894156324582,
-2.33479000225473,-2.33116065888664,-2.3300285409666,-2.32931451650866,
-2.32864927141295,-2.32777089134027,-2.32580450750855,-2.30871097218493,
-2.30795433433687,-2.21148500795778,-2.17740349962264,-2.17130406700221,
-2.16932155794159,-2.16804987991084,-2.16685786560042,-2.16529830206433,
-2.16186555155248,-2.13376380973773,-2.04300015957484,-2.03018259416502,
-2.02902064859929,-2.02623546315635,-2.02351236954705,-2.02312326527646,
-2.0220348670207,-2.00958164150667,-2.00795839386974,-2.00712560524734,
-2.00651031913182,-2.00583678158825,-2.00489581178174,-2.00262981289646,
-1.94255157521496,-1.8753141094043,-1.86999915480501,-1.85061091931076,
-1.84751433983441,-1.84600275672387,-1.84482132092562,-1.84351489979493,
-1.84137691708646,-1.83389596665621,-1.78621390301534,-1.69046509587776,
-1.68598186903667,-1.6847028005894,-1.68395582202063,-1.68336463433024,
-1.68256630618228,-1.68105177716823,-1.67214069206191,-1.65312563544515,
-1.60618808240319,-1.55857587910291,-1.54870089229428,-1.54513009798313,
-1.5277634439923,-1.5248048741991,-1.52330055441126,-1.52211977532819,-1.52080892043176,
-1.51865189280043,-1.51098608940735,-1.4852261079304,-1.44182071639483,
-1.37969492070576,-1.36443061245622,-1.36252200274486,-1.36165416321048,
-1.36099052740503,-1.36027170789321,-1.3591416760238,-1.35551061089498,
-1.33334748547279,-1.29921277754502,-1.21616519692179,-1.20973743340778,
-1.20347601002975,-1.20139492324095,-1.20023046698983,-1.19917136678551,
-1.19775983746112,-1.19519860151676,-1.18207388930441,-1.15628747752221,
-1.0798590212369,-1.06037940120976,-1.05897140949891,-1.04182132728312,
-1.03985296054016,-1.03897411040627,-1.0383086791725,-1.03759462594159,
-1.03648553617086,-1.0330470238798,-1.01276700576541,-0.978282491595887,
-0.926031259196154,-0.907175992822879,-0.901971993996287,-0.882629988255019,
-0.879535055799057,-0.878023586020754,-0.876841923804009,-0.875534930454254,
-0.873395281027855,-0.866062899257342,-0.845347959064553,-0.822499607975562,
-0.767714687448652,-0.720346744892809,-0.717637366356654,-0.716697317367491,
-0.716053055579729,-0.7154603749953,-0.714648315348204,-0.713100295116653,
-0.703295363356361,-0.681328181737579,-0.631702109315803,-0.562038965925123,
-0.557622006226427,-0.556001113337803,-0.554862175966818,-0.553797212589503,
-0.552333416039696,-0.550767739263672,-0.543513221464304,-0.510480090555925,
-0.457090986234711,-0.413789226998515,-0.396595588845203,-0.394625226119335,
-0.393746006282068,-0.393080507627494,-0.392366596534047,-0.391634700669151,
-0.390572149836311,-0.38230141922074,-0.36477321204531,-0.339801867883332,
-0.316013676478843,-0.267491300050972,-0.237991136785178,-0.2348621134535,
-0.233311232442798,-0.232191145826705,-0.230999561446941,-0.229417613474607,
-0.227688461671877,-0.224791860166281,-0.206410607915776,-0.167801940267825,
-0.153709455984689,-0.139205909096901,-0.0764075034383618,-0.0727010087366635,
-0.0715135301317433,-0.0708595309664283,-0.0702092879277642,-0.0693876372283512,
-0.0685038164500342,-0.0670778526692987,-0.0642749993481048,-0.00095719944665948),
 .UNSPECIFIED.);
#822=B_SPLINE_CURVE_WITH_KNOTS('',3,(#41864,#41865,#41866,#41867,#41868,
#41869,#41870,#41871,#41872,#41873,#41874,#41875,#41876,#41877,#41878,#41879,
#41880,#41881,#41882,#41883,#41884,#41885,#41886,#41887,#41888,#41889,#41890,
#41891,#41892,#41893,#41894,#41895,#41896,#41897,#41898,#41899,#41900,#41901,
#41902,#41903,#41904,#41905,#41906,#41907,#41908,#41909,#41910,#41911,#41912,
#41913,#41914,#41915,#41916,#41917,#41918,#41919,#41920,#41921,#41922,#41923,
#41924,#41925,#41926,#41927,#41928,#41929,#41930,#41931,#41932,#41933,#41934,
#41935,#41936,#41937,#41938,#41939,#41940,#41941,#41942,#41943,#41944,#41945,
#41946,#41947,#41948,#41949,#41950,#41951,#41952,#41953,#41954,#41955,#41956,
#41957,#41958,#41959,#41960,#41961,#41962,#41963,#41964,#41965,#41966,#41967,
#41968,#41969,#41970,#41971,#41972,#41973,#41974,#41975,#41976,#41977,#41978,
#41979,#41980,#41981,#41982,#41983,#41984,#41985,#41986,#41987,#41988,#41989,
#41990,#41991,#41992,#41993,#41994,#41995,#41996,#41997,#41998,#41999,#42000,
#42001,#42002,#42003,#42004,#42005,#42006,#42007,#42008,#42009,#42010,#42011,
#42012,#42013,#42014,#42015,#42016,#42017,#42018,#42019,#42020,#42021,#42022,
#42023,#42024,#42025,#42026,#42027,#42028,#42029,#42030,#42031,#42032,#42033,
#42034,#42035,#42036,#42037,#42038,#42039,#42040,#42041,#42042,#42043,#42044,
#42045,#42046,#42047,#42048,#42049,#42050,#42051,#42052,#42053,#42054,#42055,
#42056,#42057,#42058,#42059,#42060,#42061,#42062,#42063,#42064,#42065,#42066,
#42067,#42068,#42069,#42070,#42071,#42072,#42073,#42074,#42075,#42076,#42077,
#42078,#42079,#42080,#42081,#42082,#42083,#42084,#42085,#42086,#42087,#42088,
#42089,#42090,#42091,#42092,#42093,#42094,#42095,#42096,#42097,#42098,#42099,
#42100,#42101,#42102,#42103,#42104,#42105,#42106,#42107,#42108,#42109,#42110,
#42111,#42112,#42113,#42114,#42115,#42116,#42117,#42118,#42119,#42120,#42121,
#42122,#42123,#42124,#42125,#42126,#42127,#42128,#42129,#42130,#42131,#42132,
#42133,#42134,#42135,#42136,#42137,#42138,#42139,#42140,#42141,#42142,#42143,
#42144,#42145,#42146,#42147,#42148,#42149,#42150,#42151,#42152,#42153,#42154,
#42155,#42156,#42157,#42158,#42159,#42160,#42161,#42162,#42163,#42164,#42165,
#42166,#42167,#42168,#42169,#42170,#42171,#42172,#42173,#42174,#42175,#42176,
#42177,#42178,#42179,#42180,#42181,#42182,#42183,#42184,#42185,#42186,#42187,
#42188,#42189,#42190,#42191,#42192,#42193,#42194,#42195,#42196,#42197,#42198,
#42199,#42200,#42201,#42202,#42203,#42204,#42205,#42206,#42207,#42208,#42209,
#42210,#42211,#42212,#42213,#42214,#42215,#42216,#42217,#42218,#42219,#42220,
#42221,#42222,#42223,#42224,#42225,#42226,#42227,#42228,#42229,#42230,#42231,
#42232,#42233,#42234,#42235,#42236,#42237,#42238,#42239,#42240,#42241,#42242,
#42243,#42244,#42245,#42246,#42247,#42248,#42249,#42250,#42251,#42252,#42253,
#42254,#42255,#42256,#42257,#42258,#42259,#42260,#42261,#42262,#42263,#42264,
#42265,#42266,#42267,#42268,#42269,#42270,#42271,#42272,#42273,#42274,#42275,
#42276,#42277,#42278,#42279,#42280,#42281,#42282,#42283,#42284,#42285,#42286,
#42287,#42288,#42289,#42290,#42291,#42292,#42293,#42294,#42295,#42296,#42297,
#42298,#42299,#42300,#42301,#42302,#42303,#42304,#42305,#42306,#42307,#42308,
#42309,#42310,#42311,#42312,#42313,#42314,#42315,#42316,#42317,#42318,#42319,
#42320,#42321,#42322,#42323,#42324,#42325,#42326,#42327,#42328,#42329,#42330,
#42331,#42332,#42333,#42334,#42335,#42336,#42337,#42338,#42339,#42340,#42341,
#42342,#42343,#42344,#42345,#42346,#42347,#42348,#42349,#42350,#42351,#42352,
#42353,#42354,#42355,#42356,#42357,#42358,#42359,#42360,#42361,#42362,#42363,
#42364,#42365,#42366,#42367,#42368,#42369,#42370,#42371,#42372,#42373,#42374,
#42375,#42376,#42377,#42378,#42379,#42380,#42381,#42382,#42383,#42384,#42385,
#42386,#42387,#42388,#42389,#42390,#42391,#42392,#42393,#42394,#42395,#42396,
#42397,#42398,#42399,#42400,#42401,#42402,#42403,#42404,#42405,#42406,#42407,
#42408,#42409,#42410,#42411,#42412,#42413),.UNSPECIFIED.,.F.,.F.,(4,2,2,
2,2,2,2,2,2,2,2,2,2,2,2,2,2,2,2,2,2,2,2,2,2,2,2,2,2,2,2,2,2,2,2,2,2,2,2,
2,2,2,2,2,2,2,2,2,2,2,2,2,2,2,2,2,2,2,2,2,2,2,2,2,2,2,2,2,2,2,2,2,2,2,2,
2,2,2,2,2,2,2,2,2,2,2,2,2,2,2,2,2,2,2,2,2,2,2,2,2,2,2,2,2,2,2,2,2,2,2,2,
2,2,2,2,2,2,2,2,2,2,2,2,2,2,2,2,2,2,2,2,2,2,2,2,2,2,2,2,2,2,2,2,2,2,2,2,
2,2,2,2,2,2,2,2,2,2,2,2,2,2,2,2,2,2,2,2,2,2,2,2,2,2,2,2,2,2,2,2,2,2,2,2,
2,2,2,2,2,2,2,2,2,2,2,2,2,2,2,2,2,2,2,2,2,2,2,2,2,2,2,2,2,2,2,2,2,2,2,2,
2,2,2,2,2,2,2,2,2,2,2,2,2,2,2,2,2,2,2,2,2,2,2,2,2,2,2,2,2,2,2,2,2,2,2,2,
2,2,2,2,2,2,2,2,2,2,2,2,2,2,2,2,2,2,2,4),(-4.06118295712417,-3.98211311604588,
-3.97644294279158,-3.97363861190561,-3.97194779832783,-3.97039356686888,
-3.96920630782604,-3.96807792437117,-3.96617799409728,-3.96115936628375,
-3.88063000612101,-3.86738208081769,-3.85530621393031,-3.82455397146885,
-3.81447091198009,-3.81022650951905,-3.80933937825198,-3.80867698975359,
-3.80800771516406,-3.80738693666036,-3.80653300532399,-3.8048270122616,
-3.78996955365318,-3.74420383960097,-3.71058124848428,-3.66945208894434,
-3.65783372939953,-3.65062812128208,-3.6485023565452,-3.64719852771346,
-3.646016239894,-3.64449911967408,-3.64137547730347,-3.62141062734092,-3.61584327457818,
-3.60996843848164,-3.56324438329713,-3.51729269495054,-3.48952380635042,
-3.48716796591025,-3.4864248372299,-3.48570321263414,-3.48504058017505,
-3.48417897362813,-3.48237097094483,-3.46921022854859,-3.46865148064511,
-3.42969023402925,-3.37730868182414,-3.35520199811677,-3.33028716769455,
-3.32687968901845,-3.32528588792883,-3.32409247509484,-3.32297583243125,
-3.32143785155262,-3.31753263986351,-3.25456046812247,-3.2030118460561,
-3.16975020542093,-3.16513981973647,-3.16390663852299,-3.16316425798306,
-3.1625065981479,-3.16166922071452,-3.15996563090189,-3.14967028922102,
-3.11975194399027,-3.05528580736834,-3.01238489575362,-3.00774493928961,
-3.00426724670723,-3.00266367227569,-3.00146864842984,-3.00035461527145,
-2.99882665741777,-2.99498052075771,-2.94185030915788,-2.86921429642131,
-2.84602740326167,-2.84230128704041,-2.84115732267686,-2.84043530822821,
-2.8397727183528,-2.83891171403643,-2.83710691366071,-2.82404061289285,
-2.82341841818583,-2.81554325220902,-2.73458895160555,-2.68987839994468,
-2.68270085362783,-2.68057876481697,-2.67927572959313,-2.67809320051751,
-2.67657442987716,-2.67344262427273,-2.65330016605262,-2.6474347849823,
-2.55816159860061,-2.52436800867107,-2.52128767476886,-2.5190533820556,
-2.51811762759138,-2.51744491812701,-2.51682827845283,-2.51599063521607,
-2.51434897543042,-2.50139846809973,-2.50069396172303,-2.50030745961547,
-2.49611419600537,-2.39974424935917,-2.36568378350806,-2.35958598376295,
-2.35760331310739,-2.35633135360042,-2.3551389493318,-2.35357869400014,
-2.35014368186173,-2.32199384286331,-2.29888025520422,-2.23652893784328,
-2.20171556484457,-2.19697265285033,-2.19572567293247,-2.19498584889564,
-2.19432772821767,-2.19348611110426,-2.19176136089304,-2.18104455412962,
-2.12971248022178,-2.08066028111303,-2.04350005525189,-2.03706571655508,
-2.03504246157936,-2.03376147465491,-2.03257245622639,-2.03103342476346,
-2.02771181533641,-1.98265141333053,-1.93173207378056,-1.89325120690849,
-1.89075578823583,-1.87546977624396,-1.8735604454921,-1.87269247641007,
-1.87202882472033,-1.87131007337671,-1.87015720271819,-1.86634745038487,
-1.80231610756,-1.73520862996575,-1.73050394039338,-1.71588025371117,-1.71332703843383,
-1.71178728240709,-1.71059818782047,-1.70931759750449,-1.70729598052919,
-1.7008751298571,-1.66383362274122,-1.61480484408027,-1.55509371647749,
-1.55154713338003,-1.55038059160043,-1.5497308394822,-1.54913936049699,
-1.54833819448639,-1.54681032248342,-1.53760121559862,-1.51867611163583,
-1.43242489056261,-1.41531919246473,-1.39376633022646,-1.39057272416088,
-1.38904182794259,-1.38785779492124,-1.3865610690264,-1.38446694909769,
-1.37754816629822,-1.33545229980823,-1.2486627014256,-1.24747675315554,
-1.23014820467172,-1.22817389191375,-1.227293935712,-1.22662829719309,-1.22591465705775,
-1.22480752906661,-1.22139152473007,-1.20131909365852,-1.18020668891759,
-1.11699025287132,-1.07200283660609,-1.06825850763392,-1.0667479787668,
-1.06563840473277,-1.06444029415,-1.06281875574569,-1.0592447868625,-1.05444598372259,
-1.00897857547919,-0.942659332969499,-0.930458760582793,-0.92756937748556,
-0.925593923114355,-0.924126266116316,-0.923102869098739,-0.922744752673963,
-0.918996009614837,-0.907196344752186,-0.905421716912551,-0.904570190128336,
-0.903910878779164,-0.903176643667838,-0.901979284361568,-0.897736699952111,
-0.890656098386216,-0.864007414556588,-0.814926569374454,-0.749708244432522,
-0.745711008230603,-0.744157569267698,-0.74303679961236,-0.741845567971649,
-0.740265923008089,-0.736931913235841,-0.710715145917066,-0.687631517090654,
-0.632997939871476,-0.585963303592128,-0.583250732446281,-0.582310204413956,
-0.581665798425558,-0.581073132881324,-0.580441933148174,-0.579647286269328,
-0.576769176761861,-0.551118626112138,-0.507552637445211,-0.42819069875983,
-0.423358545685806,-0.421488347259271,-0.420365659671687,-0.419175484552386,
-0.417602475056706,-0.415885694530514,-0.405890347343375,-0.388003491259941,
-0.349198859767511,-0.317635880389431,-0.274134685423581,-0.261926768880253,
-0.260312994489756,-0.259482565055744,-0.258867793410923,-0.258193538498627,
-0.257522546673939,-0.256612516479973,-0.251983468614956,-0.216101133322779,
-0.192485391147722,-0.163640355683076,-0.104291462426126,-0.100399528533765,
-0.0988637483901995,-0.0977476442925963,-0.0965538130989758,-0.0949577418306583,
-0.0932090108039047,-0.0902650433328994,-0.0842084620057397,-0.0681728321545726,
-0.000957725592193056),.UNSPECIFIED.);
#823=B_SPLINE_CURVE_WITH_KNOTS('',3,(#42415,#42416,#42417,#42418,#42419,
#42420,#42421,#42422,#42423,#42424,#42425),.UNSPECIFIED.,.F.,.F.,(4,1,1,
1,1,1,1,1,4),(317.30085801257,317.389884548341,318.388676952109,319.387469355877,
320.386261759645,321.385054163413,322.383846567181,323.382638970949,323.584043319749),
 .UNSPECIFIED.);
#824=B_SPLINE_CURVE_WITH_KNOTS('',3,(#42427,#42428,#42429,#42430,#42431,
#42432,#42433,#42434,#42435,#42436,#42437,#42438,#42439,#42440,#42441,#42442,
#42443,#42444,#42445,#42446,#42447,#42448,#42449,#42450,#42451,#42452,#42453,
#42454,#42455,#42456,#42457,#42458,#42459,#42460,#42461,#42462,#42463,#42464,
#42465,#42466,#42467,#42468,#42469,#42470,#42471,#42472,#42473,#42474,#42475,
#42476,#42477,#42478,#42479,#42480,#42481,#42482,#42483,#42484,#42485,#42486,
#42487,#42488,#42489,#42490,#42491,#42492,#42493,#42494,#42495,#42496,#42497,
#42498,#42499,#42500,#42501,#42502,#42503,#42504,#42505,#42506,#42507,#42508,
#42509,#42510,#42511,#42512,#42513,#42514,#42515,#42516,#42517,#42518,#42519,
#42520,#42521,#42522,#42523,#42524,#42525,#42526,#42527,#42528,#42529,#42530,
#42531,#42532,#42533,#42534,#42535,#42536,#42537,#42538,#42539,#42540,#42541,
#42542,#42543,#42544,#42545,#42546,#42547,#42548,#42549,#42550,#42551,#42552,
#42553,#42554,#42555,#42556,#42557,#42558,#42559,#42560,#42561,#42562,#42563,
#42564,#42565,#42566,#42567,#42568,#42569,#42570,#42571,#42572,#42573,#42574,
#42575,#42576,#42577,#42578,#42579,#42580,#42581,#42582,#42583,#42584,#42585,
#42586,#42587,#42588,#42589,#42590,#42591,#42592,#42593,#42594,#42595,#42596,
#42597,#42598,#42599,#42600,#42601,#42602,#42603,#42604,#42605,#42606,#42607,
#42608,#42609,#42610,#42611,#42612,#42613,#42614,#42615,#42616,#42617,#42618,
#42619,#42620,#42621,#42622,#42623,#42624,#42625,#42626,#42627,#42628,#42629,
#42630,#42631,#42632,#42633,#42634,#42635,#42636,#42637,#42638,#42639,#42640,
#42641,#42642,#42643,#42644,#42645,#42646,#42647,#42648,#42649,#42650,#42651,
#42652,#42653,#42654,#42655,#42656,#42657,#42658,#42659,#42660,#42661,#42662,
#42663,#42664,#42665,#42666,#42667,#42668,#42669,#42670,#42671,#42672,#42673,
#42674,#42675,#42676,#42677,#42678,#42679,#42680,#42681,#42682,#42683,#42684,
#42685,#42686,#42687,#42688,#42689,#42690,#42691,#42692,#42693,#42694,#42695,
#42696,#42697,#42698,#42699,#42700,#42701,#42702,#42703,#42704,#42705,#42706,
#42707,#42708,#42709,#42710,#42711,#42712,#42713,#42714,#42715,#42716,#42717,
#42718,#42719,#42720,#42721,#42722,#42723,#42724,#42725,#42726,#42727,#42728,
#42729,#42730,#42731,#42732,#42733,#42734,#42735,#42736,#42737,#42738,#42739,
#42740,#42741,#42742,#42743,#42744,#42745,#42746,#42747,#42748,#42749,#42750,
#42751,#42752,#42753,#42754,#42755,#42756,#42757,#42758,#42759,#42760,#42761,
#42762,#42763,#42764,#42765,#42766,#42767,#42768,#42769,#42770,#42771,#42772,
#42773,#42774,#42775,#42776,#42777,#42778,#42779,#42780,#42781,#42782,#42783,
#42784,#42785,#42786,#42787,#42788,#42789,#42790,#42791,#42792,#42793,#42794,
#42795,#42796,#42797,#42798,#42799,#42800,#42801,#42802,#42803,#42804,#42805,
#42806,#42807,#42808,#42809,#42810,#42811,#42812,#42813,#42814,#42815,#42816,
#42817,#42818,#42819,#42820,#42821,#42822,#42823,#42824,#42825,#42826,#42827,
#42828,#42829,#42830,#42831,#42832,#42833,#42834,#42835,#42836,#42837,#42838,
#42839,#42840,#42841,#42842,#42843,#42844,#42845,#42846,#42847,#42848,#42849,
#42850,#42851,#42852,#42853,#42854,#42855,#42856,#42857,#42858,#42859,#42860,
#42861,#42862,#42863,#42864,#42865,#42866,#42867,#42868,#42869,#42870,#42871,
#42872,#42873,#42874,#42875,#42876,#42877,#42878,#42879,#42880,#42881,#42882,
#42883,#42884,#42885,#42886,#42887,#42888,#42889,#42890,#42891,#42892,#42893,
#42894,#42895,#42896,#42897,#42898,#42899,#42900,#42901,#42902,#42903,#42904,
#42905,#42906,#42907,#42908,#42909,#42910,#42911,#42912,#42913,#42914,#42915,
#42916,#42917,#42918,#42919,#42920,#42921,#42922,#42923,#42924,#42925,#42926,
#42927,#42928,#42929,#42930,#42931,#42932,#42933,#42934,#42935,#42936,#42937,
#42938,#42939,#42940,#42941,#42942,#42943,#42944,#42945,#42946,#42947,#42948,
#42949,#42950,#42951,#42952,#42953,#42954,#42955,#42956),.UNSPECIFIED.,
 .F.,.F.,(4,2,2,2,2,2,2,2,2,2,2,2,2,2,2,2,2,2,2,2,2,2,2,2,2,2,2,2,2,2,2,
2,2,2,2,2,2,2,2,2,2,2,2,2,2,2,2,2,2,2,2,2,2,2,2,2,2,2,2,2,2,2,2,2,2,2,2,
2,2,2,2,2,2,2,2,2,2,2,2,2,2,2,2,2,2,2,2,2,2,2,2,2,2,2,2,2,2,2,2,2,2,2,2,
2,2,2,2,2,2,2,2,2,2,2,2,2,2,2,2,2,2,2,2,2,2,2,2,2,2,2,2,2,2,2,2,2,2,2,2,
2,2,2,2,2,2,2,2,2,2,2,2,2,2,2,2,2,2,2,2,2,2,2,2,2,2,2,2,2,2,2,2,2,2,2,2,
2,2,2,2,2,2,2,2,2,2,2,2,2,2,2,2,2,2,2,2,2,2,2,2,2,2,2,2,2,2,2,2,2,2,2,2,
2,2,2,2,2,2,2,2,2,2,2,2,2,2,2,2,2,2,2,2,2,2,2,2,2,2,2,2,2,2,2,2,2,2,2,2,
2,2,2,2,2,2,2,2,2,2,2,2,2,2,2,2,2,4),(-4.06040964561679,-3.98577442246086,
-3.93893319569508,-3.9315307619444,-3.92940168895388,-3.92809775376205,
-3.92691662965147,-3.92540275583632,-3.92229200046219,-3.90257088644096,
-3.80854396101611,-3.79058345342708,-3.77614413483332,-3.77141276241636,
-3.76830242735159,-3.76723576547339,-3.76662166886513,-3.765961860903,-3.76511742955535,
-3.76333047339507,-3.75122530414168,-3.71729793051633,-3.69565671967811,
-3.64961571939171,-3.61495714264574,-3.6087950177933,-3.60680522868895,
-3.60553221785033,-3.60434131197846,-3.60278658230598,-3.59937816776643,
-3.57201472591715,-3.49678407291162,-3.47205391189842,-3.45613517563977,
-3.44992047336824,-3.44736175308571,-3.4460274341408,-3.4448989989047,-3.44419210142687,
-3.44352991255855,-3.4426692674781,-3.44123370278448,-3.43287802978631,
-3.3399185899079,-3.29383985603283,-3.28650847633488,-3.28438664762852,
-3.28308424158774,-3.28190259224227,-3.28038538232006,-3.27725832681917,
-3.25718681962563,-3.25101149101381,-3.17609338625293,-3.15086311026694,
-3.12728564476051,-3.12477492318587,-3.12345880661998,-3.12234405295131,
-3.12163986945302,-3.12097682627877,-3.12011051114461,-3.1182082502366,
-3.10311080545929,-3.00442537761231,-2.96983933106461,-2.96368547108904,
-2.9616968538812,-2.96042421146976,-2.95923338098841,-2.95767836361995,
-2.95426775893715,-2.92682594871354,-2.83503539249743,-2.80534153389682,
-2.80247450732444,-2.80102512600825,-2.79981812317432,-2.7990932050262,
-2.79843559929225,-2.79759534769825,-2.79587583017119,-2.78524894509229,
-2.6931370875211,-2.65877949560347,-2.64246378499209,-2.63973639527301,
-2.63830114346262,-2.63724030887634,-2.63608969596705,-2.63442466387267,
-2.6297110584361,-2.62811991407275,-2.52474010105074,-2.49030118424195,
-2.47904559697547,-2.47743960454078,-2.47662238778397,-2.47596687480535,
-2.47521172356809,-2.47392844215611,-2.46925988115289,-2.37393859904464,
-2.32619141322845,-2.31870501775659,-2.31656710587581,-2.31526108047867,
-2.31408023243763,-2.31256971968188,-2.30947645091701,-2.29013697739414,
-2.28493573117174,-2.27611629161686,-2.1887148059889,-2.17291957383105,
-2.15664482164633,-2.15490741837159,-2.15406356422295,-2.15346683357274,
-2.15283644531442,-2.1519457702465,-2.14956516720639,-2.108146195482,-2.07607399590741,
-2.03133671541162,-2.02191906619643,-1.99818686477163,-1.99494780603417,
-1.99340194042678,-1.99221236630473,-1.99093542972142,-1.98892833855414,
-1.98262427865746,-1.94665812573461,-1.83923226976501,-1.83348353798078,
-1.8322204848993,-1.83140297849735,-1.83074726726674,-1.82999192575177,
-1.8286747316449,-1.82309156854107,-1.77159308623169,-1.70783689142447,
-1.70126442191182,-1.69538244522534,-1.67525894959784,-1.67212860612456,
-1.67061037662563,-1.66942819303013,-1.6681254615819,-1.66600369477159,
-1.65867822121284,-1.61266552303177,-1.51501325243428,-1.51057129171881,
-1.50929679781292,-1.50855086734493,-1.50795958401203,-1.50715994162477,
-1.50563907405082,-1.4965860742773,-1.47743806532743,-1.43000244982692,
-1.35459493606651,-1.35012229719897,-1.3484929716044,-1.34735181663008,
-1.34628771785427,-1.34485892334156,-1.34212911942674,-1.33869325129303,
-1.3130346889574,-1.2891507358596,-1.19233242586767,-1.18783485338364,-1.18655414538241,
-1.18580675807785,-1.18521555834548,-1.18441761175837,-1.18290509183925,
-1.17404021032996,-1.1551001465338,-1.10846474531658,-1.10004340279443,
-1.03131955522699,-1.02721989757726,-1.02564956978989,-1.02452430505125,
-1.0233353541832,-1.02180216717406,-1.01856922825714,-1.01433718830831,
-0.977638117205385,-0.925356260986364,-0.868347523858927,-0.867570238411694,
-0.864739352032805,-0.863675755516375,-0.863046517893452,-0.86244871110684,
-0.86159990118064,-0.859839112739079,-0.842394362771705,-0.822215862735034,
-0.741598431603388,-0.730184971472503,-0.707266364136139,-0.70434085591106,
-0.702841646923932,-0.701734963681853,-0.700534747465418,-0.698933818264108,
-0.695343560068391,-0.690528215521247,-0.678765413623159,-0.65567590209208,
-0.618355621546792,-0.586314657975289,-0.544537318760841,-0.541994009187242,
-0.541078719614582,-0.54044135733045,-0.53984674837383,-0.539019388178445,
-0.537365370906282,-0.524589923543127,-0.49879741296503,-0.490229440657184,
-0.483193161660451,-0.42812524813827,-0.409355732401675,-0.403959957494881,
-0.384471094233728,-0.381369253702139,-0.379856397854258,-0.378674557149575,
-0.377572948198401,-0.376291827866456,-0.372541553437571,-0.367454793507337,
-0.354788965616532,-0.316603940198361,-0.238251005602333,-0.221015515594709,
-0.219043797322051,-0.218164280125862,-0.217498681633816,-0.216784789800207,
-0.215653918492291,-0.212037136454894,-0.190171432233036,-0.113280126528247,
-0.106297187583923,-0.0907254957169124,-0.0622845918280095,-0.0588402204557976,
-0.0572781379280803,-0.0560853370877337,-0.0549850786347227,-0.05373861614479,
-0.0519987323967031,-0.0490762387654415,-0.000956587084948417),
 .UNSPECIFIED.);
#825=B_SPLINE_CURVE_WITH_KNOTS('',3,(#42958,#42959,#42960,#42961,#42962,
#42963,#42964,#42965,#42966,#42967,#42968,#42969,#42970,#42971,#42972,#42973,
#42974,#42975,#42976,#42977,#42978,#42979,#42980,#42981,#42982,#42983,#42984,
#42985,#42986,#42987,#42988,#42989,#42990,#42991,#42992,#42993,#42994,#42995,
#42996,#42997,#42998,#42999,#43000,#43001,#43002,#43003,#43004,#43005,#43006,
#43007,#43008,#43009,#43010,#43011,#43012,#43013,#43014,#43015,#43016,#43017,
#43018,#43019,#43020,#43021,#43022,#43023,#43024,#43025,#43026,#43027,#43028,
#43029,#43030,#43031,#43032,#43033,#43034,#43035,#43036,#43037,#43038,#43039,
#43040,#43041,#43042,#43043,#43044,#43045,#43046,#43047,#43048,#43049,#43050,
#43051,#43052,#43053,#43054,#43055,#43056,#43057,#43058,#43059,#43060,#43061,
#43062,#43063,#43064,#43065,#43066,#43067,#43068,#43069,#43070,#43071,#43072,
#43073,#43074,#43075,#43076,#43077,#43078,#43079,#43080,#43081,#43082,#43083,
#43084,#43085,#43086,#43087,#43088,#43089,#43090,#43091,#43092,#43093,#43094,
#43095,#43096,#43097,#43098,#43099,#43100,#43101,#43102,#43103,#43104,#43105,
#43106,#43107,#43108,#43109,#43110,#43111,#43112,#43113,#43114,#43115,#43116,
#43117,#43118,#43119,#43120,#43121,#43122,#43123,#43124,#43125,#43126,#43127,
#43128,#43129,#43130,#43131,#43132,#43133,#43134,#43135,#43136,#43137,#43138,
#43139,#43140,#43141,#43142,#43143,#43144,#43145,#43146,#43147,#43148,#43149,
#43150,#43151,#43152,#43153,#43154,#43155,#43156,#43157,#43158,#43159,#43160,
#43161,#43162,#43163,#43164,#43165,#43166,#43167,#43168,#43169,#43170,#43171,
#43172,#43173,#43174,#43175,#43176,#43177,#43178,#43179,#43180,#43181,#43182,
#43183,#43184,#43185,#43186,#43187,#43188,#43189,#43190,#43191,#43192,#43193,
#43194,#43195,#43196,#43197,#43198,#43199,#43200,#43201,#43202,#43203,#43204,
#43205,#43206,#43207,#43208,#43209,#43210,#43211,#43212,#43213,#43214,#43215,
#43216,#43217,#43218,#43219,#43220,#43221,#43222,#43223,#43224,#43225,#43226,
#43227,#43228,#43229,#43230,#43231,#43232,#43233,#43234,#43235,#43236,#43237,
#43238,#43239,#43240,#43241,#43242,#43243,#43244,#43245,#43246,#43247,#43248,
#43249,#43250,#43251,#43252,#43253,#43254,#43255,#43256,#43257,#43258,#43259,
#43260,#43261,#43262,#43263,#43264,#43265,#43266,#43267,#43268,#43269,#43270,
#43271,#43272,#43273,#43274,#43275,#43276,#43277,#43278,#43279,#43280,#43281,
#43282,#43283,#43284,#43285,#43286,#43287,#43288,#43289,#43290,#43291,#43292,
#43293,#43294,#43295,#43296,#43297,#43298,#43299,#43300,#43301,#43302,#43303,
#43304,#43305,#43306,#43307,#43308,#43309,#43310,#43311,#43312,#43313,#43314,
#43315,#43316,#43317,#43318,#43319,#43320,#43321,#43322,#43323,#43324,#43325,
#43326,#43327,#43328,#43329,#43330,#43331,#43332,#43333,#43334,#43335,#43336,
#43337,#43338,#43339,#43340,#43341,#43342,#43343,#43344,#43345,#43346,#43347,
#43348,#43349,#43350,#43351,#43352,#43353,#43354,#43355,#43356,#43357,#43358,
#43359,#43360,#43361,#43362,#43363,#43364,#43365,#43366,#43367,#43368,#43369,
#43370,#43371,#43372,#43373,#43374,#43375,#43376,#43377,#43378,#43379,#43380,
#43381,#43382,#43383,#43384,#43385,#43386,#43387,#43388,#43389,#43390,#43391,
#43392,#43393,#43394,#43395,#43396,#43397,#43398,#43399,#43400,#43401,#43402,
#43403,#43404,#43405,#43406,#43407,#43408,#43409,#43410,#43411,#43412,#43413,
#43414,#43415,#43416,#43417,#43418,#43419,#43420,#43421,#43422,#43423,#43424,
#43425,#43426,#43427,#43428,#43429,#43430,#43431,#43432,#43433,#43434,#43435,
#43436,#43437,#43438,#43439,#43440,#43441,#43442,#43443,#43444,#43445,#43446,
#43447,#43448,#43449,#43450,#43451,#43452,#43453,#43454,#43455,#43456,#43457,
#43458,#43459,#43460,#43461,#43462,#43463,#43464,#43465,#43466,#43467,#43468,
#43469,#43470,#43471,#43472,#43473,#43474,#43475,#43476,#43477,#43478,#43479,
#43480,#43481),.UNSPECIFIED.,.F.,.F.,(4,2,2,2,2,2,2,2,2,2,2,2,2,2,2,2,2,
2,2,2,2,2,2,2,2,2,2,2,2,2,2,2,2,2,2,2,2,2,2,2,2,2,2,2,2,2,2,2,2,2,2,2,2,
2,2,2,2,2,2,2,2,2,2,2,2,2,2,2,2,2,2,2,2,2,2,2,2,2,2,2,2,2,2,2,2,2,2,2,2,
2,2,2,2,2,2,2,2,2,2,2,2,2,2,2,2,2,2,2,2,2,2,2,2,2,2,2,2,2,2,2,2,2,2,2,2,
2,2,2,2,2,2,2,2,2,2,2,2,2,2,2,2,2,2,2,2,2,2,2,2,2,2,2,2,2,2,2,2,2,2,2,2,
2,2,2,2,2,2,2,2,2,2,2,2,2,2,2,2,2,2,2,2,2,2,2,2,2,2,2,2,2,2,2,2,2,2,2,2,
2,2,2,2,2,2,2,2,2,2,2,2,2,2,2,2,2,2,2,2,2,2,2,2,2,2,2,2,2,2,2,2,2,2,2,2,
2,2,2,2,2,2,2,2,2,2,2,2,2,2,2,2,2,2,2,2,2,2,2,2,2,2,2,2,4),(-4.0602155392693,
-3.99823060173568,-3.96839489076751,-3.9570393989674,-3.95542940171613,
-3.95461110461063,-3.95395520086939,-3.95320013103987,-3.95191821573228,
-3.94726674682146,-3.85267067305009,-3.83142314384518,-3.79931803791138,
-3.79556874229651,-3.79428634359585,-3.79318479384265,-3.79200350565062,
-3.79049378420746,-3.78740688070022,-3.76822690106404,-3.76312316617948,
-3.74464537484264,-3.70635129238098,-3.67255223568283,-3.63843561254961,
-3.63374434705983,-3.63250222505594,-3.63176356148629,-3.63110534927944,
-3.63026210267512,-3.6285287751609,-3.61763370621091,-3.54354528604912,
-3.50514756935874,-3.48538627545259,-3.47462063049694,-3.4722087301611,
-3.47106977239965,-3.4700019387804,-3.46887210927611,-3.4672841875383,-3.46400501857127,
-3.42823187279132,-3.34993742083824,-3.31580192115324,-3.31110912856822,
-3.30986682046659,-3.30912808934533,-3.30846984511238,-3.30762659541212,
-3.30589339318106,-3.29500227145687,-3.20295867582908,-3.16872443801467,
-3.15800831240741,-3.1535147257588,-3.15114961814424,-3.14920452771105,
-3.14792185507935,-3.14674096702465,-3.14523417638961,-3.14226335011876,
-3.12465409572201,-3.12107470177142,-3.02537247551533,-2.99942481964225,
-2.98892164373728,-2.98734168212667,-2.98652961066877,-2.98593697225873,
-2.98529280508737,-2.98435297842529,-2.98164480407284,-2.93402020877064,
-2.87153303115491,-2.83479784545156,-2.83056315754493,-2.82733018007156,
-2.82579604960904,-2.82467120212098,-2.82355841583567,-2.82203515693363,
-2.81821636357285,-2.76779774313479,-2.70486907523802,-2.66706070469614,
-2.66497908350776,-2.66407005491187,-2.66340219690131,-2.66277928574838,
-2.66191729167346,-2.65971394732196,-2.6293191856938,-2.54885957167821,
-2.52560834887318,-2.50718662003834,-2.50437234604507,-2.5029182682703,
-2.50185463610962,-2.50071165429682,-2.49907579122292,-2.49456056198429,
-2.41870805169403,-2.37152835481226,-2.35244886586808,-2.34349443308676,
-2.34197795363165,-2.34117922214147,-2.34053058543046,-2.3398636071348,
-2.33861153909123,-2.33436964322727,-2.25983583946856,-2.18546836497904,
-2.18200242797144,-2.18041940391096,-2.17922779848189,-2.17810826924329,
-2.17625390127099,-2.17151779012193,-2.09757404088505,-2.04947672295402,
-2.03045394643723,-2.02099913170587,-2.01936050304138,-2.01852513816433,
-2.01786773140263,-2.01712419855575,-2.01586044975354,-2.01092901556941,
-1.98760098772583,-1.94092169293096,-1.86477752126815,-1.86000075050033,
-1.8581397283213,-1.85701892521598,-1.85582802666224,-1.85424944927688,
-1.8508071877283,-1.78549054557636,-1.70202201451824,-1.69760055350719,
-1.69632824704829,-1.69558276073249,-1.69499135181605,-1.6941909267222,
-1.69266657501858,-1.68353762834365,-1.66441984611714,-1.61690988530063,
-1.54158321115397,-1.53713227783861,-1.53550619126619,-1.53436586014014,
-1.53330138411472,-1.53184103407294,-1.52899688879344,-1.50976124773764,
-1.49997146723766,-1.47605987209602,-1.39206049736505,-1.38887298287399,
-1.38725079395284,-1.3757140981856,-1.37395113771415,-1.37310190208313,
-1.37244286177031,-1.37170734109236,-1.37047974725895,-1.36604254428399,
-1.33499202393868,-1.24773502753606,-1.24132309248633,-1.23608079615596,
-1.21672852472928,-1.21363317555186,-1.21212164977253,-1.21094001105244,
-1.20963311243577,-1.20753652026161,-1.20041761092466,-1.15627423956649,
-1.09265468754004,-1.06323654697815,-1.05291665787788,-1.05121179448688,
-1.0503741486475,-1.04971644688079,-1.04897419907327,-1.0477164148588,-1.04297989480434,
-1.00801005710205,-0.941688168879405,-0.929280981215799,-0.894878741849937,
-0.891268479386463,-0.889819639711263,-0.888615961189213,-0.887385749087742,
-0.886153129845173,-0.882874298809824,-0.861188705103079,-0.82590504431776,
-0.78176496033359,-0.744246958058379,-0.743702717531739,-0.73051609918907,
-0.728707054836243,-0.727845220868044,-0.727182535586847,-0.726460979473548,
-0.725295534527965,-0.721462390562413,-0.715266492935087,-0.698177037992769,
-0.634445914960613,-0.572797638557261,-0.568896077388422,-0.567358727415494,
-0.566242260934364,-0.565048772174144,-0.563877895180517,-0.561331822488007,
-0.547162298058298,-0.518801594335806,-0.477093344383485,-0.410757078412684,
-0.406824343885069,-0.405608733818244,-0.404949085388673,-0.404293456647265,
-0.403479401099224,-0.402606132987589,-0.398586629346373,-0.391992691841185,
-0.368965929448184,-0.342948439432188,-0.316568198202258,-0.282648837701999,
-0.272301123937339,-0.2491590419796,-0.246225282132891,-0.244723946205397,
-0.243616718716812,-0.242416901452655,-0.24123452570869,-0.239660963587682,
-0.237137319333108,-0.219061549673271,-0.186160493229908,-0.174139202419186,
-0.160956235357465,-0.0881422054516073,-0.0842268030630355,-0.0830132382568326,
-0.0823539636508675,-0.0816982199509651,-0.0808833068662808,-0.0800088694986765,
-0.0786053941585817,-0.0758631083913248,-0.000957591977515441),
 .UNSPECIFIED.);
#826=B_SPLINE_CURVE_WITH_KNOTS('',3,(#43483,#43484,#43485,#43486,#43487,
#43488,#43489,#43490,#43491,#43492,#43493,#43494,#43495,#43496,#43497,#43498,
#43499,#43500,#43501,#43502,#43503,#43504,#43505,#43506,#43507,#43508,#43509,
#43510,#43511,#43512,#43513,#43514,#43515,#43516,#43517,#43518,#43519,#43520,
#43521,#43522,#43523,#43524,#43525,#43526,#43527,#43528,#43529,#43530,#43531,
#43532,#43533,#43534,#43535,#43536,#43537,#43538,#43539,#43540,#43541,#43542,
#43543,#43544,#43545,#43546,#43547,#43548,#43549,#43550,#43551,#43552,#43553,
#43554,#43555,#43556,#43557,#43558,#43559,#43560,#43561,#43562,#43563,#43564,
#43565,#43566,#43567,#43568,#43569,#43570,#43571,#43572,#43573,#43574,#43575,
#43576,#43577,#43578,#43579,#43580,#43581,#43582,#43583,#43584,#43585,#43586,
#43587,#43588,#43589,#43590,#43591,#43592,#43593,#43594,#43595,#43596,#43597,
#43598,#43599,#43600,#43601,#43602,#43603,#43604,#43605,#43606,#43607,#43608,
#43609,#43610,#43611,#43612,#43613,#43614,#43615,#43616,#43617,#43618,#43619,
#43620,#43621,#43622,#43623,#43624,#43625,#43626,#43627,#43628,#43629,#43630,
#43631,#43632,#43633,#43634,#43635,#43636,#43637,#43638,#43639,#43640,#43641,
#43642,#43643,#43644,#43645,#43646,#43647,#43648,#43649,#43650,#43651,#43652,
#43653,#43654,#43655,#43656,#43657,#43658,#43659,#43660,#43661,#43662,#43663,
#43664,#43665,#43666,#43667,#43668,#43669,#43670,#43671,#43672,#43673,#43674,
#43675,#43676,#43677,#43678,#43679,#43680,#43681,#43682,#43683,#43684,#43685,
#43686,#43687,#43688,#43689,#43690,#43691,#43692,#43693,#43694,#43695,#43696,
#43697,#43698,#43699,#43700,#43701,#43702,#43703,#43704,#43705,#43706,#43707,
#43708,#43709,#43710,#43711,#43712,#43713,#43714,#43715,#43716,#43717,#43718,
#43719,#43720,#43721,#43722,#43723,#43724,#43725,#43726,#43727,#43728,#43729,
#43730,#43731,#43732,#43733,#43734,#43735,#43736,#43737,#43738,#43739,#43740,
#43741,#43742,#43743,#43744,#43745,#43746,#43747,#43748,#43749,#43750,#43751,
#43752,#43753,#43754,#43755,#43756,#43757,#43758,#43759,#43760,#43761,#43762,
#43763,#43764,#43765,#43766,#43767,#43768,#43769,#43770,#43771,#43772,#43773,
#43774,#43775,#43776,#43777,#43778,#43779,#43780,#43781,#43782,#43783,#43784,
#43785,#43786,#43787,#43788,#43789,#43790,#43791,#43792,#43793,#43794,#43795,
#43796,#43797,#43798,#43799,#43800,#43801,#43802,#43803,#43804,#43805,#43806,
#43807,#43808,#43809,#43810,#43811,#43812,#43813,#43814,#43815,#43816,#43817,
#43818,#43819,#43820,#43821,#43822,#43823,#43824,#43825,#43826,#43827,#43828,
#43829,#43830,#43831,#43832,#43833,#43834,#43835,#43836,#43837,#43838,#43839,
#43840,#43841,#43842,#43843,#43844,#43845,#43846,#43847,#43848,#43849,#43850,
#43851,#43852,#43853,#43854,#43855,#43856,#43857,#43858,#43859,#43860,#43861,
#43862,#43863,#43864,#43865,#43866,#43867,#43868,#43869,#43870,#43871,#43872,
#43873,#43874,#43875,#43876,#43877,#43878,#43879,#43880,#43881,#43882,#43883,
#43884,#43885,#43886,#43887,#43888,#43889,#43890,#43891,#43892,#43893,#43894,
#43895,#43896,#43897,#43898,#43899,#43900,#43901,#43902,#43903,#43904,#43905,
#43906,#43907,#43908,#43909,#43910,#43911,#43912,#43913,#43914,#43915,#43916,
#43917,#43918,#43919,#43920,#43921,#43922,#43923,#43924,#43925,#43926,#43927,
#43928,#43929,#43930,#43931,#43932,#43933,#43934,#43935,#43936,#43937,#43938,
#43939,#43940,#43941,#43942,#43943,#43944,#43945,#43946,#43947,#43948,#43949,
#43950,#43951,#43952,#43953,#43954,#43955,#43956,#43957,#43958,#43959,#43960,
#43961,#43962,#43963,#43964,#43965,#43966,#43967,#43968,#43969,#43970,#43971,
#43972,#43973,#43974,#43975,#43976,#43977,#43978,#43979,#43980,#43981,#43982,
#43983,#43984,#43985,#43986,#43987,#43988,#43989,#43990,#43991,#43992,#43993,
#43994,#43995,#43996,#43997,#43998,#43999,#44000,#44001,#44002,#44003,#44004,
#44005,#44006,#44007,#44008,#44009,#44010,#44011,#44012,#44013,#44014,#44015,
#44016,#44017,#44018,#44019,#44020,#44021,#44022),.UNSPECIFIED.,.F.,.F.,
(4,2,2,2,2,2,2,2,2,2,2,2,2,2,2,2,2,2,2,2,2,2,2,2,2,2,2,2,2,2,2,2,2,2,2,
2,2,2,2,2,2,2,2,2,2,2,2,2,2,2,2,2,2,2,2,2,2,2,2,2,2,2,2,2,2,2,2,2,2,2,2,
2,2,2,2,2,2,2,2,2,2,2,2,2,2,2,2,2,2,2,2,2,2,2,2,2,2,2,2,2,2,2,2,2,2,2,2,
2,2,2,2,2,2,2,2,2,2,2,2,2,2,2,2,2,2,2,2,2,2,2,2,2,2,2,2,2,2,2,2,2,2,2,2,
2,2,2,2,2,2,2,2,2,2,2,2,2,2,2,2,2,2,2,2,2,2,2,2,2,2,2,2,2,2,2,2,2,2,2,2,
2,2,2,2,2,2,2,2,2,2,2,2,2,2,2,2,2,2,2,2,2,2,2,2,2,2,2,2,2,2,2,2,2,2,2,2,
2,2,2,2,2,2,2,2,2,2,2,2,2,2,2,2,2,2,2,2,2,2,2,2,2,2,2,2,2,2,2,2,2,2,2,2,
2,2,2,2,2,2,2,2,2,2,2,2,2,2,2,2,2,2,4),(-4.06122042211378,-3.98730337121336,
-3.98478298796875,-3.98321096509116,-3.9817426771538,-3.98067739930817,
-3.97954090655895,-3.97792812220703,-3.97356141876023,-3.90239136750869,
-3.88744857196921,-3.87338246909838,-3.83815753939089,-3.82315510258274,
-3.8217559239748,-3.82088339969083,-3.820069942818,-3.81941453579877,-3.81875488824774,
-3.81753866236554,-3.81359905183284,-3.74561337849167,-3.71806506483374,
-3.68218021724648,-3.66982917492818,-3.66227714388483,-3.66069270293434,
-3.65921543834216,-3.65814892068119,-3.65701602956684,-3.65541648733755,
-3.65113256754568,-3.58453589773527,-3.53280112881335,-3.50307982617067,
-3.49917624551057,-3.49831109495267,-3.49750292936578,-3.49691085238028,
-3.49626501258054,-3.49511732416295,-3.49171187607518,-3.43500939814268,
-3.39559396279255,-3.35772012967898,-3.34081249585685,-3.33806787342071,
-3.33689489079826,-3.33570039657015,-3.33458625774305,-3.33305722018905,
-3.32920349293516,-3.27517438759,-3.22009809872474,-3.19939260063911,-3.18134519051984,
-3.17682314732775,-3.17556114273915,-3.17481807792218,-3.17416072589412,
-3.17332495577946,-3.17162875370144,-3.16147761245603,-3.15818554928967,
-3.13276854286616,-3.08213645610593,-3.04171154835074,-3.01938446255512,
-3.01596083833761,-3.01436766540178,-3.01317455093995,-3.01205806258737,
-3.01052009807253,-3.00661389087386,-2.9425802188186,-2.85783054741572,
-2.85401482038519,-2.85284841101573,-2.85212667964196,-2.85146412986671,
-2.85060287768581,-2.84879649434053,-2.8356755135456,-2.83261639571709,
-2.8294418849335,-2.82821064920523,-2.81567553258686,-2.73974766712154,
-2.70089663279329,-2.69651971096086,-2.6931967079389,-2.69162638755515,
-2.69043677664342,-2.68931353249669,-2.68743983348207,-2.68258497771407,
-2.67587768014566,-2.67356927017684,-2.67110782495242,-2.57183333383073,
-2.53622755813954,-2.5314277913914,-2.5301756442988,-2.52943465357279,-2.52877672603962,
-2.52793700419617,-2.5266023638827,-2.51988537181546,-2.51947214958272,
-2.41772564013066,-2.37403572369145,-2.37041209038707,-2.36879996069456,
-2.3676035913794,-2.36649190689406,-2.36497275570634,-2.36117765877328,
-2.31255583175956,-2.28650709652996,-2.23637804959072,-2.21781326933854,
-2.20913098770327,-2.20762715014145,-2.20683113650648,-2.20624021316018,
-2.20558776706399,-2.20440761635382,-2.20075624521831,-2.14050161171187,
-2.09175191631063,-2.06844345436592,-2.05019943743177,-2.04739195426642,
-2.04593932268583,-2.04477443514057,-2.04343476415978,-2.04114844799486,
-2.03319218162742,-2.03124545084192,-2.01389769449877,-1.9913965784436,
-1.89996390509604,-1.8869704300372,-1.88532734585329,-1.88448936729588,
-1.88387266975754,-1.88320009159846,-1.88226486030631,-1.88003341010227,
-1.87695807918521,-1.84327045884236,-1.75800399175919,-1.72848354193204,
-1.72535415684697,-1.72380324491251,-1.72268320532421,-1.72149173535969,
-1.71991004888465,-1.71645165664784,-1.6457963850695,-1.57544824360086,
-1.56410033746409,-1.56234596674019,-1.56149844354663,-1.56083962454671,
-1.56010317742488,-1.55887138016999,-1.55429274431194,-1.52166277449236,
-1.43836967100109,-1.43087542000263,-1.42524780827744,-1.40519956296268,
-1.40207204850946,-1.40055414024952,-1.39937173203908,-1.398068271477,-1.39594423441197,
-1.38860051188451,-1.34240265391867,-1.26300660503229,-1.25535542778925,
-1.25495320468321,-1.25373684375561,-1.24143474105209,-1.23981679469797,
-1.23898526413092,-1.23837019057029,-1.23769613931494,-1.23677211008846,
-1.23460662059235,-1.23161136531513,-1.19952162699187,-1.13704526953143,
-1.08369366942478,-1.07984521221592,-1.07831679637746,-1.07720259212926,
-1.07600753849208,-1.07440419299453,-1.07082946946612,-1.02317867966916,
-0.94435449843721,-0.936115112965031,-0.918981701666313,-0.917013651069756,
-0.91613479335376,-0.915469295708838,-0.914855791275076,-0.913835631132868,
-0.911054556891232,-0.906957898634397,-0.821252614542162,-0.760959494831596,
-0.757062876779412,-0.75552627607693,-0.754409934935059,-0.753216187307075,
-0.751620808957072,-0.748089328074736,-0.696225977430358,-0.633654586601938,
-0.618594202933411,-0.612365763547671,-0.609432652356723,-0.608021727178315,
-0.595946880155507,-0.594160278029042,-0.593315538340491,-0.592655278393957,
-0.592040705716364,-0.590972788021841,-0.587873645667218,-0.583157999019995,
-0.568790227843729,-0.527324513288269,-0.45733008687709,-0.452320031875047,
-0.43666565197809,-0.434055745011115,-0.432499174284159,-0.431307309032712,
-0.430033711634002,-0.428043914507691,-0.421888832961478,-0.387303638297796,
-0.3511214309649,-0.317569991591704,-0.274702820330594,-0.2719968592842,
-0.271057308472001,-0.270413186513801,-0.269820472695677,-0.269189143689019,
-0.268394019388826,-0.265462270474878,-0.234321212494021,-0.213785909967768,
-0.152702400364498,-0.139501408467639,-0.134046470652641,-0.114406872628747,
-0.111297993682692,-0.109783727919976,-0.108601705146172,-0.107296173994659,
-0.105163130596233,-0.0977335934131149,-0.0506185946559123,-0.000958062894794184),
 .UNSPECIFIED.);
#827=B_SPLINE_CURVE_WITH_KNOTS('',3,(#44024,#44025,#44026,#44027,#44028,
#44029,#44030,#44031,#44032,#44033,#44034,#44035,#44036,#44037,#44038,#44039,
#44040,#44041,#44042,#44043,#44044,#44045,#44046,#44047,#44048,#44049,#44050,
#44051,#44052,#44053,#44054,#44055,#44056,#44057,#44058,#44059,#44060,#44061,
#44062,#44063,#44064,#44065,#44066,#44067,#44068,#44069,#44070,#44071,#44072,
#44073,#44074,#44075,#44076,#44077,#44078,#44079,#44080,#44081,#44082,#44083,
#44084,#44085,#44086,#44087,#44088,#44089,#44090,#44091,#44092,#44093,#44094,
#44095,#44096,#44097,#44098,#44099,#44100,#44101,#44102,#44103,#44104,#44105,
#44106,#44107,#44108,#44109,#44110,#44111,#44112,#44113,#44114,#44115,#44116,
#44117,#44118,#44119,#44120,#44121,#44122,#44123,#44124,#44125,#44126,#44127,
#44128,#44129,#44130,#44131,#44132,#44133,#44134,#44135,#44136,#44137,#44138,
#44139,#44140,#44141,#44142,#44143,#44144,#44145,#44146,#44147,#44148,#44149,
#44150,#44151,#44152,#44153,#44154,#44155,#44156,#44157,#44158,#44159,#44160,
#44161,#44162,#44163,#44164,#44165,#44166,#44167,#44168,#44169,#44170,#44171,
#44172,#44173,#44174,#44175,#44176,#44177,#44178,#44179,#44180,#44181,#44182,
#44183,#44184,#44185,#44186,#44187,#44188,#44189,#44190,#44191,#44192,#44193,
#44194,#44195,#44196,#44197,#44198,#44199,#44200,#44201,#44202,#44203,#44204,
#44205,#44206,#44207,#44208,#44209,#44210,#44211,#44212,#44213,#44214,#44215,
#44216,#44217,#44218,#44219,#44220,#44221,#44222,#44223,#44224,#44225,#44226,
#44227,#44228,#44229,#44230,#44231,#44232,#44233,#44234,#44235,#44236,#44237,
#44238,#44239,#44240,#44241,#44242,#44243,#44244,#44245,#44246,#44247,#44248,
#44249,#44250,#44251,#44252,#44253,#44254,#44255,#44256,#44257,#44258,#44259,
#44260,#44261,#44262,#44263,#44264,#44265,#44266,#44267,#44268,#44269,#44270,
#44271,#44272,#44273,#44274,#44275,#44276,#44277,#44278,#44279,#44280,#44281,
#44282,#44283,#44284,#44285,#44286,#44287,#44288,#44289,#44290,#44291,#44292,
#44293,#44294,#44295,#44296,#44297,#44298,#44299,#44300,#44301,#44302,#44303,
#44304,#44305,#44306,#44307,#44308,#44309,#44310,#44311,#44312,#44313,#44314,
#44315,#44316,#44317,#44318,#44319,#44320,#44321,#44322,#44323,#44324,#44325,
#44326,#44327,#44328,#44329,#44330,#44331,#44332,#44333,#44334,#44335,#44336,
#44337,#44338,#44339,#44340,#44341,#44342,#44343,#44344,#44345,#44346,#44347,
#44348,#44349,#44350,#44351,#44352,#44353,#44354,#44355,#44356,#44357,#44358,
#44359,#44360,#44361,#44362,#44363,#44364,#44365,#44366,#44367,#44368,#44369,
#44370,#44371,#44372,#44373,#44374,#44375,#44376,#44377,#44378,#44379,#44380,
#44381,#44382,#44383,#44384,#44385,#44386,#44387,#44388,#44389,#44390,#44391,
#44392,#44393,#44394,#44395,#44396,#44397,#44398,#44399,#44400,#44401,#44402,
#44403,#44404,#44405,#44406,#44407,#44408,#44409,#44410,#44411,#44412,#44413,
#44414,#44415,#44416,#44417,#44418,#44419,#44420,#44421,#44422,#44423,#44424,
#44425,#44426,#44427,#44428,#44429,#44430,#44431,#44432,#44433,#44434,#44435,
#44436,#44437,#44438,#44439,#44440,#44441,#44442,#44443,#44444,#44445,#44446,
#44447,#44448,#44449,#44450,#44451,#44452,#44453,#44454,#44455,#44456,#44457,
#44458,#44459,#44460,#44461,#44462,#44463,#44464,#44465,#44466,#44467,#44468,
#44469,#44470,#44471,#44472,#44473,#44474,#44475,#44476,#44477,#44478,#44479,
#44480,#44481,#44482,#44483,#44484,#44485,#44486,#44487,#44488,#44489,#44490,
#44491,#44492,#44493,#44494,#44495,#44496,#44497,#44498,#44499,#44500,#44501,
#44502,#44503,#44504,#44505,#44506,#44507,#44508,#44509,#44510,#44511,#44512,
#44513,#44514,#44515,#44516,#44517,#44518,#44519,#44520,#44521,#44522,#44523,
#44524,#44525,#44526,#44527,#44528,#44529,#44530,#44531,#44532,#44533,#44534,
#44535,#44536,#44537,#44538,#44539,#44540,#44541,#44542,#44543,#44544,#44545,
#44546,#44547,#44548,#44549,#44550,#44551,#44552,#44553,#44554,#44555,#44556,
#44557),.UNSPECIFIED.,.F.,.F.,(4,2,2,2,2,2,2,2,2,2,2,2,2,2,2,2,2,2,2,2,
2,2,2,2,2,2,2,2,2,2,2,2,2,2,2,2,2,2,2,2,2,2,2,2,2,2,2,2,2,2,2,2,2,2,2,2,
2,2,2,2,2,2,2,2,2,2,2,2,2,2,2,2,2,2,2,2,2,2,2,2,2,2,2,2,2,2,2,2,2,2,2,2,
2,2,2,2,2,2,2,2,2,2,2,2,2,2,2,2,2,2,2,2,2,2,2,2,2,2,2,2,2,2,2,2,2,2,2,2,
2,2,2,2,2,2,2,2,2,2,2,2,2,2,2,2,2,2,2,2,2,2,2,2,2,2,2,2,2,2,2,2,2,2,2,2,
2,2,2,2,2,2,2,2,2,2,2,2,2,2,2,2,2,2,2,2,2,2,2,2,2,2,2,2,2,2,2,2,2,2,2,2,
2,2,2,2,2,2,2,2,2,2,2,2,2,2,2,2,2,2,2,2,2,2,2,2,2,2,2,2,2,2,2,2,2,2,2,2,
2,2,2,2,2,2,2,2,2,2,2,2,2,2,2,2,2,2,2,2,2,2,2,2,2,2,2,2,2,2,4),(-4.05973415353602,
-4.01165008765246,-4.00941701345505,-4.00820757326979,-4.00741466348188,
-4.00678423325295,-4.00619211720911,-4.00554748056146,-4.00460522964405,
-4.00187830154151,-3.953499761186,-3.9407436132943,-3.92894404673932,-3.90389673324836,
-3.85647816948271,-3.84902159477275,-3.84688660388739,-3.84558114606902,
-3.84440001653371,-3.84288804216987,-3.83978790765343,-3.82030680562777,
-3.81856999517357,-3.74357053098659,-3.70602312480943,-3.69306381939591,
-3.68868923990147,-3.68576254376805,-3.68497012177565,-3.68433980616281,
-3.68374771774191,-3.68310274248955,-3.6821593771321,-3.67942501539386,
-3.6354928188547,-3.58335735510639,-3.57536856879101,-3.54428219867686,
-3.52765264463386,-3.52491120482614,-3.52347279545918,-3.52241141106925,
-3.52126193496572,-3.51960153076107,-3.51492048885988,-3.43608850068325,
-3.39839813611484,-3.37730850941143,-3.36439194251438,-3.36273991838272,
-3.36207266482662,-3.36140074222927,-3.36078400597841,-3.35994505488879,
-3.35787425309426,-3.33500100197902,-3.3225115932881,-3.25775013710391,
-3.21138978858522,-3.20403133177031,-3.20190640750415,-3.20060314457192,
-3.19942140299544,-3.19790502983747,-3.19478308919397,-3.17483339903091,
-3.16833847387493,-3.12544874744067,-3.06951526246094,-3.0449270624279,
-3.04235441627532,-3.04043585084003,-3.03955861285647,-3.03889330104224,
-3.03826699813792,-3.03739156536359,-3.03559870241415,-3.01766680112572,
-3.01043924554607,-2.92127555932061,-2.88730218082688,-2.88121531380936,
-2.87923468500324,-2.87796364647946,-2.87677182961388,-2.87521194533933,
-2.87177613125532,-2.84355473352583,-2.82514131656146,-2.75616139052032,
-2.73702073731538,-2.7212607474561,-2.71926564682063,-2.71770178154918,
-2.71689695755096,-2.71630342083122,-2.71566405735846,-2.71454807610885,
-2.71136852971746,-2.65750448828532,-2.56470146473298,-2.55864349571014,
-2.55666653453603,-2.55539636993102,-2.55420432076727,-2.55264261500176,
-2.54919659398856,-2.52064032476493,-2.428239838504,-2.40013784496887,-2.39735922975404,
-2.39530113304027,-2.39439658872299,-2.39372974887369,-2.39310607413245,
-2.39224045303626,-2.39001417403211,-2.35786194069184,-2.32326723923747,
-2.29119389622761,-2.25429315592853,-2.2375637856402,-2.23481804435973,
-2.2333787099457,-2.23231720291208,-2.23116813713329,-2.22950925883561,
-2.22483858503327,-2.1504415040563,-2.10257062196525,-2.07735925641474,
-2.07342143193023,-2.07225479566735,-2.07153317836553,-2.07087091220759,
-2.07001027293374,-2.06820604071313,-2.05512824558456,-2.052648969683,-2.0522565185369,
-2.04549023016851,-2.0314480931122,-1.9437020134791,-1.91604838355523,-1.91263035985199,
-1.91107373796341,-1.9098824165392,-1.90860996703368,-1.906623135393,-1.900486315262,
-1.86605474786771,-1.76801477730732,-1.76588993846838,-1.76551364586657,
-1.76477055613347,-1.751876636334,-1.75023752101634,-1.74940071972699,-1.74878447710516,
-1.74811197016471,-1.74717609249539,-1.74493960392291,-1.74185521492002,
-1.70797044623799,-1.62503875622738,-1.61721685831853,-1.61220492892579,
-1.59288245182046,-1.58978938287022,-1.5882786712886,-1.5870975325393,-1.58579104736821,
-1.58365206915085,-1.57615884923341,-1.52833608089518,-1.43300273999321,
-1.42832939480946,-1.42704533676396,-1.42628984447174,-1.42563410833287,
-1.42481670858595,-1.42321065587256,-1.4119657976086,-1.37873792632746,
-1.27420013715539,-1.26822401220228,-1.26618259088209,-1.26502635141361,
-1.26387200040643,-1.2624318529962,-1.26087135638339,-1.25837829902198,
-1.253547656717,-1.20754014024346,-1.10989601028361,-1.10545456186501,-1.1041801983673,
-1.10343434048311,-1.10284311255049,-1.10204354235009,-1.10052280318078,
-1.09147032340054,-1.07232405365638,-1.02489228675618,-0.949483034791866,
-0.94501793268378,-0.94338985059188,-0.942249102753054,-0.9410914226805,
-0.939617726288424,-0.938009184552817,-0.935401826011992,-0.930266421810447,
-0.878954944912198,-0.794033865938783,-0.783522167594479,-0.781807752648127,
-0.780968247286719,-0.780310410687896,-0.779569435747449,-0.77831711744584,
-0.773514363053926,-0.737869422258917,-0.693744178714172,-0.626115874048793,
-0.622141206881874,-0.620591626859499,-0.619471990823366,-0.618304254010764,
-0.616767022916174,-0.615072223276405,-0.612258255970519,-0.606561416940706,
-0.591800522012533,-0.556561498511098,-0.473857630813761,-0.461020699778079,
-0.459383220290059,-0.458546695490058,-0.457930384791895,-0.457257522698231,
-0.456320657620648,-0.454079490688016,-0.450987246239434,-0.416950593013296,
-0.37456923187825,-0.350874429196386,-0.303200284114423,-0.299416426494504,
-0.297899091423329,-0.296787779646623,-0.295663857057532,-0.294125059982821,
-0.290864735347415,-0.286588215198992,-0.276563774393582,-0.250721402949624,
-0.142605721723476,-0.137449755167389,-0.136117170556043,-0.1353501552857,
-0.134694950961937,-0.133891441341708,-0.132353129778761,-0.122909554726513,
-0.110769040180773,-0.000958105903751487),.UNSPECIFIED.);
#828=B_SPLINE_CURVE_WITH_KNOTS('',3,(#44559,#44560,#44561,#44562,#44563,
#44564,#44565,#44566,#44567,#44568,#44569,#44570,#44571,#44572,#44573,#44574,
#44575,#44576,#44577,#44578,#44579,#44580,#44581,#44582,#44583,#44584,#44585,
#44586,#44587,#44588,#44589,#44590,#44591,#44592,#44593,#44594,#44595,#44596,
#44597,#44598,#44599,#44600,#44601,#44602,#44603,#44604,#44605,#44606,#44607,
#44608,#44609,#44610,#44611,#44612,#44613,#44614,#44615,#44616,#44617,#44618,
#44619,#44620,#44621,#44622,#44623,#44624,#44625,#44626,#44627,#44628,#44629,
#44630,#44631,#44632,#44633,#44634,#44635,#44636,#44637,#44638,#44639,#44640,
#44641,#44642,#44643,#44644,#44645,#44646,#44647,#44648,#44649,#44650,#44651,
#44652,#44653,#44654,#44655,#44656,#44657,#44658,#44659,#44660,#44661,#44662,
#44663,#44664,#44665,#44666,#44667,#44668,#44669,#44670,#44671,#44672,#44673,
#44674,#44675,#44676,#44677,#44678,#44679,#44680,#44681,#44682,#44683,#44684,
#44685,#44686,#44687,#44688,#44689,#44690,#44691,#44692,#44693,#44694,#44695,
#44696,#44697,#44698,#44699,#44700,#44701,#44702,#44703,#44704,#44705,#44706,
#44707,#44708,#44709,#44710,#44711,#44712,#44713,#44714,#44715,#44716,#44717,
#44718,#44719,#44720,#44721,#44722,#44723,#44724,#44725,#44726,#44727,#44728,
#44729,#44730,#44731,#44732,#44733,#44734,#44735,#44736,#44737,#44738,#44739,
#44740,#44741,#44742,#44743,#44744,#44745,#44746,#44747,#44748,#44749,#44750,
#44751,#44752,#44753,#44754,#44755,#44756,#44757,#44758,#44759,#44760,#44761,
#44762,#44763,#44764,#44765,#44766,#44767,#44768,#44769,#44770,#44771,#44772,
#44773,#44774,#44775,#44776,#44777,#44778,#44779,#44780,#44781,#44782,#44783,
#44784,#44785,#44786,#44787,#44788,#44789,#44790,#44791,#44792,#44793,#44794,
#44795,#44796,#44797,#44798,#44799,#44800,#44801,#44802,#44803,#44804,#44805,
#44806,#44807,#44808,#44809,#44810,#44811,#44812,#44813,#44814,#44815,#44816,
#44817,#44818,#44819,#44820,#44821,#44822,#44823,#44824,#44825,#44826,#44827,
#44828,#44829,#44830,#44831,#44832,#44833,#44834,#44835,#44836,#44837,#44838,
#44839,#44840,#44841,#44842,#44843,#44844,#44845,#44846,#44847,#44848,#44849,
#44850,#44851,#44852,#44853,#44854,#44855,#44856,#44857,#44858,#44859,#44860,
#44861,#44862,#44863,#44864,#44865,#44866,#44867,#44868,#44869,#44870,#44871,
#44872,#44873,#44874,#44875,#44876,#44877,#44878,#44879,#44880,#44881,#44882,
#44883,#44884,#44885,#44886,#44887,#44888,#44889,#44890,#44891,#44892,#44893,
#44894,#44895,#44896,#44897,#44898,#44899,#44900,#44901,#44902,#44903,#44904,
#44905,#44906,#44907,#44908,#44909,#44910,#44911,#44912,#44913,#44914,#44915,
#44916,#44917,#44918,#44919,#44920,#44921,#44922,#44923,#44924,#44925,#44926,
#44927,#44928,#44929,#44930,#44931,#44932,#44933,#44934,#44935,#44936,#44937,
#44938,#44939,#44940,#44941,#44942,#44943,#44944,#44945,#44946,#44947,#44948,
#44949,#44950,#44951,#44952,#44953,#44954,#44955,#44956,#44957,#44958,#44959,
#44960,#44961,#44962,#44963,#44964,#44965,#44966,#44967,#44968,#44969,#44970,
#44971,#44972,#44973,#44974,#44975,#44976,#44977,#44978,#44979,#44980,#44981,
#44982,#44983,#44984,#44985,#44986,#44987,#44988,#44989,#44990,#44991,#44992,
#44993,#44994,#44995,#44996,#44997,#44998,#44999,#45000,#45001,#45002,#45003,
#45004,#45005,#45006,#45007,#45008,#45009,#45010,#45011,#45012,#45013,#45014,
#45015,#45016,#45017,#45018,#45019,#45020,#45021,#45022,#45023,#45024,#45025,
#45026,#45027,#45028,#45029,#45030,#45031,#45032,#45033,#45034,#45035,#45036,
#45037,#45038,#45039,#45040,#45041,#45042,#45043,#45044,#45045,#45046,#45047,
#45048,#45049,#45050,#45051,#45052,#45053,#45054,#45055,#45056,#45057,#45058,
#45059,#45060,#45061,#45062,#45063,#45064,#45065,#45066,#45067,#45068,#45069,
#45070,#45071,#45072,#45073,#45074),.UNSPECIFIED.,.F.,.F.,(4,2,2,2,2,2,
2,2,2,2,2,2,2,2,2,2,2,2,2,2,2,2,2,2,2,2,2,2,2,2,2,2,2,2,2,2,2,2,2,2,2,2,
2,2,2,2,2,2,2,2,2,2,2,2,2,2,2,2,2,2,2,2,2,2,2,2,2,2,2,2,2,2,2,2,2,2,2,2,
2,2,2,2,2,2,2,2,2,2,2,2,2,2,2,2,2,2,2,2,2,2,2,2,2,2,2,2,2,2,2,2,2,2,2,2,
2,2,2,2,2,2,2,2,2,2,2,2,2,2,2,2,2,2,2,2,2,2,2,2,2,2,2,2,2,2,2,2,2,2,2,2,
2,2,2,2,2,2,2,2,2,2,2,2,2,2,2,2,2,2,2,2,2,2,2,2,2,2,2,2,2,2,2,2,2,2,2,2,
2,2,2,2,2,2,2,2,2,2,2,2,2,2,2,2,2,2,2,2,2,2,2,2,2,2,2,2,2,2,2,2,2,2,2,2,
2,2,2,2,2,2,2,2,2,2,2,2,2,2,2,2,2,2,2,2,2,2,2,2,2,2,2,2,2,2,2,2,2,2,2,4),
(-4.06138658790065,-4.04525241163887,-4.03846191229691,-4.03666092753074,
-4.03538999670297,-4.03428943243753,-4.0331563620915,-4.03165174002101,
-4.02869099557283,-4.01127521650964,-4.00463316959338,-3.91388733812666,
-3.88766769835203,-3.87545379763928,-3.8738164497094,-3.87299254319138,
-3.872342181756,-3.87159326005671,-3.87030535664154,-3.86574026801696,-3.77929695118869,
-3.7468547043871,-3.72658633695271,-3.71938768854679,-3.71604271295157,
-3.71337219610962,-3.71195598426428,-3.71078834129195,-3.70961535245074,
-3.70749155857786,-3.70090479208845,-3.64437843326429,-3.62082143422239,
-3.61351181260872,-3.5887119174071,-3.55374002091052,-3.55149054298406,
-3.5505523496365,-3.54987931514528,-3.54926341341319,-3.54842825567468,
-3.5467958593838,-3.53409453311114,-3.53222923279084,-3.44955845594532,
-3.41069222553109,-3.39941376081397,-3.39474637538757,-3.39231497368581,
-3.39025708166305,-3.38897900269922,-3.38785652538869,-3.38637188283222,
-3.38405385564009,-3.37306413002367,-3.27195599684365,-3.25804829741409,
-3.23889995046674,-3.22986700835319,-3.22834700082605,-3.22754752621136,
-3.22689886127196,-3.2262323638511,-3.22498266551041,-3.22076137410961,
-3.14641217631126,-3.10308740060867,-3.07744641362685,-3.07236114234358,
-3.06977232276382,-3.06817146731439,-3.06670352426636,-3.06554545092442,
-3.06440205700285,-3.06276471772964,-3.05823982532329,-2.98177355295227,
-2.93502155321649,-2.91605566486271,-2.90717834065533,-2.90566536383059,
-2.90486737099974,-2.90427622252356,-2.90352901202327,-2.90224887775492,
-2.89775581107323,-2.80095027050559,-2.77708855281743,-2.75144959754393,
-2.74801504644824,-2.74606609070927,-2.74473421884656,-2.74345823526503,
-2.74230323499458,-2.74079960205125,-2.73784371726531,-2.72052292009604,
-2.71943493637124,-2.71399311393548,-2.70338460738783,-2.68299215731286,
-2.61150387683504,-2.58762057446811,-2.58380774021796,-2.58265459193284,
-2.58193582147778,-2.5812722616217,-2.58040456433567,-2.57849643800812,
-2.56324257006605,-2.56284113790527,-2.49424016638539,-2.42646157202313,
-2.4230114609258,-2.42143141735595,-2.42024029680739,-2.41911993282674,
-2.41756753466397,-2.41443190369425,-2.38466755091193,-2.35828764980881,
-2.32971131761324,-2.30384082362538,-2.27349143018919,-2.26203079994999,
-2.26041744615178,-2.2595985131647,-2.25894863630183,-2.25819638136289,
-2.25692628545334,-2.25238598992755,-2.15596388265476,-2.10392345594794,
-2.10039235584378,-2.09879736395309,-2.09760399249313,-2.09648806514285,
-2.09495213124828,-2.0910577185451,-2.03100349848463,-1.94326144648473,
-1.93867924312219,-1.93740466986524,-1.93665135137414,-1.93599531592502,
-1.93517472307456,-1.93355340164878,-1.92184983294585,-1.89525337202058,
-1.82010363391883,-1.81634216012349,-1.78136733622026,-1.77779111100459,
-1.77632369740808,-1.7752250949,-1.77401848331915,-1.77234845688319,-1.76839743106462,
-1.7185592353649,-1.65194598019134,-1.61764235640656,-1.61538917797913,
-1.61451888789625,-1.61389381410069,-1.61322740868621,-1.61232669109436,
-1.61029096919824,-1.57144352511198,-1.47664352940298,-1.47287352042536,
-1.45751080195113,-1.45491704310786,-1.45336545826207,-1.45217467670617,
-1.45089956858808,-1.44890186683498,-1.44267891762859,-1.40746688306336,
-1.30556611214595,-1.29401768875948,-1.29229015591586,-1.29144527636687,
-1.29079797096109,-1.29018433764201,-1.28912711292849,-1.28609385627485,
-1.26980592579601,-1.24821124225988,-1.15252031810644,-1.13487340368952,
-1.13190051483468,-1.13039323847186,-1.12921224291411,-1.1279033092496,
-1.12575438319312,-1.11816714771936,-1.09256378057833,-1.0494813961342,
-0.981977876192697,-0.971243972851883,-0.969553511358955,-0.968716515004169,
-0.968073670182242,-0.96745990049205,-0.966393903719686,-0.963295090148569,
-0.946408748241712,-0.92437473002101,-0.829596135355245,-0.812158646992164,
-0.809196786859625,-0.807691939666551,-0.806511305547638,-0.805201186870975,
-0.803046688473379,-0.795403224139457,-0.769689062514448,-0.74252759107259,
-0.652294086378226,-0.647742400429921,-0.646481593411662,-0.645741227288095,
-0.645086413421815,-0.644455761117519,-0.643133303953209,-0.637483987186614,
-0.553944449314733,-0.49088067354032,-0.486975890216483,-0.485438081575016,
-0.484321564930764,-0.483128287719782,-0.481534671322991,-0.478011706145282,
-0.427749858845276,-0.343769422459311,-0.339033058243669,-0.325887387833028,
-0.324093831314113,-0.323235193404797,-0.3225841284291,-0.321970737394989,
-0.320931437945029,-0.318027856959303,-0.259287722059132,-0.189731327803648,
-0.167066713047837,-0.164150739366711,-0.162654056856414,-0.16154808284931,
-0.160347518212909,-0.15871136463824,-0.154954499626856,-0.0722293716752518,
-0.00817606052254369,-0.00244148803838146,-0.00108799394096062,-0.000957397290290128),
 .UNSPECIFIED.);
#829=B_SPLINE_CURVE_WITH_KNOTS('',3,(#45076,#45077,#45078,#45079,#45080,
#45081,#45082,#45083,#45084,#45085,#45086,#45087,#45088,#45089,#45090,#45091,
#45092,#45093,#45094,#45095,#45096,#45097,#45098,#45099,#45100,#45101,#45102,
#45103,#45104,#45105,#45106,#45107,#45108,#45109,#45110,#45111,#45112,#45113,
#45114,#45115,#45116,#45117,#45118,#45119,#45120,#45121,#45122,#45123,#45124,
#45125,#45126,#45127,#45128,#45129,#45130,#45131,#45132,#45133,#45134,#45135,
#45136,#45137,#45138,#45139,#45140,#45141,#45142,#45143,#45144,#45145,#45146,
#45147,#45148,#45149,#45150,#45151,#45152,#45153,#45154,#45155,#45156,#45157,
#45158,#45159,#45160,#45161,#45162,#45163,#45164,#45165,#45166,#45167,#45168,
#45169,#45170,#45171,#45172,#45173,#45174,#45175,#45176,#45177,#45178,#45179,
#45180,#45181,#45182,#45183,#45184,#45185,#45186,#45187,#45188,#45189,#45190,
#45191,#45192,#45193,#45194,#45195,#45196,#45197,#45198,#45199,#45200,#45201,
#45202,#45203,#45204,#45205,#45206,#45207,#45208,#45209,#45210,#45211,#45212,
#45213,#45214,#45215,#45216,#45217,#45218,#45219,#45220,#45221,#45222,#45223,
#45224,#45225,#45226,#45227,#45228,#45229,#45230,#45231,#45232,#45233,#45234,
#45235,#45236,#45237,#45238,#45239,#45240,#45241,#45242,#45243,#45244,#45245,
#45246,#45247,#45248,#45249,#45250,#45251,#45252,#45253,#45254,#45255,#45256,
#45257,#45258,#45259,#45260,#45261,#45262,#45263,#45264,#45265,#45266,#45267,
#45268,#45269,#45270,#45271,#45272,#45273,#45274,#45275,#45276,#45277,#45278,
#45279,#45280,#45281,#45282,#45283,#45284,#45285,#45286,#45287,#45288,#45289,
#45290,#45291,#45292,#45293,#45294,#45295,#45296,#45297,#45298,#45299,#45300,
#45301,#45302,#45303,#45304,#45305,#45306,#45307,#45308,#45309,#45310,#45311,
#45312,#45313,#45314,#45315,#45316,#45317,#45318,#45319,#45320,#45321,#45322,
#45323,#45324,#45325,#45326,#45327,#45328,#45329,#45330,#45331,#45332,#45333,
#45334,#45335,#45336,#45337,#45338,#45339,#45340,#45341,#45342,#45343,#45344,
#45345,#45346,#45347,#45348,#45349,#45350,#45351,#45352,#45353,#45354,#45355,
#45356,#45357,#45358,#45359,#45360,#45361,#45362,#45363,#45364,#45365,#45366,
#45367,#45368,#45369,#45370,#45371,#45372,#45373,#45374,#45375,#45376,#45377,
#45378,#45379,#45380,#45381,#45382,#45383,#45384,#45385,#45386,#45387,#45388,
#45389,#45390,#45391,#45392,#45393,#45394,#45395,#45396,#45397,#45398,#45399,
#45400,#45401,#45402,#45403,#45404,#45405,#45406,#45407,#45408,#45409,#45410,
#45411,#45412,#45413,#45414,#45415,#45416,#45417,#45418,#45419,#45420,#45421,
#45422,#45423,#45424,#45425,#45426,#45427,#45428,#45429,#45430,#45431,#45432,
#45433,#45434,#45435,#45436,#45437,#45438,#45439,#45440,#45441,#45442,#45443,
#45444,#45445,#45446,#45447,#45448,#45449,#45450,#45451,#45452,#45453,#45454,
#45455,#45456,#45457,#45458,#45459,#45460,#45461,#45462,#45463,#45464,#45465,
#45466,#45467,#45468,#45469,#45470,#45471,#45472,#45473,#45474,#45475,#45476,
#45477,#45478,#45479,#45480,#45481,#45482,#45483,#45484,#45485,#45486,#45487,
#45488,#45489,#45490,#45491,#45492,#45493,#45494,#45495,#45496,#45497,#45498,
#45499,#45500,#45501,#45502,#45503,#45504,#45505,#45506,#45507,#45508,#45509,
#45510,#45511,#45512,#45513,#45514,#45515,#45516,#45517,#45518,#45519,#45520,
#45521,#45522,#45523,#45524,#45525,#45526,#45527,#45528,#45529,#45530,#45531,
#45532,#45533,#45534,#45535,#45536,#45537,#45538,#45539,#45540,#45541,#45542,
#45543,#45544,#45545,#45546,#45547,#45548,#45549,#45550,#45551,#45552,#45553,
#45554,#45555,#45556,#45557,#45558,#45559,#45560,#45561,#45562,#45563,#45564,
#45565,#45566,#45567,#45568,#45569,#45570,#45571,#45572,#45573,#45574,#45575,
#45576,#45577,#45578,#45579,#45580,#45581,#45582,#45583,#45584,#45585,#45586,
#45587,#45588,#45589,#45590,#45591,#45592,#45593,#45594,#45595,#45596,#45597,
#45598,#45599,#45600,#45601,#45602,#45603,#45604,#45605,#45606,#45607,#45608,
#45609),.UNSPECIFIED.,.F.,.F.,(4,2,2,2,2,2,2,2,2,2,2,2,2,2,2,2,2,2,2,2,
2,2,2,2,2,2,2,2,2,2,2,2,2,2,2,2,2,2,2,2,2,2,2,2,2,2,2,2,2,2,2,2,2,2,2,2,
2,2,2,2,2,2,2,2,2,2,2,2,2,2,2,2,2,2,2,2,2,2,2,2,2,2,2,2,2,2,2,2,2,2,2,2,
2,2,2,2,2,2,2,2,2,2,2,2,2,2,2,2,2,2,2,2,2,2,2,2,2,2,2,2,2,2,2,2,2,2,2,2,
2,2,2,2,2,2,2,2,2,2,2,2,2,2,2,2,2,2,2,2,2,2,2,2,2,2,2,2,2,2,2,2,2,2,2,2,
2,2,2,2,2,2,2,2,2,2,2,2,2,2,2,2,2,2,2,2,2,2,2,2,2,2,2,2,2,2,2,2,2,2,2,2,
2,2,2,2,2,2,2,2,2,2,2,2,2,2,2,2,2,2,2,2,2,2,2,2,2,2,2,2,2,2,2,2,2,2,2,2,
2,2,2,2,2,2,2,2,2,2,2,2,2,2,2,2,2,2,2,2,2,2,2,2,2,2,2,2,2,2,4),(-4.06110231792537,
-4.06059741070819,-4.05996580577075,-4.05933590414146,-4.05826813906809,
-4.0554087310575,-4.04937630105949,-3.94277587088132,-3.90832838972063,
-3.90218897453181,-3.90020172041202,-3.89892910673986,-3.89773770683121,
-3.89618109001173,-3.89276351515535,-3.86512999257404,-3.77706897567989,
-3.75790191539855,-3.74601483661137,-3.7397702817228,-3.73878654213019,
-3.73790440067179,-3.73725014548363,-3.7366274668612,-3.73576587196678,
-3.733563234126,-3.70318058322381,-3.69255561533879,-3.67083191200692,-3.66437087297449,
-3.65695814206526,-3.64825416453209,-3.62011616390153,-3.58579194243182,
-3.5796657402366,-3.57767992654376,-3.57640750985249,-3.57521578101949,
-3.57365799694234,-3.57023487072491,-3.54243864676609,-3.47022326564263,
-3.41827233294287,-3.41689595392164,-3.41603294795876,-3.41523744421432,
-3.41459457234492,-3.41383969120689,-3.4125808892788,-3.40804684495158,
-3.32081205913109,-3.26140035644468,-3.25660247897048,-3.25479670490801,
-3.25356324461595,-3.2523629182605,-3.25092593253144,-3.24738571736261,
-3.21561771217929,-3.13063232111741,-3.10529573203479,-3.09492438590364,
-3.09381035386053,-3.09283561624489,-3.09216323351753,-3.09150098794294,
-3.09068364441675,-3.08873501335054,-3.07086385413203,-2.98790742626346,
-2.94192899190128,-2.93460586754559,-2.9324843537103,-2.93118168282318,
-2.9299994918125,-2.92848116572453,-2.92535031368259,-2.90521496225671,
-2.89938169300854,-2.82364872032709,-2.79853250517755,-2.78059361839539,
-2.7721601370065,-2.77109783418148,-2.77036611949277,-2.76966375921583,
-2.76901700678208,-2.76815550911277,-2.76638627477777,-2.75385130888327,
-2.6871097790703,-2.61422968186529,-2.61076723108315,-2.60918503011165,
-2.6079937266623,-2.60687424849963,-2.60532475605336,-2.60220022496166,
-2.57283694244002,-2.48736718002324,-2.45369478931186,-2.45062080994688,
-2.44839031707323,-2.44745538021443,-2.4467829748781,-2.44616640763326,
-2.44532856638664,-2.4436856373655,-2.43068863961419,-2.43002032068448,
-2.42959984484413,-2.42545707184824,-2.42417351647987,-2.4186935107769,
-2.36246464586216,-2.29157434075268,-2.2881161545123,-2.28653469650209,
-2.28534345408835,-2.28422366798839,-2.28267316979721,-2.27954480480314,
-2.25004398139601,-2.20147191609034,-2.1547746321519,-2.13582306906476,
-2.12695367730483,-2.12544128862174,-2.12464351748277,-2.12405249474332,
-2.12330539175791,-2.1220253188847,-2.11753134328931,-2.03168865576719,
-1.96971099301032,-1.96580945938898,-1.96427235728451,-1.96315615354021,
-1.9619630231965,-1.96036928001642,-1.9568447199659,-1.9061529388742,-1.80814635274863,
-1.80374482359099,-1.80247482054093,-1.80172990465991,-1.80113850227119,
-1.8003375129953,-1.79881021647817,-1.78961128900764,-1.77065428408413,
-1.72326988821991,-1.64818516290193,-1.64341894849573,-1.64155967795843,
-1.64043923043578,-1.63924818351396,-1.63766851560675,-1.63422032918383,
-1.56708663846734,-1.492223457132,-1.48179818789063,-1.48008807289792,-1.47924941019955,
-1.47859164268512,-1.47785010948254,-1.47659537088837,-1.47176597658992,
-1.4357416479433,-1.33991695954287,-1.32269957882989,-1.31974922991974,
-1.31824682277088,-1.31709199203695,-1.31581531081975,-1.31448254766303,
-1.3125313911441,-1.30909127835176,-1.28337600732234,-1.25947202550202,
-1.16276358981913,-1.15825399096052,-1.15697202037141,-1.15622437892236,
-1.15563325175887,-1.15483575231578,-1.15332520635122,-1.14450181567692,
-1.1256382856919,-1.07938310532923,-1.00235919364528,-0.997803538136437,
-0.996161493317348,-0.995016770317971,-0.993859025196569,-0.992393788122643,
-0.990796945037483,-0.988217733036795,-0.983158169121833,-0.957365478500339,
-0.913898705315078,-0.839693607501277,-0.835495494522066,-0.834248393551776,
-0.833582378921313,-0.832927341465691,-0.83212402627691,-0.830586056253903,
-0.821143681474916,-0.809178803263304,-0.792924440093603,-0.781210538963257,
-0.696000642247555,-0.693934704437293,-0.677191860501416,-0.674266279491795,
-0.672769072921257,-0.671639867787227,-0.670366718425579,-0.668330683683048,
-0.665931106127077,-0.661347528796306,-0.650341225383484,-0.613416194063387,
-0.517394322672244,-0.512782188437959,-0.511504230423305,-0.51074998977896,
-0.51009384310111,-0.509274003451231,-0.50765702101082,-0.496098177550979,
-0.469378204704691,-0.443954440514808,-0.436901610220834,-0.4128835759767,
-0.355950659448746,-0.352071564871792,-0.350537824893103,-0.349422142178519,
-0.348251680833586,-0.346699304797494,-0.343362176706676,-0.338965634788529,
-0.328560923706869,-0.29976664066489,-0.249535658250077,-0.193171981183607,
-0.189834820803438,-0.188695515824215,-0.188051160826892,-0.187458379460019,
-0.186646159145829,-0.185066063001477,-0.174567135399675,-0.148647967678681,
-0.053616501139824,-0.0469471354448575,-0.0315419778726503,-0.0289453529413174,
-0.0273926669385131,-0.0262014013607221,-0.0251011774085411,-0.0238508068138008,
-0.0221011664640548,-0.019155079023621,-0.00095669269283294),
 .UNSPECIFIED.);
#830=B_SPLINE_CURVE_WITH_KNOTS('',3,(#45611,#45612,#45613,#45614,#45615,
#45616,#45617,#45618,#45619,#45620,#45621,#45622,#45623,#45624,#45625,#45626,
#45627,#45628,#45629,#45630,#45631,#45632,#45633,#45634,#45635,#45636,#45637,
#45638,#45639,#45640,#45641,#45642,#45643,#45644,#45645,#45646,#45647,#45648,
#45649,#45650,#45651,#45652,#45653,#45654,#45655,#45656,#45657,#45658,#45659,
#45660,#45661,#45662,#45663,#45664,#45665,#45666,#45667,#45668,#45669,#45670,
#45671,#45672,#45673,#45674,#45675,#45676,#45677,#45678,#45679,#45680,#45681,
#45682,#45683,#45684,#45685,#45686,#45687,#45688,#45689,#45690,#45691,#45692,
#45693,#45694,#45695,#45696,#45697,#45698,#45699,#45700,#45701,#45702,#45703,
#45704,#45705,#45706,#45707,#45708,#45709,#45710,#45711,#45712,#45713,#45714,
#45715,#45716,#45717,#45718,#45719,#45720,#45721,#45722,#45723,#45724,#45725,
#45726,#45727,#45728,#45729,#45730,#45731,#45732,#45733,#45734,#45735,#45736,
#45737,#45738,#45739,#45740,#45741,#45742,#45743,#45744,#45745,#45746,#45747,
#45748,#45749,#45750,#45751,#45752,#45753,#45754,#45755,#45756,#45757,#45758,
#45759,#45760,#45761,#45762,#45763,#45764,#45765,#45766,#45767,#45768,#45769,
#45770,#45771,#45772,#45773,#45774,#45775,#45776,#45777,#45778,#45779,#45780,
#45781,#45782,#45783,#45784,#45785,#45786,#45787,#45788,#45789,#45790,#45791,
#45792,#45793,#45794,#45795,#45796,#45797,#45798,#45799,#45800,#45801,#45802,
#45803,#45804,#45805,#45806,#45807,#45808,#45809,#45810,#45811,#45812,#45813,
#45814,#45815,#45816,#45817,#45818,#45819,#45820,#45821,#45822,#45823,#45824,
#45825,#45826,#45827,#45828,#45829,#45830,#45831,#45832,#45833,#45834,#45835,
#45836,#45837,#45838,#45839,#45840,#45841,#45842,#45843,#45844,#45845,#45846,
#45847,#45848,#45849,#45850,#45851,#45852,#45853,#45854,#45855,#45856,#45857,
#45858,#45859,#45860,#45861,#45862,#45863,#45864,#45865,#45866,#45867,#45868,
#45869,#45870,#45871,#45872,#45873,#45874,#45875,#45876,#45877,#45878,#45879,
#45880,#45881,#45882,#45883,#45884,#45885,#45886,#45887,#45888,#45889,#45890,
#45891,#45892,#45893,#45894,#45895,#45896,#45897,#45898,#45899,#45900,#45901,
#45902,#45903,#45904,#45905,#45906,#45907,#45908,#45909,#45910,#45911,#45912,
#45913,#45914,#45915,#45916,#45917,#45918,#45919,#45920,#45921,#45922,#45923,
#45924,#45925,#45926,#45927,#45928,#45929,#45930,#45931,#45932,#45933,#45934,
#45935,#45936,#45937,#45938,#45939,#45940,#45941,#45942,#45943,#45944,#45945,
#45946,#45947,#45948,#45949,#45950,#45951,#45952,#45953,#45954,#45955,#45956,
#45957,#45958,#45959,#45960,#45961,#45962,#45963,#45964,#45965,#45966,#45967,
#45968,#45969,#45970,#45971,#45972,#45973,#45974,#45975,#45976,#45977,#45978,
#45979,#45980,#45981,#45982,#45983,#45984,#45985,#45986,#45987,#45988,#45989,
#45990,#45991,#45992,#45993,#45994,#45995,#45996,#45997,#45998,#45999,#46000,
#46001,#46002,#46003,#46004,#46005,#46006,#46007,#46008,#46009,#46010,#46011,
#46012,#46013,#46014,#46015,#46016,#46017,#46018,#46019,#46020,#46021,#46022,
#46023,#46024,#46025,#46026,#46027,#46028,#46029,#46030,#46031,#46032,#46033,
#46034,#46035,#46036,#46037,#46038,#46039,#46040,#46041,#46042,#46043,#46044,
#46045,#46046,#46047,#46048,#46049,#46050,#46051,#46052,#46053,#46054,#46055,
#46056,#46057,#46058,#46059,#46060,#46061,#46062,#46063,#46064,#46065,#46066,
#46067,#46068,#46069,#46070,#46071,#46072,#46073,#46074,#46075,#46076,#46077,
#46078,#46079,#46080,#46081,#46082,#46083,#46084,#46085,#46086,#46087,#46088,
#46089,#46090,#46091,#46092,#46093,#46094,#46095,#46096,#46097,#46098,#46099,
#46100,#46101,#46102,#46103,#46104,#46105,#46106,#46107,#46108,#46109,#46110,
#46111,#46112,#46113,#46114,#46115,#46116,#46117,#46118,#46119,#46120,#46121,
#46122,#46123,#46124,#46125,#46126,#46127,#46128,#46129,#46130,#46131,#46132,
#46133,#46134,#46135,#46136,#46137,#46138,#46139,#46140,#46141,#46142,#46143,
#46144,#46145,#46146,#46147,#46148,#46149,#46150,#46151,#46152,#46153,#46154,
#46155,#46156,#46157,#46158,#46159,#46160,#46161,#46162,#46163,#46164,#46165,
#46166),.UNSPECIFIED.,.F.,.F.,(4,2,2,2,2,2,2,2,2,2,2,2,2,2,2,2,2,2,2,2,
2,2,2,2,2,2,2,2,2,2,2,2,2,2,2,2,2,2,2,2,2,2,2,2,2,2,2,2,2,2,2,2,2,2,2,2,
2,2,2,2,2,2,2,2,2,2,2,2,2,2,2,2,2,2,2,2,2,2,2,2,2,2,2,2,2,2,2,2,2,2,2,2,
2,2,2,2,2,2,2,2,2,2,2,2,2,2,2,2,2,2,2,2,2,2,2,2,2,2,2,2,2,2,2,2,2,2,2,2,
2,2,2,2,2,2,2,2,2,2,2,2,2,2,2,2,2,2,2,2,2,2,2,2,2,2,2,2,2,2,2,2,2,2,2,2,
2,2,2,2,2,2,2,2,2,2,2,2,2,2,2,2,2,2,2,2,2,2,2,2,2,2,2,2,2,2,2,2,2,2,2,2,
2,2,2,2,2,2,2,2,2,2,2,2,2,2,2,2,2,2,2,2,2,2,2,2,2,2,2,2,2,2,2,2,2,2,2,2,
2,2,2,2,2,2,2,2,2,2,2,2,2,2,2,2,2,2,2,2,2,2,2,2,2,2,2,2,2,2,2,2,2,2,2,2,
2,2,2,2,2,4),(-4.0605457412234,-3.95495941481507,-3.93605529689604,-3.92721261541421,
-3.92570135227873,-3.92490377647833,-3.92431272510179,-3.92366118587011,
-3.92248546477351,-3.91886818171779,-3.85821424937071,-3.80958345116075,
-3.78440016141353,-3.77371376972052,-3.76922939015871,-3.76584033044454,
-3.76427722502882,-3.76310532795215,-3.76199310489736,-3.76047177328619,
-3.75666378541168,-3.70702156991851,-3.68142349363787,-3.63212488138626,
-3.61340035922391,-3.60464695455006,-3.60313982719317,-3.60234313118875,
-3.6017521635418,-3.6010041380274,-3.599720108492,-3.59519036891763,-3.50103821214206,
-3.4674935331529,-3.45311739894622,-3.44753063720286,-3.4447568329863,-3.44307879429006,
-3.44156915823026,-3.44040208399134,-3.43928163976136,-3.43772864791244,
-3.43373254322522,-3.36580403816991,-3.32035709763325,-3.28619006579357,
-3.28149517993135,-3.28025277480128,-3.27951407625275,-3.27885592000855,
-3.2780128624221,-3.27628033052043,-3.26540002771946,-3.18084688690849,
-3.12963207179594,-3.12450159442338,-3.12189607550668,-3.12028833303438,
-3.11881504912169,-3.1176575248148,-3.11651662893626,-3.11488782789022,
-3.11041759778343,-3.03501358337079,-2.98753685354794,-2.96838463685861,
-2.95933030812582,-2.95780956317301,-2.95701002650281,-2.95641884002651,
-2.95567305433016,-2.95439886470307,-2.94995849008219,-2.85235244396182,
-2.80636117448341,-2.80153098738271,-2.79903805153858,-2.79747759034302,
-2.79603744803748,-2.79488308071807,-2.79372680612787,-2.79168527657539,
-2.78570850087434,-2.68101841539463,-2.65204860258694,-2.63682145768169,
-2.63510579681138,-2.63426609524447,-2.63366982354743,-2.6330375626047,
-2.63214053437816,-2.62971705181821,-2.62838360526375,-2.57111421107401,
-2.52129948201764,-2.50144384006515,-2.47784068896493,-2.47486215488716,
-2.47337432032641,-2.47230619697623,-2.47117717034562,-2.46959218536517,
-2.46632492806459,-2.43107980335647,-2.36283488955639,-2.34216953783651,
-2.32301471011016,-2.3139443231393,-2.31242276755273,-2.31162301916312,
-2.31097441051002,-2.31030821754058,-2.30905979838784,-2.30484887839261,
-2.23058927259819,-2.18721893608051,-2.16146923462119,-2.1538047600535,
-2.15164811237091,-2.15033748927902,-2.14915691955492,-2.14765286726362,
-2.14469482349819,-2.12733099566277,-2.12380863786516,-2.03050706077327,
-2.00448716407665,-1.99171874193385,-1.99008379879637,-1.98924794756592,
-1.98863183023296,-1.98795886582634,-1.98702130744568,-1.98477588633959,
-1.98167619965725,-1.94748355837829,-1.87031765955104,-1.86623396982405,
-1.8564347390615,-1.8512016785329,-1.84955458623469,-1.83252383751663,-1.8295832664142,
-1.82808288913795,-1.82690264967444,-1.82558975378762,-1.82342329244579,
-1.81566172260695,-1.76482143772875,-1.68339801706031,-1.68240981448849,
-1.68074183692639,-1.66895912088893,-1.66718531308258,-1.66633397738605,
-1.66567472245422,-1.66494045377003,-1.66371830352068,-1.65924062390827,
-1.62787615169194,-1.53574800671381,-1.53007716391375,-1.50999702229069,
-1.50686822955255,-1.50535013796723,-1.50416778437731,-1.50286458428999,
-1.50074142192853,-1.49340505481238,-1.44728282375824,-1.35816464610307,
-1.34617961392421,-1.34439693098774,-1.34355296614099,-1.34289282968718,
-1.34217692863619,-1.34101378341309,-1.33962671722753,-1.33692836280511,
-1.31023881101801,-1.23992340099507,-1.18842429058249,-1.18459442000821,
-1.18306921381325,-1.18195587723007,-1.18076036198855,-1.17915397509614,
-1.17556241757058,-1.17078787472338,-1.12571707123542,-1.04241426828205,
-1.0400186392906,-1.03735999983631,-1.03693121703044,-1.03546018938973,
-1.02345391881338,-1.02167022790515,-1.02082603295498,-1.02016582700799,
-1.01955119947373,-1.01848230681004,-1.01534964374975,-0.998004841984789,
-0.979774025687205,-0.929382224820403,-0.865817219792452,-0.861910648978565,
-0.86037232695504,-0.859255504045153,-0.858061961801052,-0.856468098664971,
-0.852945024212992,-0.802814543466148,-0.735058523114656,-0.723450420410497,
-0.717572148309861,-0.716579692962732,-0.715091123950269,-0.714402455123496,
-0.713493952462066,-0.7008111751004,-0.699179115564311,-0.698343923447362,
-0.697727894595342,-0.697054615184667,-0.696134801679296,-0.693981909072773,
-0.691014472993845,-0.683411980673527,-0.668764816073677,-0.626851623497077,
-0.544816326077868,-0.539653895849157,-0.537731260439277,-0.536598291095981,
-0.535531231102925,-0.534052474615969,-0.531119627625107,-0.509160075740331,
-0.480584905678525,-0.472919564824374,-0.421344772650733,-0.379062284009604,
-0.376646090636205,-0.375749909188097,-0.375117766447727,-0.37452119778218,
-0.37388198845198,-0.373061440047274,-0.369788544786334,-0.364740988205064,
-0.348971260915309,-0.316617121280693,-0.241013005218912,-0.239368640393978,
-0.23375366102006,-0.218721242931479,-0.216145015309578,-0.214598376534375,
-0.21340811279378,-0.212130342967928,-0.210121747339512,-0.203811403693268,
-0.167800535756291,-0.13390336521264,-0.119119785035649,-0.111456026177537,
-0.102609890371343,-0.0568649904542864,-0.0541277106612172,-0.0531836123562101,
-0.0525382162060769,-0.0519458039985288,-0.0513151666505216,-0.0505224083733557,
-0.0493137674931764,-0.0470833369860782,-0.000956627395017071),
 .UNSPECIFIED.);
#831=B_SPLINE_CURVE_WITH_KNOTS('',3,(#46168,#46169,#46170,#46171,#46172,
#46173,#46174,#46175,#46176,#46177,#46178,#46179,#46180,#46181,#46182,#46183,
#46184,#46185,#46186,#46187,#46188,#46189,#46190,#46191,#46192,#46193,#46194,
#46195,#46196,#46197,#46198,#46199,#46200,#46201,#46202,#46203,#46204,#46205,
#46206,#46207,#46208,#46209,#46210,#46211,#46212,#46213,#46214,#46215,#46216,
#46217,#46218,#46219,#46220,#46221,#46222,#46223,#46224,#46225,#46226,#46227,
#46228,#46229,#46230,#46231,#46232,#46233,#46234,#46235,#46236,#46237,#46238,
#46239,#46240,#46241,#46242,#46243,#46244,#46245,#46246,#46247,#46248,#46249,
#46250,#46251,#46252,#46253,#46254,#46255,#46256,#46257,#46258,#46259,#46260,
#46261,#46262,#46263,#46264,#46265,#46266,#46267,#46268,#46269,#46270,#46271,
#46272,#46273,#46274,#46275,#46276,#46277,#46278,#46279,#46280,#46281,#46282,
#46283,#46284,#46285,#46286,#46287,#46288,#46289,#46290,#46291,#46292,#46293,
#46294,#46295,#46296,#46297,#46298,#46299,#46300,#46301,#46302,#46303,#46304,
#46305,#46306,#46307,#46308,#46309,#46310,#46311,#46312,#46313,#46314,#46315,
#46316,#46317,#46318,#46319,#46320,#46321,#46322,#46323,#46324,#46325,#46326,
#46327,#46328,#46329,#46330,#46331,#46332,#46333,#46334,#46335,#46336,#46337,
#46338,#46339,#46340,#46341,#46342,#46343,#46344,#46345,#46346,#46347,#46348,
#46349,#46350,#46351,#46352,#46353,#46354,#46355,#46356,#46357,#46358,#46359,
#46360,#46361,#46362,#46363,#46364,#46365,#46366,#46367,#46368,#46369,#46370,
#46371,#46372,#46373,#46374,#46375,#46376,#46377,#46378,#46379,#46380,#46381,
#46382,#46383,#46384,#46385,#46386,#46387,#46388,#46389,#46390,#46391,#46392,
#46393,#46394,#46395,#46396,#46397,#46398,#46399,#46400,#46401,#46402,#46403,
#46404,#46405,#46406,#46407,#46408,#46409,#46410,#46411,#46412,#46413,#46414,
#46415,#46416,#46417,#46418,#46419,#46420,#46421,#46422,#46423,#46424,#46425,
#46426,#46427,#46428,#46429,#46430,#46431,#46432,#46433,#46434,#46435,#46436,
#46437,#46438,#46439,#46440,#46441,#46442,#46443,#46444,#46445,#46446,#46447,
#46448,#46449,#46450,#46451,#46452,#46453,#46454,#46455,#46456,#46457,#46458,
#46459,#46460,#46461,#46462,#46463,#46464,#46465,#46466,#46467,#46468,#46469,
#46470,#46471,#46472,#46473,#46474,#46475,#46476,#46477,#46478,#46479,#46480,
#46481,#46482,#46483,#46484,#46485,#46486,#46487,#46488,#46489,#46490,#46491,
#46492,#46493,#46494,#46495,#46496,#46497,#46498,#46499,#46500,#46501,#46502,
#46503,#46504,#46505,#46506,#46507,#46508,#46509,#46510,#46511,#46512,#46513,
#46514,#46515,#46516,#46517,#46518,#46519,#46520,#46521,#46522,#46523,#46524,
#46525,#46526,#46527,#46528,#46529,#46530,#46531,#46532,#46533,#46534,#46535,
#46536,#46537,#46538,#46539,#46540,#46541,#46542,#46543,#46544,#46545,#46546,
#46547,#46548,#46549,#46550,#46551,#46552,#46553,#46554,#46555,#46556,#46557,
#46558,#46559,#46560,#46561,#46562,#46563,#46564,#46565,#46566,#46567,#46568,
#46569,#46570,#46571,#46572,#46573,#46574,#46575,#46576,#46577,#46578,#46579,
#46580,#46581,#46582,#46583,#46584,#46585,#46586,#46587,#46588,#46589,#46590,
#46591,#46592,#46593,#46594,#46595,#46596,#46597,#46598,#46599,#46600,#46601,
#46602,#46603,#46604,#46605,#46606,#46607,#46608,#46609,#46610,#46611,#46612,
#46613,#46614,#46615,#46616,#46617,#46618,#46619,#46620,#46621,#46622,#46623,
#46624,#46625,#46626,#46627,#46628,#46629,#46630,#46631,#46632,#46633,#46634,
#46635,#46636,#46637,#46638,#46639,#46640,#46641,#46642,#46643,#46644,#46645,
#46646,#46647,#46648,#46649,#46650,#46651,#46652,#46653,#46654,#46655,#46656,
#46657,#46658,#46659,#46660,#46661,#46662,#46663,#46664,#46665,#46666,#46667,
#46668,#46669,#46670,#46671,#46672,#46673,#46674,#46675,#46676,#46677,#46678,
#46679,#46680,#46681,#46682,#46683,#46684,#46685,#46686,#46687,#46688,#46689,
#46690,#46691,#46692,#46693,#46694,#46695,#46696,#46697,#46698,#46699,#46700,
#46701,#46702,#46703,#46704,#46705,#46706,#46707,#46708,#46709,#46710,#46711,
#46712,#46713,#46714,#46715,#46716,#46717,#46718,#46719,#46720,#46721),
 .UNSPECIFIED.,.F.,.F.,(4,2,2,2,2,2,2,2,2,2,2,2,2,2,2,2,2,2,2,2,2,2,2,2,
2,2,2,2,2,2,2,2,2,2,2,2,2,2,2,2,2,2,2,2,2,2,2,2,2,2,2,2,2,2,2,2,2,2,2,2,
2,2,2,2,2,2,2,2,2,2,2,2,2,2,2,2,2,2,2,2,2,2,2,2,2,2,2,2,2,2,2,2,2,2,2,2,
2,2,2,2,2,2,2,2,2,2,2,2,2,2,2,2,2,2,2,2,2,2,2,2,2,2,2,2,2,2,2,2,2,2,2,2,
2,2,2,2,2,2,2,2,2,2,2,2,2,2,2,2,2,2,2,2,2,2,2,2,2,2,2,2,2,2,2,2,2,2,2,2,
2,2,2,2,2,2,2,2,2,2,2,2,2,2,2,2,2,2,2,2,2,2,2,2,2,2,2,2,2,2,2,2,2,2,2,2,
2,2,2,2,2,2,2,2,2,2,2,2,2,2,2,2,2,2,2,2,2,2,2,2,2,2,2,2,2,2,2,2,2,2,2,2,
2,2,2,2,2,2,2,2,2,2,2,2,2,2,2,2,2,2,2,2,2,2,2,2,2,2,2,2,2,2,2,2,2,2,2,2,
4),(-4.0609788184019,-4.00866642356526,-3.9622189686826,-3.95485125516697,
-3.95272487499133,-3.95142098668034,-3.95023885368475,-3.94872222297658,
-3.94560061967941,-3.92567577860323,-3.91910962273465,-3.84451357365953,
-3.82463915663187,-3.79644211610828,-3.7919166627445,-3.79101266772559,
-3.79034399343397,-3.78967113518626,-3.78905495559564,-3.78821879227068,
-3.78658256831569,-3.77377743525769,-3.74567300673567,-3.7172947752388,
-3.69104820239805,-3.64012326544441,-3.63235344849039,-3.63018614150046,
-3.62887303918123,-3.62769281099133,-3.62619271709054,-3.62325354357833,
-3.60624935277244,-3.60508574413159,-3.53550558301462,-3.50395737138832,
-3.48297147628572,-3.47008198186087,-3.46843116320325,-3.46776383146117,
-3.46709174279417,-3.46647460408832,-3.46563474528434,-3.46355990069386,
-3.44052065177945,-3.42835541185941,-3.36348567029141,-3.31702672563774,
-3.30965775158974,-3.30753115721253,-3.30622717043367,-3.30504496974713,
-3.30352828225823,-3.3004066686601,-3.28048454713631,-3.27493716517512,
-3.2693006994607,-3.22139689263948,-3.16890801158127,-3.1543342565617,-3.1495700940871,
-3.14644015973378,-3.14537195735264,-3.14475745351601,-3.14409732184783,
-3.14325295577327,-3.14146791333144,-3.12942523191849,-3.1279904141707,
-3.12756547711261,-3.12493694457629,-3.11918479294339,-3.04050216464289,
-2.99436248242678,-2.98702362337251,-2.98490022564278,-2.98359698786865,
-2.98241467026504,-2.9808967227992,-2.97776857532028,-2.95770133269436,
-2.95147453944668,-2.87551111338551,-2.82649084827573,-2.82458055885322,
-2.82306933193775,-2.82227626629028,-2.82168394016734,-2.82103846324157,
-2.81989304668468,-2.81650428737606,-2.75605169087254,-2.70782513030004,
-2.69049533933717,-2.66836959595389,-2.66368090849853,-2.66189131865701,
-2.66066098283838,-2.65945751856181,-2.65800933952221,-2.65440284857104,
-2.62014814612835,-2.5554966661241,-2.5028793287234,-2.50075551801354,-2.49983898739581,
-2.49916981475595,-2.49854879982022,-2.49769405472408,-2.49598493500843,
-2.48103202026078,-2.47938604794757,-2.47724620682195,-2.46724122118361,
-2.3953263364527,-2.3490772991632,-2.34172791400156,-2.33960331099505,-2.33829973890291,
-2.33711738442581,-2.33559976116754,-2.33247360129391,-2.31245379295056,
-2.30685210527078,-2.29928541322426,-2.21216400881897,-2.18923797233965,
-2.17930383630521,-2.1777456102822,-2.17693802458532,-2.17628275195416,
-2.17561929287301,-2.17438493261303,-2.17029619948591,-2.09733814828702,
-2.05323732778228,-2.03115804564348,-2.01987506424795,-2.01753554792348,
-2.01604405972935,-2.01486464943839,-2.01354625058169,-2.0113557603419,
-2.00335045118365,-1.94957367917654,-1.90234606560747,-1.85842438290727,
-1.855688818845,-1.8547449541557,-1.85409961332037,-1.85350716850772,-1.85269726983292,
-1.85112798255955,-1.84091089063801,-1.81633934729496,-1.74554443504995,
-1.73456767888231,-1.69886672991483,-1.69558865124381,-1.69400082012411,
-1.69287085927456,-1.69180274295321,-1.69031633837819,-1.68734586074425,
-1.66406133114606,-1.64421743627329,-1.59451983909221,-1.53659719867375,
-1.53532427031233,-1.53291838693435,-1.53202365053207,-1.53139191046668,
-1.5307951968944,-1.52995341029328,-1.52822798223787,-1.51257067267507,
-1.497970204683,-1.39688420716353,-1.39533186032094,-1.37531188201319,-1.37218578383384,
-1.37066820848688,-1.36948589939231,-1.36818238550509,-1.3661003402545,
-1.35909700605417,-1.31616034360945,-1.2432399876416,-1.2122600926433,-1.2100485282218,
-1.20918513583259,-1.20856185162933,-1.20789422535592,-1.20698658023976,
-1.20500534478483,-1.18124167263197,-1.15817381780203,-1.08687740829314,
-1.07631694061834,-1.07095763301991,-1.0697347942762,-1.06881936404228,
-1.05237711931534,-1.04972624040801,-1.04815771076098,-1.046963934731,-1.04569528308365,
-1.0437668637843,-1.03807131887419,-1.00732914871179,-0.941998861679551,
-0.901176518104308,-0.888945650466202,-0.887331016101719,-0.886500371624823,
-0.885885552575492,-0.885211362260221,-0.884267418257439,-0.882048584492347,
-0.861312534551039,-0.840358333536931,-0.783870125826784,-0.73122869800768,
-0.727387367122493,-0.725860220365159,-0.724746391537273,-0.723551221274738,
-0.722377237264457,-0.71962537544249,-0.702558799711768,-0.663949053345918,
-0.626101853298485,-0.568650044098605,-0.565226594825065,-0.564076136958853,
-0.563429622347094,-0.562837485490563,-0.562030072562951,-0.561166054812463,
-0.557281884264004,-0.482338907568888,-0.456611693894247,-0.438171115204648,
-0.429792806267884,-0.423959576314824,-0.407158322533423,-0.40422941604127,
-0.402731467374079,-0.401551403795752,-0.400236905419175,-0.398879849102493,
-0.394344100034094,-0.387899407240713,-0.370455320918639,-0.340726568160529,
-0.315917526678635,-0.246441876297017,-0.242669182214931,-0.241473342321605,
-0.240817664224122,-0.24016770932153,-0.239349317046014,-0.238470025158611,
-0.237054895837823,-0.22200306052267,-0.185840048669332,-0.171380597991612,
-0.156037810867822,-0.0867025073468892,-0.082337101894122,-0.0807241987399237,
-0.0795874328015257,-0.0785217481162206,-0.0770526634393246,-0.075479676809945,
-0.0729574043667461,-0.000957116809526677),.UNSPECIFIED.);
#832=B_SPLINE_CURVE_WITH_KNOTS('',3,(#46723,#46724,#46725,#46726,#46727,
#46728,#46729,#46730,#46731,#46732,#46733),.UNSPECIFIED.,.F.,.F.,(4,1,1,
1,1,1,1,1,4),(210.486707790517,210.519097345163,211.517889748931,212.516682152699,
213.515474556467,214.514266960235,215.513059364003,216.511851767771,216.769890768902),
 .UNSPECIFIED.);
#833=B_SPLINE_CURVE_WITH_KNOTS('',3,(#46735,#46736,#46737,#46738,#46739,
#46740,#46741,#46742,#46743,#46744,#46745,#46746,#46747,#46748,#46749,#46750,
#46751,#46752,#46753,#46754,#46755,#46756,#46757,#46758,#46759,#46760,#46761,
#46762,#46763,#46764,#46765,#46766,#46767,#46768,#46769,#46770,#46771,#46772,
#46773,#46774,#46775,#46776,#46777,#46778,#46779,#46780,#46781,#46782,#46783,
#46784,#46785,#46786,#46787,#46788,#46789,#46790,#46791,#46792,#46793,#46794,
#46795,#46796,#46797,#46798,#46799,#46800,#46801,#46802,#46803,#46804,#46805,
#46806,#46807,#46808,#46809,#46810,#46811,#46812,#46813,#46814,#46815,#46816,
#46817,#46818,#46819,#46820,#46821,#46822,#46823,#46824,#46825,#46826,#46827,
#46828,#46829,#46830,#46831,#46832,#46833,#46834,#46835,#46836,#46837,#46838,
#46839,#46840,#46841,#46842,#46843,#46844,#46845,#46846,#46847,#46848,#46849,
#46850,#46851,#46852,#46853,#46854,#46855,#46856,#46857,#46858,#46859,#46860,
#46861,#46862,#46863,#46864,#46865,#46866,#46867,#46868,#46869,#46870,#46871,
#46872,#46873,#46874,#46875,#46876,#46877,#46878,#46879,#46880,#46881,#46882,
#46883,#46884,#46885,#46886,#46887,#46888,#46889,#46890,#46891,#46892,#46893,
#46894,#46895,#46896,#46897,#46898,#46899,#46900,#46901,#46902,#46903,#46904,
#46905,#46906,#46907,#46908,#46909,#46910,#46911,#46912,#46913,#46914,#46915,
#46916,#46917,#46918,#46919,#46920,#46921,#46922,#46923,#46924,#46925,#46926,
#46927,#46928,#46929,#46930,#46931,#46932,#46933,#46934,#46935,#46936,#46937,
#46938,#46939,#46940,#46941,#46942,#46943,#46944,#46945,#46946,#46947,#46948,
#46949,#46950,#46951,#46952,#46953,#46954,#46955,#46956,#46957,#46958,#46959,
#46960,#46961,#46962,#46963,#46964,#46965,#46966,#46967,#46968,#46969,#46970,
#46971,#46972,#46973,#46974,#46975,#46976,#46977,#46978,#46979,#46980,#46981,
#46982,#46983,#46984,#46985,#46986,#46987,#46988,#46989,#46990,#46991,#46992,
#46993,#46994,#46995,#46996,#46997,#46998,#46999,#47000,#47001,#47002,#47003,
#47004,#47005,#47006,#47007,#47008,#47009,#47010,#47011,#47012,#47013,#47014,
#47015,#47016,#47017,#47018,#47019,#47020,#47021,#47022,#47023,#47024,#47025,
#47026,#47027,#47028,#47029,#47030,#47031,#47032,#47033,#47034,#47035,#47036,
#47037,#47038,#47039,#47040,#47041,#47042,#47043,#47044,#47045,#47046,#47047,
#47048,#47049,#47050,#47051,#47052,#47053,#47054,#47055,#47056,#47057,#47058,
#47059,#47060,#47061,#47062,#47063,#47064,#47065,#47066,#47067,#47068,#47069,
#47070,#47071,#47072,#47073,#47074,#47075,#47076,#47077,#47078,#47079,#47080,
#47081,#47082,#47083,#47084,#47085,#47086,#47087,#47088,#47089,#47090,#47091,
#47092,#47093,#47094,#47095,#47096,#47097,#47098,#47099,#47100,#47101,#47102,
#47103,#47104,#47105,#47106,#47107,#47108,#47109,#47110,#47111,#47112,#47113,
#47114,#47115,#47116,#47117,#47118,#47119,#47120,#47121,#47122,#47123,#47124,
#47125,#47126,#47127,#47128,#47129,#47130,#47131,#47132,#47133,#47134,#47135,
#47136,#47137,#47138,#47139,#47140,#47141,#47142,#47143,#47144,#47145,#47146,
#47147,#47148,#47149,#47150,#47151,#47152,#47153,#47154,#47155,#47156,#47157,
#47158,#47159,#47160,#47161,#47162,#47163,#47164,#47165,#47166,#47167,#47168,
#47169,#47170,#47171,#47172,#47173,#47174,#47175,#47176,#47177,#47178,#47179,
#47180,#47181,#47182,#47183,#47184,#47185,#47186,#47187,#47188,#47189,#47190,
#47191,#47192,#47193,#47194,#47195,#47196,#47197,#47198,#47199,#47200,#47201,
#47202,#47203,#47204,#47205,#47206,#47207,#47208,#47209,#47210,#47211,#47212,
#47213,#47214,#47215,#47216,#47217,#47218,#47219,#47220,#47221,#47222,#47223,
#47224,#47225,#47226,#47227,#47228,#47229,#47230,#47231,#47232,#47233,#47234,
#47235,#47236,#47237,#47238,#47239,#47240,#47241,#47242,#47243,#47244,#47245,
#47246,#47247,#47248,#47249,#47250,#47251,#47252,#47253,#47254,#47255,#47256,
#47257,#47258,#47259,#47260,#47261,#47262,#47263,#47264,#47265,#47266),
 .UNSPECIFIED.,.F.,.F.,(4,2,2,2,2,2,2,2,2,2,2,2,2,2,2,2,2,2,2,2,2,2,2,2,
2,2,2,2,2,2,2,2,2,2,2,2,2,2,2,2,2,2,2,2,2,2,2,2,2,2,2,2,2,2,2,2,2,2,2,2,
2,2,2,2,2,2,2,2,2,2,2,2,2,2,2,2,2,2,2,2,2,2,2,2,2,2,2,2,2,2,2,2,2,2,2,2,
2,2,2,2,2,2,2,2,2,2,2,2,2,2,2,2,2,2,2,2,2,2,2,2,2,2,2,2,2,2,2,2,2,2,2,2,
2,2,2,2,2,2,2,2,2,2,2,2,2,2,2,2,2,2,2,2,2,2,2,2,2,2,2,2,2,2,2,2,2,2,2,2,
2,2,2,2,2,2,2,2,2,2,2,2,2,2,2,2,2,2,2,2,2,2,2,2,2,2,2,2,2,2,2,2,2,2,2,2,
2,2,2,2,2,2,2,2,2,2,2,2,2,2,2,2,2,2,2,2,2,2,2,2,2,2,2,2,2,2,2,2,2,2,2,2,
2,2,2,2,2,2,2,2,2,2,2,2,2,2,2,2,2,2,2,2,2,2,2,2,2,4),(-4.06174778365555,
-3.97407821427973,-3.93332815143193,-3.91576821953131,-3.91298827734529,
-3.91154176535403,-3.91047944312257,-3.90933381163376,-3.90768726084685,
-3.90309868088443,-3.90128705189473,-3.7968662166107,-3.77197426577817,
-3.75865740411268,-3.75419547490943,-3.75219036244142,-3.75107047055428,
-3.75031492793865,-3.74959590326309,-3.7489536188135,-3.74811123050883,
-3.74638173034892,-3.73554974641793,-3.73145347876651,-3.69061690225986,
-3.65180739794179,-3.61077431393014,-3.5931511537124,-3.59036829280424,
-3.58892100383195,-3.58785841927253,-3.58671280138022,-3.58506677492246,
-3.58048288141944,-3.57866526790208,-3.47171092280664,-3.44887812563339,
-3.43586500901309,-3.43147681479097,-3.42949603870758,-3.42838576007372,
-3.42763415577764,-3.42691790025777,-3.42627459984244,-3.42542666417021,
-3.42366972755144,-3.41226049279543,-3.3599373194685,-3.30233937946984,
-3.27682592065431,-3.2692802519617,-3.26713555588305,-3.26582757352176,
-3.26464637963791,-3.26313739178246,-3.26015648102918,-3.24235272231414,
-3.23641911176208,-3.22600132007023,-3.1387927937191,-3.11041445780607,
-3.10761965763419,-3.10619673734846,-3.10531421854298,-3.10450467607211,
-3.10386166914311,-3.10311693510834,-3.1018479120146,-3.09745577830531,
-3.01488994575547,-2.94869918100383,-2.94525399451907,-2.94367485250364,
-2.94248385015836,-2.94136318498728,-2.93980971388008,-2.93666986684746,
-2.90674795862577,-2.89987802721406,-2.81529709026957,-2.78758407885472,
-2.78482697181267,-2.78341803867974,-2.78254135301491,-2.78173594099039,
-2.78109296749668,-2.78034521141131,-2.77906269374259,-2.77454795816053,
-2.67811470950687,-2.63112048038978,-2.62370171375662,-2.62157000240831,
-2.62026490151303,-2.61908301622177,-2.61756857638303,-2.61445810436376,
-2.59477618260641,-2.58930250594203,-2.58298148302896,-2.57546014550829,
-2.49972193863163,-2.47305853847825,-2.46142033155656,-2.45980102699445,
-2.4589808149304,-2.45832476848596,-2.45757108486188,-2.45629508801446,
-2.45169994648714,-2.36452226515802,-2.30510009210387,-2.30030002260929,
-2.29849371525789,-2.29725998200503,-2.29605946051729,-2.29462232539572,
-2.29108217459988,-2.25933473238075,-2.2525732509643,-2.21408312266448,
-2.16672499017184,-2.14759593055792,-2.13859149669784,-2.13707287411684,
-2.13627373765975,-2.1356825371403,-2.13493632085368,-2.13366041418807,
-2.12920516591373,-2.03178623989194,-2.00896333428079,-1.98052293943271,
-1.97707942868522,-1.97551781026475,-1.97432539425451,-1.97305441959847,
-1.97107533607067,-1.96500428674648,-1.87191544085489,-1.82833588508653,
-1.81623548191366,-1.81444806746021,-1.81360328330832,-1.81294314013824,
-1.8122131644932,-1.81100985364388,-1.80672264779518,-1.77763136083035,
-1.69059261305607,-1.68196198475348,-1.67664345115794,-1.65725261470817,
-1.65415594585717,-1.65264435830329,-1.6514629368924,-1.65015654991202,
-1.64801866446179,-1.64053846185211,-1.59286405460848,-1.49732575892265,
-1.4926626513942,-1.49137951690636,-1.49062415903468,-1.48996827858595,
-1.48915036367255,-1.48754223627872,-1.47624249086549,-1.44667590651447,
-1.35094146560641,-1.33422005613513,-1.3312959435933,-1.32979916987074,
-1.32861940222463,-1.32733133220273,-1.32522867923072,-1.32273261500098,
-1.31789439215066,-1.27176851588104,-1.17423652309346,-1.16978371726422,
-1.16850793169171,-1.16776165523788,-1.16717033131905,-1.16637093337437,
-1.16485150288376,-1.15583369120007,-1.13669886303454,-1.08933971745287,
-1.01376294840054,-1.00930586145034,-1.00767880189868,-1.00653818296948,
-1.00537912452925,-1.00390561490426,-1.00229562642329,-0.999685083882543,
-0.994541534144163,-0.94308936070041,-0.858072665365449,-0.847761472937839,
-0.846056923665103,-0.845219286895199,-0.844561523990065,-0.843819133575337,
-0.842560936109431,-0.837694423263264,-0.814521171928508,-0.801118091233252,
-0.698692004858174,-0.690100189746012,-0.686200697117783,-0.684663684219583,
-0.683547295593433,-0.682420036920345,-0.680895677813379,-0.677701107060043,
-0.673534468134852,-0.663855264501745,-0.634474644762605,-0.584539288754084,
-0.527442131871906,-0.525459937638349,-0.523441448586807,-0.522633371478737,
-0.521963250054693,-0.52127129592785,-0.520240220579407,-0.517394766296325,
-0.467966172681365,-0.459924480473994,-0.453025925961595,-0.446982642310207,
-0.38855746526378,-0.383280281586546,-0.366006831476073,-0.36305315022849,
-0.361549871404574,-0.360369203037076,-0.359267130600406,-0.357352664030385,
-0.351748454604558,-0.343338465763197,-0.318344772119302,-0.226191147667687,
-0.202897911910209,-0.200817615268097,-0.199976705905959,-0.199359214191771,
-0.198687170903307,-0.197755130993993,-0.195542679678349,-0.192500375416105,
-0.159484016818544,-0.0764828869227818,-0.0698452084274265,-0.0633781307863137,
-0.04342066476137,-0.0402970536293278,-0.0387798227567039,-0.0375973917206149,
-0.0364959251413158,-0.0352169765653819,-0.0333966675439099,-0.0302788094196745,
-0.000956542473226251),.UNSPECIFIED.);
#834=B_SPLINE_CURVE_WITH_KNOTS('',3,(#47268,#47269,#47270,#47271,#47272,
#47273,#47274,#47275,#47276,#47277,#47278,#47279,#47280,#47281,#47282,#47283,
#47284,#47285,#47286,#47287,#47288,#47289,#47290,#47291,#47292,#47293,#47294,
#47295,#47296,#47297,#47298,#47299,#47300,#47301,#47302,#47303,#47304,#47305,
#47306,#47307,#47308,#47309,#47310,#47311,#47312,#47313,#47314,#47315,#47316,
#47317,#47318,#47319,#47320,#47321,#47322,#47323,#47324,#47325,#47326,#47327,
#47328,#47329,#47330,#47331,#47332,#47333,#47334,#47335,#47336,#47337,#47338,
#47339,#47340,#47341,#47342,#47343,#47344,#47345,#47346,#47347,#47348,#47349,
#47350,#47351,#47352,#47353,#47354,#47355,#47356,#47357,#47358,#47359,#47360,
#47361,#47362,#47363,#47364,#47365,#47366,#47367,#47368,#47369,#47370,#47371,
#47372,#47373,#47374,#47375,#47376,#47377,#47378,#47379,#47380,#47381,#47382,
#47383,#47384,#47385,#47386,#47387,#47388,#47389,#47390,#47391,#47392,#47393,
#47394,#47395,#47396,#47397,#47398,#47399,#47400,#47401,#47402,#47403,#47404,
#47405,#47406,#47407,#47408,#47409,#47410,#47411,#47412,#47413,#47414,#47415,
#47416,#47417,#47418,#47419,#47420,#47421,#47422,#47423,#47424,#47425,#47426,
#47427,#47428,#47429,#47430,#47431,#47432,#47433,#47434,#47435,#47436,#47437,
#47438,#47439,#47440,#47441,#47442,#47443,#47444,#47445,#47446,#47447,#47448,
#47449,#47450,#47451,#47452,#47453,#47454,#47455,#47456,#47457,#47458,#47459,
#47460,#47461,#47462,#47463,#47464,#47465,#47466,#47467,#47468,#47469,#47470,
#47471,#47472,#47473,#47474,#47475,#47476,#47477,#47478,#47479,#47480,#47481,
#47482,#47483,#47484,#47485,#47486,#47487,#47488,#47489,#47490,#47491,#47492,
#47493,#47494,#47495,#47496,#47497,#47498,#47499,#47500,#47501,#47502,#47503,
#47504,#47505,#47506,#47507,#47508,#47509,#47510,#47511,#47512,#47513,#47514,
#47515,#47516,#47517,#47518,#47519,#47520,#47521,#47522,#47523,#47524,#47525,
#47526,#47527,#47528,#47529,#47530,#47531,#47532,#47533,#47534,#47535,#47536,
#47537,#47538,#47539,#47540,#47541,#47542,#47543,#47544,#47545,#47546,#47547,
#47548,#47549,#47550,#47551,#47552,#47553,#47554,#47555,#47556,#47557,#47558,
#47559,#47560,#47561,#47562,#47563,#47564,#47565,#47566,#47567,#47568,#47569,
#47570,#47571,#47572,#47573,#47574,#47575,#47576,#47577,#47578,#47579,#47580,
#47581,#47582,#47583,#47584,#47585,#47586,#47587,#47588,#47589,#47590,#47591,
#47592,#47593,#47594,#47595,#47596,#47597,#47598,#47599,#47600,#47601,#47602,
#47603,#47604,#47605,#47606,#47607,#47608,#47609,#47610,#47611,#47612,#47613,
#47614,#47615,#47616,#47617,#47618,#47619,#47620,#47621,#47622,#47623,#47624,
#47625,#47626,#47627,#47628,#47629,#47630,#47631,#47632,#47633,#47634,#47635,
#47636,#47637,#47638,#47639,#47640,#47641,#47642,#47643,#47644,#47645,#47646,
#47647,#47648,#47649,#47650,#47651,#47652,#47653,#47654,#47655,#47656,#47657,
#47658,#47659,#47660,#47661,#47662,#47663,#47664,#47665,#47666,#47667,#47668,
#47669,#47670,#47671,#47672,#47673,#47674,#47675,#47676,#47677,#47678,#47679,
#47680,#47681,#47682,#47683,#47684,#47685,#47686,#47687,#47688,#47689,#47690,
#47691,#47692,#47693,#47694,#47695,#47696,#47697,#47698,#47699,#47700,#47701,
#47702,#47703,#47704,#47705,#47706,#47707,#47708,#47709,#47710,#47711,#47712,
#47713,#47714,#47715,#47716,#47717,#47718,#47719,#47720,#47721,#47722,#47723,
#47724,#47725,#47726,#47727,#47728,#47729,#47730,#47731,#47732,#47733,#47734,
#47735,#47736,#47737,#47738,#47739,#47740,#47741,#47742,#47743,#47744,#47745,
#47746,#47747,#47748,#47749,#47750,#47751,#47752,#47753,#47754,#47755,#47756,
#47757,#47758,#47759,#47760,#47761,#47762,#47763,#47764,#47765,#47766,#47767,
#47768,#47769,#47770,#47771,#47772,#47773,#47774,#47775,#47776,#47777,#47778,
#47779,#47780,#47781,#47782,#47783,#47784,#47785,#47786,#47787,#47788,#47789,
#47790,#47791,#47792,#47793,#47794,#47795,#47796,#47797,#47798,#47799),
 .UNSPECIFIED.,.F.,.F.,(4,2,2,2,2,2,2,2,2,2,2,2,2,2,2,2,2,2,2,2,2,2,2,2,
2,2,2,2,2,2,2,2,2,2,2,2,2,2,2,2,2,2,2,2,2,2,2,2,2,2,2,2,2,2,2,2,2,2,2,2,
2,2,2,2,2,2,2,2,2,2,2,2,2,2,2,2,2,2,2,2,2,2,2,2,2,2,2,2,2,2,2,2,2,2,2,2,
2,2,2,2,2,2,2,2,2,2,2,2,2,2,2,2,2,2,2,2,2,2,2,2,2,2,2,2,2,2,2,2,2,2,2,2,
2,2,2,2,2,2,2,2,2,2,2,2,2,2,2,2,2,2,2,2,2,2,2,2,2,2,2,2,2,2,2,2,2,2,2,2,
2,2,2,2,2,2,2,2,2,2,2,2,2,2,2,2,2,2,2,2,2,2,2,2,2,2,2,2,2,2,2,2,2,2,2,2,
2,2,2,2,2,2,2,2,2,2,2,2,2,2,2,2,2,2,2,2,2,2,2,2,2,2,2,2,2,2,2,2,2,2,2,2,
2,2,2,2,2,2,2,2,2,2,2,2,2,2,2,2,2,2,2,2,2,2,2,2,2,4),(-4.06096092462694,
-3.97919081284745,-3.94033500558184,-3.93805777042456,-3.93711465117569,
-3.93644048212338,-3.93582527337599,-3.93499352137346,-3.9333750346416,
-3.92106458908294,-3.91985519612799,-3.91901773292882,-3.91098115606398,
-3.81779744927564,-3.7925796260781,-3.78411144645442,-3.77847919840453,
-3.77655910402029,-3.77545667801708,-3.77427619058045,-3.77277588947607,
-3.76983669382993,-3.75284089231725,-3.74908203550039,-3.70284492101176,
-3.67125287897349,-3.62158546829895,-3.61606029256375,-3.61474721828114,
-3.61399259013788,-3.61333648551473,-3.61251718684841,-3.61124896035528,
-3.60543924597834,-3.49807606421452,-3.47068586556569,-3.46165372547933,
-3.4576955395516,-3.45463431840227,-3.45313499416033,-3.45200085814923,
-3.4508743372669,-3.4492991686473,-3.44516953008477,-3.3749519331859,-3.33250984507165,
-3.29782268325609,-3.29308893409011,-3.29184277570622,-3.29110312769775,
-3.29044496090269,-3.28960301255844,-3.2879338939263,-3.27790650441158,
-3.23332785876528,-3.14265283140812,-3.13670464526738,-3.13379964360183,
-3.1320670656346,-3.13050457567412,-3.12933354947813,-3.12822215533321,
-3.12670423181934,-3.12291646816968,-3.07486489963749,-3.00935084624,-2.98278616443645,
-2.97102064211608,-2.9693972220211,-2.96857615633364,-2.96792003390814,
-2.96716693740208,-2.96589347977399,-2.96132245636345,-2.87343455784002,
-2.81377925554977,-2.81096567830702,-2.80927104058542,-2.8077339113591,
-2.80656621012,-2.80544657157215,-2.80389692980886,-2.80077232391329,-2.77142101164101,
-2.70065042425994,-2.67527034076667,-2.65129433730004,-2.64747264838896,
-2.64631851734601,-2.64559953061925,-2.64493605350787,-2.64406885382279,
-2.64216338063635,-2.62698734961467,-2.6239264351805,-2.52767801945915,
-2.49364925344703,-2.48755539849178,-2.48557344872218,-2.48430180735438,
-2.48310959893817,-2.48154945241806,-2.4789266715549,-2.46301935409514,
-2.45825570391109,-2.45659282719115,-2.4478634850003,-2.36333676902471,
-2.32955878393936,-2.32647953231094,-2.32424596611931,-2.32331046004482,
-2.32263790868039,-2.32202139904669,-2.32118391109189,-2.31954249215766,
-2.30659127209733,-2.22404316406299,-2.16729451034805,-2.16389025215467,
-2.16231889678326,-2.16112917563126,-2.1600063256552,-2.15813446347704,
-2.15329062032496,-2.07740918849232,-2.0305643032039,-2.00372512134957,
-2.00157821529496,-2.00072596041949,-2.00010565285986,-1.99943613202562,
-1.99851721985672,-1.99637943581422,-1.96270500880362,-1.90382748872865,
-1.84548459933442,-1.84159870500729,-1.84006411146326,-1.83894845067498,
-1.83775470009993,-1.83615805739424,-1.83261862684281,-1.82792991562823,
-1.78424142083256,-1.69117083407885,-1.68033281081321,-1.67860208995183,
-1.67775928122458,-1.67710102742307,-1.67636190541698,-1.67511807014486,
-1.67040958034455,-1.6360724371505,-1.5353607953123,-1.53302452807617,-1.53086549361769,
-1.52306053400685,-1.51887907574776,-1.51729563335629,-1.5161669891372,
-1.5149799365889,-1.51342677422842,-1.51011814444593,-1.46638725455222,
-1.36703319645439,-1.35735260342995,-1.35570139520562,-1.35486325784665,
-1.35420548032741,-1.35346348126207,-1.35223209496953,-1.34762653656585,
-1.31446555010206,-1.24170156206602,-1.22297656488153,-1.21789899329235,
-1.19856427264209,-1.1954696696151,-1.1939582600312,-1.19277659894218,-1.19146955989951,
-1.18932972913495,-1.18201513977918,-1.13580444033686,-1.06350016492354,
-1.05107270995833,-1.04795365866589,-1.03491309958993,-1.03310961117931,
-1.03224885488227,-1.03158628353944,-1.03086410996496,-1.02971955350319,
-1.02597361674185,-1.00261460985047,-0.940962288820962,-0.877193553653152,
-0.873286853876515,-0.871748551065455,-0.870631766515194,-0.86943828813933,
-0.867844549661155,-0.864413867689255,-0.796413570174008,-0.749673593210714,
-0.734915281116713,-0.730123414619615,-0.727544333706052,-0.712341835463116,
-0.710435256216269,-0.709567770414391,-0.708904165946427,-0.708185134751287,
-0.70705427062878,-0.703426334404997,-0.697658431284722,-0.678985762418818,
-0.630851046052793,-0.592942186412587,-0.591456976229329,-0.578840357702262,
-0.573267665794149,-0.553286287470415,-0.55016159218077,-0.548644149694129,
-0.547461696208307,-0.546157771458345,-0.544032045744125,-0.536822288208567,
-0.501335979505161,-0.444284655203243,-0.399570296274313,-0.389411811306336,
-0.387714827289933,-0.38687872657509,-0.386221141160508,-0.385477839332605,
-0.384703735225948,-0.381994031174152,-0.378028633093763,-0.36671474966148,
-0.339395872545463,-0.315836239073396,-0.233629652658549,-0.228454237645428,
-0.226529667729118,-0.225396348703753,-0.224329473870766,-0.222851786464301,
-0.219923980427594,-0.201887954758125,-0.157677129325545,-0.141943403594944,
-0.134109145857688,-0.124858185245046,-0.0689282052345134,-0.0657149562395191,
-0.064594021162722,-0.0639534146177227,-0.063359765784039,-0.062726389614209,
-0.0619244189171355,-0.0606938192310203,-0.0584068393442843,-0.000956966008258823),
 .UNSPECIFIED.);
#835=B_SPLINE_CURVE_WITH_KNOTS('',3,(#47801,#47802,#47803,#47804,#47805,
#47806,#47807,#47808,#47809,#47810,#47811,#47812,#47813,#47814,#47815,#47816,
#47817,#47818,#47819,#47820,#47821,#47822,#47823,#47824,#47825,#47826,#47827,
#47828,#47829,#47830,#47831,#47832,#47833,#47834,#47835,#47836,#47837,#47838,
#47839,#47840,#47841,#47842,#47843,#47844,#47845,#47846,#47847,#47848,#47849,
#47850,#47851,#47852,#47853,#47854,#47855,#47856,#47857,#47858,#47859,#47860,
#47861,#47862,#47863,#47864,#47865,#47866,#47867,#47868,#47869,#47870,#47871,
#47872,#47873,#47874,#47875,#47876,#47877,#47878,#47879,#47880,#47881,#47882,
#47883,#47884,#47885,#47886,#47887,#47888,#47889,#47890,#47891,#47892,#47893,
#47894,#47895,#47896,#47897,#47898,#47899,#47900,#47901,#47902,#47903,#47904,
#47905,#47906,#47907,#47908,#47909,#47910,#47911,#47912,#47913,#47914,#47915,
#47916,#47917,#47918,#47919,#47920,#47921,#47922,#47923,#47924,#47925,#47926,
#47927,#47928,#47929,#47930,#47931,#47932,#47933,#47934,#47935,#47936,#47937,
#47938,#47939,#47940,#47941,#47942,#47943,#47944,#47945,#47946,#47947,#47948,
#47949,#47950,#47951,#47952,#47953,#47954,#47955,#47956,#47957,#47958,#47959,
#47960,#47961,#47962,#47963,#47964,#47965,#47966,#47967,#47968,#47969,#47970,
#47971,#47972,#47973,#47974,#47975,#47976,#47977,#47978,#47979,#47980,#47981,
#47982,#47983,#47984,#47985,#47986,#47987,#47988,#47989,#47990,#47991,#47992,
#47993,#47994,#47995,#47996,#47997,#47998,#47999,#48000,#48001,#48002,#48003,
#48004,#48005,#48006,#48007,#48008,#48009,#48010,#48011,#48012,#48013,#48014,
#48015,#48016,#48017,#48018,#48019,#48020,#48021,#48022,#48023,#48024,#48025,
#48026,#48027,#48028,#48029,#48030,#48031,#48032,#48033,#48034,#48035,#48036,
#48037,#48038,#48039,#48040,#48041,#48042,#48043,#48044,#48045,#48046,#48047,
#48048,#48049,#48050,#48051,#48052,#48053,#48054,#48055,#48056,#48057,#48058,
#48059,#48060,#48061,#48062,#48063,#48064,#48065,#48066,#48067,#48068,#48069,
#48070,#48071,#48072,#48073,#48074,#48075,#48076,#48077,#48078,#48079,#48080,
#48081,#48082,#48083,#48084,#48085,#48086,#48087,#48088,#48089,#48090,#48091,
#48092,#48093,#48094,#48095,#48096,#48097,#48098,#48099,#48100,#48101,#48102,
#48103,#48104,#48105,#48106,#48107,#48108,#48109,#48110,#48111,#48112,#48113,
#48114,#48115,#48116,#48117,#48118,#48119,#48120,#48121,#48122,#48123,#48124,
#48125,#48126,#48127,#48128,#48129,#48130,#48131,#48132,#48133,#48134,#48135,
#48136,#48137,#48138,#48139,#48140,#48141,#48142,#48143,#48144,#48145,#48146,
#48147,#48148,#48149,#48150,#48151,#48152,#48153,#48154,#48155,#48156,#48157,
#48158,#48159,#48160,#48161,#48162,#48163,#48164,#48165,#48166,#48167,#48168,
#48169,#48170,#48171,#48172,#48173,#48174,#48175,#48176,#48177,#48178,#48179,
#48180,#48181,#48182,#48183,#48184,#48185,#48186,#48187,#48188,#48189,#48190,
#48191,#48192,#48193,#48194,#48195,#48196,#48197,#48198,#48199,#48200,#48201,
#48202,#48203,#48204,#48205,#48206,#48207,#48208,#48209,#48210,#48211,#48212,
#48213,#48214,#48215,#48216,#48217,#48218,#48219,#48220,#48221,#48222,#48223,
#48224,#48225,#48226,#48227,#48228,#48229,#48230,#48231,#48232,#48233,#48234,
#48235,#48236,#48237,#48238,#48239,#48240,#48241,#48242,#48243,#48244,#48245,
#48246,#48247,#48248,#48249,#48250,#48251,#48252,#48253,#48254,#48255,#48256,
#48257,#48258,#48259,#48260,#48261,#48262,#48263,#48264,#48265,#48266,#48267,
#48268,#48269,#48270,#48271,#48272,#48273,#48274,#48275,#48276,#48277,#48278,
#48279,#48280,#48281,#48282,#48283,#48284,#48285,#48286,#48287,#48288,#48289,
#48290,#48291,#48292,#48293,#48294,#48295,#48296,#48297,#48298,#48299,#48300,
#48301,#48302,#48303,#48304,#48305,#48306,#48307,#48308,#48309,#48310,#48311,
#48312,#48313,#48314,#48315,#48316,#48317,#48318,#48319,#48320,#48321,#48322,
#48323,#48324,#48325,#48326,#48327,#48328,#48329,#48330,#48331,#48332,#48333,
#48334,#48335,#48336,#48337,#48338,#48339,#48340,#48341,#48342,#48343,#48344,
#48345,#48346,#48347,#48348),.UNSPECIFIED.,.F.,.F.,(4,2,2,2,2,2,2,2,2,2,
2,2,2,2,2,2,2,2,2,2,2,2,2,2,2,2,2,2,2,2,2,2,2,2,2,2,2,2,2,2,2,2,2,2,2,2,
2,2,2,2,2,2,2,2,2,2,2,2,2,2,2,2,2,2,2,2,2,2,2,2,2,2,2,2,2,2,2,2,2,2,2,2,
2,2,2,2,2,2,2,2,2,2,2,2,2,2,2,2,2,2,2,2,2,2,2,2,2,2,2,2,2,2,2,2,2,2,2,2,
2,2,2,2,2,2,2,2,2,2,2,2,2,2,2,2,2,2,2,2,2,2,2,2,2,2,2,2,2,2,2,2,2,2,2,2,
2,2,2,2,2,2,2,2,2,2,2,2,2,2,2,2,2,2,2,2,2,2,2,2,2,2,2,2,2,2,2,2,2,2,2,2,
2,2,2,2,2,2,2,2,2,2,2,2,2,2,2,2,2,2,2,2,2,2,2,2,2,2,2,2,2,2,2,2,2,2,2,2,
2,2,2,2,2,2,2,2,2,2,2,2,2,2,2,2,2,2,2,2,2,2,2,2,2,2,2,2,2,2,2,2,2,2,2,2,
2,2,2,2,2,2,2,2,2,2,2,4),(-4.06063664256222,-3.9728178653946,-3.96817330428761,
-3.9657507498166,-3.96367747480607,-3.96238573583193,-3.96120092584095,
-3.95968695719411,-3.95649406725477,-3.93493627213538,-3.86545558219806,
-3.84400846894577,-3.81634787817368,-3.8037176287448,-3.80255261287607,
-3.80177826638475,-3.80103490784806,-3.80037775516869,-3.79954284817197,
-3.79785045644931,-3.78776924566413,-3.74314913233184,-3.7028571063676,
-3.66212385612992,-3.64458691523146,-3.64179477780974,-3.64034562897998,
-3.63928290790934,-3.63813832268918,-3.6364957850218,-3.63193437846331,
-3.55354239276756,-3.52026447987411,-3.49539654248139,-3.48590024901914,
-3.48062133497725,-3.47932741146448,-3.47869710940945,-3.47810498614432,
-3.47745975370476,-3.47651564343172,-3.47377661279283,-3.42957611463609,
-3.37789844381286,-3.33913756950115,-3.32787573899105,-3.32321367863729,
-3.31969049779254,-3.31809707691609,-3.31690406525402,-3.31578788249488,
-3.31425066783107,-3.31034810324101,-3.2479466649981,-3.24466367312895,
-3.19705334943805,-3.17066212060436,-3.16805341048395,-3.16175651348737,
-3.15787657825751,-3.15671772812344,-3.15599250547556,-3.1553312746245,
-3.15447785933283,-3.15264481825705,-3.13942692546299,-3.13706519897787,
-3.13629580488889,-3.13273989195526,-3.13070018276657,-3.1187752230506,
-3.05039087455928,-3.00554675310395,-3.00078645005306,-2.9972036889808,
-2.99559930268966,-2.99440450141676,-2.99329127127823,-2.99176534197486,
-2.98792914036917,-2.93567331288154,-2.86966758136114,-2.83977626819666,
-2.83689812605837,-2.83480204324943,-2.83388997418697,-2.83321841567928,
-2.83260107284997,-2.83175993863321,-2.82967693439173,-2.80620846151174,
-2.79530017976929,-2.75282523622438,-2.70939755154346,-2.68361732756857,
-2.67855896665505,-2.67479709393872,-2.67316032287313,-2.67195990608139,
-2.67085448896474,-2.669359198528,-2.66644780319447,-2.64389122647826,-2.62797009405563,
-2.54168710712269,-2.5225670373368,-2.51343885502548,-2.51191480693229,
-2.51111456304351,-2.51052329827946,-2.50987330853131,-2.50870509694854,
-2.50514482550405,-2.4452942361457,-2.39638309240506,-2.35595728609159,
-2.35219227850474,-2.35055484572774,-2.3493542133943,-2.34824878701673,
-2.34675377107795,-2.34384375240974,-2.32133066419765,-2.3093759256781,
-2.30651133911038,-2.22614148173872,-2.21306479921595,-2.19807704877291,
-2.19069577436681,-2.18925930575926,-2.18847776658479,-2.18788798960529,
-2.18722683183057,-2.18600341058304,-2.18200512326269,-2.10839354612462,
-2.06456239763841,-2.04285411725367,-2.03128814812829,-2.02906211760091,
-2.02760605098205,-2.02643017420149,-2.02508932024748,-2.02279745460101,
-2.01366457292012,-1.92301641362903,-1.87843044210397,-1.86841663284503,
-1.86674832126655,-1.86590659186958,-1.86524850416418,-1.86450884435705,
-1.86326243714262,-1.85852509452477,-1.8237926680234,-1.75920738999232,
-1.74209262665134,-1.71032180766946,-1.70678084090183,-1.70534352766242,
-1.70414291693203,-1.70290915482323,-1.70110292152006,-1.69630372436184,
-1.63685608857803,-1.54954496195863,-1.54502339463764,-1.54374008332427,
-1.54299211938131,-1.54240099736511,-1.54160383661386,-1.54009500073034,
-1.53130980242522,-1.51252239106176,-1.46831150343087,-1.38934816350616,
-1.38462112602489,-1.38276810689587,-1.3816487374047,-1.38045680590794,
-1.37887250440868,-1.37547991775868,-1.37098840600033,-1.330394282525,-1.24904970785202,
-1.22368995246028,-1.22156928119658,-1.22072139781746,-1.22010212265929,
-1.21943153754818,-1.218526009025,-1.21644407536694,-1.21360312740583,-1.18440561095295,
-1.11378335987303,-1.09698358280725,-1.09103226273566,-1.08359681820421,
-1.06416544494335,-1.06106615847322,-1.05955375610123,-1.05837190877296,
-1.05706526618667,-1.05492745070177,-1.04762253296447,-1.00153532937066,
-0.940726580746427,-0.910788015951101,-0.900344788758057,-0.898633567308237,
-0.897794598631607,-0.897136701931812,-0.896395142303076,-0.89516580761412,
-0.890753706111515,-0.883241711181622,-0.853749490623139,-0.803324583181019,
-0.742812467511629,-0.73891469103731,-0.737377850468346,-0.736261410874336,
-0.735067629084746,-0.733472327651497,-0.730057724747939,-0.705652102521991,
-0.684040781967298,-0.632371602551695,-0.587717762908069,-0.57766970465921,
-0.57599943593632,-0.57515719891526,-0.574498950271726,-0.57375936200942,
-0.572990538453649,-0.570363704605121,-0.542260763949439,-0.495407151417223,
-0.421281763420022,-0.416570350297911,-0.41490486562672,-0.41375357292122,
-0.41269182850815,-0.411254918768642,-0.409726510486734,-0.40303963017123,
-0.392491121041141,-0.361153547439554,-0.338623823357926,-0.315775038181721,
-0.293356939098674,-0.27708334631547,-0.274302794911084,-0.270004373124783,
-0.25534124621658,-0.253641393744814,-0.252788972599971,-0.252168549433432,
-0.251498909276072,-0.250579842701529,-0.249560258049507,-0.242554944214925,
-0.205199585427156,-0.192062276384384,-0.178004956326378,-0.0987760072086423,
-0.0939756485195223,-0.0921106418679364,-0.0909889742155074,-0.0897983089261329,
-0.0882219927980785,-0.0865006229289555,-0.0836227576680198,-0.000957501929126401),
 .UNSPECIFIED.);
#836=B_SPLINE_CURVE_WITH_KNOTS('',3,(#48350,#48351,#48352,#48353,#48354,
#48355,#48356,#48357,#48358,#48359,#48360,#48361,#48362,#48363,#48364,#48365,
#48366,#48367,#48368,#48369,#48370,#48371,#48372,#48373,#48374,#48375,#48376,
#48377,#48378,#48379,#48380,#48381,#48382,#48383,#48384,#48385,#48386,#48387,
#48388,#48389,#48390,#48391,#48392,#48393,#48394,#48395,#48396,#48397,#48398,
#48399,#48400,#48401,#48402,#48403,#48404,#48405,#48406,#48407,#48408,#48409,
#48410,#48411,#48412,#48413,#48414,#48415,#48416,#48417,#48418,#48419,#48420,
#48421,#48422,#48423,#48424,#48425,#48426,#48427,#48428,#48429,#48430,#48431,
#48432,#48433,#48434,#48435,#48436,#48437,#48438,#48439,#48440,#48441,#48442,
#48443,#48444,#48445,#48446,#48447,#48448,#48449,#48450,#48451,#48452,#48453,
#48454,#48455,#48456,#48457,#48458,#48459,#48460,#48461,#48462,#48463,#48464,
#48465,#48466,#48467,#48468,#48469,#48470,#48471,#48472,#48473,#48474,#48475,
#48476,#48477,#48478,#48479,#48480,#48481,#48482,#48483,#48484,#48485,#48486,
#48487,#48488,#48489,#48490,#48491,#48492,#48493,#48494,#48495,#48496,#48497,
#48498,#48499,#48500,#48501,#48502,#48503,#48504,#48505,#48506,#48507,#48508,
#48509,#48510,#48511,#48512,#48513,#48514,#48515,#48516,#48517,#48518,#48519,
#48520,#48521,#48522,#48523,#48524,#48525,#48526,#48527,#48528,#48529,#48530,
#48531,#48532,#48533,#48534,#48535,#48536,#48537,#48538,#48539,#48540,#48541,
#48542,#48543,#48544,#48545,#48546,#48547,#48548,#48549,#48550,#48551,#48552,
#48553,#48554,#48555,#48556,#48557,#48558,#48559,#48560,#48561,#48562,#48563,
#48564,#48565,#48566,#48567,#48568,#48569,#48570,#48571,#48572,#48573,#48574,
#48575,#48576,#48577,#48578,#48579,#48580,#48581,#48582,#48583,#48584,#48585,
#48586,#48587,#48588,#48589,#48590,#48591,#48592,#48593,#48594,#48595,#48596,
#48597,#48598,#48599,#48600,#48601,#48602,#48603,#48604,#48605,#48606,#48607,
#48608,#48609,#48610,#48611,#48612,#48613,#48614,#48615,#48616,#48617,#48618,
#48619,#48620,#48621,#48622,#48623,#48624,#48625,#48626,#48627,#48628,#48629,
#48630,#48631,#48632,#48633,#48634,#48635,#48636,#48637,#48638,#48639,#48640,
#48641,#48642,#48643,#48644,#48645,#48646,#48647,#48648,#48649,#48650,#48651,
#48652,#48653,#48654,#48655,#48656,#48657,#48658,#48659,#48660,#48661,#48662,
#48663,#48664,#48665,#48666,#48667,#48668,#48669,#48670,#48671,#48672,#48673,
#48674,#48675,#48676,#48677,#48678,#48679,#48680,#48681,#48682,#48683,#48684,
#48685,#48686,#48687,#48688,#48689,#48690,#48691,#48692,#48693,#48694,#48695,
#48696,#48697,#48698,#48699,#48700,#48701,#48702,#48703,#48704,#48705,#48706,
#48707,#48708,#48709,#48710,#48711,#48712,#48713,#48714,#48715,#48716,#48717,
#48718,#48719,#48720,#48721,#48722,#48723,#48724,#48725,#48726,#48727,#48728,
#48729,#48730,#48731,#48732,#48733,#48734,#48735,#48736,#48737,#48738,#48739,
#48740,#48741,#48742,#48743,#48744,#48745,#48746,#48747,#48748,#48749,#48750,
#48751,#48752,#48753,#48754,#48755,#48756,#48757,#48758,#48759,#48760,#48761,
#48762,#48763,#48764,#48765,#48766,#48767,#48768,#48769,#48770,#48771,#48772,
#48773,#48774,#48775,#48776,#48777,#48778,#48779,#48780,#48781,#48782,#48783,
#48784,#48785,#48786,#48787,#48788,#48789,#48790,#48791,#48792,#48793,#48794,
#48795,#48796,#48797,#48798,#48799,#48800,#48801,#48802,#48803,#48804,#48805,
#48806,#48807,#48808,#48809,#48810,#48811,#48812,#48813,#48814,#48815,#48816,
#48817,#48818,#48819,#48820,#48821,#48822,#48823,#48824,#48825,#48826,#48827,
#48828,#48829,#48830,#48831,#48832,#48833,#48834,#48835,#48836,#48837,#48838,
#48839,#48840,#48841,#48842,#48843,#48844,#48845,#48846,#48847,#48848,#48849,
#48850,#48851,#48852,#48853,#48854,#48855,#48856,#48857,#48858,#48859,#48860,
#48861,#48862,#48863,#48864,#48865,#48866,#48867,#48868,#48869,#48870,#48871,
#48872,#48873,#48874,#48875,#48876,#48877,#48878,#48879,#48880,#48881,#48882,
#48883),.UNSPECIFIED.,.F.,.F.,(4,2,2,2,2,2,2,2,2,2,2,2,2,2,2,2,2,2,2,2,
2,2,2,2,2,2,2,2,2,2,2,2,2,2,2,2,2,2,2,2,2,2,2,2,2,2,2,2,2,2,2,2,2,2,2,2,
2,2,2,2,2,2,2,2,2,2,2,2,2,2,2,2,2,2,2,2,2,2,2,2,2,2,2,2,2,2,2,2,2,2,2,2,
2,2,2,2,2,2,2,2,2,2,2,2,2,2,2,2,2,2,2,2,2,2,2,2,2,2,2,2,2,2,2,2,2,2,2,2,
2,2,2,2,2,2,2,2,2,2,2,2,2,2,2,2,2,2,2,2,2,2,2,2,2,2,2,2,2,2,2,2,2,2,2,2,
2,2,2,2,2,2,2,2,2,2,2,2,2,2,2,2,2,2,2,2,2,2,2,2,2,2,2,2,2,2,2,2,2,2,2,2,
2,2,2,2,2,2,2,2,2,2,2,2,2,2,2,2,2,2,2,2,2,2,2,2,2,2,2,2,2,2,2,2,2,2,2,2,
2,2,2,2,2,2,2,2,2,2,2,2,2,2,2,2,2,2,2,2,2,2,2,2,2,2,2,2,2,2,4),(-4.05990386301481,
-3.99809978947004,-3.99329731683281,-3.99118058419593,-3.99001654462979,
-3.98924255633462,-3.98849941570817,-3.98784209154762,-3.98700648300469,
-3.98531103532073,-3.97517420561014,-3.91790465072373,-3.90349953819912,
-3.88952171232384,-3.85022696325981,-3.83220288589521,-3.83015917988238,
-3.8283518218361,-3.82711796754219,-3.82591778855667,-3.82448161296133,
-3.82094664451944,-3.78937563652594,-3.74241734817476,-3.70107118295529,
-3.67842030014143,-3.67186269223417,-3.66786055663566,-3.66698856612843,
-3.66617548566487,-3.6655828384482,-3.66493938266889,-3.66380357887516,
-3.66048214296812,-3.60021574213842,-3.54785805956159,-3.51554597851715,
-3.50831024070987,-3.50674610250057,-3.50528349867359,-3.50421894217199,
-3.50308000412431,-3.50145837970363,-3.49703494125092,-3.42735988875566,
-3.36958128648223,-3.35788674054822,-3.34999530397017,-3.34694611635174,
-3.34474696217604,-3.34380756220566,-3.34313433951493,-3.34251875596786,
-3.34168473033736,-3.34005661562455,-3.32746495053866,-3.32451647161291,
-3.32404258249264,-3.28871981961329,-3.23098335755258,-3.2119967744143,
-3.18802299072834,-3.18456695288459,-3.18296869510608,-3.18177473915713,
-3.18065961025899,-3.17912688121026,-3.17525165366302,-3.11857540687163,
-3.05358203563633,-3.0267980218711,-3.02409466204222,-3.02209086728244,
-3.02119040572553,-3.02052407569213,-3.01989898649335,-3.01902854539786,
-3.01677425456922,-2.98239576250505,-2.91469295678513,-2.89156866853065,
-2.86574662930738,-2.86208326201571,-2.86044439034833,-2.85924347024299,
-2.85813831662987,-2.8566444845232,-2.85373915870461,-2.83135527151072,
-2.81617070534995,-2.73789931218056,-2.71144423867707,-2.70084225317016,
-2.69926353447726,-2.6984450634278,-2.69779520564332,-2.6970425788064,-2.695770956751,
-2.69121656660287,-2.60047483629661,-2.56784767512706,-2.5446312311509,
-2.53980539856664,-2.53799531628337,-2.53676085042842,-2.5355610380772,
-2.53412644758612,-2.53060124549272,-2.49938595077448,-2.45210082174036,
-2.40578140197482,-2.38253098633032,-2.37763400335865,-2.37637338338913,
-2.37563060559363,-2.37497316820974,-2.37413683835302,-2.37281293792719,
-2.36624760419868,-2.33003236169214,-2.30944857313231,-2.26904627921545,
-2.22504435723991,-2.22033566737779,-2.21678402087101,-2.21518514185618,
-2.21399104248703,-2.21287601143916,-2.2113437794367,-2.20828819047212,
-2.18137788033073,-2.11010362850301,-2.05754398831667,-2.05462387519191,
-2.05358231327164,-2.05288816212063,-2.05221975457724,-2.05141810813354,
-2.04943824975472,-2.03190840475543,-2.03109405519523,-2.00923307740926,
-1.91416105030042,-1.89676801896583,-1.89380852661887,-1.8923042047372,
-1.89112365198092,-1.88981328307948,-1.88765759311611,-1.88000200014614,
-1.85426433717289,-1.8109004304892,-1.7365594184233,-1.73234282535337,-1.73109375147995,
-1.73042742447984,-1.72977882241033,-1.72897927818886,-1.72745869700733,
-1.71841014094023,-1.69926446724877,-1.65183970628718,-1.57656337189498,
-1.57199196957249,-1.57034770605514,-1.5692024871226,-1.56813962458352,
-1.56669096618924,-1.56390210499777,-1.54613431562565,-1.50440614888028,
-1.41424308808466,-1.40971241970672,-1.40844325838421,-1.40769116812338,
-1.40704118315682,-1.40622179330454,-1.40460650452707,-1.39309147515017,
-1.36634447841407,-1.29007771480206,-1.2758049359357,-1.27070870511949,
-1.25158021601765,-1.24849562692751,-1.24698632025105,-1.24580502849872,
-1.24452364449189,-1.24245962435419,-1.24001310677164,-1.23530602811917,
-1.19132536773386,-1.09816103091897,-1.08770160457215,-1.08598960818337,
-1.08515050121917,-1.08449260916141,-1.08375117640228,-1.08249716703844,
-1.07767716192421,-1.04179210820542,-0.932979853549016,-0.926861018594506,
-0.924799321776232,-0.923638811965763,-0.92248039566963,-0.921045977327254,
-0.91829137570206,-0.914816120234125,-0.907236322188173,-0.885497732320572,
-0.834913320862327,-0.827720600789962,-0.767417386168433,-0.766248960361632,
-0.763645653552049,-0.762721360619905,-0.762081541310863,-0.761487770125752,
-0.760666353912119,-0.759041138451033,-0.747217539699004,-0.720712657359132,
-0.631583153642152,-0.626015848650499,-0.606046136625364,-0.60292253799403,
-0.601405541820202,-0.600223397106319,-0.598945957379322,-0.596930387124626,
-0.590344869714719,-0.580002100953146,-0.57077636487165,-0.531147450016179,
-0.44580743247836,-0.441412174168298,-0.440142817797402,-0.439398016944631,
-0.438806554467441,-0.438005289159411,-0.436476830082254,-0.427252967703651,
-0.408395126312187,-0.36508996999871,-0.34365648788856,-0.311616565005529,
-0.283889620025191,-0.280467939168452,-0.278910157702366,-0.277718158730201,
-0.276618033213144,-0.275369989578078,-0.271954392446,-0.245419946775437,
-0.224207543775412,-0.133231880603835,-0.132268129062042,-0.119655658966594,
-0.118026183930549,-0.117191659800277,-0.11657580415066,-0.115902382723439,
-0.114962879382259,-0.112706609127926,-0.0783863747249849,-0.00095823755941713),
 .UNSPECIFIED.);
#837=B_SPLINE_CURVE_WITH_KNOTS('',3,(#48885,#48886,#48887,#48888,#48889,
#48890,#48891,#48892,#48893,#48894,#48895,#48896,#48897,#48898,#48899,#48900,
#48901,#48902,#48903,#48904,#48905,#48906,#48907,#48908,#48909,#48910,#48911,
#48912,#48913,#48914,#48915,#48916,#48917,#48918,#48919,#48920,#48921,#48922,
#48923,#48924,#48925,#48926,#48927,#48928,#48929,#48930,#48931,#48932,#48933,
#48934,#48935,#48936,#48937,#48938,#48939,#48940,#48941,#48942,#48943,#48944,
#48945,#48946,#48947,#48948,#48949,#48950,#48951,#48952,#48953,#48954,#48955,
#48956,#48957,#48958,#48959,#48960,#48961,#48962,#48963,#48964,#48965,#48966,
#48967,#48968,#48969,#48970,#48971,#48972,#48973,#48974,#48975,#48976,#48977,
#48978,#48979,#48980,#48981,#48982,#48983,#48984,#48985,#48986,#48987,#48988,
#48989,#48990,#48991,#48992,#48993,#48994,#48995,#48996,#48997,#48998,#48999,
#49000,#49001,#49002,#49003,#49004,#49005,#49006,#49007,#49008,#49009,#49010,
#49011,#49012,#49013,#49014,#49015,#49016,#49017,#49018,#49019,#49020,#49021,
#49022,#49023,#49024,#49025,#49026,#49027,#49028,#49029,#49030,#49031,#49032,
#49033,#49034,#49035,#49036,#49037,#49038,#49039,#49040,#49041,#49042,#49043,
#49044,#49045,#49046,#49047,#49048,#49049,#49050,#49051,#49052,#49053,#49054,
#49055,#49056,#49057,#49058,#49059,#49060,#49061,#49062,#49063,#49064,#49065,
#49066,#49067,#49068,#49069,#49070,#49071,#49072,#49073,#49074,#49075,#49076,
#49077,#49078,#49079,#49080,#49081,#49082,#49083,#49084,#49085,#49086,#49087,
#49088,#49089,#49090,#49091,#49092,#49093,#49094,#49095,#49096,#49097,#49098,
#49099,#49100,#49101,#49102,#49103,#49104,#49105,#49106,#49107,#49108,#49109,
#49110,#49111,#49112,#49113,#49114,#49115,#49116,#49117,#49118,#49119,#49120,
#49121,#49122,#49123,#49124,#49125,#49126,#49127,#49128,#49129,#49130,#49131,
#49132,#49133,#49134,#49135,#49136,#49137,#49138,#49139,#49140,#49141,#49142,
#49143,#49144,#49145,#49146,#49147,#49148,#49149,#49150,#49151,#49152,#49153,
#49154,#49155,#49156,#49157,#49158,#49159,#49160,#49161,#49162,#49163,#49164,
#49165,#49166,#49167,#49168,#49169,#49170,#49171,#49172,#49173,#49174,#49175,
#49176,#49177,#49178,#49179,#49180,#49181,#49182,#49183,#49184,#49185,#49186,
#49187,#49188,#49189,#49190,#49191,#49192,#49193,#49194,#49195,#49196,#49197,
#49198,#49199,#49200,#49201,#49202,#49203,#49204,#49205,#49206,#49207,#49208,
#49209,#49210,#49211,#49212,#49213,#49214,#49215,#49216,#49217,#49218,#49219,
#49220,#49221,#49222,#49223,#49224,#49225,#49226,#49227,#49228,#49229,#49230,
#49231,#49232,#49233,#49234,#49235,#49236,#49237,#49238,#49239,#49240,#49241,
#49242,#49243,#49244,#49245,#49246,#49247,#49248,#49249,#49250,#49251,#49252,
#49253,#49254,#49255,#49256,#49257,#49258,#49259,#49260,#49261,#49262,#49263,
#49264,#49265,#49266,#49267,#49268,#49269,#49270,#49271,#49272,#49273,#49274,
#49275,#49276,#49277,#49278,#49279,#49280,#49281,#49282,#49283,#49284,#49285,
#49286,#49287,#49288,#49289,#49290,#49291,#49292,#49293,#49294,#49295,#49296,
#49297,#49298,#49299,#49300,#49301,#49302,#49303,#49304,#49305,#49306,#49307,
#49308,#49309,#49310,#49311,#49312,#49313,#49314,#49315,#49316,#49317,#49318,
#49319,#49320,#49321,#49322,#49323,#49324,#49325,#49326,#49327,#49328,#49329,
#49330,#49331,#49332,#49333,#49334,#49335,#49336,#49337,#49338,#49339,#49340,
#49341,#49342,#49343,#49344,#49345,#49346,#49347,#49348,#49349,#49350,#49351,
#49352,#49353,#49354,#49355,#49356,#49357,#49358,#49359,#49360,#49361,#49362,
#49363,#49364,#49365,#49366,#49367,#49368,#49369,#49370,#49371,#49372,#49373,
#49374,#49375,#49376,#49377,#49378,#49379,#49380,#49381,#49382,#49383,#49384,
#49385,#49386,#49387,#49388,#49389,#49390,#49391,#49392,#49393,#49394,#49395,
#49396,#49397,#49398,#49399,#49400,#49401,#49402,#49403,#49404,#49405,#49406,
#49407,#49408,#49409,#49410,#49411,#49412,#49413,#49414,#49415,#49416,#49417,
#49418,#49419,#49420,#49421,#49422,#49423,#49424,#49425,#49426,#49427,#49428,
#49429,#49430,#49431,#49432),.UNSPECIFIED.,.F.,.F.,(4,2,2,2,2,2,2,2,2,2,
2,2,2,2,2,2,2,2,2,2,2,2,2,2,2,2,2,2,2,2,2,2,2,2,2,2,2,2,2,2,2,2,2,2,2,2,
2,2,2,2,2,2,2,2,2,2,2,2,2,2,2,2,2,2,2,2,2,2,2,2,2,2,2,2,2,2,2,2,2,2,2,2,
2,2,2,2,2,2,2,2,2,2,2,2,2,2,2,2,2,2,2,2,2,2,2,2,2,2,2,2,2,2,2,2,2,2,2,2,
2,2,2,2,2,2,2,2,2,2,2,2,2,2,2,2,2,2,2,2,2,2,2,2,2,2,2,2,2,2,2,2,2,2,2,2,
2,2,2,2,2,2,2,2,2,2,2,2,2,2,2,2,2,2,2,2,2,2,2,2,2,2,2,2,2,2,2,2,2,2,2,2,
2,2,2,2,2,2,2,2,2,2,2,2,2,2,2,2,2,2,2,2,2,2,2,2,2,2,2,2,2,2,2,2,2,2,2,2,
2,2,2,2,2,2,2,2,2,2,2,2,2,2,2,2,2,2,2,2,2,2,2,2,2,2,2,2,2,2,2,2,2,2,2,2,
2,2,2,2,2,2,2,2,2,2,2,4),(-4.0615853247519,-4.02242115167359,-4.01976680171588,
-4.01813846529024,-4.01693563272314,-4.0158299389595,-4.01462605130291,
-4.01317645156132,-4.0095616346049,-3.974972001932,-3.96821340270505,-3.89257618382849,
-3.86105884083779,-3.85656913179024,-3.85534576415173,-3.85461118817929,
-3.85395193827115,-3.85310099528578,-3.85132937746257,-3.83959863761468,
-3.83788523478661,-3.75570548965892,-3.73436892678005,-3.710146306358,-3.70193131382897,
-3.69643081722656,-3.69452920617676,-3.69342752729212,-3.69224586983523,
-3.69073455672694,-3.6876404737086,-3.66831681430305,-3.66067303746865,
-3.65468401750256,-3.60075211613687,-3.59467993113346,-3.58764087790891,
-3.56299376065091,-3.54412326640003,-3.53448774585898,-3.53294169785175,
-3.53213669128762,-3.5314815838859,-3.53081662888454,-3.52957474771371,
-3.52542154258814,-3.45155763404129,-3.41526421989712,-3.38857542624335,
-3.37972920512222,-3.37389724025494,-3.3719534373843,-3.37070161902936,
-3.36951133561992,-3.36796429092388,-3.36472183621126,-3.34093357471604,
-3.24942312001461,-3.21584913996433,-3.2111980544736,-3.20995940421589,
-3.20922137970232,-3.20856280298063,-3.20771782904293,-3.20597656207676,
-3.19491436744379,-3.10309116474825,-3.05853451189306,-3.05379100091248,
-3.05133054946257,-3.0492547074056,-3.04797137999622,-3.04679029313389,
-3.04528384000711,-3.04231555517221,-3.02476481368793,-3.02112813493968,
-2.92444249614953,-2.89279808066718,-2.88829787869645,-2.88707340695115,
-2.88633852702102,-2.88567924293765,-2.88482858126335,-2.88305870718342,
-2.8713708317866,-2.77888643774241,-2.73550962963286,-2.73083944201038,
-2.72840676438722,-2.72634819919006,-2.7250698082245,-2.72388755388883,
-2.72237193521343,-2.71925654731477,-2.69947892073897,-2.69397925913445,
-2.68668761940822,-2.61796497725257,-2.56719032595463,-2.56490486088029,
-2.56396041781971,-2.56328605110428,-2.56267120089874,-2.56184069926522,
-2.56022688773267,-2.557968215489,-2.50018554060422,-2.45049410969333,-2.41218437505629,
-2.4056278258838,-2.40359011374764,-2.40230578561648,-2.40111767053597,
-2.39958542040838,-2.39630024250671,-2.37250082557052,-2.35807007133607,
-2.32052232573239,-2.28966457476984,-2.25480222673668,-2.24353590746572,
-2.2419286884762,-2.24111087623875,-2.2404548998698,-2.23969923075482,-2.23841510616025,
-2.23374384282472,-2.13834438787572,-2.09057279507353,-2.08308196913468,
-2.08094263741557,-2.07963571112717,-2.0784540266717,-2.07694241371128,
-2.07384678561521,-2.0544898637708,-2.04948056942048,-2.030837653146,-1.98110066310485,
-1.95692879108548,-1.94458784122884,-1.9388605493758,-1.9213806224272,-1.9194020178155,
-1.91860051835575,-1.9179320895786,-1.91723775699851,-1.91619563234267,
-1.91327207302077,-1.86860989974576,-1.77656720039791,-1.76165632680691,
-1.7590871060386,-1.75754266172103,-1.75635289353232,-1.75507448174804,
-1.75306241357917,-1.74672137471996,-1.71042246519912,-1.65450394745586,
-1.61177042204784,-1.60981710574321,-1.59834592264835,-1.59658612180481,
-1.59573759390254,-1.59507873186691,-1.59434301774896,-1.59311421429564,
-1.58856609781781,-1.5563205587097,-1.46927492364261,-1.43996426443403,
-1.43684084698413,-1.43529153695447,-1.43417201988404,-1.43298051647101,
-1.43139778167085,-1.42793309213504,-1.35419563179135,-1.28692153919386,
-1.27560958728518,-1.27385703865407,-1.27300994774475,-1.27236701104544,
-1.27165034004064,-1.27089816105163,-1.26978653446161,-1.26780243528164,
-1.25220445802589,-1.23349399149988,-1.14616005544479,-1.1172270624114,
-1.11381296577539,-1.11237431608101,-1.11117344103699,-1.10994028382185,
-1.10813655135382,-1.10335334149979,-1.08047464184013,-1.05873879601757,
-0.955864770861231,-0.951898753551426,-0.950679066036687,-0.95001857327729,
-0.949375930009211,-0.948616738863242,-0.947774642249744,-0.946448394884249,
-0.943911683735059,-0.919926691522573,-0.919114712932559,-0.87209914397502,
-0.82512008103244,-0.819597922451927,-0.814001121436301,-0.793985308394998,
-0.790859078482923,-0.789341346565783,-0.788158873621436,-0.786855136591932,
-0.78473018760486,-0.777378867600789,-0.731103012288167,-0.687701559380429,
-0.643668720257757,-0.64185792032517,-0.630231835406725,-0.628464896421524,
-0.627614885106117,-0.626979223326688,-0.62626627194827,-0.625112765307508,
-0.623742147387329,-0.621087741911813,-0.614556601901783,-0.592231259110943,
-0.504760637523064,-0.495016552353321,-0.471522317778034,-0.468290225047729,
-0.466745308548937,-0.465555395112721,-0.464277042262853,-0.462265518216169,
-0.455929825738729,-0.419682223977332,-0.372108397671492,-0.348971229836516,
-0.327531577286781,-0.307976259323787,-0.306143325672652,-0.305257848179888,
-0.304628664821996,-0.303977708079013,-0.30311636710413,-0.302161872168732,
-0.300565515336198,-0.297294254060778,-0.288607719310095,-0.26662265207392,
-0.187935169392622,-0.181960621682548,-0.173524698132422,-0.168130440016484,
-0.148645466892783,-0.145544070868586,-0.144031410881682,-0.14284971365204,
-0.141543595625807,-0.139407450883285,-0.131946124360121,-0.084482302582598,
-0.000958182641776821),.UNSPECIFIED.);
#838=B_SPLINE_CURVE_WITH_KNOTS('',3,(#49434,#49435,#49436,#49437,#49438,
#49439,#49440,#49441,#49442,#49443,#49444,#49445,#49446,#49447,#49448,#49449,
#49450,#49451,#49452,#49453,#49454,#49455,#49456,#49457,#49458,#49459,#49460,
#49461,#49462,#49463,#49464,#49465,#49466,#49467,#49468,#49469,#49470,#49471,
#49472,#49473,#49474,#49475,#49476,#49477,#49478,#49479,#49480,#49481,#49482,
#49483,#49484,#49485,#49486,#49487,#49488,#49489,#49490,#49491,#49492,#49493,
#49494,#49495,#49496,#49497,#49498,#49499,#49500,#49501,#49502,#49503,#49504,
#49505,#49506,#49507,#49508,#49509,#49510,#49511,#49512,#49513,#49514,#49515,
#49516,#49517,#49518,#49519,#49520,#49521,#49522,#49523,#49524,#49525,#49526,
#49527,#49528,#49529,#49530,#49531,#49532,#49533,#49534,#49535,#49536,#49537,
#49538,#49539,#49540,#49541,#49542,#49543,#49544,#49545,#49546,#49547,#49548,
#49549,#49550,#49551,#49552,#49553,#49554,#49555,#49556,#49557,#49558,#49559,
#49560,#49561,#49562,#49563,#49564,#49565,#49566,#49567,#49568,#49569,#49570,
#49571,#49572,#49573,#49574,#49575,#49576,#49577,#49578,#49579,#49580,#49581,
#49582,#49583,#49584,#49585,#49586,#49587,#49588,#49589,#49590,#49591,#49592,
#49593,#49594,#49595,#49596,#49597,#49598,#49599,#49600,#49601,#49602,#49603,
#49604,#49605,#49606,#49607,#49608,#49609,#49610,#49611,#49612,#49613,#49614,
#49615,#49616,#49617,#49618,#49619,#49620,#49621,#49622,#49623,#49624,#49625,
#49626,#49627,#49628,#49629,#49630,#49631,#49632,#49633,#49634,#49635,#49636,
#49637,#49638,#49639,#49640,#49641,#49642,#49643,#49644,#49645,#49646,#49647,
#49648,#49649,#49650,#49651,#49652,#49653,#49654,#49655,#49656,#49657,#49658,
#49659,#49660,#49661,#49662,#49663,#49664,#49665,#49666,#49667,#49668,#49669,
#49670,#49671,#49672,#49673,#49674,#49675,#49676,#49677,#49678,#49679,#49680,
#49681,#49682,#49683,#49684,#49685,#49686,#49687,#49688,#49689,#49690,#49691,
#49692,#49693,#49694,#49695,#49696,#49697,#49698,#49699,#49700,#49701,#49702,
#49703,#49704,#49705,#49706,#49707,#49708,#49709,#49710,#49711,#49712,#49713,
#49714,#49715,#49716,#49717,#49718,#49719,#49720,#49721,#49722,#49723,#49724,
#49725,#49726,#49727,#49728,#49729,#49730,#49731,#49732,#49733,#49734,#49735,
#49736,#49737,#49738,#49739,#49740,#49741,#49742,#49743,#49744,#49745,#49746,
#49747,#49748,#49749,#49750,#49751,#49752,#49753,#49754,#49755,#49756,#49757,
#49758,#49759,#49760,#49761,#49762,#49763,#49764,#49765,#49766,#49767,#49768,
#49769,#49770,#49771,#49772,#49773,#49774,#49775,#49776,#49777,#49778,#49779,
#49780,#49781,#49782,#49783,#49784,#49785,#49786,#49787,#49788,#49789,#49790,
#49791,#49792,#49793,#49794,#49795,#49796,#49797,#49798,#49799,#49800,#49801,
#49802,#49803,#49804,#49805,#49806,#49807,#49808,#49809,#49810,#49811,#49812,
#49813,#49814,#49815,#49816,#49817,#49818,#49819,#49820,#49821,#49822,#49823,
#49824,#49825,#49826,#49827,#49828,#49829,#49830,#49831,#49832,#49833,#49834,
#49835,#49836,#49837,#49838,#49839,#49840,#49841,#49842,#49843,#49844,#49845,
#49846,#49847,#49848,#49849,#49850,#49851,#49852,#49853,#49854,#49855,#49856,
#49857,#49858,#49859,#49860,#49861,#49862,#49863,#49864,#49865,#49866,#49867,
#49868,#49869,#49870,#49871,#49872,#49873,#49874,#49875,#49876,#49877,#49878,
#49879,#49880,#49881,#49882,#49883,#49884,#49885,#49886,#49887,#49888,#49889,
#49890,#49891,#49892,#49893,#49894,#49895,#49896,#49897,#49898,#49899,#49900,
#49901,#49902,#49903,#49904,#49905,#49906,#49907,#49908,#49909,#49910,#49911,
#49912,#49913,#49914,#49915,#49916,#49917,#49918,#49919,#49920,#49921,#49922,
#49923,#49924,#49925,#49926,#49927,#49928,#49929,#49930,#49931,#49932,#49933,
#49934,#49935,#49936,#49937,#49938,#49939,#49940,#49941,#49942,#49943,#49944,
#49945,#49946,#49947,#49948,#49949,#49950,#49951,#49952,#49953,#49954,#49955,
#49956,#49957,#49958,#49959,#49960,#49961,#49962,#49963,#49964,#49965,#49966,
#49967,#49968,#49969,#49970,#49971,#49972,#49973,#49974,#49975,#49976,#49977,
#49978,#49979,#49980,#49981,#49982,#49983,#49984,#49985,#49986,#49987,#49988,
#49989,#49990,#49991,#49992,#49993,#49994,#49995,#49996,#49997,#49998,#49999),
 .UNSPECIFIED.,.F.,.F.,(4,2,2,2,2,2,2,2,2,2,2,2,2,2,2,2,2,2,2,2,2,2,2,2,
2,2,2,2,2,2,2,2,2,2,2,2,2,2,2,2,2,2,2,2,2,2,2,2,2,2,2,2,2,2,2,2,2,2,2,2,
2,2,2,2,2,2,2,2,2,2,2,2,2,2,2,2,2,2,2,2,2,2,2,2,2,2,2,2,2,2,2,2,2,2,2,2,
2,2,2,2,2,2,2,2,2,2,2,2,2,2,2,2,2,2,2,2,2,2,2,2,2,2,2,2,2,2,2,2,2,2,2,2,
2,2,2,2,2,2,2,2,2,2,2,2,2,2,2,2,2,2,2,2,2,2,2,2,2,2,2,2,2,2,2,2,2,2,2,2,
2,2,2,2,2,2,2,2,2,2,2,2,2,2,2,2,2,2,2,2,2,2,2,2,2,2,2,2,2,2,2,2,2,2,2,2,
2,2,2,2,2,2,2,2,2,2,2,2,2,2,2,2,2,2,2,2,2,2,2,2,2,2,2,2,2,2,2,2,2,2,2,2,
2,2,2,2,2,2,2,2,2,2,2,2,2,2,2,2,2,2,2,2,2,2,2,2,2,2,2,2,2,2,2,2,2,2,2,2,
2,2,2,2,2,2,4),(-4.06131821400407,-4.04564568548944,-4.04423736326734,-4.04336096921321,
-4.04270254315682,-4.04208025663957,-4.04146439300674,-4.04062941647786,
-4.03899775737188,-4.02631729079821,-4.02541205256894,-4.02124691612192,
-3.92430896333871,-3.8903369049557,-3.88424942352277,-3.8822683184449,-3.88099690321561,
-3.8798046826896,-3.87824419742475,-3.87480676355946,-3.84656015452383,
-3.75871054150758,-3.7329862113546,-3.72581388357961,-3.72297083700817,
-3.7215301087255,-3.72032995840551,-3.71960581947867,-3.71898397851182,
-3.71816005225614,-3.71687647612268,-3.71086537974348,-3.65137253589725,
-3.64546905306771,-3.6386940874131,-3.63076020183689,-3.60244471287889,
-3.56781024225568,-3.56164952089861,-3.55965925344438,-3.5583856993459,
-3.55719411775863,-3.55563826579553,-3.55222642121411,-3.52479766965239,
-3.43264887977656,-3.409457218603,-3.40284612211045,-3.40016802113991,-3.39878856214657,
-3.39762951250618,-3.39691509447215,-3.39628146277456,-3.39543527924312,
-3.39368758827325,-3.38248417711807,-3.37885294651681,-3.29339445746787,
-3.24656247878386,-3.23915862061927,-3.23702837819871,-3.23572356047329,
-3.23454152797887,-3.23302633834211,-3.22991234366088,-3.21015681989116,
-3.20466319199457,-3.19883819372107,-3.1259723095705,-3.08162213331746,
-3.07812412241491,-3.07644738687807,-3.07545986212116,-3.07457570657534,
-3.0739207598933,-3.07329867432616,-3.07243984129997,-3.07025506025273,
-3.04112751227071,-2.97132731880923,-2.92396025630536,-2.91650678132836,
-2.91437138282476,-2.91306539379091,-2.91188359936975,-2.91037051829683,
-2.90726721496302,-2.88774317427366,-2.88603520771294,-2.8106881892503,
-2.755636261938,-2.75386574303573,-2.752839964163,-2.75192794674054,-2.75126847074818,
-2.75065298898022,-2.74981978188696,-2.74819527025819,-2.73571486474279,
-2.73265287581106,-2.73225838126724,-2.63405043846526,-2.59956072069251,
-2.59341582964281,-2.59142746680557,-2.59015431253714,-2.58896252629415,
-2.58740557662876,-2.58398796673873,-2.55638147282693,-2.51475910784884,
-2.50711923059234,-2.45956758530017,-2.44044280636558,-2.43131547523018,
-2.42979132415948,-2.42899099848852,-2.42839966133318,-2.42774957990476,
-2.42658117168864,-2.42302008340547,-2.3590863807765,-2.33352106812079,
-2.30442029773425,-2.27879006787232,-2.2737814837377,-2.27004915666551,
-2.26841740945389,-2.26721764951944,-2.26611070583004,-2.26461010654667,
-2.26167881622215,-2.23858845479701,-2.22741245502535,-2.14053720211954,
-2.11228847391277,-2.10950092384306,-2.10743732759163,-2.10653150746877,
-2.10586417593835,-2.10524037910688,-2.10437509575746,-2.10215240373267,
-2.07035172374347,-2.03176400962034,-1.95295629825287,-1.94794654281236,
-1.94604794429724,-1.94491977411415,-1.94373231372073,-1.94217711415402,
-1.93885843641365,-1.8941040247194,-1.8433409018295,-1.81654973446563,-1.78709866599404,
-1.78490902523997,-1.78404937179746,-1.78342708060911,-1.78275881954532,
-1.78184742917021,-1.77975254094595,-1.77691192178312,-1.74771709598557,
-1.66061729017535,-1.65338674685689,-1.64760709120416,-1.62748664461858,
-1.62435604834044,-1.62283761033761,-1.62165522561563,-1.62035223322294,
-1.61822995308544,-1.61090185925383,-1.56486697364556,-1.46721507321892,
-1.4627707987802,-1.46149591163686,-1.46074981205669,-1.46015842948497,
-1.45935869750305,-1.45783780452602,-1.44878863695427,-1.42963852230472,
-1.38220501211115,-1.30678559778606,-1.30229847765498,-1.30066677079691,
-1.2995248386961,-1.29836612291056,-1.29689206018115,-1.29528460874432,
-1.29268018683795,-1.28755317628312,-1.23640758794081,-1.15280526635326,
-1.14086045406957,-1.1390793541436,-1.13823563176969,-1.1375754580195,-1.13684453127135,
-1.13563763042193,-1.13131697739016,-1.10184197864858,-1.0097799992895,
-1.00390478867719,-1.00213764007245,-0.99693115151631,-0.981478722311891,
-0.978879592153521,-0.977326186010432,-0.976159846183014,-0.975003880785112,
-0.973745564895992,-0.971976115754497,-0.968981989974722,-0.96278523948794,
-0.946245021233967,-0.926636323654967,-0.876268719643402,-0.820228425271349,
-0.816978932638856,-0.815852988955089,-0.815211364379053,-0.814617971319561,
-0.813800191930205,-0.812193023496927,-0.800926341443691,-0.765575119764493,
-0.754839614433181,-0.69177111415986,-0.689399716267035,-0.659769061711834,
-0.656635825249673,-0.655083857456858,-0.653963453773098,-0.652795820697045,
-0.651260370465129,-0.64956792169078,-0.646759854999155,-0.641079628516428,
-0.626377918485184,-0.591409248339216,-0.513683636509949,-0.4957582549922,
-0.493964678127234,-0.493088785420703,-0.492462101306534,-0.491796333240201,
-0.490900399770547,-0.488891803162583,-0.48619725163834,-0.459575420234084,
-0.432925952443986,-0.424314982348876,-0.394898026981938,-0.337786390603463,
-0.333906726971192,-0.332372884651655,-0.331257170519479,-0.330086821488342,
-0.328534911378537,-0.326819609350674,-0.323956621613555,-0.31812523584596,
-0.227248109447834,-0.182585044773427,-0.172534228610469,-0.170863609535287,
-0.17002120968391,-0.169362840582242,-0.168623124253374,-0.167377219729346,
-0.162648656051969,-0.128047325479992,-0.0182103218958969,-0.0117709783369783,
-0.00966671952489206,-0.00849750027836917,-0.00733258565330951,-0.00620266545220797,
-0.00478645794291243,-0.000957137645843165),.UNSPECIFIED.);
#839=B_SPLINE_CURVE_WITH_KNOTS('',3,(#50001,#50002,#50003,#50004,#50005,
#50006,#50007,#50008,#50009,#50010,#50011,#50012,#50013,#50014,#50015,#50016,
#50017,#50018,#50019,#50020,#50021,#50022,#50023,#50024,#50025,#50026,#50027,
#50028,#50029,#50030,#50031,#50032,#50033,#50034,#50035,#50036,#50037,#50038,
#50039,#50040,#50041,#50042,#50043,#50044,#50045,#50046,#50047,#50048,#50049,
#50050,#50051,#50052,#50053,#50054,#50055,#50056,#50057,#50058,#50059,#50060,
#50061,#50062,#50063,#50064,#50065,#50066,#50067,#50068,#50069,#50070,#50071,
#50072,#50073,#50074,#50075,#50076,#50077,#50078,#50079,#50080,#50081,#50082,
#50083,#50084,#50085,#50086,#50087,#50088,#50089,#50090,#50091,#50092,#50093,
#50094,#50095,#50096,#50097,#50098,#50099,#50100,#50101,#50102,#50103,#50104,
#50105,#50106,#50107,#50108,#50109,#50110,#50111,#50112,#50113,#50114,#50115,
#50116,#50117,#50118,#50119,#50120,#50121,#50122,#50123,#50124,#50125,#50126,
#50127,#50128,#50129,#50130,#50131,#50132,#50133,#50134,#50135,#50136,#50137,
#50138,#50139,#50140,#50141,#50142,#50143,#50144,#50145,#50146,#50147,#50148,
#50149,#50150,#50151,#50152,#50153,#50154,#50155,#50156,#50157,#50158,#50159,
#50160,#50161,#50162,#50163,#50164,#50165,#50166,#50167,#50168,#50169,#50170,
#50171,#50172,#50173,#50174,#50175,#50176,#50177,#50178,#50179,#50180,#50181,
#50182,#50183,#50184,#50185,#50186,#50187,#50188,#50189,#50190,#50191,#50192,
#50193,#50194,#50195,#50196,#50197,#50198,#50199,#50200,#50201,#50202,#50203,
#50204,#50205,#50206,#50207,#50208,#50209,#50210,#50211,#50212,#50213,#50214,
#50215,#50216,#50217,#50218,#50219,#50220,#50221,#50222,#50223,#50224,#50225,
#50226,#50227,#50228,#50229,#50230,#50231,#50232,#50233,#50234,#50235,#50236,
#50237,#50238,#50239,#50240,#50241,#50242,#50243,#50244,#50245,#50246,#50247,
#50248,#50249,#50250,#50251,#50252,#50253,#50254,#50255,#50256,#50257,#50258,
#50259,#50260,#50261,#50262,#50263,#50264,#50265,#50266,#50267,#50268,#50269,
#50270,#50271,#50272,#50273,#50274,#50275,#50276,#50277,#50278,#50279,#50280,
#50281,#50282,#50283,#50284,#50285,#50286,#50287,#50288,#50289,#50290,#50291,
#50292,#50293,#50294,#50295,#50296,#50297,#50298,#50299,#50300,#50301,#50302,
#50303,#50304,#50305,#50306,#50307,#50308,#50309,#50310,#50311,#50312,#50313,
#50314,#50315,#50316,#50317,#50318,#50319,#50320,#50321,#50322,#50323,#50324,
#50325,#50326,#50327,#50328,#50329,#50330,#50331,#50332,#50333,#50334,#50335,
#50336,#50337,#50338,#50339,#50340,#50341,#50342,#50343,#50344,#50345,#50346,
#50347,#50348,#50349,#50350,#50351,#50352,#50353,#50354,#50355,#50356,#50357,
#50358,#50359,#50360,#50361,#50362,#50363,#50364,#50365,#50366,#50367,#50368,
#50369,#50370,#50371,#50372,#50373,#50374,#50375,#50376,#50377,#50378,#50379,
#50380,#50381,#50382,#50383,#50384,#50385,#50386,#50387,#50388,#50389,#50390,
#50391,#50392,#50393,#50394,#50395,#50396,#50397,#50398,#50399,#50400,#50401,
#50402,#50403,#50404,#50405,#50406,#50407,#50408,#50409,#50410,#50411,#50412,
#50413,#50414,#50415,#50416,#50417,#50418,#50419,#50420,#50421,#50422,#50423,
#50424,#50425,#50426,#50427,#50428,#50429,#50430,#50431,#50432,#50433,#50434,
#50435,#50436,#50437,#50438,#50439,#50440,#50441,#50442,#50443,#50444,#50445,
#50446,#50447,#50448,#50449,#50450,#50451,#50452,#50453,#50454,#50455,#50456,
#50457,#50458,#50459,#50460,#50461,#50462,#50463,#50464,#50465,#50466,#50467,
#50468,#50469,#50470,#50471,#50472,#50473,#50474,#50475,#50476,#50477,#50478,
#50479,#50480,#50481,#50482,#50483,#50484,#50485,#50486,#50487,#50488,#50489,
#50490,#50491,#50492,#50493,#50494,#50495,#50496,#50497,#50498,#50499,#50500,
#50501,#50502,#50503,#50504,#50505,#50506,#50507,#50508,#50509,#50510,#50511,
#50512,#50513,#50514,#50515,#50516,#50517,#50518,#50519,#50520,#50521,#50522,
#50523,#50524,#50525,#50526,#50527,#50528,#50529,#50530,#50531,#50532,#50533,
#50534,#50535,#50536,#50537,#50538,#50539,#50540,#50541,#50542),
 .UNSPECIFIED.,.F.,.F.,(4,2,2,2,2,2,2,2,2,2,2,2,2,2,2,2,2,2,2,2,2,2,2,2,
2,2,2,2,2,2,2,2,2,2,2,2,2,2,2,2,2,2,2,2,2,2,2,2,2,2,2,2,2,2,2,2,2,2,2,2,
2,2,2,2,2,2,2,2,2,2,2,2,2,2,2,2,2,2,2,2,2,2,2,2,2,2,2,2,2,2,2,2,2,2,2,2,
2,2,2,2,2,2,2,2,2,2,2,2,2,2,2,2,2,2,2,2,2,2,2,2,2,2,2,2,2,2,2,2,2,2,2,2,
2,2,2,2,2,2,2,2,2,2,2,2,2,2,2,2,2,2,2,2,2,2,2,2,2,2,2,2,2,2,2,2,2,2,2,2,
2,2,2,2,2,2,2,2,2,2,2,2,2,2,2,2,2,2,2,2,2,2,2,2,2,2,2,2,2,2,2,2,2,2,2,2,
2,2,2,2,2,2,2,2,2,2,2,2,2,2,2,2,2,2,2,2,2,2,2,2,2,2,2,2,2,2,2,2,2,2,2,2,
2,2,2,2,2,2,2,2,2,2,2,2,2,2,2,2,2,2,2,2,2,2,2,2,2,2,2,2,2,2,4),(-4.06091416108814,
-4.0556667509442,-3.9436925009123,-3.91010830592124,-3.90797102344079,-3.90705212921347,
-3.90638254636448,-3.90576212589432,-3.90490963505416,-3.9032094234937,
-3.8885334434254,-3.88617042623338,-3.88390122518972,-3.8827905315805,-3.87843199784321,
-3.81552956527625,-3.75223282399225,-3.74938487599442,-3.74767592701344,
-3.74612844383602,-3.744958977978,-3.74384225751226,-3.74230391594249,-3.73839632725442,
-3.67353063739135,-3.66582520044604,-3.61454556991071,-3.5954565230365,
-3.58649414972096,-3.58497729887887,-3.58417848360081,-3.58358725564961,
-3.58284065139721,-3.581563240286,-3.57709509492826,-3.4799776413505,-3.42977925247706,
-3.42679373682979,-3.42502793931893,-3.42343955040443,-3.4222630654745,
-3.42115722499087,-3.41966082261222,-3.41599666233606,-3.3756269175606,
-3.31550394113404,-3.30229013156382,-3.26799199500219,-3.26488763570596,
-3.26263963984912,-3.2617016913217,-3.26102869654279,-3.260412732604,-3.25957734951944,
-3.25794409567889,-3.24521959032898,-3.24176591405113,-3.23798518151985,
-3.23593808786589,-3.23334438802609,-3.16536605761403,-3.10625205613832,
-3.1036763256634,-3.10208101039202,-3.10061575169611,-3.09945922894538,
-3.098314237039,-3.09667084970325,-3.09210683550982,-3.0152065257964,-2.96883198009591,
-2.94557025935954,-2.94066893252356,-2.93940787217447,-2.93866496412505,
-2.93800749445283,-2.93717123391376,-2.93547288269604,-2.92528228694502,
-2.89550521360718,-2.83378145309395,-2.78390625696618,-2.78120855655403,
-2.77956219286603,-2.77805996635305,-2.77689765044283,-2.77576668374344,
-2.77417463497587,-2.76993988947724,-2.70436133204095,-2.67280355717629,
-2.61968405261242,-2.61739681355262,-2.61645223209729,-2.61577797984619,
-2.61516338742918,-2.61433345179782,-2.61272137710549,-2.60055380308683,
-2.59922739949456,-2.59700610554675,-2.59461440062683,-2.58721427415502,
-2.49649018312904,-2.46386889162928,-2.45793164818458,-2.4559692501439,
-2.45470193620988,-2.45350790348953,-2.45193683120957,-2.44927674159865,
-2.43264900388173,-2.430436058951,-2.42530531166532,-2.35811727265227,-2.33168453464077,
-2.29985675129688,-2.29534262724214,-2.29411715051974,-2.29338223518648,
-2.29272329619763,-2.29187359325637,-2.29010753782797,-2.27849393606782,
-2.20343714200941,-2.14135564521112,-2.13533536153555,-2.13336258889569,
-2.13209301207089,-2.13090001554844,-2.12933490038084,-2.12669507330763,
-2.11045885270608,-2.10484327172566,-2.03072314084274,-1.9757882926889,
-1.97250065147887,-1.97136924064359,-1.97072663313535,-1.97013370922062,
-1.96931865681988,-1.96772402255746,-1.95681039801111,-1.92900910995094,
-1.87121573337088,-1.81598635147893,-1.81212211723945,-1.81059123154371,
-1.80947656257617,-1.80828226932987,-1.80668212572828,-1.80312353706856,
-1.75370694917921,-1.66228023394796,-1.65091083266486,-1.64915558540535,
-1.64830793108314,-1.64764914370586,-1.64691287346963,-1.64568169293121,
-1.64110888290018,-1.60855113487346,-1.5207548039168,-1.49247756617037,
-1.4890388110489,-1.48747795839738,-1.48628555279233,-1.48501403307291,
-1.4830329564316,-1.47694703141396,-1.38352956024237,-1.32989974993652,
-1.32692713878969,-1.32584180784821,-1.32520831786053,-1.32455927944164,
-1.32371185416105,-1.32277559304969,-1.32122341409803,-1.31807522979958,
-1.2828579225852,-1.18854229333696,-1.16911742243247,-1.16601890123848,
-1.16450683966619,-1.16332524377902,-1.16201886400042,-1.15988144407788,
-1.1524073366178,-1.10480340074239,-1.01774553687216,-1.00538332313789,
-1.0037631972345,-1.00293112475591,-1.00231593383974,-1.00165603226417,
-1.00074209091452,-0.99971405163293,-0.997937976138313,-0.994154913084048,
-0.910333229606811,-0.847648011780672,-0.843743669122313,-0.84220585481626,
-0.841089271534206,-0.839895864505766,-0.83830197385835,-0.834777991860088,
-0.784375553338656,-0.697424836094035,-0.682716460602723,-0.681015084363849,
-0.680162256653613,-0.679541707109479,-0.678916356535199,-0.678043725881779,
-0.676142772124824,-0.673604316395439,-0.667458298973885,-0.649066011455502,
-0.613828560200457,-0.54375115014343,-0.523646891457507,-0.520516633834204,
-0.518998102423274,-0.517815528623805,-0.51651220989175,-0.514389133104203,
-0.507055741874997,-0.46097035809489,-0.451408864897502,-0.443627658960177,
-0.437077711691942,-0.384066163695826,-0.379460679110359,-0.3784661848796,
-0.377226172996081,-0.374543689670793,-0.372594755724589,-0.35995792329208,
-0.358327629382752,-0.357492921968437,-0.356877046274825,-0.35625471220879,
-0.355367567839754,-0.353395220552537,-0.350734636646391,-0.344182815422075,
-0.321609991224706,-0.234226633730324,-0.225826474101105,-0.220421206119031,
-0.200914784647962,-0.197812232088737,-0.196299278479867,-0.19511747496863,
-0.193811365053867,-0.19167551799272,-0.184218022278526,-0.136798209850487,
-0.0687485708789001,-0.0641404148857407,-0.0377946982054035,-0.0356562163948424,
-0.034805315206907,-0.034185289084645,-0.0335602932984056,-0.0329057838157608,
-0.0320403943492102,-0.0306585186817549,-0.000956380862327205),
 .UNSPECIFIED.);
#840=B_SPLINE_CURVE_WITH_KNOTS('',3,(#50544,#50545,#50546,#50547,#50548,
#50549,#50550,#50551,#50552,#50553,#50554,#50555,#50556,#50557,#50558,#50559,
#50560,#50561,#50562,#50563,#50564,#50565,#50566,#50567,#50568,#50569,#50570,
#50571,#50572,#50573,#50574,#50575,#50576,#50577,#50578,#50579,#50580,#50581,
#50582,#50583,#50584,#50585,#50586,#50587,#50588,#50589,#50590,#50591,#50592,
#50593,#50594,#50595,#50596,#50597,#50598,#50599,#50600,#50601,#50602,#50603,
#50604,#50605,#50606,#50607,#50608,#50609,#50610,#50611,#50612,#50613,#50614,
#50615,#50616,#50617,#50618,#50619,#50620,#50621,#50622,#50623,#50624,#50625,
#50626,#50627,#50628,#50629,#50630,#50631,#50632,#50633,#50634,#50635,#50636,
#50637,#50638,#50639,#50640,#50641,#50642,#50643,#50644,#50645,#50646,#50647,
#50648,#50649,#50650,#50651,#50652,#50653,#50654,#50655,#50656,#50657,#50658,
#50659,#50660,#50661,#50662,#50663,#50664,#50665,#50666,#50667,#50668,#50669,
#50670,#50671,#50672,#50673,#50674,#50675,#50676,#50677,#50678,#50679,#50680,
#50681,#50682,#50683,#50684,#50685,#50686,#50687,#50688,#50689,#50690,#50691,
#50692,#50693,#50694,#50695,#50696,#50697,#50698,#50699,#50700,#50701,#50702,
#50703,#50704,#50705,#50706,#50707,#50708,#50709,#50710,#50711,#50712,#50713,
#50714,#50715,#50716,#50717,#50718,#50719,#50720,#50721,#50722,#50723,#50724,
#50725,#50726,#50727,#50728,#50729,#50730,#50731,#50732,#50733,#50734,#50735,
#50736,#50737,#50738,#50739,#50740,#50741,#50742,#50743,#50744,#50745,#50746,
#50747,#50748,#50749,#50750,#50751,#50752,#50753,#50754,#50755,#50756,#50757,
#50758,#50759,#50760,#50761,#50762,#50763,#50764,#50765,#50766,#50767,#50768,
#50769,#50770,#50771,#50772,#50773,#50774,#50775,#50776,#50777,#50778,#50779,
#50780,#50781,#50782,#50783,#50784,#50785,#50786,#50787,#50788,#50789,#50790,
#50791,#50792,#50793,#50794,#50795,#50796,#50797,#50798,#50799,#50800,#50801,
#50802,#50803,#50804,#50805,#50806,#50807,#50808,#50809,#50810,#50811,#50812,
#50813,#50814,#50815,#50816,#50817,#50818,#50819,#50820,#50821,#50822,#50823,
#50824,#50825,#50826,#50827,#50828,#50829,#50830,#50831,#50832,#50833,#50834,
#50835,#50836,#50837,#50838,#50839,#50840,#50841,#50842,#50843,#50844,#50845,
#50846,#50847,#50848,#50849,#50850,#50851,#50852,#50853,#50854,#50855,#50856,
#50857,#50858,#50859,#50860,#50861,#50862,#50863,#50864,#50865,#50866,#50867,
#50868,#50869,#50870,#50871,#50872,#50873,#50874,#50875,#50876,#50877,#50878,
#50879,#50880,#50881,#50882,#50883,#50884,#50885,#50886,#50887,#50888,#50889,
#50890,#50891,#50892,#50893,#50894,#50895,#50896,#50897,#50898,#50899,#50900,
#50901,#50902,#50903,#50904,#50905,#50906,#50907,#50908,#50909,#50910,#50911,
#50912,#50913,#50914,#50915,#50916,#50917,#50918,#50919,#50920,#50921,#50922,
#50923,#50924,#50925,#50926,#50927,#50928,#50929,#50930,#50931,#50932,#50933,
#50934,#50935,#50936,#50937,#50938,#50939,#50940,#50941,#50942,#50943,#50944,
#50945,#50946,#50947,#50948,#50949,#50950,#50951,#50952,#50953,#50954,#50955,
#50956,#50957,#50958,#50959,#50960,#50961,#50962,#50963,#50964,#50965,#50966,
#50967,#50968,#50969,#50970,#50971,#50972,#50973,#50974,#50975,#50976,#50977,
#50978,#50979,#50980,#50981,#50982,#50983,#50984,#50985,#50986,#50987,#50988,
#50989,#50990,#50991,#50992,#50993,#50994,#50995,#50996,#50997,#50998,#50999,
#51000,#51001,#51002,#51003,#51004,#51005,#51006,#51007,#51008,#51009,#51010,
#51011,#51012,#51013,#51014,#51015,#51016,#51017,#51018,#51019,#51020,#51021,
#51022,#51023,#51024,#51025,#51026,#51027,#51028,#51029,#51030,#51031,#51032,
#51033,#51034,#51035,#51036,#51037,#51038,#51039,#51040,#51041,#51042,#51043,
#51044,#51045,#51046,#51047,#51048,#51049,#51050,#51051,#51052,#51053,#51054,
#51055,#51056,#51057,#51058,#51059,#51060,#51061,#51062,#51063,#51064,#51065,
#51066,#51067,#51068,#51069,#51070,#51071,#51072,#51073,#51074,#51075,#51076,
#51077,#51078,#51079),.UNSPECIFIED.,.F.,.F.,(4,2,2,2,2,2,2,2,2,2,2,2,2,
2,2,2,2,2,2,2,2,2,2,2,2,2,2,2,2,2,2,2,2,2,2,2,2,2,2,2,2,2,2,2,2,2,2,2,2,
2,2,2,2,2,2,2,2,2,2,2,2,2,2,2,2,2,2,2,2,2,2,2,2,2,2,2,2,2,2,2,2,2,2,2,2,
2,2,2,2,2,2,2,2,2,2,2,2,2,2,2,2,2,2,2,2,2,2,2,2,2,2,2,2,2,2,2,2,2,2,2,2,
2,2,2,2,2,2,2,2,2,2,2,2,2,2,2,2,2,2,2,2,2,2,2,2,2,2,2,2,2,2,2,2,2,2,2,2,
2,2,2,2,2,2,2,2,2,2,2,2,2,2,2,2,2,2,2,2,2,2,2,2,2,2,2,2,2,2,2,2,2,2,2,2,
2,2,2,2,2,2,2,2,2,2,2,2,2,2,2,2,2,2,2,2,2,2,2,2,2,2,2,2,2,2,2,2,2,2,2,2,
2,2,2,2,2,2,2,2,2,2,2,2,2,2,2,2,2,2,2,2,2,2,2,2,2,2,2,2,2,2,2,2,2,2,2,2,
2,2,4),(-4.06173053606492,-3.99264303614414,-3.94484835785685,-3.93735559998355,
-3.93521614870415,-3.93390924307517,-3.93272763841237,-3.93121621213845,
-3.92812126335377,-3.90877612379454,-3.9036422234948,-3.89712050512331,
-3.8128236543981,-3.78845749278649,-3.77949768982423,-3.77615167430205,
-3.77378674945593,-3.77282831858377,-3.77221389430502,-3.7715453283576,
-3.770743397285,-3.76876235051928,-3.75120052475007,-3.75036001707103,-3.71927516592442,
-3.69746709833839,-3.64791831888225,-3.62231286077033,-3.61472294684731,
-3.61257343342437,-3.61126417835272,-3.61008291637658,-3.60857533248586,
-3.60560193780343,-3.5879540991384,-3.58310720217572,-3.51111422070594,
-3.47868490999338,-3.46064605434355,-3.4550531182303,-3.45268485188964,
-3.45089138372212,-3.45003730221702,-3.44940721684852,-3.44877963568405,
-3.44790032963799,-3.44559200185814,-3.40550548517388,-3.38214724556063,
-3.33866800639041,-3.29471002283131,-3.29094935811541,-3.28931233540183,
-3.28811143515288,-3.28700536304904,-3.28550886820951,-3.28259419288882,
-3.2599757286754,-3.25196197466975,-3.20451516546109,-3.15681553436925,
-3.13445693623121,-3.13099240456683,-3.12932739559036,-3.12797725110428,
-3.12721884766654,-3.12662545940449,-3.12585638729191,-3.12451460157863,
-3.11926016132402,-3.0113154327832,-2.97527745973739,-2.96896372002264,
-2.96695483347477,-2.96567707553461,-2.96448696048117,-2.96294070992385,
-2.95970198306808,-2.93600909727482,-2.92651184440248,-2.83901753091584,
-2.81037632474626,-2.80756663156588,-2.80613814904991,-2.80525327646317,
-2.80444191581472,-2.80379749096938,-2.80305330001174,-2.80178694138151,
-2.79741950095655,-2.71478282397944,-2.6486154801934,-2.64517000979253,
-2.64359071003381,-2.64239957726533,-2.64127878095986,-2.63972511469512,
-2.63658483139031,-2.60665635943988,-2.53331614478316,-2.50881070835075,
-2.48686198874991,-2.48323741860155,-2.48210568448133,-2.48139163237983,
-2.48072616472114,-2.47984721455847,-2.47787840611672,-2.46071583876957,
-2.45732241253205,-2.36294042199256,-2.32938153115206,-2.32333934188926,
-2.32136360610057,-2.32009321355554,-2.31890022777551,-2.31733625067446,
-2.31470082572,-2.29855623104818,-2.29667865817754,-2.2908076709268,-2.28006334183379,
-2.27403223640754,-2.19972198979496,-2.17319586770569,-2.16137911881433,
-2.15975402547841,-2.15893259981489,-2.15827642912776,-2.15752354308551,
-2.15625104959744,-2.15168935952669,-2.05539045819502,-2.03142774934723,
-2.00311358054126,-1.99967362779058,-1.99811253654006,-1.99692007459681,
-1.99564861676447,-1.99366788754656,-1.98758495296315,-1.89423735176611,
-1.85004337640933,-1.83875090562492,-1.83699913316001,-1.83615214829198,
-1.83549341972214,-1.83475672571841,-1.83352372569639,-1.82893189463437,
-1.79613151984194,-1.70811750861109,-1.68029497816602,-1.67687044583286,
-1.67531220196706,-1.67412019566093,-1.67284755511164,-1.67086154161174,
-1.66473588138089,-1.57029637613813,-1.5258475857883,-1.51584740628491,
-1.51417967546572,-1.51333802211168,-1.51267988705974,-1.51194005969009,
-1.51069310663446,-1.50595065573003,-1.47115109057596,-1.41273715946364,
-1.35830366104016,-1.35444511952713,-1.35291502561912,-1.35180041766073,
-1.35060570389171,-1.34903626622373,-1.34560972519387,-1.34106665314426,
-1.29967671956274,-1.23207162864324,-1.20706582530678,-1.20636022675044,
-1.19340938410148,-1.19176779043052,-1.1909301916008,-1.19031358879223,
-1.18964092329423,-1.18870523628331,-1.18647113261794,-1.18339119837556,
-1.14960945984518,-1.05588195739435,-1.03444739855447,-1.03125881967434,
-1.02974532527445,-1.02856019315321,-1.02745966805291,-1.02560020435027,
-1.02040272412348,-0.993933753576714,-0.934129392697989,-0.890644343056778,
-0.886883653438565,-0.883837406146768,-0.870704975186686,-0.868898099530721,
-0.868036727203534,-0.867374136961964,-0.866652414899742,-0.865486133933068,
-0.861554297337804,-0.836418227264234,-0.752953776746852,-0.739198709708271,
-0.712124426480502,-0.708724022951162,-0.707170302706462,-0.705979067048614,
-0.704879072209079,-0.703074810278662,-0.698257353894672,-0.691310069017453,
-0.671994125756401,-0.625410528122825,-0.551241930370032,-0.54704823483272,
-0.545801712935961,-0.545135852452928,-0.544480867136637,-0.543677472609889,
-0.542138920352289,-0.53268038504514,-0.523995392220786,-0.498244311534951,
-0.491131377823437,-0.437441734161144,-0.41923535604897,-0.389644431834765,
-0.386513155906929,-0.384961768628703,-0.383841601530186,-0.382650196159206,
-0.381483304089254,-0.378798378120559,-0.363251857950231,-0.34101501112171,
-0.314201777393347,-0.228847067213466,-0.224450586783784,-0.223180989816218,
-0.222436073329684,-0.221844533658508,-0.221043182586111,-0.219514621411093,
-0.210291879048887,-0.191420421920683,-0.122635644191065,-0.115494019344356,
-0.0967744990380212,-0.0669614794112179,-0.0638240600062391,-0.0622710547105643,
-0.0611503848441586,-0.0599590617582436,-0.0587924486679108,-0.0572628352817411,
-0.0548437482695064,-0.000956655812675297),.UNSPECIFIED.);
#841=B_SPLINE_CURVE_WITH_KNOTS('',3,(#51081,#51082,#51083,#51084,#51085,
#51086,#51087,#51088,#51089,#51090),.UNSPECIFIED.,.F.,.F.,(4,1,1,1,1,1,
1,4),(103.67256099167,104.647102545754,105.645894949522,106.64468735329,
107.643479757058,108.642272160826,109.641064564594,109.955736404437),
 .UNSPECIFIED.);
#842=B_SPLINE_CURVE_WITH_KNOTS('',3,(#51092,#51093,#51094,#51095,#51096,
#51097,#51098,#51099,#51100,#51101,#51102,#51103,#51104,#51105,#51106,#51107,
#51108,#51109,#51110,#51111,#51112,#51113,#51114,#51115,#51116,#51117,#51118,
#51119,#51120,#51121,#51122,#51123,#51124,#51125,#51126,#51127,#51128,#51129,
#51130,#51131,#51132,#51133,#51134,#51135,#51136,#51137,#51138,#51139,#51140,
#51141,#51142,#51143,#51144,#51145,#51146,#51147,#51148,#51149,#51150,#51151,
#51152,#51153,#51154,#51155,#51156,#51157,#51158,#51159,#51160,#51161,#51162,
#51163,#51164,#51165,#51166,#51167,#51168,#51169,#51170,#51171,#51172,#51173,
#51174,#51175,#51176,#51177,#51178,#51179,#51180,#51181,#51182,#51183,#51184,
#51185,#51186,#51187,#51188,#51189,#51190,#51191,#51192,#51193,#51194,#51195,
#51196,#51197,#51198,#51199,#51200,#51201,#51202,#51203,#51204,#51205,#51206,
#51207,#51208,#51209,#51210,#51211,#51212,#51213,#51214,#51215,#51216,#51217,
#51218,#51219,#51220,#51221,#51222,#51223,#51224,#51225,#51226,#51227,#51228,
#51229,#51230,#51231,#51232,#51233,#51234,#51235,#51236,#51237,#51238,#51239,
#51240,#51241,#51242,#51243,#51244,#51245,#51246,#51247,#51248,#51249,#51250,
#51251,#51252,#51253,#51254,#51255,#51256,#51257,#51258,#51259,#51260,#51261,
#51262,#51263,#51264,#51265,#51266,#51267,#51268,#51269,#51270,#51271,#51272,
#51273,#51274,#51275,#51276,#51277,#51278,#51279,#51280,#51281,#51282,#51283,
#51284,#51285,#51286,#51287,#51288,#51289,#51290,#51291,#51292,#51293,#51294,
#51295,#51296,#51297,#51298,#51299,#51300,#51301,#51302,#51303,#51304,#51305,
#51306,#51307,#51308,#51309,#51310,#51311,#51312,#51313,#51314,#51315,#51316,
#51317,#51318,#51319,#51320,#51321,#51322,#51323,#51324,#51325,#51326,#51327,
#51328,#51329,#51330,#51331,#51332,#51333,#51334,#51335,#51336,#51337,#51338,
#51339,#51340,#51341,#51342,#51343,#51344,#51345,#51346,#51347,#51348,#51349,
#51350,#51351,#51352,#51353,#51354,#51355,#51356,#51357,#51358,#51359,#51360,
#51361,#51362,#51363,#51364,#51365,#51366,#51367,#51368,#51369,#51370,#51371,
#51372,#51373,#51374,#51375,#51376,#51377,#51378,#51379,#51380,#51381,#51382,
#51383,#51384,#51385,#51386,#51387,#51388,#51389,#51390,#51391,#51392,#51393,
#51394,#51395,#51396,#51397,#51398,#51399,#51400,#51401,#51402,#51403,#51404,
#51405,#51406,#51407,#51408,#51409,#51410,#51411,#51412,#51413,#51414,#51415,
#51416,#51417,#51418,#51419,#51420,#51421,#51422,#51423,#51424,#51425,#51426,
#51427,#51428,#51429,#51430,#51431,#51432,#51433,#51434,#51435,#51436,#51437,
#51438,#51439,#51440,#51441,#51442,#51443,#51444,#51445,#51446,#51447,#51448,
#51449,#51450,#51451,#51452,#51453,#51454,#51455,#51456,#51457,#51458,#51459,
#51460,#51461,#51462,#51463,#51464,#51465,#51466,#51467,#51468,#51469,#51470,
#51471,#51472,#51473,#51474,#51475,#51476,#51477,#51478,#51479,#51480,#51481,
#51482,#51483,#51484,#51485,#51486,#51487,#51488,#51489,#51490,#51491,#51492,
#51493,#51494,#51495,#51496,#51497,#51498,#51499,#51500,#51501,#51502,#51503,
#51504,#51505,#51506,#51507,#51508,#51509,#51510,#51511,#51512,#51513,#51514,
#51515,#51516,#51517,#51518,#51519,#51520,#51521,#51522,#51523,#51524,#51525,
#51526,#51527,#51528,#51529,#51530,#51531,#51532,#51533,#51534,#51535,#51536,
#51537,#51538,#51539,#51540,#51541,#51542,#51543,#51544,#51545,#51546,#51547,
#51548,#51549,#51550,#51551,#51552,#51553,#51554,#51555,#51556,#51557,#51558,
#51559,#51560,#51561,#51562,#51563,#51564,#51565,#51566,#51567,#51568,#51569,
#51570,#51571,#51572,#51573,#51574,#51575,#51576,#51577,#51578,#51579,#51580,
#51581,#51582,#51583,#51584,#51585,#51586,#51587,#51588,#51589,#51590,#51591,
#51592,#51593,#51594,#51595,#51596,#51597,#51598,#51599,#51600,#51601,#51602,
#51603,#51604,#51605,#51606,#51607,#51608,#51609,#51610,#51611,#51612,#51613,
#51614,#51615,#51616,#51617,#51618,#51619,#51620,#51621,#51622,#51623,#51624,
#51625,#51626,#51627,#51628,#51629,#51630,#51631,#51632,#51633,#51634,#51635,
#51636,#51637,#51638,#51639,#51640,#51641,#51642,#51643,#51644,#51645,#51646,
#51647,#51648,#51649,#51650,#51651,#51652,#51653,#51654,#51655,#51656,#51657),
 .UNSPECIFIED.,.F.,.F.,(4,2,2,2,2,2,2,2,2,2,2,2,2,2,2,2,2,2,2,2,2,2,2,2,
2,2,2,2,2,2,2,2,2,2,2,2,2,2,2,2,2,2,2,2,2,2,2,2,2,2,2,2,2,2,2,2,2,2,2,2,
2,2,2,2,2,2,2,2,2,2,2,2,2,2,2,2,2,2,2,2,2,2,2,2,2,2,2,2,2,2,2,2,2,2,2,2,
2,2,2,2,2,2,2,2,2,2,2,2,2,2,2,2,2,2,2,2,2,2,2,2,2,2,2,2,2,2,2,2,2,2,2,2,
2,2,2,2,2,2,2,2,2,2,2,2,2,2,2,2,2,2,2,2,2,2,2,2,2,2,2,2,2,2,2,2,2,2,2,2,
2,2,2,2,2,2,2,2,2,2,2,2,2,2,2,2,2,2,2,2,2,2,2,2,2,2,2,2,2,2,2,2,2,2,2,2,
2,2,2,2,2,2,2,2,2,2,2,2,2,2,2,2,2,2,2,2,2,2,2,2,2,2,2,2,2,2,2,2,2,2,2,2,
2,2,2,2,2,2,2,2,2,2,2,2,2,2,2,2,2,2,2,2,2,2,2,2,2,2,2,2,2,2,2,2,2,2,2,2,
2,2,2,2,2,2,4),(-4.06063781096923,-4.05731981415401,-4.05493204612338,-4.05405547611466,
-4.05339709140699,-4.05277509561439,-4.05215957747037,-4.05132546753032,
-4.04969667783987,-4.04746614297703,-4.04326403066187,-3.94880956986452,
-3.90262327008353,-3.89528130962922,-3.89315817124286,-3.89185534755516,
-3.89067357316091,-3.88915655679123,-3.88603115813888,-3.86600337926848,
-3.8603899284599,-3.85467508185895,-3.84907160635317,-3.76365865655495,
-3.73940431971863,-3.73497260055438,-3.73297753766551,-3.73186166916856,
-3.73088572015443,-3.73021286442228,-3.72954682458925,-3.7287282515589,
-3.72672707238446,-3.70746908969222,-3.68432038179969,-3.66318293918734,
-3.65679254868836,-3.64945588456887,-3.64083689242829,-3.61260525155242,
-3.57860803202467,-3.57251809823496,-3.57053686265228,-3.56926553528361,
-3.56807351891859,-3.56651347630985,-3.56307773206154,-3.53487372840895,
-3.44427731738438,-3.42049611574097,-3.41382017520459,-3.41112300830772,
-3.40973652448865,-3.40886929940274,-3.40807086265942,-3.4074277753202,
-3.40667522572414,-3.40540365976966,-3.40084875387618,-3.31504627451749,
-3.3030766389839,-3.25246312756124,-3.24893910967758,-3.24734548121225,
-3.24615238365218,-3.24503617098564,-3.24349899437376,-3.23959694494856,
-3.17747264417216,-3.09314260630246,-3.08931743941957,-3.08752700375098,
-3.08649321755663,-3.08557553430906,-3.08514651218657,-3.08450219141766,
-3.08364870901516,-3.08186342670908,-3.06981126832831,-2.97798900654007,
-2.93442642431781,-2.92974537644303,-2.92621058904379,-2.92461492913071,
-2.92342146248629,-2.92230573934755,-2.92077054630504,-2.91688043320047,
-2.85768622918004,-2.85113583616591,-2.84358304026967,-2.79462941547942,
-2.76842342281109,-2.76575399182482,-2.76437789215205,-2.7635150158085,
-2.76271965410571,-2.76207688741806,-2.76141980250643,-2.76021630248024,
-2.75638035113015,-2.68838080293436,-2.63791704732392,-2.61241871416025,
-2.60487965747516,-2.60273585316696,-2.60142820171785,-2.60024716813251,
-2.59873819371189,-2.5956542923349,-2.57652993769076,-2.57143880879908,
-2.55715257302761,-2.48087638175396,-2.45415898466579,-2.44259823607874,
-2.4409816855277,-2.44016213160225,-2.43950624720595,-2.43884986580951,
-2.43764994699046,-2.43384303510625,-2.36765949138991,-2.3517713323542,
-2.28445680503371,-2.2810085667686,-2.2794290072221,-2.27823809670365,-2.27711781658982,
-2.27556535396729,-2.27242902849891,-2.24262579203528,-2.19463350944136,
-2.14775173422193,-2.12952698900693,-2.11991166596451,-2.11836679794293,
-2.11756218312176,-2.11690727930576,-2.1162424314581,-2.1150004660964,-2.11084458825208,
-2.03147581385238,-2.01273883292165,-1.9625415108435,-1.95872612421727,
-1.95720367157684,-1.95609127818727,-1.95489576499217,-1.9532876183956,
-1.94968477857289,-1.90768421633015,-1.85807797372953,-1.79985106899913,
-1.79656818735679,-1.79543769614386,-1.79479531335656,-1.79420240462004,
-1.79338708311564,-1.79179092470171,-1.78083064960815,-1.75281713394966,
-1.72536071318246,-1.66468690849567,-1.65897623391533,-1.6388787947221,
-1.6357496092877,-1.63423159923777,-1.63304943200903,-1.6317465619234,-1.62962421723337,
-1.62229336690498,-1.57622403306197,-1.47864046183971,-1.4741926747754,
-1.47291753111798,-1.47217145073474,-1.47158017990598,-1.47078072271387,
-1.46926075412567,-1.46022810565488,-1.44108668051645,-1.39369339702938,
-1.31821706740442,-1.31374164539671,-1.31211188378765,-1.31097060156912,
-1.30981193278721,-1.30833724215702,-1.30672860705067,-1.30412115494985,
-1.29898569538024,-1.24767773288631,-1.16277868956499,-1.15222826906672,
-1.15051179179217,-1.14967182182469,-1.14901387570077,-1.14827305076915,
-1.14702161918303,-1.14222966479954,-1.10674082459561,-1.01315844462675,
-0.993326489122193,-0.99020904934278,-0.988693212961755,-0.987536006302111,
-0.986805087038092,-0.985207420311045,-0.983427834613196,-0.980408883842235,
-0.974142071959428,-0.957346917346883,-0.93616504367092,-0.832378145149048,
-0.828486794726983,-0.827276141811284,-0.826617435097182,-0.825961584237627,
-0.825145548902246,-0.823546930831487,-0.812530941472452,-0.784274767680891,
-0.772585675630654,-0.721053344311418,-0.671698824144621,-0.667892739487543,
-0.66637147899449,-0.665259063070078,-0.664086743499903,-0.662523488591205,
-0.660792023553347,-0.657889968463439,-0.651950269948339,-0.636332925815105,
-0.61644592932972,-0.566621020365257,-0.509141635531219,-0.50571884665159,
-0.504568372423816,-0.503921785534318,-0.5033295425707,-0.502521925532216,
-0.500963786439337,-0.491034709971074,-0.468147849628446,-0.442831005654773,
-0.434738535995411,-0.407453215973505,-0.349167784872187,-0.345280978576924,
-0.343745921623834,-0.34262988776584,-0.341459615721182,-0.339910127097627,
-0.338196986888664,-0.3353392168193,-0.329522257885625,-0.314340344843652,
-0.276961113514679,-0.202877031195031,-0.200028666006729,-0.199673487941102,
-0.196055536991565,-0.184123393789331,-0.182342738898069,-0.181489934620054,
-0.180830362306391,-0.180096602163226,-0.178877228846258,-0.174430310859571,
-0.143448522374149,-0.0400412049537006,-0.0331754686402422,-0.0310183526667614,
-0.0235248573812635,-0.0212903812577373,-0.0199621151414786,-0.0188042245762228,
-0.0176704612255242,-0.0162411519802988,-0.0140600772172354,-0.000956836703198815),
 .UNSPECIFIED.);
#843=B_SPLINE_CURVE_WITH_KNOTS('',3,(#51659,#51660,#51661,#51662,#51663,
#51664,#51665,#51666,#51667,#51668,#51669,#51670,#51671,#51672,#51673,#51674,
#51675,#51676,#51677,#51678,#51679,#51680,#51681,#51682,#51683,#51684,#51685,
#51686,#51687,#51688,#51689,#51690,#51691,#51692,#51693,#51694,#51695,#51696,
#51697,#51698,#51699,#51700,#51701,#51702,#51703,#51704,#51705,#51706,#51707,
#51708,#51709,#51710,#51711,#51712,#51713,#51714,#51715,#51716,#51717,#51718,
#51719,#51720,#51721,#51722,#51723,#51724,#51725,#51726,#51727,#51728,#51729,
#51730,#51731,#51732,#51733,#51734,#51735,#51736,#51737,#51738,#51739,#51740,
#51741,#51742,#51743,#51744,#51745,#51746,#51747,#51748,#51749,#51750,#51751,
#51752,#51753,#51754,#51755,#51756,#51757,#51758,#51759,#51760,#51761,#51762,
#51763,#51764,#51765,#51766,#51767,#51768,#51769,#51770,#51771,#51772,#51773,
#51774,#51775,#51776,#51777,#51778,#51779,#51780,#51781,#51782,#51783,#51784,
#51785,#51786,#51787,#51788,#51789,#51790,#51791,#51792,#51793,#51794,#51795,
#51796,#51797,#51798,#51799,#51800,#51801,#51802,#51803,#51804,#51805,#51806,
#51807,#51808,#51809,#51810,#51811,#51812,#51813,#51814,#51815,#51816,#51817,
#51818,#51819,#51820,#51821,#51822,#51823,#51824,#51825,#51826,#51827,#51828,
#51829,#51830,#51831,#51832,#51833,#51834,#51835,#51836,#51837,#51838,#51839,
#51840,#51841,#51842,#51843,#51844,#51845,#51846,#51847,#51848,#51849,#51850,
#51851,#51852,#51853,#51854,#51855,#51856,#51857,#51858,#51859,#51860,#51861,
#51862,#51863,#51864,#51865,#51866,#51867,#51868,#51869,#51870,#51871,#51872,
#51873,#51874,#51875,#51876,#51877,#51878,#51879,#51880,#51881,#51882,#51883,
#51884,#51885,#51886,#51887,#51888,#51889,#51890,#51891,#51892,#51893,#51894,
#51895,#51896,#51897,#51898,#51899,#51900,#51901,#51902,#51903,#51904,#51905,
#51906,#51907,#51908,#51909,#51910,#51911,#51912,#51913,#51914,#51915,#51916,
#51917,#51918,#51919,#51920,#51921,#51922,#51923,#51924,#51925,#51926,#51927,
#51928,#51929,#51930,#51931,#51932,#51933,#51934,#51935,#51936,#51937,#51938,
#51939,#51940,#51941,#51942,#51943,#51944,#51945,#51946,#51947,#51948,#51949,
#51950,#51951,#51952,#51953,#51954,#51955,#51956,#51957,#51958,#51959,#51960,
#51961,#51962,#51963,#51964,#51965,#51966,#51967,#51968,#51969,#51970,#51971,
#51972,#51973,#51974,#51975,#51976,#51977,#51978,#51979,#51980,#51981,#51982,
#51983,#51984,#51985,#51986,#51987,#51988,#51989,#51990,#51991,#51992,#51993,
#51994,#51995,#51996,#51997,#51998,#51999,#52000,#52001,#52002,#52003,#52004,
#52005,#52006,#52007,#52008,#52009,#52010,#52011,#52012,#52013,#52014,#52015,
#52016,#52017,#52018,#52019,#52020,#52021,#52022,#52023,#52024,#52025,#52026,
#52027,#52028,#52029,#52030,#52031,#52032,#52033,#52034,#52035,#52036,#52037,
#52038,#52039,#52040,#52041,#52042,#52043,#52044,#52045,#52046,#52047,#52048,
#52049,#52050,#52051,#52052,#52053,#52054,#52055,#52056,#52057,#52058,#52059,
#52060,#52061,#52062,#52063,#52064,#52065,#52066,#52067,#52068,#52069,#52070,
#52071,#52072,#52073,#52074,#52075,#52076,#52077,#52078,#52079,#52080,#52081,
#52082,#52083,#52084,#52085,#52086,#52087,#52088,#52089,#52090,#52091,#52092,
#52093,#52094,#52095,#52096,#52097,#52098,#52099,#52100,#52101,#52102,#52103,
#52104,#52105,#52106,#52107,#52108,#52109,#52110,#52111,#52112,#52113,#52114,
#52115,#52116,#52117,#52118,#52119,#52120,#52121,#52122,#52123,#52124,#52125,
#52126,#52127,#52128,#52129,#52130,#52131,#52132,#52133,#52134,#52135,#52136,
#52137,#52138,#52139,#52140,#52141,#52142,#52143,#52144,#52145,#52146,#52147,
#52148,#52149,#52150,#52151,#52152,#52153,#52154,#52155,#52156,#52157,#52158,
#52159,#52160,#52161,#52162,#52163,#52164,#52165,#52166,#52167,#52168,#52169,
#52170,#52171,#52172,#52173,#52174,#52175,#52176,#52177,#52178,#52179,#52180,
#52181,#52182,#52183,#52184,#52185,#52186,#52187,#52188,#52189,#52190,#52191,
#52192,#52193,#52194),.UNSPECIFIED.,.F.,.F.,(4,2,2,2,2,2,2,2,2,2,2,2,2,
2,2,2,2,2,2,2,2,2,2,2,2,2,2,2,2,2,2,2,2,2,2,2,2,2,2,2,2,2,2,2,2,2,2,2,2,
2,2,2,2,2,2,2,2,2,2,2,2,2,2,2,2,2,2,2,2,2,2,2,2,2,2,2,2,2,2,2,2,2,2,2,2,
2,2,2,2,2,2,2,2,2,2,2,2,2,2,2,2,2,2,2,2,2,2,2,2,2,2,2,2,2,2,2,2,2,2,2,2,
2,2,2,2,2,2,2,2,2,2,2,2,2,2,2,2,2,2,2,2,2,2,2,2,2,2,2,2,2,2,2,2,2,2,2,2,
2,2,2,2,2,2,2,2,2,2,2,2,2,2,2,2,2,2,2,2,2,2,2,2,2,2,2,2,2,2,2,2,2,2,2,2,
2,2,2,2,2,2,2,2,2,2,2,2,2,2,2,2,2,2,2,2,2,2,2,2,2,2,2,2,2,2,2,2,2,2,2,2,
2,2,2,2,2,2,2,2,2,2,2,2,2,2,2,2,2,2,2,2,2,2,2,2,2,2,2,2,2,2,2,2,2,2,2,2,
2,2,4),(-4.05932261802918,-3.94718619145327,-3.92809093087277,-3.91911955207525,
-3.91760275599314,-3.91680415072275,-3.91621315676654,-3.9154669527404,
-3.91419047575874,-3.90972786546289,-3.81963845278496,-3.78303009534929,
-3.76798484889305,-3.76220738073496,-3.75936439301799,-3.7576577503187,
-3.75611523835994,-3.75494619777213,-3.7538302195544,-3.75229342938824,
-3.74839269670435,-3.68633818526492,-3.64994132301906,-3.59749009169381,
-3.59536753150999,-3.5944514929179,-3.59378266126145,-3.59316194920748,
-3.59230760096305,-3.59059921323149,-3.57564990070719,-3.49350528039842,
-3.45961154536527,-3.44515804416145,-3.43954952387634,-3.43676800928572,
-3.43508692889591,-3.43357991698403,-3.43241235435313,-3.43129387235999,
-3.42974745254961,-3.42578929679905,-3.35923772249199,-3.31285592803571,
-3.27827970434388,-3.27355529763417,-3.27231044614131,-3.27157134749633,
-3.27091352211781,-3.27007181242301,-3.26840254246408,-3.25835945977218,
-3.21377491260917,-3.12304217155674,-3.11718705469083,-3.11431604883399,
-3.11259784567634,-3.11104443473474,-3.10987611414841,-3.1087625394867,
-3.10723465212028,-3.10338578050594,-3.04975306427779,-2.99055093928644,
-2.95575563221633,-2.9510153783639,-2.94976913604699,-2.94902975720943,
-2.94837203750011,-2.94753093977968,-2.94580727683437,-2.93509776667768,
-2.85042628699211,-2.7992048379846,-2.79407490710356,-2.79146986087013,
-2.78986251625508,-2.78838865962902,-2.78723069243043,-2.78608989200054,
-2.78446046249791,-2.7799837361825,-2.70426021262851,-2.65702289994102,
-2.63793011095452,-2.62895936355373,-2.62744280433519,-2.62664433870224,
-2.62605345455559,-2.62530739780633,-2.6240311932988,-2.61956972223699,
-2.5224212750323,-2.47609700951169,-2.46874269201359,-2.46661853933616,
-2.46531565640758,-2.46413419817715,-2.46261810327591,-2.45949643285783,
-2.43954054311265,-2.43307202513359,-2.35890687780683,-2.33463762251458,
-2.31558609092321,-2.30642638894341,-2.30490148448641,-2.30410128749428,
-2.30351027160373,-2.30286077194628,-2.30169401085176,-2.29814207532942,
-2.23794795641187,-2.18917912263447,-2.16590504525583,-2.14755958793992,
-2.14474951693844,-2.14329685993158,-2.14223395771725,-2.14109146478605,
-2.1391176462441,-2.13361096972731,-2.12789383645975,-2.02995606576609,
-1.98574053698561,-1.98300114252315,-1.98205706583568,-1.98141190307608,
-1.98081987958671,-1.98001094213419,-1.97844481528347,-1.9682906528721,
-1.94402702210448,-1.89479969303414,-1.85196781063417,-1.84544048437153,
-1.82552509248755,-1.82240479476043,-1.82088878504062,-1.81970712997985,
-1.81840376263382,-1.81627821815792,-1.80891327157105,-1.76247270539797,
-1.66536748421636,-1.66090129785883,-1.65962434422935,-1.65887798358763,
-1.65828693393508,-1.65748834314583,-1.65597186177543,-1.64701003779624,
-1.62792989175814,-1.5807598081821,-1.53641146788433,-1.52662423648838,
-1.5214276050629,-1.51961808611955,-1.50270251044742,-1.49976790446488,
-1.4982690088048,-1.49708916705714,-1.49577591863669,-1.49360704095215,
-1.48581784599507,-1.43464507918231,-1.34296925524164,-1.33833599228516,
-1.33705606755409,-1.33630151172824,-1.33564563219065,-1.33484332967692,
-1.33329099785979,-1.33131500157843,-1.28021233633798,-1.21142834937144,
-1.20597253903291,-1.20032869042724,-1.18026882970569,-1.17714113711538,
-1.17562333563879,-1.17444109791264,-1.17313791385746,-1.17101452653429,
-1.16367496702171,-1.11751629708463,-1.02559224838059,-1.01624816366084,
-1.01461550586423,-1.01378139561017,-1.01312407850158,-1.01239478592759,
-1.01116959810087,-1.00969358508122,-1.00675484102546,-0.975746885084139,
-0.92590922596784,-0.883985483800203,-0.877563261099115,-0.85758806507461,
-0.854463848941587,-0.852946581351915,-0.851764238012896,-0.850460408183944,
-0.848334777470833,-0.840975982669745,-0.794618226968018,-0.72145079869608,
-0.694435476053143,-0.692285122685145,-0.691432178962731,-0.690811609428396,
-0.690142047054751,-0.689241995945121,-0.68719685873267,-0.684414828456267,
-0.677452391139539,-0.662978159807999,-0.623447930895032,-0.552965890060782,
-0.551914756275635,-0.534692463460466,-0.531741409121149,-0.530238660709844,
-0.529058014210598,-0.527746171099943,-0.525584910186803,-0.517877491787067,
-0.492036811824751,-0.461993250933704,-0.455553082600992,-0.407179502722541,
-0.394575463562312,-0.37170295819498,-0.369631365047125,-0.368792032874973,
-0.368174994851585,-0.36755193213565,-0.366894525696385,-0.365336455877824,
-0.355275959863369,-0.33148116118891,-0.311723113356212,-0.249933768699635,
-0.245226592200497,-0.239242005766237,-0.231549569889586,-0.212276439618882,
-0.209184742222764,-0.20767391298561,-0.206492322725152,-0.205184970528625,
-0.203043738003696,-0.19553436804252,-0.147549550928869,-0.0923282060039677,
-0.087045437847226,-0.0654385759082482,-0.0611863058379246,-0.0486395021768235,
-0.0470125458883691,-0.0461787094473289,-0.0455630670267084,-0.0449408873179125,
-0.0442820125657699,-0.0434045401258508,-0.041993761853196,-0.000956483055879518),
 .UNSPECIFIED.);
#844=B_SPLINE_CURVE_WITH_KNOTS('',3,(#52196,#52197,#52198,#52199,#52200,
#52201,#52202,#52203,#52204,#52205,#52206,#52207,#52208,#52209,#52210,#52211,
#52212,#52213,#52214,#52215,#52216,#52217,#52218,#52219,#52220,#52221,#52222,
#52223,#52224,#52225,#52226,#52227,#52228,#52229,#52230,#52231,#52232,#52233,
#52234,#52235,#52236,#52237,#52238,#52239,#52240,#52241,#52242,#52243,#52244,
#52245,#52246,#52247,#52248,#52249,#52250,#52251,#52252,#52253,#52254,#52255,
#52256,#52257,#52258,#52259,#52260,#52261,#52262,#52263,#52264,#52265,#52266,
#52267,#52268,#52269,#52270,#52271,#52272,#52273,#52274,#52275,#52276,#52277,
#52278,#52279,#52280,#52281,#52282,#52283,#52284,#52285,#52286,#52287,#52288,
#52289,#52290,#52291,#52292,#52293,#52294,#52295,#52296,#52297,#52298,#52299,
#52300,#52301,#52302,#52303,#52304,#52305,#52306,#52307,#52308,#52309,#52310,
#52311,#52312,#52313,#52314,#52315,#52316,#52317,#52318,#52319,#52320,#52321,
#52322,#52323,#52324,#52325,#52326,#52327,#52328,#52329,#52330,#52331,#52332,
#52333,#52334,#52335,#52336,#52337,#52338,#52339,#52340,#52341,#52342,#52343,
#52344,#52345,#52346,#52347,#52348,#52349,#52350,#52351,#52352,#52353,#52354,
#52355,#52356,#52357,#52358,#52359,#52360,#52361,#52362,#52363,#52364,#52365,
#52366,#52367,#52368,#52369,#52370,#52371,#52372,#52373,#52374,#52375,#52376,
#52377,#52378,#52379,#52380,#52381,#52382,#52383,#52384,#52385,#52386,#52387,
#52388,#52389,#52390,#52391,#52392,#52393,#52394,#52395,#52396,#52397,#52398,
#52399,#52400,#52401,#52402,#52403,#52404,#52405,#52406,#52407,#52408,#52409,
#52410,#52411,#52412,#52413,#52414,#52415,#52416,#52417,#52418,#52419,#52420,
#52421,#52422,#52423,#52424,#52425,#52426,#52427,#52428,#52429,#52430,#52431,
#52432,#52433,#52434,#52435,#52436,#52437,#52438,#52439,#52440,#52441,#52442,
#52443,#52444,#52445,#52446,#52447,#52448,#52449,#52450,#52451,#52452,#52453,
#52454,#52455,#52456,#52457,#52458,#52459,#52460,#52461,#52462,#52463,#52464,
#52465,#52466,#52467,#52468,#52469,#52470,#52471,#52472,#52473,#52474,#52475,
#52476,#52477,#52478,#52479,#52480,#52481,#52482,#52483,#52484,#52485,#52486,
#52487,#52488,#52489,#52490,#52491,#52492,#52493,#52494,#52495,#52496,#52497,
#52498,#52499,#52500,#52501,#52502,#52503,#52504,#52505,#52506,#52507,#52508,
#52509,#52510,#52511,#52512,#52513,#52514,#52515,#52516,#52517,#52518,#52519,
#52520,#52521,#52522,#52523,#52524,#52525,#52526,#52527,#52528,#52529,#52530,
#52531,#52532,#52533,#52534,#52535,#52536,#52537,#52538,#52539,#52540,#52541,
#52542,#52543,#52544,#52545,#52546,#52547,#52548,#52549,#52550,#52551,#52552,
#52553,#52554,#52555,#52556,#52557,#52558,#52559,#52560,#52561,#52562,#52563,
#52564,#52565,#52566,#52567,#52568,#52569,#52570,#52571,#52572,#52573,#52574,
#52575,#52576,#52577,#52578,#52579,#52580,#52581,#52582,#52583,#52584,#52585,
#52586,#52587,#52588,#52589,#52590,#52591,#52592,#52593,#52594,#52595,#52596,
#52597,#52598,#52599,#52600,#52601,#52602,#52603,#52604,#52605,#52606,#52607,
#52608,#52609,#52610,#52611,#52612,#52613,#52614,#52615,#52616,#52617,#52618,
#52619,#52620,#52621,#52622,#52623,#52624,#52625,#52626,#52627,#52628,#52629,
#52630,#52631,#52632,#52633,#52634,#52635,#52636,#52637,#52638,#52639,#52640,
#52641,#52642,#52643,#52644,#52645,#52646,#52647,#52648,#52649,#52650,#52651,
#52652,#52653,#52654,#52655,#52656,#52657,#52658,#52659,#52660,#52661,#52662,
#52663,#52664,#52665,#52666,#52667,#52668,#52669,#52670,#52671,#52672,#52673,
#52674,#52675,#52676,#52677,#52678,#52679,#52680,#52681,#52682,#52683,#52684,
#52685,#52686,#52687,#52688,#52689,#52690,#52691,#52692,#52693,#52694,#52695,
#52696,#52697,#52698,#52699,#52700,#52701,#52702,#52703,#52704,#52705,#52706,
#52707,#52708,#52709,#52710,#52711,#52712,#52713,#52714,#52715,#52716,#52717,
#52718,#52719,#52720,#52721,#52722,#52723,#52724,#52725,#52726,#52727,#52728,
#52729,#52730,#52731,#52732,#52733),.UNSPECIFIED.,.F.,.F.,(4,2,2,2,2,2,
2,2,2,2,2,2,2,2,2,2,2,2,2,2,2,2,2,2,2,2,2,2,2,2,2,2,2,2,2,2,2,2,2,2,2,2,
2,2,2,2,2,2,2,2,2,2,2,2,2,2,2,2,2,2,2,2,2,2,2,2,2,2,2,2,2,2,2,2,2,2,2,2,
2,2,2,2,2,2,2,2,2,2,2,2,2,2,2,2,2,2,2,2,2,2,2,2,2,2,2,2,2,2,2,2,2,2,2,2,
2,2,2,2,2,2,2,2,2,2,2,2,2,2,2,2,2,2,2,2,2,2,2,2,2,2,2,2,2,2,2,2,2,2,2,2,
2,2,2,2,2,2,2,2,2,2,2,2,2,2,2,2,2,2,2,2,2,2,2,2,2,2,2,2,2,2,2,2,2,2,2,2,
2,2,2,2,2,2,2,2,2,2,2,2,2,2,2,2,2,2,2,2,2,2,2,2,2,2,2,2,2,2,2,2,2,2,2,2,
2,2,2,2,2,2,2,2,2,2,2,2,2,2,2,2,2,2,2,2,2,2,2,2,2,2,2,2,2,2,2,2,2,2,2,2,
2,2,2,2,2,2,2,2,2,2,4),(-4.06075874161792,-3.98610762050859,-3.95340645274498,
-3.9474606547773,-3.94549738830649,-3.94423002723069,-3.94303631844564,
-3.94146620849038,-3.93880894078993,-3.92222994581067,-3.83224930180272,
-3.81338738761118,-3.78833954713899,-3.78466199201783,-3.78381231749805,
-3.78316346566348,-3.78253436033305,-3.78190809079028,-3.78103306267748,
-3.77924217307012,-3.76138047146936,-3.75549508160315,-3.74467557349034,
-3.70875708554463,-3.67353861318805,-3.63201582196343,-3.62512873620835,
-3.62305415550328,-3.62176196458069,-3.62057698380681,-3.61906313144738,
-3.61587173865262,-3.59435953321201,-3.52074269448731,-3.48166490862495,
-3.4690884380765,-3.46480754080062,-3.46193259088222,-3.46089707261786,
-3.4602835696196,-3.45962028693457,-3.45875385961736,-3.45685215405933,
-3.44178686432493,-3.44091362949828,-3.43996393494279,-3.43890085556761,
-3.42821658954846,-3.35551603382603,-3.32019785963148,-3.30374186790685,
-3.3010073976106,-3.29957024076967,-3.29850876661142,-3.29735820759772,
-3.29569454193968,-3.29099323181756,-3.21690141014196,-3.16951644080574,
-3.14359960058933,-3.14094714620724,-3.13957738556252,-3.13845756751828,
-3.13773712125085,-3.13707829057859,-3.13622941643561,-3.13446752527795,
-3.12294646837749,-3.03729236060468,-2.98233991551047,-2.97879692406513,
-2.97719975237968,-2.97600604238203,-2.97489073408241,-2.97335711798215,
-2.96947628774928,-2.91192121149933,-2.84918011621408,-2.82117667906771,
-2.81840334273092,-2.81698847611232,-2.81580484066623,-2.81508511272102,
-2.81442613587945,-2.81357587565009,-2.81180685465431,-2.80012509457277,
-2.73444980666313,-2.69097716257303,-2.66517191390396,-2.65747822020727,
-2.65531875128943,-2.65400755940859,-2.65282721722685,-2.65132446981306,
-2.64837219647718,-2.63111495355163,-2.62983958543947,-2.62591535226356,
-2.61343356176322,-2.61126508376648,-2.52897106090484,-2.49592048130302,
-2.49378806707527,-2.49287011322963,-2.49220077585795,-2.49158025672335,
-2.49072715012814,-2.489024239535,-2.47425858190168,-2.41081878901101,-2.33699496964111,
-2.33353041523372,-2.33194775507372,-2.33075631312879,-2.3296368566074,
-2.32808763474004,-2.32496439836249,-2.29565519526841,-2.20856706358912,
-2.17631048193914,-2.17176204625211,-2.1705332319086,-2.16979752728574,
-2.16913868314289,-2.16829019380492,-2.16653052333102,-2.1550616792619,
-2.15328717158991,-2.15271201634402,-2.07317271502636,-2.03108706288559,
-2.01359300382855,-2.01062807591605,-2.00912252161027,-2.00794174782285,
-2.00663190107838,-2.00447882682588,-1.99685028422291,-1.97116486856814,
-1.92790563909832,-1.85338733248369,-1.84915060408523,-1.84789916009374,
-1.84723232384135,-1.8465837049106,-1.84578482358669,-1.84426754609871,
-1.83529438921099,-1.81619944533137,-1.76898332023829,-1.69334280549139,
-1.68877911326154,-1.68713594169643,-1.68599097175559,-1.68492793907007,
-1.68347843485539,-1.68068585328748,-1.66282740169784,-1.62061964251767,
-1.53096068330205,-1.5264817316112,-1.52520309023005,-1.52445618328523,
-1.5238649512425,-1.52306643402025,-1.52155112836383,-1.51262423005136,
-1.49358583541313,-1.4465660167532,-1.37054170574068,-1.36602322587058,
-1.36438680213263,-1.36324361691271,-1.362179944736,-1.36075522499681,-1.35804794864587,
-1.35464493259904,-1.32941742698359,-1.30570090387805,-1.23661501946852,
-1.2053610088884,-1.20314559311054,-1.20228152571019,-1.201658043469,-1.20099049161116,
-1.20008343177585,-1.19801298489131,-1.17337970931843,-1.14954723994569,
-1.07324781701648,-1.04615544681051,-1.04275415699607,-1.0412001626498,
-1.04000877141227,-1.03873421980967,-1.0367797619644,-1.03087615570099,
-0.998308332499085,-0.938115476308948,-0.896417365984515,-0.895463838611336,
-0.893920111382816,-0.881997981016917,-0.880218070907458,-0.879374659349585,
-0.878714615556626,-0.877983711867653,-0.876776582342343,-0.872558965221797,
-0.852506048067094,-0.830635033430468,-0.770835500925901,-0.756434778586312,
-0.747830464485669,-0.7424976129598,-0.72309082939253,-0.719992877017493,
-0.718480814695982,-0.717299091384188,-0.715992441203287,-0.713897001627106,
-0.70677851346872,-0.695341957177579,-0.655430644261318,-0.621223779417774,
-0.595643798136869,-0.582563855194721,-0.559930677976956,-0.557864447900867,
-0.557026071541431,-0.556409293441287,-0.555736846206907,-0.554802180215169,
-0.552573871011485,-0.535911022564283,-0.512196359182349,-0.460384618762866,
-0.401806256750432,-0.397918534883089,-0.396383504313612,-0.395267625491593,
-0.394073735252269,-0.392902131807994,-0.391358267573132,-0.384442103852216,
-0.373423985716377,-0.340830663919388,-0.315466307354785,-0.240212044051322,
-0.23591280778266,-0.234654140707828,-0.233985793734345,-0.23333718013636,
-0.232540403798336,-0.231033354238017,-0.22245407097745,-0.177126902451215,
-0.160485085827147,-0.14284817708322,-0.079177482182616,-0.0752709206875294,
-0.0737326398628456,-0.072615859952655,-0.071422375926071,-0.0702516132194086,
-0.0687102326821668,-0.0662631654880025,-0.00095691374464929),
 .UNSPECIFIED.);
#845=B_SPLINE_CURVE_WITH_KNOTS('',3,(#52735,#52736,#52737,#52738,#52739,
#52740,#52741,#52742,#52743,#52744,#52745,#52746,#52747,#52748,#52749,#52750,
#52751,#52752,#52753,#52754,#52755,#52756,#52757,#52758,#52759,#52760,#52761,
#52762,#52763,#52764,#52765,#52766,#52767,#52768,#52769,#52770,#52771,#52772,
#52773,#52774,#52775,#52776,#52777,#52778,#52779,#52780,#52781,#52782,#52783,
#52784,#52785,#52786,#52787,#52788,#52789,#52790,#52791,#52792,#52793,#52794,
#52795,#52796,#52797,#52798,#52799,#52800,#52801,#52802,#52803,#52804,#52805,
#52806,#52807,#52808,#52809,#52810,#52811,#52812,#52813,#52814,#52815,#52816,
#52817,#52818,#52819,#52820,#52821,#52822,#52823,#52824,#52825,#52826,#52827,
#52828,#52829,#52830,#52831,#52832,#52833,#52834,#52835,#52836,#52837,#52838,
#52839,#52840,#52841,#52842,#52843,#52844,#52845,#52846,#52847,#52848,#52849,
#52850,#52851,#52852,#52853,#52854,#52855,#52856,#52857,#52858,#52859,#52860,
#52861,#52862,#52863,#52864,#52865,#52866,#52867,#52868,#52869,#52870,#52871,
#52872,#52873,#52874,#52875,#52876,#52877,#52878,#52879,#52880,#52881,#52882,
#52883,#52884,#52885,#52886,#52887,#52888,#52889,#52890,#52891,#52892,#52893,
#52894,#52895,#52896,#52897,#52898,#52899,#52900,#52901,#52902,#52903,#52904,
#52905,#52906,#52907,#52908,#52909,#52910,#52911,#52912,#52913,#52914,#52915,
#52916,#52917,#52918,#52919,#52920,#52921,#52922,#52923,#52924,#52925,#52926,
#52927,#52928,#52929,#52930,#52931,#52932,#52933,#52934,#52935,#52936,#52937,
#52938,#52939,#52940,#52941,#52942,#52943,#52944,#52945,#52946,#52947,#52948,
#52949,#52950,#52951,#52952,#52953,#52954,#52955,#52956,#52957,#52958,#52959,
#52960,#52961,#52962,#52963,#52964,#52965,#52966,#52967,#52968,#52969,#52970,
#52971,#52972,#52973,#52974,#52975,#52976,#52977,#52978,#52979,#52980,#52981,
#52982,#52983,#52984,#52985,#52986,#52987,#52988,#52989,#52990,#52991,#52992,
#52993,#52994,#52995,#52996,#52997,#52998,#52999,#53000,#53001,#53002,#53003,
#53004,#53005,#53006,#53007,#53008,#53009,#53010,#53011,#53012,#53013,#53014,
#53015,#53016,#53017,#53018,#53019,#53020,#53021,#53022,#53023,#53024,#53025,
#53026,#53027,#53028,#53029,#53030,#53031,#53032,#53033,#53034,#53035,#53036,
#53037,#53038,#53039,#53040,#53041,#53042,#53043,#53044,#53045,#53046,#53047,
#53048,#53049,#53050,#53051,#53052,#53053,#53054,#53055,#53056,#53057,#53058,
#53059,#53060,#53061,#53062,#53063,#53064,#53065,#53066,#53067,#53068,#53069,
#53070,#53071,#53072,#53073,#53074,#53075,#53076,#53077,#53078,#53079,#53080,
#53081,#53082,#53083,#53084,#53085,#53086,#53087,#53088,#53089,#53090,#53091,
#53092,#53093,#53094,#53095,#53096,#53097,#53098,#53099,#53100,#53101,#53102,
#53103,#53104,#53105,#53106,#53107,#53108,#53109,#53110,#53111,#53112,#53113,
#53114,#53115,#53116,#53117,#53118,#53119,#53120,#53121,#53122,#53123,#53124,
#53125,#53126,#53127,#53128,#53129,#53130,#53131,#53132,#53133,#53134,#53135,
#53136,#53137,#53138,#53139,#53140,#53141,#53142,#53143,#53144,#53145,#53146,
#53147,#53148,#53149,#53150,#53151,#53152,#53153,#53154,#53155,#53156,#53157,
#53158,#53159,#53160,#53161,#53162,#53163,#53164,#53165,#53166,#53167,#53168,
#53169,#53170,#53171,#53172,#53173,#53174,#53175,#53176,#53177,#53178,#53179,
#53180,#53181,#53182,#53183,#53184,#53185,#53186,#53187,#53188,#53189,#53190,
#53191,#53192,#53193,#53194,#53195,#53196,#53197,#53198,#53199,#53200,#53201,
#53202,#53203,#53204,#53205,#53206,#53207,#53208,#53209,#53210,#53211,#53212,
#53213,#53214,#53215,#53216,#53217,#53218,#53219,#53220,#53221,#53222,#53223,
#53224,#53225,#53226,#53227,#53228,#53229,#53230,#53231,#53232,#53233,#53234,
#53235,#53236,#53237,#53238,#53239,#53240,#53241,#53242,#53243,#53244,#53245,
#53246,#53247,#53248,#53249,#53250,#53251,#53252,#53253,#53254),
 .UNSPECIFIED.,.F.,.F.,(4,2,2,2,2,2,2,2,2,2,2,2,2,2,2,2,2,2,2,2,2,2,2,2,
2,2,2,2,2,2,2,2,2,2,2,2,2,2,2,2,2,2,2,2,2,2,2,2,2,2,2,2,2,2,2,2,2,2,2,2,
2,2,2,2,2,2,2,2,2,2,2,2,2,2,2,2,2,2,2,2,2,2,2,2,2,2,2,2,2,2,2,2,2,2,2,2,
2,2,2,2,2,2,2,2,2,2,2,2,2,2,2,2,2,2,2,2,2,2,2,2,2,2,2,2,2,2,2,2,2,2,2,2,
2,2,2,2,2,2,2,2,2,2,2,2,2,2,2,2,2,2,2,2,2,2,2,2,2,2,2,2,2,2,2,2,2,2,2,2,
2,2,2,2,2,2,2,2,2,2,2,2,2,2,2,2,2,2,2,2,2,2,2,2,2,2,2,2,2,2,2,2,2,2,2,2,
2,2,2,2,2,2,2,2,2,2,2,2,2,2,2,2,2,2,2,2,2,2,2,2,2,2,2,2,2,2,2,2,2,2,2,2,
2,2,2,2,2,2,2,2,2,2,2,2,2,2,2,2,2,2,2,4),(-4.06019698931433,-3.97695450267513,
-3.97393430511519,-3.97242861270744,-3.9711715913942,-3.97042959900369,
-3.96977199694071,-3.96893431166321,-3.96722879794313,-3.95689198784149,
-3.88192677400402,-3.8582425023994,-3.81955722427489,-3.81263606631032,
-3.81109250666641,-3.80992112016608,-3.80872743624955,-3.80761174065082,
-3.80607694701041,-3.80218974761543,-3.74361678277193,-3.70939383921679,
-3.6721353974461,-3.65743604732047,-3.65017091372532,-3.64873262127818,
-3.64795070345073,-3.64736092079791,-3.64670004868253,-3.64547797456863,
-3.64149068181466,-3.56757946105376,-3.52167896423041,-3.49287889367005,
-3.4890962464564,-3.48781037005358,-3.48654510797325,-3.48535013417216,
-3.48377362205424,-3.48024934141457,-3.44906595356631,-3.42878102578146,
-3.37143223682587,-3.34994720088628,-3.33727572783858,-3.32778759648618,
-3.32624039650016,-3.32543526253,-3.32484348615073,-3.32419604933717,-3.32304054723902,
-3.31957519008414,-3.26226178790138,-3.21498640899134,-3.18878903266453,
-3.16956631082883,-3.16638241131776,-3.16481605482077,-3.16362204206302,
-3.16250695753445,-3.16097444188294,-3.15791764472456,-3.13096404153667,
-3.11730469568757,-3.03933576752033,-3.00900464465246,-3.00610242521389,
-3.00397155059318,-3.00305384839157,-3.00238453751884,-3.00176392648197,
-3.00091052193429,-2.99920649048525,-2.98440730571568,-2.95737942641187,
-2.89625865408434,-2.85209637626979,-2.8449741804413,-2.84287802279331,
-2.84157134124282,-2.84038986344522,-2.83887849458754,-2.83578329528635,
-2.81642725008816,-2.81119577506522,-2.71219985435423,-2.68587963827327,
-2.68320313489041,-2.68120540100166,-2.68031152975641,-2.67964616826552,
-2.67901900803923,-2.67814113759271,-2.67633930714462,-2.65806568901537,
-2.57662859146933,-2.52963081727253,-2.52221147984607,-2.52007960156352,
-2.5187743978272,-2.51759241898612,-2.51607785869288,-2.51296713722453,
-2.4932835840774,-2.4878094536777,-2.47969271490891,-2.39666445416615,-2.37756620746901,
-2.36011538934497,-2.35835452905756,-2.35750572288416,-2.35690793373471,
-2.35627872838251,-2.3553932986818,-2.3535607259485,-2.33402700947926,-2.3178193934521,
-2.29581995466206,-2.25485338266581,-2.22564735180887,-2.20354607498151,
-2.19886026173639,-2.19707097617181,-2.19584059635912,-2.19463689124796,
-2.19318818370314,-2.18957912386824,-2.1552335095384,-2.15085432803292,
-2.07559028822923,-2.04131006289086,-2.03820615353857,-2.03595828626849,
-2.03502020391007,-2.03434704482447,-2.03373088098402,-2.03289515592525,
-2.03084445992978,-1.98907413668802,-1.88255440830362,-1.87653891062244,
-1.87449166139925,-1.87333399718429,-1.8722737224416,-1.87084975525582,
-1.86817825385619,-1.85310479057138,-1.82366100193944,-1.77352520511806,
-1.71697181757311,-1.71477968917716,-1.71294521429595,-1.71209134300707,
-1.71142985225814,-1.71070443984429,-1.70952175546062,-1.70543655679243,
-1.67863485773535,-1.62917572259533,-1.55777039446591,-1.55336706805946,
-1.55174834902818,-1.55061005438552,-1.54954498699203,-1.54807995007571,
-1.54521311589833,-1.5253228467184,-1.49913234576748,-1.41878552333166,
-1.39260282759426,-1.39046723933438,-1.38961683016286,-1.38899692907907,
-1.38832690018277,-1.38740566224938,-1.38525518770638,-1.35008188092155,
-1.23745863427864,-1.23110328786188,-1.22900983257798,-1.22784298537131,
-1.22667798402257,-1.22525261919757,-1.222551130484,-1.21915051180542,-1.19395106498149,
-1.15818353674507,-1.07268972362682,-1.06826463307934,-1.06699197582423,
-1.06624644089026,-1.06565508306576,-1.06485484217533,-1.06333121611249,
-1.05421702760808,-1.03508612247613,-0.948062505052561,-0.93404923849643,
-0.91041607797363,-0.907179835080305,-0.905634175246147,-0.904444247483404,
-0.903344263855925,-0.901529639300561,-0.896644063786488,-0.889572242278826,
-0.860448827482918,-0.811095125566238,-0.759527163979478,-0.746544608070626,
-0.744902095371414,-0.744064329640685,-0.743447750564691,-0.74277526222774,
-0.741840086822431,-0.739608446855437,-0.736532659260694,-0.702831044992888,
-0.633651012381926,-0.588633424816174,-0.584889148175464,-0.583378786367023,
-0.582269387496917,-0.581071516246165,-0.579892454359496,-0.577063472711181,
-0.558261868175069,-0.536261813073066,-0.502268776363443,-0.427250267455445,
-0.42296735270491,-0.421710635059904,-0.42104273377329,-0.4203941809635,
-0.41959695041246,-0.418087473885397,-0.409285138478339,-0.39046306605224,
-0.353885815073532,-0.317450310587326,-0.266166494941265,-0.262338855956694,
-0.260814088923615,-0.259700914135983,-0.258505422367755,-0.257330791189235,
-0.255778397529117,-0.248726494873167,-0.214666778752984,-0.192598282054413,
-0.104966044982071,-0.1003768607073,-0.0991013916488177,-0.098347772748269,
-0.0976916228600743,-0.0968710769117434,-0.0952504564359993,-0.083576346611283,
-0.0569497684135954,-0.000958016727391121),.UNSPECIFIED.);
#846=B_SPLINE_CURVE_WITH_KNOTS('',3,(#53256,#53257,#53258,#53259,#53260,
#53261,#53262,#53263,#53264,#53265,#53266,#53267,#53268,#53269,#53270,#53271,
#53272,#53273,#53274,#53275,#53276,#53277,#53278,#53279,#53280,#53281,#53282,
#53283,#53284,#53285,#53286,#53287,#53288,#53289,#53290,#53291,#53292,#53293,
#53294,#53295,#53296,#53297,#53298,#53299,#53300,#53301,#53302,#53303,#53304,
#53305,#53306,#53307,#53308,#53309,#53310,#53311,#53312,#53313,#53314,#53315,
#53316,#53317,#53318,#53319,#53320,#53321,#53322,#53323,#53324,#53325,#53326,
#53327,#53328,#53329,#53330,#53331,#53332,#53333,#53334,#53335,#53336,#53337,
#53338,#53339,#53340,#53341,#53342,#53343,#53344,#53345,#53346,#53347,#53348,
#53349,#53350,#53351,#53352,#53353,#53354,#53355,#53356,#53357,#53358,#53359,
#53360,#53361,#53362,#53363,#53364,#53365,#53366,#53367,#53368,#53369,#53370,
#53371,#53372,#53373,#53374,#53375,#53376,#53377,#53378,#53379,#53380,#53381,
#53382,#53383,#53384,#53385,#53386,#53387,#53388,#53389,#53390,#53391,#53392,
#53393,#53394,#53395,#53396,#53397,#53398,#53399,#53400,#53401,#53402,#53403,
#53404,#53405,#53406,#53407,#53408,#53409,#53410,#53411,#53412,#53413,#53414,
#53415,#53416,#53417,#53418,#53419,#53420,#53421,#53422,#53423,#53424,#53425,
#53426,#53427,#53428,#53429,#53430,#53431,#53432,#53433,#53434,#53435,#53436,
#53437,#53438,#53439,#53440,#53441,#53442,#53443,#53444,#53445,#53446,#53447,
#53448,#53449,#53450,#53451,#53452,#53453,#53454,#53455,#53456,#53457,#53458,
#53459,#53460,#53461,#53462,#53463,#53464,#53465,#53466,#53467,#53468,#53469,
#53470,#53471,#53472,#53473,#53474,#53475,#53476,#53477,#53478,#53479,#53480,
#53481,#53482,#53483,#53484,#53485,#53486,#53487,#53488,#53489,#53490,#53491,
#53492,#53493,#53494,#53495,#53496,#53497,#53498,#53499,#53500,#53501,#53502,
#53503,#53504,#53505,#53506,#53507,#53508,#53509,#53510,#53511,#53512,#53513,
#53514,#53515,#53516,#53517,#53518,#53519,#53520,#53521,#53522,#53523,#53524,
#53525,#53526,#53527,#53528,#53529,#53530,#53531,#53532,#53533,#53534,#53535,
#53536,#53537,#53538,#53539,#53540,#53541,#53542,#53543,#53544,#53545,#53546,
#53547,#53548,#53549,#53550,#53551,#53552,#53553,#53554,#53555,#53556,#53557,
#53558,#53559,#53560,#53561,#53562,#53563,#53564,#53565,#53566,#53567,#53568,
#53569,#53570,#53571,#53572,#53573,#53574,#53575,#53576,#53577,#53578,#53579,
#53580,#53581,#53582,#53583,#53584,#53585,#53586,#53587,#53588,#53589,#53590,
#53591,#53592,#53593,#53594,#53595,#53596,#53597,#53598,#53599,#53600,#53601,
#53602,#53603,#53604,#53605,#53606,#53607,#53608,#53609,#53610,#53611,#53612,
#53613,#53614,#53615,#53616,#53617,#53618,#53619,#53620,#53621,#53622,#53623,
#53624,#53625,#53626,#53627,#53628,#53629,#53630,#53631,#53632,#53633,#53634,
#53635,#53636,#53637,#53638,#53639,#53640,#53641,#53642,#53643,#53644,#53645,
#53646,#53647,#53648,#53649,#53650,#53651,#53652,#53653,#53654,#53655,#53656,
#53657,#53658,#53659,#53660,#53661,#53662,#53663,#53664,#53665,#53666,#53667,
#53668,#53669,#53670,#53671,#53672,#53673,#53674,#53675,#53676,#53677,#53678,
#53679,#53680,#53681,#53682,#53683,#53684,#53685,#53686,#53687,#53688,#53689,
#53690,#53691,#53692,#53693,#53694,#53695,#53696,#53697,#53698,#53699,#53700,
#53701,#53702,#53703,#53704,#53705,#53706,#53707,#53708,#53709,#53710,#53711,
#53712,#53713,#53714,#53715,#53716,#53717,#53718,#53719,#53720,#53721,#53722,
#53723,#53724,#53725,#53726,#53727,#53728,#53729,#53730,#53731,#53732,#53733,
#53734,#53735,#53736,#53737,#53738,#53739,#53740,#53741,#53742,#53743,#53744,
#53745,#53746,#53747,#53748,#53749,#53750,#53751,#53752,#53753,#53754,#53755,
#53756,#53757,#53758,#53759,#53760,#53761,#53762,#53763,#53764,#53765,#53766,
#53767,#53768,#53769,#53770,#53771,#53772,#53773,#53774,#53775,#53776,#53777,
#53778,#53779,#53780,#53781,#53782,#53783,#53784,#53785,#53786,#53787,#53788,
#53789,#53790,#53791,#53792,#53793,#53794,#53795,#53796,#53797,#53798,#53799,
#53800,#53801),.UNSPECIFIED.,.F.,.F.,(4,2,2,2,2,2,2,2,2,2,2,2,2,2,2,2,2,
2,2,2,2,2,2,2,2,2,2,2,2,2,2,2,2,2,2,2,2,2,2,2,2,2,2,2,2,2,2,2,2,2,2,2,2,
2,2,2,2,2,2,2,2,2,2,2,2,2,2,2,2,2,2,2,2,2,2,2,2,2,2,2,2,2,2,2,2,2,2,2,2,
2,2,2,2,2,2,2,2,2,2,2,2,2,2,2,2,2,2,2,2,2,2,2,2,2,2,2,2,2,2,2,2,2,2,2,2,
2,2,2,2,2,2,2,2,2,2,2,2,2,2,2,2,2,2,2,2,2,2,2,2,2,2,2,2,2,2,2,2,2,2,2,2,
2,2,2,2,2,2,2,2,2,2,2,2,2,2,2,2,2,2,2,2,2,2,2,2,2,2,2,2,2,2,2,2,2,2,2,2,
2,2,2,2,2,2,2,2,2,2,2,2,2,2,2,2,2,2,2,2,2,2,2,2,2,2,2,2,2,2,2,2,2,2,2,2,
2,2,2,2,2,2,2,2,2,2,2,2,2,2,2,2,2,2,2,2,2,2,2,2,2,2,2,2,2,2,2,2,2,2,2,2,
2,2,2,4),(-4.06084665564884,-4.0028780513959,-4.00042071920944,-3.99887522503487,
-3.99770325483983,-3.99650935743439,-3.99539454443845,-3.9938626581458,
-3.9899917009456,-3.93383984104344,-3.92080358884868,-3.86095583541986,
-3.84672535486906,-3.83806592724142,-3.83656340569911,-3.8357677761187,
-3.83511944618217,-3.83445081224778,-3.83318991971986,-3.82886834335183,
-3.75244909765839,-3.73480647265931,-3.69615736252467,-3.68491185283819,
-3.67788574330586,-3.67633496108725,-3.67516109281549,-3.67396617197069,
-3.67285297998951,-3.67132733571929,-3.66749306124244,-3.61544394587349,
-3.55821293806315,-3.53299229457196,-3.51592868449372,-3.51417556525937,
-3.51332848492551,-3.51273114960538,-3.51210170422558,-3.51121482264067,
-3.50885821992887,-3.4668078565601,-3.4348277067004,-3.38667431338305,-3.3668200882538,
-3.35601685573383,-3.3536027972697,-3.35246376412079,-3.35139595919912,
-3.35026662431209,-3.34868015515922,-3.34540643784939,-3.30985514934358,
-3.3005700992973,-3.22078252563658,-3.19747970433049,-3.1925607992896,-3.19129827756834,
-3.19055509058197,-3.18989774741418,-3.1890621439357,-3.18736680531489,
-3.17723289501793,-3.13258202339751,-3.08058586982539,-3.05976544506857,
-3.03697217692271,-3.03222675220852,-3.03043288450582,-3.02933296809575,
-3.02814049547682,-3.02657868688788,-3.02313428511907,-2.99466652576593,
-2.90315753797758,-2.87410758700642,-2.86982431227166,-2.86862134871743,
-2.86789142347827,-2.86723121591107,-2.86638620624857,-2.86459777823003,
-2.85247569190688,-2.85110979204019,-2.85069200685696,-2.84727414143885,
-2.84513313123652,-2.82636316240316,-2.75772201168065,-2.74193073828499,
-2.71497856794903,-2.71144435067359,-2.70865144481789,-2.70720887650912,
-2.70614290176253,-2.70500761431294,-2.70339977183464,-2.69906498474173,
-2.62587885863892,-2.57988900227957,-2.55141999415833,-2.54862014358062,
-2.54654932848517,-2.54564226039769,-2.54497476262775,-2.54435137631128,
-2.54348751061889,-2.54127297515948,-2.51006985440719,-2.48140761328028,
-2.43191093936057,-2.4030064846174,-2.38854961000189,-2.38590876258827,
-2.38449136636726,-2.38343174243704,-2.38210147444006,-2.37985750279757,
-2.37227965071849,-2.37029098327736,-2.366881473546,-2.32714905988595,-2.30534309580936,
-2.26611898821354,-2.23665299189941,-2.22537576825694,-2.2237684425753,
-2.22295071217099,-2.22229486916986,-2.22153942941618,-2.22025586967219,
-2.21558839374699,-2.12016188911211,-2.07244009508194,-2.0649544932126,
-2.06281599083778,-2.06150942745812,-2.06032797736067,-2.05881653432756,
-2.05572079826507,-2.03635162370017,-2.0310813328872,-2.01167690602365,
-1.96143553271675,-1.90495052660509,-1.90179129250714,-1.90067794731483,
-1.90003894762906,-1.89944499391653,-1.89862188505124,-1.8969882385081,
-1.88489180411392,-1.85859926124186,-1.78707349931804,-1.76841295810416,
-1.76337342519935,-1.74403937463855,-1.74094527104516,-1.73943415259866,
-1.73825274066622,-1.73694599922674,-1.73480670563862,-1.72731340948495,
-1.67949748196618,-1.58408696572139,-1.57944272540835,-1.57816152304118,
-1.5774065950316,-1.57675063563528,-1.57593204068365,-1.57432072956475,
-1.56292775818497,-1.53291770894004,-1.43780970500761,-1.42100691940546,
-1.41807815228675,-1.4165803315435,-1.4154003966438,-1.41408607054968,-1.41191316092933,
-1.40408607610754,-1.35247441950122,-1.2612955578568,-1.25662517075267,
-1.25534120392499,-1.25458560926862,-1.25393384482551,-1.25313455047342,
-1.25159443281484,-1.24963915897217,-1.18542342771808,-1.11665876280134,
-1.11559268784128,-1.0982783824633,-1.09532251338532,-1.09381875088855,
-1.09263801050707,-1.091326787687,-1.08916821210506,-1.08148732602759,-1.05569784653198,
-1.01223719941998,-0.979440507164036,-0.936097869553703,-0.93344378434712,
-0.932511877509622,-0.931869903682166,-0.931229692366292,-0.930405931843433,
-0.928752711667427,-0.92661632712634,-0.921753887304315,-0.90676794220684,
-0.856828288791959,-0.778147023738427,-0.773508743208243,-0.771854269118318,
-0.770706112388515,-0.769643778880089,-0.768200795315442,-0.765439601081213,
-0.748364507563801,-0.709808756004757,-0.632430689401104,-0.63046209877142,
-0.62870390076376,-0.625757180280605,-0.624980366404814,-0.612126637459858,
-0.610488505042411,-0.609651795192603,-0.609035420377114,-0.608412776176412,
-0.607527406671135,-0.605572695734177,-0.60293703929106,-0.596468565054953,
-0.575070671996718,-0.544435509044801,-0.475035657539108,-0.473386672774535,
-0.467711975043182,-0.452741656879062,-0.450168920148042,-0.448623338714239,
-0.447433273340431,-0.446155111514457,-0.44414463127366,-0.437818197101808,
-0.401657571647373,-0.359767395379664,-0.317360810816575,-0.290077606997822,
-0.28792264499455,-0.287068935790219,-0.286448182970211,-0.285822713503579,
-0.285168887176482,-0.283644376730748,-0.274415223717295,-0.255647988357035,
-0.239630346018512,-0.148702508918191,-0.147593628698093,-0.130274722700396,
-0.127318798847395,-0.125815104355112,-0.124634464223438,-0.123323401018756,
-0.121165198987564,-0.11348676927498,-0.0877030398018594,-0.000958356721493471),
 .UNSPECIFIED.);
#847=B_SPLINE_CURVE_WITH_KNOTS('',3,(#53803,#53804,#53805,#53806,#53807,
#53808,#53809,#53810,#53811,#53812,#53813,#53814,#53815,#53816,#53817,#53818,
#53819,#53820,#53821,#53822,#53823,#53824,#53825,#53826,#53827,#53828,#53829,
#53830,#53831,#53832,#53833,#53834,#53835,#53836,#53837,#53838,#53839,#53840,
#53841,#53842,#53843,#53844,#53845,#53846,#53847,#53848,#53849,#53850,#53851,
#53852,#53853,#53854,#53855,#53856,#53857,#53858,#53859,#53860,#53861,#53862,
#53863,#53864,#53865,#53866,#53867,#53868,#53869,#53870,#53871,#53872,#53873,
#53874,#53875,#53876,#53877,#53878,#53879,#53880,#53881,#53882,#53883,#53884,
#53885,#53886,#53887,#53888,#53889,#53890,#53891,#53892,#53893,#53894,#53895,
#53896,#53897,#53898,#53899,#53900,#53901,#53902,#53903,#53904,#53905,#53906,
#53907,#53908,#53909,#53910,#53911,#53912,#53913,#53914,#53915,#53916,#53917,
#53918,#53919,#53920,#53921,#53922,#53923,#53924,#53925,#53926,#53927,#53928,
#53929,#53930,#53931,#53932,#53933,#53934,#53935,#53936,#53937,#53938,#53939,
#53940,#53941,#53942,#53943,#53944,#53945,#53946,#53947,#53948,#53949,#53950,
#53951,#53952,#53953,#53954,#53955,#53956,#53957,#53958,#53959,#53960,#53961,
#53962,#53963,#53964,#53965,#53966,#53967,#53968,#53969,#53970,#53971,#53972,
#53973,#53974,#53975,#53976,#53977,#53978,#53979,#53980,#53981,#53982,#53983,
#53984,#53985,#53986,#53987,#53988,#53989,#53990,#53991,#53992,#53993,#53994,
#53995,#53996,#53997,#53998,#53999,#54000,#54001,#54002,#54003,#54004,#54005,
#54006,#54007,#54008,#54009,#54010,#54011,#54012,#54013,#54014,#54015,#54016,
#54017,#54018,#54019,#54020,#54021,#54022,#54023,#54024,#54025,#54026,#54027,
#54028,#54029,#54030,#54031,#54032,#54033,#54034,#54035,#54036,#54037,#54038,
#54039,#54040,#54041,#54042,#54043,#54044,#54045,#54046,#54047,#54048,#54049,
#54050,#54051,#54052,#54053,#54054,#54055,#54056,#54057,#54058,#54059,#54060,
#54061,#54062,#54063,#54064,#54065,#54066,#54067,#54068,#54069,#54070,#54071,
#54072,#54073,#54074,#54075,#54076,#54077,#54078,#54079,#54080,#54081,#54082,
#54083,#54084,#54085,#54086,#54087,#54088,#54089,#54090,#54091,#54092,#54093,
#54094,#54095,#54096,#54097,#54098,#54099,#54100,#54101,#54102,#54103,#54104,
#54105,#54106,#54107,#54108,#54109,#54110,#54111,#54112,#54113,#54114,#54115,
#54116,#54117,#54118,#54119,#54120,#54121,#54122,#54123,#54124,#54125,#54126,
#54127,#54128,#54129,#54130,#54131,#54132,#54133,#54134,#54135,#54136,#54137,
#54138,#54139,#54140,#54141,#54142,#54143,#54144,#54145,#54146,#54147,#54148,
#54149,#54150,#54151,#54152,#54153,#54154,#54155,#54156,#54157,#54158,#54159,
#54160,#54161,#54162,#54163,#54164,#54165,#54166,#54167,#54168,#54169,#54170,
#54171,#54172,#54173,#54174,#54175,#54176,#54177,#54178,#54179,#54180,#54181,
#54182,#54183,#54184,#54185,#54186,#54187,#54188,#54189,#54190,#54191,#54192,
#54193,#54194,#54195,#54196,#54197,#54198,#54199,#54200,#54201,#54202,#54203,
#54204,#54205,#54206,#54207,#54208,#54209,#54210,#54211,#54212,#54213,#54214,
#54215,#54216,#54217,#54218,#54219,#54220,#54221,#54222,#54223,#54224,#54225,
#54226,#54227,#54228,#54229,#54230,#54231,#54232,#54233,#54234,#54235,#54236,
#54237,#54238,#54239,#54240,#54241,#54242,#54243,#54244,#54245,#54246,#54247,
#54248,#54249,#54250,#54251,#54252,#54253,#54254,#54255,#54256,#54257,#54258,
#54259,#54260,#54261,#54262,#54263,#54264,#54265,#54266,#54267,#54268,#54269,
#54270,#54271,#54272,#54273,#54274,#54275,#54276,#54277,#54278,#54279,#54280,
#54281,#54282,#54283,#54284,#54285,#54286,#54287,#54288,#54289,#54290,#54291,
#54292,#54293,#54294,#54295,#54296,#54297,#54298,#54299,#54300,#54301,#54302,
#54303,#54304,#54305,#54306,#54307,#54308,#54309,#54310,#54311,#54312,#54313,
#54314,#54315,#54316,#54317,#54318,#54319,#54320,#54321,#54322,#54323,#54324,
#54325,#54326,#54327,#54328,#54329,#54330,#54331,#54332,#54333,#54334,#54335,
#54336),.UNSPECIFIED.,.F.,.F.,(4,2,2,2,2,2,2,2,2,2,2,2,2,2,2,2,2,2,2,2,
2,2,2,2,2,2,2,2,2,2,2,2,2,2,2,2,2,2,2,2,2,2,2,2,2,2,2,2,2,2,2,2,2,2,2,2,
2,2,2,2,2,2,2,2,2,2,2,2,2,2,2,2,2,2,2,2,2,2,2,2,2,2,2,2,2,2,2,2,2,2,2,2,
2,2,2,2,2,2,2,2,2,2,2,2,2,2,2,2,2,2,2,2,2,2,2,2,2,2,2,2,2,2,2,2,2,2,2,2,
2,2,2,2,2,2,2,2,2,2,2,2,2,2,2,2,2,2,2,2,2,2,2,2,2,2,2,2,2,2,2,2,2,2,2,2,
2,2,2,2,2,2,2,2,2,2,2,2,2,2,2,2,2,2,2,2,2,2,2,2,2,2,2,2,2,2,2,2,2,2,2,2,
2,2,2,2,2,2,2,2,2,2,2,2,2,2,2,2,2,2,2,2,2,2,2,2,2,2,2,2,2,2,2,2,2,2,2,2,
2,2,2,2,2,2,2,2,2,2,2,2,2,2,2,2,2,2,2,2,2,2,2,2,2,2,2,2,2,2,4),(-4.06037209229428,
-4.02640913549226,-4.02504603866398,-4.02418868183135,-4.02353723092419,
-4.02291060247345,-4.02228792406252,-4.02142600964768,-4.01922159591739,
-3.98868429987278,-3.98388367217803,-3.92403925518192,-3.88413301701106,
-3.86676127380683,-3.86398900393097,-3.86254414327959,-3.86148205834355,
-3.86033574298703,-3.85868660654864,-3.85408055076813,-3.85229852113474,
-3.74861586758456,-3.72193257955187,-3.70936570669668,-3.70508737885633,
-3.70221092344829,-3.70117704982093,-3.70056367975202,-3.69990033234403,
-3.69903292540613,-3.69712548783886,-3.68187895887367,-3.68122880962401,
-3.66869381646718,-3.61932981463282,-3.61314374104717,-3.60580315493032,
-3.5968202708822,-3.58518149476958,-3.54909110310954,-3.54277252429512,
-3.54076348454315,-3.53948597495551,-3.5382963327726,-3.5367510393908,-3.5341782077674,
-3.51919347886417,-3.51495083163536,-3.44437762478163,-3.40854196383101,
-3.38989915539538,-3.38377420366753,-3.38124253154513,-3.37934629172893,
-3.37847454964509,-3.37784934931223,-3.37722889397738,-3.37637576252615,
-3.37467245723807,-3.3598877648246,-3.35844118610148,-3.35460502239932,
-3.27371736841735,-3.22774720668829,-3.22042522002019,-3.2183039872667,
-3.21700147825746,-3.2158194271038,-3.2143012707974,-3.21117073383994,-3.19103648388762,
-3.18515238702846,-3.10928068650413,-3.07947728086454,-3.06057104188322,
-3.05835957185709,-3.05665988718641,-3.05582667547211,-3.05519041887597,
-3.05455387469196,-3.05345240233324,-3.05037523131688,-2.99688625709063,
-2.90357405612487,-2.89749240669817,-2.89551228981326,-2.89424127468884,
-2.89304926316966,-2.89148881197816,-2.88805047712412,-2.85975714801818,
-2.77195991838237,-2.7394119722766,-2.73639421194111,-2.73488948707351,
-2.73397300638607,-2.73317142396205,-2.73252210197848,-2.7318900687036,
-2.73099363737232,-2.72857376613876,-2.68565036073925,-2.62945420995895,
-2.58262853746982,-2.57522621292564,-2.5730965530655,-2.57179212310483,
-2.57061046215371,-2.56909577696221,-2.56598291861817,-2.54623718540984,
-2.54473181795764,-2.46928228956254,-2.41373138063906,-2.41160580883417,
-2.41068912746642,-2.41002007796818,-2.40939935053494,-2.40854525675795,
-2.4068382246516,-2.39193927397282,-2.35859793967623,-2.33141594388722,
-2.30477660417554,-2.25987678314051,-2.25511279449212,-2.2515277102166,
-2.24992277236893,-2.24872775619021,-2.24761446668442,-2.24608867520263,
-2.24225396027311,-2.1901883776986,-2.12909356783482,-2.10331941725205,
-2.09051318055266,-2.08885862139936,-2.08803128177093,-2.08743680554677,
-2.08679969794487,-2.08569564255834,-2.08260130096764,-2.03166839848904,
-1.96328263158965,-1.95698715610408,-1.95151686386301,-1.93182203520147,
-1.92871130102069,-1.92719695270389,-1.92601523826596,-1.92471042726512,
-1.92257941817028,-1.91516533044424,-1.8682064277294,-1.77172766105245,
-1.76718830661844,-1.76590318021374,-1.76515487683486,-1.76456389262974,
-1.76376743506938,-1.76226159358856,-1.75353737512461,-1.73488097787056,
-1.69112686980541,-1.6116696257496,-1.60684050115156,-1.60497095481778,
-1.6038485060017,-1.60265846984708,-1.6010854512624,-1.59767270057822,-1.53934315974291,
-1.4490957415655,-1.44445156352843,-1.44317034216603,-1.44241539511016,
-1.4417594142684,-1.44094078619409,-1.43932938935112,-1.42793501977486,
-1.39791901064057,-1.30339992452531,-1.28605971416785,-1.28310267214911,
-1.28159873893875,-1.28044232460678,-1.27916531782585,-1.27783273392812,
-1.27588213617923,-1.27244355174192,-1.24675027158748,-1.2228528709134,
-1.12609023386585,-1.12158557401631,-1.12030405986131,-1.1195564729064,
-1.11896526890078,-1.11816751267975,-1.11665598629907,-1.10781376232755,
-1.08891442821059,-1.04247108026109,-0.96567946800784,-0.961121107469808,
-0.959478555304893,-0.958333621022034,-0.957176740473526,-0.955710335608556,
-0.954113503986432,-0.951534445925017,-0.946475484320042,-0.920683521925532,
-0.877218517377548,-0.80299567884522,-0.798795782674685,-0.797548397017467,
-0.796882282142163,-0.796227178679169,-0.795423829745015,-0.793885938536731,
-0.784448233629749,-0.77172521137124,-0.729958517925943,-0.675917526938045,
-0.641539959767883,-0.637930709470467,-0.636481909022103,-0.635290303110902,
-0.634086686442692,-0.632362264141079,-0.630406783631054,-0.626956410292478,
-0.619450435106283,-0.596012373336783,-0.550961374560593,-0.490368831628682,
-0.487073050284924,-0.476917230017275,-0.47522028903973,-0.474384157934497,
-0.473726524834264,-0.472983144044041,-0.471720606754265,-0.466805406167451,
-0.443513121518276,-0.392394235644475,-0.365081507815186,-0.319217003047633,
-0.315458634800603,-0.313945552144851,-0.312835217280349,-0.311661301465675,
-0.310088981231741,-0.308345660794175,-0.305414991345334,-0.299395810212257,
-0.20874642529792,-0.164154900034783,-0.1541408492381,-0.152472106198326,
-0.151630108932222,-0.150971787274006,-0.150231838534827,-0.148984883746677,
-0.144244761686984,-0.109485172234029,-0.000957829592074313),
 .UNSPECIFIED.);
#848=B_SPLINE_CURVE_WITH_KNOTS('',3,(#54338,#54339,#54340,#54341,#54342,
#54343,#54344,#54345,#54346,#54347,#54348,#54349,#54350,#54351,#54352,#54353,
#54354,#54355,#54356,#54357,#54358,#54359,#54360,#54361,#54362,#54363,#54364,
#54365,#54366,#54367,#54368,#54369,#54370,#54371,#54372,#54373,#54374,#54375,
#54376,#54377,#54378,#54379,#54380,#54381,#54382,#54383,#54384,#54385,#54386,
#54387,#54388,#54389,#54390,#54391,#54392,#54393,#54394,#54395,#54396,#54397,
#54398,#54399,#54400,#54401,#54402,#54403,#54404,#54405,#54406,#54407,#54408,
#54409,#54410,#54411,#54412,#54413,#54414,#54415,#54416,#54417,#54418,#54419,
#54420,#54421,#54422,#54423,#54424,#54425,#54426,#54427,#54428,#54429,#54430,
#54431,#54432,#54433,#54434,#54435,#54436,#54437,#54438,#54439,#54440,#54441,
#54442,#54443,#54444,#54445,#54446,#54447,#54448,#54449,#54450,#54451,#54452,
#54453,#54454,#54455,#54456,#54457,#54458,#54459,#54460,#54461,#54462,#54463,
#54464,#54465,#54466,#54467,#54468,#54469,#54470,#54471,#54472,#54473,#54474,
#54475,#54476,#54477,#54478,#54479,#54480,#54481,#54482,#54483,#54484,#54485,
#54486,#54487,#54488,#54489,#54490,#54491,#54492,#54493,#54494,#54495,#54496,
#54497,#54498,#54499,#54500,#54501,#54502,#54503,#54504,#54505,#54506,#54507,
#54508,#54509,#54510,#54511,#54512,#54513,#54514,#54515,#54516,#54517,#54518,
#54519,#54520,#54521,#54522,#54523,#54524,#54525,#54526,#54527,#54528,#54529,
#54530,#54531,#54532,#54533,#54534,#54535,#54536,#54537,#54538,#54539,#54540,
#54541,#54542,#54543,#54544,#54545,#54546,#54547,#54548,#54549,#54550,#54551,
#54552,#54553,#54554,#54555,#54556,#54557,#54558,#54559,#54560,#54561,#54562,
#54563,#54564,#54565,#54566,#54567,#54568,#54569,#54570,#54571,#54572,#54573,
#54574,#54575,#54576,#54577,#54578,#54579,#54580,#54581,#54582,#54583,#54584,
#54585,#54586,#54587,#54588,#54589,#54590,#54591,#54592,#54593,#54594,#54595,
#54596,#54597,#54598,#54599,#54600,#54601,#54602,#54603,#54604,#54605,#54606,
#54607,#54608,#54609,#54610,#54611,#54612,#54613,#54614,#54615,#54616,#54617,
#54618,#54619,#54620,#54621,#54622,#54623,#54624,#54625,#54626,#54627,#54628,
#54629,#54630,#54631,#54632,#54633,#54634,#54635,#54636,#54637,#54638,#54639,
#54640,#54641,#54642,#54643,#54644,#54645,#54646,#54647,#54648,#54649,#54650,
#54651,#54652,#54653,#54654,#54655,#54656,#54657,#54658,#54659,#54660,#54661,
#54662,#54663,#54664,#54665,#54666,#54667,#54668,#54669,#54670,#54671,#54672,
#54673,#54674,#54675,#54676,#54677,#54678,#54679,#54680,#54681,#54682,#54683,
#54684,#54685,#54686,#54687,#54688,#54689,#54690,#54691,#54692,#54693,#54694,
#54695,#54696,#54697,#54698,#54699,#54700,#54701,#54702,#54703,#54704,#54705,
#54706,#54707,#54708,#54709,#54710,#54711,#54712,#54713,#54714,#54715,#54716,
#54717,#54718,#54719,#54720,#54721,#54722,#54723,#54724,#54725,#54726,#54727,
#54728,#54729,#54730,#54731,#54732,#54733,#54734,#54735,#54736,#54737,#54738,
#54739,#54740,#54741,#54742,#54743,#54744,#54745,#54746,#54747,#54748,#54749,
#54750,#54751,#54752,#54753,#54754,#54755,#54756,#54757,#54758,#54759,#54760,
#54761,#54762,#54763,#54764,#54765,#54766,#54767,#54768,#54769,#54770,#54771,
#54772,#54773,#54774,#54775,#54776,#54777,#54778,#54779,#54780,#54781,#54782,
#54783,#54784,#54785,#54786,#54787,#54788,#54789,#54790,#54791,#54792,#54793,
#54794,#54795,#54796,#54797,#54798,#54799,#54800,#54801,#54802,#54803,#54804,
#54805,#54806,#54807,#54808,#54809,#54810,#54811,#54812,#54813,#54814,#54815,
#54816,#54817,#54818,#54819,#54820,#54821,#54822,#54823,#54824,#54825,#54826,
#54827,#54828,#54829,#54830,#54831,#54832,#54833,#54834,#54835,#54836,#54837,
#54838,#54839,#54840,#54841,#54842,#54843,#54844,#54845,#54846,#54847,#54848,
#54849,#54850,#54851,#54852,#54853,#54854,#54855,#54856,#54857,#54858,#54859,
#54860,#54861,#54862,#54863,#54864,#54865,#54866,#54867,#54868,#54869,#54870,
#54871,#54872,#54873,#54874,#54875,#54876,#54877,#54878,#54879,#54880,#54881,
#54882,#54883,#54884,#54885),.UNSPECIFIED.,.F.,.F.,(4,2,2,2,2,2,2,2,2,2,
2,2,2,2,2,2,2,2,2,2,2,2,2,2,2,2,2,2,2,2,2,2,2,2,2,2,2,2,2,2,2,2,2,2,2,2,
2,2,2,2,2,2,2,2,2,2,2,2,2,2,2,2,2,2,2,2,2,2,2,2,2,2,2,2,2,2,2,2,2,2,2,2,
2,2,2,2,2,2,2,2,2,2,2,2,2,2,2,2,2,2,2,2,2,2,2,2,2,2,2,2,2,2,2,2,2,2,2,2,
2,2,2,2,2,2,2,2,2,2,2,2,2,2,2,2,2,2,2,2,2,2,2,2,2,2,2,2,2,2,2,2,2,2,2,2,
2,2,2,2,2,2,2,2,2,2,2,2,2,2,2,2,2,2,2,2,2,2,2,2,2,2,2,2,2,2,2,2,2,2,2,2,
2,2,2,2,2,2,2,2,2,2,2,2,2,2,2,2,2,2,2,2,2,2,2,2,2,2,2,2,2,2,2,2,2,2,2,2,
2,2,2,2,2,2,2,2,2,2,2,2,2,2,2,2,2,2,2,2,2,2,2,2,2,2,2,2,2,2,2,2,2,2,2,2,
2,2,2,2,2,2,2,2,2,2,2,4),(-4.06165407026546,-4.05740964544468,-4.05400539194529,
-4.0524781749501,-4.05131240313444,-4.05018996086548,-4.04908094134211,
-4.04757269022949,-4.04384170581745,-4.03641892777598,-3.93042213168213,
-3.89574718704119,-3.8910137597619,-3.8897674188987,-3.88902761014295,-3.88836926114119,
-3.88752703060503,-3.88585720714289,-3.87582213268271,-3.83122313814856,
-3.74048883286755,-3.7345677413575,-3.73167229838484,-3.72994353557879,
-3.72838211363205,-3.72721009201704,-3.72609708027135,-3.72457364209001,
-3.72075506851831,-3.67032219040894,-3.64596709898665,-3.61423912190594,
-3.5707475787363,-3.56782671199944,-3.56678485733794,-3.56609050411309,
-3.56542190897701,-3.5646200326619,-3.56263957493068,-3.54510307177094,
-3.45795244305617,-3.43574125061026,-3.41856748049928,-3.41219603235631,
-3.40913971441172,-3.40734464549353,-3.4057353064316,-3.40455507238027,
-3.40345379493462,-3.40197628846588,-3.39834336951894,-3.36083303398119,
-3.31247646323611,-3.29498682328827,-3.28245725928372,-3.25006695443711,
-3.24550758849709,-3.24427759259807,-3.24354153904301,-3.24288261900017,
-3.24203435416075,-3.24027628828694,-3.22884797334992,-3.15362639018163,
-3.09436451820203,-3.08883821369963,-3.08608631631904,-3.08441725337565,
-3.08290043957803,-3.0817353317018,-3.08060999758779,-3.07903937121443,
-3.07583104166304,-3.04318356447465,-2.95611042419199,-2.92697263377816,
-2.92268133746237,-2.92147736524947,-2.92074709255175,-2.92008671462688,
-2.91924170664772,-2.91745415837025,-2.90536243771982,-2.86180633726569,
-2.77143704122718,-2.76597390706601,-2.76324511150198,-2.76158563103093,
-2.760073974608,-2.75890999180129,-2.75778190457202,-2.75620124707182,-2.75203853286507,
-2.68776167341046,-2.64153826193142,-2.61194310789301,-2.6006374655522,
-2.59902896213997,-2.59821090184312,-2.59755496782113,-2.59679964666062,
-2.59551663765062,-2.59085462247898,-2.49531730542908,-2.45808649774396,
-2.44128892995578,-2.43853959175595,-2.4370992031111,-2.43603726791407,
-2.43488807738552,-2.43322960073072,-2.42856383620457,-2.35588170651182,
-2.31312004970147,-2.28166606413652,-2.27870424789595,-2.27653862753007,
-2.27561483636152,-2.27494442880766,-2.27432524226566,-2.27347741592653,
-2.27135653055447,-2.24597186350575,-2.17011162254495,-2.13498825231204,
-2.11855901736462,-2.11582520576584,-2.11438797382565,-2.11332626634158,
-2.11217528142981,-2.11051070167082,-2.10580485953711,-2.03081534233176,
-1.9586365768906,-1.95447342316307,-1.95323022550838,-1.95256491691888,
-1.95190950885699,-1.95110429127795,-1.94955878461852,-1.93995470904831,
-1.92268570516832,-1.897393739233,-1.82333119120031,-1.81567369047869,-1.79648765894569,
-1.79339925264149,-1.7918887192281,-1.79070675953333,-1.78939838312632,
-1.78725407228404,-1.77971998292058,-1.75422595681069,-1.71141794876818,
-1.63586064375099,-1.6318113298592,-1.63058152952279,-1.62991892826898,
-1.62926389575223,-1.62845553470062,-1.62689124574334,-1.61677272106587,
-1.59269104607831,-1.50287722020347,-1.47419844964061,-1.4707937429151,
-1.46935741020303,-1.46815776711736,-1.46692515368837,-1.46512088902775,
-1.46032860967519,-1.43736654712427,-1.41546954831765,-1.34284595903923,
-1.31066838506157,-1.3084423072406,-1.30757679093033,-1.30695325059003,
-1.30629960515896,-1.30542173652212,-1.30444371401243,-1.30279013778082,
-1.2623735630243,-1.16611216232519,-1.15042218510316,-1.14780965890159,
-1.14625199498803,-1.14505956892014,-1.14378564067582,-1.14179588099459,
-1.1356451969395,-1.10110282100427,-1.00240765596283,-0.987193855677619,
-0.985284903838327,-0.984416220519701,-0.983764238604498,-0.98306030625779,
-0.981955612611417,-0.980656220700224,-0.978194157829027,-0.95547247504219,
-0.93057438950738,-0.854891794714637,-0.84601465565169,-0.828427824497416,
-0.825452646625093,-0.823942490072284,-0.822758393424724,-0.821445151191329,
-0.819287150008426,-0.811647526538121,-0.785956023021821,-0.769624505543458,
-0.757708102428476,-0.70259084313062,-0.665593756811462,-0.663247552340367,
-0.662362571197941,-0.661733354881777,-0.661085221888442,-0.660231446611528,
-0.659284516030755,-0.657700729057482,-0.654455287059512,-0.645839835409615,
-0.624811803750036,-0.532107702575697,-0.523762298751068,-0.520004480876801,
-0.504716195978818,-0.502138153598254,-0.500596564254775,-0.499413821016613,
-0.498147688628208,-0.496164835837219,-0.489994672960956,-0.455126923023744,
-0.42772766814659,-0.419675561577709,-0.412813942731298,-0.4068450200568,
-0.347371747571115,-0.340932524122567,-0.339622276546277,-0.338792525752766,
-0.338168700191169,-0.337448947843508,-0.336271270044064,-0.334864202572282,
-0.332113875489203,-0.325263611732087,-0.300209541027107,-0.219742396136675,
-0.212508367882264,-0.182322803766125,-0.17916319551422,-0.177600541216223,
-0.176473531952652,-0.175276043651974,-0.173688737720666,-0.170227417512946,
-0.103878048749372,-0.0311419473554923,-0.0269734683702882,-0.0182226738461123,
-0.0167539138764466,-0.0158784160279446,-0.0152185369868466,-0.0145871428898369,
-0.0138632201451378,-0.0128415480744668,-0.00908015386448269,-0.00096178856909809),
 .UNSPECIFIED.);
#849=B_SPLINE_CURVE_WITH_KNOTS('',3,(#54887,#54888,#54889,#54890,#54891,
#54892,#54893,#54894,#54895,#54896,#54897,#54898,#54899,#54900,#54901,#54902,
#54903,#54904,#54905),.UNSPECIFIED.,.F.,.F.,(4,3,3,3,3,3,4),(14.8194310462886,
14.9820505664306,15.1443726613452,15.306670802268,15.4689507744941,15.6315623856294,
15.7079632677806),.UNSPECIFIED.);
#850=B_SPLINE_CURVE_WITH_KNOTS('',3,(#54909,#54910,#54911,#54912,#54913,
#54914,#54915,#54916,#54917,#54918,#54919,#54920,#54921,#54922,#54923,#54924,
#54925,#54926,#54927,#54928,#54929,#54930,#54931,#54932,#54933,#54934,#54935,
#54936,#54937,#54938,#54939,#54940,#54941,#54942,#54943,#54944,#54945,#54946,
#54947,#54948,#54949,#54950,#54951,#54952,#54953,#54954,#54955,#54956,#54957,
#54958,#54959,#54960,#54961,#54962,#54963,#54964,#54965,#54966,#54967,#54968,
#54969,#54970,#54971,#54972,#54973,#54974,#54975,#54976,#54977,#54978,#54979,
#54980,#54981,#54982,#54983,#54984,#54985,#54986,#54987,#54988,#54989,#54990,
#54991,#54992,#54993,#54994,#54995,#54996,#54997,#54998,#54999,#55000,#55001,
#55002,#55003,#55004,#55005,#55006,#55007,#55008,#55009,#55010,#55011,#55012,
#55013,#55014,#55015,#55016,#55017),.UNSPECIFIED.,.F.,.F.,(4,3,3,3,3,3,
3,3,3,3,3,3,3,3,3,3,3,3,3,3,3,3,3,3,3,3,3,3,3,3,3,3,3,3,3,3,4),(16.0586828769936,
16.228071424883,16.3973387439612,16.5667947821335,16.7363202110308,16.906337659739,
17.0574752807613,17.2212840646477,17.3847419026725,17.5526233481367,17.7159497278199,
17.8861087061746,18.0562676845293,18.2219517445982,18.3873187559091,18.5542540890062,
18.7195349605951,18.8872975244462,19.0550600882973,19.2208116332235,19.3862551116776,
19.5531544567745,19.7185320739229,19.8861922829941,20.0538524920653,20.2191011613401,
20.3840291050623,20.5511830527551,20.7160253663893,20.8843351311113,21.0526448958333,
21.2166948429012,21.3804312878908,21.5441304586967,21.707790871614,21.8718046546966,
21.9911485749085),.UNSPECIFIED.);
#851=B_SPLINE_CURVE_WITH_KNOTS('',3,(#55019,#55020,#55021,#55022,#55023,
#55024,#55025,#55026,#55027,#55028,#55029,#55030,#55031,#55032,#55033,#55034,
#55035,#55036,#55037,#55038,#55039,#55040,#55041,#55042,#55043,#55044,#55045,
#55046,#55047,#55048,#55049,#55050,#55051,#55052,#55053,#55054,#55055,#55056,
#55057,#55058,#55059,#55060,#55061,#55062,#55063,#55064,#55065,#55066,#55067,
#55068,#55069,#55070,#55071,#55072,#55073,#55074,#55075,#55076,#55077,#55078,
#55079,#55080,#55081,#55082,#55083,#55084,#55085,#55086,#55087,#55088,#55089,
#55090,#55091,#55092,#55093,#55094,#55095,#55096,#55097,#55098,#55099,#55100,
#55101,#55102,#55103,#55104,#55105,#55106,#55107,#55108,#55109,#55110,#55111,
#55112,#55113,#55114,#55115,#55116,#55117,#55118,#55119,#55120,#55121,#55122,
#55123,#55124,#55125,#55126,#55127,#55128,#55129,#55130,#55131,#55132,#55133,
#55134,#55135,#55136,#55137,#55138,#55139,#55140,#55141,#55142,#55143,#55144,
#55145,#55146,#55147,#55148,#55149,#55150,#55151,#55152,#55153,#55154,#55155,
#55156,#55157,#55158,#55159,#55160,#55161,#55162,#55163,#55164,#55165,#55166,
#55167,#55168,#55169,#55170,#55171,#55172,#55173,#55174,#55175,#55176,#55177,
#55178,#55179,#55180,#55181,#55182,#55183,#55184,#55185,#55186,#55187,#55188,
#55189,#55190,#55191,#55192,#55193,#55194,#55195,#55196,#55197,#55198,#55199,
#55200,#55201,#55202,#55203,#55204,#55205,#55206,#55207,#55208,#55209,#55210,
#55211,#55212,#55213,#55214,#55215,#55216,#55217,#55218,#55219,#55220,#55221,
#55222,#55223,#55224,#55225,#55226,#55227,#55228,#55229,#55230,#55231,#55232,
#55233,#55234,#55235,#55236,#55237,#55238,#55239,#55240,#55241,#55242,#55243,
#55244,#55245,#55246,#55247,#55248,#55249,#55250,#55251,#55252,#55253,#55254,
#55255,#55256,#55257,#55258,#55259,#55260,#55261,#55262,#55263,#55264,#55265,
#55266,#55267,#55268,#55269,#55270,#55271,#55272,#55273,#55274,#55275,#55276,
#55277,#55278,#55279,#55280,#55281,#55282,#55283,#55284,#55285,#55286,#55287,
#55288,#55289,#55290,#55291,#55292,#55293,#55294,#55295,#55296,#55297,#55298,
#55299,#55300,#55301,#55302,#55303,#55304,#55305,#55306,#55307,#55308,#55309,
#55310,#55311,#55312,#55313,#55314,#55315,#55316,#55317,#55318,#55319,#55320,
#55321,#55322,#55323,#55324,#55325,#55326,#55327,#55328,#55329,#55330,#55331,
#55332,#55333,#55334,#55335,#55336,#55337,#55338,#55339,#55340,#55341,#55342,
#55343,#55344,#55345,#55346,#55347,#55348,#55349,#55350,#55351,#55352,#55353,
#55354,#55355,#55356,#55357,#55358,#55359,#55360,#55361,#55362,#55363,#55364,
#55365,#55366,#55367,#55368,#55369,#55370,#55371,#55372,#55373,#55374,#55375,
#55376,#55377,#55378,#55379,#55380,#55381,#55382,#55383,#55384,#55385,#55386,
#55387,#55388,#55389,#55390,#55391,#55392,#55393,#55394,#55395,#55396,#55397,
#55398,#55399,#55400,#55401,#55402,#55403,#55404,#55405,#55406,#55407,#55408,
#55409,#55410,#55411,#55412,#55413,#55414,#55415,#55416,#55417,#55418,#55419,
#55420,#55421,#55422,#55423,#55424,#55425,#55426,#55427,#55428,#55429,#55430,
#55431,#55432,#55433,#55434,#55435,#55436,#55437,#55438,#55439,#55440,#55441,
#55442,#55443,#55444,#55445,#55446,#55447,#55448,#55449,#55450,#55451,#55452,
#55453,#55454,#55455,#55456,#55457,#55458,#55459,#55460,#55461,#55462,#55463,
#55464,#55465,#55466,#55467,#55468,#55469,#55470,#55471,#55472,#55473,#55474,
#55475,#55476,#55477,#55478,#55479,#55480,#55481,#55482,#55483,#55484,#55485,
#55486,#55487,#55488,#55489,#55490,#55491,#55492,#55493,#55494,#55495,#55496,
#55497,#55498,#55499,#55500,#55501,#55502,#55503,#55504,#55505,#55506,#55507,
#55508,#55509,#55510,#55511,#55512,#55513,#55514,#55515,#55516,#55517,#55518,
#55519,#55520,#55521,#55522,#55523,#55524,#55525,#55526,#55527,#55528,#55529,
#55530,#55531,#55532,#55533,#55534,#55535,#55536,#55537,#55538,#55539,#55540,
#55541,#55542,#55543,#55544,#55545,#55546,#55547,#55548,#55549,#55550,#55551,
#55552,#55553,#55554,#55555,#55556,#55557,#55558),.UNSPECIFIED.,.F.,.F.,
(4,2,2,2,2,2,2,2,2,2,2,2,2,2,2,2,2,2,2,2,2,2,2,2,2,2,2,2,2,2,2,2,2,2,2,
2,2,2,2,2,2,2,2,2,2,2,2,2,2,2,2,2,2,2,2,2,2,2,2,2,2,2,2,2,2,2,2,2,2,2,2,
2,2,2,2,2,2,2,2,2,2,2,2,2,2,2,2,2,2,2,2,2,2,2,2,2,2,2,2,2,2,2,2,2,2,2,2,
2,2,2,2,2,2,2,2,2,2,2,2,2,2,2,2,2,2,2,2,2,2,2,2,2,2,2,2,2,2,2,2,2,2,2,2,
2,2,2,2,2,2,2,2,2,2,2,2,2,2,2,2,2,2,2,2,2,2,2,2,2,2,2,2,2,2,2,2,2,2,2,2,
2,2,2,2,2,2,2,2,2,2,2,2,2,2,2,2,2,2,2,2,2,2,2,2,2,2,2,2,2,2,2,2,2,2,2,2,
2,2,2,2,2,2,2,2,2,2,2,2,2,2,2,2,2,2,2,2,2,2,2,2,2,2,2,2,2,2,2,2,2,2,2,2,
2,2,2,2,2,2,2,2,2,2,2,2,2,2,2,2,2,2,4),(-4.06062904163106,-4.04570360185412,
-4.04390479883215,-4.04286596618711,-4.04214226005793,-4.04152432695382,
-4.04089273972695,-4.04005118959283,-4.03833265676747,-4.02779688455913,
-4.02475212675819,-4.02057511193562,-3.95556552189716,-3.88599997279386,
-3.88254007503904,-3.8809567331219,-3.87976361458958,-3.87864172965352,
-3.87708779235204,-3.87395082788115,-3.84427456933291,-3.75729595410533,
-3.7315861969366,-3.72465186402193,-3.72187832226222,-3.72046333458138,
-3.71928077316759,-3.71856063837893,-3.71793479508989,-3.71710300984889,
-3.71579295430406,-3.70942190820894,-3.65247735656485,-3.64690576232457,
-3.64055415360531,-3.63318376102258,-3.62441538901417,-3.56502277266714,
-3.56022663834124,-3.55842182838225,-3.55718912501054,-3.55598961204051,
-3.554553692942,-3.55101658888885,-3.51930538088721,-3.47245882505677,-3.4261708206132,
-3.40730001512376,-3.40146679170015,-3.39902481377663,-3.39773501909049,
-3.39663793520301,-3.39593819392463,-3.39528770808305,-3.3944194258323,
-3.39250864501398,-3.37718292236751,-3.37582408706139,-3.29182806322054,
-3.24561168171937,-3.23826438270998,-3.23613951464844,-3.23483558510705,
-3.23365277735547,-3.23213439102603,-3.22900600880857,-3.20895314382336,
-3.20716332962316,-3.19428533140588,-3.11143431645357,-3.07989420077164,
-3.07692720542661,-3.07544061644637,-3.07453137827011,-3.07369302826554,
-3.07304702212045,-3.07240341640841,-3.0712677872062,-3.06794972666932,
-3.00879557124416,-2.9595658190066,-2.94192509180402,-2.91978835700861,
-2.91509817342019,-2.91330825880092,-2.91207777738029,-2.91087423098795,
-2.90942602564079,-2.90581984517675,-2.87158578710844,-2.78886111437125,
-2.75731205006472,-2.75434511715292,-2.7528587850803,-2.75194982978359,
-2.7511215338754,-2.75047514605092,-2.74983394496181,-2.74870988564432,
-2.74547330168384,-2.74500917989446,-2.68523401249009,-2.62649219500212,
-2.60084220835202,-2.59582627073307,-2.59208950713824,-2.59045691086623,
-2.58925694799464,-2.58815011363426,-2.58665011398216,-2.58372132561593,
-2.56070879580912,-2.54378188828005,-2.46926518708424,-2.44270686700676,
-2.4309344045196,-2.4293106959667,-2.428489544122,-2.42783933694991,-2.42718503162967,
-2.42599624872686,-2.42228006951242,-2.35734309009427,-2.32399520619353,
-2.28823251548006,-2.27170092880894,-2.26896224602825,-2.26752379568303,
-2.26646175367632,-2.26531095550206,-2.26364759133703,-2.25895135088672,
-2.18005319719431,-2.14259879251171,-2.10911490296156,-2.10697795909713,
-2.10605896326605,-2.10538921852708,-2.1047686137569,-2.1039157581023,-2.10176636888289,
-2.07481669973366,-2.03147697517407,-1.95250504854578,-1.94748580179032,
-1.94558551879651,-1.94445689301101,-1.94326935306538,-1.94171471229048,
-1.93839974162612,-1.89408825722172,-1.8435538926705,-1.78790421228387,
-1.78478477137643,-1.78367727278607,-1.78303931149941,-1.78244478899956,
-1.78161853530436,-1.77997025631581,-1.76739898769783,-1.74145618156212,
-1.67666002857445,-1.62821277920486,-1.62441926195705,-1.62290017041284,
-1.62178832510878,-1.62059158807168,-1.61897862350564,-1.61535168392906,
-1.57144159253841,-1.52087302829296,-1.46529490340021,-1.46220047248265,
-1.46109613483065,-1.46045879909683,-1.45986405594485,-1.45903626859684,
-1.45738055002091,-1.44455270247651,-1.41879700397575,-1.35883124267773,
-1.33488767436293,-1.30509399970225,-1.30195686754842,-1.30040384322776,
-1.29928308383072,-1.29811544908455,-1.29658055736026,-1.29488897303617,
-1.29208312021498,-1.23321401263478,-1.144302083178,-1.139868940756,-1.13859507713029,
-1.13784908546256,-1.13725751111051,-1.13645715746509,-1.13493389098948,
-1.12583770330936,-1.10668350589057,-1.0591714618927,-0.983887328247649,
-0.979411951856088,-0.977781807930227,-0.976640134521728,-0.975480974398116,
-0.97400765260036,-0.972399107054665,-0.969792376505275,-0.964659618590341,
-0.913416879026794,-0.828860645516561,-0.817919742226803,-0.816183877249544,
-0.815339837149445,-0.814681209609328,-0.81394229093811,-0.81270022400218,
-0.808014637431663,-0.773995699930228,-0.76176438252304,-0.708625793981986,
-0.660219245749986,-0.656424784839306,-0.654905277707063,-0.653793114794276,
-0.652620097273498,-0.651053692004251,-0.649318491389566,-0.646407763989167,
-0.640444556270726,-0.549713700438118,-0.505124847630551,-0.495108088602803,
-0.493438933812155,-0.492596731044865,-0.491938248640452,-0.491198113737797,
-0.489950832949214,-0.485209321070121,-0.450436217023383,-0.426532372750122,
-0.396421226157924,-0.337606682590258,-0.333715753423511,-0.332179690624836,
-0.331063142951378,-0.329892638562272,-0.328341719684826,-0.326627954801142,
-0.323769123622164,-0.317949950797744,-0.227034516771874,-0.182383601828387,
-0.172337998166678,-0.170667239338103,-0.169824637255569,-0.169166045185823,
-0.168426004895614,-0.16717938028982,-0.162446072367399,-0.127788719663138,
-0.0178688328568037,-0.0115443800013135,-0.00945485230489118,-0.00828833477619918,
-0.00712531855638712,-0.00599379196373133,-0.00457291864233748,-0.000957836357716254),
 .UNSPECIFIED.);
#852=B_SPLINE_CURVE_WITH_KNOTS('',3,(#55560,#55561,#55562,#55563,#55564,
#55565,#55566,#55567,#55568,#55569,#55570,#55571,#55572,#55573,#55574,#55575,
#55576,#55577,#55578,#55579,#55580,#55581,#55582,#55583,#55584,#55585,#55586,
#55587,#55588,#55589,#55590,#55591,#55592,#55593,#55594,#55595,#55596,#55597,
#55598,#55599,#55600,#55601,#55602,#55603,#55604,#55605,#55606,#55607,#55608,
#55609,#55610,#55611,#55612,#55613,#55614,#55615,#55616,#55617,#55618,#55619,
#55620,#55621,#55622,#55623,#55624,#55625,#55626,#55627,#55628,#55629,#55630,
#55631,#55632,#55633,#55634,#55635,#55636,#55637,#55638,#55639,#55640,#55641,
#55642,#55643,#55644,#55645,#55646,#55647,#55648,#55649,#55650,#55651,#55652,
#55653,#55654,#55655,#55656,#55657,#55658,#55659,#55660,#55661,#55662,#55663,
#55664,#55665,#55666,#55667,#55668,#55669,#55670,#55671,#55672,#55673,#55674,
#55675,#55676,#55677,#55678,#55679,#55680,#55681,#55682,#55683,#55684,#55685,
#55686,#55687,#55688,#55689,#55690,#55691,#55692,#55693,#55694,#55695,#55696,
#55697,#55698,#55699,#55700,#55701,#55702,#55703,#55704,#55705,#55706,#55707,
#55708,#55709,#55710,#55711,#55712,#55713,#55714,#55715,#55716,#55717,#55718,
#55719,#55720,#55721,#55722,#55723,#55724,#55725,#55726,#55727,#55728,#55729,
#55730,#55731,#55732,#55733,#55734,#55735,#55736,#55737,#55738,#55739,#55740,
#55741,#55742,#55743,#55744,#55745,#55746,#55747,#55748,#55749,#55750,#55751,
#55752,#55753,#55754,#55755,#55756,#55757,#55758,#55759,#55760,#55761,#55762,
#55763,#55764,#55765,#55766,#55767,#55768,#55769,#55770,#55771,#55772,#55773,
#55774,#55775,#55776,#55777,#55778,#55779,#55780,#55781,#55782,#55783,#55784,
#55785,#55786,#55787,#55788,#55789,#55790,#55791,#55792,#55793,#55794,#55795,
#55796,#55797,#55798,#55799,#55800,#55801,#55802,#55803,#55804,#55805,#55806,
#55807,#55808,#55809,#55810,#55811,#55812,#55813,#55814,#55815,#55816,#55817,
#55818,#55819,#55820,#55821,#55822,#55823,#55824,#55825,#55826,#55827,#55828,
#55829,#55830,#55831,#55832,#55833,#55834,#55835,#55836,#55837,#55838,#55839,
#55840,#55841,#55842,#55843,#55844,#55845,#55846,#55847,#55848,#55849,#55850,
#55851,#55852,#55853,#55854,#55855,#55856,#55857,#55858,#55859,#55860,#55861,
#55862,#55863,#55864,#55865,#55866,#55867,#55868,#55869,#55870,#55871,#55872,
#55873,#55874,#55875,#55876,#55877,#55878,#55879,#55880,#55881,#55882,#55883,
#55884,#55885,#55886,#55887,#55888,#55889,#55890,#55891,#55892,#55893,#55894,
#55895,#55896,#55897,#55898,#55899,#55900,#55901,#55902,#55903,#55904,#55905,
#55906,#55907,#55908,#55909,#55910,#55911,#55912,#55913,#55914,#55915,#55916,
#55917,#55918,#55919,#55920,#55921,#55922,#55923,#55924,#55925,#55926,#55927,
#55928,#55929,#55930,#55931,#55932,#55933,#55934,#55935,#55936,#55937,#55938,
#55939,#55940,#55941,#55942,#55943,#55944,#55945,#55946,#55947,#55948,#55949,
#55950,#55951,#55952,#55953,#55954,#55955,#55956,#55957,#55958,#55959,#55960,
#55961,#55962,#55963,#55964,#55965,#55966,#55967,#55968,#55969,#55970,#55971,
#55972,#55973,#55974,#55975,#55976,#55977,#55978,#55979,#55980,#55981,#55982,
#55983,#55984,#55985,#55986,#55987,#55988,#55989,#55990,#55991,#55992,#55993,
#55994,#55995,#55996,#55997,#55998,#55999,#56000,#56001,#56002,#56003,#56004,
#56005,#56006,#56007,#56008,#56009,#56010,#56011,#56012,#56013,#56014,#56015,
#56016,#56017,#56018,#56019,#56020,#56021,#56022,#56023,#56024,#56025,#56026,
#56027,#56028,#56029,#56030,#56031,#56032,#56033,#56034,#56035,#56036,#56037,
#56038,#56039,#56040,#56041,#56042,#56043,#56044,#56045,#56046,#56047,#56048,
#56049,#56050,#56051,#56052,#56053,#56054,#56055,#56056,#56057,#56058,#56059,
#56060,#56061,#56062,#56063,#56064,#56065,#56066,#56067,#56068,#56069,#56070,
#56071,#56072,#56073,#56074,#56075,#56076,#56077,#56078,#56079,#56080,#56081,
#56082,#56083,#56084,#56085,#56086,#56087,#56088,#56089,#56090,#56091,#56092,
#56093),.UNSPECIFIED.,.F.,.F.,(4,2,2,2,2,2,2,2,2,2,2,2,2,2,2,2,2,2,2,2,
2,2,2,2,2,2,2,2,2,2,2,2,2,2,2,2,2,2,2,2,2,2,2,2,2,2,2,2,2,2,2,2,2,2,2,2,
2,2,2,2,2,2,2,2,2,2,2,2,2,2,2,2,2,2,2,2,2,2,2,2,2,2,2,2,2,2,2,2,2,2,2,2,
2,2,2,2,2,2,2,2,2,2,2,2,2,2,2,2,2,2,2,2,2,2,2,2,2,2,2,2,2,2,2,2,2,2,2,2,
2,2,2,2,2,2,2,2,2,2,2,2,2,2,2,2,2,2,2,2,2,2,2,2,2,2,2,2,2,2,2,2,2,2,2,2,
2,2,2,2,2,2,2,2,2,2,2,2,2,2,2,2,2,2,2,2,2,2,2,2,2,2,2,2,2,2,2,2,2,2,2,2,
2,2,2,2,2,2,2,2,2,2,2,2,2,2,2,2,2,2,2,2,2,2,2,2,2,2,2,2,2,2,2,2,2,2,2,2,
2,2,2,2,2,2,2,2,2,2,2,2,2,2,2,2,2,2,2,2,2,2,2,2,2,2,2,2,2,2,4),(-4.06064425517163,
-4.05296410003843,-3.94672613835459,-3.91290974138407,-3.90982817367382,
-3.90759311330821,-3.90665714968852,-3.90598433074735,-3.90536761780485,
-3.90452991114187,-3.90288823337092,-3.88994164328037,-3.88923479658141,
-3.8888496971427,-3.81580461233557,-3.75180985328595,-3.74895640602316,
-3.74724504606555,-3.74569574611307,-3.74452575290477,-3.74340916632325,
-3.7418720093438,-3.73797272524807,-3.67711571784792,-3.61318095284064,
-3.58922058650699,-3.58539996295065,-3.58424570667373,-3.58352653706374,
-3.58286281456234,-3.58199518353242,-3.58008831861781,-3.56488463684256,
-3.56133858435174,-3.46549597030189,-3.4295816746418,-3.42650248000174,
-3.42469799407264,-3.42308168298624,-3.42189979392784,-3.42079983151505,
-3.41932776334154,-3.4158021287258,-3.3818918259257,-3.31795507364913,-3.302363586632,
-3.27693668371665,-3.26363201118395,-3.26196312442044,-3.26113268239232,
-3.26053759258747,-3.25990138556735,-3.25880265704849,-3.25574640415757,
-3.20032557994589,-3.1497432485707,-3.10659725780123,-3.1037152656533,-3.10199210514405,
-3.10043441316532,-3.09934223519345,-3.09824147695676,-3.09676621172103,
-3.09322276854617,-3.05858274861475,-2.97902836439941,-2.9449760657488,
-2.94188310706846,-2.93964150988172,-2.93870445394111,-2.93803145074841,
-2.93741500549012,-2.93657828822805,-2.9349404059872,-2.92209901734225,
-2.92131518620934,-2.92071440131782,-2.83936312339982,-2.78840430260704,
-2.78328690807435,-2.78068596175113,-2.77907991030517,-2.77760688181741,
-2.7764485949315,-2.77530620846294,-2.77367308634269,-2.76917727782508,
-2.69336270630096,-2.64615398749984,-2.62706490027276,-2.6181052545071,
-2.61658828552802,-2.61578934036829,-2.61514055230356,-2.61447343446265,
-2.61322114832562,-2.60897888032015,-2.53444309444672,-2.49124612813746,
-2.46558517549526,-2.460565659559,-2.45682660954906,-2.45519341085603,-2.45399315818889,
-2.45288616410474,-2.45138611160395,-2.44845770158678,-2.42546649641701,
-2.35658341025406,-2.32163066022849,-2.30654519623683,-2.2956295550279,
-2.29403439703826,-2.29321905585137,-2.29256322549915,-2.29190407891758,
-2.29069134203691,-2.28678328140576,-2.18352486079379,-2.14197088536682,
-2.13507991615464,-2.13300448494649,-2.13171183708642,-2.13052648596604,
-2.1290122267874,-2.12582022176927,-2.10431017386536,-2.03045972163131,
-1.9965528404156,-1.97369492010131,-1.97162356687346,-1.9707842467643,-1.97016718679459,
-1.9694948547294,-1.9685610832051,-1.96633833059885,-1.96327811573176,-1.9298978486507,
-1.84283708775814,-1.81475224998551,-1.81131923743569,-1.80975932830531,
-1.80856695515276,-1.80729480237645,-1.80531136292772,-1.79920759370235,
-1.76508705677307,-1.66838573118981,-1.65077879345792,-1.64879631290665,
-1.64799408576513,-1.64732538816017,-1.64663114419488,-1.64558981965511,
-1.64267277887198,-1.58001750174665,-1.50962490411154,-1.50857569369179,
-1.49134761577209,-1.48839605337645,-1.48689310294381,-1.48571232492881,
-1.48440036336656,-1.4822389698576,-1.47453169167166,-1.44869599340569,
-1.4051494839862,-1.33864283932188,-1.32777635012069,-1.32604402214284,
-1.32520080279432,-1.32454239999897,-1.32381820112596,-1.32261722005126,
-1.32117610379163,-1.31833241182128,-1.2890854999383,-1.20185222291373,
-1.19580780068877,-1.18818435108172,-1.16887652984217,-1.16578306136782,
-1.1642718143428,-1.16309010111076,-1.16178282079033,-1.15964217715774,
-1.15213950678408,-1.10422872324986,-1.01769456895971,-1.00518409047303,
-1.00355824665588,-1.00272461344346,-1.00210894143622,-1.00144920850849,
-1.00053666576166,-0.999510640934306,-0.997739686801674,-0.993971735812353,
-0.930979557123285,-0.849183363239738,-0.844039575339781,-0.842119746146725,
-0.840987269418947,-0.839919915458461,-0.838439551967217,-0.835499190509757,
-0.813289963621546,-0.794480429412944,-0.698841334603281,-0.696248501497367,
-0.695790285575151,-0.69400985109842,-0.682349134146024,-0.680580318391485,
-0.67972979910098,-0.679070459812087,-0.67835017053872,-0.677168291943857,
-0.675754030672242,-0.67298299125,-0.666058629994212,-0.640456317861474,
-0.553893475679808,-0.523975492498826,-0.520834931563955,-0.519281001841084,
-0.518159958519205,-0.516968510203523,-0.515388703432245,-0.511941772297602,
-0.445576812260463,-0.438678104798247,-0.432780132679777,-0.383078962686884,
-0.360182081410214,-0.358109641621491,-0.357270043848103,-0.356652838783945,
-0.356029613478544,-0.355146197413434,-0.353194309542699,-0.350568145909762,
-0.344131841931772,-0.323424997182118,-0.305118591753579,-0.235147781033413,
-0.224359710638494,-0.218294647550135,-0.200626646264396,-0.19765187304851,
-0.196143849355795,-0.19496236885282,-0.1936530005663,-0.191503594643511,
-0.183916981307173,-0.158316629533491,-0.0683540926283739,-0.0637523387064982,
-0.0375946310101134,-0.035458969575932,-0.0346083804467672,-0.0339882948652247,
-0.0333631832269334,-0.0327082914623046,-0.0318421738770758,-0.0304587988341439,
-0.000956382887790925),.UNSPECIFIED.);
#853=B_SPLINE_CURVE_WITH_KNOTS('',3,(#56095,#56096,#56097,#56098,#56099,
#56100,#56101,#56102,#56103,#56104,#56105,#56106,#56107,#56108,#56109,#56110,
#56111,#56112,#56113,#56114,#56115,#56116,#56117,#56118,#56119,#56120,#56121,
#56122,#56123,#56124,#56125,#56126,#56127,#56128,#56129,#56130,#56131,#56132,
#56133,#56134,#56135,#56136,#56137,#56138,#56139,#56140,#56141,#56142,#56143,
#56144,#56145,#56146,#56147,#56148,#56149,#56150,#56151,#56152,#56153,#56154,
#56155,#56156,#56157,#56158,#56159,#56160,#56161,#56162,#56163,#56164,#56165,
#56166,#56167,#56168,#56169,#56170,#56171,#56172,#56173,#56174,#56175,#56176,
#56177,#56178,#56179,#56180,#56181,#56182,#56183,#56184,#56185,#56186,#56187,
#56188,#56189,#56190,#56191,#56192,#56193,#56194,#56195,#56196,#56197,#56198,
#56199,#56200,#56201,#56202,#56203,#56204,#56205,#56206,#56207,#56208,#56209,
#56210,#56211,#56212,#56213,#56214,#56215,#56216,#56217,#56218,#56219,#56220,
#56221,#56222,#56223,#56224,#56225,#56226,#56227,#56228,#56229,#56230,#56231,
#56232,#56233,#56234,#56235,#56236,#56237,#56238,#56239,#56240,#56241,#56242,
#56243,#56244,#56245,#56246,#56247,#56248,#56249,#56250,#56251,#56252,#56253,
#56254,#56255,#56256,#56257,#56258,#56259,#56260,#56261,#56262,#56263,#56264,
#56265,#56266,#56267,#56268,#56269,#56270,#56271,#56272,#56273,#56274,#56275,
#56276,#56277,#56278,#56279,#56280,#56281,#56282,#56283,#56284,#56285,#56286,
#56287,#56288,#56289,#56290,#56291,#56292,#56293,#56294,#56295,#56296,#56297,
#56298,#56299,#56300,#56301,#56302,#56303,#56304,#56305,#56306,#56307,#56308,
#56309,#56310,#56311,#56312,#56313,#56314,#56315,#56316,#56317,#56318,#56319,
#56320,#56321,#56322,#56323,#56324,#56325,#56326,#56327,#56328,#56329,#56330,
#56331,#56332,#56333,#56334,#56335,#56336,#56337,#56338,#56339,#56340,#56341,
#56342,#56343,#56344,#56345,#56346,#56347,#56348,#56349,#56350,#56351,#56352,
#56353,#56354,#56355,#56356,#56357,#56358,#56359,#56360,#56361,#56362,#56363,
#56364,#56365,#56366,#56367,#56368,#56369,#56370,#56371,#56372,#56373,#56374,
#56375,#56376,#56377,#56378,#56379,#56380,#56381,#56382,#56383,#56384,#56385,
#56386,#56387,#56388,#56389,#56390,#56391,#56392,#56393,#56394,#56395,#56396,
#56397,#56398,#56399,#56400,#56401,#56402,#56403,#56404,#56405,#56406,#56407,
#56408,#56409,#56410,#56411,#56412,#56413,#56414,#56415,#56416,#56417,#56418,
#56419,#56420,#56421,#56422,#56423,#56424,#56425,#56426,#56427,#56428,#56429,
#56430,#56431,#56432,#56433,#56434,#56435,#56436,#56437,#56438,#56439,#56440,
#56441,#56442,#56443,#56444,#56445,#56446,#56447,#56448,#56449,#56450,#56451,
#56452,#56453,#56454,#56455,#56456,#56457,#56458,#56459,#56460,#56461,#56462,
#56463,#56464,#56465,#56466,#56467,#56468,#56469,#56470,#56471,#56472,#56473,
#56474,#56475,#56476,#56477,#56478,#56479,#56480,#56481,#56482,#56483,#56484,
#56485,#56486,#56487,#56488,#56489,#56490,#56491,#56492,#56493,#56494,#56495,
#56496,#56497,#56498,#56499,#56500,#56501,#56502,#56503,#56504,#56505,#56506,
#56507,#56508,#56509,#56510,#56511,#56512,#56513,#56514,#56515,#56516,#56517,
#56518,#56519,#56520,#56521,#56522,#56523,#56524,#56525,#56526,#56527,#56528,
#56529,#56530,#56531,#56532,#56533,#56534,#56535,#56536,#56537,#56538,#56539,
#56540,#56541,#56542,#56543,#56544,#56545,#56546,#56547,#56548,#56549,#56550,
#56551,#56552,#56553,#56554,#56555,#56556,#56557,#56558,#56559,#56560,#56561,
#56562,#56563,#56564,#56565,#56566,#56567,#56568,#56569,#56570,#56571,#56572,
#56573,#56574,#56575,#56576,#56577,#56578,#56579,#56580,#56581,#56582,#56583,
#56584,#56585,#56586,#56587,#56588,#56589,#56590,#56591,#56592,#56593,#56594,
#56595,#56596,#56597,#56598,#56599,#56600,#56601,#56602,#56603,#56604,#56605,
#56606,#56607,#56608,#56609,#56610,#56611,#56612,#56613,#56614,#56615,#56616,
#56617,#56618,#56619,#56620,#56621,#56622,#56623,#56624,#56625,#56626,#56627,
#56628),.UNSPECIFIED.,.F.,.F.,(4,2,2,2,2,2,2,2,2,2,2,2,2,2,2,2,2,2,2,2,
2,2,2,2,2,2,2,2,2,2,2,2,2,2,2,2,2,2,2,2,2,2,2,2,2,2,2,2,2,2,2,2,2,2,2,2,
2,2,2,2,2,2,2,2,2,2,2,2,2,2,2,2,2,2,2,2,2,2,2,2,2,2,2,2,2,2,2,2,2,2,2,2,
2,2,2,2,2,2,2,2,2,2,2,2,2,2,2,2,2,2,2,2,2,2,2,2,2,2,2,2,2,2,2,2,2,2,2,2,
2,2,2,2,2,2,2,2,2,2,2,2,2,2,2,2,2,2,2,2,2,2,2,2,2,2,2,2,2,2,2,2,2,2,2,2,
2,2,2,2,2,2,2,2,2,2,2,2,2,2,2,2,2,2,2,2,2,2,2,2,2,2,2,2,2,2,2,2,2,2,2,2,
2,2,2,2,2,2,2,2,2,2,2,2,2,2,2,2,2,2,2,2,2,2,2,2,2,2,2,2,2,2,2,2,2,2,2,2,
2,2,2,2,2,2,2,2,2,2,2,2,2,2,2,2,2,2,2,2,2,2,2,2,2,2,2,2,2,2,4),(-4.06120447951431,
-4.01260665686555,-3.93887131362229,-3.93540604210493,-3.93382296588376,
-3.93263117358277,-3.93151136039023,-3.92996160091044,-3.92683714135233,
-3.89750678502528,-3.81787782242457,-3.80243128736636,-3.78338932151216,
-3.77422208004284,-3.77270043372142,-3.77204684702149,-3.77142105707436,
-3.77079986614458,-3.76994466312798,-3.76823396344177,-3.75323657077867,
-3.75227926538786,-3.74668664122066,-3.70696599683707,-3.67376842843106,
-3.62199772577786,-3.61415562910771,-3.61198087711131,-3.6106659202612,
-3.60948572874616,-3.60798800366273,-3.60506073607164,-3.58829361111022,
-3.5824149941432,-3.51058703376588,-3.47819074083318,-3.46299987916976,
-3.45553954999855,-3.45261299812562,-3.45114140243028,-3.44991917302459,
-3.44919039258122,-3.44853281544024,-3.44769729173634,-3.44600338661094,
-3.43590700968378,-3.36412796441999,-3.29364695386967,-3.2901886820578,
-3.28860686756102,-3.28741522477499,-3.28629496536932,-3.28443776215458,
-3.2796859589146,-3.20060132336445,-3.15075079035032,-3.13607631970201,
-3.13128797754732,-3.12917558798084,-3.12753701072295,-3.12675653454788,
-3.12610832434285,-3.12547223796761,-3.12437420245592,-3.12132283834259,
-3.06713031505546,-3.06240608985419,-3.01437324688398,-2.97080273742987,
-2.96749480807397,-2.96594148108525,-2.96475408993239,-2.96362496256596,
-2.96204057941722,-2.95877695904907,-2.92373859070982,-2.84177486273639,
-2.81029361137534,-2.80732995225721,-2.80584472516268,-2.80493616102164,
-2.80410774773889,-2.80346128976041,-2.8028196407536,-2.80169395057468,
-2.79812208241094,-2.74074619701058,-2.69098903370517,-2.67110805544016,
-2.64764931588654,-2.64467358885685,-2.64318591269066,-2.64211741402926,
-2.640987539141,-2.6394006268126,-2.63612701265303,-2.60064322121399,-2.51909405544329,
-2.48764379548256,-2.48315909396866,-2.48193598520474,-2.48120133747992,
-2.48054187057482,-2.47969043388984,-2.47791702511518,-2.46615349489035,
-2.38205408096663,-2.33125874606431,-2.32349896453561,-2.32133213217007,
-2.32001882616276,-2.31883809833027,-2.31733693608956,-2.31439430635057,
-2.29733950700057,-2.29363051800344,-2.27529568818749,-2.19943762137914,
-2.172724448719,-2.16113677390182,-2.15951860234089,-2.15869842186024,-2.15804213204117,
-2.15728786505847,-2.15601017984342,-2.15140212121821,-2.05541532624224,
-2.03139406804066,-2.0028918646598,-1.99944517987408,-1.99788250010006,
-1.99668942894802,-1.99541790584765,-1.99343827550916,-1.98736788184511,
-1.89430345183146,-1.85084311801432,-1.8385861340834,-1.83696953526359,
-1.83613822857712,-1.83552309026127,-1.83484872564573,-1.83390484445389,
-1.83162342259734,-1.82846128305234,-1.79295204685174,-1.69815887357967,
-1.69580455480164,-1.67928829809879,-1.676633090897,-1.67506306522859,-1.67386876695179,
-1.67260015218366,-1.6706336640036,-1.66466853844555,-1.63180185792013,
-1.54003786222529,-1.536745482764,-1.53220038220944,-1.53173192821666,-1.53134270883874,
-1.52839018459887,-1.51579191155756,-1.51416286966213,-1.51332834613226,
-1.51271238266444,-1.5120387287282,-1.51109869415273,-1.50884016515445,
-1.50571800939087,-1.47106684709087,-1.40868175071105,-1.3860678051899,
-1.3573639958444,-1.35391074054749,-1.35234671730259,-1.35115329390594,
-1.34990792850022,-1.34799704106151,-1.34577492326821,-1.34165223899833,
-1.30655363753438,-1.23650156783843,-1.19440426308996,-1.19175888947053,
-1.19082803736432,-1.19018618886753,-1.18959257696181,-1.1887744737123,
-1.18716659005905,-1.17589180189729,-1.14645093040212,-1.05382101032975,
-1.03408129129811,-1.03096714434445,-1.02945156299714,-1.02826908018954,
-1.02716723730698,-1.02527107053875,-1.01981028025,-0.977114693117432,-0.926062068477467,
-0.882444024580411,-0.87038321409291,-0.868596883765736,-0.86775206170295,
-0.86709164283985,-0.866361096031581,-0.865156253922068,-0.86085758448151,
-0.831641875039946,-0.751344132820681,-0.750926753098481,-0.746984466294774,
-0.712196411366071,-0.708623433978229,-0.70715620423306,-0.706057308189376,
-0.704849946483502,-0.703211604329819,-0.699417452192986,-0.694260697959506,
-0.6813601458361,-0.661529662386007,-0.622040845859146,-0.589860823682174,
-0.548610061946015,-0.546293173491164,-0.545412391612473,-0.544784350831595,
-0.544119213380871,-0.543227554244988,-0.54124257409324,-0.493928781643987,
-0.437350207339252,-0.418815322744822,-0.389420111347358,-0.386293389671841,
-0.384742898303089,-0.383622741175249,-0.382430754638513,-0.381263102836175,
-0.378573637781362,-0.362942223505265,-0.351675082976487,-0.31576092867744,
-0.228857596800781,-0.224267620798758,-0.222991796692276,-0.222237937732807,
-0.221581558224078,-0.220760693292927,-0.219139338763125,-0.207455658227395,
-0.180828827667497,-0.122231133032375,-0.115094672208138,-0.0961741127566374,
-0.0667481036950851,-0.0636202284095314,-0.0620693413285802,-0.0609489808032809,
-0.0597568544353694,-0.0585890903058442,-0.0570568356257562,-0.0546319021202795,
-0.000956654129082594),.UNSPECIFIED.);
#854=B_SPLINE_CURVE_WITH_KNOTS('',3,(#56630,#56631,#56632,#56633,#56634,
#56635,#56636,#56637,#56638,#56639),.UNSPECIFIED.,.F.,.F.,(4,1,1,1,1,1,
1,4),(59.6902669190053,60.0055486427859,61.0043410465539,62.0031334503219,
63.0019258540899,64.0007182578579,64.9995106616259,65.9734422249333),
 .UNSPECIFIED.);
#855=B_SPLINE_CURVE_WITH_KNOTS('',3,(#56641,#56642,#56643,#56644,#56645,
#56646,#56647,#56648,#56649,#56650,#56651,#56652,#56653,#56654,#56655,#56656,
#56657,#56658,#56659,#56660,#56661,#56662,#56663,#56664,#56665,#56666,#56667,
#56668,#56669,#56670,#56671,#56672,#56673,#56674,#56675,#56676,#56677,#56678,
#56679,#56680,#56681,#56682,#56683,#56684,#56685,#56686,#56687,#56688,#56689,
#56690,#56691,#56692,#56693,#56694,#56695,#56696,#56697,#56698,#56699,#56700,
#56701,#56702,#56703,#56704,#56705,#56706,#56707,#56708,#56709,#56710,#56711,
#56712,#56713,#56714,#56715,#56716,#56717,#56718,#56719,#56720,#56721,#56722,
#56723,#56724,#56725,#56726,#56727,#56728,#56729,#56730,#56731,#56732,#56733,
#56734,#56735,#56736,#56737,#56738,#56739,#56740,#56741,#56742,#56743,#56744,
#56745,#56746,#56747,#56748,#56749,#56750,#56751,#56752,#56753,#56754,#56755,
#56756,#56757,#56758),.UNSPECIFIED.,.F.,.F.,(4,3,3,3,3,3,3,3,3,3,3,3,3,
3,3,3,3,3,3,3,3,3,3,3,3,3,3,3,3,3,3,3,3,3,3,3,3,3,3,4),(65.9734457253865,
65.9983030653939,66.1637658780536,66.3289121646202,66.4959579907556,66.6610242971856,
66.8290598831738,66.997095469162,67.1625582818218,67.3277045683883,67.4947503945237,
67.6598167009538,67.8278522869419,67.99588787293,68.1613506855898,68.3264969721563,
68.4935427982917,68.6586091047218,68.8266446907099,68.994680276698,69.1601430893578,
69.3252893759243,69.4923352020597,69.6574015084897,69.8254370944779,69.993472680466,
70.1589354931258,70.3240817796923,70.4911276058277,70.6561939122578,70.8242294982459,
70.992265084234,71.1577278968938,71.3228741834603,71.4899200095957,71.6549863160257,
71.8230219020139,71.991057488002,72.200388695361,72.2566310324091),
 .UNSPECIFIED.);
#856=B_SPLINE_CURVE_WITH_KNOTS('',3,(#56760,#56761,#56762,#56763,#56764,
#56765,#56766,#56767,#56768,#56769,#56770,#56771,#56772,#56773,#56774,#56775,
#56776,#56777,#56778,#56779,#56780,#56781,#56782,#56783,#56784,#56785,#56786,
#56787,#56788,#56789,#56790,#56791,#56792,#56793,#56794,#56795,#56796,#56797,
#56798,#56799,#56800,#56801,#56802,#56803,#56804,#56805,#56806,#56807,#56808,
#56809,#56810,#56811,#56812,#56813,#56814,#56815,#56816,#56817,#56818,#56819,
#56820,#56821,#56822,#56823,#56824,#56825,#56826,#56827,#56828,#56829,#56830,
#56831,#56832,#56833,#56834,#56835,#56836,#56837,#56838,#56839,#56840,#56841,
#56842,#56843,#56844,#56845,#56846,#56847,#56848,#56849,#56850,#56851,#56852,
#56853,#56854,#56855,#56856,#56857,#56858,#56859,#56860,#56861,#56862,#56863,
#56864,#56865,#56866,#56867,#56868,#56869,#56870,#56871,#56872,#56873,#56874,
#56875,#56876,#56877,#56878,#56879,#56880,#56881,#56882,#56883,#56884,#56885,
#56886,#56887,#56888,#56889,#56890,#56891,#56892,#56893,#56894,#56895,#56896,
#56897,#56898,#56899,#56900,#56901,#56902,#56903,#56904,#56905,#56906,#56907,
#56908,#56909,#56910,#56911,#56912,#56913,#56914,#56915,#56916,#56917,#56918,
#56919,#56920,#56921,#56922,#56923,#56924,#56925,#56926,#56927,#56928,#56929,
#56930,#56931,#56932,#56933,#56934,#56935,#56936,#56937,#56938,#56939,#56940,
#56941,#56942,#56943,#56944,#56945,#56946,#56947,#56948,#56949,#56950,#56951,
#56952,#56953,#56954,#56955,#56956,#56957,#56958,#56959,#56960,#56961,#56962,
#56963,#56964,#56965,#56966,#56967,#56968,#56969,#56970,#56971,#56972,#56973,
#56974,#56975,#56976,#56977,#56978,#56979,#56980,#56981,#56982,#56983,#56984,
#56985,#56986,#56987,#56988,#56989,#56990,#56991,#56992,#56993,#56994,#56995,
#56996,#56997,#56998,#56999,#57000,#57001,#57002,#57003,#57004,#57005,#57006,
#57007,#57008,#57009,#57010,#57011,#57012,#57013,#57014,#57015,#57016,#57017,
#57018,#57019,#57020,#57021,#57022,#57023,#57024,#57025,#57026,#57027,#57028,
#57029,#57030,#57031,#57032,#57033,#57034,#57035,#57036,#57037,#57038,#57039,
#57040,#57041,#57042,#57043,#57044,#57045,#57046,#57047,#57048,#57049,#57050,
#57051,#57052,#57053,#57054,#57055,#57056,#57057,#57058,#57059,#57060,#57061,
#57062,#57063,#57064,#57065,#57066,#57067,#57068,#57069,#57070,#57071,#57072,
#57073,#57074,#57075,#57076,#57077,#57078,#57079,#57080,#57081,#57082,#57083,
#57084,#57085,#57086,#57087,#57088,#57089,#57090,#57091,#57092,#57093,#57094,
#57095,#57096,#57097,#57098,#57099,#57100,#57101,#57102,#57103,#57104,#57105,
#57106,#57107,#57108,#57109,#57110,#57111,#57112,#57113,#57114,#57115,#57116,
#57117,#57118,#57119,#57120,#57121,#57122,#57123,#57124,#57125,#57126,#57127,
#57128,#57129,#57130,#57131,#57132,#57133,#57134,#57135,#57136,#57137,#57138,
#57139,#57140,#57141,#57142,#57143,#57144,#57145,#57146,#57147,#57148,#57149,
#57150,#57151,#57152,#57153,#57154,#57155,#57156,#57157,#57158,#57159,#57160,
#57161,#57162,#57163,#57164,#57165,#57166,#57167,#57168,#57169,#57170,#57171,
#57172,#57173,#57174,#57175,#57176,#57177,#57178,#57179,#57180,#57181,#57182,
#57183,#57184,#57185,#57186,#57187,#57188,#57189,#57190,#57191,#57192,#57193,
#57194,#57195,#57196,#57197,#57198,#57199,#57200,#57201,#57202,#57203,#57204,
#57205,#57206,#57207,#57208,#57209,#57210,#57211,#57212,#57213,#57214,#57215,
#57216,#57217,#57218,#57219,#57220,#57221,#57222,#57223,#57224,#57225,#57226,
#57227,#57228,#57229,#57230,#57231,#57232,#57233,#57234,#57235,#57236,#57237,
#57238,#57239,#57240,#57241,#57242,#57243,#57244,#57245,#57246,#57247,#57248,
#57249,#57250,#57251,#57252,#57253,#57254,#57255,#57256,#57257,#57258,#57259,
#57260,#57261,#57262,#57263,#57264,#57265,#57266,#57267,#57268,#57269,#57270,
#57271,#57272,#57273,#57274,#57275,#57276,#57277,#57278,#57279,#57280,#57281,
#57282,#57283,#57284,#57285,#57286,#57287,#57288,#57289,#57290,#57291,#57292,
#57293,#57294,#57295,#57296,#57297,#57298,#57299,#57300,#57301,#57302,#57303),
 .UNSPECIFIED.,.F.,.F.,(4,2,2,2,2,2,2,2,2,2,2,2,2,2,2,2,2,2,2,2,2,2,2,2,
2,2,2,2,2,2,2,2,2,2,2,2,2,2,2,2,2,2,2,2,2,2,2,2,2,2,2,2,2,2,2,2,2,2,2,2,
2,2,2,2,2,2,2,2,2,2,2,2,2,2,2,2,2,2,2,2,2,2,2,2,2,2,2,2,2,2,2,2,2,2,2,2,
2,2,2,2,2,2,2,2,2,2,2,2,2,2,2,2,2,2,2,2,2,2,2,2,2,2,2,2,2,2,2,2,2,2,2,2,
2,2,2,2,2,2,2,2,2,2,2,2,2,2,2,2,2,2,2,2,2,2,2,2,2,2,2,2,2,2,2,2,2,2,2,2,
2,2,2,2,2,2,2,2,2,2,2,2,2,2,2,2,2,2,2,2,2,2,2,2,2,2,2,2,2,2,2,2,2,2,2,2,
2,2,2,2,2,2,2,2,2,2,2,2,2,2,2,2,2,2,2,2,2,2,2,2,2,2,2,2,2,2,2,2,2,2,2,2,
2,2,2,2,2,2,2,2,2,2,2,2,2,2,2,2,2,2,2,2,2,2,2,2,2,2,2,2,2,2,2,4),(-4.06072099708927,
-3.99335883250795,-3.98986432731804,-3.98789113213452,-3.98654908115576,
-3.98524506280465,-3.98406271280404,-3.98254566511379,-3.97942270971339,
-3.95947578699461,-3.95391800962889,-3.91051859611513,-3.89505923928516,
-3.88056463606732,-3.84577748398674,-3.83314679121407,-3.82617200163564,
-3.82515357337312,-3.82423535193232,-3.82356587981738,-3.8229452778733,
-3.82209211660086,-3.82038927715486,-3.80563200668368,-3.74626137690391,
-3.7218834894641,-3.69245200208607,-3.67599833664372,-3.66982528611993,
-3.66544295850923,-3.66410013502624,-3.66279558392796,-3.66161338479511,
-3.66009741314531,-3.65697979802827,-3.63714848328601,-3.63163495430244,
-3.62471755983852,-3.6114546325119,-3.58526836572976,-3.51307499914043,
-3.50386602177083,-3.50233033768937,-3.50152749444441,-3.50093581596219,
-3.50028688677812,-3.4991245490177,-3.49561052448371,-3.43663258663599,
-3.39932239147558,-3.36653982717003,-3.3456908627346,-3.3424351978904,-3.3412026907319,
-3.33997251023921,-3.33876864411134,-3.33731931251696,-3.3337064342559,
-3.2992001267201,-3.2827255089068,-3.22500814929884,-3.20364408112494,-3.1823684717428,
-3.180194822064,-3.1792586535416,-3.17858588274869,-3.17796935610548,-3.17713210630159,
-3.17549192901851,-3.16258191564604,-3.16233608692326,-3.15930888062328,
-3.15842195058216,-3.1527272898174,-3.13846155992828,-3.08939200134123,
-3.05170411821848,-3.03236852671488,-3.02177486032964,-3.01938833865428,
-3.01824865641427,-3.01718031326076,-3.01605073694866,-3.01446446263209,
-3.01119287165909,-2.97577992317334,-2.97193228414542,-2.89135490638498,
-2.86248329602656,-2.85827740918681,-2.85704328117893,-2.85630625014124,
-2.8556474395333,-2.85480064370919,-2.85305029026807,-2.84179356387293,
-2.83822496429671,-2.83404092847237,-2.82944305127106,-2.81746956660634,
-2.74374768937198,-2.70503105063669,-2.70066263319988,-2.69734431409533,
-2.69579478259173,-2.69460320964923,-2.69348274980362,-2.6919307419077,
-2.68794289329454,-2.61977813425535,-2.57574433637417,-2.54047889482085,
-2.53570313449774,-2.53445303813546,-2.5337124404429,-2.53305432837918,
-2.53221365111005,-2.53049402119961,-2.51988415264725,-2.42252893770577,
-2.3783820321245,-2.37475266874645,-2.37313934502629,-2.37194262644947,
-2.37083100092052,-2.36931252291292,-2.36552214855692,-2.31731812633353,
-2.29253682582188,-2.24659114260684,-2.21727369035603,-2.21296733247813,
-2.21176195853327,-2.21103143410059,-2.21037126755577,-2.20952707959449,
-2.20774323554686,-2.19573123724008,-2.19427053656808,-2.19384302215281,
-2.15501915411242,-2.06164504275828,-2.05344270724838,-2.0512336373799,
-2.04991117758355,-2.04873263205055,-2.04724828292767,-2.0449315707945,
-2.0339625014908,-2.03209838231703,-2.03113092655583,-2.00381465955611,
-1.89716199242147,-1.89064747166278,-1.8893268086618,-1.88849130111971,
-1.88783371837105,-1.88708991301324,-1.88582552530768,-1.88088945973974,
-1.85755214598733,-1.81083269690741,-1.76235190115433,-1.7328539702797,
-1.72972467606081,-1.72817360178935,-1.72705334746834,-1.72586155826572,
-1.72427929289465,-1.72081901356831,-1.64966873624368,-1.57884786197904,
-1.56841732286664,-1.56670653881582,-1.56586757035643,-1.56520957304588,
-1.56446778710064,-1.56321263209929,-1.55838175820877,-1.52234578556094,
-1.43853473970214,-1.41008171286273,-1.40663665951705,-1.40507432079703,
-1.40388134562564,-1.40260976573028,-1.40062971990445,-1.39455555294364,
-1.3014081309899,-1.24789902350362,-1.24461783379485,-1.24348722478367,
-1.24284455802936,-1.2422512457827,-1.24145159462075,-1.23991044877817,
-1.23795369381672,-1.17231776782399,-1.10614949839837,-1.08677397701938,
-1.08367686565386,-1.08216470517731,-1.0809826726965,-1.07967544281879,
-1.07753579769192,-1.07004566605452,-1.02227931115542,-0.941977310151469,
-0.938514206695889,-0.923226949943139,-0.921317038015533,-0.920448756366965,
-0.919784845110124,-0.919170988122657,-0.918136522100213,-0.91525467365338,
-0.910969376460969,-0.885221855109396,-0.838361221338347,-0.791575463267311,
-0.764578602480926,-0.761519157616712,-0.759985496037017,-0.758869665614673,
-0.757674936584945,-0.75607560739648,-0.752524570562522,-0.703291855299055,
-0.634137888300082,-0.622056766666631,-0.614079229067929,-0.613298404318261,
-0.600446788120734,-0.59880824768054,-0.597971258372075,-0.5973546429039,
-0.596681484532904,-0.595763127177067,-0.593757364493382,-0.572264728431434,
-0.533756983152834,-0.464307329652044,-0.441649550359683,-0.43873280338078,
-0.4372355455115,-0.436129058403392,-0.434927851403497,-0.433290669199081,
-0.42953076741507,-0.390277941080532,-0.353032736615377,-0.317602269526929,
-0.287824194276457,-0.277625251695785,-0.275925833882827,-0.275089084212629,
-0.274431247352916,-0.273814825758799,-0.273083750482211,-0.270851228684327,
-0.241438404009671,-0.221724876065615,-0.146254067552353,-0.119252101270172,
-0.116192588404928,-0.114658937128221,-0.113543135266999,-0.112348456630963,
-0.110749229159927,-0.107198558774455,-0.0587031010197374,-0.000958174941626183),
 .UNSPECIFIED.);
#857=B_SPLINE_CURVE_WITH_KNOTS('',3,(#57305,#57306,#57307,#57308,#57309,
#57310,#57311,#57312,#57313,#57314,#57315,#57316,#57317,#57318,#57319,#57320,
#57321,#57322,#57323,#57324,#57325,#57326,#57327,#57328,#57329,#57330,#57331,
#57332,#57333,#57334,#57335,#57336,#57337,#57338,#57339,#57340,#57341,#57342,
#57343,#57344,#57345,#57346,#57347,#57348,#57349,#57350,#57351,#57352,#57353,
#57354,#57355,#57356,#57357,#57358,#57359,#57360,#57361,#57362,#57363,#57364,
#57365,#57366,#57367,#57368,#57369,#57370,#57371,#57372,#57373,#57374,#57375,
#57376,#57377,#57378,#57379,#57380,#57381,#57382,#57383,#57384,#57385,#57386,
#57387,#57388,#57389,#57390,#57391,#57392,#57393,#57394,#57395,#57396,#57397,
#57398,#57399,#57400,#57401,#57402,#57403,#57404,#57405,#57406,#57407,#57408,
#57409,#57410,#57411,#57412,#57413,#57414,#57415,#57416,#57417,#57418,#57419,
#57420,#57421,#57422,#57423,#57424,#57425,#57426,#57427,#57428,#57429,#57430,
#57431,#57432,#57433,#57434,#57435,#57436,#57437,#57438,#57439,#57440,#57441,
#57442,#57443,#57444,#57445,#57446,#57447,#57448,#57449,#57450,#57451,#57452,
#57453,#57454,#57455,#57456,#57457,#57458,#57459,#57460,#57461,#57462,#57463,
#57464,#57465,#57466,#57467,#57468,#57469,#57470,#57471,#57472,#57473,#57474,
#57475,#57476,#57477,#57478,#57479,#57480,#57481,#57482,#57483,#57484,#57485,
#57486,#57487,#57488,#57489,#57490,#57491,#57492,#57493,#57494,#57495,#57496,
#57497,#57498,#57499,#57500,#57501,#57502,#57503,#57504,#57505,#57506,#57507,
#57508,#57509,#57510,#57511,#57512,#57513,#57514,#57515,#57516,#57517,#57518,
#57519,#57520,#57521,#57522,#57523,#57524,#57525,#57526,#57527,#57528,#57529,
#57530,#57531,#57532,#57533,#57534,#57535,#57536,#57537,#57538,#57539,#57540,
#57541,#57542,#57543,#57544,#57545,#57546,#57547,#57548,#57549,#57550,#57551,
#57552,#57553,#57554,#57555,#57556,#57557,#57558,#57559,#57560,#57561,#57562,
#57563,#57564,#57565,#57566,#57567,#57568,#57569,#57570,#57571,#57572,#57573,
#57574,#57575,#57576,#57577,#57578,#57579,#57580,#57581,#57582,#57583,#57584,
#57585,#57586,#57587,#57588,#57589,#57590,#57591,#57592,#57593,#57594,#57595,
#57596,#57597,#57598,#57599,#57600,#57601,#57602,#57603,#57604,#57605,#57606,
#57607,#57608,#57609,#57610,#57611,#57612,#57613,#57614,#57615,#57616,#57617,
#57618,#57619,#57620,#57621,#57622,#57623,#57624,#57625,#57626,#57627,#57628,
#57629,#57630,#57631,#57632,#57633,#57634,#57635,#57636,#57637,#57638,#57639,
#57640,#57641,#57642,#57643,#57644,#57645,#57646,#57647,#57648,#57649,#57650,
#57651,#57652,#57653,#57654,#57655,#57656,#57657,#57658,#57659,#57660,#57661,
#57662,#57663,#57664,#57665,#57666,#57667,#57668,#57669,#57670,#57671,#57672,
#57673,#57674,#57675,#57676,#57677,#57678,#57679,#57680,#57681,#57682,#57683,
#57684,#57685,#57686,#57687,#57688,#57689,#57690,#57691,#57692,#57693,#57694,
#57695,#57696,#57697,#57698,#57699,#57700,#57701,#57702,#57703,#57704,#57705,
#57706,#57707,#57708,#57709,#57710,#57711,#57712,#57713,#57714,#57715,#57716,
#57717,#57718,#57719,#57720,#57721,#57722,#57723,#57724,#57725,#57726,#57727,
#57728,#57729,#57730,#57731,#57732,#57733,#57734,#57735,#57736,#57737,#57738,
#57739,#57740,#57741,#57742,#57743,#57744,#57745,#57746,#57747,#57748,#57749,
#57750,#57751,#57752,#57753,#57754,#57755,#57756,#57757,#57758,#57759,#57760,
#57761,#57762,#57763,#57764,#57765,#57766,#57767,#57768,#57769,#57770,#57771,
#57772,#57773,#57774,#57775,#57776,#57777,#57778,#57779,#57780,#57781,#57782,
#57783,#57784,#57785,#57786,#57787,#57788,#57789,#57790,#57791,#57792,#57793,
#57794,#57795,#57796,#57797,#57798,#57799,#57800,#57801,#57802,#57803,#57804,
#57805,#57806,#57807,#57808,#57809,#57810,#57811,#57812,#57813,#57814,#57815,
#57816,#57817,#57818,#57819,#57820,#57821,#57822,#57823,#57824,#57825,#57826,
#57827,#57828,#57829,#57830,#57831,#57832,#57833,#57834,#57835,#57836,#57837,
#57838,#57839,#57840,#57841,#57842,#57843,#57844,#57845,#57846,#57847,#57848,
#57849,#57850,#57851,#57852,#57853,#57854,#57855,#57856,#57857,#57858,#57859,
#57860,#57861,#57862,#57863,#57864,#57865,#57866,#57867,#57868,#57869,#57870,
#57871,#57872,#57873,#57874),.UNSPECIFIED.,.F.,.F.,(4,2,2,2,2,2,2,2,2,2,
2,2,2,2,2,2,2,2,2,2,2,2,2,2,2,2,2,2,2,2,2,2,2,2,2,2,2,2,2,2,2,2,2,2,2,2,
2,2,2,2,2,2,2,2,2,2,2,2,2,2,2,2,2,2,2,2,2,2,2,2,2,2,2,2,2,2,2,2,2,2,2,2,
2,2,2,2,2,2,2,2,2,2,2,2,2,2,2,2,2,2,2,2,2,2,2,2,2,2,2,2,2,2,2,2,2,2,2,2,
2,2,2,2,2,2,2,2,2,2,2,2,2,2,2,2,2,2,2,2,2,2,2,2,2,2,2,2,2,2,2,2,2,2,2,2,
2,2,2,2,2,2,2,2,2,2,2,2,2,2,2,2,2,2,2,2,2,2,2,2,2,2,2,2,2,2,2,2,2,2,2,2,
2,2,2,2,2,2,2,2,2,2,2,2,2,2,2,2,2,2,2,2,2,2,2,2,2,2,2,2,2,2,2,2,2,2,2,2,
2,2,2,2,2,2,2,2,2,2,2,2,2,2,2,2,2,2,2,2,2,2,2,2,2,2,2,2,2,2,2,2,2,2,2,2,
2,2,2,2,2,2,2,2,2,2,2,2,2,2,2,2,2,2,2,2,2,2,4),(-4.06035509702412,-4.0166517298775,
-4.01441449234829,-4.01320321613188,-4.01240935392366,-4.01177839014718,
-4.0111858386207,-4.01054102551551,-4.00959901378349,-4.00687614329751,
-3.96344012068408,-3.95513263774935,-3.94863346869362,-3.93572197765867,
-3.90829480679015,-3.86137867262917,-3.85396675872054,-3.85183550429672,
-3.85053035090128,-3.84934820007201,-3.847833116488,-3.84472024791505,-3.82499486328965,
-3.82346699629693,-3.74850398268308,-3.72815146569418,-3.70583639151684,
-3.69183241693507,-3.69015179062701,-3.68948116859182,-3.68880710987465,
-3.68819199372132,-3.68736035237359,-3.68574203743482,-3.6734309756206,
-3.67222603324444,-3.64471275551412,-3.5922979514002,-3.58458122203527,
-3.57475404198815,-3.53764502462112,-3.53121598294735,-3.52919321337834,
-3.52791224228308,-3.52672303600258,-3.52518347544333,-3.52263130483662,
-3.50803028184044,-3.50329310646057,-3.4361361105773,-3.39556471690477,
-3.38043522305897,-3.37293486249413,-3.36999684142157,-3.36786083453126,
-3.36694416536503,-3.36627148530115,-3.36565476527854,-3.36481685584832,
-3.3631742066735,-3.35019625601309,-3.34951295106431,-3.34902277559775,
-3.34171194001412,-3.32962865690209,-3.25180446507136,-3.23479466859309,
-3.21279733839221,-3.20812474648994,-3.2063374640299,-3.2051074860625,-3.20390341064808,
-3.20245333480698,-3.198836011597,-3.16414790006469,-3.15733380195568,-3.13225216005585,
-3.0813190479429,-3.05038336568593,-3.04744865076373,-3.04531489290246,
-3.04439845024177,-3.04372584797718,-3.04310911212548,-3.0422710559909,
-3.04062774696895,-3.02762913093425,-3.02747655949292,-3.02421289170875,
-2.93810625912863,-2.88864527961295,-2.88508082159158,-2.88347941107379,
-2.88228472433674,-2.88117008518121,-2.87963985990916,-2.87578052407747,
-2.82118886006901,-2.75040744906852,-2.72693675992932,-2.72443191548218,
-2.72311777253637,-2.72200460026686,-2.7213002316465,-2.72063656833257,
-2.71976872169285,-2.71786020901982,-2.7026006608473,-2.70196056742692,
-2.69958336163531,-2.69266171760252,-2.60185446692245,-2.56921604551337,
-2.56327651588692,-2.56131359441477,-2.56004600226084,-2.55885174992778,
-2.55728045008014,-2.55462011011217,-2.53799412256239,-2.44262326924299,
-2.40222025441417,-2.39997775357103,-2.39904059871654,-2.39836762626695,
-2.39775128309192,-2.39691481027123,-2.3952777203941,-2.38245512716111,
-2.37972931604978,-2.37938816853435,-2.37857158427384,-2.37538078043006,
-2.35711854414599,-2.31814068582426,-2.27463360217371,-2.24878665111095,
-2.24107033546701,-2.23890805706653,-2.23759590711746,-2.2364151844756,
-2.2349126127234,-2.23196276270387,-2.21476624792574,-2.20939448666436,
-2.13392782457848,-2.07949095587983,-2.07736505156232,-2.07644803888323,
-2.0757786753869,-2.07515760031897,-2.07430294230389,-2.07259451754829,
-2.05767098581951,-2.03154886797263,-1.93614392775167,-1.9197190911341,
-1.9170689067251,-1.91550048566944,-1.91430661639961,-1.91303769610962,
-1.91106918151433,-1.90508626731136,-1.87205682183273,-1.77964714656913,
-1.77495063079604,-1.77255254756129,-1.76933163515013,-1.75628317340285,
-1.75447920012865,-1.75361827412503,-1.75295559992204,-1.75223333896791,
-1.75106523868195,-1.74711857620357,-1.72182763167177,-1.6738899684977,
-1.59973192467694,-1.5950120821501,-1.59334523239723,-1.59219347735758,
-1.59113167848084,-1.58969525509982,-1.58696608281538,-1.570652055203,-1.53640182220655,
-1.44435135822236,-1.43342768418569,-1.43169272570572,-1.4308489015717,
-1.43019033883438,-1.42945138233257,-1.42820899750609,-1.42351932570883,
-1.38944364031986,-1.30983829910646,-1.27531095273964,-1.27169693654138,
-1.27024723482255,-1.26904309343857,-1.26783726527603,-1.2661028795937,
-1.26413351599843,-1.26064886122142,-1.23435704145997,-1.21025274677618,
-1.1145723884373,-1.1099200977961,-1.10863768251027,-1.10788225772218,-1.10722600480482,
-1.1064072159987,-1.10479606883131,-1.0934251569476,-1.06352934077086,-0.967697851666491,
-0.951413573628203,-0.948770166264878,-0.947203517049197,-0.946033568845979,
-0.944889420162937,-0.943084769295693,-0.941015624822096,-0.937281524752191,
-0.928932122532361,-0.904179144784289,-0.813229092305789,-0.806386242894336,
-0.804281506391321,-0.803229847509772,-0.788077388513619,-0.786171658095859,
-0.785304112533975,-0.78464027461973,-0.783920793555731,-0.782765650913222,
-0.778938672909169,-0.754919845777028,-0.702637641047084,-0.672052490261681,
-0.629972130168234,-0.626274618518567,-0.624771829041888,-0.623663897109187,
-0.622487666411461,-0.620999104013068,-0.619289460046474,-0.616440508327956,
-0.610648527030055,-0.595556253810271,-0.558732409586937,-0.482579963217482,
-0.478522044160389,-0.465289498241768,-0.463454652120675,-0.462600412727027,
-0.461938551423845,-0.461212638893719,-0.460028933877112,-0.455938237779528,
-0.429085467490673,-0.381173378458307,-0.355607585829613,-0.307417295202559,
-0.303625800914895,-0.30210666669628,-0.300994486561671,-0.299821039252192,
-0.298260289225738,-0.296527288122433,-0.293622078010773,-0.287674529661808,
-0.272031490896816,-0.252134646705724,-0.202282707677591,-0.144874251914233,
-0.141446793513763,-0.140295367026057,-0.139648407793025,-0.139055925684922,
-0.138248129782516,-0.136690136117058,-0.126777301712368,-0.104030397732436,
-0.000958019755019555),.UNSPECIFIED.);
#858=B_SPLINE_CURVE_WITH_KNOTS('',3,(#57876,#57877,#57878,#57879,#57880,
#57881,#57882,#57883,#57884,#57885,#57886,#57887,#57888,#57889,#57890,#57891,
#57892,#57893,#57894,#57895,#57896,#57897,#57898,#57899,#57900,#57901,#57902,
#57903,#57904,#57905,#57906,#57907,#57908,#57909,#57910,#57911,#57912,#57913,
#57914,#57915,#57916,#57917,#57918,#57919,#57920,#57921,#57922,#57923,#57924,
#57925,#57926,#57927,#57928,#57929,#57930,#57931,#57932,#57933,#57934,#57935,
#57936,#57937,#57938,#57939,#57940,#57941,#57942,#57943,#57944,#57945,#57946,
#57947,#57948,#57949,#57950,#57951,#57952,#57953,#57954,#57955,#57956,#57957,
#57958,#57959,#57960,#57961,#57962,#57963,#57964,#57965,#57966,#57967,#57968,
#57969,#57970,#57971,#57972,#57973,#57974,#57975,#57976,#57977,#57978,#57979,
#57980,#57981,#57982,#57983,#57984,#57985,#57986,#57987,#57988,#57989,#57990,
#57991,#57992,#57993,#57994,#57995,#57996,#57997,#57998,#57999,#58000,#58001,
#58002,#58003,#58004,#58005,#58006,#58007,#58008,#58009,#58010,#58011,#58012,
#58013,#58014,#58015,#58016,#58017,#58018,#58019,#58020,#58021,#58022,#58023,
#58024,#58025,#58026,#58027,#58028,#58029,#58030,#58031,#58032,#58033,#58034,
#58035,#58036,#58037,#58038,#58039,#58040,#58041,#58042,#58043,#58044,#58045,
#58046,#58047,#58048,#58049,#58050,#58051,#58052,#58053,#58054,#58055,#58056,
#58057,#58058,#58059,#58060,#58061,#58062,#58063,#58064,#58065,#58066,#58067,
#58068,#58069,#58070,#58071,#58072,#58073,#58074,#58075,#58076,#58077,#58078,
#58079,#58080,#58081,#58082,#58083,#58084,#58085,#58086,#58087,#58088,#58089,
#58090,#58091,#58092,#58093,#58094,#58095,#58096,#58097,#58098,#58099,#58100,
#58101,#58102,#58103,#58104,#58105,#58106,#58107,#58108,#58109,#58110,#58111,
#58112,#58113,#58114,#58115,#58116,#58117,#58118,#58119,#58120,#58121,#58122,
#58123,#58124,#58125,#58126,#58127,#58128,#58129,#58130,#58131,#58132,#58133,
#58134,#58135,#58136,#58137,#58138,#58139,#58140,#58141,#58142,#58143,#58144,
#58145,#58146,#58147,#58148,#58149,#58150,#58151,#58152,#58153,#58154,#58155,
#58156,#58157,#58158,#58159,#58160,#58161,#58162,#58163,#58164,#58165,#58166,
#58167,#58168,#58169,#58170,#58171,#58172,#58173,#58174,#58175,#58176,#58177,
#58178,#58179,#58180,#58181,#58182,#58183,#58184,#58185,#58186,#58187,#58188,
#58189,#58190,#58191,#58192,#58193,#58194,#58195,#58196,#58197,#58198,#58199,
#58200,#58201,#58202,#58203,#58204,#58205,#58206,#58207,#58208,#58209,#58210,
#58211,#58212,#58213,#58214,#58215,#58216,#58217,#58218,#58219,#58220,#58221,
#58222,#58223,#58224,#58225,#58226,#58227,#58228,#58229,#58230,#58231,#58232,
#58233,#58234,#58235,#58236,#58237,#58238,#58239,#58240,#58241,#58242,#58243,
#58244,#58245,#58246,#58247,#58248,#58249,#58250,#58251,#58252,#58253,#58254,
#58255,#58256,#58257,#58258,#58259,#58260,#58261,#58262,#58263,#58264,#58265,
#58266,#58267,#58268,#58269,#58270,#58271,#58272,#58273,#58274,#58275,#58276,
#58277,#58278,#58279,#58280,#58281,#58282,#58283,#58284,#58285,#58286,#58287,
#58288,#58289,#58290,#58291,#58292,#58293,#58294,#58295,#58296,#58297,#58298,
#58299,#58300,#58301,#58302,#58303,#58304,#58305,#58306,#58307,#58308,#58309,
#58310,#58311,#58312,#58313,#58314,#58315,#58316,#58317,#58318,#58319,#58320,
#58321,#58322,#58323,#58324,#58325,#58326,#58327,#58328,#58329,#58330,#58331,
#58332,#58333,#58334,#58335,#58336,#58337,#58338,#58339,#58340,#58341,#58342,
#58343,#58344,#58345,#58346,#58347,#58348,#58349,#58350,#58351,#58352,#58353,
#58354,#58355,#58356,#58357,#58358,#58359,#58360,#58361,#58362,#58363,#58364,
#58365,#58366,#58367,#58368,#58369,#58370,#58371,#58372,#58373,#58374,#58375,
#58376,#58377,#58378,#58379,#58380,#58381,#58382,#58383,#58384,#58385,#58386,
#58387,#58388,#58389,#58390,#58391,#58392,#58393,#58394,#58395,#58396,#58397,
#58398,#58399,#58400,#58401,#58402,#58403,#58404,#58405,#58406,#58407,#58408,
#58409,#58410,#58411,#58412,#58413,#58414,#58415,#58416,#58417,#58418,#58419,
#58420,#58421,#58422,#58423,#58424,#58425,#58426,#58427,#58428,#58429,#58430,
#58431,#58432,#58433,#58434,#58435),.UNSPECIFIED.,.F.,.F.,(4,2,2,2,2,2,
2,2,2,2,2,2,2,2,2,2,2,2,2,2,2,2,2,2,2,2,2,2,2,2,2,2,2,2,2,2,2,2,2,2,2,2,
2,2,2,2,2,2,2,2,2,2,2,2,2,2,2,2,2,2,2,2,2,2,2,2,2,2,2,2,2,2,2,2,2,2,2,2,
2,2,2,2,2,2,2,2,2,2,2,2,2,2,2,2,2,2,2,2,2,2,2,2,2,2,2,2,2,2,2,2,2,2,2,2,
2,2,2,2,2,2,2,2,2,2,2,2,2,2,2,2,2,2,2,2,2,2,2,2,2,2,2,2,2,2,2,2,2,2,2,2,
2,2,2,2,2,2,2,2,2,2,2,2,2,2,2,2,2,2,2,2,2,2,2,2,2,2,2,2,2,2,2,2,2,2,2,2,
2,2,2,2,2,2,2,2,2,2,2,2,2,2,2,2,2,2,2,2,2,2,2,2,2,2,2,2,2,2,2,2,2,2,2,2,
2,2,2,2,2,2,2,2,2,2,2,2,2,2,2,2,2,2,2,2,2,2,2,2,2,2,2,2,2,2,2,2,2,2,2,2,
2,2,2,2,2,2,2,2,2,2,2,2,2,2,2,2,2,2,2,2,2,4),(-4.06157938018324,-4.04929940099998,
-4.04313669884873,-4.04131232596992,-4.04003165241435,-4.03892991937186,
-4.03780813755122,-4.03632507831366,-4.03401321255865,-4.02310497446659,
-4.02139406885323,-4.02028008704974,-4.01356621420751,-3.90805438721962,
-3.88890260317504,-3.87978560112757,-3.8782613086838,-3.87746069641896,
-3.87686905537172,-3.87612314488593,-3.87484980277311,-3.87042193660157,
-3.78150287143677,-3.74386351870886,-3.72864913477018,-3.72282242989663,
-3.71996095138317,-3.71824617285081,-3.71669608891183,-3.71552538733439,
-3.71440954869489,-3.71287570741085,-3.70899694799184,-3.65204502404822,
-3.62708797663248,-3.61977440704627,-3.59500091758243,-3.56125084780741,
-3.55817238413721,-3.55593906894415,-3.55500335238149,-3.55433053383106,
-3.55371369247524,-3.55287562628584,-3.55123269384663,-3.53825350179553,
-3.53567362604543,-3.53428025433594,-3.5329163138851,-3.53156634385107,
-3.43909181058316,-3.41331882454522,-3.40314883353897,-3.39882591626416,
-3.39652617792721,-3.39504676601777,-3.39366584656413,-3.392515069685,-3.39114562703312,
-3.3887898333872,-3.37990578129682,-3.37612199512405,-3.37416965822323,
-3.27668455367688,-3.26254713810166,-3.24340234081891,-3.23427885059627,
-3.23275432905304,-3.2319536932878,-3.23130470981491,-3.2306384335494,-3.22939072103251,
-3.22518952237327,-3.15099584662564,-3.10756812923709,-3.08178807186003,
-3.07673025862297,-3.07415139383303,-3.07255448945885,-3.07108889421372,
-3.06993075953537,-3.06878539104258,-3.06714197739563,-3.062579710284,-2.98548767011597,
-2.93924193559961,-2.91600125356003,-2.91110905808973,-2.90984836153644,
-2.90910528813776,-2.90844742682768,-2.90761033645685,-2.90590917358895,
-2.89567051310861,-2.8204966298444,-2.75462558842416,-2.75176271239363,
-2.75004736479306,-2.74849554299325,-2.74732502098873,-2.74620912478893,
-2.74467500893042,-2.74079453020509,-2.683567348571,-2.61678080054094,-2.59774647492763,
-2.58882834480926,-2.58731303494897,-2.58651434407189,-2.58592290940046,
-2.58517564088467,-2.583896128718,-2.57941182824167,-2.48251434544779,-2.43084873181743,
-2.42731766836566,-2.42572216289348,-2.42452819124415,-2.42341154579004,
-2.42187437694899,-2.4179755298692,-2.35733522124522,-2.3263200895269,-2.29458188990736,
-2.26939329355178,-2.2654565459147,-2.26428949363732,-2.26356745093017,
-2.26290467449152,-2.26204320330842,-2.26023662725417,-2.24712245277621,
-2.24466784325711,-2.24429446543634,-2.24338296534809,-2.15819662764129,
-2.10817288312619,-2.10465025365646,-2.10305638775078,-2.10186275969647,
-2.10074579435196,-2.09920717801928,-2.09529933977342,-2.03084478645711,
-1.957000782158,-1.95370122822266,-1.94364921999502,-1.94197856353996,-1.94113616255659,
-1.94047780080694,-1.93973809712531,-1.93849222053185,-1.93376382991103,
-1.8991626165271,-1.84121037601963,-1.78612514958083,-1.7822608191165,-1.7807295182096,
-1.77961441375779,-1.77841952817089,-1.77681837260095,-1.77325663088332,
-1.7685316229984,-1.72427175975269,-1.63143879327304,-1.62096599449034,
-1.61925292262388,-1.61841342881897,-1.61775529863996,-1.6170136631592,
-1.6157594598391,-1.61094044978144,-1.57507911925762,-1.47935487149066,
-1.46186741121067,-1.45890189822566,-1.45739581777379,-1.45621451913527,
-1.45490397437831,-1.45274948678109,-1.44511322580062,-1.4194135619701,
-1.37612437444694,-1.32092242972616,-1.31667255096297,-1.31280623304216,
-1.31172084910497,-1.30943952881608,-1.29829376465542,-1.29654840007514,
-1.29570252906064,-1.29505906466221,-1.29434119459483,-1.29358732000092,
-1.29247189912089,-1.2904785917702,-1.27475569666923,-1.2557275134402,-1.16771063580113,
-1.13986211622061,-1.13643602005204,-1.13487719828291,-1.13368480470536,
-1.13241180352474,-1.1304253354784,-1.12429909491525,-1.0298526904658,-0.977628311817583,
-0.974405073116387,-0.973282601625687,-0.972641563368027,-0.971994872609418,
-0.971164815782008,-0.970254000503845,-0.968763426002787,-0.965785298004453,
-0.934033265607395,-0.849456122746227,-0.843525608270362,-0.835817114406746,
-0.816557359610101,-0.81346577064542,-0.811954739114466,-0.810772873511582,
-0.809465096477722,-0.807322894047626,-0.79980738511717,-0.751761812465428,
-0.740128041908324,-0.656499929790048,-0.651980566136304,-0.650697229765164,
-0.649949105456,-0.649304983865417,-0.648498982449435,-0.647621507404035,
-0.64621097044235,-0.643450014753405,-0.615681081428755,-0.530832711525216,
-0.525760435977595,-0.515414580338789,-0.493967875588897,-0.490777911785087,
-0.489263796717977,-0.488078194231609,-0.486784902593373,-0.48470762996452,
-0.477803351052211,-0.436116845752842,-0.393385536315315,-0.371882380492645,
-0.35991336209724,-0.330832676303123,-0.328648583552053,-0.327789716192758,
-0.327167496906952,-0.326512345553086,-0.32562651982592,-0.324637764769449,
-0.322958270023982,-0.319452894459693,-0.274882886790835,-0.201068384060724,
-0.171784825943187,-0.168661151373046,-0.167111434905487,-0.165991493052065,
-0.164799415412777,-0.163215709158981,-0.159748056324509,-0.0851461990511898,
-0.0100209562745193,-0.00639465879684327,-0.0052174293180658,-0.0045653640992891,
-0.00391770964333854,-0.00328293326089312,-0.00247679621787721,-0.000957169744583153),
 .UNSPECIFIED.);
#859=B_SPLINE_CURVE_WITH_KNOTS('',3,(#58437,#58438,#58439,#58440,#58441,
#58442,#58443,#58444,#58445,#58446,#58447,#58448,#58449,#58450,#58451,#58452,
#58453,#58454,#58455,#58456,#58457,#58458,#58459,#58460,#58461,#58462,#58463,
#58464,#58465,#58466,#58467,#58468,#58469,#58470,#58471,#58472,#58473,#58474,
#58475,#58476,#58477,#58478,#58479,#58480,#58481,#58482,#58483,#58484,#58485,
#58486,#58487,#58488,#58489,#58490,#58491,#58492,#58493,#58494,#58495,#58496,
#58497,#58498,#58499,#58500,#58501,#58502,#58503,#58504,#58505,#58506,#58507,
#58508,#58509,#58510,#58511,#58512,#58513,#58514,#58515,#58516,#58517,#58518,
#58519,#58520,#58521,#58522,#58523,#58524,#58525,#58526,#58527,#58528,#58529,
#58530,#58531,#58532,#58533,#58534,#58535,#58536,#58537,#58538,#58539,#58540,
#58541,#58542,#58543,#58544,#58545,#58546,#58547,#58548,#58549,#58550,#58551),
 .UNSPECIFIED.,.F.,.F.,(4,3,3,3,3,3,3,3,3,3,3,3,3,3,3,3,3,3,3,3,3,3,3,3,
3,3,3,3,3,3,3,3,3,3,3,3,3,3,4),(109.955742875847,110.120897363818,110.285736432889,
110.450546875869,110.615309592152,110.780469619239,110.943961234955,111.109424047615,
111.274570334181,111.441616160317,111.606682466747,111.774718052735,111.942753638723,
112.108216451383,112.273362737949,112.440408564085,112.605474870515,112.773510456503,
112.941546042491,113.107008855151,113.272155141717,113.439200967853,113.604267274283,
113.772302860271,113.940338446259,114.105801258919,114.270947545485,114.437993371621,
114.603059678051,114.771095264039,114.939130850027,115.104593662687,115.269739949253,
115.436785775389,115.601852081819,115.769887667807,115.937923253795,116.137885025419,
116.238928182531),.UNSPECIFIED.);
#860=B_SPLINE_CURVE_WITH_KNOTS('',3,(#58553,#58554,#58555,#58556,#58557,
#58558,#58559,#58560,#58561,#58562,#58563,#58564,#58565,#58566,#58567,#58568,
#58569,#58570,#58571,#58572,#58573,#58574,#58575,#58576,#58577,#58578,#58579,
#58580,#58581,#58582,#58583,#58584,#58585,#58586,#58587,#58588,#58589,#58590,
#58591,#58592,#58593,#58594,#58595,#58596,#58597,#58598,#58599,#58600,#58601,
#58602,#58603,#58604,#58605,#58606,#58607,#58608,#58609,#58610,#58611,#58612,
#58613,#58614,#58615,#58616,#58617,#58618,#58619,#58620,#58621,#58622,#58623,
#58624,#58625,#58626,#58627,#58628,#58629,#58630,#58631,#58632,#58633,#58634,
#58635,#58636,#58637,#58638,#58639,#58640,#58641,#58642,#58643,#58644,#58645,
#58646,#58647,#58648,#58649,#58650,#58651,#58652,#58653,#58654,#58655,#58656,
#58657,#58658,#58659,#58660,#58661,#58662,#58663,#58664,#58665,#58666,#58667,
#58668,#58669,#58670),.UNSPECIFIED.,.F.,.F.,(4,3,3,3,3,3,3,3,3,3,3,3,3,
3,3,3,3,3,3,3,3,3,3,3,3,3,3,3,3,3,3,3,3,3,3,3,3,3,3,4),(116.238928182823,
116.402979220447,116.567099493634,116.731267675343,116.895801311704,116.936715657563,
117.102178470223,117.267324756789,117.434370582925,117.599436889355,117.767472475343,
117.935508061331,118.100970873991,118.266117160557,118.433162986693,118.598229293123,
118.766264879111,118.934300465099,119.099763277759,119.264909564325,119.431955390461,
119.597021696891,119.765057282879,119.933092868867,120.098555681527,120.263701968093,
120.430747794229,120.595814100659,120.763849686647,120.931885272635,121.097348085295,
121.262494371861,121.429540197997,121.594606504427,121.762642090415,121.930677676403,
122.098914915071,122.266779046469,122.434399504567,122.522113490003),
 .UNSPECIFIED.);
#861=B_SPLINE_CURVE_WITH_KNOTS('',3,(#58672,#58673,#58674,#58675,#58676,
#58677,#58678,#58679,#58680,#58681,#58682,#58683,#58684,#58685,#58686,#58687,
#58688,#58689,#58690,#58691,#58692,#58693,#58694,#58695,#58696,#58697,#58698,
#58699,#58700,#58701,#58702,#58703,#58704,#58705,#58706,#58707,#58708,#58709,
#58710,#58711,#58712,#58713,#58714,#58715,#58716,#58717,#58718,#58719,#58720,
#58721,#58722,#58723,#58724,#58725,#58726,#58727,#58728,#58729,#58730,#58731,
#58732,#58733,#58734,#58735,#58736,#58737,#58738,#58739,#58740,#58741,#58742,
#58743,#58744,#58745,#58746,#58747,#58748,#58749,#58750,#58751,#58752,#58753,
#58754,#58755,#58756,#58757,#58758,#58759,#58760,#58761,#58762,#58763,#58764,
#58765,#58766,#58767,#58768,#58769,#58770,#58771,#58772,#58773,#58774,#58775,
#58776,#58777,#58778,#58779,#58780,#58781,#58782,#58783,#58784,#58785,#58786,
#58787,#58788,#58789,#58790,#58791,#58792,#58793,#58794,#58795,#58796,#58797,
#58798,#58799,#58800,#58801,#58802,#58803,#58804,#58805,#58806,#58807,#58808,
#58809,#58810,#58811,#58812,#58813,#58814,#58815,#58816,#58817,#58818,#58819,
#58820,#58821,#58822,#58823,#58824,#58825,#58826,#58827,#58828,#58829,#58830,
#58831,#58832,#58833,#58834,#58835,#58836,#58837,#58838,#58839,#58840,#58841,
#58842,#58843,#58844,#58845,#58846,#58847,#58848,#58849,#58850,#58851,#58852,
#58853,#58854,#58855,#58856,#58857,#58858,#58859,#58860,#58861,#58862,#58863,
#58864,#58865,#58866,#58867,#58868,#58869,#58870,#58871,#58872,#58873,#58874,
#58875,#58876,#58877,#58878,#58879,#58880,#58881,#58882,#58883,#58884,#58885,
#58886,#58887,#58888,#58889,#58890,#58891,#58892,#58893,#58894,#58895,#58896,
#58897,#58898,#58899,#58900,#58901,#58902,#58903,#58904,#58905,#58906,#58907,
#58908,#58909,#58910,#58911,#58912,#58913,#58914,#58915,#58916,#58917,#58918,
#58919,#58920,#58921,#58922,#58923,#58924,#58925,#58926,#58927,#58928,#58929,
#58930,#58931,#58932,#58933,#58934,#58935,#58936,#58937,#58938,#58939,#58940,
#58941,#58942,#58943,#58944,#58945,#58946,#58947,#58948,#58949,#58950,#58951,
#58952,#58953,#58954,#58955,#58956,#58957,#58958,#58959,#58960,#58961,#58962,
#58963,#58964,#58965,#58966,#58967,#58968,#58969,#58970,#58971,#58972,#58973,
#58974,#58975,#58976,#58977,#58978,#58979,#58980,#58981,#58982,#58983,#58984,
#58985,#58986,#58987,#58988,#58989,#58990,#58991,#58992,#58993,#58994,#58995,
#58996,#58997,#58998,#58999,#59000,#59001,#59002,#59003,#59004,#59005,#59006,
#59007,#59008,#59009,#59010,#59011,#59012,#59013,#59014,#59015,#59016,#59017,
#59018,#59019,#59020,#59021,#59022,#59023,#59024,#59025,#59026,#59027,#59028,
#59029,#59030,#59031,#59032,#59033,#59034,#59035,#59036,#59037,#59038,#59039,
#59040,#59041,#59042,#59043,#59044,#59045,#59046,#59047,#59048,#59049,#59050,
#59051,#59052,#59053,#59054,#59055,#59056,#59057,#59058,#59059,#59060,#59061,
#59062,#59063,#59064,#59065,#59066,#59067,#59068,#59069,#59070,#59071,#59072,
#59073,#59074,#59075,#59076,#59077,#59078,#59079,#59080,#59081,#59082,#59083,
#59084,#59085,#59086,#59087,#59088,#59089,#59090,#59091,#59092,#59093,#59094,
#59095,#59096,#59097,#59098,#59099,#59100,#59101,#59102,#59103,#59104,#59105,
#59106,#59107,#59108,#59109,#59110,#59111,#59112,#59113,#59114,#59115,#59116,
#59117,#59118,#59119,#59120,#59121,#59122,#59123,#59124,#59125,#59126,#59127,
#59128,#59129,#59130,#59131,#59132,#59133,#59134,#59135,#59136,#59137,#59138,
#59139,#59140,#59141,#59142,#59143,#59144,#59145,#59146,#59147,#59148,#59149,
#59150,#59151,#59152,#59153,#59154,#59155,#59156,#59157,#59158,#59159,#59160,
#59161,#59162,#59163,#59164,#59165,#59166,#59167,#59168,#59169,#59170,#59171,
#59172,#59173,#59174,#59175,#59176,#59177,#59178,#59179,#59180,#59181,#59182,
#59183,#59184,#59185,#59186,#59187,#59188,#59189,#59190,#59191,#59192,#59193,
#59194,#59195,#59196,#59197,#59198,#59199,#59200,#59201,#59202,#59203,#59204,
#59205,#59206,#59207,#59208,#59209,#59210,#59211,#59212,#59213),
 .UNSPECIFIED.,.F.,.F.,(4,2,2,2,2,2,2,2,2,2,2,2,2,2,2,2,2,2,2,2,2,2,2,2,
2,2,2,2,2,2,2,2,2,2,2,2,2,2,2,2,2,2,2,2,2,2,2,2,2,2,2,2,2,2,2,2,2,2,2,2,
2,2,2,2,2,2,2,2,2,2,2,2,2,2,2,2,2,2,2,2,2,2,2,2,2,2,2,2,2,2,2,2,2,2,2,2,
2,2,2,2,2,2,2,2,2,2,2,2,2,2,2,2,2,2,2,2,2,2,2,2,2,2,2,2,2,2,2,2,2,2,2,2,
2,2,2,2,2,2,2,2,2,2,2,2,2,2,2,2,2,2,2,2,2,2,2,2,2,2,2,2,2,2,2,2,2,2,2,2,
2,2,2,2,2,2,2,2,2,2,2,2,2,2,2,2,2,2,2,2,2,2,2,2,2,2,2,2,2,2,2,2,2,2,2,2,
2,2,2,2,2,2,2,2,2,2,2,2,2,2,2,2,2,2,2,2,2,2,2,2,2,2,2,2,2,2,2,2,2,2,2,2,
2,2,2,2,2,2,2,2,2,2,2,2,2,2,2,2,2,2,2,2,2,2,2,2,2,2,2,2,2,2,4),(-4.05964741638998,
-3.96771229126991,-3.94150414541432,-3.93094429280988,-3.92936219553924,
-3.92854966160014,-3.92795695033789,-3.92731296325643,-3.92617504777717,
-3.92284664434187,-3.8648582764161,-3.81524979992763,-3.792800589541,-3.77908159504651,
-3.77368464773745,-3.76974918824406,-3.76808607126964,-3.76698046514721,
-3.76577679679464,-3.76432797633504,-3.76071780657895,-3.71015855344816,
-3.68610806425633,-3.64110350011837,-3.61833275389342,-3.60842068353853,
-3.60686343850952,-3.60605609903267,-3.6054639815529,-3.60481744882046,
-3.60366685587539,-3.60024237368457,-3.54292283090896,-3.49313517667065,
-3.4737707172032,-3.45777677408279,-3.45173155455545,-3.44879163046223,
-3.44704457637554,-3.44546961706033,-3.44429540565269,-3.44318603656636,
-3.44167617936555,-3.43793550282111,-3.39321776437008,-3.36394521822187,
-3.31305615860536,-3.28904017461946,-3.28521462158442,-3.28405999859921,
-3.28334086270451,-3.28267735823723,-3.28181026970665,-3.27990562676699,
-3.26476514025276,-3.2190110895415,-3.16969887049525,-3.14102808116928,
-3.13162673130971,-3.12754905153014,-3.12534471108212,-3.12344521573008,
-3.12220309086274,-3.12100883422539,-3.11943771402838,-3.11677809055926,
-3.1001673370388,-3.00461560865409,-2.97477944604189,-2.96342359530593,
-2.96181335210144,-2.96099491036414,-2.96034489323205,-2.95959187004256,
-2.95831909188324,-2.95375585972012,-2.85749620001157,-2.80660749120145,
-2.80361217178845,-2.80184223584783,-2.80025078183398,-2.79907358275466,
-2.79796818669785,-2.79647406933887,-2.79282381167851,-2.75320019014866,
-2.67908456860427,-2.65253511008579,-2.64074982339514,-2.63912561218791,
-2.63830431981327,-2.63764810111837,-2.63689498376993,-2.63562169306295,
-2.63105321088003,-2.5348350736172,-2.48774411415948,-2.4803162640277,-2.47818348671641,
-2.4768780689198,-2.47569611594782,-2.47418189352805,-2.47107293877906,
-2.45142772286948,-2.44434385311394,-2.37011369653049,-2.36539503371552,
-2.34608695847689,-2.3271350577283,-2.31792870084004,-2.31640093189904,
-2.31559978112025,-2.31500829712149,-2.31426332157452,-2.31299331878772,
-2.30859270326235,-2.22327091505121,-2.1603539009291,-2.15659628645676,
-2.15495999908904,-2.15375940965304,-2.15265346301431,-2.15115689336974,
-2.14824135194245,-2.12558733384093,-2.10978650655946,-2.10105107139752,
-2.03017404498582,-2.0203502428717,-2.01782256634113,-2.01569296517961,
-2.01240743623537,-2.00965183280716,-2.00924011927456,-2.00793231192996,
-1.99574131449827,-1.99412823246604,-1.9932979943166,-1.99268328292312,
-1.99200900686524,-1.99106457642466,-1.98877858804073,-1.93679367794855,
-1.86475012865124,-1.83730324110417,-1.83389066365808,-1.83233460959198,
-1.83114292716277,-1.829869317681,-1.82787907134717,-1.82171924122576,-1.78708768356907,
-1.68814030881204,-1.67322900787048,-1.67152105273368,-1.67066653830971,
-1.67004552331697,-1.66937617952708,-1.66845911641212,-1.66633275164356,
-1.61069468857292,-1.53540209617109,-1.53395808323956,-1.51413432127003,
-1.51101682807647,-1.5095007963325,-1.50831849616965,-1.50701377849806,
-1.50488459078559,-1.49749303646297,-1.45078689121974,-1.36373313256029,
-1.36142065094032,-1.35030682318781,-1.34856303831821,-1.34771751752846,
-1.34705882554826,-1.34633588248368,-1.34514305956238,-1.3437121208279,
-1.34089600478512,-1.31214660044174,-1.24100184839937,-1.22390690020138,
-1.19212069868279,-1.18857858356026,-1.18714082784542,-1.18593985645542,
-1.18470573259045,-1.18289898532629,-1.17809850576683,-1.11864321824673,
-1.04511964565717,-1.02800063807625,-1.02603282290231,-1.02515393054467,
-1.0244883493741,-1.02377401220692,-1.0226642332556,-1.01921195057052,-0.974640679061058,
-0.925454618227494,-0.870059336861939,-0.866192405283044,-0.864660643989419,
-0.863545404928706,-0.86235056409264,-0.8607497957851,-0.857190262767763,
-0.829458600875901,-0.805606869339249,-0.742893449047942,-0.727737038477988,
-0.722951424643649,-0.705424934252106,-0.70344459236857,-0.702642668464635,
-0.701973997833251,-0.701279533861291,-0.7002584142616,-0.697472879945731,
-0.693367244688429,-0.681498816352566,-0.665552064240402,-0.626455091227633,
-0.614253972735603,-0.575093365147055,-0.546770142444156,-0.543328856613729,
-0.541767119389444,-0.540574146475342,-0.539302126462858,-0.537320484874904,
-0.53123445412487,-0.436793619122999,-0.412785742341316,-0.383120021847698,
-0.380926487465927,-0.380065944303145,-0.379443236356708,-0.378774752214637,
-0.378114064819476,-0.377231998908609,-0.373079144838368,-0.366196798443717,
-0.340885499502995,-0.315743134760332,-0.246335292556876,-0.223713824583821,
-0.220798472693206,-0.219301595709063,-0.218195225749841,-0.21699398689879,
-0.215356476855426,-0.211594576082469,-0.193456395079492,-0.146609572933761,
-0.129604422682245,-0.121071321008588,-0.111362890677887,-0.104328173526239,
-0.0612248244022761,-0.0585113140628138,-0.0575704700533938,-0.0569258502208856,
-0.0563329889305497,-0.0557015798871949,-0.0549066667988391,-0.053693128986409,
-0.0514504190834883,-0.000956747946955143),.UNSPECIFIED.);
#862=B_SPLINE_CURVE_WITH_KNOTS('',3,(#59215,#59216,#59217,#59218,#59219,
#59220,#59221,#59222,#59223,#59224,#59225,#59226,#59227,#59228,#59229,#59230,
#59231,#59232,#59233,#59234,#59235,#59236,#59237,#59238,#59239,#59240,#59241,
#59242,#59243,#59244,#59245,#59246,#59247,#59248,#59249,#59250,#59251,#59252,
#59253,#59254,#59255,#59256,#59257,#59258,#59259,#59260,#59261,#59262,#59263,
#59264,#59265,#59266,#59267,#59268,#59269,#59270,#59271,#59272,#59273,#59274,
#59275,#59276,#59277,#59278,#59279,#59280,#59281,#59282,#59283,#59284,#59285,
#59286,#59287,#59288,#59289,#59290,#59291,#59292,#59293,#59294,#59295,#59296,
#59297,#59298,#59299,#59300,#59301,#59302,#59303,#59304,#59305,#59306,#59307,
#59308,#59309,#59310,#59311,#59312,#59313,#59314,#59315,#59316,#59317,#59318,
#59319,#59320,#59321,#59322,#59323,#59324,#59325,#59326,#59327,#59328,#59329,
#59330,#59331,#59332,#59333,#59334,#59335,#59336,#59337,#59338,#59339,#59340,
#59341,#59342,#59343,#59344,#59345,#59346,#59347,#59348,#59349,#59350,#59351,
#59352,#59353,#59354,#59355,#59356,#59357,#59358,#59359,#59360,#59361,#59362,
#59363,#59364,#59365,#59366,#59367,#59368,#59369,#59370,#59371,#59372,#59373,
#59374,#59375,#59376,#59377,#59378,#59379,#59380,#59381,#59382,#59383,#59384,
#59385,#59386,#59387,#59388,#59389,#59390,#59391,#59392,#59393,#59394,#59395,
#59396,#59397,#59398,#59399,#59400,#59401,#59402,#59403,#59404,#59405,#59406,
#59407,#59408,#59409,#59410,#59411,#59412,#59413,#59414,#59415,#59416,#59417,
#59418,#59419,#59420,#59421,#59422,#59423,#59424,#59425,#59426,#59427,#59428,
#59429,#59430,#59431,#59432,#59433,#59434,#59435,#59436,#59437,#59438,#59439,
#59440,#59441,#59442,#59443,#59444,#59445,#59446,#59447,#59448,#59449,#59450,
#59451,#59452,#59453,#59454,#59455,#59456,#59457,#59458,#59459,#59460,#59461,
#59462,#59463,#59464,#59465,#59466,#59467,#59468,#59469,#59470,#59471,#59472,
#59473,#59474,#59475,#59476,#59477,#59478,#59479,#59480,#59481,#59482,#59483,
#59484,#59485,#59486,#59487,#59488,#59489,#59490,#59491,#59492,#59493,#59494,
#59495,#59496,#59497,#59498,#59499,#59500,#59501,#59502,#59503,#59504,#59505,
#59506,#59507,#59508,#59509,#59510,#59511,#59512,#59513,#59514,#59515,#59516,
#59517,#59518,#59519,#59520,#59521,#59522,#59523,#59524,#59525,#59526,#59527,
#59528,#59529,#59530,#59531,#59532,#59533,#59534,#59535,#59536,#59537,#59538,
#59539,#59540,#59541,#59542,#59543,#59544,#59545,#59546,#59547,#59548,#59549,
#59550,#59551,#59552,#59553,#59554,#59555,#59556,#59557,#59558,#59559,#59560,
#59561,#59562,#59563,#59564,#59565,#59566,#59567,#59568,#59569,#59570,#59571,
#59572,#59573,#59574,#59575,#59576,#59577,#59578,#59579,#59580,#59581,#59582,
#59583,#59584,#59585,#59586,#59587,#59588,#59589,#59590,#59591,#59592,#59593,
#59594,#59595,#59596,#59597,#59598,#59599,#59600,#59601,#59602,#59603,#59604,
#59605,#59606,#59607,#59608,#59609,#59610,#59611,#59612,#59613,#59614,#59615,
#59616,#59617,#59618,#59619,#59620,#59621,#59622,#59623,#59624,#59625,#59626,
#59627,#59628,#59629,#59630,#59631,#59632,#59633,#59634,#59635,#59636,#59637,
#59638,#59639,#59640,#59641,#59642,#59643,#59644,#59645,#59646,#59647,#59648,
#59649,#59650,#59651,#59652,#59653,#59654,#59655,#59656,#59657,#59658,#59659,
#59660,#59661,#59662,#59663,#59664,#59665,#59666,#59667,#59668,#59669,#59670,
#59671,#59672,#59673,#59674,#59675,#59676,#59677,#59678,#59679,#59680,#59681,
#59682,#59683,#59684,#59685,#59686,#59687,#59688,#59689,#59690,#59691,#59692,
#59693,#59694,#59695,#59696,#59697,#59698,#59699,#59700,#59701,#59702,#59703,
#59704,#59705,#59706,#59707,#59708,#59709,#59710,#59711,#59712,#59713,#59714,
#59715,#59716,#59717,#59718,#59719,#59720,#59721,#59722,#59723,#59724,#59725,
#59726,#59727,#59728,#59729,#59730,#59731,#59732,#59733,#59734,#59735,#59736,
#59737,#59738,#59739,#59740),.UNSPECIFIED.,.F.,.F.,(4,2,2,2,2,2,2,2,2,2,
2,2,2,2,2,2,2,2,2,2,2,2,2,2,2,2,2,2,2,2,2,2,2,2,2,2,2,2,2,2,2,2,2,2,2,2,
2,2,2,2,2,2,2,2,2,2,2,2,2,2,2,2,2,2,2,2,2,2,2,2,2,2,2,2,2,2,2,2,2,2,2,2,
2,2,2,2,2,2,2,2,2,2,2,2,2,2,2,2,2,2,2,2,2,2,2,2,2,2,2,2,2,2,2,2,2,2,2,2,
2,2,2,2,2,2,2,2,2,2,2,2,2,2,2,2,2,2,2,2,2,2,2,2,2,2,2,2,2,2,2,2,2,2,2,2,
2,2,2,2,2,2,2,2,2,2,2,2,2,2,2,2,2,2,2,2,2,2,2,2,2,2,2,2,2,2,2,2,2,2,2,2,
2,2,2,2,2,2,2,2,2,2,2,2,2,2,2,2,2,2,2,2,2,2,2,2,2,2,2,2,2,2,2,2,2,2,2,2,
2,2,2,2,2,2,2,2,2,2,2,2,2,2,2,2,2,2,2,2,2,2,2,2,2,2,2,2,2,2,2,2,2,2,2,2,
4),(-4.06114224698561,-4.00001303158136,-3.96528985380881,-3.959118626996,
-3.95712662291717,-3.95585237803074,-3.95466044648186,-3.95310456183611,
-3.95049748498737,-3.93490221555494,-3.92983053850339,-3.92821890119364,
-3.85262336244111,-3.83150826821505,-3.79897703100541,-3.79607454941721,
-3.79528181464072,-3.79465108344775,-3.79405855594289,-3.79341287334194,
-3.7924680859699,-3.78972696349286,-3.74440205570379,-3.71004024964133,
-3.67042696822791,-3.64457976068527,-3.63686433379437,-3.63470190137461,
-3.63338957264201,-3.63220863409026,-3.63070571216941,-3.62775493710997,
-3.61054768063997,-3.6094901380153,-3.53902604148103,-3.49812184619457,
-3.48202430360799,-3.47689974011342,-3.47359373374267,-3.47249849170568,
-3.47188261771507,-3.47122420957702,-3.47038172863594,-3.46865349226174,
-3.45787418778024,-3.42814344596467,-3.36427505272666,-3.33605139278129,
-3.31551897369797,-3.31262995128466,-3.31115999022718,-3.31009392816273,
-3.30895700237288,-3.30734427372795,-3.30298176152018,-3.23311418678964,
-3.1853722183985,-3.16182022701342,-3.15516852601445,-3.15247811999766,
-3.15051705649481,-3.14961512860368,-3.14894508542379,-3.14832471740542,
-3.14747299955162,-3.14533066318468,-3.11879577598211,-3.04448852433188,
-2.99390205281782,-2.99032252751395,-2.98871805885583,-2.98752258107513,
-2.98640827745896,-2.98488018612651,-2.98103494843924,-2.9280843670292,
-2.86508267184413,-2.84661426088346,-2.83110406606961,-2.82817669725758,
-2.82713361063186,-2.8265196115286,-2.82585673517008,-2.82499487006355,
-2.82355656835764,-2.81516819735642,-2.71424617545012,-2.67071867008357,
-2.66741109118186,-2.66585780917715,-2.66467040098836,-2.6635412187936,
-2.66195669583781,-2.65869258461702,-2.62363440047175,-2.55779579698852,
-2.50720989183457,-2.50508955252923,-2.50417349864469,-2.50350428200063,
-2.50288293201163,-2.50202728820265,-2.50031502419303,-2.48527276429107,
-2.44453476750168,-2.39351253240482,-2.34878880014281,-2.34503670495141,
-2.34340109613744,-2.34220033998085,-2.34109377277499,-2.33959565383928,
-2.33667500769443,-2.31389988141551,-2.29823112953338,-2.21890685638057,
-2.19403202459556,-2.18375362864259,-2.18218168756151,-2.18137111019561,
-2.18071550783119,-2.18005350831207,-2.17882691282501,-2.17480515329745,
-2.10030382621504,-2.05692714523976,-2.03117461525432,-2.02366086652744,
-2.02142375927547,-2.02009472513819,-2.0190344970597,-2.01761425589761,
-2.01496156572746,-2.00028367548369,-1.97099808392245,-1.92115105916958,
-1.86378704739135,-1.86300850996411,-1.86017785106389,-1.85911413743264,
-1.85848477272725,-1.85788680338899,-1.85703769178822,-1.85527600282917,
-1.83780101911226,-1.81865185858543,-1.73484232555152,-1.72761076611245,
-1.72215181902474,-1.70249246601315,-1.69938220727608,-1.69786746831221,
-1.69668516593646,-1.69537941702786,-1.6932462226591,-1.68581813519658,
-1.63872427347712,-1.55210306882951,-1.5501045547725,-1.53867470255187,
-1.53691617974683,-1.53606766137065,-1.53540852959051,-1.53467221650713,
-1.53344173538332,-1.52887998342651,-1.49647240665228,-1.40025392101122,
-1.39660920896643,-1.37947947046207,-1.37653288547301,-1.37503089896113,
-1.37385010855601,-1.37253733826996,-1.37041602830899,-1.36304824917662,
-1.31633468132226,-1.24245971127869,-1.21653207090875,-1.21440063136174,
-1.21355078928561,-1.21293091682349,-1.21226052724157,-1.21133811382842,
-1.20935081154521,-1.18617746785199,-1.16360025720917,-1.09483637160338,
-1.07996115238234,-1.05724080802097,-1.05432200839922,-1.05282431012563,
-1.05171779793573,-1.0505168542246,-1.04888055013317,-1.0452274786955,-1.04029765039158,
-0.992644272547453,-0.937048251885136,-0.894691841960536,-0.892004654175016,
-0.891067679287383,-0.890424162169914,-0.88983106874731,-0.889016787497805,
-0.887459009777875,-0.879396112447043,-0.862067764628417,-0.79601548088594,
-0.735676717232088,-0.731779323973176,-0.730242368410367,-0.729125751834298,
-0.727931692835962,-0.726335868815505,-0.722919528044963,-0.700375873421387,
-0.680524479667042,-0.631226351387264,-0.57274738391304,-0.569531998340495,
-0.568410581942753,-0.567769759554352,-0.567175948158349,-0.566355826027135,
-0.565474202695044,-0.561322210745656,-0.532548018902344,-0.482280282293101,
-0.461658274880054,-0.446902437031573,-0.412562908864718,-0.40895326461438,
-0.407504219745201,-0.406300191464685,-0.405069438788336,-0.403836222115316,
-0.402130094620727,-0.392366567468876,-0.375034081561154,-0.342880070155488,
-0.316554158052441,-0.250709848203937,-0.247060423852895,-0.245880168433941,
-0.245227489125309,-0.24463624563698,-0.243839638718882,-0.242990778729422,
-0.241648628012149,-0.226759001258927,-0.192580550022399,-0.178973385328588,
-0.164474901946467,-0.0910876980290721,-0.0867414813788719,-0.0851312652438351,
-0.0839949960333603,-0.082928656904803,-0.0814569148344321,-0.0798804066408968,
-0.0773501622759522,-0.00095726213492795),.UNSPECIFIED.);
#863=B_SPLINE_CURVE_WITH_KNOTS('',3,(#59742,#59743,#59744,#59745,#59746,
#59747,#59748,#59749,#59750,#59751,#59752,#59753,#59754,#59755,#59756,#59757,
#59758,#59759,#59760,#59761,#59762,#59763,#59764,#59765,#59766,#59767,#59768,
#59769,#59770,#59771,#59772,#59773,#59774,#59775,#59776,#59777,#59778,#59779,
#59780,#59781,#59782,#59783,#59784,#59785,#59786,#59787,#59788,#59789,#59790,
#59791,#59792,#59793,#59794,#59795,#59796,#59797,#59798,#59799,#59800,#59801,
#59802,#59803,#59804,#59805,#59806,#59807,#59808,#59809,#59810,#59811,#59812,
#59813,#59814,#59815,#59816,#59817,#59818,#59819,#59820,#59821,#59822,#59823,
#59824,#59825,#59826,#59827,#59828,#59829,#59830,#59831,#59832,#59833,#59834,
#59835,#59836,#59837,#59838,#59839,#59840,#59841,#59842,#59843,#59844,#59845,
#59846,#59847,#59848,#59849,#59850,#59851,#59852,#59853,#59854,#59855,#59856,
#59857,#59858,#59859,#59860,#59861,#59862,#59863,#59864,#59865,#59866,#59867,
#59868,#59869,#59870,#59871,#59872,#59873,#59874,#59875,#59876,#59877,#59878,
#59879,#59880,#59881,#59882,#59883,#59884,#59885,#59886,#59887,#59888,#59889,
#59890,#59891,#59892,#59893,#59894,#59895,#59896,#59897,#59898,#59899,#59900,
#59901,#59902,#59903,#59904,#59905,#59906,#59907,#59908,#59909,#59910,#59911,
#59912,#59913,#59914,#59915,#59916,#59917,#59918,#59919,#59920,#59921,#59922,
#59923,#59924,#59925,#59926,#59927,#59928,#59929,#59930,#59931,#59932,#59933,
#59934,#59935,#59936,#59937,#59938,#59939,#59940,#59941,#59942,#59943,#59944,
#59945,#59946,#59947,#59948,#59949,#59950,#59951,#59952,#59953,#59954,#59955,
#59956,#59957,#59958,#59959,#59960,#59961,#59962,#59963,#59964,#59965,#59966,
#59967,#59968,#59969,#59970,#59971,#59972,#59973,#59974,#59975,#59976,#59977,
#59978,#59979,#59980,#59981,#59982,#59983,#59984,#59985,#59986,#59987,#59988,
#59989,#59990,#59991,#59992,#59993,#59994,#59995,#59996,#59997,#59998,#59999,
#60000,#60001,#60002,#60003,#60004,#60005,#60006,#60007,#60008,#60009,#60010,
#60011,#60012,#60013,#60014,#60015,#60016,#60017,#60018,#60019,#60020,#60021,
#60022,#60023,#60024,#60025,#60026,#60027,#60028,#60029,#60030,#60031,#60032,
#60033,#60034,#60035,#60036,#60037,#60038,#60039,#60040,#60041,#60042,#60043,
#60044,#60045,#60046,#60047,#60048,#60049,#60050,#60051,#60052,#60053,#60054,
#60055,#60056,#60057,#60058,#60059,#60060,#60061,#60062,#60063,#60064,#60065,
#60066,#60067,#60068,#60069,#60070,#60071,#60072,#60073,#60074,#60075,#60076,
#60077,#60078,#60079,#60080,#60081,#60082,#60083,#60084,#60085,#60086,#60087,
#60088,#60089,#60090,#60091,#60092,#60093,#60094,#60095,#60096,#60097,#60098,
#60099,#60100,#60101,#60102,#60103,#60104,#60105,#60106,#60107,#60108,#60109,
#60110,#60111,#60112,#60113,#60114,#60115,#60116,#60117,#60118,#60119,#60120,
#60121,#60122,#60123,#60124,#60125,#60126,#60127,#60128,#60129,#60130,#60131,
#60132,#60133,#60134,#60135,#60136,#60137,#60138,#60139,#60140,#60141,#60142,
#60143,#60144,#60145,#60146,#60147,#60148,#60149,#60150,#60151,#60152,#60153,
#60154,#60155,#60156,#60157,#60158,#60159,#60160,#60161,#60162,#60163,#60164,
#60165,#60166,#60167,#60168,#60169,#60170,#60171,#60172,#60173,#60174,#60175,
#60176,#60177,#60178,#60179,#60180,#60181,#60182,#60183,#60184,#60185,#60186,
#60187,#60188,#60189,#60190,#60191,#60192,#60193,#60194,#60195,#60196,#60197,
#60198,#60199,#60200,#60201,#60202,#60203,#60204,#60205,#60206,#60207,#60208,
#60209,#60210,#60211,#60212,#60213,#60214,#60215,#60216,#60217,#60218,#60219,
#60220,#60221,#60222,#60223,#60224,#60225,#60226,#60227,#60228,#60229,#60230,
#60231,#60232,#60233,#60234,#60235,#60236,#60237,#60238,#60239,#60240,#60241,
#60242,#60243,#60244,#60245,#60246,#60247,#60248,#60249,#60250,#60251,#60252,
#60253,#60254,#60255,#60256,#60257,#60258,#60259,#60260,#60261,#60262,#60263,
#60264,#60265,#60266,#60267,#60268,#60269,#60270,#60271,#60272,#60273,#60274,
#60275,#60276,#60277,#60278,#60279,#60280,#60281,#60282,#60283),
 .UNSPECIFIED.,.F.,.F.,(4,2,2,2,2,2,2,2,2,2,2,2,2,2,2,2,2,2,2,2,2,2,2,2,
2,2,2,2,2,2,2,2,2,2,2,2,2,2,2,2,2,2,2,2,2,2,2,2,2,2,2,2,2,2,2,2,2,2,2,2,
2,2,2,2,2,2,2,2,2,2,2,2,2,2,2,2,2,2,2,2,2,2,2,2,2,2,2,2,2,2,2,2,2,2,2,2,
2,2,2,2,2,2,2,2,2,2,2,2,2,2,2,2,2,2,2,2,2,2,2,2,2,2,2,2,2,2,2,2,2,2,2,2,
2,2,2,2,2,2,2,2,2,2,2,2,2,2,2,2,2,2,2,2,2,2,2,2,2,2,2,2,2,2,2,2,2,2,2,2,
2,2,2,2,2,2,2,2,2,2,2,2,2,2,2,2,2,2,2,2,2,2,2,2,2,2,2,2,2,2,2,2,2,2,2,2,
2,2,2,2,2,2,2,2,2,2,2,2,2,2,2,2,2,2,2,2,2,2,2,2,2,2,2,2,2,2,2,2,2,2,2,2,
2,2,2,2,2,2,2,2,2,2,2,2,2,2,2,2,2,2,2,2,2,2,2,2,2,2,2,2,2,2,4),(-4.05869209090443,
-3.99347258329797,-3.98346120577144,-3.98208998989009,-3.98092451464955,
-3.98020309274606,-3.97954063639963,-3.97867924005389,-3.97687161016431,
-3.96371109793033,-3.90330803197401,-3.88941211170496,-3.87624746347955,
-3.83715160599044,-3.82354092163575,-3.82168028279355,-3.82038502854958,
-3.81911343292964,-3.81792135991715,-3.81636152330673,-3.81292736988021,
-3.78478033641603,-3.74368455190069,-3.71872396463521,-3.69443095110323,
-3.67053686034673,-3.6638476086542,-3.65978456155156,-3.65890867439712,
-3.65809280794549,-3.65743725174819,-3.6567789718537,-3.65556946147614,
-3.65168459272487,-3.58622242948792,-3.53618493112009,-3.50251232365159,
-3.49908882405575,-3.49749477855142,-3.49630162099827,-3.49518553492371,
-3.49364881906767,-3.48974944812107,-3.42835259914059,-3.37827520698967,
-3.35648731837807,-3.34413012705425,-3.33990362330514,-3.33705462975647,
-3.3360131527021,-3.33531912081921,-3.33465087535234,-3.33384947320327,
-3.33187047351668,-3.31435871924742,-3.31382632047267,-3.3125988638393,
-3.30854524847308,-3.28356320945582,-3.24019468590367,-3.20230389615886,
-3.18025010728797,-3.1767512160406,-3.17514500253715,-3.17394980917278,
-3.17283690956727,-3.17131251484101,-3.16748578571744,-3.11619593857404,
-3.04558135936149,-3.01900253211695,-3.01631127234367,-3.014308405995,-3.01341173944794,
-3.01274607162127,-3.01211996984645,-3.01124563256016,-3.0089672390449,
-2.9722445492164,-2.90871398816466,-2.85933728395486,-2.8547410468211,-2.85296761210967,
-2.85173329621102,-2.8505335193074,-2.84909883931475,-2.84557274001998,
-2.81431629949973,-2.73026740070147,-2.69715718415143,-2.69411100829313,
-2.69191249499498,-2.69097380915784,-2.69030069604425,-2.68968491886818,
-2.68885020798521,-2.68721950567013,-2.67456346912241,-2.67364163046961,
-2.67152532678081,-2.58650640212305,-2.54022047085763,-2.53286843056385,
-2.53074384441092,-2.52944045390558,-2.52825837622549,-2.52674126404126,
-2.52361670736036,-2.50362107215227,-2.49803349926442,-2.49106017750256,
-2.42408106944974,-2.40938055692036,-2.3747786175866,-2.37165999457705,
-2.36940385937669,-2.3684645821546,-2.36779138447463,-2.36717577572786,
-2.36634164429621,-2.36429900219243,-2.34269448234719,-2.32577188766398,
-2.3044653320574,-2.26378635877624,-2.21778784599914,-2.21046274708313,
-2.20834091785456,-2.20703810852483,-2.20585582779685,-2.20433743613603,
-2.20120662294794,-2.18107557005975,-2.17518809458094,-2.16809225126649,
-2.08376849980179,-2.05205266781258,-2.04754746600594,-2.0463227676784,
-2.04558798297482,-2.0449289364761,-2.04407878345783,-2.04231068430796,
-2.03065364045763,-2.00419858862673,-1.93092385407595,-1.91720484133572,
-1.89009050337525,-1.8866888911869,-1.88513496052345,-1.88394370547852,
-1.88266938439029,-1.88067560285052,-1.8744859227434,-1.83957993519644,
-1.73929276459037,-1.7375876994948,-1.72584766613721,-1.72407567310284,
-1.72322466373908,-1.72256541454763,-1.72183088768666,-1.72060770990543,
-1.71611983870235,-1.68462950451055,-1.60238725051932,-1.56771372954905,
-1.56409698447731,-1.56264708351932,-1.56144312909577,-1.56021325160227,
-1.55842607341528,-1.55375352080345,-1.53175274533621,-1.5147471883378,
-1.43424825479234,-1.40393268570916,-1.40173035145221,-1.40086847269809,
-1.40024554654462,-1.39957757221406,-1.39866821012499,-1.39658506680723,
-1.39376449718957,-1.36493221022214,-1.27610191022616,-1.24492844691205,
-1.24140390423043,-1.23982714316561,-1.23863192639957,-1.23739206812402,
-1.23553672083929,-1.23336869885897,-1.22938368883327,-1.13765909431138,
-1.12749760261023,-1.08196819024256,-1.07922875452862,-1.07828431096571,
-1.0776387945916,-1.0770463633003,-1.07623673967627,-1.07466884839031,-1.06448897261829,
-1.04010870110007,-0.939603093648809,-0.938552483257593,-0.921333857077579,
-0.918383186266903,-0.916880593927318,-0.915700050302603,-0.914414776111133,
-0.912459832095758,-0.910080233292249,-0.905548931503627,-0.894711326258798,
-0.859207650419671,-0.76130582002647,-0.75689293812503,-0.755621468557156,
-0.754876101976212,-0.754284574964159,-0.753483711848289,-0.751957616907415,
-0.742792813056688,-0.723726030183432,-0.680291557784628,-0.623314637256144,
-0.618189956915694,-0.598861164980214,-0.595766585476366,-0.594255066479902,
-0.593073264135499,-0.591971443730137,-0.590069670801379,-0.584577625832007,
-0.576374678789233,-0.552196945338399,-0.518410522256117,-0.438426681111395,
-0.434254081621596,-0.433009775291891,-0.43234423675009,-0.431689013672621,
-0.430884522809926,-0.429341446107404,-0.419783446657282,-0.406008561488972,
-0.36213950823656,-0.31736657151772,-0.303685341310649,-0.276741440802165,
-0.273683882194079,-0.272150807996261,-0.271035234906337,-0.269908404751917,
-0.268747950612618,-0.266234986174628,-0.253179862043125,-0.227573960953151,
-0.210980423150055,-0.11633706344912,-0.111685449240086,-0.110403127475343,
-0.10964773761638,-0.108991502158835,-0.108172718567571,-0.10656152904128,
-0.0951882948480381,-0.0652806265416462,-0.00095819449416442),
 .UNSPECIFIED.);
#864=B_SPLINE_CURVE_WITH_KNOTS('',3,(#60285,#60286,#60287,#60288,#60289,
#60290,#60291,#60292,#60293,#60294),.UNSPECIFIED.,.F.,.F.,(4,1,1,1,1,1,
1,4),(160.22122533308,160.883581423355,161.882373827123,162.881166230891,
163.879958634659,164.878751038427,165.877543442195,166.50441064026),
 .UNSPECIFIED.);
#865=B_SPLINE_CURVE_WITH_KNOTS('',3,(#60296,#60297,#60298,#60299,#60300,
#60301,#60302,#60303,#60304,#60305,#60306,#60307,#60308,#60309,#60310,#60311,
#60312,#60313,#60314,#60315,#60316,#60317,#60318,#60319,#60320,#60321,#60322,
#60323,#60324,#60325,#60326,#60327,#60328,#60329,#60330,#60331,#60332,#60333,
#60334,#60335,#60336,#60337,#60338,#60339,#60340,#60341,#60342,#60343,#60344,
#60345,#60346,#60347,#60348,#60349,#60350,#60351,#60352,#60353,#60354,#60355,
#60356,#60357,#60358,#60359,#60360,#60361,#60362,#60363,#60364,#60365,#60366,
#60367,#60368,#60369,#60370,#60371,#60372,#60373,#60374,#60375,#60376,#60377,
#60378,#60379,#60380,#60381,#60382,#60383,#60384,#60385,#60386,#60387,#60388,
#60389,#60390,#60391,#60392,#60393,#60394,#60395,#60396,#60397,#60398,#60399,
#60400,#60401,#60402,#60403,#60404,#60405,#60406,#60407,#60408,#60409,#60410,
#60411,#60412,#60413,#60414,#60415,#60416,#60417,#60418,#60419,#60420,#60421,
#60422,#60423,#60424,#60425,#60426,#60427,#60428,#60429,#60430,#60431,#60432,
#60433,#60434,#60435,#60436,#60437,#60438,#60439,#60440,#60441,#60442,#60443,
#60444,#60445,#60446,#60447,#60448,#60449,#60450,#60451,#60452,#60453,#60454,
#60455,#60456,#60457,#60458,#60459,#60460,#60461,#60462,#60463,#60464,#60465,
#60466,#60467,#60468,#60469,#60470,#60471,#60472,#60473,#60474,#60475,#60476,
#60477,#60478,#60479,#60480,#60481,#60482,#60483,#60484,#60485,#60486,#60487,
#60488,#60489,#60490,#60491,#60492,#60493,#60494,#60495,#60496,#60497,#60498,
#60499,#60500,#60501,#60502,#60503,#60504,#60505,#60506,#60507,#60508,#60509,
#60510,#60511,#60512,#60513,#60514,#60515,#60516,#60517,#60518,#60519,#60520,
#60521,#60522,#60523,#60524,#60525,#60526,#60527,#60528,#60529,#60530,#60531,
#60532,#60533,#60534,#60535,#60536,#60537,#60538,#60539,#60540,#60541,#60542,
#60543,#60544,#60545,#60546,#60547,#60548,#60549,#60550,#60551,#60552,#60553,
#60554,#60555,#60556,#60557,#60558,#60559,#60560,#60561,#60562,#60563,#60564,
#60565,#60566,#60567,#60568,#60569,#60570,#60571,#60572,#60573,#60574,#60575,
#60576,#60577,#60578,#60579,#60580,#60581,#60582,#60583,#60584,#60585,#60586,
#60587,#60588,#60589,#60590,#60591,#60592,#60593,#60594,#60595,#60596,#60597,
#60598,#60599,#60600,#60601,#60602,#60603,#60604,#60605,#60606,#60607,#60608,
#60609,#60610,#60611,#60612,#60613,#60614,#60615,#60616,#60617,#60618,#60619,
#60620,#60621,#60622,#60623,#60624,#60625,#60626,#60627,#60628,#60629,#60630,
#60631,#60632,#60633,#60634,#60635,#60636,#60637,#60638,#60639,#60640,#60641,
#60642,#60643,#60644,#60645,#60646,#60647,#60648,#60649,#60650,#60651,#60652,
#60653,#60654,#60655,#60656,#60657,#60658,#60659,#60660,#60661,#60662,#60663,
#60664,#60665,#60666,#60667,#60668,#60669,#60670,#60671,#60672,#60673,#60674,
#60675,#60676,#60677,#60678,#60679,#60680,#60681,#60682,#60683,#60684,#60685,
#60686,#60687,#60688,#60689,#60690,#60691,#60692,#60693,#60694,#60695,#60696,
#60697,#60698,#60699,#60700,#60701,#60702,#60703,#60704,#60705,#60706,#60707,
#60708,#60709,#60710,#60711,#60712,#60713,#60714,#60715,#60716,#60717,#60718,
#60719,#60720,#60721,#60722,#60723,#60724,#60725,#60726,#60727,#60728,#60729,
#60730,#60731,#60732,#60733,#60734,#60735,#60736,#60737,#60738,#60739,#60740,
#60741,#60742,#60743,#60744,#60745,#60746,#60747,#60748,#60749,#60750,#60751,
#60752,#60753,#60754,#60755,#60756,#60757,#60758,#60759,#60760,#60761,#60762,
#60763,#60764,#60765,#60766,#60767,#60768,#60769,#60770,#60771,#60772,#60773,
#60774,#60775,#60776,#60777,#60778,#60779,#60780,#60781,#60782,#60783,#60784,
#60785,#60786,#60787,#60788,#60789,#60790,#60791,#60792,#60793,#60794,#60795,
#60796,#60797,#60798,#60799,#60800,#60801,#60802,#60803,#60804,#60805,#60806,
#60807,#60808,#60809,#60810,#60811,#60812,#60813,#60814,#60815,#60816,#60817,
#60818,#60819),.UNSPECIFIED.,.F.,.F.,(4,2,2,2,2,2,2,2,2,2,2,2,2,2,2,2,2,
2,2,2,2,2,2,2,2,2,2,2,2,2,2,2,2,2,2,2,2,2,2,2,2,2,2,2,2,2,2,2,2,2,2,2,2,
2,2,2,2,2,2,2,2,2,2,2,2,2,2,2,2,2,2,2,2,2,2,2,2,2,2,2,2,2,2,2,2,2,2,2,2,
2,2,2,2,2,2,2,2,2,2,2,2,2,2,2,2,2,2,2,2,2,2,2,2,2,2,2,2,2,2,2,2,2,2,2,2,
2,2,2,2,2,2,2,2,2,2,2,2,2,2,2,2,2,2,2,2,2,2,2,2,2,2,2,2,2,2,2,2,2,2,2,2,
2,2,2,2,2,2,2,2,2,2,2,2,2,2,2,2,2,2,2,2,2,2,2,2,2,2,2,2,2,2,2,2,2,2,2,2,
2,2,2,2,2,2,2,2,2,2,2,2,2,2,2,2,2,2,2,2,2,2,2,2,2,2,2,2,2,2,2,2,2,2,2,2,
2,2,2,2,2,2,2,2,2,2,2,2,2,2,2,2,2,2,2,2,2,2,2,2,2,2,2,2,4),(-4.06096447082831,
-4.00218619815695,-3.94477647938606,-3.94253132446907,-3.94159355959484,
-3.94092033114405,-3.94030388564263,-3.93946746319739,-3.93783103262021,
-3.92503600526774,-3.92421528180793,-3.92384404994144,-3.92091631400899,
-3.91936481455205,-3.91258690982016,-3.83258152742667,-3.81363505663347,
-3.79449492223586,-3.78759300721156,-3.78280477880188,-3.78100146097245,
-3.77990095384434,-3.77870891521173,-3.77715297966182,-3.77374301963086,
-3.74640823523031,-3.69806326678204,-3.65951927375612,-3.63286771916824,
-3.62120232266677,-3.61958165477234,-3.61876097136293,-3.61810465559998,
-3.61735077774152,-3.61607471325399,-3.61148185493626,-3.52449023872323,
-3.48367139400823,-3.46942556509153,-3.46387560092107,-3.45985061544652,
-3.45817174346589,-3.45706703643878,-3.45586669751534,-3.45443160820636,
-3.45090584531046,-3.37392507615069,-3.32691600444757,-3.30161928590703,
-3.29767236744177,-3.29650417531516,-3.29578185452777,-3.29511912296023,
-3.29425811965844,-3.29245397534329,-3.27940438196209,-3.27619211305589,
-3.27127246523667,-3.19059316537041,-3.1453069782317,-3.14051838099005,
-3.13804073358735,-3.1359519726925,-3.13466593904349,-3.13348511219617,
-3.131982728221,-3.12903425580655,-3.11186844919232,-3.01612324975095,-2.97991181478353,
-2.97506901227411,-2.97381269649704,-2.97307059878349,-2.97241256541246,
-2.97157387445079,-2.96986475617299,-2.95947000414462,-2.87448059752547,
-2.82314947137994,-2.81801133204022,-2.81540252962181,-2.81379308992444,
-2.8123173458174,-2.81115816706667,-2.81001633651661,-2.80838570988961,
-2.80390740195913,-2.72833995387676,-2.68094284014332,-2.66179922003237,
-2.65278611138067,-2.65126652046725,-2.65046692997369,-2.64987541720512,
-2.64912883379502,-2.64785236033582,-2.64339567427571,-2.54598670059336,
-2.49980145970686,-2.49245734782595,-2.49033289184346,-2.4890291048637,
-2.48784635453783,-2.48632794242201,-2.483199157835,-2.46313571648298,-2.4574954764943,
-2.45202725289263,-2.36598701959304,-2.33398727655881,-2.32945840855069,
-2.32823107073707,-2.32749547474342,-2.32683621274415,-2.32598647905774,
-2.32422172579294,-2.31265302249965,-2.22873157693695,-2.18837152038456,
-2.17089175140843,-2.16811331468741,-2.16666640337302,-2.16549066861251,
-2.16414199577729,-2.16187552442417,-2.15385961439457,-2.15190754881952,
-2.05316758066489,-2.03066949219596,-2.02885137315661,-2.02393503293034,
-2.02071318300825,-2.00766199684392,-2.00585763963675,-2.00499652960808,
-2.00433371339276,-2.00361129727941,-2.00244294526099,-1.9984954249464,
-1.97319893352562,-1.92525083697928,-1.8510603639767,-1.84635179450875,
-1.84468640984145,-1.84353491495814,-1.8424727738264,-1.84103500967911,
-1.83830037014701,-1.82187124566366,-1.78678273244212,-1.69581062178425,
-1.68475214244394,-1.68301055622251,-1.68216531106741,-1.68150646991398,
-1.68076808598611,-1.67952868788944,-1.67487314505085,-1.6412568690676,
-1.53617931582387,-1.52487048793311,-1.52252859795815,-1.5210361244916,
-1.51985627315952,-1.51853773410441,-1.51634783376683,-1.5083534570595,
-1.45472595018595,-1.40249205000551,-1.37276629193726,-1.36191379794683,
-1.36018191338134,-1.35933868162962,-1.35868016350463,-1.35794081087457,
-1.35672168331944,-1.35224917882957,-1.3207772346126,-1.24485977429493,
-1.23313866151306,-1.2036113627,-1.20048095296736,-1.19892949155482,-1.19780903512143,
-1.19661710284132,-1.19503476998065,-1.19167731122357,-1.14056506878807,
-1.07107161587476,-1.04001100918898,-1.03779766557423,-1.03693376739693,
-1.03631018419738,-1.0356423012306,-1.03498269910086,-1.03340585903183,
-1.02285790269602,-0.996665709950003,-0.938832095524279,-0.881642903737174,
-0.877762424009881,-0.876228265704909,-0.875112323616314,-0.873917709857394,
-0.872318940869264,-0.868863293324374,-0.790051523509473,-0.74833230944164,
-0.717311327989627,-0.71509847592135,-0.714234645701145,-0.713611068238389,
-0.712943148479055,-0.712283496309154,-0.710706317102811,-0.700150731074761,
-0.685545466164838,-0.632432026131966,-0.559510763708878,-0.555209752309043,
-0.553606833484714,-0.552472536521956,-0.551405490517319,-0.549928747396166,
-0.548345328634094,-0.540816664643569,-0.507161542245567,-0.452574164137795,
-0.396157054923731,-0.39435466387973,-0.392282472882878,-0.391465448273148,
-0.390792767079811,-0.390103407430586,-0.389408364851707,-0.388436928662513,
-0.382613521948706,-0.37178156362884,-0.341796723288487,-0.316457124211684,
-0.237435799224814,-0.232692414017665,-0.230836305217791,-0.229716055112962,
-0.228523929692737,-0.226940637619189,-0.225209784927132,-0.222309520217191,
-0.203920827161043,-0.163957449155886,-0.149379467111453,-0.134468359562708,
-0.0738342822100937,-0.0702103412711332,-0.0690333851441698,-0.0683813659741074,
-0.0677900038366501,-0.0669921883173715,-0.066141646527258,-0.0647954905755286,
-0.054637818555212,-0.000957111951693946),.UNSPECIFIED.);
#866=B_SPLINE_CURVE_WITH_KNOTS('',3,(#60821,#60822,#60823,#60824,#60825,
#60826,#60827,#60828,#60829,#60830,#60831,#60832,#60833,#60834,#60835,#60836,
#60837,#60838,#60839,#60840,#60841,#60842,#60843,#60844,#60845,#60846,#60847,
#60848,#60849,#60850,#60851,#60852,#60853,#60854,#60855,#60856,#60857,#60858,
#60859,#60860,#60861,#60862,#60863,#60864,#60865,#60866,#60867,#60868,#60869,
#60870,#60871,#60872,#60873,#60874,#60875,#60876,#60877,#60878,#60879,#60880,
#60881,#60882,#60883,#60884,#60885,#60886,#60887,#60888,#60889,#60890,#60891,
#60892,#60893,#60894,#60895,#60896,#60897,#60898,#60899,#60900,#60901,#60902,
#60903,#60904,#60905,#60906,#60907,#60908,#60909,#60910,#60911,#60912,#60913,
#60914,#60915,#60916,#60917,#60918,#60919,#60920,#60921,#60922,#60923,#60924,
#60925,#60926,#60927,#60928,#60929,#60930,#60931,#60932,#60933,#60934,#60935,
#60936,#60937,#60938,#60939,#60940,#60941,#60942,#60943,#60944,#60945,#60946,
#60947,#60948,#60949,#60950,#60951,#60952,#60953,#60954,#60955,#60956,#60957,
#60958,#60959,#60960,#60961,#60962,#60963,#60964,#60965,#60966,#60967,#60968,
#60969,#60970,#60971,#60972,#60973,#60974,#60975,#60976,#60977,#60978,#60979,
#60980,#60981,#60982,#60983,#60984,#60985,#60986,#60987,#60988,#60989,#60990,
#60991,#60992,#60993,#60994,#60995,#60996,#60997,#60998,#60999,#61000,#61001,
#61002,#61003,#61004,#61005,#61006,#61007,#61008,#61009,#61010,#61011,#61012,
#61013,#61014,#61015,#61016,#61017,#61018,#61019,#61020,#61021,#61022,#61023,
#61024,#61025,#61026,#61027,#61028,#61029,#61030,#61031,#61032,#61033,#61034,
#61035,#61036,#61037,#61038,#61039,#61040,#61041,#61042,#61043,#61044,#61045,
#61046,#61047,#61048,#61049,#61050,#61051,#61052,#61053,#61054,#61055,#61056,
#61057,#61058,#61059,#61060,#61061,#61062,#61063,#61064,#61065,#61066,#61067,
#61068,#61069,#61070,#61071,#61072,#61073,#61074,#61075,#61076,#61077,#61078,
#61079,#61080,#61081,#61082,#61083,#61084,#61085,#61086,#61087,#61088,#61089,
#61090,#61091,#61092,#61093,#61094,#61095,#61096,#61097,#61098,#61099,#61100,
#61101,#61102,#61103,#61104,#61105,#61106,#61107,#61108,#61109,#61110,#61111,
#61112,#61113,#61114,#61115,#61116,#61117,#61118,#61119,#61120,#61121,#61122,
#61123,#61124,#61125,#61126,#61127,#61128,#61129,#61130,#61131,#61132,#61133,
#61134,#61135,#61136,#61137,#61138,#61139,#61140,#61141,#61142,#61143,#61144,
#61145,#61146,#61147,#61148,#61149,#61150,#61151,#61152,#61153,#61154,#61155,
#61156,#61157,#61158,#61159,#61160,#61161,#61162,#61163,#61164,#61165,#61166,
#61167,#61168,#61169,#61170,#61171,#61172,#61173,#61174,#61175,#61176,#61177,
#61178,#61179,#61180,#61181,#61182,#61183,#61184,#61185,#61186,#61187,#61188,
#61189,#61190,#61191,#61192,#61193,#61194,#61195,#61196,#61197,#61198,#61199,
#61200,#61201,#61202,#61203,#61204,#61205,#61206,#61207,#61208,#61209,#61210,
#61211,#61212,#61213,#61214,#61215,#61216,#61217,#61218,#61219,#61220,#61221,
#61222,#61223,#61224,#61225,#61226,#61227,#61228,#61229,#61230,#61231,#61232,
#61233,#61234,#61235,#61236,#61237,#61238,#61239,#61240,#61241,#61242,#61243,
#61244,#61245,#61246,#61247,#61248,#61249,#61250,#61251,#61252,#61253,#61254,
#61255,#61256,#61257,#61258,#61259,#61260,#61261,#61262,#61263,#61264,#61265,
#61266,#61267,#61268,#61269,#61270,#61271,#61272,#61273,#61274,#61275,#61276,
#61277,#61278,#61279,#61280,#61281,#61282,#61283,#61284,#61285,#61286,#61287,
#61288,#61289,#61290,#61291,#61292,#61293,#61294,#61295,#61296,#61297,#61298,
#61299,#61300,#61301,#61302,#61303,#61304,#61305,#61306,#61307,#61308,#61309,
#61310,#61311,#61312,#61313,#61314,#61315,#61316,#61317,#61318,#61319,#61320,
#61321,#61322,#61323,#61324,#61325,#61326,#61327,#61328,#61329,#61330,#61331,
#61332,#61333,#61334,#61335,#61336,#61337,#61338,#61339,#61340,#61341,#61342,
#61343,#61344,#61345,#61346,#61347,#61348),.UNSPECIFIED.,.F.,.F.,(4,2,2,
2,2,2,2,2,2,2,2,2,2,2,2,2,2,2,2,2,2,2,2,2,2,2,2,2,2,2,2,2,2,2,2,2,2,2,2,
2,2,2,2,2,2,2,2,2,2,2,2,2,2,2,2,2,2,2,2,2,2,2,2,2,2,2,2,2,2,2,2,2,2,2,2,
2,2,2,2,2,2,2,2,2,2,2,2,2,2,2,2,2,2,2,2,2,2,2,2,2,2,2,2,2,2,2,2,2,2,2,2,
2,2,2,2,2,2,2,2,2,2,2,2,2,2,2,2,2,2,2,2,2,2,2,2,2,2,2,2,2,2,2,2,2,2,2,2,
2,2,2,2,2,2,2,2,2,2,2,2,2,2,2,2,2,2,2,2,2,2,2,2,2,2,2,2,2,2,2,2,2,2,2,2,
2,2,2,2,2,2,2,2,2,2,2,2,2,2,2,2,2,2,2,2,2,2,2,2,2,2,2,2,2,2,2,2,2,2,2,2,
2,2,2,2,2,2,2,2,2,2,2,2,2,2,2,2,2,2,2,2,2,2,2,2,2,2,2,2,2,2,2,2,2,2,2,2,
2,2,2,2,2,2,2,2,4),(-4.06131869556804,-4.03569863910276,-3.9909247024884,
-3.97862060287754,-3.973641496883,-3.97109218908225,-3.96893113293521,-3.96761920361655,
-3.96643834324285,-3.96493513530557,-3.96198258332817,-3.94473755005551,
-3.94369087588502,-3.87455289302399,-3.85164534667204,-3.82177684670054,
-3.81190432096129,-3.80798881762499,-3.80712260526249,-3.8063135864326,
-3.8057211682998,-3.80507523640384,-3.80392809998666,-3.80052866251502,
-3.74387154325791,-3.70410143400313,-3.66646156166628,-3.65535791910726,
-3.64839952728795,-3.64685259361792,-3.6454022500706,-3.64433880479701,
-3.64319358507599,-3.641550383398,-3.63698869523099,-3.55865323911149,-3.51129861408268,
-3.49541932059155,-3.48603278702949,-3.48450035759345,-3.48369150845678,
-3.48309908098602,-3.48245300560784,-3.48150679816215,-3.47875578525753,
-3.42965437464634,-3.37622728375723,-3.35357150572134,-3.32804046310582,
-3.32463311606416,-3.32303905463316,-3.32184531422547,-3.3207282684827,
-3.31918958026955,-3.31528176495629,-3.25113314273419,-3.20099699126577,
-3.17419434676126,-3.16351302825318,-3.16193145578828,-3.16127139516624,
-3.16060330039048,-3.15998022934258,-3.15911810222608,-3.15691488123021,
-3.12656252666364,-3.06939784441054,-3.00888646940935,-3.0029096689483,
-3.00092262834493,-2.9996494589355,-2.99845704838277,-2.99689840610967,
-2.99347352437931,-2.9656665358806,-2.94232157084541,-2.87427741624493,
-2.84455319416342,-2.84168339304578,-2.83957264692708,-2.83866868810316,
-2.83799829410187,-2.83737847642198,-2.83652879637264,-2.83439820875131,
-2.80851542731251,-2.71928243170916,-2.68617904722715,-2.68021318597376,
-2.6782307809838,-2.67695868592617,-2.67576593709756,-2.6742049171214,-2.6715803005839,
-2.65565216358661,-2.65090332695905,-2.63438260868126,-2.54640469844639,
-2.52130847075577,-2.51738025194337,-2.51621407557219,-2.51549219709238,
-2.51482930559271,-2.5139673216949,-2.5121583817277,-2.49898586244086,-2.49843295858623,
-2.41253509376591,-2.36522158649048,-2.35777229496608,-2.35563691815514,
-2.35433068449459,-2.35314849971841,-2.35163468389678,-2.34852904358714,
-2.32896851302666,-2.32353606397736,-2.30467290179328,-2.23382782656863,
-2.20721949574438,-2.19550009001742,-2.19387771982011,-2.19305670131569,
-2.19240037749282,-2.19164677939242,-2.19037185099724,-2.18578950879352,
-2.08963527085972,-2.03864313074189,-2.0342141389977,-2.03246470567244,
-2.03124236597178,-2.03001660696279,-2.02825029438574,-2.02371415791498,
-1.96749169832077,-1.87657162270288,-1.87207513104574,-1.87079431379922,
-1.87004676870704,-1.86945538972021,-1.86865712709353,-1.86714376701672,
-1.85826747585291,-1.83930544008547,-1.79257604003289,-1.74409091328136,
-1.71458792360639,-1.711458113297,-1.70990678492543,-1.70878634788007,-1.70759436502605,
-1.70601184381665,-1.70255101001824,-1.63139273241994,-1.56370711464608,
-1.56214191974715,-1.55024054192167,-1.54846099971433,-1.54760831924798,
-1.54694865777873,-1.54621459971359,-1.54499428290201,-1.54053914613007,
-1.5094599330364,-1.42135597296793,-1.39180812308225,-1.38867715145079,
-1.38712554551831,-1.38600504733111,-1.38481312875505,-1.38323091301578,
-1.37988284870221,-1.36295648228376,-1.32075011352674,-1.2386392744335,
-1.22742267705983,-1.22567384535582,-1.22482721382252,-1.22416826974383,
-1.2234308096263,-1.22222010272727,-1.21786103246147,-1.18771586860836,
-1.11990263055763,-1.06969992951049,-1.06588229069133,-1.06435880953691,
-1.06324561824641,-1.06204920324017,-1.06043976576669,-1.05693302528263,
-1.05224560753613,-1.00859471534161,-0.942822426554163,-0.927204026504941,
-0.919086579621284,-0.918484199093398,-0.917698385617313,-0.904853502731454,
-0.903215209423113,-0.902378285369261,-0.901761688312629,-0.901088519373151,
-0.900419587839021,-0.898756233310041,-0.885450446991834,-0.86003378349266,
-0.810699060081097,-0.747164025227985,-0.743256605043414,-0.741717833837789,
-0.740600644362787,-0.739406672159888,-0.737812168563272,-0.734403362734202,
-0.708880510765015,-0.686224876365195,-0.632786461502381,-0.583596107392925,
-0.580842910186204,-0.57989628003352,-0.579250011864593,-0.578657482502376,
-0.577848608093183,-0.576316500275781,-0.56694299960962,-0.550478284461759,
-0.50358876610826,-0.425393255384568,-0.420832955564247,-0.419189778872074,
-0.418044431345235,-0.416980754281111,-0.415529921172911,-0.413982379816667,
-0.407018250335395,-0.395902507449545,-0.358182890253443,-0.318506204301113,
-0.261761201589244,-0.258355853819562,-0.257207716837274,-0.256561490603367,
-0.255968972722374,-0.255160073741072,-0.254294097540713,-0.250384052523628,
-0.240514951347302,-0.210607965309897,-0.187683494692836,-0.118658155605018,
-0.117613936309703,-0.100335826894927,-0.0973810513441103,-0.0958771694253617,
-0.0946960042762633,-0.0933839680649612,-0.091223268034337,-0.0886745600925323,
-0.0836973545416452,-0.0713997823159879,-0.0269275451426486,-0.00095762347367935),
 .UNSPECIFIED.);
#867=B_SPLINE_CURVE_WITH_KNOTS('',3,(#61350,#61351,#61352,#61353,#61354,
#61355,#61356,#61357,#61358,#61359,#61360,#61361,#61362,#61363,#61364,#61365,
#61366,#61367,#61368,#61369,#61370,#61371,#61372,#61373,#61374,#61375,#61376,
#61377,#61378,#61379,#61380,#61381,#61382,#61383,#61384,#61385,#61386,#61387,
#61388,#61389,#61390,#61391,#61392,#61393,#61394,#61395,#61396,#61397,#61398,
#61399,#61400,#61401,#61402,#61403,#61404,#61405,#61406,#61407,#61408,#61409,
#61410,#61411,#61412,#61413,#61414,#61415,#61416,#61417,#61418,#61419,#61420,
#61421,#61422,#61423,#61424,#61425,#61426,#61427,#61428,#61429,#61430,#61431,
#61432,#61433,#61434,#61435,#61436,#61437,#61438,#61439,#61440,#61441,#61442,
#61443,#61444,#61445,#61446,#61447,#61448,#61449,#61450,#61451,#61452,#61453,
#61454,#61455,#61456,#61457,#61458,#61459,#61460,#61461,#61462,#61463,#61464,
#61465,#61466,#61467,#61468,#61469,#61470,#61471,#61472,#61473,#61474,#61475,
#61476,#61477,#61478,#61479,#61480,#61481,#61482,#61483,#61484,#61485,#61486,
#61487,#61488,#61489,#61490,#61491,#61492,#61493,#61494,#61495,#61496,#61497,
#61498,#61499,#61500,#61501,#61502,#61503,#61504,#61505,#61506,#61507,#61508,
#61509,#61510,#61511,#61512,#61513,#61514,#61515,#61516,#61517,#61518,#61519,
#61520,#61521,#61522,#61523,#61524,#61525,#61526,#61527,#61528,#61529,#61530,
#61531,#61532,#61533,#61534,#61535,#61536,#61537,#61538,#61539,#61540,#61541,
#61542,#61543,#61544,#61545,#61546,#61547,#61548,#61549,#61550,#61551,#61552,
#61553,#61554,#61555,#61556,#61557,#61558,#61559,#61560,#61561,#61562,#61563,
#61564,#61565,#61566,#61567,#61568,#61569,#61570,#61571,#61572,#61573,#61574,
#61575,#61576,#61577,#61578,#61579,#61580,#61581,#61582,#61583,#61584,#61585,
#61586,#61587,#61588,#61589,#61590,#61591,#61592,#61593,#61594,#61595,#61596,
#61597,#61598,#61599,#61600,#61601,#61602,#61603,#61604,#61605,#61606,#61607,
#61608,#61609,#61610,#61611,#61612,#61613,#61614,#61615,#61616,#61617,#61618,
#61619,#61620,#61621,#61622,#61623,#61624,#61625,#61626,#61627,#61628,#61629,
#61630,#61631,#61632,#61633,#61634,#61635,#61636,#61637,#61638,#61639,#61640,
#61641,#61642,#61643,#61644,#61645,#61646,#61647,#61648,#61649,#61650,#61651,
#61652,#61653,#61654,#61655,#61656,#61657,#61658,#61659,#61660,#61661,#61662,
#61663,#61664,#61665,#61666,#61667,#61668,#61669,#61670,#61671,#61672,#61673,
#61674,#61675,#61676,#61677,#61678,#61679,#61680,#61681,#61682,#61683,#61684,
#61685,#61686,#61687,#61688,#61689,#61690,#61691,#61692,#61693,#61694,#61695,
#61696,#61697,#61698,#61699,#61700,#61701,#61702,#61703,#61704,#61705,#61706,
#61707,#61708,#61709,#61710,#61711,#61712,#61713,#61714,#61715,#61716,#61717,
#61718,#61719,#61720,#61721,#61722,#61723,#61724,#61725,#61726,#61727,#61728,
#61729,#61730,#61731,#61732,#61733,#61734,#61735,#61736,#61737,#61738,#61739,
#61740,#61741,#61742,#61743,#61744,#61745,#61746,#61747,#61748,#61749,#61750,
#61751,#61752,#61753,#61754,#61755,#61756,#61757,#61758,#61759,#61760,#61761,
#61762,#61763,#61764,#61765,#61766,#61767,#61768,#61769,#61770,#61771,#61772,
#61773,#61774,#61775,#61776,#61777,#61778,#61779,#61780,#61781,#61782,#61783,
#61784,#61785,#61786,#61787,#61788,#61789,#61790,#61791,#61792,#61793,#61794,
#61795,#61796,#61797,#61798,#61799,#61800,#61801,#61802,#61803,#61804,#61805,
#61806,#61807,#61808,#61809,#61810,#61811,#61812,#61813,#61814,#61815,#61816,
#61817,#61818,#61819,#61820,#61821,#61822,#61823,#61824,#61825,#61826,#61827,
#61828,#61829,#61830,#61831,#61832,#61833,#61834,#61835,#61836,#61837,#61838,
#61839,#61840,#61841,#61842,#61843,#61844,#61845,#61846,#61847,#61848,#61849,
#61850,#61851,#61852,#61853,#61854,#61855,#61856,#61857,#61858,#61859,#61860,
#61861,#61862,#61863,#61864,#61865,#61866,#61867,#61868,#61869,#61870,#61871,
#61872,#61873,#61874,#61875,#61876,#61877,#61878,#61879,#61880,#61881,#61882,
#61883,#61884,#61885,#61886,#61887,#61888,#61889,#61890,#61891,#61892,#61893,
#61894,#61895,#61896,#61897,#61898,#61899,#61900,#61901),.UNSPECIFIED.,
 .F.,.F.,(4,2,2,2,2,2,2,2,2,2,2,2,2,2,2,2,2,2,2,2,2,2,2,2,2,2,2,2,2,2,2,
2,2,2,2,2,2,2,2,2,2,2,2,2,2,2,2,2,2,2,2,2,2,2,2,2,2,2,2,2,2,2,2,2,2,2,2,
2,2,2,2,2,2,2,2,2,2,2,2,2,2,2,2,2,2,2,2,2,2,2,2,2,2,2,2,2,2,2,2,2,2,2,2,
2,2,2,2,2,2,2,2,2,2,2,2,2,2,2,2,2,2,2,2,2,2,2,2,2,2,2,2,2,2,2,2,2,2,2,2,
2,2,2,2,2,2,2,2,2,2,2,2,2,2,2,2,2,2,2,2,2,2,2,2,2,2,2,2,2,2,2,2,2,2,2,2,
2,2,2,2,2,2,2,2,2,2,2,2,2,2,2,2,2,2,2,2,2,2,2,2,2,2,2,2,2,2,2,2,2,2,2,2,
2,2,2,2,2,2,2,2,2,2,2,2,2,2,2,2,2,2,2,2,2,2,2,2,2,2,2,2,2,2,2,2,2,2,2,2,
2,2,2,2,2,2,2,2,2,2,2,2,2,2,2,2,2,2,2,2,2,2,2,2,2,2,2,2,4),(-4.06102915371521,
-4.00733943593029,-3.99716016596606,-3.99580480695467,-3.9949504102,-3.99414983477194,
-3.99355820236957,-3.99290768106946,-3.99173817561084,-3.98817165157536,
-3.92742560176029,-3.91252780523285,-3.89796188468783,-3.85798693922934,
-3.83963195849921,-3.83675661705982,-3.83503605346045,-3.83346015784654,
-3.83226914759206,-3.83114666528226,-3.82927915338896,-3.82446627265448,
-3.74513178642116,-3.71783312479859,-3.68573795207312,-3.67788349767447,
-3.67329525877463,-3.67238693041042,-3.67171643459974,-3.6710423505235,
-3.67042677706451,-3.6695938991768,-3.66797136173466,-3.65555775000817,
-3.65478127186798,-3.60932695647417,-3.55482133755643,-3.52125899810746,
-3.51366418584821,-3.51207661153792,-3.51059682767539,-3.50952929691238,
-3.50839607940177,-3.50679730927733,-3.50252253148154,-3.42955600199011,
-3.37623725490668,-3.36171349326885,-3.35120957181207,-3.34963419436093,
-3.34897469493649,-3.34830683990842,-3.34768304398592,-3.34681849411808,
-3.34460158712089,-3.31329412359299,-3.27159898642495,-3.19311887365023,
-3.1896576357764,-3.18805774882761,-3.18686288646319,-3.1857471352634,-3.18421390120989,
-3.18033922854664,-3.12402869754315,-3.06717190593994,-3.0413120806648,
-3.02860448202687,-3.02695778801249,-3.02612484009397,-3.02552923419839,
-3.02489370774551,-3.02379911704159,-3.02077236884465,-2.96695184145353,
-2.87382065025079,-2.86777086006729,-2.86577850808278,-2.86450408299875,
-2.86331201277833,-2.86175598994524,-2.85834565283953,-2.83100062857812,
-2.81409668608624,-2.73591224284481,-2.70905607729515,-2.7049804435879,
-2.70380107809911,-2.70307078825265,-2.7024102228172,-2.70156471264444,
-2.699775066108,-2.68764002322005,-2.68628112875578,-2.68356662075688,-2.67876007285917,
-2.67005486353434,-2.60470557591073,-2.57260116358125,-2.54951353833579,
-2.54470263240534,-2.54289407771874,-2.54165938086559,-2.54045836217543,
-2.53902115730969,-2.53548352684915,-2.5038804613039,-2.48656745162599,
-2.42374609865796,-2.38369548820815,-2.38168407973732,-2.38078747672822,
-2.38012144642017,-2.37949469195182,-2.37861896810163,-2.37682659522316,
-2.35894580044785,-2.35851693795969,-2.31478670737558,-2.27807710143261,
-2.23026019743436,-2.22276401309483,-2.22062352250683,-2.21931596729519,
-2.21813376532547,-2.21662156067946,-2.21352496520746,-2.19416770114435,
-2.18895088245867,-2.17548222963585,-2.09869525847194,-2.0644668122392,
-2.06136488515132,-2.0591179788927,-2.05817983692009,-2.05750646693748,
-2.05688998557783,-2.05605364868231,-2.05441778292071,-2.04164300068632,
-2.03886444312354,-2.03841120256686,-2.03740178355526,-2.03327875330647,
-2.03144781779701,-2.00920037979788,-1.9056413164506,-1.90449912440638,
-1.8994322961333,-1.89752424492679,-1.89639391422296,-1.89532543022547,
-1.8938384848014,-1.89086681759855,-1.86756711302524,-1.84771271482242,
-1.79800189317953,-1.74013642267774,-1.73996109416646,-1.73672493907313,
-1.7356006519438,-1.73495922546185,-1.7343655292388,-1.73354659020148,-1.73193456287823,
-1.72053491817359,-1.69049906955036,-1.5959482742005,-1.59496663003824,
-1.5785799831447,-1.57593138994919,-1.5743632675347,-1.57316925249797,-1.57189981823352,
-1.569929773153,-1.56393669682915,-1.53082049102495,-1.43808197957827,-1.4362701610064,
-1.43172475487711,-1.42893888336086,-1.42849726943842,-1.42689683370545,
-1.41503509845552,-1.41325728642984,-1.41240494518431,-1.41174532502459,
-1.41101108030882,-1.40978993211521,-1.40532620399357,-1.37414189396467,
-1.29584050206474,-1.2569814159065,-1.25334532376706,-1.25185339619462,
-1.25074829256064,-1.24957056019521,-1.24797587704692,-1.24620158559183,
-1.24319612859928,-1.1916146639028,-1.0960804660733,-1.09141450991743,-1.090130584307,
-1.08937475840956,-1.08871846896896,-1.08790003546813,-1.08629085912563,
-1.0749825197842,-1.04538691813522,-0.948932539611661,-0.932865072291202,
-0.930232730238419,-0.928669245188569,-0.927475857842218,-0.926229968492027,
-0.924317611371169,-0.922093497209466,-0.917965782788841,-0.908409746899213,
-0.879290315483234,-0.829577782899801,-0.771700054523462,-0.771161052022005,
-0.768204747292225,-0.767121546425524,-0.766488275933347,-0.765891822122101,
-0.765053067584421,-0.76334382578701,-0.748440415181851,-0.720937547816619,
-0.629287628851472,-0.624755913173499,-0.609992243447726,-0.607430427895019,
-0.60588779909447,-0.604697861919676,-0.60344344125612,-0.601565883206071,
-0.599337367352461,-0.59519824348891,-0.585606370726419,-0.556399448175455,
-0.506617238973183,-0.449017904541551,-0.445606806245524,-0.444457853245045,
-0.44381147346478,-0.443219008642684,-0.442410471143043,-0.440848484764004,
-0.430829263660783,-0.407359071390185,-0.365989160381794,-0.315908814486658,
-0.288281557522388,-0.284861984073732,-0.283304186065663,-0.282111768643872,
-0.281011157685621,-0.279209870485887,-0.274435765373547,-0.26755916794571,
-0.248512933410093,-0.229473094424572,-0.151451708380495,-0.124658018962657,
-0.122510880889271,-0.121658270280633,-0.121037610923996,-0.120367614628153,
-0.119447880578009,-0.117307428956169,-0.0834569910630557,-0.000958237941546336),
 .UNSPECIFIED.);
#868=B_SPLINE_CURVE_WITH_KNOTS('',3,(#61903,#61904,#61905,#61906,#61907,
#61908,#61909,#61910,#61911,#61912),.UNSPECIFIED.,.F.,.F.,(4,1,1,1,1,1,
1,4),(204.203522483337,204.830447189148,205.829239592916,206.828031996684,
207.826824400452,208.82561680422,209.824409207988,210.486707790517),
 .UNSPECIFIED.);
#869=B_SPLINE_CURVE_WITH_KNOTS('',3,(#61914,#61915,#61916,#61917,#61918,
#61919,#61920,#61921,#61922,#61923,#61924,#61925,#61926,#61927,#61928,#61929,
#61930,#61931,#61932,#61933,#61934,#61935,#61936,#61937,#61938,#61939,#61940,
#61941,#61942,#61943,#61944,#61945,#61946,#61947,#61948,#61949,#61950,#61951,
#61952,#61953,#61954,#61955,#61956,#61957,#61958,#61959,#61960,#61961,#61962,
#61963,#61964,#61965,#61966,#61967,#61968,#61969,#61970,#61971,#61972,#61973,
#61974,#61975,#61976,#61977,#61978,#61979,#61980,#61981,#61982,#61983,#61984,
#61985,#61986,#61987,#61988,#61989,#61990,#61991,#61992,#61993,#61994,#61995,
#61996,#61997,#61998,#61999,#62000,#62001,#62002,#62003,#62004,#62005,#62006,
#62007,#62008,#62009,#62010,#62011,#62012,#62013,#62014,#62015,#62016,#62017,
#62018,#62019,#62020,#62021,#62022,#62023,#62024,#62025,#62026,#62027,#62028,
#62029,#62030,#62031,#62032,#62033,#62034,#62035,#62036,#62037,#62038,#62039,
#62040,#62041,#62042,#62043,#62044,#62045,#62046,#62047,#62048,#62049,#62050,
#62051,#62052,#62053,#62054,#62055,#62056,#62057,#62058,#62059,#62060,#62061,
#62062,#62063,#62064,#62065,#62066,#62067,#62068,#62069,#62070,#62071,#62072,
#62073,#62074,#62075,#62076,#62077,#62078,#62079,#62080,#62081,#62082,#62083,
#62084,#62085,#62086,#62087,#62088,#62089,#62090,#62091,#62092,#62093,#62094,
#62095,#62096,#62097,#62098,#62099,#62100,#62101,#62102,#62103,#62104,#62105,
#62106,#62107,#62108,#62109,#62110,#62111,#62112,#62113,#62114,#62115,#62116,
#62117,#62118,#62119,#62120,#62121,#62122,#62123,#62124,#62125,#62126,#62127,
#62128,#62129,#62130,#62131,#62132,#62133,#62134,#62135,#62136,#62137,#62138,
#62139,#62140,#62141,#62142,#62143,#62144,#62145,#62146,#62147,#62148,#62149,
#62150,#62151,#62152,#62153,#62154,#62155,#62156,#62157,#62158,#62159,#62160,
#62161,#62162,#62163,#62164,#62165,#62166,#62167,#62168,#62169,#62170,#62171,
#62172,#62173,#62174,#62175,#62176,#62177,#62178,#62179,#62180,#62181,#62182,
#62183,#62184,#62185,#62186,#62187,#62188,#62189,#62190,#62191,#62192,#62193,
#62194,#62195,#62196,#62197,#62198,#62199,#62200,#62201,#62202,#62203,#62204,
#62205,#62206,#62207,#62208,#62209,#62210,#62211,#62212,#62213,#62214,#62215,
#62216,#62217,#62218,#62219,#62220,#62221,#62222,#62223,#62224,#62225,#62226,
#62227,#62228,#62229,#62230,#62231,#62232,#62233,#62234,#62235,#62236,#62237,
#62238,#62239,#62240,#62241,#62242,#62243,#62244,#62245,#62246,#62247,#62248,
#62249,#62250,#62251,#62252,#62253,#62254,#62255,#62256,#62257,#62258,#62259,
#62260,#62261,#62262,#62263,#62264,#62265,#62266,#62267,#62268,#62269,#62270,
#62271,#62272,#62273,#62274,#62275,#62276,#62277,#62278,#62279,#62280,#62281,
#62282,#62283,#62284,#62285,#62286,#62287,#62288,#62289,#62290,#62291,#62292,
#62293,#62294,#62295,#62296,#62297,#62298,#62299,#62300,#62301,#62302,#62303,
#62304,#62305,#62306,#62307,#62308,#62309,#62310,#62311,#62312,#62313,#62314,
#62315,#62316,#62317,#62318,#62319,#62320,#62321,#62322,#62323,#62324,#62325,
#62326,#62327,#62328,#62329,#62330,#62331,#62332,#62333,#62334,#62335,#62336,
#62337,#62338,#62339,#62340,#62341,#62342,#62343,#62344,#62345,#62346,#62347,
#62348,#62349,#62350,#62351,#62352,#62353,#62354,#62355,#62356,#62357,#62358,
#62359,#62360,#62361,#62362,#62363,#62364,#62365,#62366,#62367,#62368,#62369,
#62370,#62371,#62372,#62373,#62374,#62375,#62376,#62377,#62378,#62379,#62380,
#62381,#62382,#62383,#62384,#62385,#62386,#62387,#62388,#62389,#62390,#62391,
#62392,#62393,#62394,#62395,#62396,#62397,#62398,#62399,#62400,#62401,#62402,
#62403,#62404,#62405,#62406,#62407,#62408,#62409,#62410,#62411,#62412,#62413,
#62414,#62415,#62416,#62417,#62418,#62419,#62420,#62421,#62422,#62423,#62424,
#62425,#62426,#62427,#62428,#62429,#62430,#62431,#62432,#62433,#62434,#62435,
#62436,#62437,#62438,#62439,#62440,#62441,#62442,#62443,#62444,#62445,#62446,
#62447,#62448,#62449,#62450,#62451,#62452,#62453,#62454,#62455,#62456,#62457,
#62458,#62459,#62460,#62461,#62462,#62463),.UNSPECIFIED.,.F.,.F.,(4,2,2,
2,2,2,2,2,2,2,2,2,2,2,2,2,2,2,2,2,2,2,2,2,2,2,2,2,2,2,2,2,2,2,2,2,2,2,2,
2,2,2,2,2,2,2,2,2,2,2,2,2,2,2,2,2,2,2,2,2,2,2,2,2,2,2,2,2,2,2,2,2,2,2,2,
2,2,2,2,2,2,2,2,2,2,2,2,2,2,2,2,2,2,2,2,2,2,2,2,2,2,2,2,2,2,2,2,2,2,2,2,
2,2,2,2,2,2,2,2,2,2,2,2,2,2,2,2,2,2,2,2,2,2,2,2,2,2,2,2,2,2,2,2,2,2,2,2,
2,2,2,2,2,2,2,2,2,2,2,2,2,2,2,2,2,2,2,2,2,2,2,2,2,2,2,2,2,2,2,2,2,2,2,2,
2,2,2,2,2,2,2,2,2,2,2,2,2,2,2,2,2,2,2,2,2,2,2,2,2,2,2,2,2,2,2,2,2,2,2,2,
2,2,2,2,2,2,2,2,2,2,2,2,2,2,2,2,2,2,2,2,2,2,2,2,2,2,2,2,2,2,2,2,2,2,2,2,
2,2,2,2,2,2,2,2,2,2,2,2,2,2,2,2,2,2,2,4),(-4.06049657891224,-3.98971205792811,
-3.96625604543254,-3.95483641893174,-3.95322370018519,-3.95240461080479,
-3.95175437644203,-3.95100143850387,-3.94972957284891,-3.94517701314423,
-3.84881143108739,-3.82766435633166,-3.79657451171058,-3.79316968208567,
-3.79192248935369,-3.79082197477453,-3.78962905374788,-3.78806764794247,
-3.78462816818222,-3.75636230042786,-3.74444863908848,-3.70251564154461,
-3.66436601142297,-3.6356582212257,-3.63284459407056,-3.63076550651394,
-3.62985675190409,-3.62918876984315,-3.6285654962427,-3.6277026290837,-3.62549510167175,
-3.59484061183983,-3.54261933495207,-3.50827714133197,-3.48855632216326,
-3.47824711353032,-3.4738802481785,-3.47056799467337,-3.46901652871813,
-3.46789493764059,-3.46678739537104,-3.46528563748001,-3.46235105681029,
-3.43920151261024,-3.42885175141428,-3.3496950636264,-3.3105005101393,-3.30822261330623,
-3.30727930826882,-3.30660503795583,-3.30598975707241,-3.30515793335222,
-3.3035393818741,-3.29123108981414,-3.20103188379539,-3.16650419057776,
-3.15575920909221,-3.15125607801153,-3.14888699257951,-3.14693917976173,
-3.14565534873104,-3.14447397626,-3.14296736835865,-3.13999944075464,-3.12246577289303,
-3.02299541359719,-2.99055402879725,-2.98598993881807,-2.98475916396203,
-2.98402274399093,-2.98336356084332,-2.98251503926993,-2.98075672743739,
-2.96933412776831,-2.87666251348363,-2.83321092591174,-2.82853559650572,
-2.82610078466645,-2.82404533456081,-2.82276522441222,-2.82158294491178,
-2.82006938032845,-2.81696556698497,-2.79745014349672,-2.79203852421539,
-2.77325061675747,-2.70223777430702,-2.67560264228216,-2.66391184551348,
-2.66229023919452,-2.66146931637408,-2.66081892501236,-2.66006727329548,
-2.65880091497487,-2.65429990751109,-2.55755637135215,-2.51081588477976,
-2.50341956840764,-2.50128959481028,-2.49998452362602,-2.49880198704553,
-2.49728576892938,-2.49416830593207,-2.47435509144533,-2.46884712381461,
-2.45592709430216,-2.37938272439594,-2.3451672256626,-2.34206615059194,
-2.33981980719672,-2.33888184857659,-2.33820859136882,-2.33759219959382,
-2.33675596467168,-2.33512024044937,-2.32234425885274,-2.31956925691279,
-2.31922798582844,-2.26071001490321,-2.18295413425186,-2.17948170413756,
-2.17789705401794,-2.17670477615157,-2.17558501850019,-2.17403614659422,
-2.17091599780379,-2.14176647354427,-2.12969103856988,-2.05681360748445,
-2.03037373286562,-2.01865824001209,-2.01688695171465,-2.01603592856054,
-2.01537650911459,-2.0146416243322,-2.01341747238458,-2.00892195781575,
-1.97734432841322,-1.89425190193827,-1.88289619612652,-1.85993098471858,
-1.85700321945561,-1.85550322624516,-1.85439614563031,-1.85319567339058,
-1.85156195369865,-1.84782074366267,-1.84279759363904,-1.81711854060672,
-1.77387153635517,-1.71013265430017,-1.70973583963201,-1.70904989344843,
-1.69607010992939,-1.69442716024068,-1.69358909100762,-1.6929722491954,
-1.69229943142584,-1.69136371791093,-1.68913041767247,-1.68605210125461,
-1.65231053568945,-1.61779096137798,-1.53939364852726,-1.53475049940659,
-1.53309496739072,-1.53194628043425,-1.53088361488174,-1.52944042066184,
-1.52667963041437,-1.50963100387274,-1.4712083935111,-1.38536091296174,
-1.37328446361084,-1.37149736185187,-1.37065235190876,-1.36999186518111,
-1.36926132743611,-1.36805668545317,-1.3638526398519,-1.33555526487758,
-1.24927803481731,-1.21504113622242,-1.21143406220145,-1.20998545731942,
-1.20878156113753,-1.2075507053953,-1.20579605508432,-1.20132456283697,
-1.14679701555565,-1.08506050590719,-1.07539727748638,-1.07203844495038,
-1.06514349730385,-1.06352564073989,-1.05062481200013,-1.04898461878447,
-1.04814724378296,-1.04753056705026,-1.04685757210219,-1.04592098544587,
-1.04375031904111,-1.0407455760875,-1.00847699734796,-0.9422377587332,-0.941400112120224,
-0.925726967205936,-0.915296816215335,-0.909685975295693,-0.908606304480574,
-0.891454919976999,-0.888506986584862,-0.887004626773872,-0.885823696792347,
-0.884510930295395,-0.882389979490946,-0.875039506142504,-0.86311575095035,
-0.818097840061453,-0.775445501820224,-0.729381807882283,-0.726650853413126,
-0.725707491712472,-0.725062177231477,-0.724469501574668,-0.723658901347221,
-0.722118480586721,-0.712512260016122,-0.694379890664134,-0.633906409190096,
-0.570322814450785,-0.566415723232065,-0.564877101131939,-0.563760026732863,
-0.562566183907004,-0.560971864090938,-0.557550342704471,-0.523826241750137,
-0.473709151203545,-0.407891756969277,-0.404252083875212,-0.403073094854276,
-0.402420672121827,-0.401829388378052,-0.401032328587121,-0.400182836402296,
-0.396518897683616,-0.390677591280717,-0.371780069704382,-0.343698357389322,
-0.316739747637345,-0.285973126794533,-0.282585089649083,-0.247212079072741,
-0.243940513122593,-0.242353981159195,-0.241224101376784,-0.240155374211044,
-0.238667022523693,-0.237067556795919,-0.234482650685707,-0.216375519981168,
-0.182169082583788,-0.169702923985518,-0.156297498125755,-0.0981423875346418,
-0.0829063260632253,-0.0809981108166153,-0.0801301315670966,-0.0794662546876113,
-0.0787470322045957,-0.0775929299122855,-0.0762385391647315,-0.0662546035110392,
-0.000957508011488563),.UNSPECIFIED.);
#870=B_SPLINE_CURVE_WITH_KNOTS('',3,(#62465,#62466,#62467,#62468,#62469,
#62470,#62471,#62472,#62473,#62474,#62475,#62476,#62477,#62478,#62479,#62480,
#62481,#62482,#62483,#62484,#62485,#62486,#62487,#62488,#62489,#62490,#62491,
#62492,#62493,#62494,#62495,#62496,#62497,#62498,#62499,#62500,#62501,#62502,
#62503,#62504,#62505,#62506,#62507,#62508,#62509,#62510,#62511,#62512,#62513,
#62514,#62515,#62516,#62517,#62518,#62519,#62520,#62521,#62522,#62523,#62524,
#62525,#62526,#62527,#62528,#62529,#62530,#62531,#62532,#62533,#62534,#62535,
#62536,#62537,#62538,#62539,#62540,#62541,#62542,#62543,#62544,#62545,#62546,
#62547,#62548,#62549,#62550,#62551,#62552,#62553,#62554,#62555,#62556,#62557,
#62558,#62559,#62560,#62561,#62562,#62563,#62564,#62565,#62566,#62567,#62568,
#62569,#62570,#62571,#62572,#62573,#62574,#62575,#62576,#62577,#62578,#62579,
#62580,#62581,#62582,#62583,#62584,#62585,#62586,#62587,#62588,#62589,#62590,
#62591,#62592,#62593,#62594,#62595,#62596,#62597,#62598,#62599,#62600,#62601,
#62602,#62603,#62604,#62605,#62606,#62607,#62608,#62609,#62610,#62611,#62612,
#62613,#62614,#62615,#62616,#62617,#62618,#62619,#62620,#62621,#62622,#62623,
#62624,#62625,#62626,#62627,#62628,#62629,#62630,#62631,#62632,#62633,#62634,
#62635,#62636,#62637,#62638,#62639,#62640,#62641,#62642,#62643,#62644,#62645,
#62646,#62647,#62648,#62649,#62650,#62651,#62652,#62653,#62654,#62655,#62656,
#62657,#62658,#62659,#62660,#62661,#62662,#62663,#62664,#62665,#62666,#62667,
#62668,#62669,#62670,#62671,#62672,#62673,#62674,#62675,#62676,#62677,#62678,
#62679,#62680,#62681,#62682,#62683,#62684,#62685,#62686,#62687,#62688,#62689,
#62690,#62691,#62692,#62693,#62694,#62695,#62696,#62697,#62698,#62699,#62700,
#62701,#62702,#62703,#62704,#62705,#62706,#62707,#62708,#62709,#62710,#62711,
#62712,#62713,#62714,#62715,#62716,#62717,#62718,#62719,#62720,#62721,#62722,
#62723,#62724,#62725,#62726,#62727,#62728,#62729,#62730,#62731,#62732,#62733,
#62734,#62735,#62736,#62737,#62738,#62739,#62740,#62741,#62742,#62743,#62744,
#62745,#62746,#62747,#62748,#62749,#62750,#62751,#62752,#62753,#62754,#62755,
#62756,#62757,#62758,#62759,#62760,#62761,#62762,#62763,#62764,#62765,#62766,
#62767,#62768,#62769,#62770,#62771,#62772,#62773,#62774,#62775,#62776,#62777,
#62778,#62779,#62780,#62781,#62782,#62783,#62784,#62785,#62786,#62787,#62788,
#62789,#62790,#62791,#62792,#62793,#62794,#62795,#62796,#62797,#62798,#62799,
#62800,#62801,#62802,#62803,#62804,#62805,#62806,#62807,#62808,#62809,#62810,
#62811,#62812,#62813,#62814,#62815,#62816,#62817,#62818,#62819,#62820,#62821,
#62822,#62823,#62824,#62825,#62826,#62827,#62828,#62829,#62830,#62831,#62832,
#62833,#62834,#62835,#62836,#62837,#62838,#62839,#62840,#62841,#62842,#62843,
#62844,#62845,#62846,#62847,#62848,#62849,#62850,#62851,#62852,#62853,#62854,
#62855,#62856,#62857,#62858,#62859,#62860,#62861,#62862,#62863,#62864,#62865,
#62866,#62867,#62868,#62869,#62870,#62871,#62872,#62873,#62874,#62875,#62876,
#62877,#62878,#62879,#62880,#62881,#62882,#62883,#62884,#62885,#62886,#62887,
#62888,#62889,#62890,#62891,#62892,#62893,#62894,#62895,#62896,#62897,#62898,
#62899,#62900,#62901,#62902,#62903,#62904,#62905,#62906,#62907,#62908,#62909,
#62910,#62911,#62912,#62913,#62914,#62915,#62916,#62917,#62918,#62919,#62920,
#62921,#62922,#62923,#62924,#62925,#62926,#62927,#62928,#62929,#62930,#62931,
#62932,#62933,#62934,#62935,#62936,#62937,#62938,#62939,#62940,#62941,#62942,
#62943,#62944,#62945,#62946,#62947,#62948,#62949,#62950,#62951,#62952,#62953,
#62954,#62955,#62956,#62957,#62958,#62959,#62960,#62961,#62962,#62963,#62964,
#62965,#62966,#62967,#62968,#62969,#62970,#62971,#62972,#62973,#62974,#62975,
#62976,#62977,#62978,#62979,#62980,#62981,#62982,#62983,#62984,#62985,#62986,
#62987,#62988,#62989,#62990,#62991,#62992,#62993,#62994,#62995,#62996),
 .UNSPECIFIED.,.F.,.F.,(4,2,2,2,2,2,2,2,2,2,2,2,2,2,2,2,2,2,2,2,2,2,2,2,
2,2,2,2,2,2,2,2,2,2,2,2,2,2,2,2,2,2,2,2,2,2,2,2,2,2,2,2,2,2,2,2,2,2,2,2,
2,2,2,2,2,2,2,2,2,2,2,2,2,2,2,2,2,2,2,2,2,2,2,2,2,2,2,2,2,2,2,2,2,2,2,2,
2,2,2,2,2,2,2,2,2,2,2,2,2,2,2,2,2,2,2,2,2,2,2,2,2,2,2,2,2,2,2,2,2,2,2,2,
2,2,2,2,2,2,2,2,2,2,2,2,2,2,2,2,2,2,2,2,2,2,2,2,2,2,2,2,2,2,2,2,2,2,2,2,
2,2,2,2,2,2,2,2,2,2,2,2,2,2,2,2,2,2,2,2,2,2,2,2,2,2,2,2,2,2,2,2,2,2,2,2,
2,2,2,2,2,2,2,2,2,2,2,2,2,2,2,2,2,2,2,2,2,2,2,2,2,2,2,2,2,2,2,2,2,2,2,2,
2,2,2,2,2,2,2,2,2,2,2,2,2,2,2,2,2,2,2,2,2,2,2,2,2,4),(-4.06151371944992,
-3.98512772967926,-3.98259757323507,-3.98102106276342,-3.97954928378014,
-3.97848288548137,-3.97734652293743,-3.97573612284057,-3.97138910350108,
-3.89794537359405,-3.88348754773806,-3.86993036953823,-3.83605836290238,
-3.82096867995507,-3.81953415603881,-3.81864665669649,-3.81782229926178,
-3.81717159195894,-3.81651855312469,-3.81533662561074,-3.81167493976928,
-3.74443235264209,-3.70806150464538,-3.67883633606832,-3.66713263832581,
-3.65988550560989,-3.65831945020771,-3.65685522166278,-3.65578982277248,
-3.65465030490257,-3.65302839201582,-3.64860746349398,-3.58004365421,-3.52975879651499,
-3.50097983344832,-3.49682941166829,-3.49594779392835,-3.49512765855346,
-3.49453377962682,-3.49389282570049,-3.49277103518101,-3.48955353550529,
-3.43112016523926,-3.38181983635296,-3.36197267371988,-3.33938729313599,
-3.33599700736088,-3.33440605332477,-3.33321262385723,-3.33209440201768,
-3.3305517840918,-3.32662173070605,-3.26610327247955,-3.19997768644188,
-3.1827970314216,-3.17478830020052,-3.17323279859951,-3.17241891013092,
-3.17182577239953,-3.17118187832659,-3.17024380923783,-3.16754983918248,
-3.12502988638493,-3.06921765356264,-3.02194919054577,-3.01704106414756,
-3.01340077806828,-3.01176660624983,-3.01056585285235,-3.00945854786686,
-3.00795830378961,-3.00503019691679,-2.98206764730743,-2.96740115683939,
-2.89860465057851,-2.87601356231537,-2.85283235039043,-2.8508450987227,
-2.84992370337539,-2.84925338686956,-2.84863308923869,-2.84778194261741,
-2.8456435003422,-2.81934656432651,-2.74530862085288,-2.69911020929803,
-2.69426584937583,-2.69065771016551,-2.68903300826618,-2.68783391781903,
-2.68672439773346,-2.68521541659526,-2.68148237467049,-2.63733823261918,
-2.60715733754165,-2.55333643021045,-2.53893405303632,-2.52936702454637,
-2.52782326621996,-2.52701850628826,-2.52636310908942,-2.52569743251024,
-2.52445297841195,-2.52028083215,-2.4176797366519,-2.37147597069743,-2.36782265180503,
-2.36620466940427,-2.36500685952995,-2.36389590594072,-2.36238094571682,
-2.35861264328418,-2.31206555053525,-2.28669448063043,-2.24030580974222,
-2.2166598042577,-2.20661172753485,-2.20504866077235,-2.20423992187869,
-2.20364746147161,-2.203001236692,-2.20185294651217,-2.19844621702278,-2.14086705997772,
-2.09113097900259,-2.06192773154901,-2.04730029167468,-2.04465002230972,
-2.04323024984365,-2.04217001209396,-2.04084049672412,-2.0386014520073,
-2.03107154402968,-2.00528069771464,-1.9618158144137,-1.88738490256459,
-1.88336335739162,-1.88213670630677,-1.88147464932939,-1.88081897229186,
-1.88000827713126,-1.87843602751664,-1.86815282362126,-1.84325958684407,
-1.76344045258801,-1.75053923520712,-1.74506547906303,-1.7253518505943,
-1.7222388183663,-1.72072342160264,-1.71954092035503,-1.71823527210264,
-1.71610296578969,-1.70868502493469,-1.66170449585513,-1.60873048778164,
-1.56306618116939,-1.56032773237834,-1.55938326581525,-1.55873762789598,
-1.55814500055396,-1.55733498271432,-1.55576590239949,-1.54556441064946,
-1.52108085455418,-1.43728854171577,-1.4255493091801,-1.40286543265996,
-1.39994794362398,-1.39845057231878,-1.39734413242912,-1.39614310346215,
-1.39450639054982,-1.39074855873075,-1.30813586907975,-1.25149220788208,
-1.24963054633628,-1.23879017245977,-1.23705885398049,-1.23621572310077,
-1.23555720283631,-1.23483267260556,-1.23362942733197,-1.23218596063727,
-1.22933614284275,-1.19998323530304,-1.13593269534862,-1.0811690989687,
-1.07730704232857,-1.07577601865248,-1.07466089641787,-1.07346578476392,
-1.07186396755439,-1.06829927604034,-1.01937261360948,-0.943968968419398,
-0.916784754200208,-0.914630825293692,-0.913777075686765,-0.913156135410346,
-0.912486388015048,-0.911586393908492,-0.909635882158193,-0.906963362616315,
-0.90037239370779,-0.877396017037223,-0.829282053511521,-0.78429203997342,
-0.776324157434589,-0.757221241323316,-0.754136664865288,-0.752626856172148,
-0.75144493837064,-0.750136070607724,-0.747989731015974,-0.740436351969627,
-0.714901060391101,-0.672615355651724,-0.628293906667524,-0.618465867825959,
-0.614601332848636,-0.609743060308636,-0.60836457801826,-0.593725152995518,
-0.592025549668843,-0.591173008688977,-0.590552381900024,-0.589882402487084,
-0.589219044505901,-0.587607504730847,-0.576051348864818,-0.563162145589931,
-0.522875005716314,-0.452613780709759,-0.451496070038381,-0.43441463991666,
-0.431470271181607,-0.429968606292793,-0.428787672356814,-0.427474332769528,
-0.425307895873875,-0.417554179171333,-0.366824468445903,-0.342463153414464,
-0.316259115670658,-0.272343795696258,-0.269608474124362,-0.268664442477199,
-0.268018914218223,-0.267426237621165,-0.266795281734187,-0.26600197410379,
-0.263093698105171,-0.230492159776364,-0.209351413165981,-0.133776513955677,
-0.131677902535982,-0.111966237724981,-0.10885325950652,-0.107337858498801,
-0.106155340078874,-0.104849658754597,-0.102717266555907,-0.0952987163971223,
-0.048312173861197,-0.000957996441563316),.UNSPECIFIED.);
#871=B_SPLINE_CURVE_WITH_KNOTS('',3,(#62998,#62999,#63000,#63001,#63002,
#63003,#63004,#63005,#63006,#63007,#63008,#63009,#63010,#63011,#63012,#63013,
#63014,#63015,#63016,#63017,#63018,#63019,#63020,#63021,#63022,#63023,#63024,
#63025,#63026,#63027,#63028,#63029,#63030,#63031,#63032,#63033,#63034,#63035,
#63036,#63037,#63038,#63039,#63040,#63041,#63042,#63043,#63044,#63045,#63046,
#63047,#63048,#63049,#63050,#63051,#63052,#63053,#63054,#63055,#63056,#63057,
#63058,#63059,#63060,#63061,#63062,#63063,#63064,#63065,#63066,#63067,#63068,
#63069,#63070,#63071,#63072,#63073,#63074,#63075,#63076,#63077,#63078,#63079,
#63080,#63081,#63082,#63083,#63084,#63085,#63086,#63087,#63088,#63089,#63090,
#63091,#63092,#63093,#63094,#63095,#63096,#63097,#63098,#63099,#63100,#63101,
#63102,#63103,#63104,#63105,#63106,#63107,#63108,#63109,#63110,#63111,#63112,
#63113,#63114,#63115,#63116,#63117,#63118,#63119,#63120,#63121,#63122,#63123,
#63124,#63125,#63126,#63127,#63128,#63129,#63130,#63131,#63132,#63133,#63134,
#63135,#63136,#63137,#63138,#63139,#63140,#63141,#63142,#63143,#63144,#63145,
#63146,#63147,#63148,#63149,#63150,#63151,#63152,#63153,#63154,#63155,#63156,
#63157,#63158,#63159,#63160,#63161,#63162,#63163,#63164,#63165,#63166,#63167,
#63168,#63169,#63170,#63171,#63172,#63173,#63174,#63175,#63176,#63177,#63178,
#63179,#63180,#63181,#63182,#63183,#63184,#63185,#63186,#63187,#63188,#63189,
#63190,#63191,#63192,#63193,#63194,#63195,#63196,#63197,#63198,#63199,#63200,
#63201,#63202,#63203,#63204,#63205,#63206,#63207,#63208,#63209,#63210,#63211,
#63212,#63213,#63214,#63215,#63216,#63217,#63218,#63219,#63220,#63221,#63222,
#63223,#63224,#63225,#63226,#63227,#63228,#63229,#63230,#63231,#63232,#63233,
#63234,#63235,#63236,#63237,#63238,#63239,#63240,#63241,#63242,#63243,#63244,
#63245,#63246,#63247,#63248,#63249,#63250,#63251,#63252,#63253,#63254,#63255,
#63256,#63257,#63258,#63259,#63260,#63261,#63262,#63263,#63264,#63265,#63266,
#63267,#63268,#63269,#63270,#63271,#63272,#63273,#63274,#63275,#63276,#63277,
#63278,#63279,#63280,#63281,#63282,#63283,#63284,#63285,#63286,#63287,#63288,
#63289,#63290,#63291,#63292,#63293,#63294,#63295,#63296,#63297,#63298,#63299,
#63300,#63301,#63302,#63303,#63304,#63305,#63306,#63307,#63308,#63309,#63310,
#63311,#63312,#63313,#63314,#63315,#63316,#63317,#63318,#63319,#63320,#63321,
#63322,#63323,#63324,#63325,#63326,#63327,#63328,#63329,#63330,#63331,#63332,
#63333,#63334,#63335,#63336,#63337,#63338,#63339,#63340,#63341,#63342,#63343,
#63344,#63345,#63346,#63347,#63348,#63349,#63350,#63351,#63352,#63353,#63354,
#63355,#63356,#63357,#63358,#63359,#63360,#63361,#63362,#63363,#63364,#63365,
#63366,#63367,#63368,#63369,#63370,#63371,#63372,#63373,#63374,#63375,#63376,
#63377,#63378,#63379,#63380,#63381,#63382,#63383,#63384,#63385,#63386,#63387,
#63388,#63389,#63390,#63391,#63392,#63393,#63394,#63395,#63396,#63397,#63398,
#63399,#63400,#63401,#63402,#63403,#63404,#63405,#63406,#63407,#63408,#63409,
#63410,#63411,#63412,#63413,#63414,#63415,#63416,#63417,#63418,#63419,#63420,
#63421,#63422,#63423,#63424,#63425,#63426,#63427,#63428,#63429,#63430,#63431,
#63432,#63433,#63434,#63435,#63436,#63437,#63438,#63439,#63440,#63441,#63442,
#63443,#63444,#63445,#63446,#63447,#63448,#63449,#63450,#63451,#63452,#63453,
#63454,#63455,#63456,#63457,#63458,#63459,#63460,#63461,#63462,#63463,#63464,
#63465,#63466,#63467,#63468,#63469,#63470,#63471,#63472,#63473,#63474,#63475,
#63476,#63477,#63478,#63479,#63480,#63481,#63482,#63483,#63484,#63485,#63486,
#63487,#63488,#63489,#63490,#63491,#63492,#63493,#63494,#63495,#63496,#63497,
#63498,#63499,#63500,#63501,#63502,#63503,#63504,#63505,#63506,#63507,#63508,
#63509,#63510,#63511,#63512,#63513,#63514,#63515,#63516,#63517,#63518,#63519,
#63520,#63521,#63522,#63523,#63524,#63525,#63526,#63527,#63528,#63529),
 .UNSPECIFIED.,.F.,.F.,(4,2,2,2,2,2,2,2,2,2,2,2,2,2,2,2,2,2,2,2,2,2,2,2,
2,2,2,2,2,2,2,2,2,2,2,2,2,2,2,2,2,2,2,2,2,2,2,2,2,2,2,2,2,2,2,2,2,2,2,2,
2,2,2,2,2,2,2,2,2,2,2,2,2,2,2,2,2,2,2,2,2,2,2,2,2,2,2,2,2,2,2,2,2,2,2,2,
2,2,2,2,2,2,2,2,2,2,2,2,2,2,2,2,2,2,2,2,2,2,2,2,2,2,2,2,2,2,2,2,2,2,2,2,
2,2,2,2,2,2,2,2,2,2,2,2,2,2,2,2,2,2,2,2,2,2,2,2,2,2,2,2,2,2,2,2,2,2,2,2,
2,2,2,2,2,2,2,2,2,2,2,2,2,2,2,2,2,2,2,2,2,2,2,2,2,2,2,2,2,2,2,2,2,2,2,2,
2,2,2,2,2,2,2,2,2,2,2,2,2,2,2,2,2,2,2,2,2,2,2,2,2,2,2,2,2,2,2,2,2,2,2,2,
2,2,2,2,2,2,2,2,2,2,2,2,2,2,2,2,2,2,2,2,2,2,2,2,2,4),(-4.05932996479639,
-4.00703982614242,-4.00563635672431,-4.00476205512462,-4.00410446570224,
-4.00343791005599,-4.00281349106476,-4.00194531211603,-4.00018194533193,
-3.98334890264101,-3.97717005467382,-3.96452440677062,-3.94885813133185,
-3.93917667015674,-3.93067217108731,-3.91372058995674,-3.86700643780568,
-3.84888488142342,-3.84512283213122,-3.84348601181196,-3.84228556881662,
-3.84118013424965,-3.83968482992644,-3.83677343411346,-3.81421717048654,
-3.7448386342237,-3.71946790158547,-3.69429661730345,-3.68743692680702,
-3.68329543363733,-3.68241453214386,-3.68175451860975,-3.68108663303139,
-3.68046422333629,-3.67960370664482,-3.67740823265023,-3.64752124479994,
-3.62358499529834,-3.54363701481488,-3.52575002923593,-3.52244444515951,
-3.52089206562346,-3.5197053325659,-3.518576781307,-3.51667495397654,-3.51164241961022,
-3.43101402734289,-3.3833267904943,-3.36853178856557,-3.3637154724233,-3.36055970608928,
-3.35948786740035,-3.35887336566448,-3.35821371367795,-3.35737196586634,
-3.35559983403549,-3.34384623511312,-3.34216037694053,-3.33987442472209,
-3.31806982684442,-3.2567797742728,-3.23260411217912,-3.20351352799144,
-3.20006783564887,-3.1984887786853,-3.19729797129602,-3.1961775853651,-3.19462465320913,
-3.19062858379612,-3.1255126203354,-3.07076593674566,-3.04257219390286,
-3.03978816080786,-3.03774392632649,-3.03684310929708,-3.03617358557071,
-3.03555347672019,-3.0347017888063,-3.03255783649128,-3.00587177076776,
-2.91961628152862,-2.88471028454306,-2.8785204599378,-2.87652693090985,
-2.87525284681774,-2.87406186657044,-2.87250837019673,-2.86910801587083,
-2.84201495880432,-2.82863283523943,-2.75956901914329,-2.71822665751334,
-2.71638673408371,-2.71492263703646,-2.71413901188669,-2.71354783552038,
-2.71280228181256,-2.7115290054986,-2.70709647026816,-2.62509949603952,
-2.55897030408486,-2.55520132234405,-2.55356332929277,-2.55236273374501,
-2.5512576547487,-2.54976358350078,-2.5468567941117,-2.52442209582214,-2.42991088108071,
-2.39472555220532,-2.39264219885133,-2.39173297694854,-2.39106519613794,
-2.39044251849916,-2.38958108590613,-2.38738042625372,-2.35714166928091,
-2.31807715787911,-2.27996889340665,-2.2357947233799,-2.23248214006755,
-2.23092828926107,-2.22974121118285,-2.2286129170372,-2.22671293677503,
-2.22169306693046,-2.22048316405023,-2.1165075637908,-2.07238023472366,
-2.07012748202891,-2.06918867542096,-2.06851547433938,-2.06789961569855,
-2.06706479296895,-2.06543386796836,-2.05277593847135,-2.0522653880507,
-2.04923681714071,-2.04422863701577,-2.04117262619971,-2.03108909889942,
-1.96173427887808,-1.94283109231867,-1.91339387453022,-1.91026685162819,
-1.90871655690413,-1.90759670367404,-1.90640519080956,-1.90482303626466,
-1.90136197853318,-1.82948368626787,-1.75250924151542,-1.74821170334011,
-1.74695323335772,-1.74628492799194,-1.74563631421854,-1.74483947506058,
-1.74333211891183,-1.73457834702299,-1.71585620321083,-1.67078418641421,
-1.59263607492646,-1.5879148235483,-1.58624794881998,-1.58509631753747,
-1.58403474176386,-1.5825987844117,-1.57987104296965,-1.56358086213379,
-1.52950955754347,-1.4368886148485,-1.42632976694317,-1.42461269646842,
-1.42377253323136,-1.42311448054266,-1.42237357930586,-1.42112211651503,
-1.41633117323276,-1.38085949954155,-1.28632861348975,-1.28164732181547,
-1.26700715675596,-1.26445289308245,-1.26291276883899,-1.26172354668411,
-1.2604685750393,-1.25866846685609,-1.25648906401622,-1.25247510317897,
-1.21892622159933,-1.1245112041976,-1.12119813395443,-1.10395819216122,
-1.10198623560193,-1.1011066286737,-1.10044096875315,-1.09972701367949,
-1.09859604350529,-1.09497895173494,-1.07311070175187,-1.04867700039954,
-1.00948764941425,-0.94608805912035,-0.942181673646234,-0.940643291526206,
-0.939526378121796,-0.938358169899059,-0.936813034429958,-0.935105563345423,
-0.9322614742094,-0.926482301456736,-0.835552549137356,-0.790903601742188,
-0.78085098166428,-0.779159189046723,-0.778324030107459,-0.777666420327303,
-0.776922257893027,-0.775656496547922,-0.770705761192523,-0.747332565313931,
-0.696882939047241,-0.667674657542121,-0.623166883433151,-0.619428536663269,
-0.617918801550849,-0.616809227325592,-0.615634522203932,-0.614058427383091,
-0.612309915683628,-0.609366856694525,-0.603313429467553,-0.587290614074345,
-0.567986456094639,-0.518152993509329,-0.460742313680543,-0.457316669132169,
-0.456165675239484,-0.455518912550233,-0.454926581013473,-0.454118946596125,
-0.452561117978147,-0.4426447448664,-0.419858258998069,-0.374874099501909,
-0.350830450129026,-0.300214648501835,-0.297004049647198,-0.295432608608637,
-0.29430682899995,-0.293173060519748,-0.291670417036584,-0.288596339061355,
-0.284616940313561,-0.275520234167969,-0.248733762062387,-0.144802768233036,
-0.1354406663,-0.133806334307815,-0.132971565735155,-0.132313828212072,
-0.131569049363713,-0.130301129756311,-0.125328418052534,-0.101900466247598,
-0.000958141822577317),.UNSPECIFIED.);
#872=B_SPLINE_CURVE_WITH_KNOTS('',3,(#63531,#63532,#63533,#63534,#63535,
#63536,#63537,#63538,#63539,#63540,#63541,#63542,#63543,#63544,#63545,#63546,
#63547,#63548,#63549,#63550,#63551,#63552,#63553,#63554,#63555,#63556,#63557,
#63558,#63559,#63560,#63561,#63562,#63563,#63564,#63565,#63566,#63567,#63568,
#63569,#63570,#63571,#63572,#63573,#63574,#63575,#63576,#63577,#63578,#63579,
#63580,#63581,#63582,#63583,#63584,#63585,#63586,#63587,#63588,#63589,#63590,
#63591,#63592,#63593,#63594,#63595,#63596,#63597,#63598,#63599,#63600,#63601,
#63602,#63603,#63604,#63605,#63606,#63607,#63608,#63609,#63610,#63611,#63612,
#63613,#63614,#63615,#63616,#63617,#63618,#63619,#63620,#63621,#63622,#63623,
#63624,#63625,#63626,#63627,#63628,#63629,#63630,#63631,#63632,#63633,#63634,
#63635,#63636,#63637,#63638,#63639,#63640,#63641,#63642,#63643,#63644,#63645,
#63646,#63647,#63648),.UNSPECIFIED.,.F.,.F.,(4,3,3,3,3,3,3,3,3,3,3,3,3,
3,3,3,3,3,3,3,3,3,3,3,3,3,3,3,3,3,3,3,3,3,3,3,3,3,3,4),(248.185819633594,
248.353498579193,248.521277971523,248.689527055698,248.77731295494,248.9427757676,
249.107922054166,249.274967880302,249.440034186732,249.60806977272,249.776105358708,
249.941568171368,250.106714457934,250.27376028407,250.4388265905,250.606862176488,
250.774897762476,250.940360575136,251.105506861702,251.272552687838,251.437618994268,
251.605654580256,251.773690166244,251.939152978904,252.10429926547,252.271345091606,
252.436411398036,252.604446984024,252.772482570012,252.937945382672,253.103091669238,
253.270137495374,253.435203801804,253.603239387792,253.77127497378,253.935826065977,
254.100044847577,254.264077257094,254.428142795537,254.469004940774),
 .UNSPECIFIED.);
#873=B_SPLINE_CURVE_WITH_KNOTS('',3,(#63650,#63651,#63652,#63653,#63654,
#63655,#63656,#63657,#63658,#63659,#63660,#63661,#63662,#63663,#63664,#63665,
#63666,#63667,#63668,#63669,#63670,#63671,#63672,#63673,#63674,#63675,#63676,
#63677,#63678,#63679,#63680,#63681,#63682,#63683,#63684,#63685,#63686,#63687,
#63688,#63689,#63690,#63691,#63692,#63693,#63694,#63695,#63696,#63697,#63698,
#63699,#63700,#63701,#63702,#63703,#63704,#63705,#63706,#63707,#63708,#63709,
#63710,#63711,#63712,#63713,#63714,#63715,#63716,#63717,#63718,#63719,#63720,
#63721,#63722,#63723,#63724,#63725,#63726,#63727,#63728,#63729,#63730,#63731,
#63732,#63733,#63734,#63735,#63736,#63737,#63738,#63739,#63740,#63741,#63742,
#63743,#63744,#63745,#63746,#63747,#63748,#63749,#63750,#63751,#63752,#63753,
#63754,#63755,#63756,#63757,#63758,#63759,#63760,#63761,#63762,#63763,#63764,
#63765,#63766,#63767,#63768,#63769,#63770,#63771,#63772,#63773,#63774,#63775,
#63776,#63777,#63778,#63779,#63780,#63781,#63782,#63783,#63784,#63785,#63786,
#63787,#63788,#63789,#63790,#63791,#63792,#63793,#63794,#63795,#63796,#63797,
#63798,#63799,#63800,#63801,#63802,#63803,#63804,#63805,#63806,#63807,#63808,
#63809,#63810,#63811,#63812,#63813,#63814,#63815,#63816,#63817,#63818,#63819,
#63820,#63821,#63822,#63823,#63824,#63825,#63826,#63827,#63828,#63829,#63830,
#63831,#63832,#63833,#63834,#63835,#63836,#63837,#63838,#63839,#63840,#63841,
#63842,#63843,#63844,#63845,#63846,#63847,#63848,#63849,#63850,#63851,#63852,
#63853,#63854,#63855,#63856,#63857,#63858,#63859,#63860,#63861,#63862,#63863,
#63864,#63865,#63866,#63867,#63868,#63869,#63870,#63871,#63872,#63873,#63874,
#63875,#63876,#63877,#63878,#63879,#63880,#63881,#63882,#63883,#63884,#63885,
#63886,#63887,#63888,#63889,#63890,#63891,#63892,#63893,#63894,#63895,#63896,
#63897,#63898,#63899,#63900,#63901,#63902,#63903,#63904,#63905,#63906,#63907,
#63908,#63909,#63910,#63911,#63912,#63913,#63914,#63915,#63916,#63917,#63918,
#63919,#63920,#63921,#63922,#63923,#63924,#63925,#63926,#63927,#63928,#63929,
#63930,#63931,#63932,#63933,#63934,#63935,#63936,#63937,#63938,#63939,#63940,
#63941,#63942,#63943,#63944,#63945,#63946,#63947,#63948,#63949,#63950,#63951,
#63952,#63953,#63954,#63955,#63956,#63957,#63958,#63959,#63960,#63961,#63962,
#63963,#63964,#63965,#63966,#63967,#63968,#63969,#63970,#63971,#63972,#63973,
#63974,#63975,#63976,#63977,#63978,#63979,#63980,#63981,#63982,#63983,#63984,
#63985,#63986,#63987,#63988,#63989,#63990,#63991,#63992,#63993,#63994,#63995,
#63996,#63997,#63998,#63999,#64000,#64001,#64002,#64003,#64004,#64005,#64006,
#64007,#64008,#64009,#64010,#64011,#64012,#64013,#64014,#64015,#64016,#64017,
#64018,#64019,#64020,#64021,#64022,#64023,#64024,#64025,#64026,#64027,#64028,
#64029,#64030,#64031,#64032,#64033,#64034,#64035,#64036,#64037,#64038,#64039,
#64040,#64041,#64042,#64043,#64044,#64045,#64046,#64047,#64048,#64049,#64050,
#64051,#64052,#64053,#64054,#64055,#64056,#64057,#64058,#64059,#64060,#64061,
#64062,#64063,#64064,#64065,#64066,#64067,#64068,#64069,#64070,#64071,#64072,
#64073,#64074,#64075,#64076,#64077,#64078,#64079,#64080,#64081,#64082,#64083,
#64084,#64085,#64086,#64087,#64088,#64089,#64090,#64091,#64092,#64093,#64094,
#64095,#64096,#64097,#64098,#64099,#64100,#64101,#64102,#64103,#64104,#64105,
#64106,#64107,#64108,#64109,#64110,#64111,#64112,#64113,#64114,#64115,#64116,
#64117,#64118,#64119,#64120,#64121,#64122,#64123,#64124,#64125,#64126,#64127,
#64128,#64129,#64130,#64131,#64132,#64133,#64134,#64135,#64136,#64137,#64138,
#64139,#64140,#64141,#64142,#64143,#64144,#64145,#64146,#64147,#64148,#64149,
#64150,#64151,#64152,#64153,#64154,#64155,#64156,#64157,#64158,#64159,#64160,
#64161,#64162,#64163,#64164,#64165,#64166,#64167,#64168,#64169,#64170,#64171,
#64172,#64173,#64174,#64175),.UNSPECIFIED.,.F.,.F.,(4,2,2,2,2,2,2,2,2,2,
2,2,2,2,2,2,2,2,2,2,2,2,2,2,2,2,2,2,2,2,2,2,2,2,2,2,2,2,2,2,2,2,2,2,2,2,
2,2,2,2,2,2,2,2,2,2,2,2,2,2,2,2,2,2,2,2,2,2,2,2,2,2,2,2,2,2,2,2,2,2,2,2,
2,2,2,2,2,2,2,2,2,2,2,2,2,2,2,2,2,2,2,2,2,2,2,2,2,2,2,2,2,2,2,2,2,2,2,2,
2,2,2,2,2,2,2,2,2,2,2,2,2,2,2,2,2,2,2,2,2,2,2,2,2,2,2,2,2,2,2,2,2,2,2,2,
2,2,2,2,2,2,2,2,2,2,2,2,2,2,2,2,2,2,2,2,2,2,2,2,2,2,2,2,2,2,2,2,2,2,2,2,
2,2,2,2,2,2,2,2,2,2,2,2,2,2,2,2,2,2,2,2,2,2,2,2,2,2,2,2,2,2,2,2,2,2,2,2,
2,2,2,2,2,2,2,2,2,2,2,2,2,2,2,2,2,2,2,2,2,2,2,2,2,2,2,2,2,2,2,2,2,2,2,2,
4),(-4.06003765655308,-4.00423323853758,-3.9775885287128,-3.96592804501213,
-3.96430790737641,-3.96348747859677,-3.96283135961083,-3.96207770015301,
-3.9608019878455,-3.95621022710372,-3.86881393128048,-3.84672550835414,
-3.81256410512827,-3.80551531040521,-3.80396309607576,-3.80278850837579,
-3.80159301238478,-3.8004797286445,-3.79895464865576,-3.79512537359173,
-3.74366120825391,-3.70737379642536,-3.67097216501958,-3.65204456085692,
-3.6431898036797,-3.641677865137,-3.64088009303478,-3.64023149272111,-3.63956388833052,
-3.63830872623847,-3.63403976594128,-3.55922856444301,-3.52535529128013,
-3.50307352407948,-3.48431666131623,-3.48148792495554,-3.4803091431868,
-3.47911136883844,-3.47800156490333,-3.47648989053705,-3.47273849798057,
-3.42731063642589,-3.35677709939312,-3.32467510535317,-3.32013882191028,
-3.31891106924827,-3.3181755486514,-3.31751656887546,-3.31666749097112,
-3.31490513377514,-3.30337968200422,-3.26168742496592,-3.17085396910647,
-3.16431232364196,-3.15972055188708,-3.15795023183699,-3.15671643151351,
-3.15551586057287,-3.15407868472972,-3.1505385252423,-3.1187928567134,-3.03616188309034,
-2.99915565177217,-2.99688171779778,-2.99593930368405,-2.99526539983568,
-2.99465025836384,-2.99381834563154,-2.99219880649293,-2.97985150458162,
-2.95135294555784,-2.89169905793147,-2.84177160305828,-2.8386478302614,
-2.83612795362345,-2.8347420099736,-2.83368260110756,-2.83251980208,-2.83044709474672,
-2.82424815698305,-2.71192978605101,-2.67933551979252,-2.6747599490895,
-2.67352829696475,-2.67279179983287,-2.67213284323163,-2.67128501445439,
-2.66952955211513,-2.65816254402649,-2.65472269592798,-2.64805313184364,
-2.64466083950641,-2.5533927976318,-2.520640056549,-2.51468736079452,-2.5127225879152,
-2.51145445534932,-2.51026016356363,-2.50868949525341,-2.50603174446617,
-2.4894615691651,-2.39450738704549,-2.36756162523348,-2.35366808946732,
-2.35138621218681,-2.35044231620384,-2.34976800368468,-2.34915295815784,
-2.34832184192608,-2.34670580799768,-2.33446057106395,-2.2937078594994,
-2.24108978181261,-2.21934384448944,-2.19646360760062,-2.19167904642637,
-2.18987462004845,-2.18864092952215,-2.18743948903697,-2.18600010460584,
-2.18258400239798,-2.15361988057456,-2.08468387265484,-2.03065533724721,
-2.02885595946918,-2.02797856515932,-2.02735141510452,-2.02668574155726,
-2.02579090960959,-2.02378879854155,-1.96663009573278,-1.92865181113395,
-1.87266012022273,-1.86878835266972,-1.86725572573166,-1.86614022545783,
-1.8649454521817,-1.86334537567978,-1.85978985331268,-1.80752926875823,
-1.72232565715337,-1.71954689995726,-1.70761040629583,-1.7058293196915,
-1.70497633006638,-1.70431662365299,-1.70358271973112,-1.70236311598163,
-1.697915440332,-1.66692755409178,-1.59256917397857,-1.59133912298184,-1.57289532837151,
-1.56778615902482,-1.54862850687657,-1.54554145412597,-1.54403120387796,
-1.54284929285635,-1.54154079352943,-1.5393958795344,-1.53185568931526,
-1.50634800179568,-1.46349892424954,-1.38832031359065,-1.38402637410402,
-1.3827679654152,-1.38209948606301,-1.38145057325746,-1.3806531816044,-1.37914423188577,
-1.37053478152417,-1.35211878308866,-1.3268524956792,-1.23015706199185,
-1.22403187801211,-1.22196871244141,-1.22080754026395,-1.21974736891938,
-1.21835718618358,-1.21582252395606,-1.2126746980832,-1.19071019677127,
-1.17314264993399,-1.10852564953798,-1.06358363181037,-1.06083841929929,
-1.05989296892876,-1.05924705087823,-1.05865447947678,-1.057845005684,-1.05627855329976,
-1.04634157642698,-1.02332687356086,-0.944432269165112,-0.930660698989446,
-0.903632101823023,-0.900232004006861,-0.898677890553498,-0.897486130474042,
-0.896210913164362,-0.894254873758918,-0.888340314457047,-0.879329905375872,
-0.852017773563202,-0.801380849424833,-0.753755829162131,-0.753199119556926,
-0.752463250163929,-0.739552052868511,-0.73791148369758,-0.737074009902193,
-0.736457305675226,-0.735784327476104,-0.734847846166601,-0.732610158506311,
-0.729524249635282,-0.72150488685021,-0.686512005705855,-0.631860928771763,
-0.581750218193201,-0.57793509965139,-0.576412093885637,-0.575299062142194,
-0.574102640533274,-0.572926744583817,-0.570379919166202,-0.555869492164762,
-0.526818612471642,-0.49140153106653,-0.432889805969842,-0.432522067889638,
-0.430036324468666,-0.418478404806516,-0.415616991911007,-0.41454843570457,
-0.41391809443866,-0.41332050927828,-0.412474021156023,-0.410725749948347,
-0.399194352705144,-0.367404137958462,-0.343231570135268,-0.3162103712397,
-0.259244935838322,-0.255365884115638,-0.253831950644351,-0.252716052891383,
-0.251521374489583,-0.250348749371768,-0.24880276565047,-0.241855192666256,
-0.203240702388004,-0.179565560509696,-0.104341712672523,-0.0941031145889821,
-0.0924018679918587,-0.0915647213533804,-0.090906809568289,-0.0901636703847361,
-0.0889028445459993,-0.0873917716374819,-0.0843575726311591,-0.00095786616459987),
 .UNSPECIFIED.);
#874=B_SPLINE_CURVE_WITH_KNOTS('',3,(#64177,#64178,#64179,#64180,#64181,
#64182,#64183,#64184,#64185,#64186,#64187,#64188,#64189,#64190,#64191,#64192,
#64193,#64194,#64195,#64196,#64197,#64198,#64199,#64200,#64201,#64202,#64203,
#64204,#64205,#64206,#64207,#64208,#64209,#64210,#64211,#64212,#64213,#64214,
#64215,#64216,#64217,#64218,#64219,#64220,#64221,#64222,#64223,#64224,#64225,
#64226,#64227,#64228,#64229,#64230,#64231,#64232,#64233,#64234,#64235,#64236,
#64237,#64238,#64239,#64240,#64241,#64242,#64243,#64244,#64245,#64246,#64247,
#64248,#64249,#64250,#64251,#64252,#64253,#64254,#64255,#64256,#64257,#64258,
#64259,#64260,#64261,#64262,#64263,#64264,#64265,#64266,#64267,#64268,#64269,
#64270,#64271,#64272,#64273,#64274,#64275,#64276,#64277,#64278,#64279,#64280,
#64281,#64282,#64283,#64284,#64285,#64286,#64287,#64288,#64289,#64290,#64291,
#64292,#64293,#64294,#64295,#64296,#64297,#64298,#64299,#64300,#64301,#64302,
#64303,#64304,#64305,#64306,#64307,#64308,#64309,#64310,#64311,#64312,#64313,
#64314,#64315,#64316,#64317,#64318,#64319,#64320,#64321,#64322,#64323,#64324,
#64325,#64326,#64327,#64328,#64329,#64330,#64331,#64332,#64333,#64334,#64335,
#64336,#64337,#64338,#64339,#64340,#64341,#64342,#64343,#64344,#64345,#64346,
#64347,#64348,#64349,#64350,#64351,#64352,#64353,#64354,#64355,#64356,#64357,
#64358,#64359,#64360,#64361,#64362,#64363,#64364,#64365,#64366,#64367,#64368,
#64369,#64370,#64371,#64372,#64373,#64374,#64375,#64376,#64377,#64378,#64379,
#64380,#64381,#64382,#64383,#64384,#64385,#64386,#64387,#64388,#64389,#64390,
#64391,#64392,#64393,#64394,#64395,#64396,#64397,#64398,#64399,#64400,#64401,
#64402,#64403,#64404,#64405,#64406,#64407,#64408,#64409,#64410,#64411,#64412,
#64413,#64414,#64415,#64416,#64417,#64418,#64419,#64420,#64421,#64422,#64423,
#64424,#64425,#64426,#64427,#64428,#64429,#64430,#64431,#64432,#64433,#64434,
#64435,#64436,#64437,#64438,#64439,#64440,#64441,#64442,#64443,#64444,#64445,
#64446,#64447,#64448,#64449,#64450,#64451,#64452,#64453,#64454,#64455,#64456,
#64457,#64458,#64459,#64460,#64461,#64462,#64463,#64464,#64465,#64466,#64467,
#64468,#64469,#64470,#64471,#64472,#64473,#64474,#64475,#64476,#64477,#64478,
#64479,#64480,#64481,#64482,#64483,#64484,#64485,#64486,#64487,#64488,#64489,
#64490,#64491,#64492,#64493,#64494,#64495,#64496,#64497,#64498,#64499,#64500,
#64501,#64502,#64503,#64504,#64505,#64506,#64507,#64508,#64509,#64510,#64511,
#64512,#64513,#64514,#64515,#64516,#64517,#64518,#64519,#64520,#64521,#64522,
#64523,#64524,#64525,#64526,#64527,#64528,#64529,#64530,#64531,#64532,#64533,
#64534,#64535,#64536,#64537,#64538,#64539,#64540,#64541,#64542,#64543,#64544,
#64545,#64546,#64547,#64548,#64549,#64550,#64551,#64552,#64553,#64554,#64555,
#64556,#64557,#64558,#64559,#64560,#64561,#64562,#64563,#64564,#64565,#64566,
#64567,#64568,#64569,#64570,#64571,#64572,#64573,#64574,#64575,#64576,#64577,
#64578,#64579,#64580,#64581,#64582,#64583,#64584,#64585,#64586,#64587,#64588,
#64589,#64590,#64591,#64592,#64593,#64594,#64595,#64596,#64597,#64598,#64599,
#64600,#64601,#64602,#64603,#64604,#64605,#64606,#64607,#64608,#64609,#64610,
#64611,#64612,#64613,#64614,#64615,#64616,#64617,#64618,#64619,#64620,#64621,
#64622,#64623,#64624,#64625,#64626,#64627,#64628,#64629,#64630,#64631,#64632,
#64633,#64634,#64635,#64636,#64637,#64638,#64639,#64640,#64641,#64642,#64643,
#64644,#64645,#64646,#64647,#64648,#64649,#64650,#64651,#64652,#64653,#64654,
#64655,#64656,#64657,#64658,#64659,#64660,#64661,#64662,#64663,#64664,#64665,
#64666,#64667,#64668,#64669,#64670,#64671,#64672,#64673,#64674,#64675,#64676,
#64677,#64678,#64679,#64680,#64681,#64682,#64683,#64684,#64685,#64686,#64687,
#64688,#64689,#64690,#64691,#64692,#64693,#64694,#64695,#64696,#64697,#64698,
#64699,#64700,#64701,#64702,#64703,#64704),.UNSPECIFIED.,.F.,.F.,(4,2,2,
2,2,2,2,2,2,2,2,2,2,2,2,2,2,2,2,2,2,2,2,2,2,2,2,2,2,2,2,2,2,2,2,2,2,2,2,
2,2,2,2,2,2,2,2,2,2,2,2,2,2,2,2,2,2,2,2,2,2,2,2,2,2,2,2,2,2,2,2,2,2,2,2,
2,2,2,2,2,2,2,2,2,2,2,2,2,2,2,2,2,2,2,2,2,2,2,2,2,2,2,2,2,2,2,2,2,2,2,2,
2,2,2,2,2,2,2,2,2,2,2,2,2,2,2,2,2,2,2,2,2,2,2,2,2,2,2,2,2,2,2,2,2,2,2,2,
2,2,2,2,2,2,2,2,2,2,2,2,2,2,2,2,2,2,2,2,2,2,2,2,2,2,2,2,2,2,2,2,2,2,2,2,
2,2,2,2,2,2,2,2,2,2,2,2,2,2,2,2,2,2,2,2,2,2,2,2,2,2,2,2,2,2,2,2,2,2,2,2,
2,2,2,2,2,2,2,2,2,2,2,2,2,2,2,2,2,2,2,2,2,2,2,2,2,2,2,2,2,2,2,2,2,2,2,2,
2,2,2,2,2,2,2,2,4),(-4.06038590671169,-3.99533115978584,-3.99288451615544,
-3.99134341032541,-3.99017287297142,-3.98897961717822,-3.98786307860057,
-3.98632517332637,-3.98241979227162,-3.91886260821685,-3.90119545165806,
-3.88452875331077,-3.83915093933452,-3.83058095787481,-3.82907456383882,
-3.82827802040948,-3.82762953684154,-3.82696126726956,-3.82570257818847,
-3.8214018101828,-3.74614728588927,-3.7208503082374,-3.68832738513958,-3.67731598887521,
-3.67040291837945,-3.66885943099757,-3.6676880530777,-3.66649435788101,
-3.6653785945957,-3.66384361784815,-3.65995547818127,-3.60116494648335,
-3.54620435551938,-3.51955836072467,-3.50826639038863,-3.50665127275837,
-3.50583196500646,-3.50517603930975,-3.50451941198775,-3.50331848235849,
-3.49950404823833,-3.43357947647393,-3.38879027493756,-3.36453950423955,
-3.34903401280407,-3.34635056778719,-3.34518393980045,-3.34399273117545,
-3.34287257243987,-3.34132091578194,-3.33818820688385,-3.30853087914805,
-3.28787768837631,-3.21719027501515,-3.19547295422153,-3.18571897675306,
-3.18414377748797,-3.18333272647675,-3.182740235025,-3.18209563033733,-3.18115416285461,
-3.1784344875749,-3.13022316242323,-3.07845876830885,-3.03278772268032,
-3.02797645367114,-3.0243916887075,-3.02279012163587,-3.021589922032,-3.02048357087056,
-3.01898529309025,-3.01606300887088,-2.99322330893292,-2.98170133891302,
-2.89951413922132,-2.88897140780225,-2.86612785263719,-2.86243802535101,
-2.86128495050293,-2.86056616352924,-2.85990254225026,-2.85903469582242,
-2.85712596413958,-2.84185665231,-2.84123050729425,-2.83885125461131,-2.83192990478553,
-2.76341658478353,-2.73448352958715,-2.70770601607517,-2.70418487854436,
-2.70140095946039,-2.699959918848,-2.69889409011143,-2.69775803604036,-2.6961475779052,
-2.6917974291399,-2.6184276668183,-2.56859383444668,-2.54951070661052,-2.54055478622066,
-2.5390381817123,-2.538239397899,-2.53759072504984,-2.53692371165883,-2.53567158114221,
-2.53142949248462,-2.45690138500186,-2.41371548288173,-2.38806071896264,
-2.38304262582197,-2.37930455642501,-2.37767170294239,-2.37647167184569,
-2.37536485949717,-2.37386501882376,-2.37018189195767,-2.31913591187493,
-2.29422451502291,-2.24580699105114,-2.22687874109205,-2.21802365829361,
-2.21651168278256,-2.21571389333632,-2.21506528004273,-2.21439766328819,
-2.21314248082997,-2.20887347621438,-2.1340612618785,-2.09106008450369,
-2.06549021339839,-2.057914419542,-2.05576651701238,-2.05445772866599,-2.05327655330566,
-2.05176861829506,-2.04879306091321,-2.03110452184611,-1.98742809340207,
-1.8995917320736,-1.89501699559509,-1.89374303253049,-1.89298975211511,
-1.89233354118016,-1.89151245397762,-1.88988927285698,-1.87813654855862,
-1.85157472971377,-1.79129114485283,-1.73818167604261,-1.73433567324719,
-1.73280764484916,-1.7316935159328,-1.7304983472386,-1.72889450670342,-1.72531726610269,
-1.67587512379374,-1.58430610411295,-1.57312948655571,-1.57138276296661,
-1.57053665320079,-1.56987788627118,-1.56914038108417,-1.56790427173414,
-1.56328138192024,-1.53008432777748,-1.44726166379064,-1.44098101010954,
-1.43381993741566,-1.41423397001383,-1.41112730629537,-1.40961335922946,
-1.40843123904355,-1.40712524707561,-1.40499065081702,-1.39754786078178,
-1.35029219345686,-1.26306858931603,-1.25050895106294,-1.24888120344901,
-1.2480470462768,-1.24743120827324,-1.24677168968778,-1.24585971065689,
-1.24376238628546,-1.24088484071129,-1.2110237191372,-1.14883359296096,
-1.0927995609803,-1.08892758415155,-1.08739494992516,-1.08627947089618,
-1.08508474536429,-1.08348477604279,-1.07992966953421,-1.02993200486211,
-0.941374290409813,-0.940435776942215,-0.927789621217176,-0.926158554940047,
-0.925323492209265,-0.924707373701481,-0.924084798603714,-0.923197366954174,
-0.921221998688909,-0.918557925163082,-0.892459960234906,-0.845165487382356,
-0.771150630036447,-0.766487904222883,-0.764829341003457,-0.763679738270363,
-0.76261714889549,-0.761175458119865,-0.758422244573456,-0.741559916201148,
-0.704027631937379,-0.633542480812273,-0.605678782390739,-0.603513354421616,
-0.602657630643331,-0.602036173225907,-0.601410143291156,-0.60053908972563,
-0.598711417293119,-0.59625822323979,-0.590391929139022,-0.571427828814243,
-0.538277446886927,-0.468894489325305,-0.446303785723019,-0.443389492276724,
-0.441892861812162,-0.440786528475238,-0.439585188463481,-0.437947288396691,
-0.434183386407426,-0.429122409831035,-0.40332631888975,-0.35847569032206,
-0.317948250199433,-0.305946417234263,-0.298902685152201,-0.295635185601995,
-0.294588555524527,-0.282426574417055,-0.280635801625219,-0.279790080904281,
-0.279129495504108,-0.278514743861476,-0.277796405396636,-0.275649395382003,
-0.248817718028,-0.229763844089698,-0.139484360858154,-0.123137138790546,
-0.120490509893527,-0.118922931077595,-0.117728970396443,-0.116459247698824,
-0.114488047529457,-0.10848613054866,-0.07529142213324,-0.000958271623644713),
 .UNSPECIFIED.);
#875=B_SPLINE_CURVE_WITH_KNOTS('',3,(#64706,#64707,#64708,#64709,#64710,
#64711,#64712,#64713,#64714,#64715,#64716,#64717,#64718,#64719,#64720,#64721,
#64722,#64723,#64724,#64725,#64726,#64727,#64728,#64729,#64730,#64731,#64732,
#64733,#64734,#64735,#64736,#64737,#64738,#64739,#64740,#64741,#64742,#64743,
#64744,#64745,#64746,#64747,#64748,#64749,#64750,#64751,#64752,#64753,#64754,
#64755,#64756,#64757,#64758,#64759,#64760,#64761,#64762,#64763,#64764,#64765,
#64766,#64767,#64768,#64769,#64770,#64771,#64772,#64773,#64774,#64775,#64776,
#64777,#64778,#64779,#64780,#64781,#64782,#64783,#64784,#64785,#64786,#64787,
#64788,#64789,#64790,#64791,#64792,#64793,#64794,#64795,#64796,#64797,#64798,
#64799,#64800,#64801,#64802,#64803,#64804,#64805,#64806,#64807,#64808,#64809,
#64810,#64811,#64812,#64813,#64814,#64815,#64816,#64817,#64818,#64819,#64820,
#64821,#64822,#64823,#64824,#64825,#64826,#64827,#64828,#64829,#64830,#64831,
#64832,#64833,#64834,#64835,#64836,#64837,#64838,#64839,#64840,#64841,#64842,
#64843,#64844,#64845,#64846,#64847,#64848,#64849,#64850,#64851,#64852,#64853,
#64854,#64855,#64856,#64857,#64858,#64859,#64860,#64861,#64862,#64863,#64864,
#64865,#64866,#64867,#64868,#64869,#64870,#64871,#64872,#64873,#64874,#64875,
#64876,#64877,#64878,#64879,#64880,#64881,#64882,#64883,#64884,#64885,#64886,
#64887,#64888,#64889,#64890,#64891,#64892,#64893,#64894,#64895,#64896,#64897,
#64898,#64899,#64900,#64901,#64902,#64903,#64904,#64905,#64906,#64907,#64908,
#64909,#64910,#64911,#64912,#64913,#64914,#64915,#64916,#64917,#64918,#64919,
#64920,#64921,#64922,#64923,#64924,#64925,#64926,#64927,#64928,#64929,#64930,
#64931,#64932,#64933,#64934,#64935,#64936,#64937,#64938,#64939,#64940,#64941,
#64942,#64943,#64944,#64945,#64946,#64947,#64948,#64949,#64950,#64951,#64952,
#64953,#64954,#64955,#64956,#64957,#64958,#64959,#64960,#64961,#64962,#64963,
#64964,#64965,#64966,#64967,#64968,#64969,#64970,#64971,#64972,#64973,#64974,
#64975,#64976,#64977,#64978,#64979,#64980,#64981,#64982,#64983,#64984,#64985,
#64986,#64987,#64988,#64989,#64990,#64991,#64992,#64993,#64994,#64995,#64996,
#64997,#64998,#64999,#65000,#65001,#65002,#65003,#65004,#65005,#65006,#65007,
#65008,#65009,#65010,#65011,#65012,#65013,#65014,#65015,#65016,#65017,#65018,
#65019,#65020,#65021,#65022,#65023,#65024,#65025,#65026,#65027,#65028,#65029,
#65030,#65031,#65032,#65033,#65034,#65035,#65036,#65037,#65038,#65039,#65040,
#65041,#65042,#65043,#65044,#65045,#65046,#65047,#65048,#65049,#65050,#65051,
#65052,#65053,#65054,#65055,#65056,#65057,#65058,#65059,#65060,#65061,#65062,
#65063,#65064,#65065,#65066,#65067,#65068,#65069,#65070,#65071,#65072,#65073,
#65074,#65075,#65076,#65077,#65078,#65079,#65080,#65081,#65082,#65083,#65084,
#65085,#65086,#65087,#65088,#65089,#65090,#65091,#65092,#65093,#65094,#65095,
#65096,#65097,#65098,#65099,#65100,#65101,#65102,#65103,#65104,#65105,#65106,
#65107,#65108,#65109,#65110,#65111,#65112,#65113,#65114,#65115,#65116,#65117,
#65118,#65119,#65120,#65121,#65122,#65123,#65124,#65125,#65126,#65127,#65128,
#65129,#65130,#65131,#65132,#65133,#65134,#65135,#65136,#65137,#65138,#65139,
#65140,#65141,#65142,#65143,#65144,#65145,#65146,#65147,#65148,#65149,#65150,
#65151,#65152,#65153,#65154,#65155,#65156,#65157,#65158,#65159,#65160,#65161,
#65162,#65163,#65164,#65165,#65166,#65167,#65168,#65169,#65170,#65171,#65172,
#65173,#65174,#65175,#65176,#65177,#65178,#65179,#65180,#65181,#65182,#65183,
#65184,#65185,#65186,#65187,#65188,#65189,#65190,#65191,#65192,#65193,#65194,
#65195,#65196,#65197,#65198,#65199,#65200,#65201,#65202,#65203,#65204,#65205,
#65206,#65207,#65208,#65209,#65210,#65211,#65212,#65213,#65214,#65215,#65216,
#65217,#65218,#65219,#65220,#65221,#65222,#65223,#65224,#65225,#65226,#65227,
#65228,#65229,#65230,#65231,#65232,#65233,#65234,#65235,#65236,#65237,#65238,
#65239,#65240,#65241,#65242,#65243,#65244,#65245,#65246,#65247,#65248,#65249,
#65250,#65251,#65252,#65253),.UNSPECIFIED.,.F.,.F.,(4,2,2,2,2,2,2,2,2,2,
2,2,2,2,2,2,2,2,2,2,2,2,2,2,2,2,2,2,2,2,2,2,2,2,2,2,2,2,2,2,2,2,2,2,2,2,
2,2,2,2,2,2,2,2,2,2,2,2,2,2,2,2,2,2,2,2,2,2,2,2,2,2,2,2,2,2,2,2,2,2,2,2,
2,2,2,2,2,2,2,2,2,2,2,2,2,2,2,2,2,2,2,2,2,2,2,2,2,2,2,2,2,2,2,2,2,2,2,2,
2,2,2,2,2,2,2,2,2,2,2,2,2,2,2,2,2,2,2,2,2,2,2,2,2,2,2,2,2,2,2,2,2,2,2,2,
2,2,2,2,2,2,2,2,2,2,2,2,2,2,2,2,2,2,2,2,2,2,2,2,2,2,2,2,2,2,2,2,2,2,2,2,
2,2,2,2,2,2,2,2,2,2,2,2,2,2,2,2,2,2,2,2,2,2,2,2,2,2,2,2,2,2,2,2,2,2,2,2,
2,2,2,2,2,2,2,2,2,2,2,2,2,2,2,2,2,2,2,2,2,2,2,2,2,2,2,2,2,2,2,2,2,2,2,2,
2,2,2,2,2,2,2,2,2,2,2,4),(-4.06054173240988,-4.02058570238127,-4.01875545172079,
-4.01770545766817,-4.016978695896,-4.01636305788412,-4.01570464905039,-4.01486107357676,
-4.01312680093112,-4.00221193031645,-3.999924470005,-3.99674131556362,-3.97461839182422,
-3.96933614986905,-3.91205726126169,-3.86601400458494,-3.85868367516395,
-3.8565608411054,-3.85525752746501,-3.85407486318991,-3.8525560823871,-3.84942483471692,
-3.82930070060744,-3.82329163044152,-3.7473505980948,-3.7215458154747,-3.70694023010225,
-3.69992368131608,-3.69712584876673,-3.69506931722858,-3.69435889293425,
-3.69374497577411,-3.69308230207342,-3.69222118828335,-3.69041615491519,
-3.67734103291924,-3.67397582543777,-3.66720433544192,-3.65453252885351,
-3.60623937532244,-3.59981345960569,-3.56975130937846,-3.54392055922187,
-3.53621314668269,-3.5340516621585,-3.5327396336653,-3.53155878784385,-3.53005574073782,
-3.52710395333014,-3.50987351271807,-3.50882361005823,-3.43834778113679,
-3.39878957717023,-3.38431000332136,-3.37734627277779,-3.37456386876616,
-3.37251851069903,-3.37161833006428,-3.37094865912725,-3.370327977555,-3.36947486093409,
-3.36732397145806,-3.34029185485344,-3.26703533429014,-3.22085873452279,
-3.21351565049087,-3.21139139895943,-3.21008771697486,-3.20890504843565,
-3.20738672254149,-3.2042580489153,-3.18419356396322,-3.17796355599614,
-3.10200852367228,-3.05298995397825,-3.0510792522122,-3.04957054151396,
-3.0487764214578,-3.04812086195007,-3.04745893223393,-3.04623254057066,
-3.04221205371738,-2.9674289482759,-2.89304952306376,-2.8895826808681,-2.88799920623245,
-2.88680724568932,-2.88568737085695,-2.88413767893281,-2.88101383134194,
-2.85171580498124,-2.82959418464685,-2.76208704384754,-2.73219371986278,
-2.72931480815302,-2.72721133757102,-2.72630151059308,-2.72564245326429,
-2.72502624102431,-2.72419045316517,-2.72255620574681,-2.70981568283167,
-2.70799357505028,-2.70015767492631,-2.68473016274241,-2.62048216674927,
-2.58570086725821,-2.56931808134276,-2.56658586586715,-2.56514878405913,
-2.56408689617126,-2.56293543189889,-2.56126966927437,-2.5565572727695,
-2.48237962277254,-2.43439051107804,-2.40909187569006,-2.40514488526984,
-2.40397673514042,-2.40325445473263,-2.40259177033796,-2.40173084213492,
-2.39992690406947,-2.38688016150908,-2.38366191290005,-2.38151071381351,
-2.37461971462848,-2.35832772674211,-2.32828775473404,-2.29940612344123,
-2.25300654105434,-2.24564222570681,-2.24351563429889,-2.24221135282333,
-2.24102868986355,-2.23951113697194,-2.23638677399111,-2.21642123894337,
-2.21085514458431,-2.16743681442079,-2.11778017265357,-2.0934905409715,
-2.08332731900652,-2.08175986211478,-2.08095024555145,-2.08035772900889,
-2.07971202804921,-2.07876716282358,-2.07602546714092,-2.03164749009595,
-1.9353431972879,-1.92829460028116,-1.92267213925653,-1.92068042923444,
-1.9195337321908,-1.91847077824902,-1.91702394905577,-1.9142452400809,-1.89675049413491,
-1.85631167696801,-1.77177850251612,-1.76082942520942,-1.75909336191206,
-1.75824936021085,-1.75759082505384,-1.75685207677666,-1.75561044824367,
-1.75092823831163,-1.71694991556723,-1.63531349669321,-1.62647952944112,
-1.62127327998383,-1.60193394884238,-1.5988387768399,-1.59732710024486,
-1.59614523480706,-1.5948379738486,-1.59269778808553,-1.58520093141039,
-1.53735728958329,-1.44201115415768,-1.43733670299921,-1.43605204393648,
-1.43529613306126,-1.43463999104861,-1.43382202550577,-1.43221466933165,
-1.42095331918417,-1.38688105792138,-1.2831161430962,-1.28167296674716,
-1.27683524940639,-1.27496392129631,-1.27384085499594,-1.27267430091801,
-1.27114938890705,-1.26946921101127,-1.26669083658375,-1.21030353114819,
-1.12619232831601,-1.11521635008148,-1.1134789012282,-1.11263457891498,
-1.11197595651617,-1.11123728411188,-1.10999618093828,-1.10532045578578,
-1.07143114986391,-0.990394934343854,-0.95704562975981,-0.953461841862194,
-0.95201711454946,-0.950814270858487,-0.949606907521943,-0.947866065420648,
-0.945887002110378,-0.942378227593677,-0.934700707455248,-0.912584835536502,
-0.868237212244875,-0.795516726407038,-0.791623855581194,-0.790412856038334,
-0.789753988390567,-0.789097994646529,-0.788281801986684,-0.786682937855588,
-0.775667433433133,-0.74741577790899,-0.701347966776549,-0.635036239808415,
-0.631088831508773,-0.629543414468046,-0.628424552098376,-0.627255582417368,
-0.625748251891298,-0.624064291845193,-0.621276971015926,-0.615654207189192,
-0.601154475927136,-0.567080705902515,-0.483230526948228,-0.480100403342687,
-0.469782925850279,-0.468077676793534,-0.467239737234692,-0.466581755411169,
-0.46583913376575,-0.46458057795939,-0.45971306857014,-0.43653864768605,
-0.386154887574586,-0.359580447511575,-0.312114852168862,-0.310265566614375,
-0.307867135672493,-0.306357207318808,-0.305221085814658,-0.303951933507669,
-0.301939409682461,-0.299571157082405,-0.295070370780411,-0.284332911011669,
-0.249914683940878,-0.158683821464179,-0.14714091930333,-0.145377018848626,
-0.144527327768726,-0.143867932392595,-0.143132009382931,-0.141903726810655,
-0.137367016506054,-0.105281344936748,-0.000957917344321264),
 .UNSPECIFIED.);
#876=B_SPLINE_CURVE_WITH_KNOTS('',3,(#65255,#65256,#65257,#65258,#65259,
#65260,#65261,#65262,#65263,#65264,#65265,#65266,#65267,#65268,#65269,#65270,
#65271,#65272,#65273,#65274,#65275,#65276,#65277,#65278,#65279,#65280,#65281,
#65282,#65283,#65284,#65285,#65286,#65287,#65288,#65289,#65290,#65291,#65292,
#65293,#65294,#65295,#65296,#65297,#65298,#65299,#65300,#65301,#65302,#65303,
#65304,#65305,#65306,#65307,#65308,#65309,#65310,#65311,#65312,#65313,#65314,
#65315,#65316,#65317,#65318,#65319,#65320,#65321,#65322,#65323,#65324,#65325,
#65326,#65327,#65328,#65329,#65330,#65331,#65332,#65333,#65334,#65335,#65336,
#65337,#65338,#65339,#65340,#65341,#65342,#65343,#65344,#65345,#65346,#65347,
#65348,#65349,#65350,#65351,#65352,#65353,#65354,#65355,#65356,#65357,#65358,
#65359,#65360,#65361,#65362,#65363,#65364,#65365,#65366,#65367,#65368,#65369,
#65370,#65371,#65372,#65373,#65374,#65375,#65376,#65377,#65378,#65379,#65380,
#65381,#65382,#65383,#65384,#65385,#65386,#65387,#65388,#65389,#65390,#65391,
#65392,#65393,#65394,#65395,#65396,#65397,#65398,#65399,#65400,#65401,#65402,
#65403,#65404,#65405,#65406,#65407,#65408,#65409,#65410,#65411,#65412,#65413,
#65414,#65415,#65416,#65417,#65418,#65419,#65420,#65421,#65422,#65423,#65424,
#65425,#65426,#65427,#65428,#65429,#65430,#65431,#65432,#65433,#65434,#65435,
#65436,#65437,#65438,#65439,#65440,#65441,#65442,#65443,#65444,#65445,#65446,
#65447,#65448,#65449,#65450,#65451,#65452,#65453,#65454,#65455,#65456,#65457,
#65458,#65459,#65460,#65461,#65462,#65463,#65464,#65465,#65466,#65467,#65468,
#65469,#65470,#65471,#65472,#65473,#65474,#65475,#65476,#65477,#65478,#65479,
#65480,#65481,#65482,#65483,#65484,#65485,#65486,#65487,#65488,#65489,#65490,
#65491,#65492,#65493,#65494,#65495,#65496,#65497,#65498,#65499,#65500,#65501,
#65502,#65503,#65504,#65505,#65506,#65507,#65508,#65509,#65510,#65511,#65512,
#65513,#65514,#65515,#65516,#65517,#65518,#65519,#65520,#65521,#65522,#65523,
#65524,#65525,#65526,#65527,#65528,#65529,#65530,#65531,#65532,#65533,#65534,
#65535,#65536,#65537,#65538,#65539,#65540,#65541,#65542,#65543,#65544,#65545,
#65546,#65547,#65548,#65549,#65550,#65551,#65552,#65553,#65554,#65555,#65556,
#65557,#65558,#65559,#65560,#65561,#65562,#65563,#65564,#65565,#65566,#65567,
#65568,#65569,#65570,#65571,#65572,#65573,#65574,#65575,#65576,#65577,#65578,
#65579,#65580,#65581,#65582,#65583,#65584,#65585,#65586,#65587,#65588,#65589,
#65590,#65591,#65592,#65593,#65594,#65595,#65596,#65597,#65598,#65599,#65600,
#65601,#65602,#65603,#65604,#65605,#65606,#65607,#65608,#65609,#65610,#65611,
#65612,#65613,#65614,#65615,#65616,#65617,#65618,#65619,#65620,#65621,#65622,
#65623,#65624,#65625,#65626,#65627,#65628,#65629,#65630,#65631,#65632,#65633,
#65634,#65635,#65636,#65637,#65638,#65639,#65640,#65641,#65642,#65643,#65644,
#65645,#65646,#65647,#65648,#65649,#65650,#65651,#65652,#65653,#65654,#65655,
#65656,#65657,#65658,#65659,#65660,#65661,#65662,#65663,#65664,#65665,#65666,
#65667,#65668,#65669,#65670,#65671,#65672,#65673,#65674,#65675,#65676,#65677,
#65678,#65679,#65680,#65681,#65682,#65683,#65684,#65685,#65686,#65687,#65688,
#65689,#65690,#65691,#65692,#65693,#65694,#65695,#65696,#65697,#65698,#65699,
#65700,#65701,#65702,#65703,#65704,#65705,#65706,#65707,#65708,#65709,#65710,
#65711,#65712,#65713,#65714,#65715,#65716,#65717,#65718,#65719,#65720,#65721,
#65722,#65723,#65724,#65725,#65726,#65727,#65728,#65729,#65730,#65731,#65732,
#65733,#65734,#65735,#65736,#65737,#65738,#65739,#65740,#65741,#65742,#65743,
#65744,#65745,#65746,#65747,#65748,#65749,#65750,#65751,#65752,#65753,#65754,
#65755,#65756,#65757,#65758,#65759,#65760,#65761,#65762,#65763,#65764,#65765,
#65766,#65767,#65768,#65769,#65770,#65771,#65772,#65773,#65774,#65775,#65776,
#65777,#65778,#65779,#65780,#65781,#65782,#65783,#65784,#65785,#65786,#65787,
#65788,#65789,#65790,#65791,#65792,#65793,#65794,#65795,#65796,#65797,#65798,
#65799,#65800,#65801,#65802),.UNSPECIFIED.,.F.,.F.,(4,2,2,2,2,2,2,2,2,2,
2,2,2,2,2,2,2,2,2,2,2,2,2,2,2,2,2,2,2,2,2,2,2,2,2,2,2,2,2,2,2,2,2,2,2,2,
2,2,2,2,2,2,2,2,2,2,2,2,2,2,2,2,2,2,2,2,2,2,2,2,2,2,2,2,2,2,2,2,2,2,2,2,
2,2,2,2,2,2,2,2,2,2,2,2,2,2,2,2,2,2,2,2,2,2,2,2,2,2,2,2,2,2,2,2,2,2,2,2,
2,2,2,2,2,2,2,2,2,2,2,2,2,2,2,2,2,2,2,2,2,2,2,2,2,2,2,2,2,2,2,2,2,2,2,2,
2,2,2,2,2,2,2,2,2,2,2,2,2,2,2,2,2,2,2,2,2,2,2,2,2,2,2,2,2,2,2,2,2,2,2,2,
2,2,2,2,2,2,2,2,2,2,2,2,2,2,2,2,2,2,2,2,2,2,2,2,2,2,2,2,2,2,2,2,2,2,2,2,
2,2,2,2,2,2,2,2,2,2,2,2,2,2,2,2,2,2,2,2,2,2,2,2,2,2,2,2,2,2,2,2,2,2,2,2,
2,2,2,2,2,2,2,2,2,2,2,4),(-4.06119598324708,-4.04831213485074,-4.04613216796598,
-4.0447032789022,-4.0435695858176,-4.04241134613562,-4.04108248347896,-4.03884564966487,
-4.03133266086793,-4.02913402067733,-4.02226911079524,-3.91185697649888,
-3.89286452981374,-3.88397315721871,-3.88245903351183,-3.88166057909371,
-3.88106915056492,-3.88032166421199,-3.87904124063376,-3.87454882418137,
-3.78599732559944,-3.74811169684466,-3.73287020459906,-3.72703583866328,
-3.72417159316184,-3.72245567057437,-3.72090411274886,-3.71973344540439,
-3.71861775919585,-3.71708448499482,-3.71320903293776,-3.65672615559556,
-3.63036541331377,-3.62268870331163,-3.59821812146691,-3.57196980179826,
-3.56139951422218,-3.55981662924339,-3.55900376794863,-3.55841085008741,
-3.55776667046272,-3.55662849576664,-3.55329986138373,-3.49528807827662,
-3.44566369845203,-3.42583664661937,-3.41038524812807,-3.40449164447257,
-3.4016060101805,-3.39988123352774,-3.3983227302198,-3.39715105238165,-3.39603706641129,
-3.39451027206645,-3.39067278295422,-3.33859720518647,-3.28947302144958,
-3.27770195672611,-3.24294795508707,-3.23820875971718,-3.23696184576256,
-3.23622188177811,-3.23556351871944,-3.2347214280468,-3.23305236783941,
-3.22303324262004,-3.17848047476073,-3.0878010906804,-3.08183977120618,
-3.07892980232035,-3.07719500042003,-3.07562948631269,-3.07445658035381,
-3.07334468761864,-3.07182572137609,-3.06803349556223,-3.01970685160269,
-2.95489343224616,-2.92022493582164,-2.9154921082358,-2.91424582110855,
-2.9135060233453,-2.91284767419626,-2.91200542132921,-2.91027818003952,
-2.89951759804377,-2.82386997055,-2.75904561575592,-2.7561872791134,-2.75447387592398,
-2.75292337466126,-2.75175321153512,-2.75063707188765,-2.7491017027941,
-2.74521322884299,-2.68661337893046,-2.63639824644016,-2.60468183355031,
-2.59345516003901,-2.59184917015406,-2.59103156441559,-2.59043812285857,
-2.58979626910084,-2.5886694798217,-2.58541465028248,-2.52940490180812,
-2.47909580399444,-2.43561341913953,-2.43199120511317,-2.43037900862065,
-2.42918231173339,-2.42807012366431,-2.42654997558329,-2.42275079702834,
-2.3738994737391,-2.35868228349457,-2.33387987752456,-2.31109816538221,
-2.27511212623186,-2.27028541379398,-2.26903070053604,-2.26828905298795,
-2.26763109808349,-2.26679207879462,-2.26508082902035,-2.25463918114359,
-2.16155426094268,-2.11756558024354,-2.11285724236001,-2.1093056135218,
-2.10770646639083,-2.10651205460603,-2.10539665045518,-2.10386377803796,
-2.10080651930832,-2.07385997440993,-2.06017827746862,-2.03093944879856,
-1.95172518779088,-1.94756236716279,-1.94631924002593,-1.94565396275599,
-1.94499875922123,-1.94419394926238,-1.94264922557405,-1.93305016168607,
-1.91576176969738,-1.89047118732563,-1.81638810307692,-1.80902375511383,
-1.78955767135633,-1.78645664177325,-1.78494383418346,-1.78376187249125,
-1.78245530954921,-1.78031809037149,-1.77284958067353,-1.72531401690485,
-1.62959765373666,-1.62495074811905,-1.62366899216035,-1.62291377666702,
-1.62225759108585,-1.6214387390334,-1.61982699959438,-1.60843389140765,
-1.57842822327829,-1.4834096111169,-1.46652407837208,-1.46359002810906,
-1.46209076776547,-1.46091031939734,-1.45959606425452,-1.45742475703102,
-1.44961885609579,-1.39826972063741,-1.3066025801482,-1.30209966064335,
-1.30081810752998,-1.30007037774205,-1.29942620051062,-1.2986196542456,
-1.29774138718091,-1.29632895847721,-1.29356292091741,-1.26570495741673,
-1.18044578342886,-1.14476346729518,-1.14148519071065,-1.13989708953866,
-1.13876685690014,-1.1376984185932,-1.13621146183489,-1.13323949844945,
-1.10992419252317,-1.09006511377496,-1.04034555643182,-0.982556257018479,
-0.979154360057,-0.978006778257242,-0.977360698283811,-0.976715330821373,
-0.975896758639818,-0.975001931838431,-0.973549776997043,-0.970676345182222,
-0.940891509829287,-0.849400214579552,-0.821728963188047,-0.818308426466099,
-0.816750609661067,-0.815558352199623,-0.814284881599966,-0.812296410671139,
-0.806154164872239,-0.771689339545847,-0.756754354086426,-0.745142588021295,
-0.661194890293366,-0.656665019158565,-0.655395623826028,-0.654643293109446,
-0.653999718288247,-0.653199821391288,-0.652330724473448,-0.650940208704385,
-0.648232940268742,-0.641524772982774,-0.617497692152871,-0.527929709181589,
-0.499043405954087,-0.495629617301253,-0.494190651428808,-0.492989320742526,
-0.49175549807956,-0.489950427590264,-0.485161554695287,-0.462244339077295,
-0.427908411380341,-0.41813426046919,-0.409990329352877,-0.402997640182685,
-0.388979831589526,-0.34825753485031,-0.334943683653466,-0.333105859760514,
-0.33225122229192,-0.331605368496845,-0.330899696399484,-0.33016296767771,
-0.329088852740455,-0.327198820235607,-0.323082202484467,-0.31116969197251,
-0.29192970666293,-0.203992326073534,-0.176370337764317,-0.172951638971376,
-0.1713942602897,-0.17020217250957,-0.168928722126584,-0.166939949800652,
-0.160794192577671,-0.126295168089752,-0.0223944647338021,-0.0163729017965301,
-0.0113135017104637,-0.00999015043440988,-0.00922523504495427,-0.00863391393677181,
-0.00801091682884623,-0.00724723259923413,-0.00610832021660343,-0.00100602066474334),
 .UNSPECIFIED.);
#877=B_SPLINE_CURVE_WITH_KNOTS('',3,(#65804,#65805,#65806,#65807,#65808,
#65809,#65810,#65811,#65812,#65813),.UNSPECIFIED.,.F.,.F.,(4,1,1,1,1,1,
1,4),(304.734490891393,305.708479969717,306.707272373485,307.706064777253,
308.704857181021,309.703649584789,310.702441988557,311.017666207308),
 .UNSPECIFIED.);
#878=B_SPLINE_CURVE_WITH_KNOTS('',3,(#65815,#65816,#65817,#65818,#65819,
#65820,#65821,#65822,#65823,#65824,#65825,#65826,#65827,#65828,#65829,#65830,
#65831,#65832,#65833,#65834,#65835,#65836,#65837,#65838,#65839,#65840,#65841,
#65842,#65843,#65844,#65845,#65846,#65847,#65848,#65849,#65850,#65851,#65852,
#65853,#65854,#65855,#65856,#65857,#65858,#65859,#65860,#65861,#65862,#65863,
#65864,#65865,#65866,#65867,#65868,#65869,#65870,#65871,#65872,#65873,#65874,
#65875,#65876,#65877,#65878,#65879,#65880,#65881,#65882,#65883,#65884,#65885,
#65886,#65887,#65888,#65889,#65890,#65891,#65892,#65893,#65894,#65895,#65896,
#65897,#65898,#65899,#65900,#65901,#65902,#65903,#65904,#65905,#65906,#65907,
#65908,#65909,#65910,#65911,#65912,#65913,#65914,#65915,#65916,#65917,#65918,
#65919,#65920,#65921,#65922,#65923,#65924,#65925,#65926,#65927,#65928,#65929,
#65930,#65931,#65932,#65933,#65934,#65935,#65936,#65937,#65938,#65939,#65940,
#65941,#65942,#65943,#65944,#65945,#65946,#65947,#65948,#65949,#65950,#65951,
#65952,#65953,#65954,#65955,#65956,#65957,#65958,#65959,#65960,#65961,#65962,
#65963,#65964,#65965,#65966,#65967,#65968,#65969,#65970,#65971,#65972,#65973,
#65974,#65975,#65976,#65977,#65978,#65979,#65980,#65981,#65982,#65983,#65984,
#65985,#65986,#65987,#65988,#65989,#65990,#65991,#65992,#65993,#65994,#65995,
#65996,#65997,#65998,#65999,#66000,#66001,#66002,#66003,#66004,#66005,#66006,
#66007,#66008,#66009,#66010,#66011,#66012,#66013,#66014,#66015,#66016,#66017,
#66018,#66019,#66020,#66021,#66022,#66023,#66024,#66025,#66026,#66027,#66028,
#66029,#66030,#66031,#66032,#66033,#66034,#66035,#66036,#66037,#66038,#66039,
#66040,#66041,#66042,#66043,#66044,#66045,#66046,#66047,#66048,#66049,#66050,
#66051,#66052,#66053,#66054,#66055,#66056,#66057,#66058,#66059,#66060,#66061,
#66062,#66063,#66064,#66065,#66066,#66067,#66068,#66069,#66070,#66071,#66072,
#66073,#66074,#66075,#66076,#66077,#66078,#66079,#66080,#66081,#66082,#66083,
#66084,#66085,#66086,#66087,#66088,#66089,#66090,#66091,#66092,#66093,#66094,
#66095,#66096,#66097,#66098,#66099,#66100,#66101,#66102,#66103,#66104,#66105,
#66106,#66107,#66108,#66109,#66110,#66111,#66112,#66113,#66114,#66115,#66116,
#66117,#66118,#66119,#66120,#66121,#66122,#66123,#66124,#66125,#66126,#66127,
#66128,#66129,#66130,#66131,#66132,#66133,#66134,#66135,#66136,#66137,#66138,
#66139,#66140,#66141,#66142,#66143,#66144,#66145,#66146,#66147,#66148,#66149,
#66150,#66151,#66152,#66153,#66154,#66155,#66156,#66157,#66158,#66159,#66160,
#66161,#66162,#66163,#66164,#66165,#66166,#66167,#66168,#66169,#66170,#66171,
#66172,#66173,#66174,#66175,#66176,#66177,#66178,#66179,#66180,#66181,#66182,
#66183,#66184,#66185,#66186,#66187,#66188,#66189,#66190,#66191,#66192,#66193,
#66194,#66195,#66196,#66197,#66198,#66199,#66200,#66201,#66202,#66203,#66204,
#66205,#66206,#66207,#66208,#66209,#66210,#66211,#66212,#66213,#66214,#66215,
#66216,#66217,#66218,#66219,#66220,#66221,#66222,#66223,#66224,#66225,#66226,
#66227,#66228,#66229,#66230,#66231,#66232,#66233,#66234,#66235,#66236,#66237,
#66238,#66239,#66240,#66241,#66242,#66243,#66244,#66245,#66246,#66247,#66248,
#66249,#66250,#66251,#66252,#66253,#66254,#66255,#66256,#66257,#66258,#66259,
#66260,#66261,#66262,#66263,#66264,#66265,#66266,#66267,#66268,#66269,#66270,
#66271,#66272,#66273,#66274,#66275,#66276,#66277,#66278,#66279,#66280,#66281,
#66282,#66283,#66284,#66285,#66286,#66287,#66288,#66289,#66290,#66291,#66292,
#66293,#66294,#66295,#66296,#66297,#66298,#66299,#66300,#66301,#66302,#66303,
#66304,#66305,#66306,#66307,#66308,#66309,#66310,#66311,#66312,#66313,#66314,
#66315,#66316,#66317,#66318,#66319,#66320,#66321,#66322,#66323,#66324,#66325,
#66326,#66327,#66328,#66329,#66330,#66331,#66332,#66333,#66334,#66335,#66336,
#66337,#66338,#66339,#66340,#66341,#66342,#66343,#66344,#66345,#66346,#66347,
#66348,#66349,#66350),.UNSPECIFIED.,.F.,.F.,(4,2,2,2,2,2,2,2,2,2,2,2,2,
2,2,2,2,2,2,2,2,2,2,2,2,2,2,2,2,2,2,2,2,2,2,2,2,2,2,2,2,2,2,2,2,2,2,2,2,
2,2,2,2,2,2,2,2,2,2,2,2,2,2,2,2,2,2,2,2,2,2,2,2,2,2,2,2,2,2,2,2,2,2,2,2,
2,2,2,2,2,2,2,2,2,2,2,2,2,2,2,2,2,2,2,2,2,2,2,2,2,2,2,2,2,2,2,2,2,2,2,2,
2,2,2,2,2,2,2,2,2,2,2,2,2,2,2,2,2,2,2,2,2,2,2,2,2,2,2,2,2,2,2,2,2,2,2,2,
2,2,2,2,2,2,2,2,2,2,2,2,2,2,2,2,2,2,2,2,2,2,2,2,2,2,2,2,2,2,2,2,2,2,2,2,
2,2,2,2,2,2,2,2,2,2,2,2,2,2,2,2,2,2,2,2,2,2,2,2,2,2,2,2,2,2,2,2,2,2,2,2,
2,2,2,2,2,2,2,2,2,2,2,2,2,2,2,2,2,2,2,2,2,2,2,2,2,2,2,2,2,2,2,2,2,2,2,2,
2,2,4),(-4.06080606694336,-4.00717255232006,-4.0047483802516,-4.00321666452518,
-4.00204936916829,-4.00085773774574,-3.99973792161758,-3.99818791373868,
-3.9950621925593,-3.96567738302845,-3.94671800235698,-3.93958039481456,
-3.87039716115203,-3.85137641269848,-3.84246594045836,-3.84095138336434,
-3.8401530259413,-3.83956181069048,-3.83881478269707,-3.83753559479031,
-3.8330516310455,-3.74727275620697,-3.71866671116966,-3.69898629847681,
-3.68333149825631,-3.6806415774336,-3.67947416247776,-3.67828247504177,
-3.67716279529695,-3.67561327584829,-3.67248947249685,-3.64317490838713,
-3.62443646244887,-3.56672948021867,-3.55863577978085,-3.53093908446463,
-3.52004935454113,-3.51845536725507,-3.5176403710051,-3.51698469096027,
-3.5163255873877,-3.51511263069805,-3.51120150821404,-3.4384698843406,-3.39650433651383,
-3.37283344665796,-3.36475891739992,-3.35933187642299,-3.35744081558777,
-3.35633953030525,-3.3551571491848,-3.35363932993903,-3.35051218926495,
-3.33047039431957,-3.32484796131439,-3.3193609166491,-3.31161587996121,
-3.23584994889392,-3.20920342764072,-3.19754598338155,-3.19592596360619,
-3.19510556674154,-3.1944494595678,-3.19369579842393,-3.19242004826655,
-3.18782781124516,-3.10082316149683,-3.06622252926881,-3.04157224076184,
-3.03821357469777,-3.03553721628582,-3.03411816734862,-3.03294271497257,
-3.03176927726416,-3.02964360842558,-3.02304316668977,-3.01694730574734,
-2.92659565795725,-2.875625914849,-2.87350494970679,-2.87258887738458,-2.87191974391799,
-2.87129854301787,-2.87044321070968,-2.86873189684117,-2.85371290167005,
-2.85206295001582,-2.84897482984182,-2.84690299858028,-2.83493600444057,
-2.76834181078234,-2.74454869528609,-2.71908574205562,-2.71566438587501,
-2.71294415301269,-2.71151708982905,-2.71045304966401,-2.70931078535952,
-2.70767789881456,-2.70318312066917,-2.6274618114087,-2.57999225754786,
-2.56100584430165,-2.55211729444739,-2.55060365242198,-2.54980545212675,
-2.54915674747659,-2.54848925227222,-2.54723492120474,-2.54297419876359,
-2.46825245337991,-2.42518176196537,-2.39958028004199,-2.39457957936221,
-2.39085184157743,-2.38922074391765,-2.38802093522189,-2.38691357520513,
-2.38541184504491,-2.38247667044703,-2.35929748178034,-2.31414790645294,
-2.2819212021583,-2.23071364865202,-2.22844550226923,-2.22750401836176,
-2.22683024931546,-2.22621484794584,-2.22538203818414,-2.2237591490883,
-2.21132399982757,-2.16807127052786,-2.07508815950537,-2.06902094982162,
-2.06704206294794,-2.06577094108367,-2.06457819216111,-2.063015855784,-2.05956960918846,
-2.03105717956733,-2.00702157703462,-1.91104810427369,-1.90643614223651,
-1.90515820225468,-1.90440396505848,-1.90374781561744,-1.90292795987113,
-1.90131090314939,-1.88974973895514,-1.86303615956141,-1.78708628620946,
-1.77050865476943,-1.768066239237,-1.74835512299657,-1.7452427821876,-1.74372775713779,
-1.74254556189619,-1.74124026775414,-1.73910857642669,-1.73169313223271,
-1.6847308934884,-1.58824861224914,-1.58371127302196,-1.58244111285369,
-1.58168862202532,-1.58103841231353,-1.5802188904055,-1.57860382618543,
-1.567109268723,-1.54103214993805,-1.45498255754657,-1.42610875346996,-1.42269540566677,
-1.42125654028859,-1.42005525691236,-1.41882144519868,-1.41701632136877,
-1.41222690598796,-1.38930497769127,-1.36747994346505,-1.30893316381916,
-1.26336342523369,-1.2605951854004,-1.25964650128379,-1.25899973285973,
-1.2583546245898,-1.25753775615542,-1.25664527292953,-1.25519867888632,
-1.25234023328002,-1.22282720796652,-1.1308768098669,-1.10336912046584,
-1.099954050715,-1.09839733624122,-1.09720534590314,-1.09593159984851,-1.09394153857412,
-1.08778537776143,-1.05319185522816,-0.954433927690995,-0.939271681188969,
-0.937365789773948,-0.936498282402379,-0.935834520564802,-0.935129764184481,
-0.934015247787698,-0.9326992359398,-0.930189792521849,-0.906652854563262,
-0.858764365074775,-0.810255190078082,-0.780751228228655,-0.777621407962522,
-0.776070082383189,-0.774949650967242,-0.773757677457121,-0.772175174364369,
-0.768714402940023,-0.69757279831974,-0.626581586851115,-0.616278170201482,
-0.614573646300439,-0.613735856085354,-0.613077894237505,-0.612350165405804,
-0.611133045536139,-0.609669120482026,-0.606763805025855,-0.599378371739643,
-0.584169490896696,-0.551745190069182,-0.479834604328143,-0.474486626748439,
-0.457267742756472,-0.454316107312384,-0.452812902396344,-0.451631818085496,
-0.450319406434124,-0.448157019163733,-0.440443618830817,-0.414593179621914,
-0.365307984260105,-0.343551717664757,-0.312535330181327,-0.311562542197397,
-0.294071376256208,-0.292091891959814,-0.291290060812106,-0.290621365244334,
-0.290006759448331,-0.289047561039487,-0.286679245035633,-0.28332756548136,
-0.274348609237957,-0.249983084694278,-0.166218929541401,-0.160422800612661,
-0.154834242937302,-0.134827997608625,-0.131701641017142,-0.130183645579306,
-0.129000875424188,-0.127696717029503,-0.125570869464186,-0.118214375946852,
-0.0718901686108905,-0.000958363168410272),.UNSPECIFIED.);
#879=B_SPLINE_CURVE_WITH_KNOTS('',3,(#66352,#66353,#66354,#66355,#66356,
#66357,#66358,#66359,#66360,#66361,#66362,#66363,#66364,#66365,#66366,#66367,
#66368,#66369,#66370,#66371,#66372,#66373,#66374,#66375,#66376,#66377,#66378,
#66379,#66380,#66381,#66382,#66383,#66384,#66385,#66386,#66387,#66388,#66389,
#66390,#66391,#66392,#66393,#66394,#66395,#66396,#66397,#66398,#66399,#66400,
#66401,#66402,#66403,#66404,#66405,#66406,#66407,#66408,#66409,#66410,#66411,
#66412,#66413,#66414,#66415,#66416,#66417,#66418,#66419,#66420,#66421,#66422,
#66423,#66424,#66425,#66426,#66427,#66428,#66429,#66430,#66431,#66432,#66433,
#66434,#66435,#66436,#66437,#66438,#66439,#66440,#66441,#66442,#66443,#66444,
#66445,#66446,#66447,#66448,#66449,#66450,#66451,#66452,#66453,#66454,#66455,
#66456,#66457,#66458,#66459,#66460,#66461,#66462,#66463,#66464,#66465,#66466,
#66467,#66468,#66469,#66470,#66471,#66472,#66473,#66474,#66475,#66476,#66477,
#66478,#66479,#66480,#66481,#66482,#66483,#66484,#66485,#66486,#66487,#66488,
#66489,#66490,#66491,#66492,#66493,#66494,#66495,#66496,#66497,#66498,#66499,
#66500,#66501,#66502,#66503,#66504,#66505,#66506,#66507,#66508,#66509,#66510,
#66511,#66512,#66513,#66514,#66515,#66516,#66517,#66518,#66519,#66520,#66521,
#66522,#66523,#66524,#66525,#66526,#66527,#66528,#66529,#66530,#66531,#66532,
#66533,#66534,#66535,#66536,#66537,#66538,#66539,#66540,#66541,#66542,#66543,
#66544,#66545,#66546,#66547,#66548,#66549,#66550,#66551,#66552,#66553,#66554,
#66555,#66556,#66557,#66558,#66559,#66560,#66561,#66562,#66563,#66564,#66565,
#66566,#66567,#66568,#66569,#66570,#66571,#66572,#66573,#66574,#66575,#66576,
#66577,#66578,#66579,#66580,#66581,#66582,#66583,#66584,#66585,#66586,#66587,
#66588,#66589,#66590,#66591,#66592,#66593,#66594,#66595,#66596,#66597,#66598,
#66599,#66600,#66601,#66602,#66603,#66604,#66605,#66606,#66607,#66608,#66609,
#66610,#66611,#66612,#66613,#66614,#66615,#66616,#66617,#66618,#66619,#66620,
#66621,#66622,#66623,#66624,#66625,#66626,#66627,#66628,#66629,#66630,#66631,
#66632,#66633,#66634,#66635,#66636,#66637,#66638,#66639,#66640,#66641,#66642,
#66643,#66644,#66645,#66646,#66647,#66648,#66649,#66650,#66651,#66652,#66653,
#66654,#66655,#66656,#66657,#66658,#66659,#66660,#66661,#66662,#66663,#66664,
#66665,#66666,#66667,#66668,#66669,#66670,#66671,#66672,#66673,#66674,#66675,
#66676,#66677,#66678,#66679,#66680,#66681,#66682,#66683,#66684,#66685,#66686,
#66687,#66688,#66689,#66690,#66691,#66692,#66693,#66694,#66695,#66696,#66697,
#66698,#66699,#66700,#66701,#66702,#66703,#66704,#66705,#66706,#66707,#66708,
#66709,#66710,#66711,#66712,#66713,#66714,#66715,#66716,#66717,#66718,#66719,
#66720,#66721,#66722,#66723,#66724,#66725,#66726,#66727,#66728,#66729,#66730,
#66731,#66732,#66733,#66734,#66735,#66736,#66737,#66738,#66739,#66740,#66741,
#66742,#66743,#66744,#66745,#66746,#66747,#66748,#66749,#66750,#66751,#66752,
#66753,#66754,#66755,#66756,#66757,#66758,#66759,#66760,#66761,#66762,#66763,
#66764,#66765,#66766,#66767,#66768,#66769,#66770,#66771,#66772,#66773,#66774,
#66775,#66776,#66777,#66778,#66779,#66780,#66781,#66782,#66783,#66784,#66785,
#66786,#66787,#66788,#66789,#66790,#66791,#66792,#66793,#66794,#66795,#66796,
#66797,#66798,#66799,#66800,#66801,#66802,#66803,#66804,#66805,#66806,#66807,
#66808,#66809,#66810,#66811,#66812,#66813,#66814,#66815,#66816,#66817,#66818,
#66819,#66820,#66821,#66822,#66823,#66824,#66825,#66826,#66827,#66828,#66829,
#66830,#66831,#66832,#66833,#66834,#66835,#66836,#66837,#66838,#66839,#66840,
#66841,#66842,#66843,#66844,#66845,#66846,#66847,#66848,#66849,#66850,#66851,
#66852,#66853,#66854,#66855,#66856,#66857,#66858,#66859,#66860,#66861,#66862,
#66863,#66864,#66865,#66866,#66867,#66868,#66869,#66870,#66871,#66872,#66873,
#66874,#66875),.UNSPECIFIED.,.F.,.F.,(4,2,2,2,2,2,2,2,2,2,2,2,2,2,2,2,2,
2,2,2,2,2,2,2,2,2,2,2,2,2,2,2,2,2,2,2,2,2,2,2,2,2,2,2,2,2,2,2,2,2,2,2,2,
2,2,2,2,2,2,2,2,2,2,2,2,2,2,2,2,2,2,2,2,2,2,2,2,2,2,2,2,2,2,2,2,2,2,2,2,
2,2,2,2,2,2,2,2,2,2,2,2,2,2,2,2,2,2,2,2,2,2,2,2,2,2,2,2,2,2,2,2,2,2,2,2,
2,2,2,2,2,2,2,2,2,2,2,2,2,2,2,2,2,2,2,2,2,2,2,2,2,2,2,2,2,2,2,2,2,2,2,2,
2,2,2,2,2,2,2,2,2,2,2,2,2,2,2,2,2,2,2,2,2,2,2,2,2,2,2,2,2,2,2,2,2,2,2,2,
2,2,2,2,2,2,2,2,2,2,2,2,2,2,2,2,2,2,2,2,2,2,2,2,2,2,2,2,2,2,2,2,2,2,2,2,
2,2,2,2,2,2,2,2,2,2,2,2,2,2,2,2,2,2,2,2,2,2,2,2,2,2,2,2,4),(-4.0592502292357,
-4.02971377170784,-4.02833269367985,-4.02746777430755,-4.02681359033491,
-4.02618885191426,-4.02556907401911,-4.02471842136597,-4.02258008547932,
-3.99619692647021,-3.99159020568108,-3.92268324987285,-3.87624072683285,
-3.86887460694005,-3.86674882885036,-3.86544533951018,-3.86426358736687,
-3.86274747144284,-3.85962701790925,-3.83971133977558,-3.82304306502926,
-3.75513412111111,-3.73670470144439,-3.71631718798715,-3.7098965427674,
-3.70727566583918,-3.70532732615901,-3.70444490606196,-3.70382204043842,
-3.70320515508762,-3.70236569461928,-3.70029210282313,-3.67728266226473,
-3.62864470595126,-3.62291915087168,-3.61624333686055,-3.54916689486743,
-3.54541358994127,-3.54377844458771,-3.54257841023991,-3.54147277627322,
-3.53997632801371,-3.53706013624253,-3.5143664509238,-3.5052048861805,-3.41996440525756,
-3.39460006666537,-3.38771279179005,-3.38495326888161,-3.38354357269005,
-3.38236500195798,-3.38164576818019,-3.3809867545542,-3.38013578421831,
-3.37836292286758,-3.36659149151968,-3.3636358336911,-3.2778147509822,-3.23134723132067,
-3.22397866204519,-3.22185258015306,-3.22054899309389,-3.21936721048809,
-3.2178511364515,-3.21473105609792,-3.19482525808929,-3.18825160183172,
-3.11370804105403,-3.06668622824333,-3.0631138819864,-3.06141123410297,
-3.06041321938472,-3.0595207907915,-3.05886477210674,-3.05824478785809,
-3.05739344426438,-3.0552512575727,-3.02865686272347,-2.95230316484772,
-2.90388431078029,-2.90033793925088,-2.89874025406815,-2.89754656823444,
-2.89643157732694,-2.89489885865933,-2.89102271432198,-2.83407452147374,
-2.7667328697092,-2.74237768966846,-2.73981910032576,-2.7384847442697,-2.73735689928254,
-2.73664973245552,-2.73598741618292,-2.73512677991275,-2.73332279376308,
-2.7202622809692,-2.71964177312284,-2.68191441981314,-2.61253353497769,
-2.58680342430162,-2.5791449196508,-2.57698914262429,-2.57567887487318,
-2.57449851244917,-2.57299456888179,-2.57003624549943,-2.55265920153993,
-2.45741639898088,-2.43142372570276,-2.41695347429834,-2.41525540123041,
-2.41441925148273,-2.41382352781453,-2.41318995664229,-2.41210369268551,
-2.40912387498563,-2.35756011545445,-2.32850505275292,-2.29693371639008,
-2.26245477784835,-2.2563114507617,-2.25432343355344,-2.25305045845657,
-2.25185880975524,-2.25030199594488,-2.24688450374002,-2.21927023589699,
-2.13137524934467,-2.09503498197563,-2.09295846718097,-2.0920503966135,
-2.09138274518819,-2.09075965091689,-2.08989683886026,-2.08768843487486,
-2.05691851562357,-2.03119195075069,-1.95735863467018,-1.93586025489425,
-1.93266915324815,-1.9311552378453,-1.92997011807192,-1.92867768443113,
-1.92660251406883,-1.91971167549072,-1.8781458032303,-1.77487154754452,
-1.77096377132384,-1.76975113397566,-1.76909204296414,-1.76843626896615,
-1.76762100008687,-1.76602598860223,-1.75511136260808,-1.72730942662431,
-1.66994103917675,-1.64308089446468,-1.61364135102043,-1.61051385077805,
-1.60896330027604,-1.60784325334014,-1.60665152606785,-1.60506907267428,
-1.60160730478632,-1.52967363334016,-1.45273193869247,-1.448430641462,-1.44717160899822,
-1.44650311679914,-1.44585439215727,-1.44505751695631,-1.44355038913142,
-1.43480570025145,-1.41610331917782,-1.37136114636524,-1.29271074443671,
-1.28807249694865,-1.28641781882221,-1.28526945479591,-1.2841128575556,
-1.28265385833431,-1.28106721332884,-1.27851257388335,-1.27351909193643,
-1.24793397391805,-1.20489056377862,-1.13003927289164,-1.12577025917861,
-1.12451486847455,-1.12384709686803,-1.12319830560107,-1.12240025803603,
-1.1208876758493,-1.11202581912504,-1.09308930954775,-1.04646452103335,
-0.969930824152034,-0.965385320340384,-0.96374438552121,-0.962599800057412,
-0.961442595319757,-0.9599747409644,-0.958375981601473,-0.955792497741351,
-0.950721935870888,-0.924899515604346,-0.881376751963629,-0.807278818911658,
-0.803095157629477,-0.801849542657765,-0.801183726072711,-0.800528500246564,
-0.799724396747227,-0.798183239424336,-0.78867194895334,-0.775982822829522,
-0.770383974634293,-0.716610071917506,-0.646715215280458,-0.642573382785571,
-0.640995997405014,-0.63986869899485,-0.638704119463013,-0.637189273524821,
-0.635525592149643,-0.632786857356244,-0.579740233152768,-0.485086588406905,
-0.480433681635539,-0.479151226984352,-0.478395807306426,-0.477739576910882,
-0.47692083945773,-0.475309867177421,-0.463943027569456,-0.434065962925085,
-0.388476760758934,-0.323616948547831,-0.319708153250979,-0.318169182260372,
-0.317051950443698,-0.315881899024113,-0.314333558453753,-0.312623608305136,
-0.30977383667544,-0.246378726847262,-0.181458022257683,-0.17686737633803,
-0.172939757871662,-0.172074784825208,-0.170796326286433,-0.158563831078692,
-0.156948577082422,-0.156117568360779,-0.155502457131242,-0.154827920537826,
-0.153883441010261,-0.151598853725842,-0.0880982192293773,-0.0144811591141122,
-0.000957555802355253),.UNSPECIFIED.);
#880=B_SPLINE_CURVE_WITH_KNOTS('',3,(#66877,#66878,#66879,#66880,#66881,
#66882,#66883,#66884,#66885,#66886,#66887,#66888,#66889,#66890,#66891,#66892,
#66893,#66894,#66895,#66896,#66897,#66898,#66899,#66900,#66901,#66902,#66903,
#66904,#66905,#66906,#66907,#66908,#66909,#66910,#66911,#66912,#66913,#66914,
#66915,#66916,#66917,#66918,#66919,#66920,#66921,#66922,#66923,#66924,#66925,
#66926,#66927,#66928,#66929,#66930,#66931,#66932,#66933,#66934,#66935,#66936,
#66937,#66938,#66939,#66940,#66941,#66942,#66943,#66944,#66945,#66946,#66947,
#66948,#66949,#66950,#66951,#66952,#66953,#66954,#66955,#66956,#66957,#66958,
#66959,#66960,#66961,#66962,#66963,#66964,#66965,#66966,#66967,#66968,#66969,
#66970,#66971,#66972,#66973,#66974,#66975,#66976,#66977,#66978,#66979,#66980,
#66981,#66982,#66983,#66984,#66985,#66986,#66987,#66988,#66989,#66990,#66991,
#66992,#66993,#66994,#66995,#66996,#66997,#66998,#66999,#67000,#67001,#67002,
#67003,#67004,#67005,#67006,#67007,#67008,#67009,#67010,#67011,#67012,#67013,
#67014,#67015,#67016,#67017,#67018,#67019,#67020,#67021,#67022,#67023,#67024,
#67025,#67026,#67027,#67028,#67029,#67030,#67031,#67032,#67033,#67034,#67035,
#67036,#67037,#67038,#67039,#67040,#67041,#67042,#67043,#67044,#67045,#67046,
#67047,#67048,#67049,#67050,#67051,#67052,#67053,#67054,#67055,#67056,#67057,
#67058,#67059,#67060,#67061,#67062,#67063,#67064,#67065,#67066,#67067,#67068,
#67069,#67070,#67071,#67072,#67073,#67074,#67075,#67076,#67077,#67078,#67079,
#67080,#67081,#67082,#67083,#67084,#67085,#67086,#67087,#67088,#67089,#67090,
#67091,#67092,#67093,#67094,#67095,#67096,#67097,#67098,#67099,#67100,#67101,
#67102,#67103,#67104,#67105,#67106,#67107,#67108,#67109,#67110,#67111,#67112,
#67113,#67114,#67115,#67116,#67117,#67118,#67119,#67120,#67121,#67122,#67123,
#67124,#67125,#67126,#67127,#67128,#67129,#67130,#67131,#67132,#67133,#67134,
#67135,#67136,#67137,#67138,#67139,#67140,#67141,#67142,#67143,#67144,#67145,
#67146,#67147,#67148,#67149,#67150,#67151,#67152,#67153,#67154,#67155,#67156,
#67157,#67158,#67159,#67160,#67161,#67162,#67163,#67164,#67165,#67166,#67167,
#67168,#67169,#67170,#67171,#67172,#67173,#67174,#67175,#67176,#67177,#67178,
#67179,#67180,#67181,#67182,#67183,#67184,#67185,#67186,#67187,#67188,#67189,
#67190,#67191,#67192,#67193,#67194,#67195,#67196,#67197,#67198,#67199,#67200,
#67201,#67202,#67203,#67204,#67205,#67206,#67207,#67208,#67209,#67210,#67211,
#67212,#67213,#67214,#67215,#67216,#67217,#67218,#67219,#67220,#67221,#67222,
#67223,#67224,#67225,#67226,#67227,#67228,#67229,#67230,#67231,#67232,#67233,
#67234,#67235,#67236,#67237,#67238,#67239,#67240,#67241,#67242,#67243,#67244,
#67245,#67246,#67247,#67248,#67249,#67250,#67251,#67252,#67253,#67254,#67255,
#67256,#67257,#67258,#67259,#67260,#67261,#67262,#67263,#67264,#67265,#67266,
#67267,#67268,#67269,#67270,#67271,#67272,#67273,#67274,#67275,#67276,#67277,
#67278,#67279,#67280,#67281,#67282,#67283,#67284,#67285,#67286,#67287,#67288,
#67289,#67290,#67291,#67292,#67293,#67294,#67295,#67296,#67297,#67298,#67299,
#67300,#67301,#67302,#67303,#67304,#67305,#67306,#67307,#67308,#67309,#67310,
#67311,#67312,#67313,#67314,#67315,#67316,#67317,#67318,#67319,#67320,#67321,
#67322,#67323,#67324,#67325,#67326,#67327,#67328,#67329,#67330,#67331,#67332,
#67333,#67334,#67335,#67336,#67337,#67338,#67339,#67340,#67341,#67342,#67343,
#67344,#67345,#67346,#67347,#67348,#67349,#67350,#67351,#67352,#67353,#67354,
#67355,#67356,#67357,#67358,#67359,#67360,#67361,#67362,#67363,#67364,#67365,
#67366,#67367,#67368,#67369,#67370,#67371,#67372,#67373,#67374,#67375,#67376,
#67377,#67378,#67379,#67380,#67381,#67382,#67383,#67384,#67385,#67386,#67387,
#67388,#67389,#67390,#67391,#67392,#67393,#67394,#67395,#67396,#67397,#67398,
#67399,#67400,#67401,#67402,#67403,#67404,#67405,#67406,#67407,#67408,#67409,
#67410,#67411,#67412,#67413,#67414,#67415,#67416,#67417,#67418),
 .UNSPECIFIED.,.F.,.F.,(4,2,2,2,2,2,2,2,2,2,2,2,2,2,2,2,2,2,2,2,2,2,2,2,
2,2,2,2,2,2,2,2,2,2,2,2,2,2,2,2,2,2,2,2,2,2,2,2,2,2,2,2,2,2,2,2,2,2,2,2,
2,2,2,2,2,2,2,2,2,2,2,2,2,2,2,2,2,2,2,2,2,2,2,2,2,2,2,2,2,2,2,2,2,2,2,2,
2,2,2,2,2,2,2,2,2,2,2,2,2,2,2,2,2,2,2,2,2,2,2,2,2,2,2,2,2,2,2,2,2,2,2,2,
2,2,2,2,2,2,2,2,2,2,2,2,2,2,2,2,2,2,2,2,2,2,2,2,2,2,2,2,2,2,2,2,2,2,2,2,
2,2,2,2,2,2,2,2,2,2,2,2,2,2,2,2,2,2,2,2,2,2,2,2,2,2,2,2,2,2,2,2,2,2,2,2,
2,2,2,2,2,2,2,2,2,2,2,2,2,2,2,2,2,2,2,2,2,2,2,2,2,2,2,2,2,2,2,2,2,2,2,2,
2,2,2,2,2,2,2,2,2,2,2,2,2,2,2,2,2,2,2,2,2,2,2,2,2,2,2,2,2,2,4),(-4.06075182852026,
-4.05713602550796,-4.05572147461755,-4.05459203620983,-4.0534262098459,
-4.05225574680044,-4.0501453121058,-4.04365868504524,-3.93391486943271,
-3.89929173805632,-3.89456217807212,-3.8933161697968,-3.89257642336149,
-3.89191804550264,-3.89107565595412,-3.88940512112919,-3.87935627056182,
-3.83475399024018,-3.74391097474562,-3.73808824921845,-3.73522832452903,
-3.73351427019815,-3.73196323873318,-3.73079301518622,-3.72967701783565,
-3.7281421547425,-3.72425659274861,-3.66619413419257,-3.6363178160674,-3.62747131263969,
-3.5996676191543,-3.58172716477806,-3.57239894599916,-3.5708656880108,-3.57006329542363,
-3.5694715979636,-3.56882229406063,-3.56765835910751,-3.56413407376746,
-3.50389499509457,-3.45509133257403,-3.43817666677135,-3.42189973085289,
-3.4157753982106,-3.41280697835267,-3.4110480498888,-3.40946460323284,-3.40828903924013,
-3.40718159558842,-3.40567985639861,-3.40198686785289,-3.36009545553401,
-3.30118335719606,-3.28918429248858,-3.2540962543738,-3.24933314381725,
-3.24808416229119,-3.24734379640251,-3.2466856119475,-3.24584446897499,
-3.24412260257951,-3.23346870618805,-3.14870615885526,-3.09745153153282,
-3.09231801730517,-3.08971107510054,-3.08810251736758,-3.08662922778336,
-3.08547022964981,-3.08432882997043,-3.08269926861627,-3.07822669187297,
-3.0029671837174,-2.95540075120341,-2.93626788314443,-2.92713838241178,
-2.92561382195227,-2.92481327492123,-2.92422177103945,-2.92347615173796,
-2.922203586898,-2.9177809451957,-2.82886227321155,-2.7750063201366,-2.76973573344294,
-2.76707794289168,-2.76544812931981,-2.76395787734161,-2.7627969803059,
-2.76166129666719,-2.76005249720835,-2.75571279887429,-2.68771464048416,
-2.64300429590222,-2.61654839721385,-2.60464128573738,-2.60301319471541,
-2.60219109673491,-2.60154079080291,-2.60079038371751,-2.59952871334197,
-2.59506884112714,-2.5041145795129,-2.44635922355543,-2.44294910763652,
-2.44137646058749,-2.44018635208269,-2.43906357260995,-2.43719285820363,
-2.43235742893389,-2.3556186039616,-2.31463915416349,-2.29464276974331,
-2.28199443833417,-2.28034404794254,-2.27951741639506,-2.27892289654618,
-2.27828520280973,-2.27717881467369,-2.27406612251968,-2.21848179217728,
-2.16798442556103,-2.12365006701894,-2.12033520914686,-2.11878068161532,
-2.11759325401149,-2.11646475329001,-2.11456472847643,-2.10954640706296,
-2.03056631304233,-1.98625197267401,-1.96020852560816,-1.95807541347298,
-1.95722540624879,-1.9566055912339,-1.95593544386434,-1.95501367391308,
-1.95286030009851,-1.91733023238687,-1.82973793937463,-1.80119276547675,
-1.79774541700403,-1.7961828540386,-1.79499004423848,-1.79371896620784,
-1.79174037100798,-1.78567576394416,-1.69272447714349,-1.63900010488334,
-1.63575159526142,-1.63462576434238,-1.63398414622884,-1.6333907204264,
-1.63257283279629,-1.63096523114785,-1.61968703672752,-1.59022259506031,
-1.49518191015856,-1.49267422447255,-1.47752745360438,-1.47494503232474,
-1.47339660143541,-1.47220609673132,-1.47092918442724,-1.46892427052881,
-1.46264409090269,-1.42690999405084,-1.32154755052495,-1.3146200421444,
-1.31251930649618,-1.31167479258714,-1.3110563284359,-1.31039906930294,
-1.30949922829901,-1.30849058227328,-1.30676236431469,-1.257671083213,-1.18186317266664,
-1.17475107311608,-1.155135983372,-1.15202787791082,-1.15051360792592,-1.14933140816592,
-1.14802550415524,-1.14589144944102,-1.13845443727308,-1.09126263659276,
-1.01569115322376,-0.991932213817203,-0.98984229359769,-0.988999638701811,
-0.988381639070366,-0.987723788123036,-0.986822593831915,-0.985811346896852,
-0.984076772760184,-0.980413871624433,-0.955831890316237,-0.906774771954784,
-0.86096833305819,-0.833014917578596,-0.829585267799973,-0.828025701130271,
-0.826833098888544,-0.82556022544062,-0.823574680047915,-0.817456864744306,
-0.783215387031529,-0.768835710602314,-0.683196082462364,-0.682162536409167,
-0.680308173655444,-0.668726863554091,-0.666961477934312,-0.666120676476328,
-0.66548236205044,-0.664770917480712,-0.663625614522972,-0.662266381104344,
-0.659642642599554,-0.653214775777888,-0.632740345273278,-0.583319172724665,
-0.535379122049546,-0.529824524948346,-0.509872094008693,-0.506747968409015,
-0.505230323206139,-0.504047494304743,-0.502742934345031,-0.500615673948938,
-0.49324697151785,-0.446795938016764,-0.4361108543253,-0.427447163777085,
-0.420143277630098,-0.413835415115689,-0.408291773102417,-0.350202709489139,
-0.345362526340499,-0.344060842045815,-0.343300938166315,-0.342646684094746,
-0.34185101991378,-0.340331163160333,-0.33840631424111,-0.334186616723762,
-0.321861649607299,-0.300194475951382,-0.204487071698002,-0.186940368902747,
-0.183971731609116,-0.182464963680236,-0.181283563882519,-0.179973357195922,
-0.17782045512056,-0.170200196877061,-0.14453194325761,-0.116681991627422,
-0.0410510682472698,-0.0368848661310568,-0.0355407581861974,-0.0233865722114733,
-0.021596184330195,-0.0207505582788536,-0.0201095965444524,-0.0194954147846064,
-0.0187829799930978,-0.0177682625203108,-0.0160252307618027,-0.000956555014723939),
 .UNSPECIFIED.);
#881=B_SPLINE_CURVE_WITH_KNOTS('',3,(#67420,#67421,#67422,#67423,#67424,
#67425,#67426,#67427,#67428,#67429,#67430,#67431,#67432,#67433,#67434,#67435,
#67436,#67437,#67438,#67439,#67440,#67441,#67442,#67443,#67444,#67445,#67446,
#67447,#67448,#67449,#67450,#67451,#67452,#67453,#67454,#67455,#67456,#67457,
#67458,#67459,#67460,#67461,#67462,#67463,#67464,#67465,#67466,#67467,#67468,
#67469,#67470,#67471,#67472,#67473,#67474,#67475,#67476,#67477,#67478,#67479,
#67480,#67481,#67482,#67483,#67484,#67485,#67486,#67487,#67488,#67489,#67490,
#67491,#67492,#67493,#67494,#67495,#67496,#67497,#67498,#67499,#67500,#67501,
#67502,#67503,#67504,#67505,#67506,#67507,#67508,#67509,#67510,#67511,#67512,
#67513,#67514,#67515,#67516,#67517,#67518,#67519,#67520,#67521,#67522,#67523,
#67524,#67525,#67526,#67527,#67528,#67529,#67530,#67531,#67532,#67533,#67534,
#67535,#67536,#67537,#67538,#67539,#67540,#67541,#67542,#67543,#67544,#67545,
#67546,#67547,#67548,#67549,#67550,#67551,#67552,#67553,#67554,#67555,#67556,
#67557,#67558,#67559,#67560,#67561,#67562,#67563,#67564,#67565,#67566,#67567,
#67568,#67569,#67570,#67571,#67572,#67573,#67574,#67575,#67576,#67577,#67578,
#67579,#67580,#67581,#67582,#67583,#67584,#67585,#67586,#67587,#67588,#67589,
#67590,#67591,#67592,#67593,#67594,#67595,#67596,#67597,#67598,#67599,#67600,
#67601,#67602,#67603,#67604,#67605,#67606,#67607,#67608,#67609,#67610,#67611,
#67612,#67613,#67614,#67615,#67616,#67617,#67618,#67619,#67620,#67621,#67622,
#67623,#67624,#67625,#67626,#67627,#67628,#67629,#67630,#67631,#67632,#67633,
#67634,#67635,#67636,#67637,#67638,#67639,#67640,#67641,#67642,#67643,#67644,
#67645,#67646,#67647,#67648,#67649,#67650,#67651,#67652,#67653,#67654,#67655,
#67656,#67657,#67658,#67659,#67660,#67661,#67662,#67663,#67664,#67665,#67666,
#67667,#67668,#67669,#67670,#67671,#67672,#67673,#67674,#67675,#67676,#67677,
#67678,#67679,#67680,#67681,#67682,#67683,#67684,#67685,#67686,#67687,#67688,
#67689,#67690,#67691,#67692,#67693,#67694,#67695,#67696,#67697,#67698,#67699,
#67700,#67701,#67702,#67703,#67704,#67705,#67706,#67707,#67708,#67709,#67710,
#67711,#67712,#67713,#67714,#67715,#67716,#67717,#67718,#67719,#67720,#67721,
#67722,#67723,#67724,#67725,#67726,#67727,#67728,#67729,#67730,#67731,#67732,
#67733,#67734,#67735,#67736,#67737,#67738,#67739,#67740,#67741,#67742,#67743,
#67744,#67745,#67746,#67747,#67748,#67749,#67750,#67751,#67752,#67753,#67754,
#67755,#67756,#67757,#67758,#67759,#67760,#67761,#67762,#67763,#67764,#67765,
#67766,#67767,#67768,#67769,#67770,#67771,#67772,#67773,#67774,#67775,#67776,
#67777,#67778,#67779,#67780,#67781,#67782,#67783,#67784,#67785,#67786,#67787,
#67788,#67789,#67790,#67791,#67792,#67793,#67794,#67795,#67796,#67797,#67798,
#67799,#67800,#67801,#67802,#67803,#67804,#67805,#67806,#67807,#67808,#67809,
#67810,#67811,#67812,#67813,#67814,#67815,#67816,#67817,#67818,#67819,#67820,
#67821,#67822,#67823,#67824,#67825,#67826,#67827,#67828,#67829,#67830,#67831,
#67832,#67833,#67834,#67835,#67836,#67837,#67838,#67839,#67840,#67841,#67842,
#67843,#67844,#67845,#67846,#67847,#67848,#67849,#67850,#67851,#67852,#67853,
#67854,#67855,#67856,#67857,#67858,#67859,#67860,#67861,#67862,#67863,#67864,
#67865,#67866,#67867,#67868,#67869,#67870,#67871,#67872,#67873,#67874,#67875,
#67876,#67877,#67878,#67879,#67880,#67881,#67882,#67883,#67884,#67885,#67886,
#67887,#67888,#67889,#67890,#67891,#67892,#67893,#67894,#67895,#67896,#67897,
#67898,#67899,#67900,#67901,#67902,#67903,#67904,#67905,#67906,#67907,#67908,
#67909,#67910,#67911,#67912,#67913,#67914,#67915,#67916,#67917,#67918,#67919,
#67920,#67921,#67922,#67923,#67924,#67925,#67926,#67927,#67928,#67929,#67930,
#67931,#67932,#67933,#67934,#67935,#67936,#67937,#67938,#67939,#67940,#67941,
#67942,#67943,#67944,#67945,#67946,#67947,#67948,#67949),.UNSPECIFIED.,
 .F.,.F.,(4,2,2,2,2,2,2,2,2,2,2,2,2,2,2,2,2,2,2,2,2,2,2,2,2,2,2,2,2,2,2,
2,2,2,2,2,2,2,2,2,2,2,2,2,2,2,2,2,2,2,2,2,2,2,2,2,2,2,2,2,2,2,2,2,2,2,2,
2,2,2,2,2,2,2,2,2,2,2,2,2,2,2,2,2,2,2,2,2,2,2,2,2,2,2,2,2,2,2,2,2,2,2,2,
2,2,2,2,2,2,2,2,2,2,2,2,2,2,2,2,2,2,2,2,2,2,2,2,2,2,2,2,2,2,2,2,2,2,2,2,
2,2,2,2,2,2,2,2,2,2,2,2,2,2,2,2,2,2,2,2,2,2,2,2,2,2,2,2,2,2,2,2,2,2,2,2,
2,2,2,2,2,2,2,2,2,2,2,2,2,2,2,2,2,2,2,2,2,2,2,2,2,2,2,2,2,2,2,2,2,2,2,2,
2,2,2,2,2,2,2,2,2,2,2,2,2,2,2,2,2,2,2,2,2,2,2,2,2,2,2,2,2,2,2,2,2,2,2,2,
2,2,2,2,2,2,2,2,2,2,2,2,2,2,2,2,2,4),(-4.06084443590171,-3.97731844721829,
-3.93012302769939,-3.92268671047794,-3.92055359085664,-3.91924841914854,
-3.91806698699717,-3.91655384555902,-3.91344856904977,-3.89386413803157,
-3.88842159406268,-3.88089843136169,-3.79607080323638,-3.78292953552254,
-3.76765849608381,-3.76272957180426,-3.76057197191954,-3.75890746928953,
-3.75808042143403,-3.75744175032905,-3.75680184122872,-3.75587690222132,
-3.75326843823274,-3.69679524389133,-3.65912322151103,-3.6188521365159,
-3.6013974109016,-3.59862125802278,-3.59717535706437,-3.59611291663646,
-3.5949666115149,-3.59331816108274,-3.58871831869473,-3.58692534334826,
-3.48321037349395,-3.45341045788923,-3.44305029103678,-3.43933112039623,
-3.43757725524908,-3.43655829868936,-3.43565087655506,-3.43499188242287,
-3.43437530588361,-3.43353751199936,-3.43189485329819,-3.41890703208826,
-3.37418909144057,-3.33029027840057,-3.27997440763444,-3.27645134742111,
-3.27485771137402,-3.27366442825823,-3.27254791114154,-3.27101010929729,
-3.26710538130226,-3.20394976652324,-3.12055093104217,-3.11680133934631,
-3.11503688294052,-3.11401358039626,-3.11310367186522,-3.11244391816564,
-3.1118280258814,-3.11099313167253,-3.10936199057641,-3.0966993724259,-3.09381984545065,
-3.093478029282,-2.99528169901182,-2.9608008203631,-2.95465709029732,-2.95266892414645,
-2.9513958489468,-2.95020410319279,-2.94864715778687,-2.94522935727576,
-2.91761183553983,-2.82958504033269,-2.81039042432415,-2.79460568111286,
-2.79260839411531,-2.79149151042415,-2.79073712703266,-2.7900189074072,
-2.78937618016919,-2.78853174954314,-2.78679278594318,-2.77577492449043,
-2.70487375518483,-2.66572993117447,-2.64004815008967,-2.63502120430159,
-2.63127786836222,-2.62964410642004,-2.62844394520468,-2.62733739106485,
-2.62583847580987,-2.62291388032471,-2.60001453652611,-2.58450843031352,
-2.50841007158774,-2.48167750172757,-2.47013015376645,-2.46851372447391,
-2.46769406938381,-2.46703802300443,-2.46628383865707,-2.46500584022129,
-2.46039222868414,-2.36602724824773,-2.34292561561298,-2.3175308128802,
-2.30980485047108,-2.30764189774675,-2.30632976751042,-2.30514933912842,
-2.30364752055451,-2.30070034169906,-2.28354619511033,-2.18872419607834,
-2.15878715882718,-2.14741069613728,-2.14579986480449,-2.1449813418037,
-2.14438786971759,-2.14374660745554,-2.14262241561173,-2.13938528123742,
-2.08114588283808,-2.03157579402172,-2.01307693557964,-2.00797983300827,
-1.98878667378008,-1.98569870450949,-1.98418858696784,-1.98300704543098,
-1.98169922705864,-1.979556047706,-1.9720280966689,-1.92383814060439,-1.82889908868079,
-1.82422440359268,-1.82293983081376,-1.8221840032555,-1.82152795431853,
-1.82071013145765,-1.81910314005874,-1.80784754246262,-1.77418251211763,
-1.67006548941637,-1.66862339036771,-1.66375430990932,-1.66187806205275,
-1.66075414973902,-1.65956446989974,-1.65799513476366,-1.65460292151076,
-1.60011961093511,-1.50588822765113,-1.50134050655198,-1.50006927380101,
-1.4993165517208,-1.49866014642657,-1.49783793492101,-1.49620969997124,
-1.48430465313199,-1.45785444564072,-1.38333629801203,-1.36645709435033,
-1.34347683540578,-1.34054864286672,-1.33904858522402,-1.33794153254176,
-1.33676559664923,-1.33518246050896,-1.33342205990064,-1.33045010742261,
-1.28128841473332,-1.20976804633029,-1.18020074706501,-1.17800887442522,
-1.17714867511123,-1.17652610644557,-1.17585766267407,-1.17494621394699,
-1.17285201891497,-1.13082007825071,-1.02988316365458,-1.02267070891844,
-1.01813299353101,-1.01649348720987,-1.01534933406244,-1.014202716672,-1.01273950696304,
-1.0098500321605,-1.00616495475597,-0.946074159473671,-0.860317693906782,
-0.855845311144342,-0.854567174623528,-0.853820254104679,-0.853228834796903,
-0.85242983429433,-0.850912863838098,-0.841955917945522,-0.822874644488806,
-0.777053495135603,-0.702006106977066,-0.695914900793396,-0.693856525683937,
-0.692696400998567,-0.691538152374137,-0.690101798401045,-0.687340255289911,
-0.683854370429263,-0.676244259994933,-0.654390455663302,-0.61481570883021,
-0.537397001801655,-0.533130306169542,-0.531875107490516,-0.53120733567724,
-0.530558479526669,-0.529760259996369,-0.528247077842323,-0.519374398651029,
-0.500418614801332,-0.475702843733456,-0.468574661030553,-0.462436211239311,
-0.408134104551966,-0.401992201293512,-0.394546586384605,-0.375124342614916,
-0.372024920205923,-0.370512250711903,-0.369330102597084,-0.368228095799293,
-0.366327224538797,-0.360835064555212,-0.352636062866895,-0.3284755498035,
-0.307074065932593,-0.22567827891349,-0.225069469539524,-0.22427579642959,
-0.211441321875502,-0.209803396543811,-0.208966564655551,-0.208349988887942,
-0.207676794989064,-0.206739388591995,-0.204496551838612,-0.165878030590847,
-0.0945384025142255,-0.0877800856059834,-0.0532014966570062,-0.0495858368248017,
-0.0481357412690161,-0.0469313773131904,-0.045825218747467,-0.0446218283110119,
-0.0429926733844762,-0.0403368641217892,-0.000956521092448796),
 .UNSPECIFIED.);
#882=B_SPLINE_CURVE_WITH_KNOTS('',3,(#67951,#67952,#67953,#67954,#67955,
#67956,#67957,#67958,#67959,#67960,#67961,#67962,#67963,#67964,#67965,#67966,
#67967,#67968,#67969,#67970,#67971,#67972,#67973,#67974,#67975,#67976,#67977,
#67978,#67979,#67980,#67981,#67982,#67983,#67984,#67985,#67986,#67987,#67988,
#67989,#67990,#67991,#67992,#67993,#67994,#67995,#67996,#67997,#67998,#67999,
#68000,#68001,#68002,#68003,#68004,#68005,#68006,#68007,#68008,#68009,#68010,
#68011,#68012,#68013,#68014,#68015,#68016,#68017,#68018,#68019,#68020,#68021,
#68022,#68023,#68024,#68025,#68026,#68027,#68028,#68029,#68030,#68031,#68032,
#68033,#68034,#68035,#68036,#68037,#68038,#68039,#68040,#68041,#68042,#68043,
#68044,#68045,#68046,#68047,#68048,#68049,#68050,#68051,#68052,#68053,#68054,
#68055,#68056,#68057,#68058,#68059,#68060,#68061,#68062,#68063,#68064,#68065,
#68066,#68067,#68068,#68069,#68070,#68071,#68072,#68073,#68074,#68075,#68076,
#68077,#68078,#68079,#68080,#68081,#68082,#68083,#68084,#68085,#68086,#68087,
#68088,#68089,#68090,#68091,#68092,#68093,#68094,#68095,#68096,#68097,#68098,
#68099,#68100,#68101,#68102,#68103,#68104,#68105,#68106,#68107,#68108,#68109,
#68110,#68111,#68112,#68113,#68114,#68115,#68116,#68117,#68118,#68119,#68120,
#68121,#68122,#68123,#68124,#68125,#68126,#68127,#68128,#68129,#68130,#68131,
#68132,#68133,#68134,#68135,#68136,#68137,#68138,#68139,#68140,#68141,#68142,
#68143,#68144,#68145,#68146,#68147,#68148,#68149,#68150,#68151,#68152,#68153,
#68154,#68155,#68156,#68157,#68158,#68159,#68160,#68161,#68162,#68163,#68164,
#68165,#68166,#68167,#68168,#68169,#68170,#68171,#68172,#68173,#68174,#68175,
#68176,#68177,#68178,#68179,#68180,#68181,#68182,#68183,#68184,#68185,#68186,
#68187,#68188,#68189,#68190,#68191,#68192,#68193,#68194,#68195,#68196,#68197,
#68198,#68199,#68200,#68201,#68202,#68203,#68204,#68205,#68206,#68207,#68208,
#68209,#68210,#68211,#68212,#68213,#68214,#68215,#68216,#68217,#68218,#68219,
#68220,#68221,#68222,#68223,#68224,#68225,#68226,#68227,#68228,#68229,#68230,
#68231,#68232,#68233,#68234,#68235,#68236,#68237,#68238,#68239,#68240,#68241,
#68242,#68243,#68244,#68245,#68246,#68247,#68248,#68249,#68250,#68251,#68252,
#68253,#68254,#68255,#68256,#68257,#68258,#68259,#68260,#68261,#68262,#68263,
#68264,#68265,#68266,#68267,#68268,#68269,#68270,#68271,#68272,#68273,#68274,
#68275,#68276,#68277,#68278,#68279,#68280,#68281,#68282,#68283,#68284,#68285,
#68286,#68287,#68288,#68289,#68290,#68291,#68292,#68293,#68294,#68295,#68296,
#68297,#68298,#68299,#68300,#68301,#68302,#68303,#68304,#68305,#68306,#68307,
#68308,#68309,#68310,#68311,#68312,#68313,#68314,#68315,#68316,#68317,#68318,
#68319,#68320,#68321,#68322,#68323,#68324,#68325,#68326,#68327,#68328,#68329,
#68330,#68331,#68332,#68333,#68334,#68335,#68336,#68337,#68338,#68339,#68340,
#68341,#68342,#68343,#68344,#68345,#68346,#68347,#68348,#68349,#68350,#68351,
#68352,#68353,#68354,#68355,#68356,#68357,#68358,#68359,#68360,#68361,#68362,
#68363,#68364,#68365,#68366,#68367,#68368,#68369,#68370,#68371,#68372,#68373,
#68374,#68375,#68376,#68377,#68378,#68379,#68380,#68381,#68382,#68383,#68384,
#68385,#68386,#68387,#68388,#68389,#68390,#68391,#68392,#68393,#68394,#68395,
#68396,#68397,#68398,#68399,#68400,#68401,#68402,#68403,#68404,#68405,#68406,
#68407,#68408,#68409,#68410,#68411,#68412,#68413,#68414,#68415,#68416,#68417,
#68418,#68419,#68420,#68421,#68422,#68423,#68424,#68425,#68426,#68427,#68428,
#68429,#68430,#68431,#68432,#68433,#68434,#68435,#68436,#68437,#68438,#68439,
#68440,#68441,#68442,#68443,#68444,#68445,#68446,#68447,#68448,#68449,#68450,
#68451,#68452,#68453,#68454,#68455,#68456,#68457,#68458,#68459,#68460,#68461,
#68462,#68463,#68464,#68465,#68466,#68467,#68468,#68469,#68470,#68471,#68472,
#68473,#68474,#68475,#68476,#68477,#68478,#68479,#68480,#68481,#68482,#68483,
#68484,#68485,#68486,#68487,#68488,#68489,#68490,#68491,#68492,#68493,#68494,
#68495,#68496,#68497,#68498,#68499,#68500,#68501,#68502),.UNSPECIFIED.,
 .F.,.F.,(4,2,2,2,2,2,2,2,2,2,2,2,2,2,2,2,2,2,2,2,2,2,2,2,2,2,2,2,2,2,2,
2,2,2,2,2,2,2,2,2,2,2,2,2,2,2,2,2,2,2,2,2,2,2,2,2,2,2,2,2,2,2,2,2,2,2,2,
2,2,2,2,2,2,2,2,2,2,2,2,2,2,2,2,2,2,2,2,2,2,2,2,2,2,2,2,2,2,2,2,2,2,2,2,
2,2,2,2,2,2,2,2,2,2,2,2,2,2,2,2,2,2,2,2,2,2,2,2,2,2,2,2,2,2,2,2,2,2,2,2,
2,2,2,2,2,2,2,2,2,2,2,2,2,2,2,2,2,2,2,2,2,2,2,2,2,2,2,2,2,2,2,2,2,2,2,2,
2,2,2,2,2,2,2,2,2,2,2,2,2,2,2,2,2,2,2,2,2,2,2,2,2,2,2,2,2,2,2,2,2,2,2,2,
2,2,2,2,2,2,2,2,2,2,2,2,2,2,2,2,2,2,2,2,2,2,2,2,2,2,2,2,2,2,2,2,2,2,2,2,
2,2,2,2,2,2,2,2,2,2,2,2,2,2,2,2,2,2,2,2,2,2,2,2,2,2,2,2,4),(-4.06011575675384,
-3.98757700257165,-3.95179295117725,-3.94861885117166,-3.94633076893291,
-3.94538589119552,-3.94471144585061,-3.94409668820049,-3.94326654170211,
-3.94165409237231,-3.9294847635718,-3.92815873945996,-3.8371688991084,-3.81600790057753,
-3.78989226159108,-3.78616584462785,-3.78488556839697,-3.78378401734363,
-3.78260194174737,-3.78108739400615,-3.77797717769672,-3.75830867887014,
-3.75126249675961,-3.74522684226998,-3.70026359103249,-3.66294429751494,
-3.62904013491075,-3.62436444415706,-3.62312358873041,-3.62238511183924,
-3.62172669405768,-3.62088267751096,-3.61914600486653,-3.60817875336548,
-3.534204661898,-3.50011203236926,-3.48153218048321,-3.4711617681877,-3.46456192409247,
-3.46254687397687,-3.46126826934228,-3.46008609530097,-3.45857051990397,
-3.45545500749174,-3.43567052689144,-3.43017071591548,-3.34240908177447,
-3.30658352529893,-3.30176815741044,-3.30051450987388,-3.29977312798081,
-3.29911517319415,-3.29827583921713,-3.29656287114189,-3.28608566833394,
-3.19298388606223,-3.14905271954859,-3.14434807955539,-3.1408234020704,
-3.13923539261104,-3.1380590030997,-3.13695285958045,-3.13545582989029,
-3.13178905497669,-3.09138338920161,-3.01262550483756,-2.98329290309546,
-2.97898508725235,-2.97777949802357,-2.97704888398538,-2.97638866411616,
-2.97554444467752,-2.97376066980215,-2.96175290085045,-2.92069757376718,
-2.85571352021303,-2.82475412584975,-2.82092423448123,-2.81881722971635,
-2.81705683755318,-2.81581670580873,-2.81462140651379,-2.81304480258912,
-2.8095217278567,-2.77841076753186,-2.69335461663846,-2.65802227558515,
-2.65578290342084,-2.6548462207046,-2.65417328206735,-2.65355674813457,
-2.65271969856161,-2.65108053710975,-2.63820379829682,-2.63744615582557,
-2.63450514595683,-2.55770344715032,-2.5157261156125,-2.49790757702579,
-2.49511594211743,-2.49366637466137,-2.4926030644969,-2.4914575737486,-2.4898132755788,
-2.48524404129061,-2.41046298206508,-2.3626967212315,-2.33756644554804,
-2.33363522436984,-2.33246880727037,-2.3317469284101,-2.33108414115988,
-2.33022243572056,-2.32841458727274,-2.31526623985899,-2.31224590514854,
-2.30847676164208,-2.30643466094583,-2.30396204516384,-2.21246096227134,
-2.17965017689615,-2.17369100507901,-2.17172542755749,-2.17045712463039,
-2.16926292244687,-2.16769273560219,-2.16503660768012,-2.14849761943066,
-2.0531487337881,-2.0304385676575,-2.02855419268785,-2.02554854596311,-2.02457276282454,
-2.01197596165693,-2.01034713486672,-2.00951272663943,-2.0088968507714,
-2.00822329522742,-2.00728340251416,-2.0050252360139,-2.00190359451685,
-1.96725877699995,-1.91300194891421,-1.85430688137431,-1.85041792491926,
-1.84888245597491,-1.84776627522264,-1.84657207737013,-1.84497502417979,
-1.84143544803906,-1.83674695449518,-1.79307319778345,-1.70001592127376,
-1.68914489406369,-1.6874120736328,-1.68656864404352,-1.68591009071925,
-1.68517082599969,-1.68392719157903,-1.67922448193481,-1.6449754465871,
-1.53591198361227,-1.52857662093458,-1.52636040423623,-1.52503611631389,
-1.52397534737126,-1.52254879379158,-1.51986618239382,-1.50457141420902,
-1.47584647183738,-1.38520397836188,-1.38252745292843,-1.38071950166956,
-1.37985698306795,-1.37858484437319,-1.36634664710396,-1.36473132157762,
-1.3639003473568,-1.3632852967005,-1.36261086306937,-1.36166659250757,-1.35943583542082,
-1.35633503006023,-1.32212998844326,-1.24415999997894,-1.2275810356317,
-1.2074179944024,-1.2042845458431,-1.20276515978735,-1.20158223274631,-1.20027884091198,
-1.19819876358201,-1.19124424286824,-1.14876100407268,-1.07984632646153,
-1.06680786533071,-1.04415446176051,-1.042087245498,-1.04124852029701,-1.04063150433497,
-1.0399588148753,-1.03902383731458,-1.03686232211116,-1.03387335306232,
-1.00191178713765,-0.940581954475832,-0.885973531995667,-0.882112962732701,
-0.880582232716324,-0.879467220111196,-0.878272127677422,-0.876670165898123,
-0.873197286235571,-0.849273271456177,-0.83064978468061,-0.772638226546301,
-0.761543247602596,-0.731816544990858,-0.720968354552017,-0.71923673911755,
-0.718393585078587,-0.71773510295712,-0.716995764373869,-0.716227361141434,
-0.713582327241202,-0.709737068389898,-0.698893396978624,-0.682418563074156,
-0.631929507295326,-0.591124604455596,-0.562677562324951,-0.559232353497958,
-0.557669862960634,-0.556476738326142,-0.555204966663074,-0.553224555489426,
-0.54727617640514,-0.513769534126682,-0.461111344103762,-0.400772719599086,
-0.397349708037988,-0.396199057993426,-0.395552345444014,-0.394959969307072,
-0.394152139281111,-0.393287639585438,-0.389404893637406,-0.383104203831881,
-0.380657451845361,-0.34823028593471,-0.317500596304946,-0.272270897944792,
-0.266112004474246,-0.259428211114443,-0.239576022223285,-0.236456531740176,
-0.234939822637774,-0.233757127401935,-0.232452109154229,-0.231108815591459,
-0.229133120753417,-0.212888424794893,-0.172097567544964,-0.157913890404894,
-0.143347691792025,-0.0865974685278843,-0.0757781157366671,-0.0740478200476607,
-0.0732048887942819,-0.0725463861762182,-0.0718068166944389,-0.0710381076872037,
-0.069887180503094,-0.0678043440310872,-0.0631073317543311,-0.000957274032640893),
 .UNSPECIFIED.);
#883=B_SPLINE_CURVE_WITH_KNOTS('',3,(#68504,#68505,#68506,#68507,#68508,
#68509,#68510,#68511,#68512,#68513,#68514,#68515,#68516,#68517,#68518,#68519,
#68520,#68521,#68522,#68523,#68524,#68525,#68526,#68527,#68528,#68529,#68530,
#68531,#68532,#68533,#68534,#68535,#68536,#68537,#68538,#68539,#68540,#68541,
#68542,#68543,#68544,#68545,#68546,#68547,#68548,#68549,#68550,#68551,#68552,
#68553,#68554,#68555,#68556,#68557,#68558,#68559,#68560,#68561,#68562,#68563,
#68564,#68565,#68566,#68567,#68568,#68569,#68570,#68571,#68572,#68573,#68574,
#68575,#68576,#68577,#68578,#68579,#68580,#68581,#68582,#68583,#68584,#68585,
#68586,#68587,#68588,#68589,#68590,#68591,#68592,#68593,#68594,#68595,#68596,
#68597,#68598,#68599,#68600,#68601,#68602,#68603,#68604,#68605,#68606,#68607,
#68608,#68609,#68610,#68611,#68612,#68613,#68614,#68615,#68616,#68617,#68618,
#68619,#68620,#68621,#68622,#68623,#68624,#68625,#68626,#68627,#68628,#68629,
#68630,#68631,#68632,#68633,#68634,#68635,#68636,#68637,#68638,#68639,#68640,
#68641,#68642,#68643,#68644,#68645,#68646,#68647,#68648,#68649,#68650,#68651,
#68652,#68653,#68654,#68655,#68656,#68657,#68658,#68659,#68660,#68661,#68662,
#68663,#68664,#68665,#68666,#68667,#68668,#68669,#68670,#68671,#68672,#68673,
#68674,#68675,#68676,#68677,#68678,#68679,#68680,#68681,#68682,#68683,#68684,
#68685,#68686,#68687,#68688,#68689,#68690,#68691,#68692,#68693,#68694,#68695,
#68696,#68697,#68698,#68699,#68700,#68701,#68702,#68703,#68704,#68705,#68706,
#68707,#68708,#68709,#68710,#68711,#68712,#68713,#68714,#68715,#68716,#68717,
#68718,#68719,#68720,#68721,#68722,#68723,#68724,#68725,#68726,#68727,#68728,
#68729,#68730,#68731,#68732,#68733,#68734,#68735,#68736,#68737,#68738,#68739,
#68740,#68741,#68742,#68743,#68744,#68745,#68746,#68747,#68748,#68749,#68750,
#68751,#68752,#68753,#68754,#68755,#68756,#68757,#68758,#68759,#68760,#68761,
#68762,#68763,#68764,#68765,#68766,#68767,#68768,#68769,#68770,#68771,#68772,
#68773,#68774,#68775,#68776,#68777,#68778,#68779,#68780,#68781,#68782,#68783,
#68784,#68785,#68786,#68787,#68788,#68789,#68790,#68791,#68792,#68793,#68794,
#68795,#68796,#68797,#68798,#68799,#68800,#68801,#68802,#68803,#68804,#68805,
#68806,#68807,#68808,#68809,#68810,#68811,#68812,#68813,#68814,#68815,#68816,
#68817,#68818,#68819,#68820,#68821,#68822,#68823,#68824,#68825,#68826,#68827,
#68828,#68829,#68830,#68831,#68832,#68833,#68834,#68835,#68836,#68837,#68838,
#68839,#68840,#68841,#68842,#68843,#68844,#68845,#68846,#68847,#68848,#68849,
#68850,#68851,#68852,#68853,#68854,#68855,#68856,#68857,#68858,#68859,#68860,
#68861,#68862,#68863,#68864,#68865,#68866,#68867,#68868,#68869,#68870,#68871,
#68872,#68873,#68874,#68875,#68876,#68877,#68878,#68879,#68880,#68881,#68882,
#68883,#68884,#68885,#68886,#68887,#68888,#68889,#68890,#68891,#68892,#68893,
#68894,#68895,#68896,#68897,#68898,#68899,#68900,#68901,#68902,#68903,#68904,
#68905,#68906,#68907,#68908,#68909,#68910,#68911,#68912,#68913,#68914,#68915,
#68916,#68917,#68918,#68919,#68920,#68921,#68922,#68923,#68924,#68925,#68926,
#68927,#68928,#68929,#68930,#68931,#68932,#68933,#68934,#68935,#68936,#68937,
#68938,#68939,#68940,#68941,#68942,#68943,#68944,#68945,#68946,#68947,#68948,
#68949,#68950,#68951,#68952,#68953,#68954,#68955,#68956,#68957,#68958,#68959,
#68960,#68961,#68962,#68963,#68964,#68965,#68966,#68967,#68968,#68969,#68970,
#68971,#68972,#68973,#68974,#68975,#68976,#68977,#68978,#68979,#68980,#68981,
#68982,#68983,#68984,#68985,#68986,#68987,#68988,#68989,#68990,#68991,#68992,
#68993,#68994,#68995,#68996,#68997,#68998,#68999,#69000,#69001,#69002,#69003,
#69004,#69005,#69006,#69007,#69008,#69009,#69010,#69011,#69012,#69013,#69014,
#69015,#69016,#69017,#69018,#69019,#69020,#69021,#69022,#69023,#69024,#69025,
#69026,#69027,#69028,#69029,#69030,#69031,#69032,#69033,#69034,#69035,#69036,
#69037,#69038,#69039),.UNSPECIFIED.,.F.,.F.,(4,2,2,2,2,2,2,2,2,2,2,2,2,
2,2,2,2,2,2,2,2,2,2,2,2,2,2,2,2,2,2,2,2,2,2,2,2,2,2,2,2,2,2,2,2,2,2,2,2,
2,2,2,2,2,2,2,2,2,2,2,2,2,2,2,2,2,2,2,2,2,2,2,2,2,2,2,2,2,2,2,2,2,2,2,2,
2,2,2,2,2,2,2,2,2,2,2,2,2,2,2,2,2,2,2,2,2,2,2,2,2,2,2,2,2,2,2,2,2,2,2,2,
2,2,2,2,2,2,2,2,2,2,2,2,2,2,2,2,2,2,2,2,2,2,2,2,2,2,2,2,2,2,2,2,2,2,2,2,
2,2,2,2,2,2,2,2,2,2,2,2,2,2,2,2,2,2,2,2,2,2,2,2,2,2,2,2,2,2,2,2,2,2,2,2,
2,2,2,2,2,2,2,2,2,2,2,2,2,2,2,2,2,2,2,2,2,2,2,2,2,2,2,2,2,2,2,2,2,2,2,2,
2,2,2,2,2,2,2,2,2,2,2,2,2,2,2,2,2,2,2,2,2,2,2,2,2,2,2,2,2,2,2,2,2,2,2,2,
2,2,4),(-4.06100195960022,-3.97862899521379,-3.975726211888,-3.97399450084426,
-3.97241069470506,-3.97121883560045,-3.97009931297994,-3.9682455270532,
-3.96351385378274,-3.88450523397763,-3.87102826455039,-3.85862758370722,
-3.82721889707641,-3.81688445820489,-3.81230049299831,-3.81139301648855,
-3.81072297947515,-3.81004928207542,-3.80943384896562,-3.80860085773195,
-3.80697720747016,-3.79452034828951,-3.79343651670533,-3.79265394528713,
-3.74355949624964,-3.70412651921958,-3.67004977845332,-3.65934447765577,
-3.65258031504339,-3.65104663765605,-3.64960591595634,-3.64854374960308,
-3.64739432248811,-3.64573552695692,-3.64106900295924,-3.56702032070852,
-3.52008512077055,-3.49199828347988,-3.48931196432979,-3.48853761920477,
-3.487794153824,-3.48713659060821,-3.48630073692835,-3.48460498843525,-3.47447073051979,
-3.4298234015499,-3.37824996769656,-3.35670039542035,-3.33234988232163,
-3.32893566749388,-3.32734043032294,-3.326146651058,-3.32503017944141,-3.3234932403519,
-3.31959492563555,-3.2589082594984,-3.20794941930971,-3.17902172502668,
-3.17159441385538,-3.16723800355652,-3.16600309071061,-3.16526025329817,
-3.16460256402472,-3.16376564346453,-3.16206465917049,-3.15182327288676,
-3.121932906067,-3.06177317081537,-3.01497428168572,-3.00760173456035,-3.00545688269464,
-3.00414864410296,-3.0029671135387,-3.00145754966638,-2.99837260032162,
-2.97924519558001,-2.97611557523412,-2.96755722429297,-2.95015561030973,
-2.88087076760129,-2.84914898335842,-2.84617294660422,-2.84401224332467,
-2.84309270843413,-2.8424194752211,-2.84180336428273,-2.84096788074587,
-2.83933472216725,-2.82662224290997,-2.82574073141467,-2.82536810031513,
-2.81781353991909,-2.73947889040378,-2.69240103249051,-2.68499915694957,
-2.68285341278672,-2.68154498750054,-2.68036352084798,-2.67885435969665,
-2.6757713553391,-2.65668405106025,-2.64867288027682,-2.55788468760732,
-2.52362255340759,-2.52135176543623,-2.52040975057213,-2.51973580573709,
-2.51912039121322,-2.51828777363767,-2.51666587637117,-2.50426233389479,
-2.41723490725594,-2.3697152588366,-2.36224731954546,-2.36011016997924,
-2.35880362887595,-2.35762167338357,-2.35610885494249,-2.35300773732636,
-2.33353905516213,-2.32815347891129,-2.30937354338989,-2.27545181797462,
-2.22803466344111,-2.20888777219725,-2.19986547228952,-2.1983457270625,
-2.19754621477197,-2.19695482889031,-2.19620849758587,-2.1949326737715,
-2.19048023761434,-2.10172838425506,-2.04775783822248,-2.03973639725366,
-2.03754434992121,-2.03622559749815,-2.03504624151239,-2.0335553224936,
-2.03121765742446,-2.01759028407343,-1.99057914725422,-1.88690433179769,
-1.87730510045499,-1.87565793686551,-1.87482055450431,-1.87416272281584,
-1.8734199605097,-1.87216044280701,-1.86728058781452,-1.84407759867751,
-1.79801636916948,-1.75408599160187,-1.71937799571806,-1.715806871268,-1.71433995229095,
-1.71324112016464,-1.7120336612542,-1.71036136535635,-1.7063998721415,-1.65612314841707,
-1.56594781731917,-1.55474359554411,-1.55299533303979,-1.55214881284511,
-1.55148988008721,-1.55075235259725,-1.54951657773581,-1.54489908216215,
-1.51177779063074,-1.42589358949798,-1.39636497592263,-1.39323445933923,
-1.39168294766779,-1.390562456198,-1.38937048781632,-1.38778810902263,-1.38432807756073,
-1.36673379967075,-1.35061402519731,-1.30531227803955,-1.24422311397194,
-1.23210107052551,-1.23031204068527,-1.22946666986523,-1.22880614675318,
-1.22807583025985,-1.22689626393047,-1.22284184182671,-1.19617980012805,
-1.1284526045915,-1.07437601000282,-1.07052003403702,-1.0689900616717,-1.06787522581011,
-1.0666799690242,-1.0650771733889,-1.06150707000265,-1.05676838840711,-1.01229101143329,
-0.943429311678271,-0.93141617378817,-0.929278532842363,-0.924753906773191,
-0.909602926568883,-0.90769735812237,-0.906829883771583,-0.906166099287072,
-0.905446675041333,-0.904314803233453,-0.900679453593819,-0.894897069443431,
-0.876176506298365,-0.821707988418639,-0.75238293335182,-0.748045292673333,
-0.746436558509093,-0.745300694707331,-0.744234222110286,-0.742761489522267,
-0.739859193975525,-0.719320944712954,-0.689516220297427,-0.633298405655588,
-0.588200843627052,-0.585456242761711,-0.584510892211894,-0.583865010115297,
-0.583272445978597,-0.582641719848806,-0.581347539870029,-0.576073715852917,
-0.566593280987147,-0.541810763526414,-0.508511272998862,-0.430038070900999,
-0.425472286470002,-0.423828339898572,-0.422682822785653,-0.421619276202319,
-0.420169061877189,-0.417375078376827,-0.399832948230513,-0.359096910092,
-0.318631021463136,-0.274005810371374,-0.263971419869908,-0.262301571293539,
-0.261459305973149,-0.260800916626039,-0.260061038955666,-0.259291871724942,
-0.258139799704044,-0.246234842469268,-0.218053254730235,-0.196473021979129,
-0.127113466610081,-0.125487720877041,-0.120143229730793,-0.104830416061291,
-0.102238367774451,-0.100686838965146,-0.0994955297405637,-0.0982192981729564,
-0.096218672422179,-0.0939009296580686,-0.0844466177707292,-0.00095780636328563),
 .UNSPECIFIED.);
#884=B_SPLINE_CURVE_WITH_KNOTS('',3,(#69041,#69042,#69043,#69044,#69045,
#69046,#69047,#69048,#69049,#69050,#69051,#69052,#69053,#69054,#69055,#69056,
#69057,#69058,#69059,#69060,#69061,#69062,#69063,#69064,#69065,#69066,#69067,
#69068,#69069,#69070,#69071,#69072,#69073,#69074,#69075,#69076,#69077,#69078,
#69079,#69080,#69081,#69082,#69083,#69084,#69085,#69086,#69087,#69088,#69089,
#69090,#69091,#69092,#69093,#69094,#69095,#69096,#69097,#69098,#69099,#69100,
#69101,#69102,#69103,#69104,#69105,#69106,#69107,#69108,#69109,#69110,#69111,
#69112,#69113,#69114,#69115,#69116,#69117,#69118,#69119,#69120,#69121,#69122,
#69123,#69124,#69125,#69126,#69127,#69128,#69129,#69130,#69131,#69132,#69133,
#69134,#69135,#69136,#69137,#69138,#69139,#69140,#69141,#69142,#69143,#69144,
#69145,#69146,#69147,#69148,#69149,#69150,#69151,#69152,#69153,#69154,#69155,
#69156,#69157,#69158,#69159,#69160,#69161,#69162,#69163,#69164,#69165,#69166,
#69167,#69168,#69169,#69170,#69171,#69172,#69173,#69174,#69175,#69176,#69177,
#69178,#69179,#69180,#69181,#69182,#69183,#69184,#69185,#69186,#69187,#69188,
#69189,#69190,#69191,#69192,#69193,#69194,#69195,#69196,#69197,#69198,#69199,
#69200,#69201,#69202,#69203,#69204,#69205,#69206,#69207,#69208,#69209,#69210,
#69211,#69212,#69213,#69214,#69215,#69216,#69217,#69218,#69219,#69220,#69221,
#69222,#69223,#69224,#69225,#69226,#69227,#69228,#69229,#69230,#69231,#69232,
#69233,#69234,#69235,#69236,#69237,#69238,#69239,#69240,#69241,#69242,#69243,
#69244,#69245,#69246,#69247,#69248,#69249,#69250,#69251,#69252,#69253,#69254,
#69255,#69256,#69257,#69258,#69259,#69260,#69261,#69262,#69263,#69264,#69265,
#69266,#69267,#69268,#69269,#69270,#69271,#69272,#69273,#69274,#69275,#69276,
#69277,#69278,#69279,#69280,#69281,#69282,#69283,#69284,#69285,#69286,#69287,
#69288,#69289,#69290,#69291,#69292,#69293,#69294,#69295,#69296,#69297,#69298,
#69299,#69300,#69301,#69302,#69303,#69304,#69305,#69306,#69307,#69308,#69309,
#69310,#69311,#69312,#69313,#69314,#69315,#69316,#69317,#69318,#69319,#69320,
#69321,#69322,#69323,#69324,#69325,#69326,#69327,#69328,#69329,#69330,#69331,
#69332,#69333,#69334,#69335,#69336,#69337,#69338,#69339,#69340,#69341,#69342,
#69343,#69344,#69345,#69346,#69347,#69348,#69349,#69350,#69351,#69352,#69353,
#69354,#69355,#69356,#69357,#69358,#69359,#69360,#69361,#69362,#69363,#69364,
#69365,#69366,#69367,#69368,#69369,#69370,#69371,#69372,#69373,#69374,#69375,
#69376,#69377,#69378,#69379,#69380,#69381,#69382,#69383,#69384,#69385,#69386,
#69387,#69388,#69389,#69390,#69391,#69392,#69393,#69394,#69395,#69396,#69397,
#69398,#69399,#69400,#69401,#69402,#69403,#69404,#69405,#69406,#69407,#69408,
#69409,#69410,#69411,#69412,#69413,#69414,#69415,#69416,#69417,#69418,#69419,
#69420,#69421,#69422,#69423,#69424,#69425,#69426,#69427,#69428,#69429,#69430,
#69431,#69432,#69433,#69434,#69435,#69436,#69437,#69438,#69439,#69440,#69441,
#69442,#69443,#69444,#69445,#69446,#69447,#69448,#69449,#69450,#69451,#69452,
#69453,#69454,#69455,#69456,#69457,#69458,#69459,#69460,#69461,#69462,#69463,
#69464,#69465,#69466,#69467,#69468,#69469,#69470,#69471,#69472,#69473,#69474,
#69475,#69476,#69477,#69478,#69479,#69480,#69481,#69482,#69483,#69484,#69485,
#69486,#69487,#69488,#69489,#69490,#69491,#69492,#69493,#69494,#69495,#69496,
#69497,#69498,#69499,#69500,#69501,#69502,#69503,#69504,#69505,#69506,#69507,
#69508,#69509,#69510,#69511,#69512,#69513,#69514,#69515,#69516,#69517,#69518,
#69519,#69520,#69521,#69522,#69523,#69524,#69525,#69526,#69527,#69528,#69529,
#69530,#69531,#69532,#69533,#69534,#69535,#69536,#69537,#69538,#69539,#69540,
#69541,#69542,#69543,#69544,#69545,#69546,#69547,#69548,#69549,#69550,#69551,
#69552,#69553,#69554,#69555,#69556,#69557,#69558,#69559,#69560,#69561,#69562,
#69563,#69564,#69565,#69566),.UNSPECIFIED.,.F.,.F.,(4,2,2,2,2,2,2,2,2,2,
2,2,2,2,2,2,2,2,2,2,2,2,2,2,2,2,2,2,2,2,2,2,2,2,2,2,2,2,2,2,2,2,2,2,2,2,
2,2,2,2,2,2,2,2,2,2,2,2,2,2,2,2,2,2,2,2,2,2,2,2,2,2,2,2,2,2,2,2,2,2,2,2,
2,2,2,2,2,2,2,2,2,2,2,2,2,2,2,2,2,2,2,2,2,2,2,2,2,2,2,2,2,2,2,2,2,2,2,2,
2,2,2,2,2,2,2,2,2,2,2,2,2,2,2,2,2,2,2,2,2,2,2,2,2,2,2,2,2,2,2,2,2,2,2,2,
2,2,2,2,2,2,2,2,2,2,2,2,2,2,2,2,2,2,2,2,2,2,2,2,2,2,2,2,2,2,2,2,2,2,2,2,
2,2,2,2,2,2,2,2,2,2,2,2,2,2,2,2,2,2,2,2,2,2,2,2,2,2,2,2,2,2,2,2,2,2,2,2,
2,2,2,2,2,2,2,2,2,2,2,2,2,2,2,2,2,2,2,2,2,2,2,2,2,2,2,2,2,2,2,2,2,2,2,2,
4),(-4.05837967880851,-4.00114997962759,-3.99885786767353,-3.99762552912259,
-3.9968230236056,-3.99618974499812,-3.99559634508342,-3.99495669272019,
-3.99383912483112,-3.99064763807603,-3.93486593044823,-3.92562478079503,
-3.9177941050812,-3.90206842493183,-3.85787989888074,-3.83986311131241,
-3.83693028810942,-3.8354521413208,-3.83438575770854,-3.83325372643113,
-3.83133322295104,-3.82617954040288,-3.74423570466487,-3.72164401947659,
-3.69693646754935,-3.68295670012722,-3.67833511550716,-3.67527997458224,
-3.67447698972937,-3.67384354395003,-3.67325004887753,-3.67261057582201,
-3.67149401834921,-3.66831022658899,-3.61575703947775,-3.55873903585013,
-3.52326972702981,-3.51606349064379,-3.51393903226155,-3.51263593240743,
-3.51145425774148,-3.50993785711651,-3.50681545538903,-3.48685168599715,
-3.48128191897757,-3.47363585076932,-3.42895771502899,-3.37983569981381,
-3.36480205136965,-3.35757572516932,-3.35326806809867,-3.35206477311877,
-3.35132947919183,-3.35067091860498,-3.34982267463912,-3.34806308764843,
-3.33658332861734,-3.31098042527118,-3.26459306558094,-3.19598542264968,
-3.192557372488,-3.19096473634342,-3.18977203488181,-3.18865594071235,-3.18711853085315,
-3.18321379086585,-3.11886334614989,-3.05648873116259,-3.03436856739687,
-3.03074516316081,-3.02961509163815,-3.02889651243075,-3.0282332986454,
-3.02736628258029,-3.02546056866849,-3.01025878225391,-3.00680051026876,
-3.00378788423812,-2.93647193934366,-2.8766535399211,-2.87105717568062,
-2.86907633029981,-2.86780523232915,-2.86661341576706,-2.86505361211981,
-2.86161829918681,-2.83341231061393,-2.815004636839,-2.73990169365395,-2.71257500815404,
-2.70845844726987,-2.70727562505949,-2.70654498179522,-2.70588530443346,
-2.70504253310068,-2.70326460044982,-2.69137289692048,-2.6877317867718,
-2.68737613379298,-2.68429807624357,-2.63314262600088,-2.58250911237497,
-2.55674143124803,-2.54906285762393,-2.54690523274297,-2.54559464938686,
-2.54441452442639,-2.54291159956409,-2.53995754234237,-2.5226575879747,
-2.5191350607216,-2.42067527257305,-2.38752228907476,-2.38538930504742,
-2.38447133717972,-2.38380207756533,-2.38318169309282,-2.38232886095255,
-2.38062677085322,-2.3658801709741,-2.35939375785636,-2.35734266875868,
-2.31700919515784,-2.28179809527985,-2.2513664799281,-2.2280157565012,-2.22504431493079,
-2.22355802214818,-2.22249021865752,-2.22136080331619,-2.21945477307557,
-2.21439592966997,-2.13352045214246,-2.12430573290513,-2.09851889040651,
-2.06510833763195,-2.06297302656451,-2.06205461606913,-2.0613852467922,
-2.06076491858795,-2.05991239625014,-2.0577635704893,-2.03080139871175,
-1.98370736019489,-1.90830253150715,-1.90348917916552,-1.90162239558283,
-1.90050062103354,-1.89931056244168,-1.89773626739029,-1.89431584255193,
-1.83425328504353,-1.74563975339823,-1.74116314654907,-1.73988490510131,
-1.7391381705834,-1.73854703916434,-1.73774860741926,-1.73623329897262,
-1.72730188506405,-1.70825709689502,-1.66120989655085,-1.58549595068009,
-1.58084248980402,-1.57918589124235,-1.5780372497445,-1.57697523735169,
-1.57553385715438,-1.57277965170257,-1.55586440902599,-1.51804879986678,
-1.4232609877706,-1.41859394327791,-1.41731037572708,-1.41655490287901,
-1.41589901077637,-1.41508118940544,-1.41347358625866,-1.40219037402685,
-1.37269913975616,-1.27694991347926,-1.26020459675332,-1.25727909565672,
-1.25578199647074,-1.25460216174129,-1.25331414678017,-1.25122068988163,
-1.2487318234765,-1.24391272763347,-1.19810329257103,-1.10022234669614,
-1.09580824655952,-1.09453670633292,-1.09379136187305,-1.09319988876281,
-1.09239914529803,-1.09087343062266,-1.08171516639059,-1.06263818577135,
-1.0151427816789,-0.939786839406562,-0.935373431755597,-0.933753071190259,
-0.9326142666752,-0.931455592388888,-0.930062482405305,-0.928486024192247,
-0.925955481012324,-0.921025987709515,-0.873367884512564,-0.777824541968153,
-0.77316343434182,-0.771880296305007,-0.771124815659568,-0.770468750426268,
-0.769650499400428,-0.76804137382139,-0.756721636735015,-0.727063697712971,
-0.685810661766175,-0.616606839776575,-0.612535849646385,-0.610970079098724,
-0.609845919125714,-0.608713315289243,-0.607207532235838,-0.604115197254895,
-0.600107654068119,-0.590923698141503,-0.562977806945251,-0.514144239050153,
-0.453867872614956,-0.450316554562721,-0.449149216138912,-0.448499203394114,
-0.447907599998148,-0.447106427231515,-0.445579068966624,-0.436387808020264,
-0.41738512345892,-0.371366899622648,-0.348027623676495,-0.30869990580444,
-0.292253558609206,-0.289601929278322,-0.288032938038533,-0.28683879994682,
-0.285738265939946,-0.283951240467609,-0.279262048675758,-0.27254205137593,
-0.254080987998467,-0.235082400694175,-0.131592404963221,-0.127688789537731,
-0.126476362980388,-0.125817145815021,-0.125161086886395,-0.124345229269591,
-0.122748329517448,-0.111794078331155,-0.0838223294241255,-0.000958211236916205),
 .UNSPECIFIED.);
#885=B_SPLINE_CURVE_WITH_KNOTS('',3,(#69568,#69569,#69570,#69571,#69572,
#69573,#69574,#69575,#69576,#69577,#69578,#69579,#69580,#69581,#69582,#69583,
#69584,#69585,#69586,#69587,#69588,#69589,#69590,#69591,#69592,#69593,#69594,
#69595,#69596,#69597,#69598,#69599,#69600,#69601,#69602,#69603,#69604,#69605,
#69606,#69607,#69608,#69609,#69610,#69611,#69612,#69613,#69614,#69615,#69616,
#69617,#69618,#69619,#69620,#69621,#69622,#69623,#69624,#69625,#69626,#69627,
#69628,#69629,#69630,#69631,#69632,#69633,#69634,#69635,#69636,#69637,#69638,
#69639,#69640,#69641,#69642,#69643,#69644,#69645,#69646,#69647,#69648,#69649,
#69650,#69651,#69652,#69653,#69654,#69655,#69656,#69657,#69658,#69659,#69660,
#69661,#69662,#69663,#69664,#69665,#69666,#69667,#69668,#69669,#69670,#69671,
#69672,#69673,#69674,#69675,#69676,#69677,#69678,#69679,#69680,#69681,#69682,
#69683,#69684,#69685,#69686,#69687,#69688,#69689,#69690,#69691,#69692,#69693,
#69694,#69695,#69696,#69697,#69698,#69699,#69700,#69701,#69702,#69703,#69704,
#69705,#69706,#69707,#69708,#69709,#69710,#69711,#69712,#69713,#69714,#69715,
#69716,#69717,#69718,#69719,#69720,#69721,#69722,#69723,#69724,#69725,#69726,
#69727,#69728,#69729,#69730,#69731,#69732,#69733,#69734,#69735,#69736,#69737,
#69738,#69739,#69740,#69741,#69742,#69743,#69744,#69745,#69746,#69747,#69748,
#69749,#69750,#69751,#69752,#69753,#69754,#69755,#69756,#69757,#69758,#69759,
#69760,#69761,#69762,#69763,#69764,#69765,#69766,#69767,#69768,#69769,#69770,
#69771,#69772,#69773,#69774,#69775,#69776,#69777,#69778,#69779,#69780,#69781,
#69782,#69783,#69784,#69785,#69786,#69787,#69788,#69789,#69790,#69791,#69792,
#69793,#69794,#69795,#69796,#69797,#69798,#69799,#69800,#69801,#69802,#69803,
#69804,#69805,#69806,#69807,#69808,#69809,#69810,#69811,#69812,#69813,#69814,
#69815,#69816,#69817,#69818,#69819,#69820,#69821,#69822,#69823,#69824,#69825,
#69826,#69827,#69828,#69829,#69830,#69831,#69832,#69833,#69834,#69835,#69836,
#69837,#69838,#69839,#69840,#69841,#69842,#69843,#69844,#69845,#69846,#69847,
#69848,#69849,#69850,#69851,#69852,#69853,#69854,#69855,#69856,#69857,#69858,
#69859,#69860,#69861,#69862,#69863,#69864,#69865,#69866,#69867,#69868,#69869,
#69870,#69871,#69872,#69873,#69874,#69875,#69876,#69877,#69878,#69879,#69880,
#69881,#69882,#69883,#69884,#69885,#69886,#69887,#69888,#69889,#69890,#69891,
#69892,#69893,#69894,#69895,#69896,#69897,#69898,#69899,#69900,#69901,#69902,
#69903,#69904,#69905,#69906,#69907,#69908,#69909,#69910,#69911,#69912,#69913,
#69914,#69915,#69916,#69917,#69918,#69919,#69920,#69921,#69922,#69923,#69924,
#69925,#69926,#69927,#69928,#69929,#69930,#69931,#69932,#69933,#69934,#69935,
#69936,#69937,#69938,#69939,#69940,#69941,#69942,#69943,#69944,#69945,#69946,
#69947,#69948,#69949,#69950,#69951,#69952,#69953,#69954,#69955,#69956,#69957,
#69958,#69959,#69960,#69961,#69962,#69963,#69964,#69965,#69966,#69967,#69968,
#69969,#69970,#69971,#69972,#69973,#69974,#69975,#69976,#69977,#69978,#69979,
#69980,#69981,#69982,#69983,#69984,#69985,#69986,#69987,#69988,#69989,#69990,
#69991,#69992,#69993,#69994,#69995,#69996,#69997,#69998,#69999,#70000,#70001,
#70002,#70003,#70004,#70005,#70006,#70007,#70008,#70009,#70010,#70011,#70012,
#70013,#70014,#70015,#70016,#70017,#70018,#70019,#70020,#70021,#70022,#70023,
#70024,#70025,#70026,#70027,#70028,#70029,#70030,#70031,#70032,#70033,#70034,
#70035,#70036,#70037,#70038,#70039,#70040,#70041,#70042,#70043,#70044,#70045,
#70046,#70047,#70048,#70049,#70050,#70051,#70052,#70053,#70054,#70055,#70056,
#70057,#70058,#70059,#70060,#70061,#70062,#70063,#70064,#70065,#70066,#70067,
#70068,#70069,#70070,#70071,#70072,#70073,#70074,#70075,#70076,#70077,#70078,
#70079,#70080,#70081,#70082,#70083,#70084,#70085,#70086,#70087,#70088,#70089,
#70090,#70091,#70092,#70093,#70094,#70095),.UNSPECIFIED.,.F.,.F.,(4,2,2,
2,2,2,2,2,2,2,2,2,2,2,2,2,2,2,2,2,2,2,2,2,2,2,2,2,2,2,2,2,2,2,2,2,2,2,2,
2,2,2,2,2,2,2,2,2,2,2,2,2,2,2,2,2,2,2,2,2,2,2,2,2,2,2,2,2,2,2,2,2,2,2,2,
2,2,2,2,2,2,2,2,2,2,2,2,2,2,2,2,2,2,2,2,2,2,2,2,2,2,2,2,2,2,2,2,2,2,2,2,
2,2,2,2,2,2,2,2,2,2,2,2,2,2,2,2,2,2,2,2,2,2,2,2,2,2,2,2,2,2,2,2,2,2,2,2,
2,2,2,2,2,2,2,2,2,2,2,2,2,2,2,2,2,2,2,2,2,2,2,2,2,2,2,2,2,2,2,2,2,2,2,2,
2,2,2,2,2,2,2,2,2,2,2,2,2,2,2,2,2,2,2,2,2,2,2,2,2,2,2,2,2,2,2,2,2,2,2,2,
2,2,2,2,2,2,2,2,2,2,2,2,2,2,2,2,2,2,2,2,2,2,2,2,2,2,2,2,2,2,2,2,2,2,2,2,
2,2,2,2,2,2,2,2,4),(-4.06120156146985,-4.03210757396722,-4.02898962223826,
-4.02716923153719,-4.02589021951178,-4.02478870107512,-4.02360620612062,
-4.02208890672558,-4.01896520012184,-3.9990073799305,-3.99251745116898,
-3.98587636646403,-3.90492614531435,-3.87687630781146,-3.86590705178375,
-3.86430996816114,-3.86349421197578,-3.86283833298179,-3.86217937966733,
-3.86096766763953,-3.85706816786919,-3.75355810273542,-3.72233241612452,
-3.71193739985365,-3.70754385493776,-3.70421038782226,-3.70265777093699,
-3.70153674915908,-3.70042994104384,-3.69893038731804,-3.69600367842245,
-3.67305405653463,-3.61133036129914,-3.60472086317543,-3.59707456127475,
-3.54399453666206,-3.54187001850888,-3.54095330337529,-3.54028404202883,
-3.5396629762727,-3.53880820490921,-3.53709916588012,-3.5221526334199,-3.52113650057503,
-3.52009181161374,-3.51874348920431,-3.5143740386739,-3.42162329407878,
-3.39650004326749,-3.38805641206967,-3.38429131185362,-3.3813495959608,
-3.37987624134638,-3.3787336160924,-3.37759496928168,-3.37564322543333,
-3.37029052139437,-3.36298556912049,-3.25915209091068,-3.2245225180134,
-3.21979274183245,-3.21854680863072,-3.21780713268899,-3.21714883445646,
-3.21630656947934,-3.21463635321678,-3.20459111334289,-3.15999698161363,
-3.069175260887,-3.0633442102124,-3.06048136102256,-3.05876615550513,-3.05721650914028,
-3.05604599358132,-3.05493075006046,-3.05339845558342,-3.04952742355869,
-2.9935117479299,-2.93679635755297,-2.90188242769568,-2.89713209289675,
-2.89588434381003,-2.89514429430316,-2.89448612186026,-2.89364463297165,
-2.89192081389984,-2.88122545896731,-2.78889099056695,-2.74088725901194,
-2.73793223075628,-2.73617892301259,-2.73460039378158,-2.73342538628342,
-2.73231727455111,-2.73081241588302,-2.72710067123767,-2.68416031586473,
-2.61382134399594,-2.58599886270908,-2.57508077374812,-2.57348567875365,
-2.57267041044276,-2.57201465909501,-2.57135560923095,-2.5701430982173,
-2.56623614249461,-2.46297033493821,-2.4171649235412,-2.41351736121602,
-2.41190085425706,-2.41070371274285,-2.40959307686894,-2.40807808403072,
-2.40430561535023,-2.35739818734881,-2.32243777142454,-2.29081059076187,
-2.26425096416842,-2.26182673534768,-2.2523498306447,-2.25081056107775,
-2.25000704140691,-2.24935208326961,-2.24868635861321,-2.2474403980938,
-2.24325120571912,-2.16489884879582,-2.0943380880748,-2.09088060328921,
-2.08929921653918,-2.08810792401065,-2.08698801442365,-2.08543722359272,
-2.082307886553,-2.05277444455319,-2.03089391965558,-1.93366913198929,-1.92920708808078,
-1.92793030522512,-1.92718381571344,-1.92659253274293,-1.92579345413335,
-1.9242754851656,-1.91528957935169,-1.89617921795791,-1.84891360244464,
-1.80729748762842,-1.77201419985588,-1.76874558330729,-1.767160082276,-1.76603075518482,
-1.76496240284194,-1.76347433697782,-1.76049566222153,-1.73690710647679,
-1.71703078689443,-1.66717080638795,-1.60974807636699,-1.60644110870235,
-1.60530711256131,-1.6046638834551,-1.60407093025589,-1.60325665295594,
-1.60166633036362,-1.59088223098859,-1.56366616301844,-1.48148523758425,
-1.47555659102584,-1.46794113588852,-1.44863083767028,-1.44553747319105,
-1.44402633731195,-1.4428447385262,-1.44153761296112,-1.43939728664751,
-1.43189635997558,-1.38400122075942,-1.28871555710387,-1.28406442637754,
-1.28278235878451,-1.28202714487373,-1.28138499384764,-1.28058955198037,
-1.27972680600245,-1.27835135481755,-1.27568418191224,-1.2495287345976,
-1.20066870967902,-1.12778343313502,-1.12351067297052,-1.12191250764918,
-1.12077966932391,-1.11971245657581,-1.11823305138376,-1.11529734185162,
-1.09324603946533,-1.05861260428938,-0.966055005163889,-0.961370678346296,
-0.960085047261387,-0.959328940478198,-0.958687231744595,-0.957893015902392,
-0.95703193160292,-0.955660542804421,-0.953004339971197,-0.927037404740657,
-0.878358327099164,-0.805153349665185,-0.800815022830284,-0.799206257082382,
-0.798070443248395,-0.797004075573314,-0.795531578903331,-0.792630071959325,
-0.771706381770003,-0.740582406387014,-0.695463179798476,-0.68895080292122,
-0.640955160043092,-0.638241416235582,-0.637300594714132,-0.636656020582063,
-0.636011195459987,-0.63518996880752,-0.634291356655268,-0.632830073313045,
-0.629931780106595,-0.622570278351487,-0.59408512482129,-0.499234711943945,
-0.496242225825804,-0.480245119230678,-0.477616947653999,-0.476054907710212,
-0.474862021359495,-0.473590401293034,-0.471610015611962,-0.46553268557093,
-0.372314046198989,-0.331458232353176,-0.327697006359998,-0.316686748383605,
-0.314948012015827,-0.314103472062978,-0.313460612642792,-0.312742031671555,
-0.31198730133634,-0.310869802223092,-0.308871244738963,-0.304430255999315,
-0.291203734391308,-0.266470356942769,-0.166067276683062,-0.16396932658475,
-0.156270181840844,-0.154012157762357,-0.152678592687857,-0.151619138598524,
-0.150205529603611,-0.147583083518611,-0.13348898393143,-0.105349081958357,
-0.00100413960794193),.UNSPECIFIED.);
#886=B_SPLINE_CURVE_WITH_KNOTS('',3,(#70097,#70098,#70099,#70100,#70101,
#70102,#70103,#70104,#70105,#70106,#70107),.UNSPECIFIED.,.F.,.F.,(4,1,1,
1,1,1,1,1,4),(411.548637620263,411.580474769127,412.579267172895,413.578059576663,
414.576851980431,415.575644384199,416.574436787967,417.573229191735,417.831820549658),
 .UNSPECIFIED.);
#887=B_SPLINE_CURVE_WITH_KNOTS('',3,(#70109,#70110,#70111,#70112,#70113,
#70114,#70115,#70116,#70117,#70118,#70119,#70120,#70121,#70122,#70123,#70124,
#70125,#70126,#70127,#70128,#70129,#70130,#70131,#70132,#70133,#70134,#70135,
#70136,#70137,#70138,#70139,#70140,#70141,#70142,#70143,#70144,#70145,#70146,
#70147,#70148,#70149,#70150,#70151,#70152,#70153,#70154,#70155,#70156,#70157,
#70158,#70159,#70160,#70161,#70162,#70163,#70164,#70165,#70166,#70167,#70168,
#70169,#70170,#70171,#70172,#70173,#70174,#70175,#70176,#70177,#70178,#70179,
#70180,#70181,#70182,#70183,#70184,#70185,#70186,#70187,#70188,#70189,#70190,
#70191,#70192,#70193,#70194,#70195,#70196,#70197,#70198,#70199,#70200,#70201,
#70202,#70203,#70204,#70205,#70206,#70207,#70208,#70209,#70210,#70211,#70212,
#70213,#70214,#70215,#70216,#70217,#70218,#70219,#70220,#70221,#70222,#70223,
#70224,#70225,#70226,#70227,#70228,#70229,#70230,#70231,#70232,#70233,#70234,
#70235,#70236,#70237,#70238,#70239,#70240,#70241,#70242,#70243,#70244,#70245,
#70246,#70247,#70248,#70249,#70250,#70251,#70252,#70253,#70254,#70255,#70256,
#70257,#70258,#70259,#70260,#70261,#70262,#70263,#70264,#70265,#70266,#70267,
#70268,#70269,#70270,#70271,#70272,#70273,#70274,#70275,#70276,#70277,#70278,
#70279,#70280,#70281,#70282,#70283,#70284,#70285,#70286,#70287,#70288,#70289,
#70290,#70291,#70292,#70293,#70294,#70295,#70296,#70297,#70298,#70299,#70300,
#70301,#70302,#70303,#70304,#70305,#70306,#70307,#70308,#70309,#70310,#70311,
#70312,#70313,#70314,#70315,#70316,#70317,#70318,#70319,#70320,#70321,#70322,
#70323,#70324,#70325,#70326,#70327,#70328,#70329,#70330,#70331,#70332,#70333,
#70334,#70335,#70336,#70337,#70338,#70339,#70340,#70341,#70342,#70343,#70344,
#70345,#70346,#70347,#70348,#70349,#70350,#70351,#70352,#70353,#70354,#70355,
#70356,#70357,#70358,#70359,#70360,#70361,#70362,#70363,#70364,#70365,#70366,
#70367,#70368,#70369,#70370,#70371,#70372,#70373,#70374,#70375,#70376,#70377,
#70378,#70379,#70380,#70381,#70382,#70383,#70384,#70385,#70386,#70387,#70388,
#70389,#70390,#70391,#70392,#70393,#70394,#70395,#70396,#70397,#70398,#70399,
#70400,#70401,#70402,#70403,#70404,#70405,#70406,#70407,#70408,#70409,#70410,
#70411,#70412,#70413,#70414,#70415,#70416,#70417,#70418,#70419,#70420,#70421,
#70422,#70423,#70424,#70425,#70426,#70427,#70428,#70429,#70430,#70431,#70432,
#70433,#70434,#70435,#70436,#70437,#70438,#70439,#70440,#70441,#70442,#70443,
#70444,#70445,#70446,#70447,#70448,#70449,#70450,#70451,#70452,#70453,#70454,
#70455,#70456,#70457,#70458,#70459,#70460,#70461,#70462,#70463,#70464,#70465,
#70466,#70467,#70468,#70469,#70470,#70471,#70472,#70473,#70474,#70475,#70476,
#70477,#70478,#70479,#70480,#70481,#70482,#70483,#70484,#70485,#70486,#70487,
#70488,#70489,#70490,#70491,#70492,#70493,#70494,#70495,#70496,#70497,#70498,
#70499,#70500,#70501,#70502,#70503,#70504,#70505,#70506,#70507,#70508,#70509,
#70510,#70511,#70512,#70513,#70514,#70515,#70516,#70517,#70518,#70519,#70520,
#70521,#70522,#70523,#70524,#70525,#70526,#70527,#70528,#70529,#70530,#70531,
#70532,#70533,#70534,#70535,#70536,#70537,#70538,#70539,#70540,#70541,#70542,
#70543,#70544,#70545,#70546,#70547,#70548,#70549,#70550,#70551,#70552,#70553,
#70554,#70555,#70556,#70557,#70558,#70559,#70560,#70561,#70562,#70563,#70564,
#70565,#70566,#70567,#70568,#70569,#70570,#70571,#70572,#70573,#70574,#70575,
#70576,#70577,#70578,#70579,#70580,#70581,#70582,#70583,#70584,#70585,#70586,
#70587,#70588,#70589,#70590,#70591,#70592,#70593,#70594,#70595,#70596,#70597,
#70598,#70599,#70600,#70601,#70602,#70603,#70604,#70605,#70606,#70607,#70608,
#70609,#70610,#70611,#70612,#70613,#70614,#70615,#70616,#70617,#70618,#70619,
#70620,#70621,#70622,#70623,#70624,#70625,#70626,#70627,#70628,#70629,#70630,
#70631,#70632,#70633,#70634,#70635,#70636,#70637,#70638,#70639,#70640,#70641,
#70642,#70643,#70644,#70645,#70646,#70647,#70648,#70649,#70650,#70651,#70652,
#70653,#70654,#70655,#70656,#70657,#70658,#70659,#70660,#70661,#70662,#70663,
#70664,#70665,#70666),.UNSPECIFIED.,.F.,.F.,(4,2,2,2,2,2,2,2,2,2,2,2,2,
2,2,2,2,2,2,2,2,2,2,2,2,2,2,2,2,2,2,2,2,2,2,2,2,2,2,2,2,2,2,2,2,2,2,2,2,
2,2,2,2,2,2,2,2,2,2,2,2,2,2,2,2,2,2,2,2,2,2,2,2,2,2,2,2,2,2,2,2,2,2,2,2,
2,2,2,2,2,2,2,2,2,2,2,2,2,2,2,2,2,2,2,2,2,2,2,2,2,2,2,2,2,2,2,2,2,2,2,2,
2,2,2,2,2,2,2,2,2,2,2,2,2,2,2,2,2,2,2,2,2,2,2,2,2,2,2,2,2,2,2,2,2,2,2,2,
2,2,2,2,2,2,2,2,2,2,2,2,2,2,2,2,2,2,2,2,2,2,2,2,2,2,2,2,2,2,2,2,2,2,2,2,
2,2,2,2,2,2,2,2,2,2,2,2,2,2,2,2,2,2,2,2,2,2,2,2,2,2,2,2,2,2,2,2,2,2,2,2,
2,2,2,2,2,2,2,2,2,2,2,2,2,2,2,2,2,2,2,2,2,2,2,2,2,2,2,2,2,2,2,2,2,2,2,2,
2,2,2,2,2,2,2,2,2,2,2,2,2,4),(-4.06049910102836,-3.98885752482128,-3.98628571019544,
-3.98469195091486,-3.98320785462953,-3.98214011736032,-3.9810093730988,
-3.97941850301221,-3.97519186879429,-3.90584130610861,-3.89048237730222,
-3.87601308438949,-3.83994592728347,-3.82475055393006,-3.82328769351999,
-3.82205961830065,-3.82132402914361,-3.82066507049597,-3.81981613209028,
-3.8180544617547,-3.8065440587236,-3.80463201303284,-3.74452665069794,-3.71401735447342,
-3.68094396614464,-3.67031011533946,-3.66358104600662,-3.66204983183634,
-3.66088270039567,-3.65969114215245,-3.6585711253673,-3.65702041234628,
-3.6538919375063,-3.62440639169627,-3.60547728889943,-3.57970784813515,
-3.50454695758624,-3.50065847777196,-3.49979412513344,-3.49898646866834,
-3.4983942741377,-3.49774781264562,-3.49659774668816,-3.49317735950503,
-3.43577708954707,-3.39818249297175,-3.35941524947579,-3.34231305900054,
-3.33955954318896,-3.33838531284719,-3.33718995189852,-3.33607614731679,
-3.33454934771791,-3.330710524477,-3.27841791799949,-3.22220749706289,-3.20118990040303,
-3.18238133233035,-3.17819929710273,-3.17699573014311,-3.1762655865804,
-3.17560528023819,-3.17476027025618,-3.17297230734869,-3.16086617571934,
-3.15829614981815,-3.15289177171601,-3.12080639242039,-3.05789909109812,
-3.02435686494712,-3.01834472207156,-3.01637595085011,-3.01509808306824,
-3.01390780363821,-3.01236125089029,-3.00912157059228,-2.98541029678503,
-2.97593596687526,-2.96791131043136,-2.88978496784511,-2.85999150429394,
-2.85570655511072,-2.85446452580222,-2.8537257345788,-2.8530672878009,-2.85222357263386,
-2.85048869651388,-2.83956215441281,-2.83728759360666,-2.83410228178253,
-2.8162338862243,-2.7416067843407,-2.70249494515861,-2.69810030260833,-2.69476602185416,
-2.6932133266055,-2.69202126468134,-2.69090176758201,-2.68935334751774,
-2.68538686174789,-2.61778475726787,-2.57376432014592,-2.54489019247849,
-2.53374011603199,-2.53213685814006,-2.53131986292278,-2.53066394368582,
-2.53000576025179,-2.52879769656697,-2.52492737844062,-2.42262746359116,
-2.37581983736633,-2.37216122534024,-2.37054264092001,-2.36934507155384,
-2.36823482956124,-2.36672159202005,-2.36296140621004,-2.31688755773626,
-2.29268467759209,-2.24969069604329,-2.22378449648682,-2.21115359728144,
-2.20950378823812,-2.20867730418549,-2.20808283274479,-2.20744513494251,
-2.20652858199373,-2.20397682426801,-2.20275491099092,-2.14250844297962,
-2.09370324500228,-2.070439592343,-2.0520335572599,-2.04921974607596,-2.04776570837877,
-2.04670202316632,-2.04555890540741,-2.04358455769836,-2.03807977099596,
-2.03091957374525,-2.0088737925009,-1.96460962312695,-1.89201062909916,
-1.88790816209106,-1.88667220203356,-1.88600842877215,-1.88535319867153,
-1.88454617224062,-1.88299056578486,-1.87312112517939,-1.85068301791431,
-1.76329320216655,-1.75416049926012,-1.7490647448628,-1.72987149661922,
-1.72678373944993,-1.7252737530139,-1.72409232657149,-1.72278464840351,
-1.72064172793675,-1.7131149752923,-1.66493477361444,-1.56983484418296,
-1.56529755976216,-1.56401247269335,-1.56326406995635,-1.56267293719772,
-1.56187618556825,-1.56036948442738,-1.55163231260533,-1.53294639006951,
-1.45375183039616,-1.40828474145392,-1.40453208640381,-1.40302006536907,
-1.40191006474474,-1.40071213340248,-1.39909196526675,-1.3954251179766,
-1.34786659278294,-1.24663285367013,-1.24246159355445,-1.24121738462658,
-1.24055183401719,-1.23989655780716,-1.2391081559464,-1.23761938106537,
-1.23574417883147,-1.1908037710805,-1.1293734115829,-1.11151490207392,-1.10348120616627,
-1.09802719382188,-1.09603595836976,-1.09307498461364,-1.09110670233415,
-1.08308579972866,-1.08081876610682,-1.0794699487634,-1.0782942069575,-1.0768474390265,
-1.07406974893305,-1.05660942503629,-1.01633193898139,-0.940996949372963,
-0.937395956764601,-0.93454042075786,-0.933992201958512,-0.920808756031269,
-0.91899932210531,-0.918137208769172,-0.917474265716635,-0.916860245296265,
-0.915817349368871,-0.912876367626713,-0.908478066816871,-0.882596613499722,
-0.835420366930702,-0.800808312108693,-0.793162479332177,-0.787691040513085,
-0.781983520004337,-0.761880625849114,-0.758749679727123,-0.757230697762973,
-0.756047719895461,-0.754743901503228,-0.752619887647664,-0.745282053454694,
-0.69915887202195,-0.633861981779868,-0.621714483177402,-0.618939913866563,
-0.616040596135668,-0.598422963831734,-0.596439795397862,-0.595637331722109,
-0.594968453735436,-0.594353789719638,-0.593395318234527,-0.591036614993808,
-0.587699413217694,-0.578773695082703,-0.556463444922131,-0.525893291528445,
-0.457582848829746,-0.456197936212814,-0.438994727746949,-0.436043903744468,
-0.43454086463401,-0.433359789442815,-0.43204726287174,-0.429884398786693,
-0.422166357163926,-0.396306967814914,-0.354576703673571,-0.317909442154778,
-0.276434382547346,-0.274056119835759,-0.273165317344658,-0.272534510490315,
-0.271937099890703,-0.271296460826856,-0.270471889413739,-0.267408673664023,
-0.237730563324097,-0.217684110991243,-0.142968757481856,-0.136548772213743,
-0.11657231593272,-0.113447187371181,-0.111929381906384,-0.110746576003267,
-0.109442191602947,-0.107315555633617,-0.0999522814260519,-0.053557751782706,
-0.000958120265015606),.UNSPECIFIED.);
#888=B_SPLINE_CURVE_WITH_KNOTS('',3,(#70668,#70669,#70670,#70671,#70672,
#70673,#70674,#70675,#70676,#70677,#70678,#70679,#70680,#70681,#70682,#70683,
#70684,#70685,#70686,#70687,#70688,#70689,#70690,#70691,#70692,#70693,#70694,
#70695,#70696,#70697,#70698,#70699,#70700,#70701,#70702,#70703,#70704,#70705,
#70706,#70707,#70708,#70709,#70710,#70711,#70712,#70713,#70714,#70715,#70716,
#70717,#70718,#70719,#70720,#70721,#70722,#70723,#70724,#70725,#70726,#70727,
#70728,#70729,#70730,#70731,#70732,#70733,#70734,#70735,#70736,#70737,#70738,
#70739,#70740,#70741,#70742,#70743,#70744,#70745,#70746,#70747,#70748,#70749,
#70750,#70751,#70752,#70753,#70754,#70755,#70756,#70757,#70758,#70759,#70760,
#70761,#70762,#70763,#70764,#70765,#70766,#70767,#70768,#70769,#70770,#70771,
#70772,#70773,#70774,#70775,#70776,#70777,#70778,#70779,#70780,#70781,#70782,
#70783,#70784,#70785,#70786,#70787,#70788,#70789,#70790,#70791,#70792,#70793,
#70794,#70795,#70796,#70797,#70798,#70799,#70800,#70801,#70802,#70803,#70804,
#70805,#70806,#70807,#70808,#70809,#70810,#70811,#70812,#70813,#70814,#70815,
#70816,#70817,#70818,#70819,#70820,#70821,#70822,#70823,#70824,#70825,#70826,
#70827,#70828,#70829,#70830,#70831,#70832,#70833,#70834,#70835,#70836,#70837,
#70838,#70839,#70840,#70841,#70842,#70843,#70844,#70845,#70846,#70847,#70848,
#70849,#70850,#70851,#70852,#70853,#70854,#70855,#70856,#70857,#70858,#70859,
#70860,#70861,#70862,#70863,#70864,#70865,#70866,#70867,#70868,#70869,#70870,
#70871,#70872,#70873,#70874,#70875,#70876,#70877,#70878,#70879,#70880,#70881,
#70882,#70883,#70884,#70885,#70886,#70887,#70888,#70889,#70890,#70891,#70892,
#70893,#70894,#70895,#70896,#70897,#70898,#70899,#70900,#70901,#70902,#70903,
#70904,#70905,#70906,#70907,#70908,#70909,#70910,#70911,#70912,#70913,#70914,
#70915,#70916,#70917,#70918,#70919,#70920,#70921,#70922,#70923,#70924,#70925,
#70926,#70927,#70928,#70929,#70930,#70931,#70932,#70933,#70934,#70935,#70936,
#70937,#70938,#70939,#70940,#70941,#70942,#70943,#70944,#70945,#70946,#70947,
#70948,#70949,#70950,#70951,#70952,#70953,#70954,#70955,#70956,#70957,#70958,
#70959,#70960,#70961,#70962,#70963,#70964,#70965,#70966,#70967,#70968,#70969,
#70970,#70971,#70972,#70973,#70974,#70975,#70976,#70977,#70978,#70979,#70980,
#70981,#70982,#70983,#70984,#70985,#70986,#70987,#70988,#70989,#70990,#70991,
#70992,#70993,#70994,#70995,#70996,#70997,#70998,#70999,#71000,#71001,#71002,
#71003,#71004,#71005,#71006,#71007,#71008,#71009,#71010,#71011,#71012,#71013,
#71014,#71015,#71016,#71017,#71018,#71019,#71020,#71021,#71022,#71023,#71024,
#71025,#71026,#71027,#71028,#71029,#71030,#71031,#71032,#71033,#71034,#71035,
#71036,#71037,#71038,#71039,#71040,#71041,#71042,#71043,#71044,#71045,#71046,
#71047,#71048,#71049,#71050,#71051,#71052,#71053,#71054,#71055,#71056,#71057,
#71058,#71059,#71060,#71061,#71062,#71063,#71064,#71065,#71066,#71067,#71068,
#71069,#71070,#71071,#71072,#71073,#71074,#71075,#71076,#71077,#71078,#71079,
#71080,#71081,#71082,#71083,#71084,#71085,#71086,#71087,#71088,#71089,#71090,
#71091,#71092,#71093,#71094,#71095,#71096,#71097,#71098,#71099,#71100,#71101,
#71102,#71103,#71104,#71105,#71106,#71107,#71108,#71109,#71110,#71111,#71112,
#71113,#71114,#71115,#71116,#71117,#71118,#71119,#71120,#71121,#71122,#71123,
#71124,#71125,#71126,#71127,#71128,#71129,#71130,#71131,#71132,#71133,#71134,
#71135,#71136,#71137,#71138,#71139,#71140,#71141,#71142,#71143,#71144,#71145,
#71146,#71147,#71148,#71149,#71150,#71151,#71152,#71153,#71154,#71155,#71156,
#71157,#71158,#71159,#71160,#71161,#71162,#71163,#71164,#71165,#71166,#71167,
#71168,#71169,#71170,#71171,#71172,#71173,#71174,#71175,#71176,#71177,#71178,
#71179,#71180,#71181,#71182,#71183,#71184,#71185,#71186,#71187,#71188,#71189,
#71190,#71191,#71192,#71193,#71194,#71195,#71196,#71197,#71198,#71199,#71200,
#71201),.UNSPECIFIED.,.F.,.F.,(4,2,2,2,2,2,2,2,2,2,2,2,2,2,2,2,2,2,2,2,
2,2,2,2,2,2,2,2,2,2,2,2,2,2,2,2,2,2,2,2,2,2,2,2,2,2,2,2,2,2,2,2,2,2,2,2,
2,2,2,2,2,2,2,2,2,2,2,2,2,2,2,2,2,2,2,2,2,2,2,2,2,2,2,2,2,2,2,2,2,2,2,2,
2,2,2,2,2,2,2,2,2,2,2,2,2,2,2,2,2,2,2,2,2,2,2,2,2,2,2,2,2,2,2,2,2,2,2,2,
2,2,2,2,2,2,2,2,2,2,2,2,2,2,2,2,2,2,2,2,2,2,2,2,2,2,2,2,2,2,2,2,2,2,2,2,
2,2,2,2,2,2,2,2,2,2,2,2,2,2,2,2,2,2,2,2,2,2,2,2,2,2,2,2,2,2,2,2,2,2,2,2,
2,2,2,2,2,2,2,2,2,2,2,2,2,2,2,2,2,2,2,2,2,2,2,2,2,2,2,2,2,2,2,2,2,2,2,2,
2,2,2,2,2,2,2,2,2,2,2,2,2,2,2,2,2,2,2,2,2,2,2,2,2,2,2,2,2,2,4),(-4.05995377572391,
-4.01400246747446,-4.01177154444041,-4.01056281431475,-4.00977009445503,
-4.00913956836879,-4.00854729014005,-4.00790213991193,-4.00695856989801,
-4.00422396151782,-3.95855758109048,-3.94974625837205,-3.94211776551452,
-3.92741103186041,-3.89376938653784,-3.85747901825741,-3.85113851675836,
-3.84912662567192,-3.84784832654309,-3.84665866287938,-3.84511435293067,
-3.84254534276043,-3.82763516026328,-3.82190593181161,-3.82005063205414,
-3.74452293753362,-3.71125939823236,-3.69624643017317,-3.69137826647667,
-3.68819647998594,-3.68738314770942,-3.68674632972713,-3.68615106200478,
-3.68551601504203,-3.68460889888909,-3.68211844133079,-3.6400014950322,
-3.58836716214006,-3.58068159176122,-3.55199496804809,-3.5303112652294,
-3.52738719040587,-3.525910422878,-3.52484382715423,-3.5237104454478,-3.52178488726442,
-3.516601769143,-3.43425896573359,-3.39147744723565,-3.3770460237176,-3.37010233023217,
-3.36732603006827,-3.36528527798725,-3.36438559122186,-3.36371616443874,
-3.36309561792888,-3.36224255261446,-3.36053996521379,-3.34578761395255,
-3.34084897727765,-3.33872045605109,-3.3267222450338,-3.26009308420307,
-3.20873038533377,-3.20517671471311,-3.20357739193803,-3.20238314927038,
-3.20126812007694,-3.19973610230576,-3.19586567633618,-3.13986222297861,
-3.09135204547227,-3.04584090507054,-3.04306545438893,-3.04204617534767,
-3.04143280730987,-3.04076736907386,-3.03988817812,-3.03791766483837,-3.02071296851616,
-3.01929473866048,-2.93599591256572,-2.89100460269533,-2.88623486374829,
-2.8826462213513,-2.88104051895364,-2.87984526450297,-2.87873199072358,
-2.8772065900912,-2.87337477368271,-2.82161048964312,-2.75110192876342,
-2.72483912826716,-2.72216619863406,-2.72018481375698,-2.71929714934193,
-2.7186298596449,-2.71800618246504,-2.71714118322686,-2.71491985330561,
-2.68320058823522,-2.60427179187408,-2.5762213926229,-2.56216410406148,
-2.55954413243011,-2.55813129763701,-2.55696883133844,-2.55559783189003,
-2.55323396547082,-2.54426183583299,-2.54057346086215,-2.53861963074762,
-2.44801699085874,-2.4235795518854,-2.40172973975032,-2.39811519434472,
-2.39698470232759,-2.39627097185911,-2.39560546454292,-2.39472598014229,
-2.39275396679636,-2.37549944454451,-2.37324268897085,-2.36955568888835,
-2.35729532833842,-2.31903765467566,-2.27905061989296,-2.24459663141503,
-2.2384555718358,-2.23646758360399,-2.23519444708779,-2.23400252002539,
-2.23244515985288,-2.22902572873452,-2.20136674129527,-2.1098761421412,
-2.080063628466,-2.07571501422694,-2.07450537978201,-2.07377386619003,-2.07311388027818,
-2.07227134675223,-2.07049624015617,-2.0586869921538,-2.03151183110093,
-1.93768582828269,-1.91773894619717,-1.9146160265192,-1.91309900710585,
-1.91191668402246,-1.9106127003078,-1.9084864209234,-1.90112151627912,-1.85469715316082,
-1.75754713182159,-1.75308027059876,-1.75180281420884,-1.75105608935098,
-1.75046471014248,-1.74966561687974,-1.7481479941862,-1.73917429703633,
-1.72007457800104,-1.6728486127334,-1.59747311081948,-1.59273564553788,
-1.59088074985169,-1.58976090372091,-1.58856896044566,-1.58698548805259,
-1.58351856837576,-1.50913360032373,-1.43456899114881,-1.43032760249357,
-1.42907534677448,-1.42840819590629,-1.42775934481914,-1.42696027801401,
-1.4254429456969,-1.4164774746771,-1.39738627488976,-1.35019021136672,-1.27439697017666,
-1.26991985430255,-1.26828950197514,-1.26714781367578,-1.26598873624409,
-1.26451305503826,-1.26290364082852,-1.26029476076451,-1.25515611370009,
-1.20380233072963,-1.11878046657677,-1.10839277852334,-1.10668407267769,
-1.10584548448627,-1.1051874858975,-1.10444537597366,-1.10318892273092,
-1.09834419291398,-1.0621105099933,-0.967320426640924,-0.966246121807509,
-0.949271459751717,-0.946333226743836,-0.944833057224183,-0.943677226015442,
-0.94239752142191,-0.941061394927552,-0.939102687463249,-0.935644433181199,
-0.928115537650841,-0.905649194183061,-0.861229863714368,-0.836503950591983,
-0.787270204849993,-0.784517322255822,-0.783570859245963,-0.7829247223026,
-0.782332326887393,-0.781523655669347,-0.779960644602817,-0.769910391568304,
-0.746247913068194,-0.698323535060005,-0.628453073134337,-0.624373580611973,
-0.622806405755344,-0.621681864659135,-0.620516052873785,-0.619004516850361,
-0.617335132726419,-0.6145826687902,-0.60905502830531,-0.59488530601837,
-0.562267698950175,-0.466966483521416,-0.46229035383612,-0.461005510610261,
-0.460249551268411,-0.459593405381632,-0.458775484052763,-0.457168370057543,
-0.445914597657873,-0.412535385543892,-0.373207296041935,-0.308192821483237,
-0.30682643585624,-0.301953614440325,-0.300076428659167,-0.29895210150243,
-0.297819315679176,-0.296313071123386,-0.293217396221707,-0.28920593574069,
-0.280010478350127,-0.253529604370361,-0.150423073130263,-0.140168445430379,
-0.138466201320709,-0.137628779896677,-0.136970753884912,-0.136227595512537,
-0.134966993683787,-0.130078008043466,-0.106848936157074,-0.000958066444032279),
 .UNSPECIFIED.);
#889=B_SPLINE_CURVE_WITH_KNOTS('',3,(#71202,#71203,#71204,#71205,#71206,
#71207,#71208,#71209,#71210,#71211,#71212,#71213,#71214,#71215,#71216,#71217,
#71218,#71219,#71220,#71221,#71222,#71223,#71224,#71225,#71226,#71227,#71228,
#71229,#71230,#71231,#71232,#71233,#71234,#71235,#71236,#71237,#71238,#71239,
#71240,#71241,#71242,#71243,#71244,#71245,#71246,#71247,#71248,#71249,#71250,
#71251,#71252,#71253,#71254,#71255,#71256,#71257,#71258,#71259,#71260,#71261,
#71262,#71263,#71264,#71265,#71266,#71267,#71268,#71269,#71270,#71271,#71272,
#71273,#71274,#71275,#71276,#71277,#71278,#71279,#71280,#71281,#71282,#71283,
#71284,#71285,#71286,#71287,#71288,#71289,#71290,#71291,#71292,#71293,#71294,
#71295,#71296,#71297,#71298,#71299,#71300,#71301,#71302,#71303,#71304,#71305,
#71306,#71307,#71308,#71309,#71310,#71311,#71312,#71313,#71314,#71315,#71316,
#71317,#71318,#71319,#71320,#71321,#71322,#71323,#71324,#71325,#71326,#71327,
#71328,#71329,#71330,#71331,#71332,#71333,#71334,#71335,#71336,#71337,#71338,
#71339,#71340,#71341,#71342,#71343,#71344,#71345,#71346,#71347,#71348,#71349,
#71350,#71351,#71352,#71353,#71354,#71355,#71356,#71357,#71358,#71359,#71360,
#71361,#71362,#71363,#71364,#71365,#71366,#71367,#71368,#71369,#71370,#71371,
#71372,#71373,#71374,#71375,#71376,#71377,#71378,#71379,#71380,#71381,#71382,
#71383,#71384,#71385,#71386,#71387,#71388,#71389,#71390,#71391,#71392,#71393,
#71394,#71395,#71396,#71397,#71398,#71399,#71400,#71401,#71402,#71403,#71404,
#71405,#71406,#71407,#71408,#71409,#71410,#71411,#71412,#71413,#71414,#71415,
#71416,#71417,#71418,#71419,#71420,#71421,#71422,#71423,#71424,#71425,#71426,
#71427,#71428,#71429,#71430,#71431,#71432,#71433,#71434,#71435,#71436,#71437,
#71438,#71439,#71440,#71441,#71442,#71443,#71444,#71445,#71446,#71447,#71448,
#71449,#71450,#71451,#71452,#71453,#71454,#71455,#71456,#71457,#71458,#71459,
#71460,#71461,#71462,#71463,#71464,#71465,#71466,#71467,#71468,#71469,#71470,
#71471,#71472,#71473,#71474,#71475,#71476,#71477,#71478,#71479,#71480,#71481,
#71482,#71483,#71484,#71485,#71486,#71487,#71488,#71489,#71490,#71491,#71492,
#71493,#71494,#71495,#71496,#71497,#71498,#71499,#71500,#71501,#71502,#71503,
#71504,#71505,#71506,#71507,#71508,#71509,#71510,#71511,#71512,#71513,#71514,
#71515,#71516,#71517,#71518,#71519,#71520,#71521,#71522,#71523,#71524,#71525,
#71526,#71527,#71528,#71529,#71530,#71531,#71532,#71533,#71534,#71535,#71536,
#71537,#71538,#71539,#71540,#71541,#71542,#71543,#71544,#71545,#71546,#71547,
#71548,#71549,#71550,#71551,#71552,#71553,#71554,#71555,#71556,#71557,#71558,
#71559,#71560,#71561,#71562,#71563,#71564,#71565,#71566,#71567,#71568,#71569,
#71570,#71571,#71572,#71573,#71574,#71575,#71576,#71577,#71578,#71579,#71580,
#71581,#71582,#71583,#71584,#71585,#71586,#71587,#71588,#71589,#71590,#71591,
#71592,#71593,#71594,#71595,#71596,#71597,#71598,#71599,#71600,#71601,#71602,
#71603,#71604,#71605,#71606,#71607,#71608,#71609,#71610,#71611,#71612,#71613,
#71614,#71615,#71616,#71617,#71618,#71619,#71620,#71621,#71622,#71623,#71624,
#71625,#71626,#71627,#71628,#71629,#71630,#71631,#71632,#71633,#71634,#71635,
#71636,#71637,#71638,#71639,#71640,#71641,#71642,#71643,#71644,#71645,#71646,
#71647,#71648,#71649,#71650,#71651,#71652,#71653,#71654,#71655,#71656,#71657,
#71658,#71659,#71660,#71661,#71662,#71663,#71664,#71665,#71666,#71667,#71668,
#71669,#71670,#71671,#71672,#71673,#71674,#71675,#71676,#71677,#71678,#71679,
#71680,#71681,#71682,#71683,#71684,#71685,#71686,#71687,#71688,#71689,#71690,
#71691,#71692,#71693,#71694,#71695,#71696,#71697,#71698,#71699,#71700,#71701,
#71702,#71703,#71704,#71705,#71706,#71707,#71708,#71709,#71710,#71711,#71712,
#71713,#71714,#71715,#71716,#71717,#71718,#71719,#71720,#71721,#71722,#71723,
#71724,#71725,#71726,#71727,#71728,#71729,#71730,#71731,#71732,#71733,#71734,
#71735,#71736,#71737,#71738,#71739,#71740,#71741,#71742,#71743,#71744,#71745,
#71746,#71747,#71748,#71749,#71750,#71751,#71752,#71753),.UNSPECIFIED.,
 .F.,.F.,(4,2,2,2,2,2,2,2,2,2,2,2,2,2,2,2,2,2,2,2,2,2,2,2,2,2,2,2,2,2,2,
2,2,2,2,2,2,2,2,2,2,2,2,2,2,2,2,2,2,2,2,2,2,2,2,2,2,2,2,2,2,2,2,2,2,2,2,
2,2,2,2,2,2,2,2,2,2,2,2,2,2,2,2,2,2,2,2,2,2,2,2,2,2,2,2,2,2,2,2,2,2,2,2,
2,2,2,2,2,2,2,2,2,2,2,2,2,2,2,2,2,2,2,2,2,2,2,2,2,2,2,2,2,2,2,2,2,2,2,2,
2,2,2,2,2,2,2,2,2,2,2,2,2,2,2,2,2,2,2,2,2,2,2,2,2,2,2,2,2,2,2,2,2,2,2,2,
2,2,2,2,2,2,2,2,2,2,2,2,2,2,2,2,2,2,2,2,2,2,2,2,2,2,2,2,2,2,2,2,2,2,2,2,
2,2,2,2,2,2,2,2,2,2,2,2,2,2,2,2,2,2,2,2,2,2,2,2,2,2,2,2,2,2,2,2,2,2,2,2,
2,2,2,2,2,2,2,2,2,2,2,2,2,2,2,2,2,2,2,2,2,2,2,2,2,2,2,2,4),(-4.06264891370286,
-4.04466481678739,-4.04171944035511,-4.03996985759614,-4.03871927843569,
-4.03761859860726,-4.03642671242435,-4.03487264716332,-4.03227246129462,
-4.01681467878756,-4.01014125613746,-3.90573478602837,-3.8871846779329,
-3.87850842302826,-3.87700395232275,-3.87620740433803,-3.87561599675183,
-3.87496292345712,-3.87378138823818,-3.87012395580404,-3.80980203232441,
-3.76104296925034,-3.73316357016784,-3.72399629271692,-3.71999348829215,
-3.71690092715767,-3.71539616443503,-3.71426245673253,-3.7131369394838,
-3.71156744014438,-3.70747653186516,-3.64881087907444,-3.62401254388835,
-3.61656188127699,-3.60789424833173,-3.59740056822543,-3.56736416612173,
-3.55596378725396,-3.55435136909462,-3.55353220732303,-3.55288180596164,
-3.5521285504499,-3.55085586509878,-3.54629764461666,-3.45204318794294,
-3.41364352788284,-3.40242957146284,-3.39778104250459,-3.39535627288935,
-3.3938239864202,-3.39240498643094,-3.39125143545477,-3.38991201369727,
-3.38762951064948,-3.37971709624268,-3.37747988972333,-3.3746353645517,
-3.37263237261971,-3.36720801473551,-3.28252509320965,-3.27084231774962,
-3.23709310366739,-3.23401418446853,-3.23178044683541,-3.23084446535944,
-3.23017142411008,-3.22955435515529,-3.22871594608443,-3.22707224142077,
-3.21408280073917,-3.21258201094603,-3.13144330822818,-3.08047434810702,
-3.07535528653699,-3.07275338730131,-3.07114668987156,-3.06967411033925,
-3.06851480809128,-3.06737197226251,-3.06573842047608,-3.06124276196288,
-2.98549381977511,-2.93819581239956,-2.9190780865949,-2.91009694569104,
-2.9085784733559,-2.90777898152405,-2.90718732933246,-2.90644028681986,
-2.90516235469261,-2.90069445661373,-2.80352244961704,-2.77972659583146,
-2.75427434874244,-2.75085308393796,-2.74890909770608,-2.74757892818489,
-2.74630379729038,-2.7451475854759,-2.74363936600893,-2.740664919527,-2.72301519728503,
-2.71692084504026,-2.70649715419583,-2.68570361411242,-2.62591533664153,
-2.59152072844372,-2.58680738603405,-2.58556264122349,-2.58482305240464,
-2.58416442844553,-2.58332120437218,-2.58158982747912,-2.57075243747133,
-2.47770335757685,-2.43401398621811,-2.42932359070342,-2.42578259617335,
-2.42418506236398,-2.42299056965065,-2.42187415897067,-2.42033844524547,
-2.41644924676154,-2.35792623016082,-2.32567410053728,-2.29273912264715,
-2.27373897086213,-2.26453994747926,-2.26301199780479,-2.26221059521409,
-2.2616188576344,-2.26087347288027,-2.25960256010805,-2.25519688990326,
-2.1572357926411,-2.10651633922664,-2.10298966090939,-2.10139490091177,
-2.10020098467784,-2.09908402647144,-2.09754585470916,-2.09364144259511,
-2.03143342376781,-1.94568588945432,-1.94121698804714,-1.93993908572206,
-1.93919213110808,-1.93860058744174,-1.93780129439016,-1.93628336519513,
-1.92730983372192,-1.9082076668517,-1.86097829719755,-1.81750874641717,
-1.80678277047357,-1.80099151151946,-1.80001860086326,-1.78295564961322,
-1.78001214956565,-1.77851062024225,-1.77732964203715,-1.77601609720063,
-1.77384896224531,-1.76608904582066,-1.71528954659117,-1.63723895592994,
-1.61967407370476,-1.61769219268508,-1.61688987243586,-1.61622096245566,
-1.61552635018331,-1.61448420297336,-1.61156312607422,-1.56827757619857,
-1.46434374419021,-1.46271710076099,-1.45798394544778,-1.45612947616272,
-1.45500951206666,-1.45381715969488,-1.45223266033903,-1.44876155980102,
-1.37235721928435,-1.29937739262119,-1.2954602912155,-1.29424619105613,
-1.29358662310028,-1.29294348821077,-1.29215074485718,-1.29129178900118,
-1.28992563280379,-1.24556146210342,-1.14140955031371,-1.14001302734392,
-1.13510811926426,-1.1332257918778,-1.13210048334515,-1.13091099351039,
-1.12934470803984,-1.12596994972009,-1.07434393310633,-1.00208523049849,
-0.974195601435886,-0.972029966830966,-0.971174235177764,-0.970552785005667,
-0.969896912539696,-0.969023552505082,-0.968038602582755,-0.961778676708886,
-0.949855964905436,-0.930587346958811,-0.842672860523167,-0.815039886352264,
-0.811620300002119,-0.81006256115565,-0.808870216021372,-0.807596508539697,
-0.805607371545677,-0.799460772993834,-0.764958629994796,-0.749888589531647,
-0.738227608248846,-0.654482738438058,-0.649959783302609,-0.648676001491574,
-0.647927745510757,-0.647283587130959,-0.646477620639891,-0.6456002326701,
-0.644189950782242,-0.606020150324919,-0.560186106112749,-0.518588038663505,
-0.511559193756308,-0.491891115511732,-0.488779975478132,-0.487264866943717,
-0.48608230319546,-0.48477629321908,-0.482642734719899,-0.475213988144116,
-0.428120201063305,-0.416854710770204,-0.407719220631319,-0.399998861959737,
-0.393305527808217,-0.371011617528432,-0.352438741898368,-0.328724171930144,
-0.326635097231675,-0.325792516975249,-0.325174475984557,-0.324516105602696,
-0.323613095556591,-0.322600375285419,-0.315647102101332,-0.301857080080799,
-0.275421913256252,-0.186220713459997,-0.169003008704053,-0.166051551319051,
-0.164548433991943,-0.163367416991245,-0.162055078578265,-0.159892808409297,
-0.152179789379607,-0.126330690551008,-0.097875296897731,-0.0372463253441361,
-0.00709930852854725,-0.00423362856377661,-0.00316447147116906,-0.00253401405903737,
-0.00190190014399343,-0.00125763970154655),.UNSPECIFIED.);
#890=B_SPLINE_CURVE_WITH_KNOTS('',3,(#71792,#71793,#71794,#71795,#71796,
#71797,#71798,#71799,#71800,#71801,#71802,#71803,#71804,#71805,#71806,#71807,
#71808,#71809,#71810,#71811,#71812,#71813,#71814,#71815,#71816,#71817,#71818,
#71819,#71820,#71821,#71822,#71823,#71824,#71825,#71826,#71827,#71828,#71829,
#71830,#71831,#71832,#71833,#71834,#71835,#71836,#71837,#71838,#71839,#71840,
#71841,#71842,#71843,#71844,#71845,#71846,#71847,#71848,#71849,#71850,#71851,
#71852),.UNSPECIFIED.,.F.,.F.,(4,3,3,3,3,3,3,3,3,3,3,3,3,3,3,3,3,3,3,3,
4),(-0.733313182989362,-0.716294493786964,-0.670821266456911,-0.640789190757952,
-0.62133617984982,-0.569925089098463,-0.543537875173823,-0.523380244131678,
-0.461289689980783,-0.415691816844391,-0.398550463653533,-0.341537216799208,
-0.279356146584203,-0.262754828049987,-0.241371242852862,-0.181974595834089,
-0.136653796141601,-0.117467040668732,-0.0607494647494775,-0.00403188883022294,
0.),.UNSPECIFIED.);
#891=B_SPLINE_CURVE_WITH_KNOTS('',3,(#71854,#71855,#71856,#71857),
 .UNSPECIFIED.,.F.,.F.,(4,4),(0.,0.0148351583007577),.UNSPECIFIED.);
#892=B_SPLINE_CURVE_WITH_KNOTS('',3,(#71858,#71859,#71860,#71861,#71862,
#71863,#71864,#71865,#71866,#71867,#71868,#71869,#71870,#71871,#71872,#71873,
#71874,#71875,#71876,#71877,#71878,#71879,#71880,#71881,#71882,#71883,#71884,
#71885,#71886,#71887,#71888,#71889,#71890,#71891,#71892,#71893,#71894,#71895,
#71896,#71897,#71898,#71899,#71900,#71901,#71902,#71903,#71904,#71905,#71906,
#71907,#71908,#71909,#71910,#71911,#71912,#71913,#71914,#71915,#71916,#71917,
#71918),.UNSPECIFIED.,.F.,.F.,(4,3,3,3,3,3,3,3,3,3,3,3,3,3,3,3,3,3,3,3,
4),(-0.744397949170595,-0.723616735492759,-0.67829295687754,-0.65916345595812,
-0.604538037765455,-0.577309499118107,-0.555880865424909,-0.495420190252057,
-0.44066178318746,-0.425583850132311,-0.378804123990258,-0.331770874270554,
-0.304228573210021,-0.284737624550849,-0.222500848162153,-0.158731754394471,
-0.15102870873837,-0.135594328587619,-0.0696436621400311,-0.00369299569244323,
0.),.UNSPECIFIED.);
#893=B_SPLINE_CURVE_WITH_KNOTS('',3,(#73751,#73752,#73753,#73754,#73755,
#73756,#73757,#73758,#73759,#73760,#73761,#73762,#73763,#73764,#73765,#73766,
#73767,#73768,#73769,#73770,#73771,#73772,#73773,#73774,#73775,#73776,#73777,
#73778,#73779,#73780,#73781,#73782,#73783,#73784,#73785,#73786,#73787,#73788,
#73789,#73790,#73791,#73792,#73793,#73794,#73795,#73796,#73797,#73798,#73799,
#73800,#73801,#73802,#73803,#73804,#73805,#73806,#73807,#73808,#73809,#73810,
#73811,#73812,#73813,#73814),.UNSPECIFIED.,.F.,.F.,(4,3,3,3,3,3,3,3,3,3,
3,3,3,3,3,3,3,3,3,3,3,4),(-0.744397949170525,-0.723616735492616,-0.667849821071476,
-0.659163469387309,-0.641214414426581,-0.591076386810976,-0.569755772081005,
-0.54382354565886,-0.483363318569143,-0.440662303964159,-0.421846140318383,
-0.37880412399009,-0.325805172793596,-0.300222673925967,-0.279280379085805,
-0.216042753422732,-0.166808319204116,-0.15102867511565,-0.104251465971131,
-0.0393806484926011,-0.00369301913285791,0.),.UNSPECIFIED.);
#894=B_SPLINE_CURVE_WITH_KNOTS('',3,(#73816,#73817,#73818,#73819,#73820,
#73821,#73822,#73823,#73824,#73825,#73826,#73827,#73828,#73829,#73830,#73831,
#73832,#73833,#73834,#73835,#73836,#73837,#73838,#73839,#73840,#73841,#73842,
#73843,#73844,#73845,#73846,#73847,#73848,#73849,#73850,#73851,#73852,#73853,
#73854,#73855,#73856,#73857,#73858,#73859,#73860,#73861,#73862,#73863,#73864,
#73865,#73866,#73867,#73868,#73869,#73870,#73871,#73872,#73873,#73874,#73875,
#73876,#73877,#73878,#73879,#73880,#73881,#73882),.UNSPECIFIED.,.F.,.F.,
(4,3,3,3,3,3,3,3,3,3,3,3,3,3,3,3,3,3,3,3,3,3,4),(-0.733313036857812,-0.71629449378717,
-0.650953385595915,-0.640774184990949,-0.621184304739324,-0.570131565600329,
-0.547731071725486,-0.528561181480364,-0.466083910280972,-0.429328908955862,
-0.40653620544786,-0.387326345085585,-0.341537216799262,-0.27727496749461,
-0.259045768830733,-0.236144865812168,-0.178116580240476,-0.147890161229715,
-0.127897896546065,-0.109092903344164,-0.0531230889165709,-0.00403172352540138,
-8.60864227220048E-14),.UNSPECIFIED.);
#895=B_SPLINE_CURVE_WITH_KNOTS('',3,(#75815,#75816,#75817,#75818,#75819,
#75820,#75821,#75822,#75823,#75824,#75825,#75826),.UNSPECIFIED.,.F.,.F.,
(4,2,2,2,2,4),(-1.91155738203844,-1.85120908901733,-1.79086079599622,-1.670164209954,
-1.55191612324141,-1.43366803652883),.UNSPECIFIED.);
#896=B_SPLINE_CURVE_WITH_KNOTS('',3,(#75828,#75829,#75830,#75831,#75832,
#75833,#75834,#75835,#75836,#75837,#75838,#75839),.UNSPECIFIED.,.F.,.F.,
(4,2,2,2,2,4),(-0.477889345509609,-0.359641258797025,-0.24139317208444,
-0.12069658604222,-0.06034829302111,0.),.UNSPECIFIED.);
#897=B_SPLINE_CURVE_WITH_KNOTS('',3,(#75840,#75841,#75842,#75843,#75844,
#75845,#75846,#75847,#75848,#75849,#75850,#75851,#75852,#75853,#75854,#75855,
#75856,#75857,#75858,#75859,#75860,#75861),.UNSPECIFIED.,.F.,.F.,(4,2,2,
2,2,2,2,2,2,2,4),(-1.43366803652883,-1.31541994981624,-1.19717186310366,
-1.07647527706144,-1.01612698404033,-0.955778691019219,-0.895430397998109,
-0.835082104976999,-0.714385518934779,-0.596137432222194,-0.477889345509609),
 .UNSPECIFIED.);
#898=B_SPLINE_CURVE_WITH_KNOTS('',3,(#75865,#75866,#75867,#75868,#75869,
#75870,#75871,#75872,#75873,#75874,#75875,#75876,#75877,#75878,#75879,#75880,
#75881,#75882,#75883,#75884,#75885,#75886,#75887,#75888,#75889,#75890,#75891,
#75892,#75893,#75894,#75895,#75896),.UNSPECIFIED.,.F.,.F.,(4,2,2,2,2,2,
2,2,2,2,2,2,2,2,2,4),(-1.91155738203844,-1.85120908901733,-1.79086079599622,
-1.670164209954,-1.55191612324141,-1.43366803652883,-1.31541994981624,-1.19717186310366,
-1.07647527706144,-1.01612698404033,-0.955778691019219,-0.895430397998109,
-0.835082104976999,-0.714385518934779,-0.596137432222194,-0.47788934550961),
 .UNSPECIFIED.);
#899=B_SPLINE_CURVE_WITH_KNOTS('',3,(#75897,#75898,#75899,#75900,#75901,
#75902,#75903,#75904,#75905,#75906,#75907,#75908),.UNSPECIFIED.,.F.,.F.,
(4,2,2,2,2,4),(-0.47788934550961,-0.359641258797025,-0.241393172084441,
-0.12069658604222,-0.0603482930211102,0.),.UNSPECIFIED.);
#900=B_SPLINE_CURVE_WITH_KNOTS('',3,(#75918,#75919,#75920,#75921,#75922,
#75923,#75924,#75925,#75926,#75927),.UNSPECIFIED.,.F.,.F.,(4,2,2,2,4),(-1.22969838857394,
-1.15274028568534,-1.07578218279674,-0.9990279871136,-0.922273791430456),
 .UNSPECIFIED.);
#901=B_SPLINE_CURVE_WITH_KNOTS('',3,(#75929,#75930,#75931,#75932,#75933,
#75934,#75935,#75936,#75937,#75938),.UNSPECIFIED.,.F.,.F.,(4,2,2,2,4),(-0.307424597143485,
-0.230670401460341,-0.153916205777197,-0.0769581028885983,0.),
 .UNSPECIFIED.);
#902=B_SPLINE_CURVE_WITH_KNOTS('',3,(#75939,#75940,#75941,#75942,#75943,
#75944,#75945,#75946,#75947,#75948,#75949,#75950,#75951,#75952,#75953,#75954,
#75955,#75956),.UNSPECIFIED.,.F.,.F.,(4,2,2,2,2,2,2,2,4),(-0.922273791430456,
-0.845519595747312,-0.768765400064167,-0.691807297175569,-0.614849194286971,
-0.537891091398373,-0.460932988509774,-0.38417879282663,-0.307424597143485),
 .UNSPECIFIED.);
#903=B_SPLINE_CURVE_WITH_KNOTS('',3,(#75960,#75961,#75962,#75963,#75964,
#75965,#75966,#75967,#75968,#75969,#75970,#75971,#75972,#75973,#75974,#75975,
#75976,#75977,#75978,#75979,#75980,#75981,#75982,#75983,#75984,#75985),
 .UNSPECIFIED.,.F.,.F.,(4,2,2,2,2,2,2,2,2,2,2,2,4),(-1.22969838857394,-1.15274028568534,
-1.07578218279674,-0.9990279871136,-0.922273791430456,-0.845519595747312,
-0.768765400064167,-0.691807297175569,-0.614849194286971,-0.537891091398373,
-0.460932988509774,-0.38417879282663,-0.307424597143485),.UNSPECIFIED.);
#904=B_SPLINE_CURVE_WITH_KNOTS('',3,(#75986,#75987,#75988,#75989,#75990,
#75991,#75992,#75993,#75994,#75995),.UNSPECIFIED.,.F.,.F.,(4,2,2,2,4),(-0.307424597143485,
-0.230670401460341,-0.153916205777197,-0.0769581028885983,0.),
 .UNSPECIFIED.);
#905=B_SPLINE_CURVE_WITH_KNOTS('',3,(#77139,#77140,#77141,#77142,#77143,
#77144,#77145,#77146,#77147,#77148,#77149,#77150,#77151,#77152,#77153,#77154,
#77155,#77156,#77157,#77158,#77159,#77160,#77161,#77162,#77163,#77164,#77165,
#77166,#77167,#77168,#77169,#77170,#77171,#77172,#77173,#77174,#77175,#77176),
 .UNSPECIFIED.,.T.,.F.,(4,2,2,2,2,2,2,2,2,2,2,2,2,2,2,2,2,2,4),(-0.605125399548974,
-0.601986519691417,-0.572296417272211,-0.544506901286991,-0.51205526449825,
-0.473980307125887,-0.436263250016685,-0.397515325089208,-0.367226247639718,
-0.338720455098409,-0.30995049023698,-0.27886558943038,-0.238746391927005,
-0.193651773165657,-0.137323097666455,-0.0888290194031273,-0.0473891574083154,
-0.00368586125467713,0.),.UNSPECIFIED.);
#906=B_SPLINE_CURVE_WITH_KNOTS('',3,(#77178,#77179,#77180,#77181,#77182,
#77183,#77184,#77185,#77186,#77187,#77188,#77189,#77190,#77191,#77192,#77193,
#77194,#77195,#77196,#77197,#77198,#77199,#77200,#77201,#77202,#77203,#77204,
#77205,#77206,#77207,#77208,#77209,#77210,#77211,#77212,#77213,#77214,#77215,
#77216,#77217,#77218,#77219,#77220,#77221,#77222,#77223,#77224,#77225,#77226,
#77227,#77228,#77229,#77230,#77231,#77232,#77233,#77234,#77235,#77236,#77237,
#77238,#77239,#77240,#77241,#77242,#77243,#77244,#77245,#77246,#77247,#77248,
#77249,#77250,#77251,#77252,#77253,#77254,#77255,#77256,#77257,#77258,#77259,
#77260,#77261,#77262,#77263,#77264,#77265,#77266,#77267,#77268,#77269,#77270,
#77271,#77272,#77273,#77274,#77275,#77276,#77277,#77278,#77279,#77280,#77281,
#77282,#77283,#77284,#77285,#77286,#77287),.UNSPECIFIED.,.F.,.F.,(4,1,1,
1,1,1,1,1,1,1,1,1,1,1,1,1,1,1,1,1,1,1,1,1,1,1,1,1,1,1,1,1,1,1,1,1,1,1,1,
1,1,1,1,1,1,1,1,1,1,1,1,1,1,1,1,1,1,1,1,1,1,1,1,1,1,1,1,1,1,1,1,1,1,1,1,
1,1,1,1,1,1,1,1,1,1,1,1,1,1,1,1,1,1,1,1,1,1,1,1,1,1,1,1,1,1,1,1,4),(0.,
0.00446428571428571,0.00892857142857143,0.0178571428571429,0.0267857142857143,
0.0357142857142857,0.0446428571428571,0.0535714285714286,0.0625,0.0714285714285714,
0.0803571428571428,0.0892857142857143,0.0982142857142857,0.107142857142857,
0.116071428571429,0.125,0.133928571428571,0.142857142857143,0.154761904761905,
0.166666666666667,0.178571428571429,0.18452380952381,0.19047619047619,0.196428571428571,
0.202380952380952,0.214285714285714,0.222222222222222,0.23015873015873,
0.238095238095238,0.244047619047619,0.25,0.261904761904762,0.273809523809524,
0.285714285714286,0.297619047619048,0.30952380952381,0.321428571428571,
0.333333333333333,0.341269841269841,0.349206349206349,0.357142857142857,
0.365079365079365,0.373015873015873,0.380952380952381,0.392857142857143,
0.404761904761905,0.416666666666667,0.428571428571429,0.44047619047619,
0.452380952380952,0.46031746031746,0.468253968253968,0.472222222222222,
0.476190476190476,0.486772486772487,0.492063492063492,0.5,0.507936507936508,
0.515873015873016,0.523809523809524,0.535714285714286,0.547619047619048,
0.55952380952381,0.571428571428571,0.583333333333333,0.595238095238095,
0.607142857142857,0.619047619047619,0.626984126984127,0.634920634920635,
0.642857142857143,0.650793650793651,0.658730158730159,0.666666666666667,
0.674603174603175,0.682539682539683,0.69047619047619,0.702380952380952,
0.714285714285714,0.726190476190476,0.738095238095238,0.75,0.761904761904762,
0.773809523809524,0.785714285714286,0.797619047619047,0.809523809523809,
0.821428571428571,0.833333333333333,0.845238095238095,0.857142857142857,
0.866071428571429,0.875,0.883928571428571,0.892857142857143,0.901785714285714,
0.910714285714286,0.919642857142857,0.928571428571429,0.9375,0.946428571428571,
0.955357142857143,0.964285714285714,0.973214285714286,0.982142857142857,
0.991071428571429,0.995535714285714,1.),.UNSPECIFIED.);
#907=B_SPLINE_CURVE_WITH_KNOTS('',3,(#77288,#77289,#77290,#77291,#77292,
#77293,#77294,#77295,#77296,#77297,#77298,#77299,#77300,#77301,#77302,#77303,
#77304,#77305,#77306,#77307,#77308,#77309,#77310,#77311,#77312,#77313,#77314,
#77315,#77316,#77317,#77318,#77319,#77320,#77321,#77322,#77323,#77324,#77325),
 .UNSPECIFIED.,.T.,.F.,(4,2,2,2,2,2,2,2,2,2,2,2,2,2,2,2,2,2,4),(-0.605125399680566,
-0.601986519826148,-0.572296417399655,-0.544506901407513,-0.512055264610774,
-0.473980307229046,-0.436263250110675,-0.397515325173783,-0.367226247717055,
-0.338720455168909,-0.309950490300473,-0.278865589486237,-0.238746391973086,
-0.1936517732017,-0.137323097692225,-0.0888290194200642,-0.0473891574177423,
-0.00368586125594956,0.),.UNSPECIFIED.);
#908=B_SPLINE_CURVE_WITH_KNOTS('',3,(#77896,#77897,#77898,#77899,#77900,
#77901,#77902,#77903,#77904,#77905,#77906,#77907,#77908,#77909,#77910,#77911,
#77912,#77913,#77914,#77915,#77916,#77917,#77918,#77919,#77920,#77921,#77922,
#77923,#77924,#77925,#77926,#77927,#77928,#77929,#77930,#77931,#77932,#77933,
#77934,#77935,#77936,#77937,#77938,#77939,#77940,#77941,#77942,#77943,#77944),
 .UNSPECIFIED.,.F.,.F.,(4,3,3,3,3,3,3,3,3,3,3,3,3,3,3,3,4),(10.3761261730577,
10.5727849197489,10.7692055827359,10.9654664845638,11.1621727918026,11.2954213083143,
11.494377948575,11.6933749873077,11.8919022657422,12.0911341846241,12.2903661035059,
12.4887047013559,12.6878562506913,12.8857302559588,13.0855205773281,13.2853108986974,
13.4195932955372),.UNSPECIFIED.);
#909=B_SPLINE_CURVE_WITH_KNOTS('',3,(#77947,#77948,#77949,#77950,#77951,
#77952,#77953,#77954,#77955,#77956,#77957,#77958,#77959,#77960,#77961,#77962,
#77963,#77964,#77965,#77966,#77967,#77968,#77969,#77970,#77971,#77972,#77973,
#77974),.UNSPECIFIED.,.F.,.F.,(4,3,3,3,3,3,3,3,3,4),(11.6154215191106,11.818758087608,
12.02219938105,12.2256382911152,12.4297226410097,12.6103663143021,12.8124062223988,
13.0085336172549,13.213529781972,13.418525946689),.UNSPECIFIED.);
#910=B_SPLINE_CURVE_WITH_KNOTS('',3,(#77980,#77981,#77982,#77983,#77984,
#77985,#77986,#77987,#77988,#77989,#77990,#77991,#77992,#77993,#77994,#77995,
#77996,#77997,#77998,#77999,#78000,#78001,#78002,#78003,#78004,#78005,#78006,
#78007,#78008,#78009,#78010,#78011,#78012,#78013,#78014,#78015,#78016,#78017,
#78018,#78019,#78020,#78021,#78022,#78023,#78024,#78025,#78026,#78027,#78028,
#78029,#78030,#78031,#78032,#78033,#78034,#78035,#78036,#78037,#78038,#78039,
#78040,#78041,#78042,#78043),.UNSPECIFIED.,.F.,.F.,(4,3,3,3,3,3,3,3,3,3,
3,3,3,3,3,3,3,3,3,3,3,4),(15.7079632679489,15.9107481580219,16.1142494687792,
16.270145284272,16.4687682481423,16.6678487059726,16.8660184761811,17.0655542778223,
17.2650900794635,17.463705654094,17.6627879592342,17.8609505715831,18.0604927231191,
18.2600348746551,18.4586404264755,18.6577252373183,18.8558771547285,19.0554284122876,
19.2549796698466,19.4536004000213,19.6518004795038,19.7024262307223),
 .UNSPECIFIED.);
#911=B_SPLINE_CURVE_WITH_KNOTS('',3,(#78044,#78045,#78046,#78047,#78048,
#78049,#78050,#78051,#78052,#78053,#78054,#78055,#78056,#78057,#78058,#78059,
#78060,#78061,#78062,#78063,#78064,#78065,#78066,#78067,#78068,#78069,#78070,
#78071,#78072,#78073,#78074,#78075,#78076,#78077,#78078,#78079,#78080),
 .UNSPECIFIED.,.F.,.F.,(4,3,3,3,3,3,3,3,3,3,3,3,4),(13.4195932955372,13.6179476079485,
13.816207268142,14.0144158621728,14.2130841295482,14.2802556938889,14.4789073498003,
14.6779806346204,14.8761820439794,15.0756912665299,15.2752004890805,15.4915818782546,
15.7079632674287),.UNSPECIFIED.);
#912=B_SPLINE_CURVE_WITH_KNOTS('',3,(#78082,#78083,#78084,#78085,#78086,
#78087,#78088,#78089,#78090,#78091,#78092,#78093,#78094,#78095,#78096,#78097,
#78098,#78099,#78100,#78101,#78102,#78103,#78104,#78105,#78106,#78107,#78108,
#78109,#78110,#78111,#78112,#78113,#78114,#78115,#78116,#78117,#78118),
 .UNSPECIFIED.,.F.,.F.,(4,3,3,3,3,3,3,3,3,3,3,3,4),(13.418525946689,13.6053111094936,
13.8042318364677,14.003237853522,14.2017004757908,14.400978190238,14.6002559046852,
14.7992124415244,14.9982095061125,15.1967366702124,15.3959686850445,15.5952006998767,
15.7079632679489),.UNSPECIFIED.);
#913=B_SPLINE_CURVE_WITH_KNOTS('',3,(#78119,#78120,#78121,#78122,#78123,
#78124,#78125,#78126,#78127,#78128,#78129,#78130,#78131,#78132,#78133,#78134,
#78135,#78136,#78137,#78138,#78139,#78140,#78141,#78142,#78143,#78144,#78145,
#78146,#78147,#78148,#78149,#78150,#78151,#78152,#78153,#78154,#78155,#78156,
#78157,#78158,#78159,#78160,#78161,#78162,#78163,#78164,#78165,#78166,#78167,
#78168,#78169,#78170,#78171,#78172,#78173,#78174,#78175,#78176,#78177,#78178,
#78179,#78180,#78181,#78182,#78183,#78184,#78185,#78186,#78187,#78188,#78189,
#78190,#78191,#78192,#78193,#78194,#78195,#78196,#78197,#78198,#78199,#78200,
#78201,#78202,#78203,#78204,#78205,#78206,#78207,#78208,#78209,#78210,#78211,
#78212,#78213,#78214,#78215,#78216,#78217,#78218,#78219,#78220,#78221,#78222,
#78223,#78224,#78225,#78226,#78227,#78228,#78229,#78230,#78231,#78232,#78233,
#78234,#78235,#78236,#78237,#78238,#78239,#78240,#78241,#78242),
 .UNSPECIFIED.,.F.,.F.,(4,2,2,2,2,2,2,2,2,2,2,2,2,2,2,2,2,2,2,2,2,2,2,2,
2,2,2,2,2,2,2,2,2,2,2,2,2,2,2,2,2,2,2,2,2,2,2,2,2,2,2,2,2,2,2,2,2,2,2,2,
2,4),(-1.96103056545371,-1.92615510476781,-1.90994104798314,-1.9046916544681,
-1.90116335747262,-1.89772121026667,-1.89353123364095,-1.8830555785659,
-1.84636429336028,-1.83469395897624,-1.82971190344123,-1.82587053879483,
-1.82382632031197,-1.82191411745611,-1.81939311968034,-1.81356733650211,
-1.77965416666506,-1.76360355394232,-1.75280328971649,-1.74820347743362,
-1.74476514754024,-1.74105759432205,-1.73505605688044,-1.70682592759978,
-1.6841639181994,-1.67334525175968,-1.67015445276645,-1.66812211217972,
-1.66633132628009,-1.66333921335296,-1.65504429895045,-1.62400305204443,
-1.60514022362692,-1.59676356512943,-1.59258448468083,-1.58919905483207,
-1.5852684928244,-1.57835914547407,-1.54422662487699,-1.52704989903113,
-1.51777093811399,-1.51474603772319,-1.51275491824691,-1.51094365904601,
-1.50782252160796,-1.49846413471266,-1.47181634411575,-1.44773006870327,
-1.44064466762602,-1.43672150260578,-1.43334093274202,-1.42916612578598,
-1.42263789249716,-1.39594967959925,-1.37360499022705,-1.3663301636072,
-1.3611348244643,-1.35870036542346,-1.35679264787092,-1.35442699301585,
-1.34960688579188,-1.33784917433159),.UNSPECIFIED.);
#914=B_SPLINE_CURVE_WITH_KNOTS('',3,(#78248,#78249,#78250,#78251,#78252,
#78253,#78254,#78255,#78256,#78257,#78258,#78259,#78260,#78261,#78262,#78263,
#78264,#78265,#78266,#78267,#78268,#78269,#78270,#78271,#78272,#78273,#78274,
#78275,#78276,#78277,#78278,#78279,#78280,#78281,#78282,#78283,#78284,#78285,
#78286,#78287,#78288,#78289,#78290,#78291,#78292,#78293,#78294,#78295,#78296,
#78297,#78298,#78299,#78300,#78301,#78302,#78303,#78304,#78305,#78306,#78307,
#78308),.UNSPECIFIED.,.F.,.F.,(4,3,3,3,3,3,3,3,3,3,3,3,3,3,3,3,3,3,3,3,
4),(21.991148575456,22.2398140554212,22.4384256549512,22.6375089538666,
22.8356672026196,23.0352130266162,23.2347588506128,23.4333701243398,23.6324535047059,
23.8306114233726,24.0301575345884,24.2297036458043,24.4283147914976,24.6273982038722,
24.8255559829737,25.0251022119848,25.2246484409959,25.4232904579861,25.6215093722145,
25.8197872076773,25.9848803801132),.UNSPECIFIED.);
#915=B_SPLINE_CURVE_WITH_KNOTS('',3,(#78309,#78310,#78311,#78312,#78313,
#78314,#78315,#78316,#78317,#78318,#78319,#78320,#78321,#78322,#78323,#78324,
#78325,#78326,#78327,#78328,#78329,#78330,#78331,#78332,#78333,#78334,#78335,
#78336,#78337,#78338,#78339,#78340,#78341,#78342,#78343,#78344,#78345),
 .UNSPECIFIED.,.F.,.F.,(4,3,3,3,3,3,3,3,3,3,3,3,4),(19.7024262307223,19.9005709735403,
20.0991973388965,20.2499244650382,20.4485361071857,20.6476193954467,20.845777725713,
21.0453234929714,21.2448692602297,21.4412420479956,21.6371996234507,21.8332504102883,
21.9911485751285),.UNSPECIFIED.);
#916=B_SPLINE_CURVE_WITH_KNOTS('',3,(#78346,#78347,#78348,#78349,#78350,
#78351,#78352,#78353,#78354,#78355,#78356,#78357,#78358,#78359,#78360,#78361,
#78362,#78363,#78364,#78365,#78366,#78367,#78368,#78369,#78370,#78371,#78372,
#78373,#78374,#78375,#78376,#78377,#78378,#78379,#78380,#78381,#78382,#78383,
#78384,#78385,#78386,#78387,#78388,#78389,#78390,#78391,#78392,#78393,#78394,
#78395,#78396,#78397,#78398,#78399,#78400,#78401,#78402,#78403,#78404,#78405,
#78406,#78407,#78408,#78409,#78410,#78411,#78412,#78413,#78414,#78415,#78416,
#78417,#78418,#78419,#78420,#78421,#78422,#78423,#78424,#78425,#78426,#78427,
#78428,#78429,#78430,#78431,#78432,#78433,#78434,#78435,#78436,#78437,#78438,
#78439,#78440,#78441,#78442,#78443,#78444,#78445,#78446,#78447,#78448,#78449,
#78450,#78451,#78452,#78453,#78454,#78455,#78456,#78457,#78458,#78459,#78460,
#78461,#78462,#78463,#78464,#78465,#78466,#78467,#78468,#78469,#78470,#78471,
#78472,#78473,#78474,#78475,#78476,#78477,#78478,#78479,#78480,#78481,#78482,
#78483,#78484,#78485,#78486,#78487,#78488,#78489,#78490,#78491,#78492,#78493,
#78494,#78495,#78496,#78497,#78498,#78499,#78500,#78501,#78502,#78503,#78504,
#78505,#78506,#78507,#78508,#78509,#78510,#78511,#78512,#78513,#78514,#78515,
#78516,#78517,#78518,#78519,#78520,#78521,#78522,#78523,#78524,#78525,#78526,
#78527,#78528,#78529,#78530,#78531,#78532,#78533,#78534,#78535),
 .UNSPECIFIED.,.F.,.F.,(4,2,2,2,2,2,2,2,2,2,2,2,2,2,2,2,2,2,2,2,2,2,2,2,
2,2,2,2,2,2,2,2,2,2,2,2,2,2,2,2,2,2,2,2,2,2,2,2,2,2,2,2,2,2,2,2,2,2,2,2,
2,2,2,2,2,2,2,2,2,2,2,2,2,2,2,2,2,2,2,2,2,2,2,2,2,2,2,2,2,2,2,2,2,2,4),
(-1.33784917433159,-1.32756271885982,-1.30746809628493,-1.28939857659663,
-1.28395387447302,-1.28036685748039,-1.27691930054231,-1.2727846053549,
-1.26276650569296,-1.22575346202038,-1.21407469874287,-1.20681188390887,
-1.20403977707747,-1.20209398347381,-1.19993728032837,-1.19614402680512,
-1.1729430995681,-1.15449759215625,-1.14117856246438,-1.13168731495249,
-1.12730885836149,-1.12390720854947,-1.12011025153647,-1.11365057866505,
-1.07528746513936,-1.0553370235293,-1.05052825197158,-1.04816492281006,
-1.04644637863359,-1.04410710587933,-1.03942200525473,-1.01275043165541,
-0.980829421102169,-0.974447844548088,-0.970667458066885,-0.9672627866578,
-0.962855203362212,-0.953192246538504,-0.939528089692697,-0.921336843879064,
-0.898406338458633,-0.894624793607861,-0.89247094204319,-0.890525409423738,
-0.887750286363114,-0.880459212620312,-0.868713363789876,-0.831175749903035,
-0.822319674972369,-0.817511683875312,-0.814081167966399,-0.810469415682009,
-0.804899683798356,-0.78523918108987,-0.766557014422738,-0.744919619905274,
-0.740103169427347,-0.737738155416985,-0.735829107829343,-0.733390517868837,
-0.728181935370119,-0.720884753609942,-0.69840605593486,-0.671982171455758,
-0.665440679358723,-0.661259612770394,-0.657875180711825,-0.653948729818894,
-0.646860388854981,-0.622776219453138,-0.596138296662889,-0.586737876282968,
-0.58360986965392,-0.581796092624829,-0.579804634036784,-0.576781103437763,
-0.567518514649867,-0.5503895920759,-0.516283668413562,-0.509384121107263,
-0.505456557571469,-0.502072217283729,-0.497892614783625,-0.489508899082389,
-0.470574667497139,-0.439334079795521,-0.431182458349704,-0.428211654249095,
-0.426426865138206,-0.424400132297633,-0.421208225679968,-0.410292686384152,
-0.387244928865465,-0.359349102730245,-0.35767490124526),.UNSPECIFIED.);
#917=B_SPLINE_CURVE_WITH_KNOTS('',3,(#78541,#78542,#78543,#78544,#78545,
#78546,#78547,#78548,#78549,#78550,#78551,#78552,#78553,#78554,#78555,#78556,
#78557,#78558,#78559,#78560,#78561,#78562,#78563,#78564,#78565,#78566,#78567,
#78568,#78569,#78570,#78571,#78572,#78573,#78574,#78575,#78576,#78577,#78578,
#78579,#78580,#78581,#78582,#78583,#78584,#78585,#78586,#78587,#78588,#78589,
#78590,#78591,#78592,#78593,#78594,#78595,#78596,#78597,#78598,#78599,#78600,
#78601,#78602,#78603,#78604),.UNSPECIFIED.,.F.,.F.,(4,3,3,3,3,3,3,3,3,3,
3,3,3,3,3,3,3,3,3,3,3,4),(28.2743338827622,28.471046494824,28.667522646786,
28.8638355561955,29.0606093893357,29.204427621762,29.4030388737554,29.602122259555,
29.8002801509351,29.9998262839443,30.1993724169535,30.3979836682494,30.5970670542233,
30.7952249447415,30.9947710784433,31.1943172121451,31.3929284665306,31.5920118517321,
31.7901697455092,31.9897158764229,32.1892620073366,32.2690227615599),
 .UNSPECIFIED.);
#918=B_SPLINE_CURVE_WITH_KNOTS('',3,(#78605,#78606,#78607,#78608,#78609,
#78610,#78611,#78612,#78613,#78614,#78615,#78616,#78617,#78618,#78619,#78620,
#78621,#78622,#78623,#78624,#78625,#78626,#78627,#78628,#78629,#78630,#78631,
#78632,#78633,#78634,#78635,#78636,#78637,#78638,#78639,#78640,#78641,#78642,
#78643,#78644),.UNSPECIFIED.,.F.,.F.,(4,3,3,3,3,3,3,3,3,3,3,3,3,4),(25.9848803801132,
26.1834953229633,26.2195932361874,26.4182044870052,26.6172878730986,26.8154457638341,
27.0149918976065,27.2145380313789,27.4131492703702,27.6122326594203,27.8103905369092,
28.0099366817399,28.2094828265705,28.2743338823081),.UNSPECIFIED.);
#919=B_SPLINE_CURVE_WITH_KNOTS('',3,(#78646,#78647,#78648,#78649,#78650,
#78651,#78652,#78653,#78654,#78655,#78656,#78657,#78658,#78659,#78660,#78661,
#78662,#78663,#78664,#78665,#78666,#78667,#78668,#78669,#78670,#78671,#78672,
#78673,#78674,#78675,#78676,#78677,#78678,#78679,#78680,#78681,#78682,#78683,
#78684,#78685,#78686,#78687,#78688,#78689,#78690,#78691,#78692,#78693,#78694,
#78695,#78696,#78697,#78698,#78699,#78700,#78701,#78702,#78703,#78704,#78705,
#78706,#78707,#78708,#78709,#78710,#78711,#78712,#78713,#78714,#78715,#78716,
#78717,#78718,#78719,#78720,#78721,#78722,#78723),.UNSPECIFIED.,.F.,.F.,
(4,2,2,2,2,2,2,2,2,2,2,2,2,2,2,2,2,2,2,2,2,2,2,2,2,2,2,2,2,2,2,2,2,2,2,
2,2,2,4),(-0.35767490124526,-0.353305421574032,-0.349595255689124,-0.346170349734198,
-0.341613025527349,-0.331039317409103,-0.315467840449632,-0.284630569162204,
-0.276082485707659,-0.273059191968105,-0.271264872944148,-0.26925104854512,
-0.266119814035009,-0.255837730626168,-0.235260851599245,-0.206256226033263,
-0.199755621329898,-0.195586231881908,-0.192202201704497,-0.188266060712361,
-0.181130922108284,-0.156680755239567,-0.129309790545012,-0.12084135672295,
-0.117828378943232,-0.116035930774091,-0.114019618232537,-0.111292342370151,
-0.10519671203938,-0.102721920333533,-0.0876272756893066,-0.058692799791427,
-0.0465427107185492,-0.0416200658294285,-0.0381695350916806,-0.0345894279611084,
-0.0309667648357375,-0.0258029228333309,-0.000454559668527777),
 .UNSPECIFIED.);
#920=B_SPLINE_CURVE_WITH_KNOTS('',3,(#78724,#78725,#78726,#78727,#78728,
#78729,#78730,#78731,#78732,#78733,#78734,#78735,#78736,#78737,#78738,#78739,
#78740,#78741,#78742,#78743,#78744,#78745,#78746,#78747,#78748,#78749,#78750,
#78751,#78752,#78753,#78754,#78755,#78756,#78757,#78758,#78759,#78760,#78761,
#78762,#78763,#78764,#78765,#78766,#78767,#78768,#78769,#78770,#78771,#78772,
#78773,#78774,#78775,#78776,#78777,#78778,#78779,#78780,#78781,#78782,#78783,
#78784,#78785,#78786,#78787,#78788,#78789,#78790,#78791,#78792,#78793,#78794,
#78795,#78796,#78797,#78798,#78799,#78800,#78801,#78802,#78803,#78804,#78805,
#78806,#78807,#78808,#78809,#78810,#78811,#78812,#78813,#78814,#78815,#78816,
#78817,#78818,#78819,#78820,#78821,#78822,#78823,#78824,#78825,#78826,#78827,
#78828,#78829,#78830,#78831,#78832,#78833,#78834,#78835,#78836,#78837,#78838,
#78839,#78840,#78841,#78842,#78843,#78844,#78845,#78846,#78847,#78848,#78849,
#78850,#78851,#78852,#78853,#78854,#78855,#78856,#78857),.UNSPECIFIED.,
 .F.,.F.,(4,2,2,2,2,2,2,2,2,2,2,2,2,2,2,2,2,2,2,2,2,2,2,2,2,2,2,2,2,2,2,
2,2,2,2,2,2,2,2,2,2,2,2,2,2,2,2,2,2,2,2,2,2,2,2,2,2,2,2,2,2,2,2,2,2,2,4),
(-1.96074742950682,-1.92903103891679,-1.92565394037489,-1.92276149113017,
-1.92079576416029,-1.91868782038145,-1.91511919124233,-1.9004272637792,
-1.87491209959576,-1.85410453753753,-1.84813467188929,-1.8479163875349,
-1.84770085619269,-1.84748534465099,-1.84726696921916,-1.8470425292415,
-1.84680828683192,-1.84655965391311,-1.8462907190531,-1.84285619153888,
-1.83917562130058,-1.83327062379081,-1.80958144579062,-1.78819556450568,
-1.77185176006219,-1.76828771149167,-1.76618076264445,-1.76423727298914,
-1.76136039858266,-1.75390897523033,-1.72574504428177,-1.70091214406183,
-1.69373013799826,-1.68978518091811,-1.68640266589147,-1.68224669189248,
-1.67579014886227,-1.64469048785606,-1.62559436177049,-1.61890027333474,
-1.61401473550339,-1.61163686591323,-1.60991777261583,-1.60759235705981,
-1.60311921587875,-1.56755879210728,-1.54516146622278,-1.53829655404521,
-1.53441625718776,-1.53102828603607,-1.52678609995889,-1.52003079834842,
-1.4794373383665,-1.46156592197152,-1.45793400775734,-1.45581228428364,
-1.45387566523685,-1.45103839222197,-1.44383935846247,-1.41163093054835,
-1.39220114476349,-1.38398165704351,-1.37983323323713,-1.3764507990235,
-1.37249905929152,-1.36548575233231,-1.33781741101813),.UNSPECIFIED.);
#921=B_SPLINE_CURVE_WITH_KNOTS('',3,(#78863,#78864,#78865,#78866,#78867,
#78868,#78869,#78870,#78871,#78872,#78873,#78874,#78875,#78876,#78877,#78878,
#78879,#78880,#78881,#78882,#78883,#78884,#78885,#78886,#78887,#78888,#78889,
#78890,#78891,#78892,#78893,#78894,#78895,#78896,#78897,#78898,#78899,#78900,
#78901,#78902,#78903,#78904,#78905,#78906,#78907,#78908,#78909,#78910,#78911,
#78912,#78913,#78914,#78915,#78916,#78917,#78918,#78919,#78920,#78921,#78922,
#78923),.UNSPECIFIED.,.F.,.F.,(4,3,3,3,3,3,3,3,3,3,3,3,3,3,3,3,3,3,3,3,
4),(34.5575191894876,34.7574162785789,34.9657563357451,35.1740963929112,
35.3727076459311,35.571791031474,35.7699489238318,35.9694950559673,36.1690411881028,
36.3676524411512,36.566735826687,36.7648937190718,36.9644398511831,37.1639859832943,
37.3625972363943,37.5616806219172,37.7598385143569,37.9593846464214,38.1589307784859,
38.3575822166857,38.5521360709588),.UNSPECIFIED.);
#922=B_SPLINE_CURVE_WITH_KNOTS('',3,(#78924,#78925,#78926,#78927,#78928,
#78929,#78930,#78931,#78932,#78933,#78934,#78935,#78936,#78937,#78938,#78939,
#78940,#78941,#78942,#78943,#78944,#78945,#78946,#78947,#78948,#78949,#78950,
#78951,#78952,#78953,#78954,#78955,#78956,#78957,#78958,#78959,#78960),
 .UNSPECIFIED.,.F.,.F.,(4,3,3,3,3,3,3,3,3,3,3,3,4),(32.2690227615599,32.4674315365707,
32.6656817064457,32.8638217074933,33.0624351927568,33.1842068025282,33.3828180553875,
33.5819014409705,33.7800593331526,33.9796054654362,34.1791515977197,34.4020312303527,
34.5575191891138),.UNSPECIFIED.);
#923=B_SPLINE_CURVE_WITH_KNOTS('',3,(#78961,#78962,#78963,#78964,#78965,
#78966,#78967,#78968,#78969,#78970,#78971,#78972,#78973,#78974,#78975,#78976,
#78977,#78978,#78979,#78980,#78981,#78982,#78983,#78984,#78985,#78986,#78987,
#78988,#78989,#78990,#78991,#78992,#78993,#78994,#78995,#78996,#78997,#78998,
#78999,#79000,#79001,#79002,#79003,#79004,#79005,#79006,#79007,#79008,#79009,
#79010,#79011,#79012,#79013,#79014,#79015,#79016,#79017,#79018,#79019,#79020,
#79021,#79022,#79023,#79024,#79025,#79026,#79027,#79028,#79029,#79030,#79031,
#79032,#79033,#79034,#79035,#79036,#79037,#79038,#79039,#79040,#79041,#79042,
#79043,#79044,#79045,#79046,#79047,#79048,#79049,#79050,#79051,#79052,#79053,
#79054,#79055,#79056,#79057,#79058,#79059,#79060,#79061,#79062,#79063,#79064,
#79065,#79066,#79067,#79068,#79069,#79070,#79071,#79072,#79073,#79074,#79075,
#79076,#79077,#79078,#79079,#79080,#79081,#79082,#79083,#79084,#79085,#79086,
#79087,#79088,#79089,#79090,#79091,#79092,#79093,#79094,#79095,#79096,#79097,
#79098,#79099,#79100,#79101,#79102,#79103,#79104,#79105,#79106,#79107,#79108,
#79109,#79110,#79111,#79112,#79113,#79114,#79115,#79116,#79117,#79118,#79119,
#79120,#79121,#79122,#79123,#79124,#79125,#79126,#79127,#79128,#79129,#79130,
#79131,#79132,#79133,#79134,#79135,#79136,#79137,#79138,#79139,#79140,#79141,
#79142,#79143,#79144,#79145,#79146,#79147,#79148,#79149,#79150,#79151,#79152,
#79153,#79154),.UNSPECIFIED.,.F.,.F.,(4,2,2,2,2,2,2,2,2,2,2,2,2,2,2,2,2,
2,2,2,2,2,2,2,2,2,2,2,2,2,2,2,2,2,2,2,2,2,2,2,2,2,2,2,2,2,2,2,2,2,2,2,2,
2,2,2,2,2,2,2,2,2,2,2,2,2,2,2,2,2,2,2,2,2,2,2,2,2,2,2,2,2,2,2,2,2,2,2,2,
2,2,2,2,2,2,2,4),(-1.33781741101813,-1.32557054748569,-1.30642325762965,
-1.30274443726903,-1.3006124784046,-1.29868008249966,-1.29586834752457,
-1.28882936678198,-1.25644145308868,-1.24063435784198,-1.22995239379204,
-1.22537824600346,-1.22195104437654,-1.21824825123111,-1.21223927049898,
-1.18597264853726,-1.16660703127076,-1.15094181272081,-1.1474117560645,
-1.14531188838297,-1.14336405551559,-1.14093291874721,-1.13473541317179,
-1.10549895970416,-1.08015610547455,-1.07291039461136,-1.06895207515003,
-1.06556957871674,-1.0614280936387,-1.05502288041877,-1.01515152809839,
-0.997476336090281,-0.992916540144445,-0.990601665430235,-0.988689696233156,
-0.986232812579258,-0.980778604028425,-0.953630680690489,-0.924854703890282,
-0.918350583704046,-0.914180129903392,-0.910795981752568,-0.906860541147936,
-0.899729092546172,-0.875308682999262,-0.847998749724382,-0.839453654853804,
-0.836430689067862,-0.834636393737101,-0.832622393064683,-0.82949058378624,
-0.819203594884595,-0.798609412213889,-0.769625876465328,-0.763124628596293,
-0.75895495005321,-0.755570762541077,-0.751634525082281,-0.744499459965995,
-0.720051244764577,-0.692685845095345,-0.684209210936487,-0.681195075399877,
-0.679402357538995,-0.677386193267486,-0.674244322217734,-0.663856014568973,
-0.642886016807153,-0.61441246624213,-0.60790414398511,-0.603732352207339,
-0.600347967854745,-0.596413206435946,-0.589285745128215,-0.564898521241319,
-0.537656523833296,-0.529023735626237,-0.52598939754516,-0.524192955143136,
-0.522181455130139,-0.519061844668738,-0.508897862206567,-0.488752430631048,
-0.459147264159303,-0.452656356672005,-0.448489564172418,-0.445105368015876,
-0.441166475658373,-0.434018934636533,-0.409473381633096,-0.381912546958663,
-0.37367728374367,-0.370694922915517,-0.368907871851527,-0.366883711054085,
-0.363704659428616,-0.357528053359181),.UNSPECIFIED.);
#924=B_SPLINE_CURVE_WITH_KNOTS('',3,(#79160,#79161,#79162,#79163,#79164,
#79165,#79166,#79167,#79168,#79169,#79170,#79171,#79172,#79173,#79174,#79175,
#79176,#79177,#79178,#79179,#79180,#79181,#79182,#79183,#79184,#79185,#79186,
#79187,#79188,#79189,#79190,#79191,#79192,#79193,#79194,#79195,#79196,#79197,
#79198,#79199,#79200,#79201,#79202,#79203,#79204,#79205,#79206,#79207,#79208,
#79209,#79210,#79211,#79212,#79213,#79214,#79215,#79216,#79217,#79218,#79219,
#79220,#79221,#79222,#79223),.UNSPECIFIED.,.F.,.F.,(4,3,3,3,3,3,3,3,3,3,
3,3,3,3,3,3,3,3,3,3,3,4),(40.8407044972538,41.0794323899344,41.1437651640605,
41.3423764171309,41.5414598026612,41.7396176950701,41.939163827161,42.138709959252,
42.3373212123239,42.5364045978538,42.7345624902641,42.9341086223539,43.1336547544436,
43.3322660075162,43.5313493930459,43.729507285457,43.929053417546,44.1285995496351,
44.3272255543724,44.5254262229014,44.7236012490529,44.8344902319945),
 .UNSPECIFIED.);
#925=B_SPLINE_CURVE_WITH_KNOTS('',3,(#79224,#79225,#79226,#79227,#79228,
#79229,#79230,#79231,#79232,#79233,#79234,#79235,#79236,#79237,#79238,#79239,
#79240,#79241,#79242,#79243,#79244,#79245,#79246,#79247,#79248,#79249,#79250,
#79251,#79252,#79253,#79254,#79255,#79256,#79257,#79258,#79259,#79260),
 .UNSPECIFIED.,.F.,.F.,(4,3,3,3,3,3,3,3,3,3,3,3,4),(38.5521360709588,38.7502960103253,
38.9520857920013,39.1538755736774,39.3524868267472,39.5515702122776,39.7497281046856,
39.9492742367772,40.1488203688689,40.3464146547053,40.5435759929651,40.740698017163,
40.8407044966673),.UNSPECIFIED.);
#926=B_SPLINE_CURVE_WITH_KNOTS('',3,(#79262,#79263,#79264,#79265,#79266,
#79267,#79268,#79269,#79270,#79271,#79272,#79273,#79274,#79275,#79276,#79277,
#79278,#79279,#79280,#79281,#79282,#79283,#79284,#79285,#79286,#79287,#79288,
#79289,#79290,#79291,#79292,#79293,#79294,#79295,#79296,#79297,#79298,#79299,
#79300,#79301,#79302,#79303,#79304,#79305,#79306,#79307,#79308,#79309,#79310,
#79311,#79312,#79313,#79314,#79315,#79316,#79317,#79318,#79319,#79320,#79321,
#79322,#79323,#79324,#79325,#79326,#79327,#79328,#79329,#79330,#79331,#79332,
#79333,#79334,#79335,#79336,#79337,#79338,#79339,#79340,#79341,#79342,#79343,
#79344,#79345,#79346,#79347,#79348,#79349,#79350,#79351),.UNSPECIFIED.,
 .F.,.F.,(4,2,2,2,2,2,2,2,2,2,2,2,2,2,2,2,2,2,2,2,2,2,2,2,2,2,2,2,2,2,2,
2,2,2,2,2,2,2,2,2,2,2,2,2,4),(-0.357528053359181,-0.352930405912873,-0.330462642455156,
-0.304009230386146,-0.297468152475844,-0.293286744040802,-0.289901657857665,
-0.28597402498536,-0.278882326711891,-0.254777871301631,-0.228102710486401,
-0.218743244390323,-0.215619612249958,-0.213806399782365,-0.211813531796777,
-0.208784517756886,-0.199476651462255,-0.182208505324855,-0.14831736500732,
-0.141398888399427,-0.137466728906528,-0.134291370221815,-0.133828565823825,
-0.133649087723284,-0.133563820798045,-0.133266687893385,-0.132993635286933,
-0.13273680585135,-0.132490289554489,-0.13224935607113,-0.132009976436451,
-0.131768500529493,-0.131521419772047,-0.131265174605576,-0.125091814624551,
-0.117449814466257,-0.100593419334615,-0.0755948938769075,-0.063960119168855,
-0.0606101279504411,-0.0585490235715298,-0.0565519714899307,-0.0535023239476616,
-0.044006928678212,-0.000454731073245817),.UNSPECIFIED.);
#927=B_SPLINE_CURVE_WITH_KNOTS('',3,(#79352,#79353,#79354,#79355,#79356,
#79357,#79358,#79359,#79360,#79361,#79362,#79363,#79364,#79365,#79366,#79367,
#79368,#79369,#79370,#79371,#79372,#79373,#79374,#79375,#79376,#79377,#79378,
#79379,#79380,#79381,#79382,#79383,#79384,#79385,#79386,#79387,#79388,#79389,
#79390,#79391,#79392,#79393,#79394,#79395,#79396,#79397,#79398,#79399,#79400,
#79401,#79402,#79403,#79404,#79405,#79406,#79407,#79408,#79409,#79410,#79411,
#79412,#79413,#79414,#79415,#79416,#79417,#79418,#79419,#79420,#79421,#79422,
#79423,#79424,#79425,#79426,#79427,#79428,#79429,#79430,#79431,#79432,#79433,
#79434,#79435,#79436,#79437,#79438,#79439,#79440,#79441,#79442,#79443,#79444,
#79445,#79446,#79447,#79448,#79449,#79450,#79451,#79452,#79453,#79454,#79455,
#79456,#79457,#79458,#79459,#79460,#79461,#79462,#79463,#79464,#79465,#79466,
#79467,#79468,#79469,#79470,#79471,#79472,#79473,#79474,#79475,#79476,#79477),
 .UNSPECIFIED.,.F.,.F.,(4,2,2,2,2,2,2,2,2,2,2,2,2,2,2,2,2,2,2,2,2,2,2,2,
2,2,2,2,2,2,2,2,2,2,2,2,2,2,2,2,2,2,2,2,2,2,2,2,2,2,2,2,2,2,2,2,2,2,2,2,
2,2,4),(-1.96083796406488,-1.95304681045243,-1.94724249161864,-1.94387972686813,
-1.94064315409192,-1.9369955779625,-1.9312507196165,-1.91060233647322,-1.8795195359313,
-1.86874028479968,-1.86556113495289,-1.86353727366749,-1.8617507481269,
-1.85876976042871,-1.85054114363201,-1.82300332314382,-1.79847602423964,
-1.79133165142375,-1.78739393655562,-1.78401041883277,-1.77984403926801,
-1.77335286974085,-1.74374147656501,-1.72358232948348,-1.71341515720326,
-1.71029554206995,-1.70828432844667,-1.70648834936082,-1.70345520650015,
-1.69482822147054,-1.66760920879968,-1.64323986200272,-1.63611542445173,
-1.63218174894907,-1.62879795656762,-1.62462645986952,-1.61811766535295,
-1.58963305853873,-1.56865179009997,-1.55826088380347,-1.55511901872939,
-1.5531031074038,-1.55131078736854,-1.54829766882227,-1.53982580348723,
-1.51248326195216,-1.48805261014567,-1.48092042094419,-1.47698517392718,
-1.47360148933081,-1.46943198782833,-1.46293006829784,-1.43393941257665,
-1.41332999833887,-1.40303920067864,-1.3999072202002,-1.397893400297,-1.39609947380278,
-1.39307754034751,-1.38453773086663,-1.35371901011083,-1.3381574739814,
-1.33767722568999),.UNSPECIFIED.);
#928=B_SPLINE_CURVE_WITH_KNOTS('',3,(#79483,#79484,#79485,#79486,#79487,
#79488,#79489,#79490,#79491,#79492,#79493,#79494,#79495,#79496,#79497,#79498,
#79499,#79500,#79501,#79502,#79503,#79504,#79505,#79506,#79507,#79508,#79509,
#79510,#79511,#79512,#79513,#79514,#79515,#79516,#79517,#79518,#79519,#79520,
#79521,#79522,#79523,#79524,#79525,#79526,#79527,#79528,#79529,#79530,#79531,
#79532,#79533,#79534,#79535,#79536,#79537,#79538,#79539,#79540,#79541,#79542,
#79543,#79544,#79545,#79546),.UNSPECIFIED.,.F.,.F.,(4,3,3,3,3,3,3,3,3,3,
3,3,3,3,3,3,3,3,3,3,3,4),(47.123889804236,47.3221361842061,47.5201262658007,
47.7179229753624,47.9162111610125,48.1083787304012,48.3069899834732,48.5060733690031,
48.7042312614136,48.9037773935032,49.1033235255928,49.3019347786649,49.5010181641948,
49.6991760566053,49.8987221886948,50.0982683207843,50.2968795738564,50.4959629593862,
50.6941208517967,50.8936669838863,51.0932131159759,51.1183439304616),
 .UNSPECIFIED.);
#929=B_SPLINE_CURVE_WITH_KNOTS('',3,(#79547,#79548,#79549,#79550,#79551,
#79552,#79553,#79554,#79555,#79556,#79557,#79558,#79559,#79560,#79561,#79562,
#79563,#79564,#79565,#79566,#79567,#79568,#79569,#79570,#79571,#79572,#79573,
#79574,#79575,#79576,#79577,#79578,#79579,#79580,#79581,#79582,#79583,#79584,
#79585,#79586),.UNSPECIFIED.,.F.,.F.,(4,3,3,3,3,3,3,3,3,3,3,3,3,4),(44.8344902319945,
45.0330984607145,45.1235443448266,45.3221555978987,45.5212389834285,45.719396875839,
45.9189430079286,46.1184891400182,46.3171003930903,46.5161837786202,46.7143416710308,
46.9138878031202,47.1134339352097,47.1238898038468),.UNSPECIFIED.);
#930=B_SPLINE_CURVE_WITH_KNOTS('',3,(#79587,#79588,#79589,#79590,#79591,
#79592,#79593,#79594,#79595,#79596,#79597,#79598,#79599,#79600,#79601,#79602,
#79603,#79604,#79605,#79606,#79607,#79608,#79609,#79610,#79611,#79612,#79613,
#79614,#79615,#79616,#79617,#79618,#79619,#79620,#79621,#79622,#79623,#79624,
#79625,#79626,#79627,#79628,#79629,#79630,#79631,#79632,#79633,#79634,#79635,
#79636,#79637,#79638,#79639,#79640,#79641,#79642,#79643,#79644,#79645,#79646,
#79647,#79648,#79649,#79650,#79651,#79652,#79653,#79654,#79655,#79656,#79657,
#79658,#79659,#79660,#79661,#79662,#79663,#79664,#79665,#79666,#79667,#79668,
#79669,#79670,#79671,#79672,#79673,#79674,#79675,#79676,#79677,#79678,#79679,
#79680,#79681,#79682,#79683,#79684,#79685,#79686,#79687,#79688,#79689,#79690,
#79691,#79692,#79693,#79694,#79695,#79696,#79697,#79698,#79699,#79700,#79701,
#79702,#79703,#79704,#79705,#79706,#79707,#79708,#79709,#79710,#79711,#79712,
#79713,#79714,#79715,#79716,#79717,#79718,#79719,#79720,#79721,#79722,#79723,
#79724,#79725,#79726,#79727,#79728,#79729,#79730,#79731,#79732,#79733,#79734,
#79735,#79736,#79737,#79738,#79739,#79740,#79741,#79742,#79743,#79744,#79745,
#79746,#79747,#79748,#79749,#79750,#79751,#79752,#79753,#79754,#79755,#79756,
#79757,#79758,#79759,#79760,#79761,#79762,#79763,#79764,#79765,#79766,#79767,
#79768,#79769,#79770,#79771,#79772,#79773,#79774,#79775,#79776,#79777,#79778,
#79779,#79780,#79781,#79782),.UNSPECIFIED.,.F.,.F.,(4,2,2,2,2,2,2,2,2,2,
2,2,2,2,2,2,2,2,2,2,2,2,2,2,2,2,2,2,2,2,2,2,2,2,2,2,2,2,2,2,2,2,2,2,2,2,
2,2,2,2,2,2,2,2,2,2,2,2,2,2,2,2,2,2,2,2,2,2,2,2,2,2,2,2,2,2,2,2,2,2,2,2,
2,2,2,2,2,2,2,2,2,2,2,2,2,2,2,4),(-1.33767722568999,-1.32758777835359,-1.32303141189846,
-1.31960689481019,-1.31589682880466,-1.30985261830067,-1.28200486595905,
-1.25889484858637,-1.2479638977264,-1.24477060909482,-1.24274369745994,
-1.24095924370782,-1.23798994641985,-1.22984828668527,-1.19862340166705,
-1.18299694366057,-1.17239746123665,-1.16783636691018,-1.16441114532542,
-1.16070304138677,-1.15466831111083,-1.12822432422046,-1.10839672328695,
-1.09335746220029,-1.089862024917,-1.08776969451602,-1.08581776867339,-1.08337029254853,
-1.07706421998885,-1.04792697751804,-1.02948176853583,-1.01766536794776,
-1.01292130677384,-1.00946746300486,-1.00582766322246,-1.0001210976762,
-0.980514545331224,-0.96197577279904,-0.940414488641052,-0.935599294137241,
-0.93323466224333,-0.931325724820888,-0.928887069720718,-0.923678001038157,
-0.916379871327629,-0.893895414815347,-0.867479001548879,-0.860936771001032,
-0.856755471721608,-0.853371001053217,-0.84944467137143,-0.842357015678196,
-0.818278089212355,-0.791649530879589,-0.78223812635065,-0.779108791531489,
-0.777294729088857,-0.775303450714145,-0.772280983307875,-0.76302829228506,
-0.74593035437169,-0.711772565981,-0.70487778738906,-0.700951198169582,
-0.697566705836158,-0.693385641202473,-0.684994395317839,-0.665838028072912,
-0.633685399221897,-0.626409251452694,-0.623559327457625,-0.621620302616725,
-0.619502848649844,-0.615891682982514,-0.598524199894345,-0.560768142117848,
-0.551129245076641,-0.546772689462995,-0.543364963454298,-0.539595914197941,
-0.533269818437004,-0.525557076908771,-0.508439917774552,-0.482781675156979,
-0.47207557040729,-0.468808028733748,-0.466765084395115,-0.46475404720377,
-0.461635447271984,-0.451477651476305,-0.431351458565568,-0.401730227951145,
-0.395240924444836,-0.391075019245416,-0.387691454355756,-0.383753196137418,
-0.376606514099715,-0.357534662796563),.UNSPECIFIED.);
#931=B_SPLINE_CURVE_WITH_KNOTS('',3,(#79788,#79789,#79790,#79791,#79792,
#79793,#79794,#79795,#79796,#79797,#79798,#79799,#79800,#79801,#79802,#79803,
#79804,#79805,#79806,#79807,#79808,#79809,#79810,#79811,#79812,#79813,#79814,
#79815,#79816,#79817,#79818,#79819,#79820,#79821,#79822,#79823,#79824,#79825,
#79826,#79827,#79828,#79829,#79830,#79831,#79832,#79833,#79834,#79835,#79836,
#79837,#79838,#79839,#79840,#79841,#79842,#79843,#79844,#79845,#79846,#79847,
#79848,#79849,#79850,#79851),.UNSPECIFIED.,.F.,.F.,(4,3,3,3,3,3,3,3,3,3,
3,3,3,3,3,3,3,3,3,3,3,4),(53.4070751110264,53.60487683556,53.8026307996998,
54.000871365885,54.0780475015505,54.2766587546226,54.4757421401524,54.6739000325629,
54.8734461646525,55.072992296742,55.271603549814,55.4706869353439,55.6688448277544,
55.868390959844,56.0679370919336,56.2665483450057,56.4656317305355,56.663789622946,
56.8633357550356,57.0628818871251,57.2615016254264,57.4018228384941),
 .UNSPECIFIED.);
#932=B_SPLINE_CURVE_WITH_KNOTS('',3,(#79852,#79853,#79854,#79855,#79856,
#79857,#79858,#79859,#79860,#79861,#79862,#79863,#79864,#79865,#79866,#79867,
#79868,#79869,#79870,#79871,#79872,#79873,#79874,#79875,#79876,#79877,#79878,
#79879,#79880,#79881,#79882,#79883,#79884,#79885,#79886,#79887,#79888),
 .UNSPECIFIED.,.F.,.F.,(4,3,3,3,3,3,3,3,3,3,3,3,4),(51.1183439304616,51.316887193595,
51.5152054837938,51.7133542196496,51.9119926666512,52.0881579111674,52.2867691642395,
52.4858525497693,52.6840104421798,52.8835565742693,53.0831027063589,53.3166318695731,
53.4070751106813),.UNSPECIFIED.);
#933=B_SPLINE_CURVE_WITH_KNOTS('',3,(#79890,#79891,#79892,#79893,#79894,
#79895,#79896,#79897,#79898,#79899,#79900,#79901,#79902,#79903,#79904,#79905,
#79906,#79907,#79908,#79909,#79910,#79911,#79912,#79913,#79914,#79915,#79916,
#79917,#79918,#79919,#79920,#79921,#79922,#79923,#79924,#79925,#79926,#79927,
#79928,#79929,#79930,#79931,#79932,#79933,#79934,#79935,#79936,#79937,#79938,
#79939,#79940,#79941,#79942,#79943,#79944,#79945,#79946,#79947,#79948,#79949,
#79950,#79951,#79952,#79953,#79954,#79955,#79956,#79957,#79958,#79959,#79960,
#79961,#79962,#79963),.UNSPECIFIED.,.F.,.F.,(4,2,2,2,2,2,2,2,2,2,2,2,2,
2,2,2,2,2,2,2,2,2,2,2,2,2,2,2,2,2,2,2,2,2,2,2,4),(-0.357534662796563,-0.352061828879747,
-0.324498669175415,-0.316274119770007,-0.313293541342923,-0.311507040490122,
-0.3094829386353,-0.306303005978516,-0.295515099266277,-0.272988406159206,
-0.246636203584961,-0.240088643261087,-0.235905779400237,-0.232521189203807,
-0.228596001578112,-0.221514077821605,-0.197480187724382,-0.170941112393686,
-0.161412833877342,-0.158269898576684,-0.156453226423311,-0.154464468402554,
-0.151454605303766,-0.142313863550418,-0.125561751627027,-0.0908133378192396,
-0.083976867451929,-0.0800628176783954,-0.0766773044227989,-0.0724797197577981,
-0.0639999283873764,-0.0425180059851325,-0.0086660516945617,-0.00422403248952863,
-0.00211299992500007,-0.00103772143207282,-0.000454279888563791),
 .UNSPECIFIED.);
#934=B_SPLINE_CURVE_WITH_KNOTS('',3,(#79964,#79965,#79966,#79967,#79968,
#79969,#79970,#79971,#79972,#79973,#79974,#79975,#79976,#79977,#79978,#79979,
#79980,#79981,#79982,#79983,#79984,#79985,#79986,#79987,#79988,#79989,#79990,
#79991,#79992,#79993,#79994,#79995,#79996,#79997,#79998,#79999,#80000,#80001,
#80002,#80003,#80004,#80005,#80006,#80007,#80008,#80009,#80010,#80011,#80012,
#80013,#80014,#80015,#80016,#80017,#80018,#80019,#80020,#80021,#80022,#80023,
#80024,#80025,#80026,#80027,#80028,#80029,#80030,#80031,#80032,#80033,#80034,
#80035,#80036,#80037,#80038,#80039,#80040,#80041,#80042,#80043,#80044,#80045,
#80046,#80047,#80048,#80049,#80050,#80051,#80052,#80053,#80054,#80055,#80056,
#80057,#80058,#80059,#80060,#80061,#80062,#80063,#80064,#80065,#80066,#80067,
#80068,#80069,#80070,#80071,#80072,#80073,#80074,#80075,#80076,#80077,#80078,
#80079,#80080,#80081,#80082,#80083,#80084,#80085,#80086,#80087,#80088,#80089),
 .UNSPECIFIED.,.F.,.F.,(4,2,2,2,2,2,2,2,2,2,2,2,2,2,2,2,2,2,2,2,2,2,2,2,
2,2,2,2,2,2,2,2,2,2,2,2,2,2,2,2,2,2,2,2,2,2,2,2,2,2,2,2,2,2,2,2,2,2,2,2,
2,2,4),(-1.96085464133602,-1.95969799413353,-1.95743610396883,-1.95136541439688,
-1.92040753629392,-1.89819815000253,-1.88995811661379,-1.88580586328573,
-1.88242331915766,-1.87847486509316,-1.87147666912248,-1.83859073280341,
-1.82068973381756,-1.81118460161822,-1.80813445813614,-1.80613776241746,
-1.8043294845226,-1.8012297961438,-1.79206528041586,-1.7618730798397,-1.74321140454887,
-1.73483965017737,-1.73066261100245,-1.72727876573915,-1.72335000353586,
-1.71644366423225,-1.68238854497493,-1.66521092016379,-1.65593327085967,
-1.65290818501971,-1.65091656906165,-1.64910334223822,-1.64597760466422,
-1.63659397407287,-1.60996931413919,-1.58589774378847,-1.57881149071345,
-1.57488574142084,-1.57150163731259,-1.56732062158679,-1.56077843628138,
-1.53431396178902,-1.51184206421005,-1.50454535163472,-1.49933763829812,
-1.49689937938828,-1.49499064763575,-1.49262612752588,-1.48781073918378,
-1.46615109303773,-1.44741320562003,-1.43435348658196,-1.42499341976237,
-1.4206378635691,-1.41723895996088,-1.41342954093794,-1.40690902358106,
-1.36898803671565,-1.34877064913869,-1.34393436047819,-1.34156569697933,
-1.33984681549977,-1.33778719751885),.UNSPECIFIED.);
#935=B_SPLINE_CURVE_WITH_KNOTS('',3,(#80095,#80096,#80097,#80098,#80099,
#80100,#80101,#80102,#80103,#80104,#80105,#80106,#80107,#80108,#80109,#80110,
#80111,#80112,#80113,#80114,#80115,#80116,#80117,#80118,#80119,#80120,#80121,
#80122,#80123,#80124,#80125,#80126,#80127,#80128,#80129,#80130,#80131,#80132,
#80133,#80134,#80135,#80136,#80137,#80138,#80139,#80140,#80141,#80142,#80143,
#80144,#80145,#80146,#80147,#80148,#80149,#80150,#80151,#80152,#80153,#80154,
#80155,#80156,#80157,#80158),.UNSPECIFIED.,.F.,.F.,(4,3,3,3,3,3,3,3,3,3,
3,3,3,3,3,3,3,3,3,3,3,4),(59.6902604185821,59.9168207671643,60.0477162726997,
60.2463275257718,60.4454109113016,60.6435688037121,60.8431149358017,61.0426610678912,
61.241272320963,61.4403557064929,61.6385135989031,61.838059730993,62.0376058630828,
62.2362171161554,62.4353005016851,62.6334583940962,62.8330045261852,63.0325506582743,
63.2311657262726,63.4293532087799,63.6274455226886,63.6841456582349),
 .UNSPECIFIED.);
#936=B_SPLINE_CURVE_WITH_KNOTS('',3,(#80159,#80160,#80161,#80162,#80163,
#80164,#80165,#80166,#80167,#80168,#80169,#80170,#80171,#80172,#80173,#80174,
#80175,#80176,#80177,#80178,#80179,#80180,#80181,#80182,#80183,#80184,#80185,
#80186,#80187,#80188,#80189,#80190,#80191,#80192,#80193,#80194,#80195,#80196,
#80197,#80198),.UNSPECIFIED.,.F.,.F.,(4,3,3,3,3,3,3,3,3,3,3,3,3,4),(57.4018228384941,
57.6000162812558,57.7981657536071,57.9967750996259,58.0578266823166,58.2564379353886,
58.4555213209185,58.653679213329,58.8532253454186,59.0527714775082,59.2522974269614,
59.4513573899721,59.6502389193865,59.690260418206),.UNSPECIFIED.);
#937=B_SPLINE_CURVE_WITH_KNOTS('',3,(#80199,#80200,#80201,#80202,#80203,
#80204,#80205,#80206,#80207,#80208,#80209,#80210,#80211,#80212,#80213,#80214,
#80215,#80216,#80217,#80218,#80219,#80220,#80221,#80222,#80223,#80224,#80225,
#80226,#80227,#80228,#80229,#80230,#80231,#80232,#80233,#80234,#80235,#80236,
#80237,#80238,#80239,#80240,#80241,#80242,#80243,#80244,#80245,#80246,#80247,
#80248,#80249,#80250,#80251,#80252,#80253,#80254,#80255,#80256,#80257,#80258,
#80259,#80260,#80261,#80262,#80263,#80264,#80265,#80266,#80267,#80268,#80269,
#80270,#80271,#80272,#80273,#80274,#80275,#80276,#80277,#80278,#80279,#80280,
#80281,#80282,#80283,#80284,#80285,#80286,#80287,#80288,#80289,#80290,#80291,
#80292,#80293,#80294,#80295,#80296,#80297,#80298,#80299,#80300,#80301,#80302,
#80303,#80304,#80305,#80306,#80307,#80308,#80309,#80310,#80311,#80312,#80313,
#80314,#80315,#80316,#80317,#80318,#80319,#80320,#80321,#80322,#80323,#80324,
#80325,#80326,#80327,#80328,#80329,#80330,#80331,#80332,#80333,#80334,#80335,
#80336,#80337,#80338,#80339,#80340,#80341,#80342,#80343,#80344,#80345,#80346,
#80347,#80348,#80349,#80350,#80351,#80352,#80353,#80354,#80355,#80356,#80357,
#80358,#80359,#80360,#80361,#80362,#80363,#80364,#80365,#80366,#80367,#80368,
#80369,#80370,#80371,#80372,#80373,#80374,#80375,#80376,#80377,#80378,#80379,
#80380,#80381,#80382,#80383,#80384,#80385,#80386,#80387,#80388,#80389,#80390),
 .UNSPECIFIED.,.F.,.F.,(4,2,2,2,2,2,2,2,2,2,2,2,2,2,2,2,2,2,2,2,2,2,2,2,
2,2,2,2,2,2,2,2,2,2,2,2,2,2,2,2,2,2,2,2,2,2,2,2,2,2,2,2,2,2,2,2,2,2,2,2,
2,2,2,2,2,2,2,2,2,2,2,2,2,2,2,2,2,2,2,2,2,2,2,2,2,2,2,2,2,2,2,2,2,2,2,4),
(-1.33778719751885,-1.33751221745128,-1.33299621567242,-1.30464861401804,
-1.27749033601146,-1.26919469364743,-1.26503172412641,-1.26164837235187,
-1.25770791599161,-1.25074805823796,-1.21731603656382,-1.19975554880528,
-1.19035618530923,-1.187317437687,-1.1853229416187,-1.18351223618444,-1.18040029179032,
-1.17113481752426,-1.14441608402247,-1.12029635960102,-1.11320362196044,
-1.10927635227059,-1.10589206099999,-1.10171225452133,-1.09517488784827,
-1.06863332557585,-1.04620953932327,-1.03892047779849,-1.03371667406926,
-1.03127901133978,-1.02937014559124,-1.0270047120971,-1.02218518799183,
-1.0001975563674,-0.980868736069392,-0.962327044704108,-0.956718033819915,
-0.953098403216103,-0.949633816287525,-0.9448261467839,-0.932557469639629,
-0.912970084656786,-0.882492446579291,-0.878124913519015,-0.875821504477149,
-0.873908638244104,-0.871395435592714,-0.865769678650637,-0.857661050152863,
-0.829582926953075,-0.80760515716153,-0.80175517977091,-0.798085498906799,
-0.794645301848536,-0.789986232540218,-0.778751472055754,-0.761694217390857,
-0.736186915923587,-0.725269080691368,-0.721982143950538,-0.719934925976592,
-0.717927345570818,-0.714825618514982,-0.704834755305202,-0.685301868483314,
-0.654847463860384,-0.648374947689261,-0.644213790441317,-0.64083028904122,
-0.636887828407406,-0.629721089012569,-0.605018364310719,-0.577135759114778,
-0.569301444026419,-0.566374195312102,-0.564421104361875,-0.562330412970304,
-0.558843043965974,-0.543942320337303,-0.524061475833301,-0.497570131108314,
-0.491525515830468,-0.487815162631819,-0.484390336839105,-0.479833502674628,
-0.469262855973516,-0.453698106628933,-0.422903971952484,-0.414312407371696,
-0.41128352262908,-0.409488188760745,-0.407475666834736,-0.404350639104759,
-0.394130897914863,-0.373782171446824,-0.357647925279928),.UNSPECIFIED.);
#938=B_SPLINE_CURVE_WITH_KNOTS('',3,(#80396,#80397,#80398,#80399,#80400,
#80401,#80402,#80403,#80404,#80405,#80406,#80407,#80408,#80409,#80410,#80411,
#80412,#80413,#80414,#80415,#80416,#80417,#80418,#80419,#80420,#80421,#80422,
#80423,#80424,#80425,#80426,#80427,#80428,#80429,#80430,#80431,#80432,#80433,
#80434,#80435,#80436,#80437,#80438,#80439,#80440,#80441,#80442,#80443,#80444,
#80445,#80446,#80447,#80448,#80449,#80450,#80451,#80452,#80453,#80454,#80455,
#80456,#80457,#80458,#80459),.UNSPECIFIED.,.F.,.F.,(4,3,3,3,3,3,3,3,3,3,
3,3,3,3,3,3,3,3,3,3,3,4),(65.9734457253856,66.0173850438489,66.2159962969183,
66.4150796824488,66.6132375748568,66.8127837069487,67.0123298390405,67.210941092103,
67.4100244776353,67.6081823700362,67.8077285021341,68.007274634232,68.2058858873335,
68.404969272856,68.6031271652955,68.8026732973595,69.0022194294236,69.2008324314782,
69.3991652159293,69.5972999332797,69.7958687306036,69.9675922406437),
 .UNSPECIFIED.);
#939=B_SPLINE_CURVE_WITH_KNOTS('',3,(#80460,#80461,#80462,#80463,#80464,
#80465,#80466,#80467,#80468,#80469,#80470,#80471,#80472,#80473,#80474,#80475,
#80476,#80477,#80478,#80479,#80480,#80481,#80482,#80483,#80484,#80485,#80486,
#80487,#80488,#80489,#80490,#80491,#80492,#80493,#80494,#80495,#80496),
 .UNSPECIFIED.,.F.,.F.,(4,3,3,3,3,3,3,3,3,3,3,3,4),(63.6841456582349,63.8827672257363,
64.0274954534659,64.2261067065363,64.4251900920666,64.6233479844754,64.8228941165664,
65.0224402486574,65.2196936990435,65.4166824879541,65.6134849313515,65.8107437883567,
65.973445725034),.UNSPECIFIED.);
#940=B_SPLINE_CURVE_WITH_KNOTS('',3,(#80498,#80499,#80500,#80501,#80502,
#80503,#80504,#80505,#80506,#80507,#80508,#80509,#80510,#80511,#80512,#80513,
#80514,#80515,#80516,#80517,#80518,#80519,#80520,#80521,#80522,#80523,#80524,
#80525,#80526,#80527,#80528,#80529,#80530,#80531,#80532,#80533,#80534,#80535,
#80536,#80537,#80538,#80539,#80540,#80541,#80542,#80543,#80544,#80545,#80546,
#80547,#80548,#80549,#80550,#80551,#80552,#80553,#80554,#80555,#80556,#80557,
#80558,#80559,#80560,#80561,#80562,#80563,#80564,#80565,#80566,#80567,#80568,
#80569,#80570,#80571,#80572,#80573),.UNSPECIFIED.,.F.,.F.,(4,2,2,2,2,2,
2,2,2,2,2,2,2,2,2,2,2,2,2,2,2,2,2,2,2,2,2,2,2,2,2,2,2,2,2,2,2,4),(-0.357647925279928,
-0.34446326816879,-0.33796778868358,-0.333799866922246,-0.330415886590131,
-0.326478519861799,-0.319337440272169,-0.294840394575903,-0.267375679006825,
-0.259024642703012,-0.256027048405568,-0.254237370812583,-0.252217280794945,
-0.24905671709191,-0.238475133453672,-0.21676731689736,-0.189279745222121,
-0.18276485676467,-0.178591240326989,-0.175206867602713,-0.171273793452703,
-0.164154219425701,-0.139828126827636,-0.112708213190028,-0.10392262960473,
-0.100868987359338,-0.0990690282240539,-0.0970619704908127,-0.093963339168338,
-0.0840043631129348,-0.0531050154374437,-0.0314392653121238,-0.0256302262713167,
-0.0219688461200183,-0.0187254011670891,-0.0153699123580542,-0.00916901388829356,
-0.000453918773602445),.UNSPECIFIED.);
#941=B_SPLINE_CURVE_WITH_KNOTS('',3,(#80574,#80575,#80576,#80577,#80578,
#80579,#80580,#80581,#80582,#80583,#80584,#80585,#80586,#80587,#80588,#80589,
#80590,#80591,#80592,#80593,#80594,#80595,#80596,#80597,#80598,#80599,#80600,
#80601,#80602,#80603,#80604,#80605,#80606,#80607,#80608,#80609,#80610,#80611,
#80612,#80613,#80614,#80615,#80616,#80617,#80618,#80619,#80620,#80621,#80622,
#80623,#80624,#80625,#80626,#80627,#80628,#80629,#80630,#80631,#80632,#80633,
#80634,#80635,#80636,#80637,#80638,#80639,#80640,#80641,#80642,#80643,#80644,
#80645,#80646,#80647,#80648,#80649,#80650,#80651,#80652,#80653,#80654,#80655,
#80656,#80657,#80658,#80659,#80660,#80661,#80662,#80663,#80664,#80665,#80666,
#80667,#80668,#80669,#80670,#80671,#80672,#80673,#80674,#80675,#80676,#80677,
#80678,#80679,#80680,#80681,#80682,#80683,#80684,#80685,#80686,#80687,#80688,
#80689,#80690,#80691,#80692,#80693,#80694,#80695,#80696,#80697,#80698,#80699,
#80700,#80701,#80702,#80703,#80704,#80705,#80706,#80707,#80708,#80709,#80710,
#80711,#80712,#80713,#80714,#80715,#80716,#80717),.UNSPECIFIED.,.F.,.F.,
(4,2,2,2,2,2,2,2,2,2,2,2,2,2,2,2,2,2,2,2,2,2,2,2,2,2,2,2,2,2,2,2,2,2,2,
2,2,2,2,2,2,2,2,2,2,2,2,2,2,2,2,2,2,2,2,2,2,2,2,2,2,2,2,2,2,2,2,2,2,2,2,
4),(-1.96070394248481,-1.92933497661198,-1.91166965002557,-1.90711115802255,
-1.90479663559414,-1.90288477673997,-1.90042780996585,-1.89497254781089,
-1.86064015508601,-1.84455014458124,-1.83712307143501,-1.83108918642525,
-1.830844570577,-1.83060683710871,-1.83037264552342,-1.83013861566442,-1.82990113197663,
-1.82965609209598,-1.82939855324977,-1.82912219347787,-1.82881842813478,
-1.82864790734816,-1.82820317743472,-1.82502933496934,-1.82110692176938,
-1.81423173783217,-1.77988936358417,-1.76286992464413,-1.75364254252336,
-1.75062279968158,-1.74863206018267,-1.74681739760326,-1.74368505697505,
-1.73424749517593,-1.70765945710643,-1.68360477817426,-1.67652010598994,
-1.67259431692131,-1.66920968157123,-1.66502737182054,-1.6584818650549,
-1.63204390313268,-1.60954879192493,-1.60224773093705,-1.59703753317579,
-1.59459860323716,-1.59268958544777,-1.59032500857371,-1.58551040970868,
-1.56394268442181,-1.54538465953001,-1.53216356351257,-1.52272129385147,
-1.51835109220562,-1.5149501691811,-1.51114817892382,-1.50466508386144,
-1.46647073413673,-1.44641973752589,-1.44160023140202,-1.43923458101903,
-1.43751559759742,-1.43517749651291,-1.4304999968888,-1.39570889877599,
-1.37916181007943,-1.36814838523904,-1.36352266638425,-1.36008745121614,
-1.35640476373227,-1.35049328168514,-1.33764393648806),.UNSPECIFIED.);
#942=B_SPLINE_CURVE_WITH_KNOTS('',3,(#80723,#80724,#80725,#80726,#80727,
#80728,#80729,#80730,#80731,#80732,#80733,#80734,#80735,#80736,#80737,#80738,
#80739,#80740,#80741,#80742,#80743,#80744,#80745,#80746,#80747,#80748,#80749,
#80750,#80751,#80752,#80753,#80754,#80755,#80756,#80757,#80758,#80759,#80760,
#80761,#80762,#80763,#80764,#80765,#80766,#80767,#80768,#80769,#80770,#80771,
#80772,#80773,#80774,#80775,#80776,#80777,#80778,#80779,#80780,#80781,#80782,
#80783,#80784,#80785,#80786),.UNSPECIFIED.,.F.,.F.,(4,3,3,3,3,3,3,3,3,3,
3,3,3,3,3,3,3,3,3,3,3,4),(72.2566310325652,72.453061509527,72.6493422534457,
72.8460888556948,72.9819986101897,73.1806098630103,73.379693248603,73.5778511407525,
73.7773972730668,73.9769434053812,74.1755546598248,74.3746380450118,74.5727959387811,
74.772342069677,74.9718882005728,75.1704994517123,75.3695828377253,75.5677407282643,
75.7672868620143,75.9668329957643,76.1654410178161,76.2514750095923),
 .UNSPECIFIED.);
#943=B_SPLINE_CURVE_WITH_KNOTS('',3,(#80787,#80788,#80789,#80790,#80791,
#80792,#80793,#80794,#80795,#80796,#80797,#80798,#80799,#80800,#80801,#80802,
#80803,#80804,#80805,#80806,#80807,#80808,#80809,#80810,#80811,#80812,#80813,
#80814,#80815,#80816,#80817,#80818,#80819,#80820,#80821,#80822,#80823,#80824,
#80825,#80826),.UNSPECIFIED.,.F.,.F.,(4,3,3,3,3,3,3,3,3,3,3,3,3,4),(69.9675922406437,
69.9971642246151,70.1957754776355,70.3948588631782,70.593016755536,70.7925628876713,
70.9921090198066,71.1907202730821,71.3898036585611,71.5879615511726,71.7875076830854,
71.9870538149982,72.2359502938216,72.2566310322155),.UNSPECIFIED.);
#944=B_SPLINE_CURVE_WITH_KNOTS('',3,(#80827,#80828,#80829,#80830,#80831,
#80832,#80833,#80834,#80835,#80836,#80837,#80838,#80839,#80840,#80841,#80842,
#80843,#80844,#80845,#80846,#80847,#80848,#80849,#80850,#80851,#80852,#80853,
#80854,#80855,#80856,#80857,#80858,#80859,#80860,#80861,#80862,#80863,#80864,
#80865,#80866,#80867,#80868,#80869,#80870,#80871,#80872,#80873,#80874,#80875,
#80876,#80877,#80878,#80879,#80880,#80881,#80882,#80883,#80884,#80885,#80886,
#80887,#80888,#80889,#80890,#80891,#80892,#80893,#80894,#80895,#80896,#80897,
#80898,#80899,#80900,#80901,#80902,#80903,#80904,#80905,#80906,#80907,#80908,
#80909,#80910,#80911,#80912,#80913,#80914,#80915,#80916,#80917,#80918,#80919,
#80920,#80921,#80922,#80923,#80924,#80925,#80926,#80927,#80928,#80929,#80930,
#80931,#80932,#80933,#80934,#80935,#80936,#80937,#80938,#80939,#80940,#80941,
#80942,#80943,#80944,#80945,#80946,#80947,#80948,#80949,#80950,#80951,#80952,
#80953,#80954,#80955,#80956,#80957,#80958,#80959,#80960,#80961,#80962,#80963,
#80964,#80965,#80966,#80967,#80968,#80969,#80970,#80971,#80972,#80973,#80974,
#80975,#80976,#80977,#80978,#80979,#80980,#80981,#80982,#80983,#80984,#80985,
#80986,#80987,#80988,#80989,#80990,#80991,#80992,#80993,#80994,#80995,#80996,
#80997,#80998,#80999,#81000,#81001,#81002,#81003,#81004,#81005,#81006,#81007,
#81008,#81009,#81010,#81011,#81012),.UNSPECIFIED.,.F.,.F.,(4,2,2,2,2,2,
2,2,2,2,2,2,2,2,2,2,2,2,2,2,2,2,2,2,2,2,2,2,2,2,2,2,2,2,2,2,2,2,2,2,2,2,
2,2,2,2,2,2,2,2,2,2,2,2,2,2,2,2,2,2,2,2,2,2,2,2,2,2,2,2,2,2,2,2,2,2,2,2,
2,2,2,2,2,2,2,2,2,2,2,2,2,2,4),(-1.33764393648806,-1.32659078915027,-1.30533210274314,
-1.28905713672738,-1.28549559930562,-1.2833887772993,-1.28144427872074,
-1.27902714312095,-1.27291844346281,-1.24359623341503,-1.21958569955851,
-1.21150514551954,-1.2073825602272,-1.204328930668,-1.20047835292542,-1.19393580256984,
-1.15671053439527,-1.13603744734816,-1.13115414686181,-1.12877618766843,
-1.12705652003219,-1.12472958073054,-1.12010936254975,-1.0922176721032,
-1.06093976508601,-1.05480389243963,-1.05107419399002,-1.04765506714192,
-1.04321785182638,-1.03309270536602,-0.999032385775235,-0.980434221343209,
-0.975770041141681,-0.973434445539726,-0.97171519949576,-0.969346528418303,
-0.964511847067524,-0.944315365601489,-0.906384348460499,-0.899866903221876,
-0.896057567158741,-0.892657694546348,-0.888299452911519,-0.878927844766484,
-0.865844975839041,-0.847103500686982,-0.825432853771757,-0.820615263050581,
-0.818249962230202,-0.816340759208371,-0.81390211377172,-0.808694265744745,
-0.801398835773369,-0.778933909603497,-0.752479200204457,-0.745938637483802,
-0.741757491251353,-0.738372575491306,-0.734445093587934,-0.727353533703111,
-0.703248611653748,-0.676571474066634,-0.667216739693597,-0.664093764547102,
-0.66228073727372,-0.660287871163014,-0.657258529329938,-0.647946832937712,
-0.6306660697191,-0.596804025816962,-0.589881042019555,-0.585948034885406,
-0.582563473020931,-0.578389310060931,-0.570036953811306,-0.552118977504699,
-0.546085025841321,-0.516057029883534,-0.510522080404953,-0.508050958350324,
-0.506137845802918,-0.503833910757756,-0.499329667921236,-0.482133399455728,
-0.441382183921242,-0.434548845941095,-0.430635280611452,-0.42724943539701,
-0.423050467938173,-0.414564336920297,-0.392952636386033,-0.366603901696779,
-0.35724220641513),.UNSPECIFIED.);
#945=B_SPLINE_CURVE_WITH_KNOTS('',3,(#81018,#81019,#81020,#81021,#81022,
#81023,#81024,#81025,#81026,#81027,#81028,#81029,#81030,#81031,#81032,#81033,
#81034,#81035,#81036,#81037,#81038,#81039,#81040,#81041,#81042,#81043,#81044,
#81045,#81046,#81047,#81048,#81049,#81050,#81051,#81052,#81053,#81054,#81055,
#81056,#81057,#81058,#81059,#81060,#81061,#81062,#81063,#81064,#81065,#81066,
#81067,#81068,#81069,#81070,#81071,#81072,#81073,#81074,#81075,#81076,#81077,
#81078),.UNSPECIFIED.,.F.,.F.,(4,3,3,3,3,3,3,3,3,3,3,3,3,3,3,3,3,3,3,3,
4),(78.5398163403645,78.7576486565568,78.951667381339,79.1502786332354,
79.3493620190592,79.5475199096511,79.7470660430908,79.9466121765305,80.1452234870737,
80.3443068582357,80.5424648079831,80.7420108898526,80.941556971722,81.1401681098791,
81.3392515241377,81.5374093042427,81.7369555355781,81.9365017669136,82.1351109303009,
82.334472825171,82.533834720041),.UNSPECIFIED.);
#946=B_SPLINE_CURVE_WITH_KNOTS('',3,(#81079,#81080,#81081,#81082,#81083,
#81084,#81085,#81086,#81087,#81088,#81089,#81090,#81091,#81092,#81093,#81094,
#81095,#81096,#81097,#81098,#81099,#81100,#81101,#81102,#81103,#81104,#81105,
#81106,#81107,#81108,#81109,#81110,#81111,#81112,#81113,#81114,#81115),
 .UNSPECIFIED.,.F.,.F.,(4,3,3,3,3,3,3,3,3,3,3,3,4),(76.2514750095923,76.4497181715849,
76.647858216347,76.8464700708751,76.9617777909559,77.160389053035,77.3594724363131,
77.5576303376766,77.757176461912,77.9567225861474,78.1589910006078,78.360779972492,
78.5398163397448),.UNSPECIFIED.);
#947=B_SPLINE_CURVE_WITH_KNOTS('',3,(#81117,#81118,#81119,#81120,#81121,
#81122,#81123,#81124,#81125,#81126,#81127,#81128,#81129,#81130,#81131,#81132,
#81133,#81134,#81135,#81136,#81137,#81138,#81139,#81140,#81141,#81142,#81143,
#81144,#81145,#81146,#81147,#81148,#81149,#81150,#81151,#81152,#81153,#81154,
#81155,#81156,#81157,#81158,#81159,#81160,#81161,#81162,#81163,#81164,#81165,
#81166,#81167,#81168,#81169,#81170,#81171,#81172,#81173,#81174,#81175,#81176,
#81177,#81178,#81179,#81180,#81181,#81182,#81183,#81184,#81185,#81186,#81187,
#81188,#81189,#81190,#81191,#81192,#81193,#81194,#81195,#81196,#81197,#81198,
#81199,#81200,#81201,#81202,#81203,#81204),.UNSPECIFIED.,.F.,.F.,(4,2,2,
2,2,2,2,2,2,2,2,2,2,2,2,2,2,2,2,2,2,2,2,2,2,2,2,2,2,2,2,2,2,2,2,2,2,2,2,
2,2,2,2,4),(-0.35724220641513,-0.356822408920814,-0.353650496406972,-0.3518281511151,
-0.349844379338791,-0.346860167994689,-0.337943880317512,-0.321868961818697,
-0.285909469762527,-0.279209178812092,-0.275324385738072,-0.271968054207344,
-0.267745605652009,-0.259132422140335,-0.235607204093075,-0.205624844051143,
-0.200044979049397,-0.197566145235043,-0.195652521087392,-0.193354747262324,
-0.188880964176308,-0.157624336541427,-0.129180683138258,-0.123199353091418,
-0.119502124419729,-0.116072497057409,-0.115798552356404,-0.115546404610803,
-0.1153097713868,-0.115083828284873,-0.114864686845464,-0.114649053761756,
-0.114433994481021,-0.114216757482325,-0.108301119632023,-0.0877394866270328,
-0.0619269363182737,-0.0471301183757394,-0.0435555235041537,-0.0414458869549523,
-0.0394800878424068,-0.0365897386922399,-0.0332164226697334,-0.000252836880366436),
 .UNSPECIFIED.);
#948=B_SPLINE_CURVE_WITH_KNOTS('',3,(#81205,#81206,#81207,#81208,#81209,
#81210,#81211,#81212,#81213,#81214,#81215,#81216,#81217,#81218,#81219,#81220,
#81221,#81222,#81223,#81224,#81225,#81226,#81227,#81228,#81229,#81230,#81231,
#81232,#81233,#81234,#81235,#81236,#81237,#81238,#81239,#81240,#81241,#81242,
#81243,#81244,#81245,#81246,#81247,#81248,#81249,#81250,#81251,#81252,#81253,
#81254,#81255,#81256,#81257,#81258,#81259,#81260,#81261,#81262,#81263,#81264,
#81265,#81266,#81267,#81268,#81269,#81270,#81271,#81272,#81273,#81274,#81275,
#81276,#81277,#81278,#81279,#81280,#81281,#81282,#81283,#81284,#81285,#81286,
#81287,#81288,#81289,#81290,#81291,#81292,#81293,#81294,#81295,#81296,#81297,
#81298,#81299,#81300,#81301,#81302,#81303,#81304,#81305,#81306,#81307,#81308,
#81309,#81310,#81311,#81312,#81313,#81314,#81315,#81316,#81317,#81318,#81319,
#81320,#81321,#81322,#81323,#81324,#81325,#81326,#81327,#81328),
 .UNSPECIFIED.,.F.,.F.,(4,2,2,2,2,2,2,2,2,2,2,2,2,2,2,2,2,2,2,2,2,2,2,2,
2,2,2,2,2,2,2,2,2,2,2,2,2,2,2,2,2,2,2,2,2,2,2,2,2,2,2,2,2,2,2,2,2,2,2,2,
2,4),(-1.96097123673854,-1.93544878824503,-1.9307836078925,-1.92734818430412,
-1.92388135748319,-1.92069499585623,-1.91548164960046,-1.90109442939945,
-1.865759950493,-1.85552578794693,-1.85022311985131,-1.84774122912439,-1.8458479462265,
-1.84352848164422,-1.8389454120148,-1.80368554852454,-1.78733620019686,
-1.77641042110183,-1.77179826467768,-1.7683652435406,-1.76467751706006,
-1.75874133784427,-1.73365165564656,-1.70819814799854,-1.70044158786916,
-1.69499498755983,-1.69251328204544,-1.69062004338693,-1.68830051147821,
-1.68371696872555,-1.64843377421369,-1.63210007874355,-1.62118132453413,
-1.61657030320878,-1.61313750516251,-1.60944943405163,-1.60351138407857,
-1.5783449692973,-1.55295665930332,-1.54520954754212,-1.53976781837696,
-1.53728700949584,-1.53539386058388,-1.53307369614114,-1.52848681416989,
-1.49322206834498,-1.4768811387022,-1.46595924005697,-1.46134779237403,
-1.457914983222,-1.45422718802596,-1.44829023075563,-1.42316176599186,-1.39774250440246,
-1.38999101924419,-1.38454707648446,-1.38206590265396,-1.38017276496632,
-1.37785297666854,-1.37326785735491,-1.33799504523619,-1.33764837993426),
 .UNSPECIFIED.);
#949=B_SPLINE_CURVE_WITH_KNOTS('',3,(#81334,#81335,#81336,#81337,#81338,
#81339,#81340,#81341,#81342,#81343,#81344,#81345,#81346,#81347,#81348,#81349,
#81350,#81351,#81352,#81353,#81354,#81355,#81356,#81357,#81358,#81359,#81360,
#81361,#81362,#81363,#81364,#81365,#81366,#81367,#81368,#81369,#81370,#81371,
#81372,#81373,#81374,#81375,#81376,#81377,#81378,#81379,#81380,#81381,#81382,
#81383,#81384,#81385,#81386,#81387,#81388,#81389,#81390,#81391,#81392,#81393,
#81394,#81395,#81396,#81397),.UNSPECIFIED.,.F.,.F.,(4,3,3,3,3,3,3,3,3,3,
3,3,3,3,3,3,3,3,3,3,3,4),(84.8230016469244,84.9213361524882,85.1199478699099,
85.3190311393523,85.5171894595963,85.716735203638,85.9162809476797,86.1148942966719,
86.3139771582217,86.5121371632032,86.7116814530373,86.9112257428713,87.1098309667632,
87.3089158595881,87.5070678206575,87.7066191793601,87.9061705380628,88.1047926557453,
88.303092888702,88.5011927562955,88.699619191771,88.8169224278005),
 .UNSPECIFIED.);
#950=B_SPLINE_CURVE_WITH_KNOTS('',3,(#81398,#81399,#81400,#81401,#81402,
#81403,#81404,#81405,#81406,#81407,#81408,#81409,#81410,#81411,#81412,#81413,
#81414,#81415,#81416,#81417,#81418,#81419,#81420,#81421,#81422,#81423,#81424,
#81425,#81426,#81427,#81428,#81429,#81430,#81431,#81432,#81433,#81434),
 .UNSPECIFIED.,.F.,.F.,(4,3,3,3,3,3,3,3,3,3,3,3,4),(82.533834720041,82.732640641073,
82.9314465621051,83.1300581696947,83.3291414665952,83.5272997142751,83.7268455357858,
83.9263913572966,84.1225530095749,84.3184285456288,84.5141253382016,84.7102046185275,
84.8230016464018),.UNSPECIFIED.);
#951=B_SPLINE_CURVE_WITH_KNOTS('',3,(#81435,#81436,#81437,#81438,#81439,
#81440,#81441,#81442,#81443,#81444,#81445,#81446,#81447,#81448,#81449,#81450,
#81451,#81452,#81453,#81454,#81455,#81456,#81457,#81458,#81459,#81460,#81461,
#81462,#81463,#81464,#81465,#81466,#81467,#81468,#81469,#81470,#81471,#81472,
#81473,#81474,#81475,#81476,#81477,#81478,#81479,#81480,#81481,#81482,#81483,
#81484,#81485,#81486,#81487,#81488,#81489,#81490,#81491,#81492,#81493,#81494,
#81495,#81496,#81497,#81498,#81499,#81500,#81501,#81502,#81503,#81504,#81505,
#81506,#81507,#81508,#81509,#81510,#81511,#81512,#81513,#81514,#81515,#81516,
#81517,#81518,#81519,#81520,#81521,#81522,#81523,#81524,#81525,#81526,#81527,
#81528,#81529,#81530,#81531,#81532,#81533,#81534,#81535,#81536,#81537,#81538,
#81539,#81540,#81541,#81542,#81543,#81544,#81545,#81546,#81547,#81548,#81549,
#81550,#81551,#81552,#81553,#81554,#81555,#81556,#81557,#81558,#81559,#81560,
#81561,#81562,#81563,#81564,#81565,#81566,#81567,#81568,#81569,#81570,#81571,
#81572,#81573,#81574,#81575,#81576,#81577,#81578,#81579,#81580,#81581,#81582,
#81583,#81584,#81585,#81586,#81587,#81588,#81589,#81590,#81591,#81592,#81593,
#81594,#81595,#81596,#81597,#81598,#81599,#81600,#81601,#81602,#81603,#81604,
#81605,#81606,#81607,#81608,#81609,#81610,#81611,#81612,#81613,#81614,#81615,
#81616,#81617,#81618,#81619,#81620,#81621,#81622,#81623,#81624,#81625,#81626,
#81627,#81628,#81629,#81630),.UNSPECIFIED.,.F.,.F.,(4,2,2,2,2,2,2,2,2,2,
2,2,2,2,2,2,2,2,2,2,2,2,2,2,2,2,2,2,2,2,2,2,2,2,2,2,2,2,2,2,2,2,2,2,2,2,
2,2,2,2,2,2,2,2,2,2,2,2,2,2,2,2,2,2,2,2,2,2,2,2,2,2,2,2,2,2,2,2,2,2,2,2,
2,2,2,2,2,2,2,2,2,2,2,2,2,2,2,4),(-1.33764837993426,-1.32165810253604,-1.31073804337826,
-1.30612693446348,-1.30269422892397,-1.2990064054951,-1.29306908852945,
-1.26792279772655,-1.24627596486119,-1.23153357172201,-1.22805536621762,
-1.22596672666616,-1.22401255626506,-1.22155650316898,-1.21518196032515,
-1.18610221571187,-1.16083126561247,-1.15359433587048,-1.1496377758412,
-1.14625517243094,-1.14211152867885,-1.13569894365946,-1.10336918517922,
-1.08510125263788,-1.07548312239255,-1.07242048652656,-1.07042103974912,
-1.06836389702773,-1.06503111073197,-1.05358746507316,-1.02847935360512,
-1.00726130090864,-0.999027706381584,-0.994876273035988,-0.991493280153546,
-0.987543036962968,-0.980538232961267,-0.956451018629418,-0.929806678131979,
-0.92041441546276,-0.917287266944642,-0.915473588273764,-0.913481828396923,
-0.910457150452979,-0.90118517021443,-0.88402744118857,-0.849967606465764,
-0.843063428827941,-0.839134747891653,-0.835750304186665,-0.83157167268334,
-0.823193836926178,-0.804446510178452,-0.773948860844069,-0.765061632318366,
-0.761995393534293,-0.760193158739031,-0.75818895983127,-0.755103802600909,
-0.745273606516182,-0.726295947047053,-0.695049120900939,-0.688596761355418,
-0.684441364973233,-0.681058003851479,-0.677110567447394,-0.66991977471846,
-0.645025481726327,-0.616751452980132,-0.609394446240116,-0.606531407471489,
-0.604589995903919,-0.602477227718807,-0.598887961390896,-0.582018916142274,
-0.546915379310128,-0.535219056371545,-0.530376653344707,-0.526940370528925,
-0.523338876336458,-0.517818758274082,-0.498812804566657,-0.479636234585103,
-0.457731627679638,-0.452911554985154,-0.450545945761603,-0.448636991192947,
-0.446199306962801,-0.440995736158348,-0.43370816828533,-0.411288894065386,
-0.384769545814982,-0.378234104175473,-0.374054671587356,-0.37067017430508,
-0.366742096133908,-0.359646354434851,-0.357466815432906),.UNSPECIFIED.);
#952=B_SPLINE_CURVE_WITH_KNOTS('',3,(#81636,#81637,#81638,#81639,#81640,
#81641,#81642,#81643,#81644,#81645,#81646,#81647,#81648,#81649,#81650,#81651,
#81652,#81653,#81654,#81655,#81656,#81657,#81658,#81659,#81660,#81661,#81662,
#81663,#81664,#81665,#81666,#81667,#81668,#81669,#81670,#81671,#81672,#81673,
#81674,#81675,#81676,#81677,#81678,#81679,#81680,#81681,#81682,#81683,#81684,
#81685,#81686,#81687,#81688,#81689,#81690,#81691,#81692,#81693,#81694,#81695,
#81696,#81697,#81698,#81699),.UNSPECIFIED.,.F.,.F.,(4,3,3,3,3,3,3,3,3,3,
3,3,3,3,3,3,3,3,3,3,3,4),(91.1061869544955,91.3019231704377,91.4974252818407,
91.6933906075753,91.885949718829,92.0846205836694,92.2836890662572,92.4819083883214,
92.681401451171,92.8808945140205,93.0792205808948,93.2783752629741,93.4762509314101,
93.676045120311,93.875839309212,94.0748286238527,94.2738174939904,94.4723404042387,
94.6715622543211,94.8707841044036,95.0696932795969,95.1011120778127),
 .UNSPECIFIED.);
#953=B_SPLINE_CURVE_WITH_KNOTS('',3,(#81700,#81701,#81702,#81703,#81704,
#81705,#81706,#81707,#81708,#81709,#81710,#81711,#81712,#81713,#81714,#81715,
#81716,#81717,#81718,#81719,#81720,#81721,#81722,#81723,#81724,#81725,#81726,
#81727,#81728,#81729,#81730,#81731,#81732,#81733,#81734,#81735,#81736),
 .UNSPECIFIED.,.F.,.F.,(4,3,3,3,3,3,3,3,3,3,3,3,4),(88.8169224278005,88.9011153332543,
89.0997382756417,89.2988187388427,89.4969885119119,89.6965243201789,89.8960601284459,
90.0946293819821,90.2937232673959,90.4918397176078,90.6914223206226,90.8910049236374,
91.106186954104),.UNSPECIFIED.);
#954=B_SPLINE_CURVE_WITH_KNOTS('',3,(#81738,#81739,#81740,#81741,#81742,
#81743,#81744,#81745,#81746,#81747,#81748,#81749,#81750,#81751,#81752,#81753,
#81754,#81755,#81756,#81757,#81758,#81759,#81760,#81761,#81762,#81763,#81764,
#81765,#81766,#81767,#81768,#81769,#81770,#81771,#81772,#81773,#81774,#81775,
#81776,#81777,#81778,#81779,#81780,#81781,#81782,#81783,#81784,#81785,#81786,
#81787,#81788,#81789,#81790,#81791,#81792,#81793,#81794,#81795,#81796,#81797,
#81798,#81799,#81800,#81801,#81802,#81803,#81804,#81805,#81806,#81807,#81808,
#81809,#81810,#81811,#81812,#81813,#81814,#81815,#81816,#81817,#81818,#81819,
#81820,#81821,#81822,#81823,#81824,#81825,#81826,#81827,#81828,#81829,#81830,
#81831,#81832,#81833,#81834,#81835,#81836,#81837,#81838,#81839,#81840,#81841,
#81842,#81843,#81844,#81845,#81846,#81847,#81848,#81849,#81850,#81851),
 .UNSPECIFIED.,.F.,.F.,(4,2,2,2,2,2,2,2,2,2,2,2,2,2,2,2,2,2,2,2,2,2,2,2,
2,2,2,2,2,2,2,2,2,2,2,2,2,2,2,2,2,2,2,2,2,2,2,2,2,2,2,2,2,2,2,2,4),(-0.357466815432906,
-0.335505369566104,-0.308753656232884,-0.299500133901965,-0.296389308718004,
-0.294578676695416,-0.292583469853657,-0.289542586091397,-0.280126391837006,
-0.262513679674971,-0.229204091676723,-0.222237301328509,-0.21829495824427,
-0.214911098029315,-0.210748904360708,-0.202459882276656,-0.175758644558994,
-0.14683741003079,-0.142356826979249,-0.140029425723709,-0.138310021477257,
-0.138266268667842,-0.138228291607211,-0.138195152653209,-0.138166103444295,
-0.138140538750668,-0.138117963388781,-0.138073152228888,-0.138029311126522,
-0.137986357293708,-0.137944214086576,-0.137902810316141,-0.137862079643245,
-0.137821960045959,-0.137782393344716,-0.137743324782,-0.137704702646856,
-0.137666477938929,-0.137628604064892,-0.137591036565843,-0.137553732869206,
-0.137516652063368,-0.137479754690233,-0.137443002555816,-0.137406358554429,
-0.134792103433566,-0.131519171259025,-0.125370551601353,-0.108938515655659,
-0.0736210289563799,-0.066845749561155,-0.0629450966540203,-0.059558690499896,
-0.0553437885576436,-0.0467694157111863,-0.0235830156413483,-0.00025810012616317),
 .UNSPECIFIED.);
#955=B_SPLINE_CURVE_WITH_KNOTS('',3,(#81852,#81853,#81854,#81855,#81856,
#81857,#81858,#81859),.UNSPECIFIED.,.F.,.F.,(4,1,1,1,1,4),(91.106186954104,
91.2110051344337,92.2059499296252,93.2008947248167,94.1958395200083,95.0999839528908),
 .UNSPECIFIED.);
#956=B_SPLINE_CURVE_WITH_KNOTS('',3,(#81863,#81864,#81865,#81866,#81867,
#81868),.UNSPECIFIED.,.F.,.F.,(4,1,1,4),(-4.09254174883834,-3.97977918076615,
-2.98483438557462,-2.06533154845012),.UNSPECIFIED.);
#957=B_SPLINE_CURVE_WITH_KNOTS('',3,(#81872,#81873,#81874,#81875,#81876),
 .UNSPECIFIED.,.F.,.F.,(4,1,4),(0.,0.994944795191534,1.11419103802954),
 .UNSPECIFIED.);
#958=B_SPLINE_CURVE_WITH_KNOTS('',3,(#81878,#81879,#81880,#81881,#81882,
#81883,#81884,#81885,#81886,#81887,#81888,#81889,#81890,#81891,#81892,#81893,
#81894,#81895,#81896,#81897,#81898,#81899,#81900,#81901,#81902,#81903,#81904,
#81905,#81906,#81907,#81908,#81909,#81910,#81911,#81912,#81913,#81914,#81915,
#81916,#81917,#81918,#81919,#81920,#81921,#81922,#81923,#81924,#81925,#81926,
#81927,#81928,#81929,#81930,#81931,#81932,#81933,#81934,#81935,#81936,#81937,
#81938,#81939,#81940,#81941,#81942,#81943,#81944,#81945,#81946,#81947,#81948,
#81949,#81950,#81951,#81952,#81953,#81954,#81955,#81956,#81957,#81958,#81959,
#81960,#81961,#81962,#81963,#81964,#81965,#81966,#81967,#81968,#81969,#81970,
#81971,#81972,#81973,#81974,#81975,#81976,#81977,#81978,#81979,#81980,#81981,
#81982,#81983,#81984,#81985,#81986,#81987,#81988,#81989,#81990,#81991,#81992),
 .UNSPECIFIED.,.F.,.F.,(4,3,3,3,3,3,3,3,3,3,3,3,3,3,3,3,3,3,3,3,3,3,3,3,
3,3,3,3,3,3,3,3,3,3,3,3,3,3,4),(1.11419103802954,1.29735287581724,1.48032203138593,
1.66315115312043,1.84640621249915,1.98988959038307,2.17778566050261,2.36529042623222,
2.55276479925355,2.7402270554159,2.92810799385181,2.98483438557461,3.17276381816055,
3.36031274498174,3.54784651507135,3.73537708606522,3.92333837693577,3.97977918076615,
4.16712482605355,4.35407332305044,4.54099162516431,4.72789741546226,4.91523160890231,
4.97472397595769,5.16238494385731,5.34965485800517,5.53689856155208,5.7241324002202,
5.91179256293985,5.96966877114923,6.15731012319844,6.34456142792096,6.53178829851298,
6.71900632200928,6.90665247879335,6.96461356634077,7.1682696460741,7.3706362873007,
7.39737602502259),.UNSPECIFIED.);
#959=B_SPLINE_CURVE_WITH_KNOTS('',3,(#81994,#81995,#81996,#81997,#81998,
#81999,#82000,#82001,#82002,#82003),.UNSPECIFIED.,.F.,.F.,(4,1,1,1,1,1,
1,4),(7.39737634520912,7.95955836153231,8.95450315672385,9.94944795191539,
10.9443927471069,11.9393375422985,12.93428233749,13.6805616523887),
 .UNSPECIFIED.);
#960=B_SPLINE_CURVE_WITH_KNOTS('',3,(#82005,#82006,#82007,#82008,#82009,
#82010,#82011,#82012,#82013,#82014,#82015),.UNSPECIFIED.,.F.,.F.,(4,1,1,
1,1,1,1,1,4),(13.6805616523887,13.9292271326815,14.9241719278731,15.9191167230646,
16.9140615182562,17.9090063134477,18.9039511086392,19.8988959038308,19.9637469595683),
 .UNSPECIFIED.);
#961=B_SPLINE_CURVE_WITH_KNOTS('',3,(#82017,#82018,#82019,#82020,#82021,
#82022,#82023,#82024,#82025,#82026),.UNSPECIFIED.,.F.,.F.,(4,1,1,1,1,1,
1,4),(19.9637469595683,20.8938406990223,21.8887854942138,22.8837302894054,
23.8786750845969,24.8736198797885,25.86856467498,26.2469322667479),
 .UNSPECIFIED.);
#962=B_SPLINE_CURVE_WITH_KNOTS('',3,(#82028,#82029,#82030,#82031,#82032,
#82033,#82034,#82035,#82036,#82037),.UNSPECIFIED.,.F.,.F.,(4,1,1,1,1,1,
1,4),(26.2469322667479,26.8635094701715,27.8584542653631,28.8533990605546,
29.8483438557462,30.8432886509377,31.8382334461292,32.5301175739275),
 .UNSPECIFIED.);
#963=B_SPLINE_CURVE_WITH_KNOTS('',3,(#82039,#82040,#82041,#82042,#82043,
#82044,#82045,#82046,#82047,#82048,#82049,#82050,#82051,#82052,#82053,#82054,
#82055,#82056,#82057,#82058,#82059,#82060,#82061,#82062,#82063,#82064,#82065,
#82066,#82067,#82068,#82069,#82070,#82071,#82072,#82073,#82074,#82075,#82076,
#82077,#82078,#82079,#82080,#82081,#82082,#82083,#82084,#82085,#82086,#82087,
#82088,#82089,#82090,#82091,#82092,#82093,#82094,#82095,#82096,#82097,#82098,
#82099,#82100,#82101,#82102,#82103,#82104,#82105,#82106,#82107,#82108,#82109,
#82110,#82111,#82112,#82113,#82114,#82115,#82116,#82117,#82118,#82119,#82120,
#82121,#82122,#82123,#82124,#82125,#82126,#82127,#82128,#82129,#82130,#82131,
#82132,#82133,#82134,#82135,#82136,#82137,#82138,#82139,#82140,#82141,#82142,
#82143,#82144,#82145,#82146,#82147,#82148,#82149,#82150,#82151,#82152,#82153,
#82154,#82155,#82156),.UNSPECIFIED.,.F.,.F.,(4,3,3,3,3,3,3,3,3,3,3,3,3,
3,3,3,3,3,3,3,3,3,3,3,3,3,3,3,3,3,3,3,3,3,3,3,3,3,3,4),(32.530117758059,
32.7556141163704,32.8331782413208,33.0207814298638,33.2079931850932,33.3951790868026,
33.5823552778384,33.7699590877266,33.8281230365123,34.0157262250567,34.2029379802876,
34.3901238819984,34.5773000730357,34.7649038829253,34.8230678317039,35.010671020249,
35.1978827754804,35.3850686771919,35.5722448682299,35.7598486781202,35.8180126268954,
36.0056158154396,36.1928275706703,36.3800134723809,36.5671896634181,36.7547934733075,
36.8129574220869,37.0005606106315,37.1877723658625,37.3749582675735,37.562134458611,
37.7497382685008,37.8079022172785,37.9955054058231,38.1827171610541,38.3699030627651,
38.5570792538025,38.7446830636923,38.80284701247,38.8133028811071),
 .UNSPECIFIED.);
#964=B_SPLINE_CURVE_WITH_KNOTS('',3,(#82158,#82159,#82160,#82161,#82162,
#82163,#82164,#82165,#82166,#82167,#82168,#82169,#82170,#82171,#82172,#82173,
#82174,#82175,#82176,#82177,#82178,#82179,#82180,#82181,#82182,#82183,#82184,
#82185,#82186,#82187,#82188,#82189,#82190,#82191,#82192,#82193,#82194,#82195,
#82196,#82197,#82198,#82199,#82200,#82201,#82202,#82203,#82204,#82205,#82206,
#82207,#82208,#82209,#82210,#82211,#82212,#82213,#82214,#82215,#82216,#82217,
#82218,#82219,#82220,#82221,#82222,#82223,#82224,#82225,#82226,#82227,#82228,
#82229,#82230,#82231,#82232,#82233,#82234,#82235,#82236,#82237,#82238,#82239,
#82240,#82241,#82242,#82243,#82244,#82245,#82246,#82247,#82248,#82249,#82250,
#82251,#82252,#82253,#82254,#82255,#82256,#82257,#82258,#82259,#82260,#82261,
#82262,#82263,#82264,#82265,#82266,#82267,#82268,#82269,#82270,#82271,#82272),
 .UNSPECIFIED.,.F.,.F.,(4,3,3,3,3,3,3,3,3,3,3,3,3,3,3,3,3,3,3,3,3,3,3,3,
3,3,3,3,3,3,3,3,3,3,3,3,3,3,4),(38.8133028814085,39.0005614200088,39.1874299894609,
39.3742739703344,39.5611126744816,39.7483747801438,39.7977918076615,39.9853949962061,
40.1726067514371,40.3597926531481,40.5469688441856,40.7345726540754,40.7927366028531,
40.9803397913976,41.1675515466286,41.3547374483395,41.5419136393771,41.7295174492668,
41.7876813980446,41.9752845865891,42.1624963418201,42.3496822435311,42.5368584345686,
42.7244622444584,42.7826261932362,42.9702293817808,43.1574411370118,43.3446270387228,
43.5318032297602,43.7194070396501,43.7775709884277,43.9651741769722,44.1523859322031,
44.3395718339139,44.5267480249514,44.714351834841,44.7725157836192,44.9931015508383,
45.0964881878767),.UNSPECIFIED.);
#965=B_SPLINE_CURVE_WITH_KNOTS('',3,(#82274,#82275,#82276,#82277,#82278,
#82279,#82280,#82281,#82282,#82283,#82284,#82285,#82286,#82287,#82288,#82289,
#82290,#82291,#82292,#82293,#82294,#82295,#82296,#82297,#82298,#82299,#82300,
#82301,#82302,#82303,#82304,#82305,#82306,#82307,#82308,#82309,#82310,#82311,
#82312,#82313,#82314,#82315,#82316,#82317,#82318,#82319,#82320,#82321,#82322,
#82323,#82324,#82325,#82326,#82327,#82328,#82329,#82330,#82331,#82332,#82333,
#82334,#82335,#82336,#82337,#82338,#82339,#82340,#82341,#82342,#82343,#82344,
#82345,#82346,#82347,#82348,#82349,#82350,#82351,#82352,#82353,#82354,#82355,
#82356,#82357,#82358,#82359,#82360,#82361,#82362,#82363,#82364,#82365,#82366,
#82367,#82368,#82369,#82370,#82371,#82372,#82373,#82374,#82375,#82376,#82377,
#82378,#82379,#82380,#82381,#82382,#82383,#82384,#82385,#82386,#82387,#82388),
 .UNSPECIFIED.,.F.,.F.,(4,3,3,3,3,3,3,3,3,3,3,3,3,3,3,3,3,3,3,3,3,3,3,3,
3,3,3,3,3,3,3,3,3,3,3,3,3,3,4),(45.0964881882867,45.2833267165581,45.4701172611129,
45.6573702632114,45.7674605788108,45.9550637673553,46.1422755225862,46.3294614242972,
46.5166376153346,46.7042414252244,46.7624053740023,46.9500085625469,47.1372203177779,
47.3244062194889,47.5115824105264,47.6991862204162,47.7573501691939,47.9449533577385,
48.1321651129695,48.3193510146805,48.506527205718,48.6941310156078,48.7522949643854,
48.9398981529299,49.1271099081609,49.3142958098718,49.5014720009093,49.689075810799,
49.7472397595769,49.9348429481215,50.1220547033524,50.3092406050634,50.4964167961009,
50.6840206059907,50.7421845547685,50.9306517424822,51.1186979603826,51.3065834404951,
51.3796734954662),.UNSPECIFIED.);
#966=B_SPLINE_CURVE_WITH_KNOTS('',3,(#82390,#82391,#82392,#82393,#82394,
#82395,#82396,#82397,#82398,#82399,#82400,#82401,#82402,#82403,#82404,#82405,
#82406,#82407,#82408,#82409,#82410,#82411,#82412,#82413,#82414,#82415,#82416,
#82417,#82418,#82419,#82420,#82421,#82422,#82423,#82424,#82425,#82426,#82427,
#82428,#82429,#82430,#82431,#82432,#82433,#82434,#82435,#82436,#82437,#82438,
#82439,#82440,#82441,#82442,#82443,#82444,#82445,#82446,#82447,#82448,#82449,
#82450,#82451,#82452,#82453,#82454,#82455,#82456,#82457,#82458,#82459,#82460,
#82461,#82462,#82463,#82464,#82465,#82466,#82467,#82468,#82469,#82470,#82471,
#82472,#82473,#82474,#82475,#82476,#82477,#82478,#82479,#82480,#82481,#82482,
#82483,#82484,#82485,#82486,#82487,#82488,#82489,#82490,#82491,#82492,#82493,
#82494,#82495,#82496,#82497,#82498,#82499,#82500,#82501),.UNSPECIFIED.,
 .F.,.F.,(4,3,3,3,3,3,3,3,3,3,3,3,3,3,3,3,3,3,3,3,3,3,3,3,3,3,3,3,3,3,3,
3,3,3,3,3,3,4),(51.3796734959224,51.5936766963176,51.73712934996,51.9247325385046,
52.1119442937356,52.2991301954466,52.4863063864841,52.6739101963739,52.7320741451516,
52.9196773336959,53.1068890889265,53.2940749906372,53.4812511816744,53.6688549915638,
53.7270189403431,53.9146221288881,54.1018338841196,54.289019785831,54.476195976869,
54.6637997867592,54.7219637355346,54.909566924079,55.0967786793098,55.2839645810207,
55.471140772058,55.6587445819477,55.7169085307262,55.9045117192692,56.0917234744985,
56.2789093762079,56.4660855672438,56.653689377132,56.7118533259177,56.8981739682351,
57.0893451767646,57.2752466163079,57.4690527093306,57.6628588023532),
 .UNSPECIFIED.);
#967=B_SPLINE_CURVE_WITH_KNOTS('',3,(#82503,#82504,#82505,#82506,#82507,
#82508,#82509,#82510,#82511,#82512,#82513,#82514,#82515,#82516,#82517,#82518,
#82519,#82520,#82521,#82522,#82523,#82524,#82525,#82526,#82527,#82528,#82529,
#82530,#82531,#82532,#82533,#82534,#82535,#82536,#82537,#82538,#82539,#82540,
#82541,#82542,#82543,#82544,#82545,#82546,#82547,#82548,#82549,#82550,#82551,
#82552,#82553,#82554,#82555,#82556,#82557,#82558,#82559,#82560,#82561,#82562,
#82563,#82564,#82565,#82566,#82567,#82568,#82569,#82570,#82571,#82572,#82573,
#82574,#82575,#82576,#82577,#82578,#82579,#82580,#82581,#82582,#82583,#82584,
#82585,#82586,#82587,#82588,#82589,#82590,#82591,#82592,#82593,#82594,#82595,
#82596,#82597,#82598,#82599,#82600,#82601,#82602,#82603,#82604,#82605,#82606,
#82607,#82608,#82609,#82610,#82611,#82612,#82613,#82614,#82615,#82616,#82617,
#82618,#82619,#82620),.UNSPECIFIED.,.F.,.F.,(4,3,3,3,3,3,3,3,3,3,3,3,3,
3,3,3,3,3,3,3,3,3,3,3,3,3,3,3,3,3,3,3,3,3,3,3,3,3,3,4),(57.6628588026459,
57.7067981211093,57.8944013096513,58.0816130648797,58.2687989665883,58.4559751576235,
58.643578967511,58.7017429163008,58.8893461048363,59.0765578600581,59.2637437617599,
59.4509199527882,59.638523762669,59.6966877114923,59.8842909000647,60.0715026553235,
60.258688557062,60.4458647481267,60.6334685580429,60.6916325066839,60.8792356952034,
61.0664474504096,61.2536333520967,61.4408095431107,61.6284133529781,61.6865773018754,
61.8741804903711,62.0613922455524,62.2485781472136,62.435754338201,62.6233581480414,
62.6815220970669,62.8691252858037,63.0563370412272,63.243522943128,63.4306991343541,
63.6183029444271,63.6764668922585,63.9115682388477,63.9460441094081),
 .UNSPECIFIED.);
#968=B_SPLINE_CURVE_WITH_KNOTS('',3,(#82622,#82623,#82624,#82625,#82626,
#82627,#82628,#82629,#82630,#82631,#82632,#82633,#82634,#82635,#82636,#82637,
#82638,#82639,#82640,#82641,#82642,#82643,#82644,#82645,#82646,#82647,#82648,
#82649,#82650,#82651,#82652,#82653,#82654,#82655,#82656,#82657,#82658,#82659,
#82660,#82661,#82662,#82663,#82664,#82665,#82666,#82667,#82668,#82669,#82670,
#82671,#82672,#82673,#82674,#82675,#82676,#82677,#82678,#82679,#82680,#82681,
#82682,#82683,#82684,#82685,#82686,#82687,#82688,#82689,#82690,#82691,#82692,
#82693,#82694,#82695,#82696,#82697,#82698,#82699,#82700,#82701,#82702,#82703,
#82704,#82705,#82706,#82707,#82708,#82709,#82710,#82711,#82712,#82713,#82714,
#82715,#82716,#82717,#82718,#82719,#82720,#82721,#82722,#82723,#82724,#82725,
#82726,#82727,#82728,#82729,#82730,#82731,#82732,#82733),.UNSPECIFIED.,
 .F.,.F.,(4,3,3,3,3,3,3,3,3,3,3,3,3,3,3,3,3,3,3,3,3,3,3,3,3,3,3,3,3,3,3,
3,3,3,3,3,3,4),(63.9460441098254,64.131587392169,64.3169915432042,64.5028443208997,
64.67141168745,64.8590148757571,65.0462266307455,65.2334125322104,65.4205887229996,
65.6081925326422,65.6663564826416,65.8539596724817,66.0411714290113,66.2283573320057,
66.4155335243191,66.6031373354505,66.6613012778331,66.8489044645521,67.0361162179695,
67.223302117911,67.4104783072031,67.5980821154138,67.6562460730246,67.8438492606578,
68.0310610149416,68.2182469156685,68.4054231056998,68.5930269145697,68.6511908682162,
68.8387940652687,69.0260058290388,69.2131917392048,69.4003679386567,69.5879717567479,
69.6461356634077,69.8371933145111,70.033211365758,70.229229417005),
 .UNSPECIFIED.);
#969=B_SPLINE_CURVE_WITH_KNOTS('',3,(#82735,#82736,#82737,#82738,#82739,
#82740,#82741,#82742,#82743,#82744,#82745,#82746,#82747,#82748,#82749,#82750,
#82751,#82752,#82753,#82754,#82755,#82756,#82757,#82758,#82759,#82760,#82761,
#82762,#82763,#82764,#82765,#82766,#82767,#82768,#82769,#82770,#82771,#82772,
#82773,#82774,#82775,#82776,#82777,#82778,#82779,#82780,#82781,#82782,#82783,
#82784,#82785,#82786,#82787,#82788,#82789,#82790,#82791,#82792,#82793,#82794,
#82795,#82796,#82797,#82798,#82799,#82800,#82801,#82802,#82803,#82804,#82805,
#82806,#82807,#82808,#82809,#82810,#82811,#82812,#82813,#82814,#82815,#82816,
#82817,#82818,#82819,#82820,#82821,#82822,#82823,#82824,#82825,#82826,#82827,
#82828,#82829,#82830,#82831,#82832,#82833,#82834,#82835,#82836,#82837,#82838,
#82839,#82840,#82841,#82842,#82843,#82844,#82845,#82846),.UNSPECIFIED.,
 .F.,.F.,(4,3,3,3,3,3,3,3,3,3,3,3,3,3,3,3,3,3,3,3,3,3,3,3,3,3,3,3,3,3,3,
3,3,3,3,3,3,4),(70.2292294173832,70.4351549379912,70.6410804585992,70.8286836460334,
71.0158953999048,71.203081299923,71.3902574890733,71.5778612968305,71.6360252537908,
71.8236284966211,72.0108403064174,72.1980262622685,72.3852025072517,72.5728063698176,
72.6309700489823,72.8185731289811,73.0057847759896,73.192970571568,73.3801466575811,
73.5677503659684,73.6259148441739,73.8135180610028,74.000729842834,74.1879157683528,
74.375091981605,74.5626958110086,74.6208596393654,74.8084631627783,74.9956752551974,
75.1828614923107,75.3700380180363,75.5576421554465,75.6158044345569,75.8010937918736,
75.9861285115055,76.1709869704709,76.3562168039986,76.5124147237435),
 .UNSPECIFIED.);
#970=B_SPLINE_CURVE_WITH_KNOTS('',3,(#82848,#82849,#82850,#82851,#82852,
#82853,#82854,#82855,#82856,#82857,#82858,#82859,#82860,#82861,#82862,#82863,
#82864,#82865,#82866,#82867,#82868,#82869,#82870,#82871,#82872,#82873,#82874,
#82875,#82876,#82877,#82878,#82879,#82880,#82881,#82882,#82883,#82884,#82885,
#82886,#82887,#82888,#82889,#82890,#82891,#82892,#82893,#82894,#82895,#82896,
#82897,#82898,#82899,#82900,#82901,#82902,#82903,#82904,#82905,#82906,#82907,
#82908,#82909,#82910,#82911,#82912,#82913,#82914,#82915,#82916,#82917,#82918,
#82919,#82920,#82921,#82922,#82923,#82924,#82925,#82926,#82927,#82928,#82929,
#82930,#82931,#82932,#82933,#82934,#82935,#82936,#82937,#82938,#82939,#82940,
#82941,#82942,#82943,#82944,#82945,#82946,#82947,#82948,#82949,#82950,#82951,
#82952,#82953,#82954,#82955,#82956,#82957,#82958,#82959,#82960,#82961,#82962),
 .UNSPECIFIED.,.F.,.F.,(4,3,3,3,3,3,3,3,3,3,3,3,3,3,3,3,3,3,3,3,3,3,3,3,
3,3,3,3,3,3,3,3,3,3,3,3,3,3,4),(76.5124147241846,76.6107492297485,76.7983528569055,
76.9855650396531,77.1727513466827,77.3599279305794,77.5475321081861,77.60569402494,
77.7932991932381,77.9805129465394,78.1677008422247,78.3548790267638,78.5424847929033,
78.6006388201316,78.7882363136644,78.9754423761354,79.162622674032,79.3497933073766,
79.5373917279101,79.5955836153231,79.7831914375022,79.9704077552958,80.1575980498889,
80.3447785397938,80.5323864343542,80.5905284105146,80.7781426404921,80.9653655764656,
81.152562688196,81.339750116825,81.5273649977987,81.5854732057062,81.7730367225467,
81.960208775334,82.1473555280425,82.334492852466,82.5220589147969,82.5804180008977,
82.7956000313642),.UNSPECIFIED.);
#971=B_SPLINE_CURVE_WITH_KNOTS('',3,(#82964,#82965,#82966,#82967,#82968,
#82969,#82970,#82971),.UNSPECIFIED.,.F.,.F.,(4,1,1,1,1,4),(82.7956015954281,
83.5753627960893,84.5703075912808,85.5652523864723,86.5601971816639,87.4798914339604),
 .UNSPECIFIED.);
#972=B_SPLINE_CURVE_WITH_KNOTS('',3,(#82975,#82976,#82977,#82978,#82979,
#82980,#82981),.UNSPECIFIED.,.F.,.F.,(4,1,1,1,4),(-89.5450315672385,-88.550086772047,
-87.5551419768554,-86.5601971816639,-85.773952932868),.UNSPECIFIED.);
#973=B_SPLINE_CURVE_WITH_KNOTS('',3,(#82983,#82984,#82985,#82986,#82987,
#82988,#82989,#82990,#82991,#82992,#82993,#82994,#82995,#82996,#82997,#82998,
#82999,#83000,#83001,#83002,#83003,#83004,#83005,#83006,#83007,#83008,#83009,
#83010,#83011,#83012,#83013,#83014,#83015,#83016,#83017,#83018,#83019,#83020,
#83021,#83022,#83023,#83024,#83025,#83026,#83027,#83028,#83029,#83030,#83031,
#83032,#83033,#83034,#83035,#83036,#83037,#83038,#83039,#83040,#83041,#83042,
#83043,#83044,#83045,#83046,#83047,#83048,#83049,#83050,#83051,#83052,#83053,
#83054,#83055,#83056,#83057,#83058,#83059,#83060,#83061,#83062,#83063,#83064,
#83065,#83066,#83067,#83068,#83069,#83070,#83071,#83072,#83073,#83074,#83075,
#83076,#83077,#83078,#83079,#83080,#83081,#83082,#83083,#83084,#83085,#83086,
#83087,#83088,#83089,#83090,#83091,#83092,#83093,#83094,#83095,#83096,#83097),
 .UNSPECIFIED.,.F.,.F.,(4,3,3,3,3,3,3,3,3,3,3,3,3,3,3,3,3,3,3,3,3,3,3,3,
3,3,3,3,3,3,3,3,3,3,3,3,3,3,4),(-85.773950742173,-85.5652523864724,-85.3779064829695,
-85.1909577220866,-85.0040391516937,-84.8171330902571,-84.6297986263033,
-84.5703075912808,-84.3826467392874,-84.1953769427502,-84.0081333574826,
-83.8208996375907,-83.6332395922033,-83.5753627960893,-83.3877214692297,
-83.2004701908784,-83.013243347994,-82.8260253530088,-82.6383792254152,
-82.5804180008977,-82.392852474649,-82.2056792726101,-82.0185326323522,
-81.8313961522527,-81.6438319912061,-81.5854732057062,-81.397858980688,
-81.2106360590108,-81.0234389748642,-80.8362515815531,-80.6486367465815,
-80.5905284105147,-80.4029211436349,-80.2157051380387,-80.0285147992829,
-79.8413340584639,-79.6537256147139,-79.5955836153231,-79.4907654349934),
 .UNSPECIFIED.);
#974=B_SPLINE_CURVE_WITH_KNOTS('',3,(#83099,#83100,#83101,#83102,#83103,
#83104,#83105,#83106,#83107,#83108,#83109,#83110,#83111,#83112,#83113,#83114,
#83115,#83116,#83117,#83118,#83119,#83120,#83121,#83122,#83123,#83124,#83125,
#83126,#83127,#83128,#83129,#83130,#83131,#83132,#83133,#83134,#83135,#83136,
#83137,#83138,#83139,#83140,#83141,#83142,#83143,#83144,#83145,#83146,#83147,
#83148,#83149,#83150,#83151,#83152,#83153,#83154,#83155,#83156,#83157,#83158,
#83159,#83160,#83161,#83162,#83163,#83164,#83165,#83166,#83167,#83168,#83169,
#83170,#83171,#83172,#83173,#83174,#83175,#83176,#83177,#83178,#83179,#83180,
#83181,#83182,#83183,#83184,#83185,#83186,#83187,#83188,#83189,#83190,#83191,
#83192,#83193,#83194,#83195,#83196,#83197,#83198,#83199,#83200,#83201,#83202,
#83203,#83204,#83205,#83206,#83207,#83208,#83209,#83210),.UNSPECIFIED.,
 .F.,.F.,(4,3,3,3,3,3,3,3,3,3,3,3,3,3,3,3,3,3,3,3,3,3,3,3,3,3,3,3,3,3,3,
3,3,3,3,3,3,4),(-79.4907654345562,-79.3056659286142,-79.1207476836018,-78.9359630581407,
-78.7507490396709,-78.6006388201316,-78.4130336821603,-78.2258199481935,
-78.0386320556497,-77.8514538648623,-77.6638480788338,-77.60569402494,-77.4180904691762,
-77.2308783264915,-77.0436920136003,-76.856515397198,-76.6689111486492,
-76.6107492297485,-76.4231467887123,-76.2359358006407,-76.048750682992,
-75.861575286587,-75.673972272423,-75.6158044345569,-75.4282009197706,-75.2409888326382,
-75.0538025959008,-74.8666260677027,-74.6790219236929,-74.6208596393654,
-74.4332564312801,-74.2460446543263,-74.0588587280189,-73.8716825106907,
-73.6840786724701,-73.6259148441739,-73.4167474861729,-73.2075801281719),
 .UNSPECIFIED.);
#975=B_SPLINE_CURVE_WITH_KNOTS('',3,(#83212,#83213,#83214,#83215,#83216,
#83217,#83218,#83219,#83220,#83221,#83222,#83223,#83224,#83225,#83226,#83227,
#83228,#83229,#83230,#83231,#83232,#83233,#83234,#83235,#83236,#83237,#83238,
#83239,#83240,#83241,#83242,#83243,#83244,#83245,#83246,#83247,#83248,#83249,
#83250,#83251,#83252,#83253,#83254,#83255,#83256,#83257,#83258,#83259,#83260,
#83261,#83262,#83263,#83264,#83265,#83266,#83267,#83268,#83269,#83270,#83271,
#83272,#83273,#83274,#83275,#83276,#83277,#83278,#83279,#83280,#83281,#83282,
#83283,#83284,#83285,#83286,#83287,#83288,#83289,#83290,#83291,#83292,#83293,
#83294,#83295,#83296,#83297,#83298,#83299,#83300,#83301,#83302,#83303,#83304,
#83305,#83306,#83307,#83308,#83309,#83310,#83311,#83312,#83313,#83314,#83315,
#83316,#83317,#83318,#83319,#83320,#83321,#83322,#83323),.UNSPECIFIED.,
 .F.,.F.,(4,3,3,3,3,3,3,3,3,3,3,3,3,3,3,3,3,3,3,3,3,3,3,3,3,3,3,3,3,3,3,
3,3,3,3,3,3,4),(-73.2075801278138,-73.016815520887,-72.8238927849347,-72.6309700489823,
-72.4433668079907,-72.2561549993083,-72.0689690435056,-71.8817927979529,
-71.6941889339227,-71.6360252537908,-71.4484220673553,-71.2612103140335,
-71.074024413907,-70.8868482242669,-70.6992444154695,-70.6410804585993,
-70.4534772833099,-70.2662655417254,-70.0790796540231,-69.8919034772181,
-69.7042996816319,-69.6461356634077,-69.4585324667012,-69.2713207031396,
-69.0841347929803,-68.8969585934182,-68.7093547750472,-68.6511908682162,
-68.4635876806845,-68.276375926455,-68.0891900257129,-67.9020138356261,
-67.7144100266428,-67.6562460730246,-67.4705123135506,-67.2851577710245,
-67.0997342737558,-66.9243948206342),.UNSPECIFIED.);
#976=B_SPLINE_CURVE_WITH_KNOTS('',3,(#83325,#83326,#83327,#83328,#83329,
#83330,#83331,#83332,#83333,#83334,#83335,#83336,#83337,#83338,#83339,#83340,
#83341,#83342,#83343,#83344,#83345,#83346,#83347,#83348,#83349,#83350,#83351,
#83352,#83353,#83354,#83355,#83356,#83357,#83358,#83359,#83360,#83361,#83362,
#83363,#83364,#83365,#83366,#83367,#83368,#83369,#83370,#83371,#83372,#83373,
#83374,#83375,#83376,#83377,#83378,#83379,#83380,#83381,#83382,#83383,#83384,
#83385,#83386,#83387,#83388,#83389,#83390,#83391,#83392,#83393,#83394,#83395,
#83396,#83397,#83398,#83399,#83400,#83401,#83402,#83403,#83404,#83405,#83406,
#83407,#83408,#83409,#83410,#83411,#83412,#83413,#83414,#83415,#83416,#83417,
#83418,#83419,#83420,#83421,#83422,#83423,#83424,#83425,#83426,#83427,#83428,
#83429,#83430,#83431,#83432,#83433,#83434,#83435,#83436,#83437,#83438,#83439,
#83440,#83441,#83442),.UNSPECIFIED.,.F.,.F.,(4,3,3,3,3,3,3,3,3,3,3,3,3,
3,3,3,3,3,3,3,3,3,3,3,3,3,3,3,3,3,3,3,3,3,3,3,3,3,3,4),(-66.9243948202828,
-66.6871196879193,-66.6613012778331,-66.4736980880535,-66.2864863315603,
-66.0993004285668,-65.9121242362338,-65.7245204250532,-65.6663564826416,
-65.4787532943425,-65.2915415393579,-65.1043556378908,-64.9171794470959,
-64.7295756374425,-64.67141168745,-64.4838084991056,-64.2965967440818,-64.109410842585,
-63.9222346517659,-63.734630842097,-63.6764668922585,-63.4888637035318,
-63.3016519481145,-63.1144660462139,-62.9272898549847,-62.7396860449035,
-62.681522097067,-62.4939189085714,-62.3067071533899,-62.1195212517283,
-61.9323450607403,-61.7447412508991,-61.6865773018754,-61.498974113353,
-61.3117623581451,-61.1245764564582,-60.9374002654453,-60.7497964555805,
-60.6916325066839,-60.6412095134547),.UNSPECIFIED.);
#977=B_SPLINE_CURVE_WITH_KNOTS('',3,(#83444,#83445,#83446,#83447,#83448,
#83449,#83450,#83451,#83452,#83453,#83454,#83455,#83456,#83457,#83458,#83459,
#83460,#83461,#83462,#83463,#83464,#83465,#83466,#83467,#83468,#83469,#83470,
#83471,#83472,#83473,#83474,#83475,#83476,#83477,#83478,#83479,#83480,#83481,
#83482,#83483,#83484,#83485,#83486,#83487,#83488,#83489,#83490,#83491,#83492,
#83493,#83494,#83495,#83496,#83497,#83498,#83499,#83500,#83501,#83502,#83503,
#83504,#83505,#83506,#83507,#83508,#83509,#83510,#83511,#83512,#83513,#83514,
#83515,#83516,#83517,#83518,#83519,#83520,#83521,#83522,#83523,#83524,#83525,
#83526,#83527,#83528,#83529,#83530,#83531,#83532,#83533,#83534,#83535,#83536,
#83537,#83538,#83539,#83540,#83541,#83542,#83543,#83544,#83545,#83546,#83547,
#83548,#83549,#83550,#83551,#83552,#83553,#83554,#83555),.UNSPECIFIED.,
 .F.,.F.,(4,3,3,3,3,3,3,3,3,3,3,3,3,3,3,3,3,3,3,3,3,3,3,3,3,3,3,3,3,3,3,
3,3,3,3,3,3,4),(-60.6412095131385,-60.4550710274,-60.2654751984231,-60.0797248474358,
-59.888206279464,-59.6966877114923,-59.5090845229566,-59.3218727677347,
-59.1346868660328,-58.9475106750045,-58.7599068651237,-58.7017429163008,
-58.5141397277585,-58.3269279725298,-58.1397420708213,-57.9525658797863,
-57.7649620698991,-57.7067981211093,-57.519194932561,-57.3319831773264,
-57.1447972756115,-56.9576210845701,-56.7700172746764,-56.7118533259177,
-56.5242501373747,-56.3370383821452,-56.1498524804358,-55.9626762894,-55.7750724795118,
-55.7169085307262,-55.5293053421818,-55.342093586951,-55.1549076852402,
-54.9677314942029,-54.7801276843134,-54.7219637355346,-54.5090848399423,
-54.3580242067312),.UNSPECIFIED.);
#978=B_SPLINE_CURVE_WITH_KNOTS('',3,(#83557,#83558,#83559,#83560,#83561,
#83562,#83563,#83564,#83565,#83566,#83567,#83568,#83569,#83570,#83571,#83572,
#83573,#83574,#83575,#83576,#83577,#83578,#83579,#83580,#83581,#83582,#83583,
#83584,#83585,#83586,#83587,#83588,#83589,#83590,#83591,#83592,#83593,#83594,
#83595,#83596,#83597,#83598,#83599,#83600,#83601,#83602,#83603,#83604,#83605,
#83606,#83607,#83608,#83609,#83610,#83611,#83612,#83613,#83614,#83615,#83616,
#83617,#83618,#83619,#83620,#83621,#83622,#83623,#83624,#83625,#83626,#83627,
#83628,#83629,#83630,#83631,#83632,#83633,#83634,#83635,#83636,#83637,#83638,
#83639,#83640,#83641,#83642,#83643,#83644,#83645,#83646,#83647,#83648,#83649,
#83650,#83651,#83652,#83653,#83654,#83655,#83656,#83657,#83658,#83659,#83660,
#83661,#83662,#83663,#83664,#83665,#83666,#83667,#83668,#83669,#83670,#83671),
 .UNSPECIFIED.,.F.,.F.,(4,3,3,3,3,3,3,3,3,3,3,3,3,3,3,3,3,3,3,3,3,3,3,3,
3,3,3,3,3,3,3,3,3,3,3,3,3,3,4),(-54.3580242062751,-54.1698030157393,-53.9815482560258,
-53.7928058472959,-53.7270189403431,-53.5394157517988,-53.3522039965681,
-53.1650180948574,-52.9778419038202,-52.7902380939308,-52.7320741451516,
-52.544470956607,-52.357259201376,-52.170073299665,-51.9828971086275,-51.7952932987378,
-51.73712934996,-51.5495261614154,-51.3623144061844,-51.1751285044734,-50.9879523134359,
-50.8003485035461,-50.7421845547685,-50.554581366224,-50.367369610993,-50.1801837092821,
-49.9930075182446,-49.8054037083549,-49.7472397595769,-49.5596365710323,
-49.3724248158012,-49.1852389140902,-48.9980627230527,-48.810458913163,
-48.7522949643854,-48.5652370035731,-48.3785769311802,-48.1919778865844,
-48.0748388990955),.UNSPECIFIED.);
#979=B_SPLINE_CURVE_WITH_KNOTS('',3,(#83673,#83674,#83675,#83676,#83677,
#83678,#83679,#83680,#83681,#83682,#83683,#83684,#83685,#83686,#83687,#83688,
#83689,#83690,#83691,#83692,#83693,#83694,#83695,#83696,#83697,#83698,#83699,
#83700,#83701,#83702,#83703,#83704,#83705,#83706,#83707,#83708,#83709,#83710,
#83711,#83712,#83713,#83714,#83715,#83716,#83717,#83718,#83719,#83720,#83721,
#83722,#83723,#83724,#83725,#83726,#83727,#83728,#83729,#83730,#83731,#83732,
#83733,#83734,#83735,#83736,#83737,#83738,#83739,#83740,#83741,#83742,#83743,
#83744,#83745,#83746,#83747,#83748,#83749,#83750,#83751,#83752,#83753,#83754,
#83755,#83756,#83757,#83758,#83759,#83760,#83761,#83762,#83763,#83764,#83765,
#83766,#83767,#83768,#83769,#83770,#83771,#83772,#83773,#83774,#83775,#83776,
#83777,#83778,#83779,#83780,#83781,#83782,#83783,#83784,#83785,#83786,#83787),
 .UNSPECIFIED.,.F.,.F.,(4,3,3,3,3,3,3,3,3,3,3,3,3,3,3,3,3,3,3,3,3,3,3,3,
3,3,3,3,3,3,3,3,3,3,3,3,3,3,4),(-48.0748388987013,-47.8528052031575,-47.7573501691939,
-47.5697469806493,-47.3825352254183,-47.1953493237073,-47.0081731326697,
-46.82056932278,-46.7624053740023,-46.5748021854578,-46.3875904302269,-46.200404528516,
-46.0132283374785,-45.8256245275888,-45.7674605788108,-45.5798573902662,
-45.3926456350353,-45.2054597333243,-45.0182835422868,-44.830679732397,
-44.7725157836192,-44.5849125950746,-44.3977008398437,-44.2105149381327,
-44.0233387470952,-43.8357349372054,-43.7775709884277,-43.5899677998832,
-43.4027560446523,-43.2155701429414,-43.0283939519039,-42.8407901420143,
-42.7826261932362,-42.5951562904176,-42.4080774892545,-42.221024314044,
-42.0339793110198,-41.8465084281791,-41.791653592194),.UNSPECIFIED.);
#980=B_SPLINE_CURVE_WITH_KNOTS('',3,(#83789,#83790,#83791,#83792,#83793,
#83794,#83795,#83796,#83797,#83798,#83799,#83800,#83801,#83802,#83803,#83804,
#83805,#83806,#83807,#83808,#83809,#83810,#83811,#83812,#83813,#83814,#83815,
#83816,#83817,#83818,#83819,#83820,#83821,#83822,#83823,#83824,#83825,#83826,
#83827,#83828,#83829,#83830,#83831,#83832,#83833,#83834,#83835,#83836,#83837,
#83838,#83839,#83840,#83841,#83842,#83843,#83844,#83845,#83846,#83847,#83848,
#83849,#83850,#83851,#83852,#83853,#83854,#83855,#83856,#83857,#83858,#83859,
#83860,#83861,#83862,#83863,#83864,#83865,#83866,#83867,#83868,#83869,#83870,
#83871,#83872,#83873,#83874,#83875,#83876,#83877,#83878,#83879,#83880,#83881,
#83882,#83883,#83884,#83885,#83886,#83887,#83888,#83889,#83890,#83891,#83892,
#83893,#83894,#83895,#83896,#83897,#83898,#83899,#83900,#83901,#83902,#83903),
 .UNSPECIFIED.,.F.,.F.,(4,3,3,3,3,3,3,3,3,3,3,3,3,3,3,3,3,3,3,3,3,3,3,3,
3,3,3,3,3,3,3,3,3,3,3,3,3,3,4),(-41.7916535919159,-41.6039138088844,-41.4165657069799,
-41.2292436594185,-41.0419328482664,-40.854192754235,-40.7927366028531,
-40.6051334143086,-40.4179216590777,-40.2307357573668,-40.0435595663293,
-39.8559557564396,-39.7977918076616,-39.610188619117,-39.4229768638861,
-39.2357909621751,-39.0486147711376,-38.8610109612479,-38.80284701247,-38.6152438239254,
-38.4280320686944,-38.2408461669834,-38.0536699759458,-37.8660661660561,
-37.8079022172785,-37.620299028734,-37.433087273503,-37.245901371792,-37.0587251807545,
-36.8711213708648,-36.8129574220869,-36.6253542335426,-36.4381424783119,
-36.2509565766011,-36.0637803855639,-35.8761765756744,-35.8180126268954,
-35.5941154784001,-35.5084682851079),.UNSPECIFIED.);
#981=B_SPLINE_CURVE_WITH_KNOTS('',3,(#83905,#83906,#83907,#83908,#83909,
#83910,#83911,#83912,#83913,#83914,#83915,#83916,#83917,#83918,#83919,#83920,
#83921,#83922,#83923,#83924,#83925,#83926,#83927,#83928,#83929,#83930,#83931,
#83932,#83933,#83934,#83935,#83936,#83937,#83938,#83939,#83940,#83941,#83942,
#83943,#83944,#83945,#83946,#83947,#83948,#83949,#83950,#83951,#83952,#83953,
#83954,#83955,#83956,#83957,#83958,#83959,#83960,#83961,#83962,#83963,#83964,
#83965,#83966,#83967,#83968,#83969,#83970,#83971,#83972,#83973,#83974,#83975,
#83976,#83977,#83978,#83979,#83980,#83981,#83982,#83983,#83984,#83985,#83986,
#83987,#83988,#83989,#83990,#83991,#83992,#83993,#83994,#83995,#83996,#83997,
#83998,#83999,#84000,#84001,#84002,#84003,#84004,#84005,#84006,#84007,#84008,
#84009,#84010,#84011,#84012,#84013,#84014,#84015,#84016,#84017,#84018,#84019),
 .UNSPECIFIED.,.F.,.F.,(4,3,3,3,3,3,3,3,3,3,3,3,3,3,3,3,3,3,3,3,3,3,3,3,
3,3,3,3,3,3,3,3,3,3,3,3,3,3,4),(-35.5084682847363,-35.3220367280429,-35.1356792786183,
-34.9488651523034,-34.8230678317039,-34.6354646431595,-34.4482528879287,
-34.2610669862178,-34.0738907951805,-33.8862869852908,-33.8281230365123,
-33.6405198479693,-33.45330809274,-33.2661221910306,-33.0789459999947,-32.8913421901065,
-32.8331782413208,-32.6455750527723,-32.4583632975375,-32.2711773958227,
-32.0840012047815,-31.896397394888,-31.8382334461292,-31.6506302575872,
-31.4634185023586,-31.27623260065,-31.0890564096147,-30.9014525997272,-30.8432886509377,
-30.6556854624021,-30.4684737071803,-30.2812878054784,-30.09411161445,-29.9065078045693,
-29.8483438557462,-29.6592690772485,-29.4706263248811,-29.2821819130397,
-29.2252829775567),.UNSPECIFIED.);
#982=B_SPLINE_CURVE_WITH_KNOTS('',3,(#84021,#84022,#84023,#84024,#84025,
#84026,#84027,#84028,#84029,#84030,#84031,#84032,#84033,#84034,#84035,#84036,
#84037,#84038,#84039,#84040,#84041,#84042,#84043,#84044,#84045,#84046,#84047,
#84048,#84049,#84050,#84051,#84052,#84053,#84054,#84055,#84056,#84057,#84058,
#84059,#84060,#84061,#84062,#84063,#84064,#84065,#84066,#84067,#84068,#84069,
#84070,#84071,#84072,#84073,#84074,#84075,#84076,#84077,#84078,#84079,#84080,
#84081,#84082,#84083,#84084,#84085,#84086,#84087,#84088,#84089,#84090,#84091,
#84092,#84093,#84094,#84095,#84096,#84097,#84098,#84099,#84100,#84101,#84102,
#84103,#84104,#84105,#84106,#84107,#84108,#84109,#84110,#84111,#84112,#84113,
#84114,#84115,#84116,#84117,#84118,#84119,#84120,#84121,#84122,#84123,#84124,
#84125,#84126,#84127,#84128,#84129,#84130,#84131,#84132),.UNSPECIFIED.,
 .F.,.F.,(4,3,3,3,3,3,3,3,3,3,3,3,3,3,3,3,3,3,3,3,3,3,3,3,3,3,3,3,3,3,3,
3,3,3,3,3,3,4),(-29.2252829771043,-29.0137239014305,-28.8533990605546,-28.6657958720351,
-28.4785841168289,-28.2913982151417,-28.1042220241277,-27.9166182142602,
-27.8584542653631,-27.6708510768672,-27.4836393216855,-27.2964534200241,
-27.1092772290363,-26.9216734191956,-26.8635094701716,-26.6759062814358,
-26.4886945260133,-26.3015086241134,-26.1143324328882,-25.9267286228161,
-25.86856467498,-25.680961486656,-25.4937497316436,-25.306563830145,-25.1193876393166,
-24.9317838296272,-24.8736198797885,-24.6860166914801,-24.4988049364903,
-24.311619035024,-24.1244428442335,-23.9368390345895,-23.8786750845969,
-23.6926863022266,-23.5050391443534,-23.3194703520081,-23.1307840113709,
-22.9420976707337),.UNSPECIFIED.);
#983=B_SPLINE_CURVE_WITH_KNOTS('',3,(#84134,#84135,#84136,#84137,#84138,
#84139,#84140,#84141,#84142,#84143,#84144,#84145,#84146,#84147,#84148,#84149,
#84150,#84151,#84152,#84153,#84154,#84155,#84156,#84157,#84158,#84159,#84160,
#84161,#84162,#84163,#84164,#84165,#84166,#84167,#84168,#84169,#84170,#84171,
#84172,#84173,#84174,#84175,#84176,#84177,#84178,#84179,#84180,#84181,#84182,
#84183,#84184,#84185,#84186,#84187,#84188,#84189,#84190,#84191,#84192,#84193,
#84194,#84195,#84196,#84197,#84198,#84199,#84200,#84201,#84202,#84203,#84204,
#84205,#84206,#84207,#84208,#84209,#84210,#84211,#84212,#84213,#84214,#84215,
#84216,#84217,#84218,#84219,#84220,#84221,#84222,#84223,#84224,#84225,#84226,
#84227,#84228,#84229,#84230,#84231,#84232,#84233,#84234,#84235,#84236,#84237,
#84238,#84239,#84240,#84241,#84242,#84243,#84244,#84245,#84246,#84247,#84248,
#84249,#84250,#84251),.UNSPECIFIED.,.F.,.F.,(4,3,3,3,3,3,3,3,3,3,3,3,3,
3,3,3,3,3,3,3,3,3,3,3,3,3,3,3,3,3,3,3,3,3,3,3,3,3,3,4),(-22.9420976703771,
-22.8837302894054,-22.6961271026793,-22.508915349255,-22.3217294493065,
-22.1345532600077,-21.9469494517905,-21.8887854942139,-21.7011823065751,
-21.5139705522857,-21.3267846515529,-21.1396084615158,-20.9520046526399,
-20.8938406990223,-20.7062375020042,-20.5190257382684,-20.3318398281365,
-20.1446636287185,-19.9570598106604,-19.8988959038308,-19.7112927295762,
-19.52408098857,-19.336895100777,-19.1497189234932,-18.9621151268684,-18.9039511086392,
-18.7163479211876,-18.5291361672979,-18.3419502672604,-18.1547740780903,
-17.9671702703128,-17.9090063134477,-17.7214030708108,-17.5341912612088,
-17.3470053055504,-17.1598290607591,-16.9722251983805,-16.9140615182562,
-16.6739534983264,-16.6589123634645),.UNSPECIFIED.);
#984=B_SPLINE_CURVE_WITH_KNOTS('',3,(#84253,#84254,#84255,#84256,#84257,
#84258,#84259,#84260,#84261,#84262,#84263,#84264,#84265,#84266,#84267,#84268,
#84269,#84270,#84271,#84272,#84273,#84274,#84275,#84276,#84277,#84278,#84279,
#84280,#84281,#84282,#84283,#84284,#84285,#84286,#84287,#84288,#84289,#84290,
#84291,#84292,#84293,#84294,#84295,#84296,#84297,#84298,#84299,#84300,#84301,
#84302,#84303,#84304,#84305,#84306,#84307,#84308,#84309,#84310,#84311,#84312,
#84313,#84314,#84315,#84316,#84317,#84318,#84319,#84320,#84321,#84322,#84323,
#84324,#84325,#84326,#84327,#84328,#84329,#84330,#84331,#84332,#84333,#84334,
#84335,#84336,#84337,#84338,#84339,#84340,#84341,#84342,#84343,#84344,#84345,
#84346,#84347,#84348,#84349,#84350,#84351,#84352,#84353,#84354,#84355,#84356,
#84357,#84358,#84359,#84360,#84361,#84362,#84363,#84364),.UNSPECIFIED.,
 .F.,.F.,(4,3,3,3,3,3,3,3,3,3,3,3,3,3,3,3,3,3,3,3,3,3,3,3,3,3,3,3,3,3,3,
3,3,3,3,3,3,4),(-16.6589123631975,-16.4736069552956,-16.2884618531051,-16.1028684349565,
-15.9191167230646,-15.7315135062259,-15.54430172438,-15.3571157988396,-15.169939585562,
-14.9823357561277,-14.9241719278731,-14.7365684055012,-14.5493563141293,
-14.3621700780567,-14.1749935533688,-13.9873894169731,-13.9292271326815,
-13.7416247391222,-13.5544137775851,-13.3672286557758,-13.1800532374019,
-12.9924501755822,-12.93428233749,-12.7466787107606,-12.5594665284143,-12.3722802217423,
-12.1851036381787,-11.9974994608632,-11.9393375422985,-11.7517323793176,
-11.5645186313735,-11.3773307410216,-11.1901525618073,-11.0025468008832,
-10.9443927471069,-10.7525085527175,-10.56110757904,-10.3757270560179),
 .UNSPECIFIED.);
#985=B_SPLINE_CURVE_WITH_KNOTS('',3,(#84365,#84366,#84367,#84368,#84369,
#84370,#84371,#84372,#84373,#84374),.UNSPECIFIED.,.F.,.F.,(4,1,1,1,1,1,
1,4),(-10.3757218525839,-9.94944795191539,-8.95450315672385,-7.95955836153231,
-6.96461356634077,-5.96966877114923,-4.97472397595769,-4.09254174883834),
 .UNSPECIFIED.);
#986=B_SPLINE_CURVE_WITH_KNOTS('',3,(#84377,#84378,#84379,#84380,#84381,
#84382,#84383),.UNSPECIFIED.,.F.,.F.,(4,1,1,1,4),(95.0999839528908,95.1907843151998,
96.1857291103914,97.1806739055829,97.3893722612836),.UNSPECIFIED.);
#987=B_SPLINE_CURVE_WITH_KNOTS('',3,(#84385,#84386,#84387,#84388,#84389,
#84390,#84391,#84392,#84393,#84394,#84395,#84396,#84397,#84398,#84399,#84400,
#84401,#84402,#84403,#84404,#84405,#84406,#84407,#84408,#84409,#84410,#84411,
#84412),.UNSPECIFIED.,.F.,.F.,(4,3,3,3,3,3,3,3,3,4),(97.3893724044164,97.5859339785059,
97.7815995754182,97.9786091380963,98.1756187007744,98.3723125568378,98.5687414387062,
98.7649953873722,98.9616717847817,99.0952857495152),.UNSPECIFIED.);
#988=B_SPLINE_CURVE_WITH_KNOTS('',3,(#84416,#84417,#84418,#84419,#84420,
#84421,#84422,#84423,#84424,#84425,#84426,#84427,#84428,#84429,#84430,#84431,
#84432,#84433,#84434,#84435),.UNSPECIFIED.,.F.,.F.,(4,2,2,2,2,2,2,2,2,4),
(0.000182933856833843,0.00211949330641253,0.00426999235183267,0.00836840074118015,
0.0151774046226676,0.0366484253322754,0.0654492646296514,0.0700723566601802,
0.0716586735729506,0.0730520430944184),.UNSPECIFIED.);
#989=B_SPLINE_CURVE_WITH_KNOTS('',3,(#84436,#84437,#84438,#84439,#84440,
#84441,#84442,#84443,#84444,#84445,#84446,#84447,#84448,#84449,#84450,#84451,
#84452,#84453,#84454,#84455,#84456,#84457,#84458,#84459,#84460,#84461,#84462,
#84463,#84464,#84465,#84466,#84467,#84468,#84469,#84470,#84471,#84472),
 .UNSPECIFIED.,.F.,.F.,(4,3,3,3,3,3,3,3,3,3,3,3,4),(95.1011120778127,95.2997246445013,
95.4981796586158,95.6971224053591,95.8657288995951,96.062179531293,96.2618030721664,
96.4578350224103,96.6592543585984,96.8606736947866,97.075180245871,97.2884928513503,
97.3893722612836),.UNSPECIFIED.);
#990=B_SPLINE_CURVE_WITH_KNOTS('',3,(#84845,#84846,#84847,#84848,#84849,
#84850,#84851,#84852,#84853,#84854,#84855,#84856,#84857,#84858,#84859,#84860,
#84861,#84862,#84863,#84864,#84865,#84866,#84867,#84868,#84869,#84870,#84871,
#84872,#84873,#84874,#84875,#84876,#84877,#84878,#84879,#84880,#84881,#84882,
#84883,#84884,#84885,#84886,#84887,#84888,#84889,#84890,#84891,#84892,#84893,
#84894,#84895,#84896,#84897,#84898,#84899),.UNSPECIFIED.,.F.,.F.,(4,3,3,
3,3,3,3,3,3,3,3,3,3,3,3,3,3,3,4),(-0.364609086663937,-0.349955759834691,
-0.322148792467856,-0.301818556032635,-0.269021332414628,-0.255281697682016,
-0.220959067372234,-0.202353981127163,-0.188377705920309,-0.186636437062452,
-0.165752269796004,-0.142062715941464,-0.129304435383701,-0.117755883775514,
-0.0883169128316359,-0.069851718219777,-0.0532071563521246,-0.020916945320546,
0.),.UNSPECIFIED.);
#991=B_SPLINE_CURVE_WITH_KNOTS('',3,(#84900,#84901,#84902,#84903,#84904,
#84905,#84906,#84907,#84908,#84909,#84910,#84911,#84912,#84913,#84914,#84915,
#84916,#84917,#84918,#84919,#84920,#84921,#84922,#84923,#84924,#84925,#84926,
#84927,#84928,#84929,#84930,#84931,#84932,#84933,#84934,#84935,#84936,#84937,
#84938,#84939,#84940,#84941,#84942,#84943,#84944,#84945,#84946,#84947,#84948,
#84949,#84950,#84951),.UNSPECIFIED.,.F.,.F.,(4,3,3,3,3,3,3,3,3,3,3,3,3,
3,3,3,3,4),(-0.366397579005849,-0.354487143711378,-0.327235825426289,-0.312257563612696,
-0.287192971194593,-0.271636001607225,-0.236484251747428,-0.218731998635388,
-0.204568081622605,-0.186662998246843,-0.163330123465988,-0.147055277061879,
-0.13340270893607,-0.100052031702053,-0.080940924208064,-0.0644514768169998,
-0.0259839405418483,-2.77882917038371E-15),.UNSPECIFIED.);
#992=B_SPLINE_CURVE_WITH_KNOTS('',3,(#84957,#84958,#84959,#84960,#84961,
#84962,#84963,#84964,#84965,#84966,#84967,#84968,#84969,#84970,#84971,#84972,
#84973,#84974,#84975,#84976,#84977,#84978,#84979,#84980,#84981,#84982,#84983,
#84984,#84985,#84986,#84987,#84988,#84989,#84990,#84991,#84992,#84993,#84994,
#84995,#84996,#84997,#84998,#84999,#85000,#85001,#85002,#85003,#85004,#85005,
#85006,#85007,#85008,#85009,#85010,#85011),.UNSPECIFIED.,.F.,.F.,(4,3,3,
3,3,3,3,3,3,3,3,3,3,3,3,3,3,3,4),(-0.361287482968457,-0.349955759834647,
-0.323048888644992,-0.302534193252467,-0.279099431199845,-0.265528167404287,
-0.252514851361878,-0.222201740894643,-0.202919079809183,-0.184570412842509,
-0.165752269795994,-0.142063101534203,-0.129304205568179,-0.117754438538821,
-0.0883158289041158,-0.0698511326658658,-0.0532073016903481,-0.0209171118703778,
0.),.UNSPECIFIED.);
#993=B_SPLINE_CURVE_WITH_KNOTS('',3,(#85384,#85385,#85386,#85387,#85388,
#85389,#85390,#85391,#85392,#85393,#85394,#85395,#85396,#85397,#85398,#85399,
#85400,#85401,#85402,#85403,#85404,#85405,#85406,#85407,#85408,#85409,#85410,
#85411,#85412,#85413,#85414,#85415,#85416,#85417,#85418,#85419,#85420,#85421,
#85422,#85423,#85424,#85425,#85426,#85427,#85428,#85429,#85430,#85431,#85432,
#85433,#85434,#85435),.UNSPECIFIED.,.F.,.F.,(4,3,3,3,3,3,3,3,3,3,3,3,3,
3,3,3,3,4),(-0.366397579005855,-0.354487143711385,-0.327235824669574,-0.312257556235388,
-0.287192226768709,-0.271635974620829,-0.23648422270589,-0.218732050894258,
-0.204568071899735,-0.186662998246842,-0.163330123465987,-0.147055270097115,
-0.133402728476446,-0.100052046357334,-0.0809409309648167,-0.0644514752458169,
-0.0259839471903043,0.),.UNSPECIFIED.);
#994=B_SPLINE_CURVE_WITH_KNOTS('',3,(#85436,#85437,#85438,#85439),
 .UNSPECIFIED.,.F.,.F.,(4,4),(0.,0.00337788989814126),.UNSPECIFIED.);
#995=PLANE('',#10108);
#996=PLANE('',#10113);
#997=PLANE('',#10122);
#998=PLANE('',#10126);
#999=PLANE('',#10180);
#1000=PLANE('',#10206);
#1001=PLANE('',#10217);
#1002=PLANE('',#10225);
#1003=PLANE('',#10245);
#1004=PLANE('',#10247);
#1005=PLANE('',#10264);
#1006=PLANE('',#10270);
#1007=PLANE('',#10272);
#1008=PLANE('',#10273);
#1009=PLANE('',#10294);
#1010=PLANE('',#10300);
#1011=PLANE('',#10301);
#1012=PLANE('',#10302);
#1013=PLANE('',#10304);
#1014=PLANE('',#10305);
#1015=PLANE('',#10306);
#1016=PLANE('',#10307);
#1017=PLANE('',#10308);
#1018=PLANE('',#10309);
#1019=PLANE('',#10310);
#1020=PLANE('',#10311);
#1021=PLANE('',#10312);
#1022=PLANE('',#10313);
#1023=PLANE('',#10314);
#1024=PLANE('',#10315);
#1025=PLANE('',#10316);
#1026=PLANE('',#10358);
#1027=PLANE('',#10359);
#1028=PLANE('',#10360);
#1029=PLANE('',#10361);
#1030=PLANE('',#10362);
#1031=PLANE('',#10363);
#1032=PLANE('',#10364);
#1033=PLANE('',#10365);
#1034=PLANE('',#10366);
#1035=PLANE('',#10367);
#1036=PLANE('',#10368);
#1037=PLANE('',#10369);
#1038=PLANE('',#10370);
#1039=PLANE('',#10371);
#1040=PLANE('',#10372);
#1041=PLANE('',#10373);
#1042=PLANE('',#10374);
#1043=PLANE('',#10375);
#1044=PLANE('',#10380);
#1045=PLANE('',#10384);
#1046=PLANE('',#10388);
#1047=PLANE('',#10392);
#1048=PLANE('',#10396);
#1049=PLANE('',#10400);
#1050=PLANE('',#10404);
#1051=PLANE('',#10408);
#1052=PLANE('',#10412);
#1053=PLANE('',#10416);
#1054=PLANE('',#10420);
#1055=PLANE('',#10424);
#1056=PLANE('',#10443);
#1057=PLANE('',#10444);
#1058=PLANE('',#10445);
#1059=PLANE('',#10446);
#1060=PLANE('',#10447);
#1061=PLANE('',#10448);
#1062=PLANE('',#10449);
#1063=PLANE('',#10450);
#1064=PLANE('',#10451);
#1065=PLANE('',#10452);
#1066=PLANE('',#10454);
#1067=PLANE('',#10455);
#1068=PLANE('',#10456);
#1069=PLANE('',#10457);
#1070=PLANE('',#10458);
#1071=PLANE('',#10459);
#1072=PLANE('',#10460);
#1073=PLANE('',#10461);
#1074=PLANE('',#10462);
#1075=PLANE('',#10463);
#1076=PLANE('',#10476);
#1077=PLANE('',#10477);
#1078=PLANE('',#10478);
#1079=PLANE('',#10479);
#1080=PLANE('',#10489);
#1081=PLANE('',#10490);
#1082=PLANE('',#10491);
#1083=PLANE('',#10492);
#1084=PLANE('',#10493);
#1085=PLANE('',#10494);
#1086=PLANE('',#10495);
#1087=PLANE('',#10496);
#1088=PLANE('',#10497);
#1089=PLANE('',#10498);
#1090=PLANE('',#10503);
#1091=PLANE('',#10509);
#1092=PLANE('',#10515);
#1093=PLANE('',#10520);
#1094=PLANE('',#10526);
#1095=PLANE('',#10527);
#1096=PLANE('',#10528);
#1097=PLANE('',#10529);
#1098=PLANE('',#10530);
#1099=PLANE('',#10531);
#1100=PLANE('',#10543);
#1101=PLANE('',#10546);
#1102=PLANE('',#10548);
#1103=PLANE('',#10550);
#1104=PLANE('',#10556);
#1105=PLANE('',#10557);
#1106=PLANE('',#10558);
#1107=PLANE('',#10559);
#1108=PLANE('',#10560);
#1109=PLANE('',#10561);
#1110=PLANE('',#10563);
#1111=PLANE('',#10564);
#1112=PLANE('',#10571);
#1113=PLANE('',#10575);
#1114=PLANE('',#10579);
#1115=PLANE('',#10587);
#1116=PLANE('',#10591);
#1117=PLANE('',#10595);
#1118=PLANE('',#10599);
#1119=PLANE('',#10600);
#1120=PLANE('',#10601);
#1121=PLANE('',#10602);
#1122=PLANE('',#10604);
#1123=PLANE('',#10618);
#1124=PLANE('',#10619);
#1125=PLANE('',#10620);
#1126=PLANE('',#10621);
#1127=PLANE('',#10625);
#1128=PLANE('',#10626);
#1129=PLANE('',#10627);
#1130=PLANE('',#10628);
#1131=PLANE('',#10632);
#1132=PLANE('',#10633);
#1133=PLANE('',#10634);
#1134=PLANE('',#10635);
#1135=PLANE('',#10640);
#1136=PLANE('',#10641);
#1137=PLANE('',#10642);
#1138=PLANE('',#10643);
#1139=PLANE('',#10647);
#1140=PLANE('',#10648);
#1141=PLANE('',#10649);
#1142=PLANE('',#10650);
#1143=PLANE('',#10654);
#1144=PLANE('',#10655);
#1145=PLANE('',#10656);
#1146=PLANE('',#10657);
#1147=PLANE('',#10661);
#1148=PLANE('',#10662);
#1149=PLANE('',#10663);
#1150=PLANE('',#10664);
#1151=PLANE('',#10669);
#1152=PLANE('',#10673);
#1153=PLANE('',#10678);
#1154=PLANE('',#10680);
#1155=PLANE('',#10681);
#1156=PLANE('',#10682);
#1157=PLANE('',#10683);
#1158=PLANE('',#10690);
#1159=PLANE('',#10697);
#1160=PLANE('',#10701);
#1161=PLANE('',#10705);
#1162=PLANE('',#10713);
#1163=PLANE('',#10717);
#1164=PLANE('',#10721);
#1165=PLANE('',#10730);
#1166=PLANE('',#10738);
#1167=PLANE('',#10742);
#1168=PLANE('',#10748);
#1169=PLANE('',#10752);
#1170=PLANE('',#10758);
#1171=PLANE('',#10760);
#1172=PLANE('',#10766);
#1173=PLANE('',#10770);
#1174=PLANE('',#10776);
#1175=PLANE('',#10784);
#1176=PLANE('',#10785);
#1177=PLANE('',#10809);
#1178=PLANE('',#10842);
#1179=PLANE('',#10843);
#1180=PLANE('',#10844);
#1181=PLANE('',#10845);
#1182=PLANE('',#10846);
#1183=PLANE('',#10847);
#1184=PLANE('',#10848);
#1185=PLANE('',#10849);
#1186=PLANE('',#10852);
#1187=PLANE('',#10856);
#1188=PLANE('',#10857);
#1189=PLANE('',#10858);
#1190=PLANE('',#10859);
#1191=PLANE('',#10875);
#1192=PLANE('',#10891);
#1193=PLANE('',#10893);
#1194=PLANE('',#10894);
#1195=PLANE('',#10895);
#1196=PLANE('',#10896);
#1197=PLANE('',#10912);
#1198=PLANE('',#10928);
#1199=LINE('',#13229,#1735);
#1200=LINE('',#13236,#1736);
#1201=LINE('',#13243,#1737);
#1202=LINE('',#13245,#1738);
#1203=LINE('',#13306,#1739);
#1204=LINE('',#13414,#1740);
#1205=LINE('',#13421,#1741);
#1206=LINE('',#13431,#1742);
#1207=LINE('',#13626,#1743);
#1208=LINE('',#13662,#1744);
#1209=LINE('',#13665,#1745);
#1210=LINE('',#13697,#1746);
#1211=LINE('',#14824,#1747);
#1212=LINE('',#15430,#1748);
#1213=LINE('',#15655,#1749);
#1214=LINE('',#15961,#1750);
#1215=LINE('',#16625,#1751);
#1216=LINE('',#17097,#1752);
#1217=LINE('',#17753,#1753);
#1218=LINE('',#17756,#1754);
#1219=LINE('',#17768,#1755);
#1220=LINE('',#17783,#1756);
#1221=LINE('',#17784,#1757);
#1222=LINE('',#18904,#1758);
#1223=LINE('',#20174,#1759);
#1224=LINE('',#20177,#1760);
#1225=LINE('',#20445,#1761);
#1226=LINE('',#20760,#1762);
#1227=LINE('',#20764,#1763);
#1228=LINE('',#21021,#1764);
#1229=LINE('',#21030,#1765);
#1230=LINE('',#21032,#1766);
#1231=LINE('',#21042,#1767);
#1232=LINE('',#21049,#1768);
#1233=LINE('',#21060,#1769);
#1234=LINE('',#21066,#1770);
#1235=LINE('',#21069,#1771);
#1236=LINE('',#21072,#1772);
#1237=LINE('',#21074,#1773);
#1238=LINE('',#21081,#1774);
#1239=LINE('',#21085,#1775);
#1240=LINE('',#21095,#1776);
#1241=LINE('',#21097,#1777);
#1242=LINE('',#21136,#1778);
#1243=LINE('',#21162,#1779);
#1244=LINE('',#21169,#1780);
#1245=LINE('',#21170,#1781);
#1246=LINE('',#21176,#1782);
#1247=LINE('',#21177,#1783);
#1248=LINE('',#21179,#1784);
#1249=LINE('',#21851,#1785);
#1250=LINE('',#22028,#1786);
#1251=LINE('',#22045,#1787);
#1252=LINE('',#22082,#1788);
#1253=LINE('',#22116,#1789);
#1254=LINE('',#22623,#1790);
#1255=LINE('',#22650,#1791);
#1256=LINE('',#22795,#1792);
#1257=LINE('',#22798,#1793);
#1258=LINE('',#23320,#1794);
#1259=LINE('',#23322,#1795);
#1260=LINE('',#23324,#1796);
#1261=LINE('',#23326,#1797);
#1262=LINE('',#23334,#1798);
#1263=LINE('',#23336,#1799);
#1264=LINE('',#23338,#1800);
#1265=LINE('',#23339,#1801);
#1266=LINE('',#23342,#1802);
#1267=LINE('',#23344,#1803);
#1268=LINE('',#23345,#1804);
#1269=LINE('',#23348,#1805);
#1270=LINE('',#23350,#1806);
#1271=LINE('',#23351,#1807);
#1272=LINE('',#23354,#1808);
#1273=LINE('',#23356,#1809);
#1274=LINE('',#23357,#1810);
#1275=LINE('',#23360,#1811);
#1276=LINE('',#23362,#1812);
#1277=LINE('',#23363,#1813);
#1278=LINE('',#23366,#1814);
#1279=LINE('',#23368,#1815);
#1280=LINE('',#23369,#1816);
#1281=LINE('',#23372,#1817);
#1282=LINE('',#23374,#1818);
#1283=LINE('',#23375,#1819);
#1284=LINE('',#23377,#1820);
#1285=LINE('',#23378,#1821);
#1286=LINE('',#23381,#1822);
#1287=LINE('',#23383,#1823);
#1288=LINE('',#23384,#1824);
#1289=LINE('',#23387,#1825);
#1290=LINE('',#23388,#1826);
#1291=LINE('',#23391,#1827);
#1292=LINE('',#23392,#1828);
#1293=LINE('',#23395,#1829);
#1294=LINE('',#23396,#1830);
#1295=LINE('',#23400,#1831);
#1296=LINE('',#23402,#1832);
#1297=LINE('',#23404,#1833);
#1298=LINE('',#23406,#1834);
#1299=LINE('',#23408,#1835);
#1300=LINE('',#23410,#1836);
#1301=LINE('',#23412,#1837);
#1302=LINE('',#23414,#1838);
#1303=LINE('',#23416,#1839);
#1304=LINE('',#23418,#1840);
#1305=LINE('',#23420,#1841);
#1306=LINE('',#23421,#1842);
#1307=LINE('',#23437,#1843);
#1308=LINE('',#23441,#1844);
#1309=LINE('',#23444,#1845);
#1310=LINE('',#23448,#1846);
#1311=LINE('',#23452,#1847);
#1312=LINE('',#23455,#1848);
#1313=LINE('',#23459,#1849);
#1314=LINE('',#23463,#1850);
#1315=LINE('',#23466,#1851);
#1316=LINE('',#23470,#1852);
#1317=LINE('',#23474,#1853);
#1318=LINE('',#23477,#1854);
#1319=LINE('',#23481,#1855);
#1320=LINE('',#23485,#1856);
#1321=LINE('',#23490,#1857);
#1322=LINE('',#23494,#1858);
#1323=LINE('',#23499,#1859);
#1324=LINE('',#23503,#1860);
#1325=LINE('',#23508,#1861);
#1326=LINE('',#23512,#1862);
#1327=LINE('',#23514,#1863);
#1328=LINE('',#23515,#1864);
#1329=LINE('',#23518,#1865);
#1330=LINE('',#23519,#1866);
#1331=LINE('',#23522,#1867);
#1332=LINE('',#23523,#1868);
#1333=LINE('',#23526,#1869);
#1334=LINE('',#23527,#1870);
#1335=LINE('',#23530,#1871);
#1336=LINE('',#23531,#1872);
#1337=LINE('',#23534,#1873);
#1338=LINE('',#23535,#1874);
#1339=LINE('',#23538,#1875);
#1340=LINE('',#23539,#1876);
#1341=LINE('',#23542,#1877);
#1342=LINE('',#23543,#1878);
#1343=LINE('',#23546,#1879);
#1344=LINE('',#23547,#1880);
#1345=LINE('',#23550,#1881);
#1346=LINE('',#23551,#1882);
#1347=LINE('',#23554,#1883);
#1348=LINE('',#23555,#1884);
#1349=LINE('',#23557,#1885);
#1350=LINE('',#23561,#1886);
#1351=LINE('',#23562,#1887);
#1352=LINE('',#23565,#1888);
#1353=LINE('',#23566,#1889);
#1354=LINE('',#23569,#1890);
#1355=LINE('',#23570,#1891);
#1356=LINE('',#23572,#1892);
#1357=LINE('',#23580,#1893);
#1358=LINE('',#23583,#1894);
#1359=LINE('',#23586,#1895);
#1360=LINE('',#23588,#1896);
#1361=LINE('',#23589,#1897);
#1362=LINE('',#23595,#1898);
#1363=LINE('',#23598,#1899);
#1364=LINE('',#23600,#1900);
#1365=LINE('',#23601,#1901);
#1366=LINE('',#23606,#1902);
#1367=LINE('',#23610,#1903);
#1368=LINE('',#23612,#1904);
#1369=LINE('',#23613,#1905);
#1370=LINE('',#23618,#1906);
#1371=LINE('',#23621,#1907);
#1372=LINE('',#23622,#1908);
#1373=LINE('',#23628,#1909);
#1374=LINE('',#23631,#1910);
#1375=LINE('',#23634,#1911);
#1376=LINE('',#23636,#1912);
#1377=LINE('',#23637,#1913);
#1378=LINE('',#23643,#1914);
#1379=LINE('',#23646,#1915);
#1380=LINE('',#23648,#1916);
#1381=LINE('',#23649,#1917);
#1382=LINE('',#23654,#1918);
#1383=LINE('',#23658,#1919);
#1384=LINE('',#23660,#1920);
#1385=LINE('',#23661,#1921);
#1386=LINE('',#23666,#1922);
#1387=LINE('',#23669,#1923);
#1388=LINE('',#23670,#1924);
#1389=LINE('',#23676,#1925);
#1390=LINE('',#23679,#1926);
#1391=LINE('',#23682,#1927);
#1392=LINE('',#23684,#1928);
#1393=LINE('',#23685,#1929);
#1394=LINE('',#23691,#1930);
#1395=LINE('',#23694,#1931);
#1396=LINE('',#23696,#1932);
#1397=LINE('',#23697,#1933);
#1398=LINE('',#23702,#1934);
#1399=LINE('',#23706,#1935);
#1400=LINE('',#23708,#1936);
#1401=LINE('',#23709,#1937);
#1402=LINE('',#23714,#1938);
#1403=LINE('',#23717,#1939);
#1404=LINE('',#23718,#1940);
#1405=LINE('',#23723,#1941);
#1406=LINE('',#23729,#1942);
#1407=LINE('',#23735,#1943);
#1408=LINE('',#23741,#1944);
#1409=LINE('',#23747,#1945);
#1410=LINE('',#23753,#1946);
#1411=LINE('',#23758,#1947);
#1412=LINE('',#23760,#1948);
#1413=LINE('',#23762,#1949);
#1414=LINE('',#23763,#1950);
#1415=LINE('',#23766,#1951);
#1416=LINE('',#23768,#1952);
#1417=LINE('',#23769,#1953);
#1418=LINE('',#23772,#1954);
#1419=LINE('',#23774,#1955);
#1420=LINE('',#23775,#1956);
#1421=LINE('',#23778,#1957);
#1422=LINE('',#23780,#1958);
#1423=LINE('',#23781,#1959);
#1424=LINE('',#23784,#1960);
#1425=LINE('',#23786,#1961);
#1426=LINE('',#23787,#1962);
#1427=LINE('',#23790,#1963);
#1428=LINE('',#23792,#1964);
#1429=LINE('',#23793,#1965);
#1430=LINE('',#23796,#1966);
#1431=LINE('',#23798,#1967);
#1432=LINE('',#23799,#1968);
#1433=LINE('',#23801,#1969);
#1434=LINE('',#23802,#1970);
#1435=LINE('',#23809,#1971);
#1436=LINE('',#23811,#1972);
#1437=LINE('',#23813,#1973);
#1438=LINE('',#23814,#1974);
#1439=LINE('',#23817,#1975);
#1440=LINE('',#23819,#1976);
#1441=LINE('',#23820,#1977);
#1442=LINE('',#23823,#1978);
#1443=LINE('',#23825,#1979);
#1444=LINE('',#23826,#1980);
#1445=LINE('',#23829,#1981);
#1446=LINE('',#23831,#1982);
#1447=LINE('',#23832,#1983);
#1448=LINE('',#23835,#1984);
#1449=LINE('',#23837,#1985);
#1450=LINE('',#23838,#1986);
#1451=LINE('',#23840,#1987);
#1452=LINE('',#23841,#1988);
#1453=LINE('',#23844,#1989);
#1454=LINE('',#23846,#1990);
#1455=LINE('',#23847,#1991);
#1456=LINE('',#23850,#1992);
#1457=LINE('',#23851,#1993);
#1458=LINE('',#23854,#1994);
#1459=LINE('',#23855,#1995);
#1460=LINE('',#23868,#1996);
#1461=LINE('',#23872,#1997);
#1462=LINE('',#23876,#1998);
#1463=LINE('',#23880,#1999);
#1464=LINE('',#23883,#2000);
#1465=LINE('',#23884,#2001);
#1466=LINE('',#23887,#2002);
#1467=LINE('',#23888,#2003);
#1468=LINE('',#23890,#2004);
#1469=LINE('',#71757,#2005);
#1470=LINE('',#71759,#2006);
#1471=LINE('',#71761,#2007);
#1472=LINE('',#71762,#2008);
#1473=LINE('',#71765,#2009);
#1474=LINE('',#71767,#2010);
#1475=LINE('',#71768,#2011);
#1476=LINE('',#71771,#2012);
#1477=LINE('',#71773,#2013);
#1478=LINE('',#71774,#2014);
#1479=LINE('',#71777,#2015);
#1480=LINE('',#71779,#2016);
#1481=LINE('',#71780,#2017);
#1482=LINE('',#71783,#2018);
#1483=LINE('',#71785,#2019);
#1484=LINE('',#71786,#2020);
#1485=LINE('',#71788,#2021);
#1486=LINE('',#71789,#2022);
#1487=LINE('',#75719,#2023);
#1488=LINE('',#75722,#2024);
#1489=LINE('',#75731,#2025);
#1490=LINE('',#75735,#2026);
#1491=LINE('',#75740,#2027);
#1492=LINE('',#75748,#2028);
#1493=LINE('',#75751,#2029);
#1494=LINE('',#75753,#2030);
#1495=LINE('',#75754,#2031);
#1496=LINE('',#75760,#2032);
#1497=LINE('',#75764,#2033);
#1498=LINE('',#75769,#2034);
#1499=LINE('',#75777,#2035);
#1500=LINE('',#75780,#2036);
#1501=LINE('',#75782,#2037);
#1502=LINE('',#75783,#2038);
#1503=LINE('',#75786,#2039);
#1504=LINE('',#75788,#2040);
#1505=LINE('',#75790,#2041);
#1506=LINE('',#75791,#2042);
#1507=LINE('',#75794,#2043);
#1508=LINE('',#75796,#2044);
#1509=LINE('',#75797,#2045);
#1510=LINE('',#75800,#2046);
#1511=LINE('',#75801,#2047);
#1512=LINE('',#75804,#2048);
#1513=LINE('',#75805,#2049);
#1514=LINE('',#75807,#2050);
#1515=LINE('',#75813,#2051);
#1516=LINE('',#75910,#2052);
#1517=LINE('',#75916,#2053);
#1518=LINE('',#75997,#2054);
#1519=LINE('',#76002,#2055);
#1520=LINE('',#76003,#2056);
#1521=LINE('',#76005,#2057);
#1522=LINE('',#76009,#2058);
#1523=LINE('',#76017,#2059);
#1524=LINE('',#76024,#2060);
#1525=LINE('',#76029,#2061);
#1526=LINE('',#76031,#2062);
#1527=LINE('',#76033,#2063);
#1528=LINE('',#76035,#2064);
#1529=LINE('',#77333,#2065);
#1530=LINE('',#77337,#2066);
#1531=LINE('',#77345,#2067);
#1532=LINE('',#77352,#2068);
#1533=LINE('',#77359,#2069);
#1534=LINE('',#77363,#2070);
#1535=LINE('',#77366,#2071);
#1536=LINE('',#77374,#2072);
#1537=LINE('',#77381,#2073);
#1538=LINE('',#77386,#2074);
#1539=LINE('',#77391,#2075);
#1540=LINE('',#77393,#2076);
#1541=LINE('',#77395,#2077);
#1542=LINE('',#77397,#2078);
#1543=LINE('',#77404,#2079);
#1544=LINE('',#77410,#2080);
#1545=LINE('',#77412,#2081);
#1546=LINE('',#77413,#2082);
#1547=LINE('',#77415,#2083);
#1548=LINE('',#77416,#2084);
#1549=LINE('',#77423,#2085);
#1550=LINE('',#77425,#2086);
#1551=LINE('',#77427,#2087);
#1552=LINE('',#77431,#2088);
#1553=LINE('',#77433,#2089);
#1554=LINE('',#77435,#2090);
#1555=LINE('',#77439,#2091);
#1556=LINE('',#77441,#2092);
#1557=LINE('',#77443,#2093);
#1558=LINE('',#77447,#2094);
#1559=LINE('',#77449,#2095);
#1560=LINE('',#77451,#2096);
#1561=LINE('',#77455,#2097);
#1562=LINE('',#77457,#2098);
#1563=LINE('',#77459,#2099);
#1564=LINE('',#77463,#2100);
#1565=LINE('',#77465,#2101);
#1566=LINE('',#77467,#2102);
#1567=LINE('',#77471,#2103);
#1568=LINE('',#77473,#2104);
#1569=LINE('',#77475,#2105);
#1570=LINE('',#77494,#2106);
#1571=LINE('',#77496,#2107);
#1572=LINE('',#77497,#2108);
#1573=LINE('',#77503,#2109);
#1574=LINE('',#77505,#2110);
#1575=LINE('',#77506,#2111);
#1576=LINE('',#77508,#2112);
#1577=LINE('',#77520,#2113);
#1578=LINE('',#77522,#2114);
#1579=LINE('',#77523,#2115);
#1580=LINE('',#77529,#2116);
#1581=LINE('',#77531,#2117);
#1582=LINE('',#77532,#2118);
#1583=LINE('',#77534,#2119);
#1584=LINE('',#77546,#2120);
#1585=LINE('',#77548,#2121);
#1586=LINE('',#77549,#2122);
#1587=LINE('',#77555,#2123);
#1588=LINE('',#77557,#2124);
#1589=LINE('',#77558,#2125);
#1590=LINE('',#77560,#2126);
#1591=LINE('',#77574,#2127);
#1592=LINE('',#77576,#2128);
#1593=LINE('',#77577,#2129);
#1594=LINE('',#77583,#2130);
#1595=LINE('',#77585,#2131);
#1596=LINE('',#77586,#2132);
#1597=LINE('',#77588,#2133);
#1598=LINE('',#77600,#2134);
#1599=LINE('',#77602,#2135);
#1600=LINE('',#77603,#2136);
#1601=LINE('',#77609,#2137);
#1602=LINE('',#77611,#2138);
#1603=LINE('',#77612,#2139);
#1604=LINE('',#77614,#2140);
#1605=LINE('',#77625,#2141);
#1606=LINE('',#77627,#2142);
#1607=LINE('',#77628,#2143);
#1608=LINE('',#77635,#2144);
#1609=LINE('',#77637,#2145);
#1610=LINE('',#77638,#2146);
#1611=LINE('',#77640,#2147);
#1612=LINE('',#77651,#2148);
#1613=LINE('',#77653,#2149);
#1614=LINE('',#77654,#2150);
#1615=LINE('',#77657,#2151);
#1616=LINE('',#77659,#2152);
#1617=LINE('',#77660,#2153);
#1618=LINE('',#77662,#2154);
#1619=LINE('',#77669,#2155);
#1620=LINE('',#77676,#2156);
#1621=LINE('',#77682,#2157);
#1622=LINE('',#77686,#2158);
#1623=LINE('',#77692,#2159);
#1624=LINE('',#77694,#2160);
#1625=LINE('',#77696,#2161);
#1626=LINE('',#77697,#2162);
#1627=LINE('',#77701,#2163);
#1628=LINE('',#77703,#2164);
#1629=LINE('',#77705,#2165);
#1630=LINE('',#77706,#2166);
#1631=LINE('',#77708,#2167);
#1632=LINE('',#77709,#2168);
#1633=LINE('',#77717,#2169);
#1634=LINE('',#77726,#2170);
#1635=LINE('',#77730,#2171);
#1636=LINE('',#77738,#2172);
#1637=LINE('',#77745,#2173);
#1638=LINE('',#77752,#2174);
#1639=LINE('',#77756,#2175);
#1640=LINE('',#77759,#2176);
#1641=LINE('',#77767,#2177);
#1642=LINE('',#77774,#2178);
#1643=LINE('',#77779,#2179);
#1644=LINE('',#77785,#2180);
#1645=LINE('',#77789,#2181);
#1646=LINE('',#77797,#2182);
#1647=LINE('',#77801,#2183);
#1648=LINE('',#77804,#2184);
#1649=LINE('',#77810,#2185);
#1650=LINE('',#77818,#2186);
#1651=LINE('',#77822,#2187);
#1652=LINE('',#77829,#2188);
#1653=LINE('',#77836,#2189);
#1654=LINE('',#77839,#2190);
#1655=LINE('',#77849,#2191);
#1656=LINE('',#77853,#2192);
#1657=LINE('',#77860,#2193);
#1658=LINE('',#77867,#2194);
#1659=LINE('',#77870,#2195);
#1660=LINE('',#77882,#2196);
#1661=LINE('',#77889,#2197);
#1662=LINE('',#77894,#2198);
#1663=LINE('',#77978,#2199);
#1664=LINE('',#78246,#2200);
#1665=LINE('',#78539,#2201);
#1666=LINE('',#78861,#2202);
#1667=LINE('',#79158,#2203);
#1668=LINE('',#79481,#2204);
#1669=LINE('',#79786,#2205);
#1670=LINE('',#80093,#2206);
#1671=LINE('',#80394,#2207);
#1672=LINE('',#80721,#2208);
#1673=LINE('',#81016,#2209);
#1674=LINE('',#81332,#2210);
#1675=LINE('',#81634,#2211);
#1676=LINE('',#85509,#2212);
#1677=LINE('',#85513,#2213);
#1678=LINE('',#85515,#2214);
#1679=LINE('',#85516,#2215);
#1680=LINE('',#85519,#2216);
#1681=LINE('',#85520,#2217);
#1682=LINE('',#85523,#2218);
#1683=LINE('',#85524,#2219);
#1684=LINE('',#85527,#2220);
#1685=LINE('',#85528,#2221);
#1686=LINE('',#85531,#2222);
#1687=LINE('',#85532,#2223);
#1688=LINE('',#85534,#2224);
#1689=LINE('',#85540,#2225);
#1690=LINE('',#85545,#2226);
#1691=LINE('',#85550,#2227);
#1692=LINE('',#85552,#2228);
#1693=LINE('',#85554,#2229);
#1694=LINE('',#85555,#2230);
#1695=LINE('',#85559,#2231);
#1696=LINE('',#85561,#2232);
#1697=LINE('',#85563,#2233);
#1698=LINE('',#85564,#2234);
#1699=LINE('',#85568,#2235);
#1700=LINE('',#85570,#2236);
#1701=LINE('',#85572,#2237);
#1702=LINE('',#85573,#2238);
#1703=LINE('',#85577,#2239);
#1704=LINE('',#85579,#2240);
#1705=LINE('',#85581,#2241);
#1706=LINE('',#85582,#2242);
#1707=LINE('',#85587,#2243);
#1708=LINE('',#85593,#2244);
#1709=LINE('',#85599,#2245);
#1710=LINE('',#85605,#2246);
#1711=LINE('',#85623,#2247);
#1712=LINE('',#85627,#2248);
#1713=LINE('',#85637,#2249);
#1714=LINE('',#85639,#2250);
#1715=LINE('',#85641,#2251);
#1716=LINE('',#85642,#2252);
#1717=LINE('',#85646,#2253);
#1718=LINE('',#85648,#2254);
#1719=LINE('',#85650,#2255);
#1720=LINE('',#85651,#2256);
#1721=LINE('',#85655,#2257);
#1722=LINE('',#85657,#2258);
#1723=LINE('',#85659,#2259);
#1724=LINE('',#85660,#2260);
#1725=LINE('',#85664,#2261);
#1726=LINE('',#85666,#2262);
#1727=LINE('',#85668,#2263);
#1728=LINE('',#85669,#2264);
#1729=LINE('',#85674,#2265);
#1730=LINE('',#85680,#2266);
#1731=LINE('',#85686,#2267);
#1732=LINE('',#85692,#2268);
#1733=LINE('',#85710,#2269);
#1734=LINE('',#85714,#2270);
#1735=VECTOR('',#10975,1.35);
#1736=VECTOR('',#10982,1.);
#1737=VECTOR('',#10983,1.);
#1738=VECTOR('',#10984,1.);
#1739=VECTOR('',#10995,1.);
#1740=VECTOR('',#11008,1.35);
#1741=VECTOR('',#11015,1.);
#1742=VECTOR('',#11016,1.);
#1743=VECTOR('',#11025,1.);
#1744=VECTOR('',#11026,1.);
#1745=VECTOR('',#11029,1.);
#1746=VECTOR('',#11034,1.);
#1747=VECTOR('',#11075,1.);
#1748=VECTOR('',#11088,1.);
#1749=VECTOR('',#11089,1.);
#1750=VECTOR('',#11110,1.);
#1751=VECTOR('',#11113,1.);
#1752=VECTOR('',#11142,1.);
#1753=VECTOR('',#11145,1.);
#1754=VECTOR('',#11150,1.);
#1755=VECTOR('',#11151,1.);
#1756=VECTOR('',#11156,1.);
#1757=VECTOR('',#11157,1.);
#1758=VECTOR('',#11186,1.);
#1759=VECTOR('',#11203,1.);
#1760=VECTOR('',#11206,1.);
#1761=VECTOR('',#11219,1.);
#1762=VECTOR('',#11226,1.);
#1763=VECTOR('',#11231,1.);
#1764=VECTOR('',#11242,1.);
#1765=VECTOR('',#11245,1.);
#1766=VECTOR('',#11246,1.);
#1767=VECTOR('',#11251,1.);
#1768=VECTOR('',#11252,1.);
#1769=VECTOR('',#11263,1.);
#1770=VECTOR('',#11270,1.);
#1771=VECTOR('',#11273,1.);
#1772=VECTOR('',#11276,1.);
#1773=VECTOR('',#11279,1.);
#1774=VECTOR('',#11290,1.);
#1775=VECTOR('',#11295,1.);
#1776=VECTOR('',#11296,1.);
#1777=VECTOR('',#11299,1.);
#1778=VECTOR('',#11302,1.);
#1779=VECTOR('',#11303,1.);
#1780=VECTOR('',#11304,1.);
#1781=VECTOR('',#11305,1.);
#1782=VECTOR('',#11306,1.);
#1783=VECTOR('',#11307,1.);
#1784=VECTOR('',#11308,1.);
#1785=VECTOR('',#11337,1.);
#1786=VECTOR('',#11352,1.);
#1787=VECTOR('',#11353,1.);
#1788=VECTOR('',#11354,1.);
#1789=VECTOR('',#11365,1.);
#1790=VECTOR('',#11394,1.);
#1791=VECTOR('',#11395,1.);
#1792=VECTOR('',#11408,1.);
#1793=VECTOR('',#11413,1.);
#1794=VECTOR('',#11416,0.3);
#1795=VECTOR('',#11419,0.36);
#1796=VECTOR('',#11422,0.36);
#1797=VECTOR('',#11425,0.3);
#1798=VECTOR('',#11436,1.);
#1799=VECTOR('',#11437,1.);
#1800=VECTOR('',#11438,1.);
#1801=VECTOR('',#11439,0.999999999999999);
#1802=VECTOR('',#11442,1.);
#1803=VECTOR('',#11443,1.);
#1804=VECTOR('',#11444,1.);
#1805=VECTOR('',#11447,1.);
#1806=VECTOR('',#11448,1.);
#1807=VECTOR('',#11449,1.);
#1808=VECTOR('',#11452,1.);
#1809=VECTOR('',#11453,1.);
#1810=VECTOR('',#11454,1.);
#1811=VECTOR('',#11457,1.);
#1812=VECTOR('',#11458,1.);
#1813=VECTOR('',#11459,1.);
#1814=VECTOR('',#11462,1.);
#1815=VECTOR('',#11463,1.);
#1816=VECTOR('',#11464,1.);
#1817=VECTOR('',#11467,1.);
#1818=VECTOR('',#11468,1.);
#1819=VECTOR('',#11469,1.);
#1820=VECTOR('',#11472,1.);
#1821=VECTOR('',#11473,1.);
#1822=VECTOR('',#11476,1.);
#1823=VECTOR('',#11477,1.);
#1824=VECTOR('',#11478,1.);
#1825=VECTOR('',#11481,1.);
#1826=VECTOR('',#11482,1.);
#1827=VECTOR('',#11485,1.);
#1828=VECTOR('',#11486,1.);
#1829=VECTOR('',#11489,1.);
#1830=VECTOR('',#11490,1.);
#1831=VECTOR('',#11493,1.);
#1832=VECTOR('',#11494,1.);
#1833=VECTOR('',#11495,1.);
#1834=VECTOR('',#11496,1.);
#1835=VECTOR('',#11497,1.);
#1836=VECTOR('',#11498,1.);
#1837=VECTOR('',#11499,1.);
#1838=VECTOR('',#11500,1.);
#1839=VECTOR('',#11501,1.);
#1840=VECTOR('',#11502,1.);
#1841=VECTOR('',#11503,1.);
#1842=VECTOR('',#11504,1.);
#1843=VECTOR('',#11519,0.1025);
#1844=VECTOR('',#11524,0.205);
#1845=VECTOR('',#11529,0.255);
#1846=VECTOR('',#11532,0.1025);
#1847=VECTOR('',#11537,0.205);
#1848=VECTOR('',#11542,0.255);
#1849=VECTOR('',#11545,0.1025);
#1850=VECTOR('',#11550,0.205);
#1851=VECTOR('',#11555,0.255);
#1852=VECTOR('',#11558,0.1025);
#1853=VECTOR('',#11563,0.205);
#1854=VECTOR('',#11568,0.255);
#1855=VECTOR('',#11571,0.15);
#1856=VECTOR('',#11576,0.3);
#1857=VECTOR('',#11581,0.15);
#1858=VECTOR('',#11586,0.3);
#1859=VECTOR('',#11593,0.36);
#1860=VECTOR('',#11598,0.36);
#1861=VECTOR('',#11603,0.5);
#1862=VECTOR('',#11608,1.);
#1863=VECTOR('',#11609,1.);
#1864=VECTOR('',#11610,1.);
#1865=VECTOR('',#11613,1.);
#1866=VECTOR('',#11614,1.);
#1867=VECTOR('',#11617,1.);
#1868=VECTOR('',#11618,1.);
#1869=VECTOR('',#11621,1.);
#1870=VECTOR('',#11622,1.);
#1871=VECTOR('',#11625,1.);
#1872=VECTOR('',#11626,1.);
#1873=VECTOR('',#11629,1.);
#1874=VECTOR('',#11630,1.);
#1875=VECTOR('',#11633,1.);
#1876=VECTOR('',#11634,1.);
#1877=VECTOR('',#11637,1.);
#1878=VECTOR('',#11638,1.);
#1879=VECTOR('',#11641,1.);
#1880=VECTOR('',#11642,1.);
#1881=VECTOR('',#11645,1.);
#1882=VECTOR('',#11646,1.);
#1883=VECTOR('',#11649,1.);
#1884=VECTOR('',#11650,1.);
#1885=VECTOR('',#11653,1.);
#1886=VECTOR('',#11658,1.);
#1887=VECTOR('',#11659,1.);
#1888=VECTOR('',#11662,1.);
#1889=VECTOR('',#11663,1.);
#1890=VECTOR('',#11666,1.);
#1891=VECTOR('',#11667,1.);
#1892=VECTOR('',#11670,1.);
#1893=VECTOR('',#11679,1.);
#1894=VECTOR('',#11682,1.);
#1895=VECTOR('',#11685,1.);
#1896=VECTOR('',#11686,1.);
#1897=VECTOR('',#11687,1.);
#1898=VECTOR('',#11692,1.);
#1899=VECTOR('',#11695,1.);
#1900=VECTOR('',#11698,1.);
#1901=VECTOR('',#11699,1.);
#1902=VECTOR('',#11704,1.);
#1903=VECTOR('',#11709,1.);
#1904=VECTOR('',#11710,1.);
#1905=VECTOR('',#11711,1.);
#1906=VECTOR('',#11716,1.);
#1907=VECTOR('',#11721,1.);
#1908=VECTOR('',#11722,1.);
#1909=VECTOR('',#11727,1.);
#1910=VECTOR('',#11730,1.);
#1911=VECTOR('',#11733,1.);
#1912=VECTOR('',#11734,1.);
#1913=VECTOR('',#11735,1.);
#1914=VECTOR('',#11740,1.);
#1915=VECTOR('',#11743,1.);
#1916=VECTOR('',#11746,1.);
#1917=VECTOR('',#11747,1.);
#1918=VECTOR('',#11752,1.);
#1919=VECTOR('',#11757,1.);
#1920=VECTOR('',#11758,1.);
#1921=VECTOR('',#11759,1.);
#1922=VECTOR('',#11764,1.);
#1923=VECTOR('',#11769,1.);
#1924=VECTOR('',#11770,1.);
#1925=VECTOR('',#11775,1.);
#1926=VECTOR('',#11778,1.);
#1927=VECTOR('',#11781,1.);
#1928=VECTOR('',#11782,1.);
#1929=VECTOR('',#11783,1.);
#1930=VECTOR('',#11788,1.);
#1931=VECTOR('',#11791,1.);
#1932=VECTOR('',#11794,1.);
#1933=VECTOR('',#11795,1.);
#1934=VECTOR('',#11800,1.);
#1935=VECTOR('',#11805,1.);
#1936=VECTOR('',#11806,1.);
#1937=VECTOR('',#11807,1.);
#1938=VECTOR('',#11812,1.);
#1939=VECTOR('',#11817,1.);
#1940=VECTOR('',#11818,1.);
#1941=VECTOR('',#11823,0.225);
#1942=VECTOR('',#11830,0.36);
#1943=VECTOR('',#11837,0.36);
#1944=VECTOR('',#11844,0.225);
#1945=VECTOR('',#11851,0.225);
#1946=VECTOR('',#11858,0.225);
#1947=VECTOR('',#11863,1.);
#1948=VECTOR('',#11864,1.);
#1949=VECTOR('',#11865,1.);
#1950=VECTOR('',#11866,1.);
#1951=VECTOR('',#11869,1.);
#1952=VECTOR('',#11870,1.);
#1953=VECTOR('',#11871,1.);
#1954=VECTOR('',#11874,1.);
#1955=VECTOR('',#11875,1.);
#1956=VECTOR('',#11876,1.);
#1957=VECTOR('',#11879,1.);
#1958=VECTOR('',#11880,1.);
#1959=VECTOR('',#11881,1.);
#1960=VECTOR('',#11884,1.);
#1961=VECTOR('',#11885,1.);
#1962=VECTOR('',#11886,1.);
#1963=VECTOR('',#11889,1.);
#1964=VECTOR('',#11890,1.);
#1965=VECTOR('',#11891,1.);
#1966=VECTOR('',#11894,1.);
#1967=VECTOR('',#11895,1.);
#1968=VECTOR('',#11896,1.);
#1969=VECTOR('',#11899,1.);
#1970=VECTOR('',#11900,1.);
#1971=VECTOR('',#11909,1.);
#1972=VECTOR('',#11910,1.);
#1973=VECTOR('',#11911,1.);
#1974=VECTOR('',#11912,1.);
#1975=VECTOR('',#11915,1.);
#1976=VECTOR('',#11916,1.);
#1977=VECTOR('',#11917,1.);
#1978=VECTOR('',#11920,1.);
#1979=VECTOR('',#11921,1.);
#1980=VECTOR('',#11922,1.);
#1981=VECTOR('',#11925,1.);
#1982=VECTOR('',#11926,1.);
#1983=VECTOR('',#11927,1.);
#1984=VECTOR('',#11930,1.);
#1985=VECTOR('',#11931,1.);
#1986=VECTOR('',#11932,1.);
#1987=VECTOR('',#11935,1.);
#1988=VECTOR('',#11936,1.);
#1989=VECTOR('',#11939,1.);
#1990=VECTOR('',#11940,1.);
#1991=VECTOR('',#11941,1.);
#1992=VECTOR('',#11944,1.);
#1993=VECTOR('',#11945,1.);
#1994=VECTOR('',#11948,1.);
#1995=VECTOR('',#11949,1.);
#1996=VECTOR('',#11964,0.36);
#1997=VECTOR('',#11969,0.3);
#1998=VECTOR('',#11974,0.3);
#1999=VECTOR('',#11979,0.36);
#2000=VECTOR('',#11982,1.);
#2001=VECTOR('',#11983,1.);
#2002=VECTOR('',#11986,1.);
#2003=VECTOR('',#11987,1.);
#2004=VECTOR('',#11990,1.);
#2005=VECTOR('',#12013,0.999999999999999);
#2006=VECTOR('',#12014,1.);
#2007=VECTOR('',#12015,0.999999999999999);
#2008=VECTOR('',#12016,1.);
#2009=VECTOR('',#12019,1.);
#2010=VECTOR('',#12020,1.);
#2011=VECTOR('',#12021,1.);
#2012=VECTOR('',#12024,1.);
#2013=VECTOR('',#12025,1.);
#2014=VECTOR('',#12026,1.);
#2015=VECTOR('',#12029,1.);
#2016=VECTOR('',#12030,1.);
#2017=VECTOR('',#12031,1.);
#2018=VECTOR('',#12034,1.);
#2019=VECTOR('',#12035,1.);
#2020=VECTOR('',#12036,1.);
#2021=VECTOR('',#12039,1.);
#2022=VECTOR('',#12040,1.);
#2023=VECTOR('',#12053,0.375);
#2024=VECTOR('',#12056,0.38);
#2025=VECTOR('',#12067,1.);
#2026=VECTOR('',#12070,1.);
#2027=VECTOR('',#12077,1.);
#2028=VECTOR('',#12084,1.);
#2029=VECTOR('',#12087,1.);
#2030=VECTOR('',#12090,1.);
#2031=VECTOR('',#12091,1.);
#2032=VECTOR('',#12096,1.);
#2033=VECTOR('',#12099,1.);
#2034=VECTOR('',#12106,1.);
#2035=VECTOR('',#12113,1.);
#2036=VECTOR('',#12116,1.);
#2037=VECTOR('',#12119,1.);
#2038=VECTOR('',#12120,1.);
#2039=VECTOR('',#12121,1.);
#2040=VECTOR('',#12122,1.);
#2041=VECTOR('',#12123,1.);
#2042=VECTOR('',#12124,1.);
#2043=VECTOR('',#12127,1.);
#2044=VECTOR('',#12128,1.);
#2045=VECTOR('',#12129,1.);
#2046=VECTOR('',#12132,1.);
#2047=VECTOR('',#12133,1.);
#2048=VECTOR('',#12136,1.);
#2049=VECTOR('',#12137,1.);
#2050=VECTOR('',#12140,1.);
#2051=VECTOR('',#12147,0.3);
#2052=VECTOR('',#12150,0.3);
#2053=VECTOR('',#12157,0.199999999999999);
#2054=VECTOR('',#12160,0.199999999999999);
#2055=VECTOR('',#12167,0.4025);
#2056=VECTOR('',#12168,0.4025);
#2057=VECTOR('',#12169,0.4025);
#2058=VECTOR('',#12174,1.);
#2059=VECTOR('',#12185,1.);
#2060=VECTOR('',#12196,1.1);
#2061=VECTOR('',#12205,1.);
#2062=VECTOR('',#12208,1.);
#2063=VECTOR('',#12211,1.);
#2064=VECTOR('',#12214,1.);
#2065=VECTOR('',#12229,0.4);
#2066=VECTOR('',#12234,0.415);
#2067=VECTOR('',#12245,0.62);
#2068=VECTOR('',#12254,0.92);
#2069=VECTOR('',#12263,1.085);
#2070=VECTOR('',#12268,1.1);
#2071=VECTOR('',#12271,1.085);
#2072=VECTOR('',#12282,0.92);
#2073=VECTOR('',#12291,0.62);
#2074=VECTOR('',#12298,0.415);
#2075=VECTOR('',#12303,1.);
#2076=VECTOR('',#12304,1.);
#2077=VECTOR('',#12305,1.);
#2078=VECTOR('',#12306,1.);
#2079=VECTOR('',#12309,1.);
#2080=VECTOR('',#12310,1.);
#2081=VECTOR('',#12311,1.);
#2082=VECTOR('',#12312,1.);
#2083=VECTOR('',#12315,1.);
#2084=VECTOR('',#12316,1.);
#2085=VECTOR('',#12325,1.);
#2086=VECTOR('',#12326,1.);
#2087=VECTOR('',#12327,1.);
#2088=VECTOR('',#12330,1.);
#2089=VECTOR('',#12331,1.);
#2090=VECTOR('',#12332,1.);
#2091=VECTOR('',#12335,1.);
#2092=VECTOR('',#12336,1.);
#2093=VECTOR('',#12337,1.);
#2094=VECTOR('',#12340,1.);
#2095=VECTOR('',#12341,1.);
#2096=VECTOR('',#12342,1.);
#2097=VECTOR('',#12345,1.);
#2098=VECTOR('',#12346,1.);
#2099=VECTOR('',#12347,1.);
#2100=VECTOR('',#12350,1.);
#2101=VECTOR('',#12351,1.);
#2102=VECTOR('',#12352,1.);
#2103=VECTOR('',#12355,1.);
#2104=VECTOR('',#12356,1.);
#2105=VECTOR('',#12357,1.);
#2106=VECTOR('',#12372,1.);
#2107=VECTOR('',#12373,1.);
#2108=VECTOR('',#12374,1.);
#2109=VECTOR('',#12377,1.);
#2110=VECTOR('',#12378,1.);
#2111=VECTOR('',#12379,1.);
#2112=VECTOR('',#12382,1.);
#2113=VECTOR('',#12393,1.);
#2114=VECTOR('',#12394,1.);
#2115=VECTOR('',#12395,1.);
#2116=VECTOR('',#12398,1.);
#2117=VECTOR('',#12399,1.);
#2118=VECTOR('',#12400,1.);
#2119=VECTOR('',#12403,1.);
#2120=VECTOR('',#12414,1.);
#2121=VECTOR('',#12415,1.);
#2122=VECTOR('',#12416,1.);
#2123=VECTOR('',#12419,1.);
#2124=VECTOR('',#12420,1.);
#2125=VECTOR('',#12421,1.);
#2126=VECTOR('',#12424,1.);
#2127=VECTOR('',#12437,1.);
#2128=VECTOR('',#12438,1.);
#2129=VECTOR('',#12439,1.);
#2130=VECTOR('',#12442,1.);
#2131=VECTOR('',#12443,1.);
#2132=VECTOR('',#12444,1.);
#2133=VECTOR('',#12447,1.);
#2134=VECTOR('',#12458,1.);
#2135=VECTOR('',#12459,1.);
#2136=VECTOR('',#12460,1.);
#2137=VECTOR('',#12463,1.);
#2138=VECTOR('',#12464,1.);
#2139=VECTOR('',#12465,1.);
#2140=VECTOR('',#12468,1.);
#2141=VECTOR('',#12479,1.);
#2142=VECTOR('',#12480,1.);
#2143=VECTOR('',#12481,1.);
#2144=VECTOR('',#12484,1.);
#2145=VECTOR('',#12485,1.);
#2146=VECTOR('',#12486,1.);
#2147=VECTOR('',#12489,1.);
#2148=VECTOR('',#12500,1.);
#2149=VECTOR('',#12501,1.);
#2150=VECTOR('',#12502,1.);
#2151=VECTOR('',#12505,1.);
#2152=VECTOR('',#12506,1.);
#2153=VECTOR('',#12507,1.);
#2154=VECTOR('',#12510,1.);
#2155=VECTOR('',#12519,1.1);
#2156=VECTOR('',#12528,0.46);
#2157=VECTOR('',#12537,1.5);
#2158=VECTOR('',#12542,0.6);
#2159=VECTOR('',#12549,1.);
#2160=VECTOR('',#12550,1.);
#2161=VECTOR('',#12551,1.);
#2162=VECTOR('',#12552,1.);
#2163=VECTOR('',#12555,1.);
#2164=VECTOR('',#12556,1.);
#2165=VECTOR('',#12557,1.);
#2166=VECTOR('',#12558,1.);
#2167=VECTOR('',#12561,1.);
#2168=VECTOR('',#12562,1.);
#2169=VECTOR('',#12573,1.5);
#2170=VECTOR('',#12586,0.302);
#2171=VECTOR('',#12591,0.322);
#2172=VECTOR('',#12602,0.86);
#2173=VECTOR('',#12611,0.94);
#2174=VECTOR('',#12620,0.975);
#2175=VECTOR('',#12625,1.);
#2176=VECTOR('',#12628,0.975);
#2177=VECTOR('',#12639,0.94);
#2178=VECTOR('',#12648,0.86);
#2179=VECTOR('',#12655,0.322);
#2180=VECTOR('',#12662,0.202);
#2181=VECTOR('',#12667,0.217);
#2182=VECTOR('',#12678,0.335);
#2183=VECTOR('',#12683,0.35);
#2184=VECTOR('',#12686,0.335);
#2185=VECTOR('',#12695,0.217);
#2186=VECTOR('',#12706,0.285);
#2187=VECTOR('',#12711,0.3);
#2188=VECTOR('',#12720,0.25);
#2189=VECTOR('',#12729,0.3);
#2190=VECTOR('',#12732,0.285);
#2191=VECTOR('',#12747,0.185);
#2192=VECTOR('',#12752,0.2);
#2193=VECTOR('',#12761,0.16);
#2194=VECTOR('',#12770,0.2);
#2195=VECTOR('',#12773,0.185);
#2196=VECTOR('',#12790,0.3);
#2197=VECTOR('',#12801,0.28);
#2198=VECTOR('',#12806,0.15555);
#2199=VECTOR('',#12811,0.15555);
#2200=VECTOR('',#12814,0.15555);
#2201=VECTOR('',#12817,0.15555);
#2202=VECTOR('',#12820,0.15555);
#2203=VECTOR('',#12823,0.15555);
#2204=VECTOR('',#12826,0.15555);
#2205=VECTOR('',#12829,0.15555);
#2206=VECTOR('',#12832,0.15555);
#2207=VECTOR('',#12835,0.15555);
#2208=VECTOR('',#12838,0.15555);
#2209=VECTOR('',#12841,0.15555);
#2210=VECTOR('',#12844,0.15555);
#2211=VECTOR('',#12847,0.15555);
#2212=VECTOR('',#12922,0.06125);
#2213=VECTOR('',#12927,1.);
#2214=VECTOR('',#12928,1.);
#2215=VECTOR('',#12929,1.);
#2216=VECTOR('',#12932,1.);
#2217=VECTOR('',#12933,1.);
#2218=VECTOR('',#12936,1.);
#2219=VECTOR('',#12937,1.);
#2220=VECTOR('',#12940,1.);
#2221=VECTOR('',#12941,1.);
#2222=VECTOR('',#12944,1.);
#2223=VECTOR('',#12945,1.);
#2224=VECTOR('',#12948,1.);
#2225=VECTOR('',#12957,0.185);
#2226=VECTOR('',#12964,0.38);
#2227=VECTOR('',#12969,1.);
#2228=VECTOR('',#12970,1.);
#2229=VECTOR('',#12971,1.);
#2230=VECTOR('',#12972,1.);
#2231=VECTOR('',#12975,1.);
#2232=VECTOR('',#12976,1.);
#2233=VECTOR('',#12977,1.);
#2234=VECTOR('',#12978,1.);
#2235=VECTOR('',#12981,1.);
#2236=VECTOR('',#12982,1.);
#2237=VECTOR('',#12983,1.);
#2238=VECTOR('',#12984,1.);
#2239=VECTOR('',#12987,1.);
#2240=VECTOR('',#12988,1.);
#2241=VECTOR('',#12989,1.);
#2242=VECTOR('',#12990,1.);
#2243=VECTOR('',#12995,1.);
#2244=VECTOR('',#13002,1.);
#2245=VECTOR('',#13009,1.);
#2246=VECTOR('',#13016,1.);
#2247=VECTOR('',#13045,1.);
#2248=VECTOR('',#13050,1.);
#2249=VECTOR('',#13065,1.);
#2250=VECTOR('',#13066,1.);
#2251=VECTOR('',#13067,1.);
#2252=VECTOR('',#13068,1.);
#2253=VECTOR('',#13071,1.);
#2254=VECTOR('',#13072,1.);
#2255=VECTOR('',#13073,1.);
#2256=VECTOR('',#13074,1.);
#2257=VECTOR('',#13077,1.);
#2258=VECTOR('',#13078,1.);
#2259=VECTOR('',#13079,1.);
#2260=VECTOR('',#13080,1.);
#2261=VECTOR('',#13083,1.);
#2262=VECTOR('',#13084,1.);
#2263=VECTOR('',#13085,1.);
#2264=VECTOR('',#13086,1.);
#2265=VECTOR('',#13091,1.);
#2266=VECTOR('',#13098,1.);
#2267=VECTOR('',#13105,1.);
#2268=VECTOR('',#13112,1.);
#2269=VECTOR('',#13141,1.);
#2270=VECTOR('',#13146,1.);
#2271=CYLINDRICAL_SURFACE('',#10105,1.35);
#2272=CYLINDRICAL_SURFACE('',#10119,1.35);
#2273=CYLINDRICAL_SURFACE('',#10128,0.08);
#2274=CYLINDRICAL_SURFACE('',#10148,0.9);
#2275=CYLINDRICAL_SURFACE('',#10183,0.9);
#2276=CYLINDRICAL_SURFACE('',#10184,0.0800457110804505);
#2277=CYLINDRICAL_SURFACE('',#10203,0.08);
#2278=CYLINDRICAL_SURFACE('',#10207,0.08);
#2279=CYLINDRICAL_SURFACE('',#10219,0.9);
#2280=CYLINDRICAL_SURFACE('',#10224,0.9);
#2281=CYLINDRICAL_SURFACE('',#10232,0.08);
#2282=CYLINDRICAL_SURFACE('',#10234,0.08);
#2283=CYLINDRICAL_SURFACE('',#10237,0.08);
#2284=CYLINDRICAL_SURFACE('',#10243,0.08);
#2285=CYLINDRICAL_SURFACE('',#10246,0.08);
#2286=CYLINDRICAL_SURFACE('',#10262,0.0800457110810776);
#2287=CYLINDRICAL_SURFACE('',#10267,0.4);
#2288=CYLINDRICAL_SURFACE('',#10268,0.4);
#2289=CYLINDRICAL_SURFACE('',#10293,0.4);
#2290=CYLINDRICAL_SURFACE('',#10295,0.4);
#2291=CYLINDRICAL_SURFACE('',#10296,0.3);
#2292=CYLINDRICAL_SURFACE('',#10297,0.36);
#2293=CYLINDRICAL_SURFACE('',#10298,0.36);
#2294=CYLINDRICAL_SURFACE('',#10299,0.3);
#2295=CYLINDRICAL_SURFACE('',#10325,0.205);
#2296=CYLINDRICAL_SURFACE('',#10330,0.205);
#2297=CYLINDRICAL_SURFACE('',#10335,0.205);
#2298=CYLINDRICAL_SURFACE('',#10340,0.205);
#2299=CYLINDRICAL_SURFACE('',#10345,0.3);
#2300=CYLINDRICAL_SURFACE('',#10349,0.3);
#2301=CYLINDRICAL_SURFACE('',#10351,0.36);
#2302=CYLINDRICAL_SURFACE('',#10353,0.36);
#2303=CYLINDRICAL_SURFACE('',#10355,0.5);
#2304=CYLINDRICAL_SURFACE('',#10377,0.2);
#2305=CYLINDRICAL_SURFACE('',#10381,0.2);
#2306=CYLINDRICAL_SURFACE('',#10385,0.2);
#2307=CYLINDRICAL_SURFACE('',#10389,0.2);
#2308=CYLINDRICAL_SURFACE('',#10393,0.2);
#2309=CYLINDRICAL_SURFACE('',#10397,0.2);
#2310=CYLINDRICAL_SURFACE('',#10401,0.2);
#2311=CYLINDRICAL_SURFACE('',#10405,0.2);
#2312=CYLINDRICAL_SURFACE('',#10409,0.2);
#2313=CYLINDRICAL_SURFACE('',#10413,0.2);
#2314=CYLINDRICAL_SURFACE('',#10417,0.2);
#2315=CYLINDRICAL_SURFACE('',#10421,0.2);
#2316=CYLINDRICAL_SURFACE('',#10425,0.225);
#2317=CYLINDRICAL_SURFACE('',#10428,0.36);
#2318=CYLINDRICAL_SURFACE('',#10431,0.36);
#2319=CYLINDRICAL_SURFACE('',#10434,0.225);
#2320=CYLINDRICAL_SURFACE('',#10437,0.225);
#2321=CYLINDRICAL_SURFACE('',#10440,0.225);
#2322=CYLINDRICAL_SURFACE('',#10468,0.36);
#2323=CYLINDRICAL_SURFACE('',#10470,0.3);
#2324=CYLINDRICAL_SURFACE('',#10472,0.3);
#2325=CYLINDRICAL_SURFACE('',#10474,0.36);
#2326=CYLINDRICAL_SURFACE('',#10481,0.3933);
#2327=CYLINDRICAL_SURFACE('',#10486,0.322275);
#2328=CYLINDRICAL_SURFACE('',#10505,0.15);
#2329=CYLINDRICAL_SURFACE('',#10511,0.15);
#2330=CYLINDRICAL_SURFACE('',#10516,0.15);
#2331=CYLINDRICAL_SURFACE('',#10522,0.15);
#2332=CYLINDRICAL_SURFACE('',#10532,0.3);
#2333=CYLINDRICAL_SURFACE('',#10534,0.3);
#2334=CYLINDRICAL_SURFACE('',#10536,0.199999999999999);
#2335=CYLINDRICAL_SURFACE('',#10538,0.199999999999999);
#2336=CYLINDRICAL_SURFACE('',#10540,0.4025);
#2337=CYLINDRICAL_SURFACE('',#10552,1.1);
#2338=CYLINDRICAL_SURFACE('',#10566,0.4);
#2339=CYLINDRICAL_SURFACE('',#10573,0.62);
#2340=CYLINDRICAL_SURFACE('',#10577,0.92);
#2341=CYLINDRICAL_SURFACE('',#10583,1.1);
#2342=CYLINDRICAL_SURFACE('',#10589,0.92);
#2343=CYLINDRICAL_SURFACE('',#10593,0.62);
#2344=CYLINDRICAL_SURFACE('',#10666,1.1);
#2345=CYLINDRICAL_SURFACE('',#10671,0.46);
#2346=CYLINDRICAL_SURFACE('',#10675,1.5);
#2347=CYLINDRICAL_SURFACE('',#10676,0.6);
#2348=CYLINDRICAL_SURFACE('',#10686,1.5);
#2349=CYLINDRICAL_SURFACE('',#10688,1.58);
#2350=CYLINDRICAL_SURFACE('',#10692,0.302);
#2351=CYLINDRICAL_SURFACE('',#10699,0.86);
#2352=CYLINDRICAL_SURFACE('',#10703,0.94);
#2353=CYLINDRICAL_SURFACE('',#10709,1.);
#2354=CYLINDRICAL_SURFACE('',#10715,0.94);
#2355=CYLINDRICAL_SURFACE('',#10719,0.86);
#2356=CYLINDRICAL_SURFACE('',#10725,0.202);
#2357=CYLINDRICAL_SURFACE('',#10734,0.35);
#2358=CYLINDRICAL_SURFACE('',#10746,0.3);
#2359=CYLINDRICAL_SURFACE('',#10750,0.25);
#2360=CYLINDRICAL_SURFACE('',#10754,0.3);
#2361=CYLINDRICAL_SURFACE('',#10764,0.2);
#2362=CYLINDRICAL_SURFACE('',#10768,0.16);
#2363=CYLINDRICAL_SURFACE('',#10772,0.2);
#2364=CYLINDRICAL_SURFACE('',#10782,0.3);
#2365=CYLINDRICAL_SURFACE('',#10789,0.15555);
#2366=CYLINDRICAL_SURFACE('',#10791,0.15555);
#2367=CYLINDRICAL_SURFACE('',#10792,0.15555);
#2368=CYLINDRICAL_SURFACE('',#10793,0.15555);
#2369=CYLINDRICAL_SURFACE('',#10794,0.15555);
#2370=CYLINDRICAL_SURFACE('',#10795,0.15555);
#2371=CYLINDRICAL_SURFACE('',#10796,0.15555);
#2372=CYLINDRICAL_SURFACE('',#10797,0.15555);
#2373=CYLINDRICAL_SURFACE('',#10798,0.15555);
#2374=CYLINDRICAL_SURFACE('',#10799,0.15555);
#2375=CYLINDRICAL_SURFACE('',#10800,0.15555);
#2376=CYLINDRICAL_SURFACE('',#10801,0.15555);
#2377=CYLINDRICAL_SURFACE('',#10802,0.15555);
#2378=CYLINDRICAL_SURFACE('',#10803,0.15555);
#2379=CYLINDRICAL_SURFACE('',#10804,0.1954);
#2380=CYLINDRICAL_SURFACE('',#10807,0.15555);
#2381=CYLINDRICAL_SURFACE('',#10854,0.38);
#2382=CYLINDRICAL_SURFACE('',#10860,0.059240625);
#2383=CYLINDRICAL_SURFACE('',#10863,0.059240625);
#2384=CYLINDRICAL_SURFACE('',#10866,0.059240625);
#2385=CYLINDRICAL_SURFACE('',#10869,0.059240625);
#2386=CYLINDRICAL_SURFACE('',#10872,0.33848125);
#2387=CYLINDRICAL_SURFACE('',#10881,0.33848125);
#2388=CYLINDRICAL_SURFACE('',#10883,0.33848125);
#2389=CYLINDRICAL_SURFACE('',#10885,0.059240625);
#2390=CYLINDRICAL_SURFACE('',#10887,0.33848125);
#2391=CYLINDRICAL_SURFACE('',#10889,0.5425);
#2392=CYLINDRICAL_SURFACE('',#10897,0.04298125);
#2393=CYLINDRICAL_SURFACE('',#10900,0.04298125);
#2394=CYLINDRICAL_SURFACE('',#10903,0.04298125);
#2395=CYLINDRICAL_SURFACE('',#10906,0.04298125);
#2396=CYLINDRICAL_SURFACE('',#10909,0.2159625);
#2397=CYLINDRICAL_SURFACE('',#10918,0.2159625);
#2398=CYLINDRICAL_SURFACE('',#10920,0.2159625);
#2399=CYLINDRICAL_SURFACE('',#10922,0.04298125);
#2400=CYLINDRICAL_SURFACE('',#10924,0.2159625);
#2401=CYLINDRICAL_SURFACE('',#10926,0.345);
#2402=FACE_OUTER_BOUND('',#2903,.T.);
#2403=FACE_OUTER_BOUND('',#2904,.T.);
#2404=FACE_OUTER_BOUND('',#2905,.T.);
#2405=FACE_OUTER_BOUND('',#2907,.T.);
#2406=FACE_OUTER_BOUND('',#2908,.T.);
#2407=FACE_OUTER_BOUND('',#2910,.T.);
#2408=FACE_OUTER_BOUND('',#2911,.T.);
#2409=FACE_OUTER_BOUND('',#2912,.T.);
#2410=FACE_OUTER_BOUND('',#2914,.T.);
#2411=FACE_OUTER_BOUND('',#2915,.T.);
#2412=FACE_OUTER_BOUND('',#2917,.T.);
#2413=FACE_OUTER_BOUND('',#2918,.T.);
#2414=FACE_OUTER_BOUND('',#2919,.T.);
#2415=FACE_OUTER_BOUND('',#2920,.T.);
#2416=FACE_OUTER_BOUND('',#2921,.T.);
#2417=FACE_OUTER_BOUND('',#2922,.T.);
#2418=FACE_OUTER_BOUND('',#2923,.T.);
#2419=FACE_OUTER_BOUND('',#2924,.T.);
#2420=FACE_OUTER_BOUND('',#2925,.T.);
#2421=FACE_OUTER_BOUND('',#2926,.T.);
#2422=FACE_OUTER_BOUND('',#2927,.T.);
#2423=FACE_OUTER_BOUND('',#2928,.T.);
#2424=FACE_OUTER_BOUND('',#2929,.T.);
#2425=FACE_OUTER_BOUND('',#2930,.T.);
#2426=FACE_OUTER_BOUND('',#2931,.T.);
#2427=FACE_OUTER_BOUND('',#2932,.T.);
#2428=FACE_OUTER_BOUND('',#2933,.T.);
#2429=FACE_OUTER_BOUND('',#2934,.T.);
#2430=FACE_OUTER_BOUND('',#2935,.T.);
#2431=FACE_OUTER_BOUND('',#2936,.T.);
#2432=FACE_OUTER_BOUND('',#2937,.T.);
#2433=FACE_OUTER_BOUND('',#2938,.T.);
#2434=FACE_OUTER_BOUND('',#2939,.T.);
#2435=FACE_OUTER_BOUND('',#2940,.T.);
#2436=FACE_OUTER_BOUND('',#2941,.T.);
#2437=FACE_OUTER_BOUND('',#2942,.T.);
#2438=FACE_OUTER_BOUND('',#2943,.T.);
#2439=FACE_OUTER_BOUND('',#2944,.T.);
#2440=FACE_OUTER_BOUND('',#2945,.T.);
#2441=FACE_OUTER_BOUND('',#2946,.T.);
#2442=FACE_OUTER_BOUND('',#2947,.T.);
#2443=FACE_OUTER_BOUND('',#2948,.T.);
#2444=FACE_OUTER_BOUND('',#2949,.T.);
#2445=FACE_OUTER_BOUND('',#2950,.T.);
#2446=FACE_OUTER_BOUND('',#2951,.T.);
#2447=FACE_OUTER_BOUND('',#2952,.T.);
#2448=FACE_OUTER_BOUND('',#2953,.T.);
#2449=FACE_OUTER_BOUND('',#2954,.T.);
#2450=FACE_OUTER_BOUND('',#2955,.T.);
#2451=FACE_OUTER_BOUND('',#2956,.T.);
#2452=FACE_OUTER_BOUND('',#2957,.T.);
#2453=FACE_OUTER_BOUND('',#2958,.T.);
#2454=FACE_OUTER_BOUND('',#2959,.T.);
#2455=FACE_OUTER_BOUND('',#2960,.T.);
#2456=FACE_OUTER_BOUND('',#2961,.T.);
#2457=FACE_OUTER_BOUND('',#2962,.T.);
#2458=FACE_OUTER_BOUND('',#2963,.T.);
#2459=FACE_OUTER_BOUND('',#2964,.T.);
#2460=FACE_OUTER_BOUND('',#2965,.T.);
#2461=FACE_OUTER_BOUND('',#2966,.T.);
#2462=FACE_OUTER_BOUND('',#2967,.T.);
#2463=FACE_OUTER_BOUND('',#2968,.T.);
#2464=FACE_OUTER_BOUND('',#2969,.T.);
#2465=FACE_OUTER_BOUND('',#2970,.T.);
#2466=FACE_OUTER_BOUND('',#2971,.T.);
#2467=FACE_OUTER_BOUND('',#2972,.T.);
#2468=FACE_OUTER_BOUND('',#2973,.T.);
#2469=FACE_OUTER_BOUND('',#2974,.T.);
#2470=FACE_OUTER_BOUND('',#2975,.T.);
#2471=FACE_OUTER_BOUND('',#2976,.T.);
#2472=FACE_OUTER_BOUND('',#2977,.T.);
#2473=FACE_OUTER_BOUND('',#2978,.T.);
#2474=FACE_OUTER_BOUND('',#2979,.T.);
#2475=FACE_OUTER_BOUND('',#2980,.T.);
#2476=FACE_OUTER_BOUND('',#2981,.T.);
#2477=FACE_OUTER_BOUND('',#2982,.T.);
#2478=FACE_OUTER_BOUND('',#2983,.T.);
#2479=FACE_OUTER_BOUND('',#2984,.T.);
#2480=FACE_OUTER_BOUND('',#2985,.T.);
#2481=FACE_OUTER_BOUND('',#2986,.T.);
#2482=FACE_OUTER_BOUND('',#2987,.T.);
#2483=FACE_OUTER_BOUND('',#2988,.T.);
#2484=FACE_OUTER_BOUND('',#2989,.T.);
#2485=FACE_OUTER_BOUND('',#2990,.T.);
#2486=FACE_OUTER_BOUND('',#2991,.T.);
#2487=FACE_OUTER_BOUND('',#2992,.T.);
#2488=FACE_OUTER_BOUND('',#2993,.T.);
#2489=FACE_OUTER_BOUND('',#2994,.T.);
#2490=FACE_OUTER_BOUND('',#2995,.T.);
#2491=FACE_OUTER_BOUND('',#2996,.T.);
#2492=FACE_OUTER_BOUND('',#2997,.T.);
#2493=FACE_OUTER_BOUND('',#2998,.T.);
#2494=FACE_OUTER_BOUND('',#2999,.T.);
#2495=FACE_OUTER_BOUND('',#3000,.T.);
#2496=FACE_OUTER_BOUND('',#3001,.T.);
#2497=FACE_OUTER_BOUND('',#3002,.T.);
#2498=FACE_OUTER_BOUND('',#3003,.T.);
#2499=FACE_OUTER_BOUND('',#3004,.T.);
#2500=FACE_OUTER_BOUND('',#3009,.T.);
#2501=FACE_OUTER_BOUND('',#3010,.T.);
#2502=FACE_OUTER_BOUND('',#3011,.T.);
#2503=FACE_OUTER_BOUND('',#3012,.T.);
#2504=FACE_OUTER_BOUND('',#3013,.T.);
#2505=FACE_OUTER_BOUND('',#3014,.T.);
#2506=FACE_OUTER_BOUND('',#3015,.T.);
#2507=FACE_OUTER_BOUND('',#3016,.T.);
#2508=FACE_OUTER_BOUND('',#3017,.T.);
#2509=FACE_OUTER_BOUND('',#3022,.T.);
#2510=FACE_OUTER_BOUND('',#3023,.T.);
#2511=FACE_OUTER_BOUND('',#3024,.T.);
#2512=FACE_OUTER_BOUND('',#3025,.T.);
#2513=FACE_OUTER_BOUND('',#3026,.T.);
#2514=FACE_OUTER_BOUND('',#3027,.T.);
#2515=FACE_OUTER_BOUND('',#3028,.T.);
#2516=FACE_OUTER_BOUND('',#3029,.T.);
#2517=FACE_OUTER_BOUND('',#3030,.T.);
#2518=FACE_OUTER_BOUND('',#3031,.T.);
#2519=FACE_OUTER_BOUND('',#3032,.T.);
#2520=FACE_OUTER_BOUND('',#3033,.T.);
#2521=FACE_OUTER_BOUND('',#3034,.T.);
#2522=FACE_OUTER_BOUND('',#3035,.T.);
#2523=FACE_OUTER_BOUND('',#3036,.T.);
#2524=FACE_OUTER_BOUND('',#3037,.T.);
#2525=FACE_OUTER_BOUND('',#3038,.T.);
#2526=FACE_OUTER_BOUND('',#3039,.T.);
#2527=FACE_OUTER_BOUND('',#3040,.T.);
#2528=FACE_OUTER_BOUND('',#3041,.T.);
#2529=FACE_OUTER_BOUND('',#3042,.T.);
#2530=FACE_OUTER_BOUND('',#3043,.T.);
#2531=FACE_OUTER_BOUND('',#3044,.T.);
#2532=FACE_OUTER_BOUND('',#3045,.T.);
#2533=FACE_OUTER_BOUND('',#3046,.T.);
#2534=FACE_OUTER_BOUND('',#3047,.T.);
#2535=FACE_OUTER_BOUND('',#3048,.T.);
#2536=FACE_OUTER_BOUND('',#3049,.T.);
#2537=FACE_OUTER_BOUND('',#3050,.T.);
#2538=FACE_OUTER_BOUND('',#3051,.T.);
#2539=FACE_OUTER_BOUND('',#3052,.T.);
#2540=FACE_OUTER_BOUND('',#3053,.T.);
#2541=FACE_OUTER_BOUND('',#3054,.T.);
#2542=FACE_OUTER_BOUND('',#3055,.T.);
#2543=FACE_OUTER_BOUND('',#3056,.T.);
#2544=FACE_OUTER_BOUND('',#3057,.T.);
#2545=FACE_OUTER_BOUND('',#3058,.T.);
#2546=FACE_OUTER_BOUND('',#3059,.T.);
#2547=FACE_OUTER_BOUND('',#3060,.T.);
#2548=FACE_OUTER_BOUND('',#3061,.T.);
#2549=FACE_OUTER_BOUND('',#3062,.T.);
#2550=FACE_OUTER_BOUND('',#3063,.T.);
#2551=FACE_OUTER_BOUND('',#3064,.T.);
#2552=FACE_OUTER_BOUND('',#3065,.T.);
#2553=FACE_OUTER_BOUND('',#3066,.T.);
#2554=FACE_OUTER_BOUND('',#3067,.T.);
#2555=FACE_OUTER_BOUND('',#3068,.T.);
#2556=FACE_OUTER_BOUND('',#3069,.T.);
#2557=FACE_OUTER_BOUND('',#3070,.T.);
#2558=FACE_OUTER_BOUND('',#3071,.T.);
#2559=FACE_OUTER_BOUND('',#3072,.T.);
#2560=FACE_OUTER_BOUND('',#3073,.T.);
#2561=FACE_OUTER_BOUND('',#3074,.T.);
#2562=FACE_OUTER_BOUND('',#3075,.T.);
#2563=FACE_OUTER_BOUND('',#3076,.T.);
#2564=FACE_OUTER_BOUND('',#3077,.T.);
#2565=FACE_OUTER_BOUND('',#3078,.T.);
#2566=FACE_OUTER_BOUND('',#3079,.T.);
#2567=FACE_OUTER_BOUND('',#3080,.T.);
#2568=FACE_OUTER_BOUND('',#3081,.T.);
#2569=FACE_OUTER_BOUND('',#3082,.T.);
#2570=FACE_OUTER_BOUND('',#3083,.T.);
#2571=FACE_OUTER_BOUND('',#3091,.T.);
#2572=FACE_OUTER_BOUND('',#3092,.T.);
#2573=FACE_OUTER_BOUND('',#3093,.T.);
#2574=FACE_OUTER_BOUND('',#3094,.T.);
#2575=FACE_OUTER_BOUND('',#3095,.T.);
#2576=FACE_OUTER_BOUND('',#3096,.T.);
#2577=FACE_OUTER_BOUND('',#3097,.T.);
#2578=FACE_OUTER_BOUND('',#3098,.T.);
#2579=FACE_OUTER_BOUND('',#3099,.T.);
#2580=FACE_OUTER_BOUND('',#3100,.T.);
#2581=FACE_OUTER_BOUND('',#3101,.T.);
#2582=FACE_OUTER_BOUND('',#3102,.T.);
#2583=FACE_OUTER_BOUND('',#3103,.T.);
#2584=FACE_OUTER_BOUND('',#3104,.T.);
#2585=FACE_OUTER_BOUND('',#3105,.T.);
#2586=FACE_OUTER_BOUND('',#3106,.T.);
#2587=FACE_OUTER_BOUND('',#3107,.T.);
#2588=FACE_OUTER_BOUND('',#3108,.T.);
#2589=FACE_OUTER_BOUND('',#3109,.T.);
#2590=FACE_OUTER_BOUND('',#3110,.T.);
#2591=FACE_OUTER_BOUND('',#3111,.T.);
#2592=FACE_OUTER_BOUND('',#3112,.T.);
#2593=FACE_OUTER_BOUND('',#3113,.T.);
#2594=FACE_OUTER_BOUND('',#3115,.T.);
#2595=FACE_OUTER_BOUND('',#3116,.T.);
#2596=FACE_OUTER_BOUND('',#3117,.T.);
#2597=FACE_OUTER_BOUND('',#3118,.T.);
#2598=FACE_OUTER_BOUND('',#3119,.T.);
#2599=FACE_OUTER_BOUND('',#3120,.T.);
#2600=FACE_OUTER_BOUND('',#3121,.T.);
#2601=FACE_OUTER_BOUND('',#3122,.T.);
#2602=FACE_OUTER_BOUND('',#3123,.T.);
#2603=FACE_OUTER_BOUND('',#3124,.T.);
#2604=FACE_OUTER_BOUND('',#3125,.T.);
#2605=FACE_OUTER_BOUND('',#3127,.T.);
#2606=FACE_OUTER_BOUND('',#3128,.T.);
#2607=FACE_OUTER_BOUND('',#3129,.T.);
#2608=FACE_OUTER_BOUND('',#3134,.T.);
#2609=FACE_OUTER_BOUND('',#3135,.T.);
#2610=FACE_OUTER_BOUND('',#3136,.T.);
#2611=FACE_OUTER_BOUND('',#3137,.T.);
#2612=FACE_OUTER_BOUND('',#3138,.T.);
#2613=FACE_OUTER_BOUND('',#3139,.T.);
#2614=FACE_OUTER_BOUND('',#3140,.T.);
#2615=FACE_OUTER_BOUND('',#3141,.T.);
#2616=FACE_OUTER_BOUND('',#3142,.T.);
#2617=FACE_OUTER_BOUND('',#3143,.T.);
#2618=FACE_OUTER_BOUND('',#3144,.T.);
#2619=FACE_OUTER_BOUND('',#3145,.T.);
#2620=FACE_OUTER_BOUND('',#3146,.T.);
#2621=FACE_OUTER_BOUND('',#3147,.T.);
#2622=FACE_OUTER_BOUND('',#3148,.T.);
#2623=FACE_OUTER_BOUND('',#3149,.T.);
#2624=FACE_OUTER_BOUND('',#3150,.T.);
#2625=FACE_OUTER_BOUND('',#3151,.T.);
#2626=FACE_OUTER_BOUND('',#3152,.T.);
#2627=FACE_OUTER_BOUND('',#3153,.T.);
#2628=FACE_OUTER_BOUND('',#3154,.T.);
#2629=FACE_OUTER_BOUND('',#3155,.T.);
#2630=FACE_OUTER_BOUND('',#3156,.T.);
#2631=FACE_OUTER_BOUND('',#3157,.T.);
#2632=FACE_OUTER_BOUND('',#3158,.T.);
#2633=FACE_OUTER_BOUND('',#3159,.T.);
#2634=FACE_OUTER_BOUND('',#3160,.T.);
#2635=FACE_OUTER_BOUND('',#3161,.T.);
#2636=FACE_OUTER_BOUND('',#3162,.T.);
#2637=FACE_OUTER_BOUND('',#3163,.T.);
#2638=FACE_OUTER_BOUND('',#3164,.T.);
#2639=FACE_OUTER_BOUND('',#3165,.T.);
#2640=FACE_OUTER_BOUND('',#3166,.T.);
#2641=FACE_OUTER_BOUND('',#3167,.T.);
#2642=FACE_OUTER_BOUND('',#3168,.T.);
#2643=FACE_OUTER_BOUND('',#3169,.T.);
#2644=FACE_OUTER_BOUND('',#3170,.T.);
#2645=FACE_OUTER_BOUND('',#3171,.T.);
#2646=FACE_OUTER_BOUND('',#3172,.T.);
#2647=FACE_OUTER_BOUND('',#3182,.T.);
#2648=FACE_OUTER_BOUND('',#3192,.T.);
#2649=FACE_OUTER_BOUND('',#3193,.T.);
#2650=FACE_OUTER_BOUND('',#3194,.T.);
#2651=FACE_OUTER_BOUND('',#3195,.T.);
#2652=FACE_OUTER_BOUND('',#3196,.T.);
#2653=FACE_OUTER_BOUND('',#3197,.T.);
#2654=FACE_OUTER_BOUND('',#3198,.T.);
#2655=FACE_OUTER_BOUND('',#3199,.T.);
#2656=FACE_OUTER_BOUND('',#3200,.T.);
#2657=FACE_OUTER_BOUND('',#3201,.T.);
#2658=FACE_OUTER_BOUND('',#3206,.T.);
#2659=FACE_OUTER_BOUND('',#3207,.T.);
#2660=FACE_OUTER_BOUND('',#3208,.T.);
#2661=FACE_OUTER_BOUND('',#3209,.T.);
#2662=FACE_OUTER_BOUND('',#3210,.T.);
#2663=FACE_OUTER_BOUND('',#3211,.T.);
#2664=FACE_OUTER_BOUND('',#3212,.T.);
#2665=FACE_OUTER_BOUND('',#3213,.T.);
#2666=FACE_OUTER_BOUND('',#3218,.T.);
#2667=FACE_OUTER_BOUND('',#3221,.T.);
#2668=FACE_OUTER_BOUND('',#3222,.T.);
#2669=FACE_OUTER_BOUND('',#3223,.T.);
#2670=FACE_OUTER_BOUND('',#3224,.T.);
#2671=FACE_OUTER_BOUND('',#3225,.T.);
#2672=FACE_OUTER_BOUND('',#3226,.T.);
#2673=FACE_OUTER_BOUND('',#3227,.T.);
#2674=FACE_OUTER_BOUND('',#3228,.T.);
#2675=FACE_OUTER_BOUND('',#3229,.T.);
#2676=FACE_OUTER_BOUND('',#3230,.T.);
#2677=FACE_OUTER_BOUND('',#3231,.T.);
#2678=FACE_OUTER_BOUND('',#3232,.T.);
#2679=FACE_OUTER_BOUND('',#3233,.T.);
#2680=FACE_OUTER_BOUND('',#3234,.T.);
#2681=FACE_OUTER_BOUND('',#3235,.T.);
#2682=FACE_OUTER_BOUND('',#3236,.T.);
#2683=FACE_OUTER_BOUND('',#3238,.T.);
#2684=FACE_OUTER_BOUND('',#3239,.T.);
#2685=FACE_OUTER_BOUND('',#3240,.T.);
#2686=FACE_OUTER_BOUND('',#3241,.T.);
#2687=FACE_OUTER_BOUND('',#3242,.T.);
#2688=FACE_OUTER_BOUND('',#3243,.T.);
#2689=FACE_OUTER_BOUND('',#3244,.T.);
#2690=FACE_OUTER_BOUND('',#3245,.T.);
#2691=FACE_OUTER_BOUND('',#3247,.T.);
#2692=FACE_OUTER_BOUND('',#3248,.T.);
#2693=FACE_OUTER_BOUND('',#3249,.T.);
#2694=FACE_OUTER_BOUND('',#3250,.T.);
#2695=FACE_OUTER_BOUND('',#3251,.T.);
#2696=FACE_OUTER_BOUND('',#3252,.T.);
#2697=FACE_OUTER_BOUND('',#3253,.T.);
#2698=FACE_OUTER_BOUND('',#3254,.T.);
#2699=FACE_OUTER_BOUND('',#3255,.T.);
#2700=FACE_OUTER_BOUND('',#3256,.T.);
#2701=FACE_OUTER_BOUND('',#3259,.T.);
#2702=FACE_OUTER_BOUND('',#3260,.T.);
#2703=FACE_OUTER_BOUND('',#3261,.T.);
#2704=FACE_OUTER_BOUND('',#3262,.T.);
#2705=FACE_OUTER_BOUND('',#3263,.T.);
#2706=FACE_OUTER_BOUND('',#3264,.T.);
#2707=FACE_OUTER_BOUND('',#3266,.T.);
#2708=FACE_OUTER_BOUND('',#3267,.T.);
#2709=FACE_OUTER_BOUND('',#3268,.T.);
#2710=FACE_OUTER_BOUND('',#3271,.T.);
#2711=FACE_OUTER_BOUND('',#3274,.T.);
#2712=FACE_OUTER_BOUND('',#3276,.T.);
#2713=FACE_OUTER_BOUND('',#3277,.T.);
#2714=FACE_OUTER_BOUND('',#3278,.T.);
#2715=FACE_OUTER_BOUND('',#3279,.T.);
#2716=FACE_OUTER_BOUND('',#3280,.T.);
#2717=FACE_OUTER_BOUND('',#3281,.T.);
#2718=FACE_OUTER_BOUND('',#3283,.T.);
#2719=FACE_OUTER_BOUND('',#3284,.T.);
#2720=FACE_OUTER_BOUND('',#3286,.T.);
#2721=FACE_OUTER_BOUND('',#3287,.T.);
#2722=FACE_OUTER_BOUND('',#3289,.T.);
#2723=FACE_OUTER_BOUND('',#3290,.T.);
#2724=FACE_OUTER_BOUND('',#3291,.T.);
#2725=FACE_OUTER_BOUND('',#3292,.T.);
#2726=FACE_OUTER_BOUND('',#3294,.T.);
#2727=FACE_OUTER_BOUND('',#3295,.T.);
#2728=FACE_OUTER_BOUND('',#3297,.T.);
#2729=FACE_OUTER_BOUND('',#3298,.T.);
#2730=FACE_OUTER_BOUND('',#3300,.T.);
#2731=FACE_OUTER_BOUND('',#3301,.T.);
#2732=FACE_OUTER_BOUND('',#3302,.T.);
#2733=FACE_OUTER_BOUND('',#3303,.T.);
#2734=FACE_OUTER_BOUND('',#3304,.T.);
#2735=FACE_OUTER_BOUND('',#3305,.T.);
#2736=FACE_OUTER_BOUND('',#3307,.T.);
#2737=FACE_OUTER_BOUND('',#3308,.T.);
#2738=FACE_OUTER_BOUND('',#3309,.T.);
#2739=FACE_OUTER_BOUND('',#3310,.T.);
#2740=FACE_OUTER_BOUND('',#3311,.T.);
#2741=FACE_OUTER_BOUND('',#3312,.T.);
#2742=FACE_OUTER_BOUND('',#3313,.T.);
#2743=FACE_OUTER_BOUND('',#3314,.T.);
#2744=FACE_OUTER_BOUND('',#3315,.T.);
#2745=FACE_OUTER_BOUND('',#3316,.T.);
#2746=FACE_OUTER_BOUND('',#3317,.T.);
#2747=FACE_OUTER_BOUND('',#3318,.T.);
#2748=FACE_OUTER_BOUND('',#3319,.T.);
#2749=FACE_OUTER_BOUND('',#3320,.T.);
#2750=FACE_OUTER_BOUND('',#3321,.T.);
#2751=FACE_OUTER_BOUND('',#3322,.T.);
#2752=FACE_OUTER_BOUND('',#3323,.T.);
#2753=FACE_OUTER_BOUND('',#3324,.T.);
#2754=FACE_OUTER_BOUND('',#3325,.T.);
#2755=FACE_OUTER_BOUND('',#3326,.T.);
#2756=FACE_OUTER_BOUND('',#3327,.T.);
#2757=FACE_OUTER_BOUND('',#3328,.T.);
#2758=FACE_OUTER_BOUND('',#3329,.T.);
#2759=FACE_OUTER_BOUND('',#3330,.T.);
#2760=FACE_OUTER_BOUND('',#3331,.T.);
#2761=FACE_OUTER_BOUND('',#3332,.T.);
#2762=FACE_OUTER_BOUND('',#3333,.T.);
#2763=FACE_OUTER_BOUND('',#3334,.T.);
#2764=FACE_OUTER_BOUND('',#3335,.T.);
#2765=FACE_OUTER_BOUND('',#3336,.T.);
#2766=FACE_OUTER_BOUND('',#3337,.T.);
#2767=FACE_OUTER_BOUND('',#3338,.T.);
#2768=FACE_OUTER_BOUND('',#3339,.T.);
#2769=FACE_OUTER_BOUND('',#3340,.T.);
#2770=FACE_OUTER_BOUND('',#3341,.T.);
#2771=FACE_OUTER_BOUND('',#3342,.T.);
#2772=FACE_OUTER_BOUND('',#3343,.T.);
#2773=FACE_OUTER_BOUND('',#3344,.T.);
#2774=FACE_OUTER_BOUND('',#3346,.T.);
#2775=FACE_OUTER_BOUND('',#3347,.T.);
#2776=FACE_OUTER_BOUND('',#3349,.T.);
#2777=FACE_OUTER_BOUND('',#3350,.T.);
#2778=FACE_OUTER_BOUND('',#3351,.T.);
#2779=FACE_OUTER_BOUND('',#3353,.T.);
#2780=FACE_OUTER_BOUND('',#3354,.T.);
#2781=FACE_OUTER_BOUND('',#3355,.T.);
#2782=FACE_OUTER_BOUND('',#3356,.T.);
#2783=FACE_OUTER_BOUND('',#3358,.T.);
#2784=FACE_OUTER_BOUND('',#3359,.T.);
#2785=FACE_OUTER_BOUND('',#3360,.T.);
#2786=FACE_OUTER_BOUND('',#3362,.T.);
#2787=FACE_OUTER_BOUND('',#3363,.T.);
#2788=FACE_OUTER_BOUND('',#3364,.T.);
#2789=FACE_OUTER_BOUND('',#3366,.T.);
#2790=FACE_OUTER_BOUND('',#3367,.T.);
#2791=FACE_OUTER_BOUND('',#3369,.T.);
#2792=FACE_OUTER_BOUND('',#3370,.T.);
#2793=FACE_OUTER_BOUND('',#3372,.T.);
#2794=FACE_OUTER_BOUND('',#3373,.T.);
#2795=FACE_OUTER_BOUND('',#3374,.T.);
#2796=FACE_OUTER_BOUND('',#3375,.T.);
#2797=FACE_OUTER_BOUND('',#3377,.T.);
#2798=FACE_OUTER_BOUND('',#3378,.T.);
#2799=FACE_OUTER_BOUND('',#3380,.T.);
#2800=FACE_OUTER_BOUND('',#3381,.T.);
#2801=FACE_OUTER_BOUND('',#3383,.T.);
#2802=FACE_OUTER_BOUND('',#3384,.T.);
#2803=FACE_OUTER_BOUND('',#3385,.T.);
#2804=FACE_OUTER_BOUND('',#3386,.T.);
#2805=FACE_OUTER_BOUND('',#3388,.T.);
#2806=FACE_OUTER_BOUND('',#3389,.T.);
#2807=FACE_OUTER_BOUND('',#3390,.T.);
#2808=FACE_OUTER_BOUND('',#3391,.T.);
#2809=FACE_OUTER_BOUND('',#3393,.T.);
#2810=FACE_OUTER_BOUND('',#3394,.T.);
#2811=FACE_OUTER_BOUND('',#3395,.T.);
#2812=FACE_OUTER_BOUND('',#3396,.T.);
#2813=FACE_OUTER_BOUND('',#3397,.T.);
#2814=FACE_OUTER_BOUND('',#3399,.T.);
#2815=FACE_OUTER_BOUND('',#3400,.T.);
#2816=FACE_OUTER_BOUND('',#3402,.T.);
#2817=FACE_OUTER_BOUND('',#3403,.T.);
#2818=FACE_OUTER_BOUND('',#3404,.T.);
#2819=FACE_OUTER_BOUND('',#3405,.T.);
#2820=FACE_OUTER_BOUND('',#3406,.T.);
#2821=FACE_OUTER_BOUND('',#3407,.T.);
#2822=FACE_OUTER_BOUND('',#3408,.T.);
#2823=FACE_OUTER_BOUND('',#3410,.T.);
#2824=FACE_OUTER_BOUND('',#3411,.T.);
#2825=FACE_OUTER_BOUND('',#3413,.T.);
#2826=FACE_OUTER_BOUND('',#3414,.T.);
#2827=FACE_OUTER_BOUND('',#3415,.T.);
#2828=FACE_OUTER_BOUND('',#3416,.T.);
#2829=FACE_OUTER_BOUND('',#3417,.T.);
#2830=FACE_OUTER_BOUND('',#3418,.T.);
#2831=FACE_OUTER_BOUND('',#3419,.T.);
#2832=FACE_OUTER_BOUND('',#3420,.T.);
#2833=FACE_OUTER_BOUND('',#3421,.T.);
#2834=FACE_OUTER_BOUND('',#3422,.T.);
#2835=FACE_OUTER_BOUND('',#3423,.T.);
#2836=FACE_OUTER_BOUND('',#3424,.T.);
#2837=FACE_OUTER_BOUND('',#3425,.T.);
#2838=FACE_OUTER_BOUND('',#3426,.T.);
#2839=FACE_OUTER_BOUND('',#3427,.T.);
#2840=FACE_OUTER_BOUND('',#3428,.T.);
#2841=FACE_OUTER_BOUND('',#3429,.T.);
#2842=FACE_OUTER_BOUND('',#3430,.T.);
#2843=FACE_OUTER_BOUND('',#3431,.T.);
#2844=FACE_OUTER_BOUND('',#3432,.T.);
#2845=FACE_OUTER_BOUND('',#3433,.T.);
#2846=FACE_OUTER_BOUND('',#3434,.T.);
#2847=FACE_OUTER_BOUND('',#3435,.T.);
#2848=FACE_OUTER_BOUND('',#3436,.T.);
#2849=FACE_OUTER_BOUND('',#3437,.T.);
#2850=FACE_OUTER_BOUND('',#3438,.T.);
#2851=FACE_OUTER_BOUND('',#3439,.T.);
#2852=FACE_OUTER_BOUND('',#3440,.T.);
#2853=FACE_OUTER_BOUND('',#3441,.T.);
#2854=FACE_OUTER_BOUND('',#3442,.T.);
#2855=FACE_OUTER_BOUND('',#3443,.T.);
#2856=FACE_OUTER_BOUND('',#3444,.T.);
#2857=FACE_OUTER_BOUND('',#3445,.T.);
#2858=FACE_OUTER_BOUND('',#3446,.T.);
#2859=FACE_OUTER_BOUND('',#3447,.T.);
#2860=FACE_OUTER_BOUND('',#3448,.T.);
#2861=FACE_OUTER_BOUND('',#3449,.T.);
#2862=FACE_OUTER_BOUND('',#3450,.T.);
#2863=FACE_OUTER_BOUND('',#3451,.T.);
#2864=FACE_OUTER_BOUND('',#3452,.T.);
#2865=FACE_OUTER_BOUND('',#3453,.T.);
#2866=FACE_OUTER_BOUND('',#3454,.T.);
#2867=FACE_OUTER_BOUND('',#3456,.T.);
#2868=FACE_OUTER_BOUND('',#3457,.T.);
#2869=FACE_OUTER_BOUND('',#3458,.T.);
#2870=FACE_OUTER_BOUND('',#3460,.T.);
#2871=FACE_OUTER_BOUND('',#3461,.T.);
#2872=FACE_OUTER_BOUND('',#3462,.T.);
#2873=FACE_OUTER_BOUND('',#3463,.T.);
#2874=FACE_OUTER_BOUND('',#3464,.T.);
#2875=FACE_OUTER_BOUND('',#3465,.T.);
#2876=FACE_OUTER_BOUND('',#3466,.T.);
#2877=FACE_OUTER_BOUND('',#3467,.T.);
#2878=FACE_OUTER_BOUND('',#3468,.T.);
#2879=FACE_OUTER_BOUND('',#3469,.T.);
#2880=FACE_OUTER_BOUND('',#3470,.T.);
#2881=FACE_OUTER_BOUND('',#3471,.T.);
#2882=FACE_OUTER_BOUND('',#3472,.T.);
#2883=FACE_OUTER_BOUND('',#3473,.T.);
#2884=FACE_OUTER_BOUND('',#3474,.T.);
#2885=FACE_OUTER_BOUND('',#3475,.T.);
#2886=FACE_OUTER_BOUND('',#3476,.T.);
#2887=FACE_OUTER_BOUND('',#3477,.T.);
#2888=FACE_OUTER_BOUND('',#3478,.T.);
#2889=FACE_OUTER_BOUND('',#3479,.T.);
#2890=FACE_OUTER_BOUND('',#3480,.T.);
#2891=FACE_OUTER_BOUND('',#3481,.T.);
#2892=FACE_OUTER_BOUND('',#3482,.T.);
#2893=FACE_OUTER_BOUND('',#3483,.T.);
#2894=FACE_OUTER_BOUND('',#3484,.T.);
#2895=FACE_OUTER_BOUND('',#3485,.T.);
#2896=FACE_OUTER_BOUND('',#3486,.T.);
#2897=FACE_OUTER_BOUND('',#3487,.T.);
#2898=FACE_OUTER_BOUND('',#3488,.T.);
#2899=FACE_OUTER_BOUND('',#3489,.T.);
#2900=FACE_OUTER_BOUND('',#3490,.T.);
#2901=FACE_OUTER_BOUND('',#3491,.T.);
#2902=FACE_OUTER_BOUND('',#3492,.T.);
#2903=EDGE_LOOP('',(#6415,#6416,#6417,#6418,#6419));
#2904=EDGE_LOOP('',(#6420,#6421,#6422,#6423,#6424,#6425));
#2905=EDGE_LOOP('',(#6426,#6427,#6428,#6429,#6430,#6431));
#2906=EDGE_LOOP('',(#6432));
#2907=EDGE_LOOP('',(#6433,#6434,#6435,#6436,#6437));
#2908=EDGE_LOOP('',(#6438,#6439,#6440,#6441,#6442,#6443,#6444,#6445,#6446));
#2909=EDGE_LOOP('',(#6447));
#2910=EDGE_LOOP('',(#6448,#6449,#6450,#6451,#6452));
#2911=EDGE_LOOP('',(#6453,#6454,#6455,#6456,#6457,#6458));
#2912=EDGE_LOOP('',(#6459,#6460,#6461,#6462,#6463));
#2913=EDGE_LOOP('',(#6464));
#2914=EDGE_LOOP('',(#6465,#6466,#6467,#6468,#6469));
#2915=EDGE_LOOP('',(#6470,#6471,#6472,#6473,#6474,#6475,#6476,#6477,#6478,
#6479,#6480));
#2916=EDGE_LOOP('',(#6481));
#2917=EDGE_LOOP('',(#6482,#6483,#6484,#6485,#6486));
#2918=EDGE_LOOP('',(#6487,#6488,#6489,#6490));
#2919=EDGE_LOOP('',(#6491,#6492,#6493));
#2920=EDGE_LOOP('',(#6494,#6495,#6496,#6497,#6498,#6499,#6500,#6501));
#2921=EDGE_LOOP('',(#6502,#6503,#6504,#6505));
#2922=EDGE_LOOP('',(#6506,#6507,#6508));
#2923=EDGE_LOOP('',(#6509,#6510,#6511,#6512));
#2924=EDGE_LOOP('',(#6513,#6514,#6515));
#2925=EDGE_LOOP('',(#6516,#6517,#6518,#6519));
#2926=EDGE_LOOP('',(#6520,#6521,#6522,#6523,#6524));
#2927=EDGE_LOOP('',(#6525,#6526,#6527,#6528));
#2928=EDGE_LOOP('',(#6529,#6530,#6531,#6532));
#2929=EDGE_LOOP('',(#6533,#6534,#6535,#6536));
#2930=EDGE_LOOP('',(#6537,#6538,#6539,#6540));
#2931=EDGE_LOOP('',(#6541,#6542,#6543,#6544));
#2932=EDGE_LOOP('',(#6545,#6546,#6547,#6548,#6549,#6550));
#2933=EDGE_LOOP('',(#6551,#6552,#6553,#6554));
#2934=EDGE_LOOP('',(#6555,#6556,#6557,#6558));
#2935=EDGE_LOOP('',(#6559,#6560,#6561,#6562,#6563,#6564));
#2936=EDGE_LOOP('',(#6565,#6566));
#2937=EDGE_LOOP('',(#6567,#6568,#6569));
#2938=EDGE_LOOP('',(#6570,#6571,#6572,#6573));
#2939=EDGE_LOOP('',(#6574,#6575,#6576,#6577,#6578,#6579));
#2940=EDGE_LOOP('',(#6580,#6581,#6582,#6583,#6584));
#2941=EDGE_LOOP('',(#6585,#6586,#6587,#6588,#6589));
#2942=EDGE_LOOP('',(#6590,#6591,#6592,#6593));
#2943=EDGE_LOOP('',(#6594,#6595,#6596,#6597));
#2944=EDGE_LOOP('',(#6598,#6599,#6600));
#2945=EDGE_LOOP('',(#6601,#6602,#6603,#6604));
#2946=EDGE_LOOP('',(#6605,#6606,#6607,#6608));
#2947=EDGE_LOOP('',(#6609,#6610,#6611,#6612,#6613));
#2948=EDGE_LOOP('',(#6614,#6615,#6616,#6617,#6618,#6619,#6620,#6621,#6622,
#6623));
#2949=EDGE_LOOP('',(#6624,#6625,#6626,#6627,#6628,#6629,#6630));
#2950=EDGE_LOOP('',(#6631,#6632,#6633,#6634));
#2951=EDGE_LOOP('',(#6635,#6636,#6637,#6638));
#2952=EDGE_LOOP('',(#6639,#6640,#6641,#6642));
#2953=EDGE_LOOP('',(#6643,#6644,#6645,#6646));
#2954=EDGE_LOOP('',(#6647,#6648,#6649,#6650));
#2955=EDGE_LOOP('',(#6651,#6652,#6653));
#2956=EDGE_LOOP('',(#6654,#6655,#6656));
#2957=EDGE_LOOP('',(#6657,#6658,#6659,#6660));
#2958=EDGE_LOOP('',(#6661,#6662,#6663,#6664,#6665));
#2959=EDGE_LOOP('',(#6666,#6667,#6668,#6669,#6670));
#2960=EDGE_LOOP('',(#6671,#6672,#6673,#6674));
#2961=EDGE_LOOP('',(#6675,#6676,#6677,#6678,#6679,#6680,#6681,#6682,#6683));
#2962=EDGE_LOOP('',(#6684,#6685,#6686,#6687,#6688));
#2963=EDGE_LOOP('',(#6689,#6690,#6691,#6692));
#2964=EDGE_LOOP('',(#6693,#6694,#6695,#6696,#6697,#6698,#6699,#6700));
#2965=EDGE_LOOP('',(#6701,#6702,#6703,#6704,#6705));
#2966=EDGE_LOOP('',(#6706,#6707,#6708,#6709));
#2967=EDGE_LOOP('',(#6710,#6711,#6712));
#2968=EDGE_LOOP('',(#6713,#6714,#6715,#6716));
#2969=EDGE_LOOP('',(#6717,#6718,#6719,#6720));
#2970=EDGE_LOOP('',(#6721,#6722,#6723,#6724,#6725));
#2971=EDGE_LOOP('',(#6726,#6727,#6728,#6729));
#2972=EDGE_LOOP('',(#6730,#6731,#6732,#6733,#6734));
#2973=EDGE_LOOP('',(#6735,#6736,#6737,#6738));
#2974=EDGE_LOOP('',(#6739,#6740,#6741,#6742));
#2975=EDGE_LOOP('',(#6743,#6744,#6745,#6746));
#2976=EDGE_LOOP('',(#6747,#6748,#6749,#6750));
#2977=EDGE_LOOP('',(#6751,#6752,#6753,#6754));
#2978=EDGE_LOOP('',(#6755,#6756,#6757,#6758));
#2979=EDGE_LOOP('',(#6759,#6760,#6761,#6762,#6763));
#2980=EDGE_LOOP('',(#6764,#6765,#6766,#6767,#6768));
#2981=EDGE_LOOP('',(#6769,#6770,#6771,#6772,#6773));
#2982=EDGE_LOOP('',(#6774,#6775,#6776,#6777));
#2983=EDGE_LOOP('',(#6778,#6779,#6780,#6781));
#2984=EDGE_LOOP('',(#6782,#6783,#6784,#6785,#6786));
#2985=EDGE_LOOP('',(#6787,#6788,#6789,#6790));
#2986=EDGE_LOOP('',(#6791,#6792,#6793,#6794));
#2987=EDGE_LOOP('',(#6795,#6796,#6797,#6798));
#2988=EDGE_LOOP('',(#6799,#6800,#6801,#6802));
#2989=EDGE_LOOP('',(#6803,#6804,#6805,#6806));
#2990=EDGE_LOOP('',(#6807,#6808,#6809,#6810));
#2991=EDGE_LOOP('',(#6811,#6812,#6813,#6814));
#2992=EDGE_LOOP('',(#6815,#6816,#6817,#6818));
#2993=EDGE_LOOP('',(#6819,#6820,#6821,#6822,#6823));
#2994=EDGE_LOOP('',(#6824,#6825,#6826,#6827));
#2995=EDGE_LOOP('',(#6828,#6829,#6830,#6831));
#2996=EDGE_LOOP('',(#6832,#6833,#6834,#6835));
#2997=EDGE_LOOP('',(#6836,#6837,#6838,#6839,#6840,#6841,#6842,#6843));
#2998=EDGE_LOOP('',(#6844,#6845,#6846,#6847,#6848,#6849));
#2999=EDGE_LOOP('',(#6850,#6851,#6852,#6853));
#3000=EDGE_LOOP('',(#6854,#6855,#6856,#6857));
#3001=EDGE_LOOP('',(#6858,#6859,#6860,#6861));
#3002=EDGE_LOOP('',(#6862,#6863,#6864,#6865));
#3003=EDGE_LOOP('',(#6866,#6867,#6868,#6869));
#3004=EDGE_LOOP('',(#6870,#6871,#6872,#6873,#6874,#6875,#6876,#6877,#6878,
#6879,#6880,#6881,#6882,#6883,#6884,#6885,#6886,#6887,#6888));
#3005=EDGE_LOOP('',(#6889));
#3006=EDGE_LOOP('',(#6890));
#3007=EDGE_LOOP('',(#6891));
#3008=EDGE_LOOP('',(#6892));
#3009=EDGE_LOOP('',(#6893,#6894,#6895,#6896));
#3010=EDGE_LOOP('',(#6897,#6898,#6899,#6900));
#3011=EDGE_LOOP('',(#6901,#6902,#6903,#6904));
#3012=EDGE_LOOP('',(#6905,#6906,#6907));
#3013=EDGE_LOOP('',(#6908,#6909,#6910));
#3014=EDGE_LOOP('',(#6911,#6912,#6913,#6914));
#3015=EDGE_LOOP('',(#6915,#6916,#6917,#6918,#6919));
#3016=EDGE_LOOP('',(#6920,#6921,#6922,#6923,#6924));
#3017=EDGE_LOOP('',(#6925,#6926,#6927,#6928,#6929,#6930,#6931,#6932,#6933,
#6934,#6935,#6936,#6937,#6938,#6939,#6940,#6941,#6942,#6943,#6944,#6945,
#6946,#6947,#6948,#6949,#6950,#6951));
#3018=EDGE_LOOP('',(#6952));
#3019=EDGE_LOOP('',(#6953));
#3020=EDGE_LOOP('',(#6954));
#3021=EDGE_LOOP('',(#6955));
#3022=EDGE_LOOP('',(#6956,#6957,#6958,#6959));
#3023=EDGE_LOOP('',(#6960,#6961,#6962,#6963));
#3024=EDGE_LOOP('',(#6964,#6965,#6966,#6967));
#3025=EDGE_LOOP('',(#6968,#6969,#6970,#6971));
#3026=EDGE_LOOP('',(#6972,#6973,#6974,#6975));
#3027=EDGE_LOOP('',(#6976,#6977,#6978));
#3028=EDGE_LOOP('',(#6979,#6980,#6981));
#3029=EDGE_LOOP('',(#6982,#6983,#6984,#6985));
#3030=EDGE_LOOP('',(#6986,#6987,#6988,#6989));
#3031=EDGE_LOOP('',(#6990,#6991,#6992,#6993,#6994,#6995));
#3032=EDGE_LOOP('',(#6996,#6997,#6998,#6999,#7000,#7001,#7002,#7003,#7004,
#7005,#7006,#7007,#7008,#7009));
#3033=EDGE_LOOP('',(#7010,#7011,#7012,#7013,#7014));
#3034=EDGE_LOOP('',(#7015,#7016,#7017,#7018));
#3035=EDGE_LOOP('',(#7019,#7020,#7021,#7022,#7023));
#3036=EDGE_LOOP('',(#7024,#7025,#7026,#7027,#7028));
#3037=EDGE_LOOP('',(#7029,#7030,#7031,#7032,#7033,#7034,#7035,#7036));
#3038=EDGE_LOOP('',(#7037,#7038,#7039,#7040,#7041));
#3039=EDGE_LOOP('',(#7042,#7043,#7044));
#3040=EDGE_LOOP('',(#7045,#7046,#7047));
#3041=EDGE_LOOP('',(#7048,#7049,#7050,#7051));
#3042=EDGE_LOOP('',(#7052,#7053,#7054,#7055));
#3043=EDGE_LOOP('',(#7056,#7057,#7058,#7059,#7060));
#3044=EDGE_LOOP('',(#7061,#7062,#7063,#7064,#7065));
#3045=EDGE_LOOP('',(#7066,#7067,#7068,#7069));
#3046=EDGE_LOOP('',(#7070,#7071,#7072,#7073,#7074,#7075));
#3047=EDGE_LOOP('',(#7076,#7077,#7078));
#3048=EDGE_LOOP('',(#7079,#7080,#7081));
#3049=EDGE_LOOP('',(#7082,#7083,#7084,#7085));
#3050=EDGE_LOOP('',(#7086,#7087,#7088,#7089));
#3051=EDGE_LOOP('',(#7090,#7091,#7092,#7093,#7094,#7095));
#3052=EDGE_LOOP('',(#7096,#7097,#7098,#7099));
#3053=EDGE_LOOP('',(#7100,#7101,#7102,#7103,#7104));
#3054=EDGE_LOOP('',(#7105,#7106,#7107,#7108));
#3055=EDGE_LOOP('',(#7109,#7110,#7111,#7112));
#3056=EDGE_LOOP('',(#7113,#7114,#7115,#7116));
#3057=EDGE_LOOP('',(#7117,#7118,#7119));
#3058=EDGE_LOOP('',(#7120,#7121,#7122,#7123,#7124,#7125));
#3059=EDGE_LOOP('',(#7126,#7127,#7128,#7129));
#3060=EDGE_LOOP('',(#7130,#7131,#7132,#7133,#7134));
#3061=EDGE_LOOP('',(#7135,#7136,#7137,#7138));
#3062=EDGE_LOOP('',(#7139,#7140,#7141,#7142,#7143,#7144,#7145,#7146));
#3063=EDGE_LOOP('',(#7147,#7148,#7149,#7150,#7151,#7152,#7153));
#3064=EDGE_LOOP('',(#7154,#7155,#7156,#7157));
#3065=EDGE_LOOP('',(#7158,#7159,#7160,#7161));
#3066=EDGE_LOOP('',(#7162,#7163,#7164,#7165));
#3067=EDGE_LOOP('',(#7166,#7167,#7168,#7169));
#3068=EDGE_LOOP('',(#7170,#7171,#7172));
#3069=EDGE_LOOP('',(#7173,#7174,#7175));
#3070=EDGE_LOOP('',(#7176,#7177,#7178));
#3071=EDGE_LOOP('',(#7179,#7180,#7181,#7182));
#3072=EDGE_LOOP('',(#7183,#7184,#7185,#7186));
#3073=EDGE_LOOP('',(#7187,#7188,#7189,#7190));
#3074=EDGE_LOOP('',(#7191,#7192,#7193,#7194));
#3075=EDGE_LOOP('',(#7195,#7196,#7197,#7198));
#3076=EDGE_LOOP('',(#7199,#7200,#7201,#7202));
#3077=EDGE_LOOP('',(#7203,#7204,#7205,#7206));
#3078=EDGE_LOOP('',(#7207,#7208,#7209,#7210));
#3079=EDGE_LOOP('',(#7211,#7212,#7213,#7214));
#3080=EDGE_LOOP('',(#7215,#7216,#7217,#7218));
#3081=EDGE_LOOP('',(#7219,#7220,#7221,#7222));
#3082=EDGE_LOOP('',(#7223,#7224,#7225,#7226));
#3083=EDGE_LOOP('',(#7227,#7228,#7229,#7230,#7231,#7232,#7233,#7234));
#3084=EDGE_LOOP('',(#7235,#7236,#7237,#7238,#7239,#7240,#7241,#7242,#7243,
#7244,#7245,#7246));
#3085=EDGE_LOOP('',(#7247));
#3086=EDGE_LOOP('',(#7248));
#3087=EDGE_LOOP('',(#7249));
#3088=EDGE_LOOP('',(#7250));
#3089=EDGE_LOOP('',(#7251));
#3090=EDGE_LOOP('',(#7252));
#3091=EDGE_LOOP('',(#7253,#7254,#7255));
#3092=EDGE_LOOP('',(#7256,#7257,#7258,#7259));
#3093=EDGE_LOOP('',(#7260,#7261,#7262,#7263));
#3094=EDGE_LOOP('',(#7264,#7265,#7266));
#3095=EDGE_LOOP('',(#7267,#7268,#7269,#7270));
#3096=EDGE_LOOP('',(#7271,#7272,#7273,#7274));
#3097=EDGE_LOOP('',(#7275,#7276,#7277));
#3098=EDGE_LOOP('',(#7278,#7279,#7280,#7281));
#3099=EDGE_LOOP('',(#7282,#7283,#7284,#7285));
#3100=EDGE_LOOP('',(#7286,#7287,#7288));
#3101=EDGE_LOOP('',(#7289,#7290,#7291,#7292));
#3102=EDGE_LOOP('',(#7293,#7294,#7295,#7296));
#3103=EDGE_LOOP('',(#7297,#7298,#7299));
#3104=EDGE_LOOP('',(#7300,#7301,#7302,#7303));
#3105=EDGE_LOOP('',(#7304,#7305,#7306));
#3106=EDGE_LOOP('',(#7307,#7308,#7309,#7310));
#3107=EDGE_LOOP('',(#7311,#7312,#7313,#7314));
#3108=EDGE_LOOP('',(#7315,#7316,#7317,#7318));
#3109=EDGE_LOOP('',(#7319,#7320,#7321,#7322));
#3110=EDGE_LOOP('',(#7323,#7324,#7325,#7326));
#3111=EDGE_LOOP('',(#7327,#7328,#7329,#7330));
#3112=EDGE_LOOP('',(#7331,#7332,#7333,#7334));
#3113=EDGE_LOOP('',(#7335,#7336,#7337,#7338));
#3114=EDGE_LOOP('',(#7339));
#3115=EDGE_LOOP('',(#7340,#7341,#7342,#7343));
#3116=EDGE_LOOP('',(#7344,#7345,#7346,#7347));
#3117=EDGE_LOOP('',(#7348,#7349,#7350,#7351));
#3118=EDGE_LOOP('',(#7352,#7353,#7354,#7355));
#3119=EDGE_LOOP('',(#7356,#7357,#7358,#7359));
#3120=EDGE_LOOP('',(#7360,#7361,#7362,#7363));
#3121=EDGE_LOOP('',(#7364,#7365,#7366,#7367));
#3122=EDGE_LOOP('',(#7368,#7369,#7370,#7371));
#3123=EDGE_LOOP('',(#7372,#7373,#7374,#7375,#7376,#7377,#7378,#7379,#7380,
#7381,#7382,#7383));
#3124=EDGE_LOOP('',(#7384,#7385,#7386,#7387));
#3125=EDGE_LOOP('',(#7388,#7389,#7390,#7391));
#3126=EDGE_LOOP('',(#7392));
#3127=EDGE_LOOP('',(#7393,#7394,#7395,#7396));
#3128=EDGE_LOOP('',(#7397,#7398,#7399,#7400));
#3129=EDGE_LOOP('',(#7401,#7402,#7403,#7404,#7405,#7406,#7407,#7408));
#3130=EDGE_LOOP('',(#7409));
#3131=EDGE_LOOP('',(#7410));
#3132=EDGE_LOOP('',(#7411));
#3133=EDGE_LOOP('',(#7412));
#3134=EDGE_LOOP('',(#7413,#7414,#7415,#7416));
#3135=EDGE_LOOP('',(#7417,#7418,#7419,#7420));
#3136=EDGE_LOOP('',(#7421,#7422,#7423,#7424));
#3137=EDGE_LOOP('',(#7425,#7426,#7427,#7428));
#3138=EDGE_LOOP('',(#7429,#7430,#7431,#7432));
#3139=EDGE_LOOP('',(#7433,#7434,#7435,#7436));
#3140=EDGE_LOOP('',(#7437,#7438,#7439,#7440));
#3141=EDGE_LOOP('',(#7441,#7442,#7443,#7444));
#3142=EDGE_LOOP('',(#7445,#7446,#7447,#7448));
#3143=EDGE_LOOP('',(#7449,#7450,#7451,#7452));
#3144=EDGE_LOOP('',(#7453,#7454,#7455,#7456));
#3145=EDGE_LOOP('',(#7457,#7458,#7459,#7460));
#3146=EDGE_LOOP('',(#7461,#7462,#7463,#7464));
#3147=EDGE_LOOP('',(#7465,#7466,#7467,#7468));
#3148=EDGE_LOOP('',(#7469,#7470,#7471,#7472));
#3149=EDGE_LOOP('',(#7473,#7474,#7475,#7476));
#3150=EDGE_LOOP('',(#7477,#7478,#7479,#7480));
#3151=EDGE_LOOP('',(#7481,#7482,#7483,#7484));
#3152=EDGE_LOOP('',(#7485,#7486,#7487,#7488));
#3153=EDGE_LOOP('',(#7489,#7490,#7491,#7492));
#3154=EDGE_LOOP('',(#7493,#7494,#7495,#7496));
#3155=EDGE_LOOP('',(#7497,#7498,#7499,#7500));
#3156=EDGE_LOOP('',(#7501,#7502,#7503,#7504));
#3157=EDGE_LOOP('',(#7505,#7506,#7507,#7508));
#3158=EDGE_LOOP('',(#7509,#7510,#7511,#7512));
#3159=EDGE_LOOP('',(#7513,#7514,#7515,#7516));
#3160=EDGE_LOOP('',(#7517,#7518,#7519,#7520));
#3161=EDGE_LOOP('',(#7521,#7522,#7523,#7524));
#3162=EDGE_LOOP('',(#7525,#7526,#7527,#7528));
#3163=EDGE_LOOP('',(#7529,#7530,#7531,#7532));
#3164=EDGE_LOOP('',(#7533,#7534,#7535,#7536));
#3165=EDGE_LOOP('',(#7537,#7538,#7539,#7540));
#3166=EDGE_LOOP('',(#7541,#7542,#7543,#7544));
#3167=EDGE_LOOP('',(#7545,#7546,#7547,#7548));
#3168=EDGE_LOOP('',(#7549,#7550,#7551,#7552));
#3169=EDGE_LOOP('',(#7553,#7554,#7555,#7556));
#3170=EDGE_LOOP('',(#7557,#7558,#7559,#7560));
#3171=EDGE_LOOP('',(#7561,#7562,#7563,#7564));
#3172=EDGE_LOOP('',(#7565,#7566,#7567,#7568,#7569,#7570,#7571,#7572));
#3173=EDGE_LOOP('',(#7573));
#3174=EDGE_LOOP('',(#7574));
#3175=EDGE_LOOP('',(#7575));
#3176=EDGE_LOOP('',(#7576));
#3177=EDGE_LOOP('',(#7577));
#3178=EDGE_LOOP('',(#7578));
#3179=EDGE_LOOP('',(#7579,#7580,#7581,#7582,#7583,#7584,#7585,#7586));
#3180=EDGE_LOOP('',(#7587,#7588,#7589,#7590,#7591,#7592,#7593,#7594));
#3181=EDGE_LOOP('',(#7595,#7596,#7597,#7598,#7599,#7600,#7601,#7602));
#3182=EDGE_LOOP('',(#7603,#7604,#7605,#7606,#7607,#7608,#7609,#7610));
#3183=EDGE_LOOP('',(#7611));
#3184=EDGE_LOOP('',(#7612));
#3185=EDGE_LOOP('',(#7613));
#3186=EDGE_LOOP('',(#7614));
#3187=EDGE_LOOP('',(#7615));
#3188=EDGE_LOOP('',(#7616));
#3189=EDGE_LOOP('',(#7617,#7618,#7619,#7620,#7621,#7622,#7623,#7624));
#3190=EDGE_LOOP('',(#7625,#7626,#7627,#7628,#7629,#7630,#7631,#7632));
#3191=EDGE_LOOP('',(#7633,#7634,#7635,#7636,#7637,#7638,#7639,#7640));
#3192=EDGE_LOOP('',(#7641,#7642,#7643,#7644));
#3193=EDGE_LOOP('',(#7645,#7646,#7647,#7648));
#3194=EDGE_LOOP('',(#7649,#7650,#7651,#7652));
#3195=EDGE_LOOP('',(#7653,#7654,#7655,#7656));
#3196=EDGE_LOOP('',(#7657,#7658,#7659,#7660));
#3197=EDGE_LOOP('',(#7661,#7662,#7663,#7664));
#3198=EDGE_LOOP('',(#7665,#7666,#7667,#7668));
#3199=EDGE_LOOP('',(#7669,#7670,#7671,#7672));
#3200=EDGE_LOOP('',(#7673,#7674,#7675,#7676));
#3201=EDGE_LOOP('',(#7677,#7678,#7679,#7680,#7681,#7682));
#3202=EDGE_LOOP('',(#7683));
#3203=EDGE_LOOP('',(#7684));
#3204=EDGE_LOOP('',(#7685));
#3205=EDGE_LOOP('',(#7686));
#3206=EDGE_LOOP('',(#7687,#7688,#7689,#7690));
#3207=EDGE_LOOP('',(#7691,#7692,#7693,#7694));
#3208=EDGE_LOOP('',(#7695,#7696,#7697,#7698));
#3209=EDGE_LOOP('',(#7699,#7700,#7701,#7702));
#3210=EDGE_LOOP('',(#7703,#7704,#7705,#7706));
#3211=EDGE_LOOP('',(#7707,#7708,#7709,#7710));
#3212=EDGE_LOOP('',(#7711,#7712,#7713,#7714));
#3213=EDGE_LOOP('',(#7715,#7716,#7717,#7718,#7719,#7720));
#3214=EDGE_LOOP('',(#7721));
#3215=EDGE_LOOP('',(#7722));
#3216=EDGE_LOOP('',(#7723));
#3217=EDGE_LOOP('',(#7724));
#3218=EDGE_LOOP('',(#7725));
#3219=EDGE_LOOP('',(#7726,#7727,#7728,#7729,#7730,#7731,#7732,#7733,#7734,
#7735,#7736,#7737,#7738,#7739,#7740,#7741,#7742,#7743,#7744,#7745,#7746,
#7747,#7748,#7749,#7750,#7751,#7752,#7753,#7754,#7755,#7756,#7757,#7758,
#7759,#7760,#7761,#7762,#7763,#7764,#7765,#7766,#7767,#7768,#7769,#7770,
#7771,#7772,#7773,#7774,#7775,#7776,#7777,#7778,#7779,#7780,#7781,#7782,
#7783,#7784,#7785,#7786,#7787,#7788,#7789,#7790,#7791,#7792,#7793,#7794,
#7795,#7796,#7797,#7798,#7799,#7800,#7801,#7802,#7803,#7804,#7805,#7806,
#7807,#7808,#7809,#7810,#7811,#7812,#7813,#7814,#7815,#7816,#7817,#7818,
#7819,#7820,#7821,#7822,#7823,#7824,#7825,#7826,#7827,#7828,#7829,#7830,
#7831,#7832,#7833,#7834,#7835,#7836,#7837,#7838,#7839,#7840,#7841,#7842,
#7843,#7844,#7845,#7846,#7847,#7848,#7849,#7850,#7851,#7852,#7853,#7854,
#7855,#7856,#7857,#7858,#7859,#7860,#7861,#7862,#7863,#7864,#7865,#7866,
#7867,#7868,#7869,#7870,#7871,#7872,#7873,#7874,#7875));
#3220=EDGE_LOOP('',(#7876));
#3221=EDGE_LOOP('',(#7877,#7878,#7879,#7880,#7881,#7882,#7883,#7884,#7885,
#7886,#7887,#7888,#7889,#7890,#7891,#7892,#7893,#7894,#7895,#7896,#7897,
#7898,#7899,#7900,#7901,#7902,#7903,#7904,#7905,#7906,#7907,#7908,#7909,
#7910,#7911,#7912,#7913,#7914,#7915,#7916,#7917,#7918,#7919,#7920,#7921,
#7922,#7923,#7924,#7925,#7926,#7927,#7928,#7929,#7930,#7931,#7932,#7933,
#7934,#7935,#7936,#7937,#7938,#7939,#7940,#7941,#7942,#7943,#7944,#7945,
#7946,#7947,#7948,#7949,#7950,#7951,#7952,#7953,#7954,#7955,#7956,#7957,
#7958,#7959));
#3222=EDGE_LOOP('',(#7960,#7961,#7962,#7963));
#3223=EDGE_LOOP('',(#7964,#7965,#7966,#7967));
#3224=EDGE_LOOP('',(#7968,#7969,#7970,#7971));
#3225=EDGE_LOOP('',(#7972,#7973,#7974,#7975));
#3226=EDGE_LOOP('',(#7976,#7977,#7978,#7979));
#3227=EDGE_LOOP('',(#7980,#7981,#7982,#7983));
#3228=EDGE_LOOP('',(#7984,#7985,#7986,#7987,#7988,#7989));
#3229=EDGE_LOOP('',(#7990,#7991,#7992,#7993,#7994));
#3230=EDGE_LOOP('',(#7995,#7996,#7997,#7998,#7999,#8000,#8001,#8002,#8003,
#8004,#8005,#8006,#8007,#8008,#8009,#8010,#8011,#8012,#8013,#8014,#8015,
#8016,#8017,#8018,#8019,#8020,#8021,#8022,#8023,#8024,#8025,#8026,#8027,
#8028,#8029,#8030,#8031,#8032,#8033,#8034,#8035,#8036,#8037,#8038,#8039,
#8040,#8041,#8042,#8043,#8044,#8045,#8046,#8047,#8048,#8049,#8050,#8051,
#8052,#8053,#8054,#8055,#8056,#8057,#8058,#8059,#8060,#8061,#8062,#8063,
#8064,#8065,#8066,#8067,#8068,#8069,#8070,#8071,#8072,#8073,#8074,#8075,
#8076,#8077,#8078,#8079,#8080,#8081,#8082,#8083,#8084,#8085,#8086,#8087,
#8088,#8089,#8090,#8091,#8092,#8093,#8094,#8095,#8096,#8097,#8098,#8099,
#8100,#8101,#8102,#8103,#8104,#8105,#8106,#8107,#8108,#8109,#8110));
#3231=EDGE_LOOP('',(#8111,#8112,#8113,#8114));
#3232=EDGE_LOOP('',(#8115,#8116,#8117,#8118,#8119,#8120,#8121,#8122,#8123,
#8124,#8125,#8126,#8127,#8128,#8129,#8130,#8131,#8132,#8133,#8134,#8135,
#8136,#8137,#8138,#8139,#8140,#8141,#8142,#8143,#8144,#8145,#8146,#8147,
#8148,#8149,#8150,#8151,#8152,#8153,#8154,#8155,#8156,#8157,#8158,#8159,
#8160,#8161,#8162,#8163,#8164,#8165,#8166,#8167,#8168,#8169,#8170,#8171,
#8172,#8173,#8174,#8175,#8176,#8177,#8178,#8179,#8180,#8181,#8182,#8183,
#8184,#8185,#8186,#8187,#8188,#8189,#8190,#8191,#8192,#8193,#8194,#8195,
#8196,#8197,#8198,#8199,#8200,#8201,#8202,#8203,#8204,#8205,#8206,#8207,
#8208,#8209,#8210,#8211,#8212,#8213,#8214,#8215,#8216,#8217,#8218,#8219,
#8220,#8221,#8222,#8223,#8224,#8225,#8226,#8227,#8228,#8229,#8230,#8231,
#8232));
#3233=EDGE_LOOP('',(#8233));
#3234=EDGE_LOOP('',(#8234,#8235,#8236,#8237));
#3235=EDGE_LOOP('',(#8238,#8239,#8240,#8241));
#3236=EDGE_LOOP('',(#8242));
#3237=EDGE_LOOP('',(#8243,#8244,#8245,#8246,#8247,#8248));
#3238=EDGE_LOOP('',(#8249,#8250,#8251,#8252,#8253));
#3239=EDGE_LOOP('',(#8254,#8255,#8256));
#3240=EDGE_LOOP('',(#8257,#8258,#8259,#8260,#8261));
#3241=EDGE_LOOP('',(#8262,#8263,#8264,#8265));
#3242=EDGE_LOOP('',(#8266,#8267,#8268,#8269,#8270));
#3243=EDGE_LOOP('',(#8271,#8272,#8273));
#3244=EDGE_LOOP('',(#8274,#8275,#8276,#8277,#8278));
#3245=EDGE_LOOP('',(#8279,#8280,#8281,#8282));
#3246=EDGE_LOOP('',(#8283,#8284,#8285,#8286));
#3247=EDGE_LOOP('',(#8287,#8288,#8289,#8290));
#3248=EDGE_LOOP('',(#8291,#8292,#8293,#8294));
#3249=EDGE_LOOP('',(#8295,#8296,#8297,#8298));
#3250=EDGE_LOOP('',(#8299,#8300,#8301,#8302));
#3251=EDGE_LOOP('',(#8303,#8304,#8305,#8306));
#3252=EDGE_LOOP('',(#8307,#8308,#8309,#8310,#8311,#8312));
#3253=EDGE_LOOP('',(#8313,#8314,#8315,#8316,#8317));
#3254=EDGE_LOOP('',(#8318,#8319,#8320,#8321,#8322,#8323));
#3255=EDGE_LOOP('',(#8324,#8325,#8326,#8327,#8328));
#3256=EDGE_LOOP('',(#8329,#8330,#8331,#8332,#8333,#8334,#8335,#8336,#8337,
#8338,#8339,#8340,#8341,#8342));
#3257=EDGE_LOOP('',(#8343,#8344));
#3258=EDGE_LOOP('',(#8345,#8346));
#3259=EDGE_LOOP('',(#8347,#8348,#8349));
#3260=EDGE_LOOP('',(#8350,#8351,#8352,#8353));
#3261=EDGE_LOOP('',(#8354,#8355));
#3262=EDGE_LOOP('',(#8356,#8357,#8358,#8359));
#3263=EDGE_LOOP('',(#8360,#8361,#8362,#8363,#8364,#8365,#8366,#8367,#8368,
#8369,#8370,#8371));
#3264=EDGE_LOOP('',(#8372));
#3265=EDGE_LOOP('',(#8373));
#3266=EDGE_LOOP('',(#8374,#8375,#8376));
#3267=EDGE_LOOP('',(#8377,#8378,#8379));
#3268=EDGE_LOOP('',(#8380,#8381,#8382,#8383,#8384,#8385));
#3269=EDGE_LOOP('',(#8386));
#3270=EDGE_LOOP('',(#8387));
#3271=EDGE_LOOP('',(#8388,#8389,#8390,#8391,#8392,#8393));
#3272=EDGE_LOOP('',(#8394));
#3273=EDGE_LOOP('',(#8395));
#3274=EDGE_LOOP('',(#8396,#8397,#8398,#8399,#8400,#8401,#8402,#8403));
#3275=EDGE_LOOP('',(#8404));
#3276=EDGE_LOOP('',(#8405,#8406,#8407,#8408));
#3277=EDGE_LOOP('',(#8409));
#3278=EDGE_LOOP('',(#8410));
#3279=EDGE_LOOP('',(#8411,#8412,#8413,#8414));
#3280=EDGE_LOOP('',(#8415,#8416,#8417,#8418));
#3281=EDGE_LOOP('',(#8419));
#3282=EDGE_LOOP('',(#8420));
#3283=EDGE_LOOP('',(#8421,#8422,#8423,#8424));
#3284=EDGE_LOOP('',(#8425));
#3285=EDGE_LOOP('',(#8426));
#3286=EDGE_LOOP('',(#8427,#8428,#8429,#8430));
#3287=EDGE_LOOP('',(#8431));
#3288=EDGE_LOOP('',(#8432));
#3289=EDGE_LOOP('',(#8433,#8434,#8435,#8436));
#3290=EDGE_LOOP('',(#8437,#8438,#8439,#8440));
#3291=EDGE_LOOP('',(#8441,#8442,#8443,#8444));
#3292=EDGE_LOOP('',(#8445));
#3293=EDGE_LOOP('',(#8446));
#3294=EDGE_LOOP('',(#8447,#8448,#8449,#8450));
#3295=EDGE_LOOP('',(#8451));
#3296=EDGE_LOOP('',(#8452));
#3297=EDGE_LOOP('',(#8453,#8454,#8455,#8456));
#3298=EDGE_LOOP('',(#8457));
#3299=EDGE_LOOP('',(#8458));
#3300=EDGE_LOOP('',(#8459,#8460,#8461,#8462));
#3301=EDGE_LOOP('',(#8463,#8464,#8465,#8466,#8467));
#3302=EDGE_LOOP('',(#8468,#8469,#8470,#8471,#8472));
#3303=EDGE_LOOP('',(#8473,#8474,#8475,#8476));
#3304=EDGE_LOOP('',(#8477,#8478,#8479,#8480));
#3305=EDGE_LOOP('',(#8481,#8482,#8483,#8484,#8485,#8486,#8487,#8488,#8489,
#8490,#8491,#8492,#8493,#8494,#8495,#8496,#8497,#8498,#8499,#8500,#8501,
#8502,#8503,#8504,#8505,#8506,#8507,#8508,#8509,#8510,#8511,#8512));
#3306=EDGE_LOOP('',(#8513));
#3307=EDGE_LOOP('',(#8514,#8515,#8516,#8517));
#3308=EDGE_LOOP('',(#8518,#8519,#8520,#8521));
#3309=EDGE_LOOP('',(#8522,#8523,#8524,#8525,#8526));
#3310=EDGE_LOOP('',(#8527,#8528,#8529,#8530,#8531));
#3311=EDGE_LOOP('',(#8532,#8533,#8534,#8535));
#3312=EDGE_LOOP('',(#8536,#8537,#8538,#8539));
#3313=EDGE_LOOP('',(#8540,#8541,#8542,#8543));
#3314=EDGE_LOOP('',(#8544,#8545,#8546,#8547,#8548));
#3315=EDGE_LOOP('',(#8549,#8550,#8551,#8552,#8553));
#3316=EDGE_LOOP('',(#8554,#8555,#8556,#8557));
#3317=EDGE_LOOP('',(#8558,#8559,#8560,#8561));
#3318=EDGE_LOOP('',(#8562,#8563,#8564,#8565));
#3319=EDGE_LOOP('',(#8566,#8567,#8568,#8569,#8570));
#3320=EDGE_LOOP('',(#8571,#8572,#8573,#8574,#8575));
#3321=EDGE_LOOP('',(#8576,#8577,#8578,#8579));
#3322=EDGE_LOOP('',(#8580,#8581,#8582,#8583,#8584));
#3323=EDGE_LOOP('',(#8585,#8586,#8587,#8588));
#3324=EDGE_LOOP('',(#8589,#8590,#8591,#8592,#8593));
#3325=EDGE_LOOP('',(#8594,#8595,#8596,#8597,#8598));
#3326=EDGE_LOOP('',(#8599,#8600,#8601,#8602));
#3327=EDGE_LOOP('',(#8603,#8604,#8605,#8606));
#3328=EDGE_LOOP('',(#8607,#8608,#8609,#8610));
#3329=EDGE_LOOP('',(#8611,#8612,#8613,#8614,#8615));
#3330=EDGE_LOOP('',(#8616,#8617,#8618,#8619,#8620));
#3331=EDGE_LOOP('',(#8621,#8622,#8623,#8624));
#3332=EDGE_LOOP('',(#8625,#8626,#8627,#8628));
#3333=EDGE_LOOP('',(#8629,#8630,#8631,#8632));
#3334=EDGE_LOOP('',(#8633,#8634,#8635,#8636,#8637));
#3335=EDGE_LOOP('',(#8638,#8639,#8640,#8641,#8642));
#3336=EDGE_LOOP('',(#8643,#8644,#8645,#8646));
#3337=EDGE_LOOP('',(#8647,#8648,#8649,#8650));
#3338=EDGE_LOOP('',(#8651,#8652,#8653,#8654));
#3339=EDGE_LOOP('',(#8655,#8656,#8657,#8658,#8659));
#3340=EDGE_LOOP('',(#8660,#8661,#8662,#8663,#8664));
#3341=EDGE_LOOP('',(#8665,#8666,#8667,#8668));
#3342=EDGE_LOOP('',(#8669,#8670,#8671,#8672));
#3343=EDGE_LOOP('',(#8673,#8674,#8675,#8676));
#3344=EDGE_LOOP('',(#8677));
#3345=EDGE_LOOP('',(#8678));
#3346=EDGE_LOOP('',(#8679,#8680,#8681,#8682));
#3347=EDGE_LOOP('',(#8683));
#3348=EDGE_LOOP('',(#8684));
#3349=EDGE_LOOP('',(#8685,#8686,#8687,#8688,#8689,#8690,#8691,#8692,#8693,
#8694,#8695,#8696,#8697,#8698,#8699,#8700,#8701,#8702,#8703,#8704,#8705,
#8706,#8707,#8708,#8709,#8710,#8711,#8712,#8713,#8714,#8715,#8716,#8717,
#8718,#8719,#8720));
#3350=EDGE_LOOP('',(#8721,#8722,#8723,#8724));
#3351=EDGE_LOOP('',(#8725));
#3352=EDGE_LOOP('',(#8726));
#3353=EDGE_LOOP('',(#8727,#8728,#8729,#8730));
#3354=EDGE_LOOP('',(#8731,#8732,#8733,#8734));
#3355=EDGE_LOOP('',(#8735,#8736,#8737,#8738));
#3356=EDGE_LOOP('',(#8739,#8740,#8741,#8742));
#3357=EDGE_LOOP('',(#8743));
#3358=EDGE_LOOP('',(#8744,#8745,#8746,#8747));
#3359=EDGE_LOOP('',(#8748,#8749,#8750,#8751));
#3360=EDGE_LOOP('',(#8752,#8753,#8754,#8755));
#3361=EDGE_LOOP('',(#8756));
#3362=EDGE_LOOP('',(#8757,#8758,#8759,#8760));
#3363=EDGE_LOOP('',(#8761,#8762,#8763,#8764));
#3364=EDGE_LOOP('',(#8765));
#3365=EDGE_LOOP('',(#8766));
#3366=EDGE_LOOP('',(#8767,#8768,#8769,#8770));
#3367=EDGE_LOOP('',(#8771));
#3368=EDGE_LOOP('',(#8772));
#3369=EDGE_LOOP('',(#8773,#8774,#8775,#8776));
#3370=EDGE_LOOP('',(#8777));
#3371=EDGE_LOOP('',(#8778));
#3372=EDGE_LOOP('',(#8779,#8780,#8781,#8782));
#3373=EDGE_LOOP('',(#8783,#8784,#8785,#8786));
#3374=EDGE_LOOP('',(#8787,#8788,#8789,#8790));
#3375=EDGE_LOOP('',(#8791));
#3376=EDGE_LOOP('',(#8792));
#3377=EDGE_LOOP('',(#8793,#8794,#8795,#8796));
#3378=EDGE_LOOP('',(#8797));
#3379=EDGE_LOOP('',(#8798));
#3380=EDGE_LOOP('',(#8799,#8800,#8801,#8802));
#3381=EDGE_LOOP('',(#8803));
#3382=EDGE_LOOP('',(#8804));
#3383=EDGE_LOOP('',(#8805,#8806,#8807,#8808));
#3384=EDGE_LOOP('',(#8809,#8810,#8811,#8812));
#3385=EDGE_LOOP('',(#8813,#8814,#8815,#8816));
#3386=EDGE_LOOP('',(#8817));
#3387=EDGE_LOOP('',(#8818));
#3388=EDGE_LOOP('',(#8819,#8820,#8821,#8822));
#3389=EDGE_LOOP('',(#8823,#8824,#8825,#8826));
#3390=EDGE_LOOP('',(#8827,#8828,#8829,#8830));
#3391=EDGE_LOOP('',(#8831));
#3392=EDGE_LOOP('',(#8832));
#3393=EDGE_LOOP('',(#8833,#8834,#8835,#8836));
#3394=EDGE_LOOP('',(#8837));
#3395=EDGE_LOOP('',(#8838,#8839,#8840,#8841));
#3396=EDGE_LOOP('',(#8842,#8843,#8844,#8845));
#3397=EDGE_LOOP('',(#8846));
#3398=EDGE_LOOP('',(#8847));
#3399=EDGE_LOOP('',(#8848,#8849,#8850,#8851));
#3400=EDGE_LOOP('',(#8852));
#3401=EDGE_LOOP('',(#8853));
#3402=EDGE_LOOP('',(#8854,#8855,#8856,#8857));
#3403=EDGE_LOOP('',(#8858,#8859,#8860,#8861));
#3404=EDGE_LOOP('',(#8862));
#3405=EDGE_LOOP('',(#8863));
#3406=EDGE_LOOP('',(#8864,#8865,#8866,#8867));
#3407=EDGE_LOOP('',(#8868,#8869,#8870,#8871));
#3408=EDGE_LOOP('',(#8872));
#3409=EDGE_LOOP('',(#8873));
#3410=EDGE_LOOP('',(#8874,#8875,#8876,#8877));
#3411=EDGE_LOOP('',(#8878));
#3412=EDGE_LOOP('',(#8879));
#3413=EDGE_LOOP('',(#8880,#8881,#8882,#8883));
#3414=EDGE_LOOP('',(#8884,#8885,#8886,#8887));
#3415=EDGE_LOOP('',(#8888));
#3416=EDGE_LOOP('',(#8889,#8890,#8891,#8892));
#3417=EDGE_LOOP('',(#8893,#8894,#8895,#8896));
#3418=EDGE_LOOP('',(#8897));
#3419=EDGE_LOOP('',(#8898));
#3420=EDGE_LOOP('',(#8899,#8900,#8901,#8902));
#3421=EDGE_LOOP('',(#8903,#8904,#8905,#8906));
#3422=EDGE_LOOP('',(#8907,#8908,#8909,#8910,#8911,#8912));
#3423=EDGE_LOOP('',(#8913,#8914,#8915,#8916,#8917));
#3424=EDGE_LOOP('',(#8918,#8919,#8920,#8921,#8922,#8923));
#3425=EDGE_LOOP('',(#8924,#8925,#8926,#8927,#8928));
#3426=EDGE_LOOP('',(#8929,#8930,#8931,#8932,#8933,#8934));
#3427=EDGE_LOOP('',(#8935,#8936,#8937,#8938,#8939));
#3428=EDGE_LOOP('',(#8940,#8941,#8942,#8943,#8944,#8945));
#3429=EDGE_LOOP('',(#8946,#8947,#8948,#8949,#8950));
#3430=EDGE_LOOP('',(#8951,#8952,#8953,#8954,#8955,#8956));
#3431=EDGE_LOOP('',(#8957,#8958,#8959,#8960,#8961));
#3432=EDGE_LOOP('',(#8962,#8963,#8964,#8965,#8966,#8967));
#3433=EDGE_LOOP('',(#8968,#8969,#8970,#8971,#8972));
#3434=EDGE_LOOP('',(#8973,#8974,#8975,#8976,#8977,#8978));
#3435=EDGE_LOOP('',(#8979,#8980,#8981,#8982,#8983,#8984,#8985,#8986,#8987,
#8988,#8989,#8990,#8991,#8992,#8993,#8994,#8995,#8996,#8997,#8998,#8999,
#9000,#9001,#9002,#9003,#9004,#9005,#9006,#9007,#9008,#9009,#9010));
#3436=EDGE_LOOP('',(#9011,#9012,#9013,#9014,#9015,#9016));
#3437=EDGE_LOOP('',(#9017,#9018,#9019,#9020,#9021,#9022,#9023,#9024,#9025,
#9026,#9027,#9028,#9029,#9030,#9031,#9032,#9033,#9034,#9035,#9036,#9037,
#9038,#9039,#9040,#9041,#9042,#9043,#9044,#9045,#9046,#9047,#9048,#9049,
#9050,#9051,#9052,#9053,#9054,#9055,#9056,#9057,#9058,#9059,#9060,#9061,
#9062));
#3438=EDGE_LOOP('',(#9063,#9064,#9065,#9066,#9067));
#3439=EDGE_LOOP('',(#9068,#9069,#9070,#9071,#9072,#9073,#9074,#9075,#9076,
#9077,#9078,#9079,#9080,#9081,#9082,#9083,#9084,#9085,#9086,#9087,#9088,
#9089,#9090,#9091,#9092,#9093,#9094,#9095,#9096,#9097,#9098,#9099,#9100,
#9101,#9102,#9103,#9104,#9105,#9106,#9107,#9108));
#3440=EDGE_LOOP('',(#9109,#9110));
#3441=EDGE_LOOP('',(#9111,#9112));
#3442=EDGE_LOOP('',(#9113,#9114));
#3443=EDGE_LOOP('',(#9115,#9116));
#3444=EDGE_LOOP('',(#9117,#9118,#9119));
#3445=EDGE_LOOP('',(#9120,#9121));
#3446=EDGE_LOOP('',(#9122,#9123,#9124,#9125,#9126,#9127,#9128,#9129,#9130,
#9131,#9132,#9133,#9134,#9135,#9136,#9137,#9138,#9139,#9140,#9141,#9142,
#9143));
#3447=EDGE_LOOP('',(#9144,#9145,#9146));
#3448=EDGE_LOOP('',(#9147,#9148,#9149,#9150,#9151,#9152));
#3449=EDGE_LOOP('',(#9153,#9154,#9155,#9156,#9157,#9158));
#3450=EDGE_LOOP('',(#9159,#9160,#9161,#9162,#9163,#9164));
#3451=EDGE_LOOP('',(#9165,#9166,#9167,#9168,#9169,#9170));
#3452=EDGE_LOOP('',(#9171,#9172,#9173,#9174,#9175,#9176));
#3453=EDGE_LOOP('',(#9177,#9178,#9179,#9180,#9181,#9182));
#3454=EDGE_LOOP('',(#9183,#9184,#9185,#9186,#9187,#9188));
#3455=EDGE_LOOP('',(#9189));
#3456=EDGE_LOOP('',(#9190));
#3457=EDGE_LOOP('',(#9191,#9192,#9193,#9194,#9195,#9196,#9197));
#3458=EDGE_LOOP('',(#9198));
#3459=EDGE_LOOP('',(#9199,#9200,#9201,#9202));
#3460=EDGE_LOOP('',(#9203,#9204,#9205,#9206));
#3461=EDGE_LOOP('',(#9207,#9208,#9209,#9210));
#3462=EDGE_LOOP('',(#9211,#9212,#9213,#9214));
#3463=EDGE_LOOP('',(#9215,#9216,#9217,#9218));
#3464=EDGE_LOOP('',(#9219,#9220,#9221,#9222));
#3465=EDGE_LOOP('',(#9223,#9224,#9225,#9226));
#3466=EDGE_LOOP('',(#9227,#9228,#9229,#9230));
#3467=EDGE_LOOP('',(#9231,#9232,#9233,#9234));
#3468=EDGE_LOOP('',(#9235,#9236,#9237,#9238));
#3469=EDGE_LOOP('',(#9239,#9240,#9241,#9242));
#3470=EDGE_LOOP('',(#9243,#9244,#9245,#9246,#9247,#9248,#9249,#9250,#9251,
#9252,#9253,#9254,#9255,#9256));
#3471=EDGE_LOOP('',(#9257,#9258,#9259,#9260));
#3472=EDGE_LOOP('',(#9261,#9262,#9263,#9264));
#3473=EDGE_LOOP('',(#9265,#9266,#9267,#9268));
#3474=EDGE_LOOP('',(#9269,#9270,#9271,#9272));
#3475=EDGE_LOOP('',(#9273,#9274,#9275,#9276));
#3476=EDGE_LOOP('',(#9277,#9278,#9279,#9280,#9281,#9282,#9283,#9284,#9285,
#9286,#9287,#9288,#9289,#9290));
#3477=EDGE_LOOP('',(#9291,#9292,#9293,#9294));
#3478=EDGE_LOOP('',(#9295,#9296,#9297,#9298));
#3479=EDGE_LOOP('',(#9299,#9300,#9301,#9302));
#3480=EDGE_LOOP('',(#9303,#9304,#9305,#9306));
#3481=EDGE_LOOP('',(#9307,#9308,#9309,#9310));
#3482=EDGE_LOOP('',(#9311,#9312,#9313,#9314));
#3483=EDGE_LOOP('',(#9315,#9316,#9317,#9318));
#3484=EDGE_LOOP('',(#9319,#9320,#9321,#9322));
#3485=EDGE_LOOP('',(#9323,#9324,#9325,#9326));
#3486=EDGE_LOOP('',(#9327,#9328,#9329,#9330,#9331,#9332,#9333,#9334,#9335,
#9336,#9337,#9338,#9339,#9340));
#3487=EDGE_LOOP('',(#9341,#9342,#9343,#9344));
#3488=EDGE_LOOP('',(#9345,#9346,#9347,#9348));
#3489=EDGE_LOOP('',(#9349,#9350,#9351,#9352));
#3490=EDGE_LOOP('',(#9353,#9354,#9355,#9356));
#3491=EDGE_LOOP('',(#9357,#9358,#9359,#9360));
#3492=EDGE_LOOP('',(#9361,#9362,#9363,#9364,#9365,#9366,#9367,#9368,#9369,
#9370,#9371,#9372,#9373,#9374));
#3493=CIRCLE('',#10101,1.35);
#3494=CIRCLE('',#10102,0.1);
#3495=CIRCLE('',#10103,1.45);
#3496=CIRCLE('',#10104,1.35);
#3497=CIRCLE('',#10106,1.35);
#3498=CIRCLE('',#10107,1.35);
#3499=CIRCLE('',#10111,1.45);
#3500=CIRCLE('',#10112,0.1);
#3501=CIRCLE('',#10115,1.35);
#3502=CIRCLE('',#10116,0.1);
#3503=CIRCLE('',#10117,1.45);
#3504=CIRCLE('',#10118,1.35);
#3505=CIRCLE('',#10120,1.35);
#3506=CIRCLE('',#10121,1.35);
#3507=CIRCLE('',#10124,1.45);
#3508=CIRCLE('',#10125,0.1);
#3509=CIRCLE('',#10127,0.0799999999999994);
#3510=CIRCLE('',#10129,0.0799999999999999);
#3511=CIRCLE('',#10131,0.0799999999999997);
#3512=CIRCLE('',#10132,5.07999306553394);
#3513=CIRCLE('',#10133,4.3279926764569);
#3514=CIRCLE('',#10134,4.06447495376015);
#3515=CIRCLE('',#10135,0.08);
#3516=CIRCLE('',#10136,0.0800000000000001);
#3517=CIRCLE('',#10137,0.0799999999999998);
#3518=CIRCLE('',#10139,0.0800000000000027);
#3519=CIRCLE('',#10140,0.0800000000000007);
#3520=CIRCLE('',#10141,0.0800000000000003);
#3521=CIRCLE('',#10142,0.0799999999999987);
#3522=CIRCLE('',#10143,0.0799999999999991);
#3523=CIRCLE('',#10144,0.0800000000000008);
#3524=CIRCLE('',#10145,10.2333842526355);
#3525=CIRCLE('',#10146,42.0215436445756);
#3526=CIRCLE('',#10147,0.0800000000000006);
#3527=CIRCLE('',#10149,0.0800261246651755);
#3528=CIRCLE('',#10150,0.0800000000000003);
#3529=CIRCLE('',#10151,0.0799999999999982);
#3530=CIRCLE('',#10152,0.0799999999999997);
#3531=CIRCLE('',#10153,0.0800000000000006);
#3532=CIRCLE('',#10154,0.08);
#3533=CIRCLE('',#10155,0.0800000000000001);
#3534=CIRCLE('',#10156,1.70356712371079);
#3535=CIRCLE('',#10157,0.0799999999999989);
#3536=CIRCLE('',#10158,0.0799999999999979);
#3537=CIRCLE('',#10159,0.0800000000000002);
#3538=CIRCLE('',#10162,0.0785861158743583);
#3539=CIRCLE('',#10164,0.0800000000000012);
#3540=CIRCLE('',#10166,0.0796968010654983);
#3541=CIRCLE('',#10167,0.900090261485887);
#3542=CIRCLE('',#10168,0.08);
#3543=CIRCLE('',#10169,0.0800000001034237);
#3544=CIRCLE('',#10170,0.0800000000000002);
#3545=CIRCLE('',#10171,0.0800000000000002);
#3546=CIRCLE('',#10172,0.08);
#3547=CIRCLE('',#10173,0.0800000000013423);
#3548=CIRCLE('',#10174,0.0800000000000002);
#3549=CIRCLE('',#10175,0.08);
#3550=CIRCLE('',#10176,0.160164856730608);
#3551=CIRCLE('',#10179,0.0800000000000005);
#3552=CIRCLE('',#10181,0.0786789453077166);
#3553=CIRCLE('',#10182,0.400861721832437);
#3554=CIRCLE('',#10185,0.0800261745356576);
#3555=CIRCLE('',#10186,0.0799999999999995);
#3556=CIRCLE('',#10187,0.08);
#3557=CIRCLE('',#10188,0.0800000000000001);
#3558=CIRCLE('',#10189,0.08);
#3559=CIRCLE('',#10190,0.0800000000000003);
#3560=CIRCLE('',#10191,0.0800000000000001);
#3561=CIRCLE('',#10192,0.0800000000000005);
#3562=CIRCLE('',#10193,0.0799999999999994);
#3563=CIRCLE('',#10194,0.0799999999999999);
#3564=CIRCLE('',#10195,0.0800000000000008);
#3565=CIRCLE('',#10196,0.0798672614997588);
#3566=CIRCLE('',#10197,0.159293405838516);
#3567=CIRCLE('',#10198,0.0799999999999999);
#3568=CIRCLE('',#10199,0.0799999999999984);
#3569=CIRCLE('',#10201,0.08);
#3570=CIRCLE('',#10202,0.0800000000000024);
#3571=CIRCLE('',#10205,0.08);
#3572=CIRCLE('',#10208,0.08);
#3573=CIRCLE('',#10209,0.0799999999999999);
#3574=CIRCLE('',#10210,0.0800000000000002);
#3575=CIRCLE('',#10211,0.08);
#3576=CIRCLE('',#10212,0.0800000000000001);
#3577=CIRCLE('',#10213,0.160172033197375);
#3578=CIRCLE('',#10215,0.0800000000000002);
#3579=CIRCLE('',#10216,0.0800000000000001);
#3580=CIRCLE('',#10218,0.160207196111625);
#3581=CIRCLE('',#10220,0.0799999999999994);
#3582=CIRCLE('',#10221,0.080000000000001);
#3583=CIRCLE('',#10222,0.08);
#3584=CIRCLE('',#10223,0.0799999999999999);
#3585=CIRCLE('',#10226,0.160052182261364);
#3586=CIRCLE('',#10228,0.3);
#3587=CIRCLE('',#10229,0.36);
#3588=CIRCLE('',#10230,0.36);
#3589=CIRCLE('',#10231,0.3);
#3590=CIRCLE('',#10233,0.0800000000000003);
#3591=CIRCLE('',#10235,0.0800000000000001);
#3592=CIRCLE('',#10236,0.0800000000000003);
#3593=CIRCLE('',#10238,0.08);
#3594=CIRCLE('',#10240,0.0800000000000002);
#3595=CIRCLE('',#10242,0.0800000000000002);
#3596=CIRCLE('',#10244,0.0800000000000001);
#3597=CIRCLE('',#10248,0.3);
#3598=CIRCLE('',#10249,0.36);
#3599=CIRCLE('',#10250,0.36);
#3600=CIRCLE('',#10251,0.3);
#3601=CIRCLE('',#10252,0.0799999999999996);
#3602=CIRCLE('',#10253,0.0800260911298561);
#3603=CIRCLE('',#10254,0.0800000000000002);
#3604=CIRCLE('',#10255,0.0800000000000007);
#3605=CIRCLE('',#10256,0.0799999999999999);
#3606=CIRCLE('',#10258,0.0800000000000018);
#3607=CIRCLE('',#10261,0.0800000000000009);
#3608=CIRCLE('',#10263,0.264924618445784);
#3609=CIRCLE('',#10265,0.999721614072078);
#3610=CIRCLE('',#10266,0.08);
#3611=CIRCLE('',#10269,0.0799999999999983);
#3612=CIRCLE('',#10271,0.159956770110596);
#3613=CIRCLE('',#10274,0.0800000000000106);
#3614=CIRCLE('',#10275,0.0799999999999999);
#3615=CIRCLE('',#10276,0.487504928302448);
#3616=CIRCLE('',#10278,0.0799999999999999);
#3617=CIRCLE('',#10279,0.0661513100184898);
#3618=CIRCLE('',#10280,0.0799999999999999);
#3619=CIRCLE('',#10281,0.0799999999999998);
#3620=CIRCLE('',#10283,0.0800000000000001);
#3621=CIRCLE('',#10284,0.0800000000000001);
#3622=CIRCLE('',#10287,0.0800000000000004);
#3623=CIRCLE('',#10288,0.0799999999999999);
#3624=CIRCLE('',#10289,0.0799999999999998);
#3625=CIRCLE('',#10290,0.0799999999999995);
#3626=CIRCLE('',#10317,0.36);
#3627=CIRCLE('',#10318,0.36);
#3628=CIRCLE('',#10319,0.255);
#3629=CIRCLE('',#10320,0.255);
#3630=CIRCLE('',#10321,0.255);
#3631=CIRCLE('',#10322,0.255);
#3632=CIRCLE('',#10324,0.205);
#3633=CIRCLE('',#10326,0.205);
#3634=CIRCLE('',#10329,0.205);
#3635=CIRCLE('',#10331,0.205);
#3636=CIRCLE('',#10334,0.205);
#3637=CIRCLE('',#10336,0.205);
#3638=CIRCLE('',#10339,0.205);
#3639=CIRCLE('',#10341,0.205);
#3640=CIRCLE('',#10344,0.3);
#3641=CIRCLE('',#10346,0.3);
#3642=CIRCLE('',#10348,0.3);
#3643=CIRCLE('',#10350,0.3);
#3644=CIRCLE('',#10352,0.36);
#3645=CIRCLE('',#10354,0.36);
#3646=CIRCLE('',#10356,0.5);
#3647=CIRCLE('',#10357,0.5);
#3648=CIRCLE('',#10378,0.2);
#3649=CIRCLE('',#10379,0.2);
#3650=CIRCLE('',#10382,0.2);
#3651=CIRCLE('',#10383,0.2);
#3652=CIRCLE('',#10386,0.2);
#3653=CIRCLE('',#10387,0.2);
#3654=CIRCLE('',#10390,0.2);
#3655=CIRCLE('',#10391,0.2);
#3656=CIRCLE('',#10394,0.2);
#3657=CIRCLE('',#10395,0.2);
#3658=CIRCLE('',#10398,0.2);
#3659=CIRCLE('',#10399,0.2);
#3660=CIRCLE('',#10402,0.2);
#3661=CIRCLE('',#10403,0.2);
#3662=CIRCLE('',#10406,0.2);
#3663=CIRCLE('',#10407,0.2);
#3664=CIRCLE('',#10410,0.2);
#3665=CIRCLE('',#10411,0.2);
#3666=CIRCLE('',#10414,0.2);
#3667=CIRCLE('',#10415,0.2);
#3668=CIRCLE('',#10418,0.2);
#3669=CIRCLE('',#10419,0.2);
#3670=CIRCLE('',#10422,0.2);
#3671=CIRCLE('',#10423,0.2);
#3672=CIRCLE('',#10426,0.225);
#3673=CIRCLE('',#10427,0.225);
#3674=CIRCLE('',#10429,0.36);
#3675=CIRCLE('',#10430,0.36);
#3676=CIRCLE('',#10432,0.36);
#3677=CIRCLE('',#10433,0.36);
#3678=CIRCLE('',#10435,0.225);
#3679=CIRCLE('',#10436,0.225);
#3680=CIRCLE('',#10438,0.225);
#3681=CIRCLE('',#10439,0.225);
#3682=CIRCLE('',#10441,0.225);
#3683=CIRCLE('',#10442,0.225);
#3684=CIRCLE('',#10464,0.36);
#3685=CIRCLE('',#10465,0.3);
#3686=CIRCLE('',#10466,0.3);
#3687=CIRCLE('',#10467,0.36);
#3688=CIRCLE('',#10469,0.36);
#3689=CIRCLE('',#10471,0.3);
#3690=CIRCLE('',#10473,0.3);
#3691=CIRCLE('',#10475,0.36);
#3692=CIRCLE('',#10482,0.3933);
#3693=CIRCLE('',#10483,0.3933);
#3694=CIRCLE('',#10484,0.3933);
#3695=CIRCLE('',#10485,0.3933);
#3696=CIRCLE('',#10487,0.322275);
#3697=CIRCLE('',#10488,0.322275);
#3698=CIRCLE('',#10499,0.35);
#3699=CIRCLE('',#10502,0.36);
#3700=CIRCLE('',#10506,0.15);
#3701=CIRCLE('',#10507,0.15);
#3702=CIRCLE('',#10508,0.15);
#3703=CIRCLE('',#10510,1.1);
#3704=CIRCLE('',#10512,0.15);
#3705=CIRCLE('',#10513,0.15);
#3706=CIRCLE('',#10514,0.15);
#3707=CIRCLE('',#10517,0.15);
#3708=CIRCLE('',#10518,0.15);
#3709=CIRCLE('',#10519,0.15);
#3710=CIRCLE('',#10521,1.1);
#3711=CIRCLE('',#10523,0.15);
#3712=CIRCLE('',#10524,0.15);
#3713=CIRCLE('',#10525,0.15);
#3714=CIRCLE('',#10533,0.3);
#3715=CIRCLE('',#10535,0.3);
#3716=CIRCLE('',#10537,0.199999999999999);
#3717=CIRCLE('',#10539,0.199999999999999);
#3718=CIRCLE('',#10541,0.4025);
#3719=CIRCLE('',#10542,0.4025);
#3720=CIRCLE('',#10544,1.1);
#3721=CIRCLE('',#10545,1.1);
#3722=CIRCLE('',#10547,1.1);
#3723=CIRCLE('',#10549,1.1);
#3724=CIRCLE('',#10551,1.1);
#3725=CIRCLE('',#10553,1.1);
#3726=CIRCLE('',#10554,1.1);
#3727=CIRCLE('',#10555,1.1);
#3728=CIRCLE('',#10567,0.4);
#3729=CIRCLE('',#10568,0.4);
#3730=CIRCLE('',#10570,0.43);
#3731=CIRCLE('',#10572,0.62);
#3732=CIRCLE('',#10574,0.62);
#3733=CIRCLE('',#10576,0.92);
#3734=CIRCLE('',#10578,0.92);
#3735=CIRCLE('',#10580,1.07);
#3736=CIRCLE('',#10582,1.1);
#3737=CIRCLE('',#10584,1.1);
#3738=CIRCLE('',#10586,1.07);
#3739=CIRCLE('',#10588,0.92);
#3740=CIRCLE('',#10590,0.92);
#3741=CIRCLE('',#10592,0.62);
#3742=CIRCLE('',#10594,0.62);
#3743=CIRCLE('',#10596,0.43);
#3744=CIRCLE('',#10603,1.5);
#3745=CIRCLE('',#10605,1.44);
#3746=CIRCLE('',#10606,1.44);
#3747=CIRCLE('',#10607,1.44);
#3748=CIRCLE('',#10608,1.44);
#3749=CIRCLE('',#10609,1.44);
#3750=CIRCLE('',#10610,1.44);
#3751=CIRCLE('',#10611,1.44);
#3752=CIRCLE('',#10612,1.44);
#3753=CIRCLE('',#10613,0.6);
#3754=CIRCLE('',#10615,1.5);
#3755=CIRCLE('',#10617,1.5);
#3756=CIRCLE('',#10622,1.5);
#3757=CIRCLE('',#10624,1.5);
#3758=CIRCLE('',#10629,1.5);
#3759=CIRCLE('',#10631,1.5);
#3760=CIRCLE('',#10636,1.5);
#3761=CIRCLE('',#10637,1.5);
#3762=CIRCLE('',#10639,1.5);
#3763=CIRCLE('',#10644,1.5);
#3764=CIRCLE('',#10646,1.5);
#3765=CIRCLE('',#10651,1.5);
#3766=CIRCLE('',#10653,1.5);
#3767=CIRCLE('',#10658,1.5);
#3768=CIRCLE('',#10660,1.5);
#3769=CIRCLE('',#10665,1.5);
#3770=CIRCLE('',#10667,1.1);
#3771=CIRCLE('',#10668,1.1);
#3772=CIRCLE('',#10670,0.46);
#3773=CIRCLE('',#10672,0.46);
#3774=CIRCLE('',#10674,1.5);
#3775=CIRCLE('',#10677,0.6);
#3776=CIRCLE('',#10684,1.58);
#3777=CIRCLE('',#10685,1.5);
#3778=CIRCLE('',#10687,1.5);
#3779=CIRCLE('',#10689,1.58);
#3780=CIRCLE('',#10693,0.302);
#3781=CIRCLE('',#10694,0.302);
#3782=CIRCLE('',#10696,0.342);
#3783=CIRCLE('',#10698,0.86);
#3784=CIRCLE('',#10700,0.86);
#3785=CIRCLE('',#10702,0.94);
#3786=CIRCLE('',#10704,0.94);
#3787=CIRCLE('',#10706,0.95);
#3788=CIRCLE('',#10708,1.);
#3789=CIRCLE('',#10710,1.);
#3790=CIRCLE('',#10712,0.95);
#3791=CIRCLE('',#10714,0.94);
#3792=CIRCLE('',#10716,0.94);
#3793=CIRCLE('',#10718,0.86);
#3794=CIRCLE('',#10720,0.86);
#3795=CIRCLE('',#10722,0.342);
#3796=CIRCLE('',#10726,0.202);
#3797=CIRCLE('',#10727,0.202);
#3798=CIRCLE('',#10729,0.232);
#3799=CIRCLE('',#10731,0.32);
#3800=CIRCLE('',#10733,0.35);
#3801=CIRCLE('',#10735,0.35);
#3802=CIRCLE('',#10737,0.32);
#3803=CIRCLE('',#10739,0.232);
#3804=CIRCLE('',#10743,0.27);
#3805=CIRCLE('',#10745,0.3);
#3806=CIRCLE('',#10747,0.3);
#3807=CIRCLE('',#10749,0.25);
#3808=CIRCLE('',#10751,0.25);
#3809=CIRCLE('',#10753,0.3);
#3810=CIRCLE('',#10755,0.3);
#3811=CIRCLE('',#10757,0.27);
#3812=CIRCLE('',#10761,0.17);
#3813=CIRCLE('',#10763,0.2);
#3814=CIRCLE('',#10765,0.2);
#3815=CIRCLE('',#10767,0.16);
#3816=CIRCLE('',#10769,0.16);
#3817=CIRCLE('',#10771,0.2);
#3818=CIRCLE('',#10773,0.2);
#3819=CIRCLE('',#10775,0.17);
#3820=CIRCLE('',#10779,0.2);
#3821=CIRCLE('',#10780,0.1);
#3822=CIRCLE('',#10781,0.3);
#3823=CIRCLE('',#10783,0.3);
#3824=CIRCLE('',#10786,0.26);
#3825=CIRCLE('',#10790,0.15555);
#3826=CIRCLE('',#10805,0.1954);
#3827=CIRCLE('',#10806,0.1954);
#3828=CIRCLE('',#10808,0.15555);
#3829=CIRCLE('',#10810,0.1954);
#3830=CIRCLE('',#10811,0.1954);
#3831=CIRCLE('',#10813,0.131954512102672);
#3832=CIRCLE('',#10815,0.131954512102672);
#3833=CIRCLE('',#10817,0.131954512102672);
#3834=CIRCLE('',#10819,0.131954512102672);
#3835=CIRCLE('',#10821,0.131954512102672);
#3836=CIRCLE('',#10822,0.131954512102672);
#3837=CIRCLE('',#10824,0.131954512102672);
#3838=CIRCLE('',#10826,0.475);
#3839=CIRCLE('',#10827,0.38);
#3840=CIRCLE('',#10828,0.458257569495584);
#3841=CIRCLE('',#10829,0.458257569495584);
#3842=CIRCLE('',#10830,0.458257569495584);
#3843=CIRCLE('',#10831,0.458257569495584);
#3844=CIRCLE('',#10832,0.458257569495584);
#3845=CIRCLE('',#10833,0.458257569495584);
#3846=CIRCLE('',#10834,0.458257569495584);
#3847=CIRCLE('',#10835,0.458257569495584);
#3848=CIRCLE('',#10836,0.458257569495584);
#3849=CIRCLE('',#10837,0.458257569495584);
#3850=CIRCLE('',#10838,0.458257569495584);
#3851=CIRCLE('',#10839,0.458257569495584);
#3852=CIRCLE('',#10841,0.120858028271594);
#3853=CIRCLE('',#10850,0.17);
#3854=CIRCLE('',#10853,0.38);
#3855=CIRCLE('',#10861,0.059240625);
#3856=CIRCLE('',#10862,0.059240625);
#3857=CIRCLE('',#10864,0.059240625);
#3858=CIRCLE('',#10865,0.059240625);
#3859=CIRCLE('',#10867,0.059240625);
#3860=CIRCLE('',#10868,0.059240625);
#3861=CIRCLE('',#10870,0.059240625);
#3862=CIRCLE('',#10871,0.059240625);
#3863=CIRCLE('',#10873,0.33848125);
#3864=CIRCLE('',#10874,0.33848125);
#3865=CIRCLE('',#10876,0.33848125);
#3866=CIRCLE('',#10877,0.059240625);
#3867=CIRCLE('',#10878,0.33848125);
#3868=CIRCLE('',#10879,0.5425);
#3869=CIRCLE('',#10880,0.33848125);
#3870=CIRCLE('',#10882,0.33848125);
#3871=CIRCLE('',#10884,0.33848125);
#3872=CIRCLE('',#10886,0.059240625);
#3873=CIRCLE('',#10888,0.33848125);
#3874=CIRCLE('',#10890,0.5425);
#3875=CIRCLE('',#10898,0.04298125);
#3876=CIRCLE('',#10899,0.04298125);
#3877=CIRCLE('',#10901,0.04298125);
#3878=CIRCLE('',#10902,0.04298125);
#3879=CIRCLE('',#10904,0.04298125);
#3880=CIRCLE('',#10905,0.04298125);
#3881=CIRCLE('',#10907,0.04298125);
#3882=CIRCLE('',#10908,0.04298125);
#3883=CIRCLE('',#10910,0.2159625);
#3884=CIRCLE('',#10911,0.2159625);
#3885=CIRCLE('',#10913,0.2159625);
#3886=CIRCLE('',#10914,0.04298125);
#3887=CIRCLE('',#10915,0.2159625);
#3888=CIRCLE('',#10916,0.345);
#3889=CIRCLE('',#10917,0.2159625);
#3890=CIRCLE('',#10919,0.2159625);
#3891=CIRCLE('',#10921,0.2159625);
#3892=CIRCLE('',#10923,0.04298125);
#3893=CIRCLE('',#10925,0.2159625);
#3894=CIRCLE('',#10927,0.345);
#3895=VERTEX_POINT('',#13220);
#3896=VERTEX_POINT('',#13221);
#3897=VERTEX_POINT('',#13223);
#3898=VERTEX_POINT('',#13228);
#3899=VERTEX_POINT('',#13230);
#3900=VERTEX_POINT('',#13234);
#3901=VERTEX_POINT('',#13235);
#3902=VERTEX_POINT('',#13237);
#3903=VERTEX_POINT('',#13242);
#3904=VERTEX_POINT('',#13244);
#3905=VERTEX_POINT('',#13246);
#3906=VERTEX_POINT('',#13283);
#3907=VERTEX_POINT('',#13287);
#3908=VERTEX_POINT('',#13288);
#3909=VERTEX_POINT('',#13293);
#3910=VERTEX_POINT('',#13298);
#3911=VERTEX_POINT('',#13305);
#3912=VERTEX_POINT('',#13307);
#3913=VERTEX_POINT('',#13314);
#3914=VERTEX_POINT('',#13320);
#3915=VERTEX_POINT('',#13390);
#3916=VERTEX_POINT('',#13405);
#3917=VERTEX_POINT('',#13406);
#3918=VERTEX_POINT('',#13408);
#3919=VERTEX_POINT('',#13413);
#3920=VERTEX_POINT('',#13415);
#3921=VERTEX_POINT('',#13419);
#3922=VERTEX_POINT('',#13420);
#3923=VERTEX_POINT('',#13422);
#3924=VERTEX_POINT('',#13430);
#3925=VERTEX_POINT('',#13432);
#3926=VERTEX_POINT('',#13473);
#3927=VERTEX_POINT('',#13477);
#3928=VERTEX_POINT('',#13478);
#3929=VERTEX_POINT('',#13486);
#3930=VERTEX_POINT('',#13493);
#3931=VERTEX_POINT('',#13561);
#3932=VERTEX_POINT('',#13568);
#3933=VERTEX_POINT('',#13575);
#3934=VERTEX_POINT('',#13596);
#3935=VERTEX_POINT('',#13603);
#3936=VERTEX_POINT('',#13610);
#3937=VERTEX_POINT('',#13617);
#3938=VERTEX_POINT('',#13641);
#3939=VERTEX_POINT('',#13661);
#3940=VERTEX_POINT('',#13663);
#3941=VERTEX_POINT('',#13667);
#3942=VERTEX_POINT('',#14220);
#3943=VERTEX_POINT('',#14256);
#3944=VERTEX_POINT('',#14265);
#3945=VERTEX_POINT('',#14267);
#3946=VERTEX_POINT('',#14272);
#3947=VERTEX_POINT('',#14475);
#3948=VERTEX_POINT('',#14477);
#3949=VERTEX_POINT('',#14523);
#3950=VERTEX_POINT('',#14588);
#3951=VERTEX_POINT('',#14628);
#3952=VERTEX_POINT('',#14656);
#3953=VERTEX_POINT('',#14658);
#3954=VERTEX_POINT('',#14687);
#3955=VERTEX_POINT('',#14794);
#3956=VERTEX_POINT('',#14798);
#3957=VERTEX_POINT('',#14821);
#3958=VERTEX_POINT('',#14823);
#3959=VERTEX_POINT('',#14849);
#3960=VERTEX_POINT('',#14875);
#3961=VERTEX_POINT('',#14967);
#3962=VERTEX_POINT('',#14989);
#3963=VERTEX_POINT('',#15100);
#3964=VERTEX_POINT('',#15324);
#3965=VERTEX_POINT('',#15429);
#3966=VERTEX_POINT('',#15431);
#3967=VERTEX_POINT('',#15796);
#3968=VERTEX_POINT('',#15826);
#3969=VERTEX_POINT('',#15827);
#3970=VERTEX_POINT('',#15829);
#3971=VERTEX_POINT('',#15836);
#3972=VERTEX_POINT('',#15876);
#3973=VERTEX_POINT('',#15877);
#3974=VERTEX_POINT('',#15908);
#3975=VERTEX_POINT('',#15927);
#3976=VERTEX_POINT('',#15929);
#3977=VERTEX_POINT('',#15948);
#3978=VERTEX_POINT('',#15949);
#3979=VERTEX_POINT('',#16002);
#3980=VERTEX_POINT('',#16011);
#3981=VERTEX_POINT('',#16594);
#3982=VERTEX_POINT('',#16602);
#3983=VERTEX_POINT('',#16609);
#3984=VERTEX_POINT('',#16624);
#3985=VERTEX_POINT('',#16626);
#3986=VERTEX_POINT('',#16643);
#3987=VERTEX_POINT('',#16746);
#3988=VERTEX_POINT('',#16766);
#3989=VERTEX_POINT('',#16965);
#3990=VERTEX_POINT('',#16966);
#3991=VERTEX_POINT('',#16968);
#3992=VERTEX_POINT('',#16970);
#3993=VERTEX_POINT('',#16997);
#3994=VERTEX_POINT('',#16998);
#3995=VERTEX_POINT('',#17000);
#3996=VERTEX_POINT('',#17005);
#3997=VERTEX_POINT('',#17031);
#3998=VERTEX_POINT('',#17032);
#3999=VERTEX_POINT('',#17090);
#4000=VERTEX_POINT('',#17146);
#4001=VERTEX_POINT('',#17191);
#4002=VERTEX_POINT('',#17196);
#4003=VERTEX_POINT('',#17220);
#4004=VERTEX_POINT('',#17752);
#4005=VERTEX_POINT('',#17767);
#4006=VERTEX_POINT('',#17780);
#4007=VERTEX_POINT('',#17781);
#4008=VERTEX_POINT('',#18331);
#4009=VERTEX_POINT('',#18332);
#4010=VERTEX_POINT('',#18334);
#4011=VERTEX_POINT('',#18339);
#4012=VERTEX_POINT('',#18341);
#4013=VERTEX_POINT('',#18366);
#4014=VERTEX_POINT('',#18367);
#4015=VERTEX_POINT('',#18393);
#4016=VERTEX_POINT('',#18432);
#4017=VERTEX_POINT('',#18439);
#4018=VERTEX_POINT('',#18446);
#4019=VERTEX_POINT('',#18492);
#4020=VERTEX_POINT('',#18571);
#4021=VERTEX_POINT('',#18597);
#4022=VERTEX_POINT('',#18604);
#4023=VERTEX_POINT('',#18672);
#4024=VERTEX_POINT('',#18673);
#4025=VERTEX_POINT('',#18675);
#4026=VERTEX_POINT('',#18680);
#4027=VERTEX_POINT('',#18716);
#4028=VERTEX_POINT('',#18742);
#4029=VERTEX_POINT('',#18743);
#4030=VERTEX_POINT('',#18789);
#4031=VERTEX_POINT('',#18832);
#4032=VERTEX_POINT('',#18833);
#4033=VERTEX_POINT('',#18865);
#4034=VERTEX_POINT('',#18866);
#4035=VERTEX_POINT('',#18881);
#4036=VERTEX_POINT('',#18902);
#4037=VERTEX_POINT('',#19954);
#4038=VERTEX_POINT('',#20173);
#4039=VERTEX_POINT('',#20175);
#4040=VERTEX_POINT('',#20198);
#4041=VERTEX_POINT('',#20199);
#4042=VERTEX_POINT('',#20201);
#4043=VERTEX_POINT('',#20206);
#4044=VERTEX_POINT('',#20232);
#4045=VERTEX_POINT('',#20237);
#4046=VERTEX_POINT('',#20263);
#4047=VERTEX_POINT('',#20264);
#4048=VERTEX_POINT('',#20334);
#4049=VERTEX_POINT('',#20335);
#4050=VERTEX_POINT('',#20430);
#4051=VERTEX_POINT('',#20432);
#4052=VERTEX_POINT('',#20437);
#4053=VERTEX_POINT('',#20563);
#4054=VERTEX_POINT('',#20584);
#4055=VERTEX_POINT('',#20759);
#4056=VERTEX_POINT('',#20763);
#4057=VERTEX_POINT('',#20765);
#4058=VERTEX_POINT('',#20776);
#4059=VERTEX_POINT('',#20805);
#4060=VERTEX_POINT('',#20810);
#4061=VERTEX_POINT('',#20921);
#4062=VERTEX_POINT('',#20923);
#4063=VERTEX_POINT('',#21020);
#4064=VERTEX_POINT('',#21029);
#4065=VERTEX_POINT('',#21031);
#4066=VERTEX_POINT('',#21033);
#4067=VERTEX_POINT('',#21035);
#4068=VERTEX_POINT('',#21041);
#4069=VERTEX_POINT('',#21043);
#4070=VERTEX_POINT('',#21050);
#4071=VERTEX_POINT('',#21052);
#4072=VERTEX_POINT('',#21054);
#4073=VERTEX_POINT('',#21056);
#4074=VERTEX_POINT('',#21059);
#4075=VERTEX_POINT('',#21063);
#4076=VERTEX_POINT('',#21065);
#4077=VERTEX_POINT('',#21067);
#4078=VERTEX_POINT('',#21071);
#4079=VERTEX_POINT('',#21080);
#4080=VERTEX_POINT('',#21084);
#4081=VERTEX_POINT('',#21086);
#4082=VERTEX_POINT('',#21113);
#4083=VERTEX_POINT('',#21114);
#4084=VERTEX_POINT('',#21119);
#4085=VERTEX_POINT('',#21126);
#4086=VERTEX_POINT('',#21135);
#4087=VERTEX_POINT('',#21137);
#4088=VERTEX_POINT('',#21146);
#4089=VERTEX_POINT('',#21161);
#4090=VERTEX_POINT('',#21163);
#4091=VERTEX_POINT('',#21171);
#4092=VERTEX_POINT('',#21178);
#4093=VERTEX_POINT('',#21191);
#4094=VERTEX_POINT('',#21193);
#4095=VERTEX_POINT('',#21195);
#4096=VERTEX_POINT('',#21197);
#4097=VERTEX_POINT('',#21219);
#4098=VERTEX_POINT('',#21242);
#4099=VERTEX_POINT('',#21278);
#4100=VERTEX_POINT('',#21280);
#4101=VERTEX_POINT('',#21325);
#4102=VERTEX_POINT('',#21850);
#4103=VERTEX_POINT('',#21890);
#4104=VERTEX_POINT('',#21977);
#4105=VERTEX_POINT('',#22019);
#4106=VERTEX_POINT('',#22020);
#4107=VERTEX_POINT('',#22027);
#4108=VERTEX_POINT('',#22029);
#4109=VERTEX_POINT('',#22083);
#4110=VERTEX_POINT('',#22115);
#4111=VERTEX_POINT('',#22174);
#4112=VERTEX_POINT('',#22179);
#4113=VERTEX_POINT('',#22202);
#4114=VERTEX_POINT('',#22204);
#4115=VERTEX_POINT('',#22307);
#4116=VERTEX_POINT('',#22312);
#4117=VERTEX_POINT('',#22479);
#4118=VERTEX_POINT('',#22481);
#4119=VERTEX_POINT('',#22524);
#4120=VERTEX_POINT('',#22569);
#4121=VERTEX_POINT('',#22671);
#4122=VERTEX_POINT('',#22697);
#4123=VERTEX_POINT('',#23332);
#4124=VERTEX_POINT('',#23333);
#4125=VERTEX_POINT('',#23335);
#4126=VERTEX_POINT('',#23337);
#4127=VERTEX_POINT('',#23341);
#4128=VERTEX_POINT('',#23343);
#4129=VERTEX_POINT('',#23347);
#4130=VERTEX_POINT('',#23349);
#4131=VERTEX_POINT('',#23353);
#4132=VERTEX_POINT('',#23355);
#4133=VERTEX_POINT('',#23359);
#4134=VERTEX_POINT('',#23361);
#4135=VERTEX_POINT('',#23365);
#4136=VERTEX_POINT('',#23367);
#4137=VERTEX_POINT('',#23371);
#4138=VERTEX_POINT('',#23373);
#4139=VERTEX_POINT('',#23380);
#4140=VERTEX_POINT('',#23382);
#4141=VERTEX_POINT('',#23386);
#4142=VERTEX_POINT('',#23390);
#4143=VERTEX_POINT('',#23394);
#4144=VERTEX_POINT('',#23398);
#4145=VERTEX_POINT('',#23399);
#4146=VERTEX_POINT('',#23401);
#4147=VERTEX_POINT('',#23403);
#4148=VERTEX_POINT('',#23405);
#4149=VERTEX_POINT('',#23407);
#4150=VERTEX_POINT('',#23409);
#4151=VERTEX_POINT('',#23411);
#4152=VERTEX_POINT('',#23413);
#4153=VERTEX_POINT('',#23415);
#4154=VERTEX_POINT('',#23417);
#4155=VERTEX_POINT('',#23419);
#4156=VERTEX_POINT('',#23422);
#4157=VERTEX_POINT('',#23424);
#4158=VERTEX_POINT('',#23426);
#4159=VERTEX_POINT('',#23428);
#4160=VERTEX_POINT('',#23430);
#4161=VERTEX_POINT('',#23432);
#4162=VERTEX_POINT('',#23435);
#4163=VERTEX_POINT('',#23436);
#4164=VERTEX_POINT('',#23440);
#4165=VERTEX_POINT('',#23446);
#4166=VERTEX_POINT('',#23447);
#4167=VERTEX_POINT('',#23451);
#4168=VERTEX_POINT('',#23457);
#4169=VERTEX_POINT('',#23458);
#4170=VERTEX_POINT('',#23462);
#4171=VERTEX_POINT('',#23468);
#4172=VERTEX_POINT('',#23469);
#4173=VERTEX_POINT('',#23473);
#4174=VERTEX_POINT('',#23479);
#4175=VERTEX_POINT('',#23480);
#4176=VERTEX_POINT('',#23484);
#4177=VERTEX_POINT('',#23488);
#4178=VERTEX_POINT('',#23489);
#4179=VERTEX_POINT('',#23493);
#4180=VERTEX_POINT('',#23497);
#4181=VERTEX_POINT('',#23501);
#4182=VERTEX_POINT('',#23505);
#4183=VERTEX_POINT('',#23507);
#4184=VERTEX_POINT('',#23511);
#4185=VERTEX_POINT('',#23513);
#4186=VERTEX_POINT('',#23517);
#4187=VERTEX_POINT('',#23521);
#4188=VERTEX_POINT('',#23525);
#4189=VERTEX_POINT('',#23529);
#4190=VERTEX_POINT('',#23533);
#4191=VERTEX_POINT('',#23537);
#4192=VERTEX_POINT('',#23541);
#4193=VERTEX_POINT('',#23545);
#4194=VERTEX_POINT('',#23549);
#4195=VERTEX_POINT('',#23553);
#4196=VERTEX_POINT('',#23560);
#4197=VERTEX_POINT('',#23564);
#4198=VERTEX_POINT('',#23568);
#4199=VERTEX_POINT('',#23576);
#4200=VERTEX_POINT('',#23577);
#4201=VERTEX_POINT('',#23579);
#4202=VERTEX_POINT('',#23581);
#4203=VERTEX_POINT('',#23585);
#4204=VERTEX_POINT('',#23587);
#4205=VERTEX_POINT('',#23591);
#4206=VERTEX_POINT('',#23592);
#4207=VERTEX_POINT('',#23594);
#4208=VERTEX_POINT('',#23596);
#4209=VERTEX_POINT('',#23603);
#4210=VERTEX_POINT('',#23605);
#4211=VERTEX_POINT('',#23609);
#4212=VERTEX_POINT('',#23611);
#4213=VERTEX_POINT('',#23615);
#4214=VERTEX_POINT('',#23617);
#4215=VERTEX_POINT('',#23624);
#4216=VERTEX_POINT('',#23625);
#4217=VERTEX_POINT('',#23627);
#4218=VERTEX_POINT('',#23629);
#4219=VERTEX_POINT('',#23633);
#4220=VERTEX_POINT('',#23635);
#4221=VERTEX_POINT('',#23639);
#4222=VERTEX_POINT('',#23640);
#4223=VERTEX_POINT('',#23642);
#4224=VERTEX_POINT('',#23644);
#4225=VERTEX_POINT('',#23651);
#4226=VERTEX_POINT('',#23653);
#4227=VERTEX_POINT('',#23657);
#4228=VERTEX_POINT('',#23659);
#4229=VERTEX_POINT('',#23663);
#4230=VERTEX_POINT('',#23665);
#4231=VERTEX_POINT('',#23672);
#4232=VERTEX_POINT('',#23673);
#4233=VERTEX_POINT('',#23675);
#4234=VERTEX_POINT('',#23677);
#4235=VERTEX_POINT('',#23681);
#4236=VERTEX_POINT('',#23683);
#4237=VERTEX_POINT('',#23687);
#4238=VERTEX_POINT('',#23688);
#4239=VERTEX_POINT('',#23690);
#4240=VERTEX_POINT('',#23692);
#4241=VERTEX_POINT('',#23699);
#4242=VERTEX_POINT('',#23701);
#4243=VERTEX_POINT('',#23705);
#4244=VERTEX_POINT('',#23707);
#4245=VERTEX_POINT('',#23711);
#4246=VERTEX_POINT('',#23713);
#4247=VERTEX_POINT('',#23720);
#4248=VERTEX_POINT('',#23722);
#4249=VERTEX_POINT('',#23726);
#4250=VERTEX_POINT('',#23728);
#4251=VERTEX_POINT('',#23732);
#4252=VERTEX_POINT('',#23734);
#4253=VERTEX_POINT('',#23738);
#4254=VERTEX_POINT('',#23740);
#4255=VERTEX_POINT('',#23744);
#4256=VERTEX_POINT('',#23746);
#4257=VERTEX_POINT('',#23750);
#4258=VERTEX_POINT('',#23752);
#4259=VERTEX_POINT('',#23756);
#4260=VERTEX_POINT('',#23757);
#4261=VERTEX_POINT('',#23759);
#4262=VERTEX_POINT('',#23761);
#4263=VERTEX_POINT('',#23765);
#4264=VERTEX_POINT('',#23767);
#4265=VERTEX_POINT('',#23771);
#4266=VERTEX_POINT('',#23773);
#4267=VERTEX_POINT('',#23777);
#4268=VERTEX_POINT('',#23779);
#4269=VERTEX_POINT('',#23783);
#4270=VERTEX_POINT('',#23785);
#4271=VERTEX_POINT('',#23789);
#4272=VERTEX_POINT('',#23791);
#4273=VERTEX_POINT('',#23795);
#4274=VERTEX_POINT('',#23797);
#4275=VERTEX_POINT('',#23807);
#4276=VERTEX_POINT('',#23808);
#4277=VERTEX_POINT('',#23810);
#4278=VERTEX_POINT('',#23812);
#4279=VERTEX_POINT('',#23816);
#4280=VERTEX_POINT('',#23818);
#4281=VERTEX_POINT('',#23822);
#4282=VERTEX_POINT('',#23824);
#4283=VERTEX_POINT('',#23828);
#4284=VERTEX_POINT('',#23830);
#4285=VERTEX_POINT('',#23834);
#4286=VERTEX_POINT('',#23836);
#4287=VERTEX_POINT('',#23843);
#4288=VERTEX_POINT('',#23845);
#4289=VERTEX_POINT('',#23849);
#4290=VERTEX_POINT('',#23853);
#4291=VERTEX_POINT('',#23857);
#4292=VERTEX_POINT('',#23859);
#4293=VERTEX_POINT('',#23861);
#4294=VERTEX_POINT('',#23863);
#4295=VERTEX_POINT('',#23866);
#4296=VERTEX_POINT('',#23870);
#4297=VERTEX_POINT('',#23874);
#4298=VERTEX_POINT('',#23878);
#4299=VERTEX_POINT('',#23882);
#4300=VERTEX_POINT('',#23886);
#4301=VERTEX_POINT('',#23894);
#4302=VERTEX_POINT('',#23896);
#4303=VERTEX_POINT('',#23897);
#4304=VERTEX_POINT('',#23899);
#4305=VERTEX_POINT('',#23906);
#4306=VERTEX_POINT('',#23917);
#4307=VERTEX_POINT('',#24051);
#4308=VERTEX_POINT('',#24188);
#4309=VERTEX_POINT('',#24322);
#4310=VERTEX_POINT('',#24456);
#4311=VERTEX_POINT('',#24468);
#4312=VERTEX_POINT('',#24602);
#4313=VERTEX_POINT('',#24613);
#4314=VERTEX_POINT('',#24750);
#4315=VERTEX_POINT('',#24884);
#4316=VERTEX_POINT('',#25018);
#4317=VERTEX_POINT('',#25029);
#4318=VERTEX_POINT('',#25163);
#4319=VERTEX_POINT('',#25174);
#4320=VERTEX_POINT('',#25308);
#4321=VERTEX_POINT('',#25320);
#4322=VERTEX_POINT('',#25451);
#4323=VERTEX_POINT('',#25462);
#4324=VERTEX_POINT('',#25593);
#4325=VERTEX_POINT('',#25606);
#4326=VERTEX_POINT('',#25740);
#4327=VERTEX_POINT('',#25751);
#4328=VERTEX_POINT('',#25885);
#4329=VERTEX_POINT('',#26019);
#4330=VERTEX_POINT('',#26030);
#4331=VERTEX_POINT('',#26164);
#4332=VERTEX_POINT('',#26301);
#4333=VERTEX_POINT('',#26435);
#4334=VERTEX_POINT('',#26446);
#4335=VERTEX_POINT('',#26580);
#4336=VERTEX_POINT('',#26591);
#4337=VERTEX_POINT('',#26725);
#4338=VERTEX_POINT('',#26862);
#4339=VERTEX_POINT('',#26996);
#4340=VERTEX_POINT('',#27007);
#4341=VERTEX_POINT('',#27141);
#4342=VERTEX_POINT('',#27153);
#4343=VERTEX_POINT('',#27287);
#4344=VERTEX_POINT('',#27298);
#4345=VERTEX_POINT('',#27435);
#4346=VERTEX_POINT('',#27566);
#4347=VERTEX_POINT('',#27700);
#4348=VERTEX_POINT('',#27711);
#4349=VERTEX_POINT('',#27845);
#4350=VERTEX_POINT('',#27856);
#4351=VERTEX_POINT('',#27867);
#4352=VERTEX_POINT('',#28001);
#4353=VERTEX_POINT('',#28012);
#4354=VERTEX_POINT('',#28146);
#4355=VERTEX_POINT('',#28277);
#4356=VERTEX_POINT('',#28414);
#4357=VERTEX_POINT('',#28425);
#4358=VERTEX_POINT('',#28559);
#4359=VERTEX_POINT('',#28571);
#4360=VERTEX_POINT('',#28705);
#4361=VERTEX_POINT('',#28716);
#4362=VERTEX_POINT('',#28850);
#4363=VERTEX_POINT('',#28987);
#4364=VERTEX_POINT('',#29121);
#4365=VERTEX_POINT('',#29132);
#4366=VERTEX_POINT('',#29266);
#4367=VERTEX_POINT('',#29277);
#4368=VERTEX_POINT('',#29411);
#4369=VERTEX_POINT('',#29548);
#4370=VERTEX_POINT('',#29682);
#4371=VERTEX_POINT('',#29693);
#4372=VERTEX_POINT('',#29827);
#4373=VERTEX_POINT('',#29961);
#4374=VERTEX_POINT('',#29972);
#4375=VERTEX_POINT('',#30106);
#4376=VERTEX_POINT('',#30118);
#4377=VERTEX_POINT('',#30198);
#4378=VERTEX_POINT('',#30203);
#4379=VERTEX_POINT('',#30205);
#4380=VERTEX_POINT('',#30212);
#4381=VERTEX_POINT('',#30224);
#4382=VERTEX_POINT('',#30235);
#4383=VERTEX_POINT('',#30369);
#4384=VERTEX_POINT('',#30381);
#4385=VERTEX_POINT('',#30515);
#4386=VERTEX_POINT('',#30526);
#4387=VERTEX_POINT('',#30660);
#4388=VERTEX_POINT('',#30797);
#4389=VERTEX_POINT('',#30931);
#4390=VERTEX_POINT('',#30942);
#4391=VERTEX_POINT('',#31076);
#4392=VERTEX_POINT('',#31087);
#4393=VERTEX_POINT('',#31221);
#4394=VERTEX_POINT('',#31358);
#4395=VERTEX_POINT('',#31492);
#4396=VERTEX_POINT('',#31503);
#4397=VERTEX_POINT('',#31637);
#4398=VERTEX_POINT('',#31771);
#4399=VERTEX_POINT('',#31782);
#4400=VERTEX_POINT('',#31916);
#4401=VERTEX_POINT('',#31928);
#4402=VERTEX_POINT('',#32059);
#4403=VERTEX_POINT('',#32070);
#4404=VERTEX_POINT('',#32201);
#4405=VERTEX_POINT('',#32213);
#4406=VERTEX_POINT('',#32347);
#4407=VERTEX_POINT('',#32358);
#4408=VERTEX_POINT('',#32492);
#4409=VERTEX_POINT('',#32503);
#4410=VERTEX_POINT('',#32637);
#4411=VERTEX_POINT('',#32771);
#4412=VERTEX_POINT('',#32908);
#4413=VERTEX_POINT('',#32919);
#4414=VERTEX_POINT('',#33053);
#4415=VERTEX_POINT('',#33065);
#4416=VERTEX_POINT('',#33199);
#4417=VERTEX_POINT('',#33333);
#4418=VERTEX_POINT('',#33470);
#4419=VERTEX_POINT('',#33604);
#4420=VERTEX_POINT('',#33738);
#4421=VERTEX_POINT('',#33872);
#4422=VERTEX_POINT('',#33884);
#4423=VERTEX_POINT('',#34018);
#4424=VERTEX_POINT('',#34029);
#4425=VERTEX_POINT('',#34166);
#4426=VERTEX_POINT('',#34177);
#4427=VERTEX_POINT('',#34311);
#4428=VERTEX_POINT('',#34322);
#4429=VERTEX_POINT('',#34456);
#4430=VERTEX_POINT('',#34590);
#4431=VERTEX_POINT('',#34721);
#4432=VERTEX_POINT('',#34733);
#4433=VERTEX_POINT('',#34864);
#4434=VERTEX_POINT('',#34998);
#4435=VERTEX_POINT('',#35129);
#4436=VERTEX_POINT('',#35142);
#4437=VERTEX_POINT('',#35276);
#4438=VERTEX_POINT('',#35287);
#4439=VERTEX_POINT('',#35299);
#4440=VERTEX_POINT('',#35433);
#4441=VERTEX_POINT('',#35444);
#4442=VERTEX_POINT('',#35578);
#4443=VERTEX_POINT('',#35591);
#4444=VERTEX_POINT('',#35725);
#4445=VERTEX_POINT('',#35736);
#4446=VERTEX_POINT('',#35870);
#4447=VERTEX_POINT('',#35881);
#4448=VERTEX_POINT('',#36015);
#4449=VERTEX_POINT('',#36027);
#4450=VERTEX_POINT('',#36161);
#4451=VERTEX_POINT('',#36172);
#4452=VERTEX_POINT('',#36247);
#4453=VERTEX_POINT('',#36250);
#4454=VERTEX_POINT('',#36251);
#4455=VERTEX_POINT('',#36758);
#4456=VERTEX_POINT('',#36760);
#4457=VERTEX_POINT('',#36861);
#4458=VERTEX_POINT('',#37408);
#4459=VERTEX_POINT('',#37527);
#4460=VERTEX_POINT('',#38058);
#4461=VERTEX_POINT('',#38070);
#4462=VERTEX_POINT('',#38605);
#4463=VERTEX_POINT('',#39160);
#4464=VERTEX_POINT('',#39691);
#4465=VERTEX_POINT('',#40230);
#4466=VERTEX_POINT('',#40769);
#4467=VERTEX_POINT('',#41314);
#4468=VERTEX_POINT('',#41863);
#4469=VERTEX_POINT('',#42414);
#4470=VERTEX_POINT('',#42426);
#4471=VERTEX_POINT('',#42957);
#4472=VERTEX_POINT('',#43482);
#4473=VERTEX_POINT('',#44023);
#4474=VERTEX_POINT('',#44558);
#4475=VERTEX_POINT('',#45075);
#4476=VERTEX_POINT('',#45610);
#4477=VERTEX_POINT('',#46167);
#4478=VERTEX_POINT('',#46722);
#4479=VERTEX_POINT('',#46734);
#4480=VERTEX_POINT('',#47267);
#4481=VERTEX_POINT('',#47800);
#4482=VERTEX_POINT('',#48349);
#4483=VERTEX_POINT('',#48884);
#4484=VERTEX_POINT('',#49433);
#4485=VERTEX_POINT('',#50000);
#4486=VERTEX_POINT('',#50543);
#4487=VERTEX_POINT('',#51080);
#4488=VERTEX_POINT('',#51091);
#4489=VERTEX_POINT('',#51658);
#4490=VERTEX_POINT('',#52195);
#4491=VERTEX_POINT('',#52734);
#4492=VERTEX_POINT('',#53255);
#4493=VERTEX_POINT('',#53802);
#4494=VERTEX_POINT('',#54337);
#4495=VERTEX_POINT('',#54886);
#4496=VERTEX_POINT('',#54906);
#4497=VERTEX_POINT('',#54908);
#4498=VERTEX_POINT('',#55018);
#4499=VERTEX_POINT('',#55559);
#4500=VERTEX_POINT('',#56094);
#4501=VERTEX_POINT('',#56629);
#4502=VERTEX_POINT('',#56640);
#4503=VERTEX_POINT('',#56759);
#4504=VERTEX_POINT('',#57304);
#4505=VERTEX_POINT('',#57875);
#4506=VERTEX_POINT('',#58436);
#4507=VERTEX_POINT('',#58552);
#4508=VERTEX_POINT('',#58671);
#4509=VERTEX_POINT('',#59214);
#4510=VERTEX_POINT('',#59741);
#4511=VERTEX_POINT('',#60284);
#4512=VERTEX_POINT('',#60295);
#4513=VERTEX_POINT('',#60820);
#4514=VERTEX_POINT('',#61349);
#4515=VERTEX_POINT('',#61902);
#4516=VERTEX_POINT('',#61913);
#4517=VERTEX_POINT('',#62464);
#4518=VERTEX_POINT('',#62997);
#4519=VERTEX_POINT('',#63530);
#4520=VERTEX_POINT('',#63649);
#4521=VERTEX_POINT('',#64176);
#4522=VERTEX_POINT('',#64705);
#4523=VERTEX_POINT('',#65254);
#4524=VERTEX_POINT('',#65803);
#4525=VERTEX_POINT('',#65814);
#4526=VERTEX_POINT('',#66351);
#4527=VERTEX_POINT('',#66876);
#4528=VERTEX_POINT('',#67419);
#4529=VERTEX_POINT('',#67950);
#4530=VERTEX_POINT('',#68503);
#4531=VERTEX_POINT('',#69040);
#4532=VERTEX_POINT('',#69567);
#4533=VERTEX_POINT('',#70096);
#4534=VERTEX_POINT('',#70108);
#4535=VERTEX_POINT('',#70667);
#4536=VERTEX_POINT('',#71755);
#4537=VERTEX_POINT('',#71756);
#4538=VERTEX_POINT('',#71758);
#4539=VERTEX_POINT('',#71760);
#4540=VERTEX_POINT('',#71764);
#4541=VERTEX_POINT('',#71766);
#4542=VERTEX_POINT('',#71770);
#4543=VERTEX_POINT('',#71772);
#4544=VERTEX_POINT('',#71776);
#4545=VERTEX_POINT('',#71778);
#4546=VERTEX_POINT('',#71782);
#4547=VERTEX_POINT('',#71784);
#4548=VERTEX_POINT('',#71853);
#4549=VERTEX_POINT('',#75716);
#4550=VERTEX_POINT('',#75721);
#4551=VERTEX_POINT('',#75727);
#4552=VERTEX_POINT('',#75728);
#4553=VERTEX_POINT('',#75730);
#4554=VERTEX_POINT('',#75732);
#4555=VERTEX_POINT('',#75734);
#4556=VERTEX_POINT('',#75738);
#4557=VERTEX_POINT('',#75742);
#4558=VERTEX_POINT('',#75743);
#4559=VERTEX_POINT('',#75745);
#4560=VERTEX_POINT('',#75747);
#4561=VERTEX_POINT('',#75749);
#4562=VERTEX_POINT('',#75756);
#4563=VERTEX_POINT('',#75757);
#4564=VERTEX_POINT('',#75759);
#4565=VERTEX_POINT('',#75761);
#4566=VERTEX_POINT('',#75763);
#4567=VERTEX_POINT('',#75767);
#4568=VERTEX_POINT('',#75771);
#4569=VERTEX_POINT('',#75772);
#4570=VERTEX_POINT('',#75774);
#4571=VERTEX_POINT('',#75776);
#4572=VERTEX_POINT('',#75778);
#4573=VERTEX_POINT('',#75784);
#4574=VERTEX_POINT('',#75785);
#4575=VERTEX_POINT('',#75787);
#4576=VERTEX_POINT('',#75789);
#4577=VERTEX_POINT('',#75793);
#4578=VERTEX_POINT('',#75795);
#4579=VERTEX_POINT('',#75799);
#4580=VERTEX_POINT('',#75803);
#4581=VERTEX_POINT('',#75810);
#4582=VERTEX_POINT('',#75812);
#4583=VERTEX_POINT('',#75814);
#4584=VERTEX_POINT('',#75827);
#4585=VERTEX_POINT('',#75863);
#4586=VERTEX_POINT('',#75864);
#4587=VERTEX_POINT('',#75909);
#4588=VERTEX_POINT('',#75913);
#4589=VERTEX_POINT('',#75915);
#4590=VERTEX_POINT('',#75917);
#4591=VERTEX_POINT('',#75928);
#4592=VERTEX_POINT('',#75958);
#4593=VERTEX_POINT('',#75959);
#4594=VERTEX_POINT('',#75996);
#4595=VERTEX_POINT('',#76000);
#4596=VERTEX_POINT('',#76004);
#4597=VERTEX_POINT('',#76008);
#4598=VERTEX_POINT('',#76010);
#4599=VERTEX_POINT('',#76016);
#4600=VERTEX_POINT('',#76022);
#4601=VERTEX_POINT('',#77138);
#4602=VERTEX_POINT('',#77177);
#4603=VERTEX_POINT('',#77330);
#4604=VERTEX_POINT('',#77332);
#4605=VERTEX_POINT('',#77336);
#4606=VERTEX_POINT('',#77340);
#4607=VERTEX_POINT('',#77343);
#4608=VERTEX_POINT('',#77347);
#4609=VERTEX_POINT('',#77350);
#4610=VERTEX_POINT('',#77354);
#4611=VERTEX_POINT('',#77357);
#4612=VERTEX_POINT('',#77361);
#4613=VERTEX_POINT('',#77365);
#4614=VERTEX_POINT('',#77369);
#4615=VERTEX_POINT('',#77372);
#4616=VERTEX_POINT('',#77376);
#4617=VERTEX_POINT('',#77379);
#4618=VERTEX_POINT('',#77383);
#4619=VERTEX_POINT('',#77389);
#4620=VERTEX_POINT('',#77390);
#4621=VERTEX_POINT('',#77392);
#4622=VERTEX_POINT('',#77394);
#4623=VERTEX_POINT('',#77396);
#4624=VERTEX_POINT('',#77402);
#4625=VERTEX_POINT('',#77403);
#4626=VERTEX_POINT('',#77405);
#4627=VERTEX_POINT('',#77409);
#4628=VERTEX_POINT('',#77411);
#4629=VERTEX_POINT('',#77420);
#4630=VERTEX_POINT('',#77422);
#4631=VERTEX_POINT('',#77424);
#4632=VERTEX_POINT('',#77426);
#4633=VERTEX_POINT('',#77428);
#4634=VERTEX_POINT('',#77430);
#4635=VERTEX_POINT('',#77432);
#4636=VERTEX_POINT('',#77434);
#4637=VERTEX_POINT('',#77436);
#4638=VERTEX_POINT('',#77438);
#4639=VERTEX_POINT('',#77440);
#4640=VERTEX_POINT('',#77442);
#4641=VERTEX_POINT('',#77444);
#4642=VERTEX_POINT('',#77446);
#4643=VERTEX_POINT('',#77448);
#4644=VERTEX_POINT('',#77450);
#4645=VERTEX_POINT('',#77452);
#4646=VERTEX_POINT('',#77454);
#4647=VERTEX_POINT('',#77456);
#4648=VERTEX_POINT('',#77458);
#4649=VERTEX_POINT('',#77460);
#4650=VERTEX_POINT('',#77462);
#4651=VERTEX_POINT('',#77464);
#4652=VERTEX_POINT('',#77466);
#4653=VERTEX_POINT('',#77468);
#4654=VERTEX_POINT('',#77470);
#4655=VERTEX_POINT('',#77472);
#4656=VERTEX_POINT('',#77474);
#4657=VERTEX_POINT('',#77477);
#4658=VERTEX_POINT('',#77480);
#4659=VERTEX_POINT('',#77486);
#4660=VERTEX_POINT('',#77492);
#4661=VERTEX_POINT('',#77493);
#4662=VERTEX_POINT('',#77495);
#4663=VERTEX_POINT('',#77502);
#4664=VERTEX_POINT('',#77504);
#4665=VERTEX_POINT('',#77512);
#4666=VERTEX_POINT('',#77518);
#4667=VERTEX_POINT('',#77519);
#4668=VERTEX_POINT('',#77521);
#4669=VERTEX_POINT('',#77528);
#4670=VERTEX_POINT('',#77530);
#4671=VERTEX_POINT('',#77538);
#4672=VERTEX_POINT('',#77544);
#4673=VERTEX_POINT('',#77545);
#4674=VERTEX_POINT('',#77547);
#4675=VERTEX_POINT('',#77554);
#4676=VERTEX_POINT('',#77556);
#4677=VERTEX_POINT('',#77562);
#4678=VERTEX_POINT('',#77566);
#4679=VERTEX_POINT('',#77572);
#4680=VERTEX_POINT('',#77573);
#4681=VERTEX_POINT('',#77575);
#4682=VERTEX_POINT('',#77582);
#4683=VERTEX_POINT('',#77584);
#4684=VERTEX_POINT('',#77592);
#4685=VERTEX_POINT('',#77598);
#4686=VERTEX_POINT('',#77599);
#4687=VERTEX_POINT('',#77601);
#4688=VERTEX_POINT('',#77608);
#4689=VERTEX_POINT('',#77610);
#4690=VERTEX_POINT('',#77618);
#4691=VERTEX_POINT('',#77624);
#4692=VERTEX_POINT('',#77626);
#4693=VERTEX_POINT('',#77630);
#4694=VERTEX_POINT('',#77634);
#4695=VERTEX_POINT('',#77636);
#4696=VERTEX_POINT('',#77644);
#4697=VERTEX_POINT('',#77650);
#4698=VERTEX_POINT('',#77652);
#4699=VERTEX_POINT('',#77656);
#4700=VERTEX_POINT('',#77658);
#4701=VERTEX_POINT('',#77666);
#4702=VERTEX_POINT('',#77668);
#4703=VERTEX_POINT('',#77672);
#4704=VERTEX_POINT('',#77675);
#4705=VERTEX_POINT('',#77679);
#4706=VERTEX_POINT('',#77684);
#4707=VERTEX_POINT('',#77690);
#4708=VERTEX_POINT('',#77691);
#4709=VERTEX_POINT('',#77693);
#4710=VERTEX_POINT('',#77695);
#4711=VERTEX_POINT('',#77699);
#4712=VERTEX_POINT('',#77700);
#4713=VERTEX_POINT('',#77702);
#4714=VERTEX_POINT('',#77704);
#4715=VERTEX_POINT('',#77712);
#4716=VERTEX_POINT('',#77715);
#4717=VERTEX_POINT('',#77723);
#4718=VERTEX_POINT('',#77725);
#4719=VERTEX_POINT('',#77729);
#4720=VERTEX_POINT('',#77733);
#4721=VERTEX_POINT('',#77736);
#4722=VERTEX_POINT('',#77740);
#4723=VERTEX_POINT('',#77743);
#4724=VERTEX_POINT('',#77747);
#4725=VERTEX_POINT('',#77750);
#4726=VERTEX_POINT('',#77754);
#4727=VERTEX_POINT('',#77758);
#4728=VERTEX_POINT('',#77762);
#4729=VERTEX_POINT('',#77765);
#4730=VERTEX_POINT('',#77769);
#4731=VERTEX_POINT('',#77772);
#4732=VERTEX_POINT('',#77776);
#4733=VERTEX_POINT('',#77782);
#4734=VERTEX_POINT('',#77784);
#4735=VERTEX_POINT('',#77788);
#4736=VERTEX_POINT('',#77792);
#4737=VERTEX_POINT('',#77795);
#4738=VERTEX_POINT('',#77799);
#4739=VERTEX_POINT('',#77803);
#4740=VERTEX_POINT('',#77807);
#4741=VERTEX_POINT('',#77813);
#4742=VERTEX_POINT('',#77816);
#4743=VERTEX_POINT('',#77820);
#4744=VERTEX_POINT('',#77824);
#4745=VERTEX_POINT('',#77827);
#4746=VERTEX_POINT('',#77831);
#4747=VERTEX_POINT('',#77834);
#4748=VERTEX_POINT('',#77838);
#4749=VERTEX_POINT('',#77844);
#4750=VERTEX_POINT('',#77847);
#4751=VERTEX_POINT('',#77851);
#4752=VERTEX_POINT('',#77855);
#4753=VERTEX_POINT('',#77858);
#4754=VERTEX_POINT('',#77862);
#4755=VERTEX_POINT('',#77865);
#4756=VERTEX_POINT('',#77869);
#4757=VERTEX_POINT('',#77875);
#4758=VERTEX_POINT('',#77877);
#4759=VERTEX_POINT('',#77881);
#4760=VERTEX_POINT('',#77886);
#4761=VERTEX_POINT('',#77892);
#4762=VERTEX_POINT('',#77893);
#4763=VERTEX_POINT('',#77895);
#4764=VERTEX_POINT('',#77945);
#4765=VERTEX_POINT('',#77976);
#4766=VERTEX_POINT('',#77977);
#4767=VERTEX_POINT('',#77979);
#4768=VERTEX_POINT('',#78081);
#4769=VERTEX_POINT('',#78244);
#4770=VERTEX_POINT('',#78245);
#4771=VERTEX_POINT('',#78247);
#4772=VERTEX_POINT('',#78537);
#4773=VERTEX_POINT('',#78538);
#4774=VERTEX_POINT('',#78540);
#4775=VERTEX_POINT('',#78645);
#4776=VERTEX_POINT('',#78859);
#4777=VERTEX_POINT('',#78860);
#4778=VERTEX_POINT('',#78862);
#4779=VERTEX_POINT('',#79156);
#4780=VERTEX_POINT('',#79157);
#4781=VERTEX_POINT('',#79159);
#4782=VERTEX_POINT('',#79261);
#4783=VERTEX_POINT('',#79479);
#4784=VERTEX_POINT('',#79480);
#4785=VERTEX_POINT('',#79482);
#4786=VERTEX_POINT('',#79784);
#4787=VERTEX_POINT('',#79785);
#4788=VERTEX_POINT('',#79787);
#4789=VERTEX_POINT('',#79889);
#4790=VERTEX_POINT('',#80091);
#4791=VERTEX_POINT('',#80092);
#4792=VERTEX_POINT('',#80094);
#4793=VERTEX_POINT('',#80392);
#4794=VERTEX_POINT('',#80393);
#4795=VERTEX_POINT('',#80395);
#4796=VERTEX_POINT('',#80497);
#4797=VERTEX_POINT('',#80719);
#4798=VERTEX_POINT('',#80720);
#4799=VERTEX_POINT('',#80722);
#4800=VERTEX_POINT('',#81014);
#4801=VERTEX_POINT('',#81015);
#4802=VERTEX_POINT('',#81017);
#4803=VERTEX_POINT('',#81116);
#4804=VERTEX_POINT('',#81330);
#4805=VERTEX_POINT('',#81331);
#4806=VERTEX_POINT('',#81333);
#4807=VERTEX_POINT('',#81632);
#4808=VERTEX_POINT('',#81633);
#4809=VERTEX_POINT('',#81635);
#4810=VERTEX_POINT('',#81737);
#4811=VERTEX_POINT('',#81861);
#4812=VERTEX_POINT('',#81862);
#4813=VERTEX_POINT('',#81869);
#4814=VERTEX_POINT('',#81871);
#4815=VERTEX_POINT('',#81877);
#4816=VERTEX_POINT('',#81993);
#4817=VERTEX_POINT('',#82004);
#4818=VERTEX_POINT('',#82016);
#4819=VERTEX_POINT('',#82027);
#4820=VERTEX_POINT('',#82038);
#4821=VERTEX_POINT('',#82157);
#4822=VERTEX_POINT('',#82273);
#4823=VERTEX_POINT('',#82389);
#4824=VERTEX_POINT('',#82502);
#4825=VERTEX_POINT('',#82621);
#4826=VERTEX_POINT('',#82734);
#4827=VERTEX_POINT('',#82847);
#4828=VERTEX_POINT('',#82963);
#4829=VERTEX_POINT('',#82972);
#4830=VERTEX_POINT('',#82974);
#4831=VERTEX_POINT('',#82982);
#4832=VERTEX_POINT('',#83098);
#4833=VERTEX_POINT('',#83211);
#4834=VERTEX_POINT('',#83324);
#4835=VERTEX_POINT('',#83443);
#4836=VERTEX_POINT('',#83556);
#4837=VERTEX_POINT('',#83672);
#4838=VERTEX_POINT('',#83788);
#4839=VERTEX_POINT('',#83904);
#4840=VERTEX_POINT('',#84020);
#4841=VERTEX_POINT('',#84133);
#4842=VERTEX_POINT('',#84252);
#4843=VERTEX_POINT('',#84376);
#4844=VERTEX_POINT('',#84384);
#4845=VERTEX_POINT('',#84413);
#4846=VERTEX_POINT('',#84415);
#4847=VERTEX_POINT('',#84953);
#4848=VERTEX_POINT('',#84955);
#4849=VERTEX_POINT('',#85441);
#4850=VERTEX_POINT('',#85442);
#4851=VERTEX_POINT('',#85448);
#4852=VERTEX_POINT('',#85449);
#4853=VERTEX_POINT('',#85455);
#4854=VERTEX_POINT('',#85456);
#4855=VERTEX_POINT('',#85462);
#4856=VERTEX_POINT('',#85463);
#4857=VERTEX_POINT('',#85469);
#4858=VERTEX_POINT('',#85470);
#4859=VERTEX_POINT('',#85474);
#4860=VERTEX_POINT('',#85478);
#4861=VERTEX_POINT('',#85479);
#4862=VERTEX_POINT('',#85485);
#4863=VERTEX_POINT('',#85488);
#4864=VERTEX_POINT('',#85491);
#4865=VERTEX_POINT('',#85494);
#4866=VERTEX_POINT('',#85497);
#4867=VERTEX_POINT('',#85500);
#4868=VERTEX_POINT('',#85503);
#4869=VERTEX_POINT('',#85507);
#4870=VERTEX_POINT('',#85508);
#4871=VERTEX_POINT('',#85512);
#4872=VERTEX_POINT('',#85514);
#4873=VERTEX_POINT('',#85518);
#4874=VERTEX_POINT('',#85522);
#4875=VERTEX_POINT('',#85526);
#4876=VERTEX_POINT('',#85530);
#4877=VERTEX_POINT('',#85537);
#4878=VERTEX_POINT('',#85542);
#4879=VERTEX_POINT('',#85548);
#4880=VERTEX_POINT('',#85549);
#4881=VERTEX_POINT('',#85551);
#4882=VERTEX_POINT('',#85553);
#4883=VERTEX_POINT('',#85557);
#4884=VERTEX_POINT('',#85558);
#4885=VERTEX_POINT('',#85560);
#4886=VERTEX_POINT('',#85562);
#4887=VERTEX_POINT('',#85566);
#4888=VERTEX_POINT('',#85567);
#4889=VERTEX_POINT('',#85569);
#4890=VERTEX_POINT('',#85571);
#4891=VERTEX_POINT('',#85575);
#4892=VERTEX_POINT('',#85576);
#4893=VERTEX_POINT('',#85578);
#4894=VERTEX_POINT('',#85580);
#4895=VERTEX_POINT('',#85584);
#4896=VERTEX_POINT('',#85586);
#4897=VERTEX_POINT('',#85590);
#4898=VERTEX_POINT('',#85592);
#4899=VERTEX_POINT('',#85596);
#4900=VERTEX_POINT('',#85598);
#4901=VERTEX_POINT('',#85602);
#4902=VERTEX_POINT('',#85604);
#4903=VERTEX_POINT('',#85611);
#4904=VERTEX_POINT('',#85613);
#4905=VERTEX_POINT('',#85621);
#4906=VERTEX_POINT('',#85625);
#4907=VERTEX_POINT('',#85635);
#4908=VERTEX_POINT('',#85636);
#4909=VERTEX_POINT('',#85638);
#4910=VERTEX_POINT('',#85640);
#4911=VERTEX_POINT('',#85644);
#4912=VERTEX_POINT('',#85645);
#4913=VERTEX_POINT('',#85647);
#4914=VERTEX_POINT('',#85649);
#4915=VERTEX_POINT('',#85653);
#4916=VERTEX_POINT('',#85654);
#4917=VERTEX_POINT('',#85656);
#4918=VERTEX_POINT('',#85658);
#4919=VERTEX_POINT('',#85662);
#4920=VERTEX_POINT('',#85663);
#4921=VERTEX_POINT('',#85665);
#4922=VERTEX_POINT('',#85667);
#4923=VERTEX_POINT('',#85671);
#4924=VERTEX_POINT('',#85673);
#4925=VERTEX_POINT('',#85677);
#4926=VERTEX_POINT('',#85679);
#4927=VERTEX_POINT('',#85683);
#4928=VERTEX_POINT('',#85685);
#4929=VERTEX_POINT('',#85689);
#4930=VERTEX_POINT('',#85691);
#4931=VERTEX_POINT('',#85698);
#4932=VERTEX_POINT('',#85700);
#4933=VERTEX_POINT('',#85708);
#4934=VERTEX_POINT('',#85712);
#4935=EDGE_CURVE('',#3895,#3896,#3493,.T.);
#4936=EDGE_CURVE('',#3896,#3897,#3494,.T.);
#4937=EDGE_CURVE('',#3897,#3897,#3495,.T.);
#4938=EDGE_CURVE('',#3896,#3895,#3496,.T.);
#4939=EDGE_CURVE('',#3895,#3898,#1199,.T.);
#4940=EDGE_CURVE('',#3899,#3898,#3497,.T.);
#4941=EDGE_CURVE('',#3898,#3899,#3498,.T.);
#4942=EDGE_CURVE('',#3900,#3901,#1200,.T.);
#4943=EDGE_CURVE('',#3902,#3900,#490,.T.);
#4944=EDGE_CURVE('',#3903,#3902,#1201,.T.);
#4945=EDGE_CURVE('',#3904,#3903,#1202,.T.);
#4946=EDGE_CURVE('',#3905,#3904,#475,.T.);
#4947=EDGE_CURVE('',#3901,#3905,#491,.T.);
#4948=EDGE_CURVE('',#3906,#3906,#3499,.T.);
#4949=EDGE_CURVE('',#3906,#3899,#3500,.T.);
#4950=EDGE_CURVE('',#3907,#3908,#492,.T.);
#4951=EDGE_CURVE('',#3909,#3907,#493,.T.);
#4952=EDGE_CURVE('',#3910,#3909,#494,.T.);
#4953=EDGE_CURVE('',#3911,#3910,#1203,.T.);
#4954=EDGE_CURVE('',#3912,#3911,#495,.T.);
#4955=EDGE_CURVE('',#3913,#3912,#496,.T.);
#4956=EDGE_CURVE('',#3913,#3914,#497,.T.);
#4957=EDGE_CURVE('',#3914,#3915,#498,.T.);
#4958=EDGE_CURVE('',#3908,#3915,#499,.T.);
#4959=EDGE_CURVE('',#3916,#3917,#3501,.T.);
#4960=EDGE_CURVE('',#3917,#3918,#3502,.T.);
#4961=EDGE_CURVE('',#3918,#3918,#3503,.T.);
#4962=EDGE_CURVE('',#3917,#3916,#3504,.T.);
#4963=EDGE_CURVE('',#3916,#3919,#1204,.T.);
#4964=EDGE_CURVE('',#3920,#3919,#3505,.T.);
#4965=EDGE_CURVE('',#3919,#3920,#3506,.T.);
#4966=EDGE_CURVE('',#3921,#3922,#1205,.T.);
#4967=EDGE_CURVE('',#3923,#3921,#500,.T.);
#4968=EDGE_CURVE('',#3923,#3924,#1206,.T.);
#4969=EDGE_CURVE('',#3925,#3924,#501,.T.);
#4970=EDGE_CURVE('',#3922,#3925,#502,.T.);
#4971=EDGE_CURVE('',#3926,#3926,#3507,.T.);
#4972=EDGE_CURVE('',#3926,#3920,#3508,.T.);
#4973=EDGE_CURVE('',#3927,#3928,#503,.T.);
#4974=EDGE_CURVE('',#3929,#3927,#504,.T.);
#4975=EDGE_CURVE('',#3929,#3930,#505,.T.);
#4976=EDGE_CURVE('',#3931,#3930,#506,.T.);
#4977=EDGE_CURVE('',#3932,#3931,#507,.T.);
#4978=EDGE_CURVE('',#3933,#3932,#508,.T.);
#4979=EDGE_CURVE('',#3934,#3933,#509,.T.);
#4980=EDGE_CURVE('',#3935,#3934,#510,.T.);
#4981=EDGE_CURVE('',#3936,#3935,#511,.T.);
#4982=EDGE_CURVE('',#3937,#3936,#512,.T.);
#4983=EDGE_CURVE('',#3937,#3928,#1207,.T.);
#4984=EDGE_CURVE('',#3938,#3927,#513,.T.);
#4985=EDGE_CURVE('',#3938,#3939,#1208,.T.);
#4986=EDGE_CURVE('',#3939,#3940,#3509,.T.);
#4987=EDGE_CURVE('',#3940,#3929,#1209,.T.);
#4988=EDGE_CURVE('',#3921,#3941,#514,.T.);
#4989=EDGE_CURVE('',#3922,#3939,#3510,.T.);
#4990=EDGE_CURVE('',#3939,#3941,#1210,.T.);
#4991=EDGE_CURVE('',#3922,#3940,#3511,.T.);
#4992=EDGE_CURVE('',#3942,#3940,#515,.T.);
#4993=EDGE_CURVE('',#3943,#3942,#516,.T.);
#4994=EDGE_CURVE('',#3944,#3943,#3512,.T.);
#4995=EDGE_CURVE('',#3945,#3944,#517,.T.);
#4996=EDGE_CURVE('',#3946,#3945,#3513,.T.);
#4997=EDGE_CURVE('',#3930,#3946,#3514,.T.);
#4998=EDGE_CURVE('',#3925,#3942,#3515,.T.);
#4999=EDGE_CURVE('',#3947,#3924,#3516,.T.);
#5000=EDGE_CURVE('',#3924,#3948,#518,.T.);
#5001=EDGE_CURVE('',#3948,#3947,#519,.T.);
#5002=EDGE_CURVE('',#3949,#3925,#3517,.T.);
#5003=EDGE_CURVE('',#3947,#3949,#520,.T.);
#5004=EDGE_CURVE('',#3949,#3942,#3518,.T.);
#5005=EDGE_CURVE('',#3949,#3950,#521,.T.);
#5006=EDGE_CURVE('',#3943,#3950,#3519,.T.);
#5007=EDGE_CURVE('',#3948,#3951,#522,.T.);
#5008=EDGE_CURVE('',#3950,#3951,#3520,.T.);
#5009=EDGE_CURVE('',#3952,#3945,#3521,.T.);
#5010=EDGE_CURVE('',#3944,#3953,#3522,.T.);
#5011=EDGE_CURVE('',#3953,#3952,#523,.T.);
#5012=EDGE_CURVE('',#3954,#3946,#3523,.T.);
#5013=EDGE_CURVE('',#3952,#3954,#524,.T.);
#5014=EDGE_CURVE('',#3950,#3953,#3524,.T.);
#5015=EDGE_CURVE('',#3954,#3931,#525,.T.);
#5016=EDGE_CURVE('',#3951,#3955,#3525,.T.);
#5017=EDGE_CURVE('',#3955,#3953,#3526,.T.);
#5018=EDGE_CURVE('',#3956,#3923,#526,.T.);
#5019=EDGE_CURVE('',#3957,#3956,#3527,.T.);
#5020=EDGE_CURVE('',#3957,#3958,#1211,.T.);
#5021=EDGE_CURVE('',#3948,#3958,#527,.T.);
#5022=EDGE_CURVE('',#3955,#3959,#528,.T.);
#5023=EDGE_CURVE('',#3959,#3952,#3528,.T.);
#5024=EDGE_CURVE('',#3959,#3960,#529,.T.);
#5025=EDGE_CURVE('',#3960,#3954,#3529,.T.);
#5026=EDGE_CURVE('',#3960,#3934,#530,.T.);
#5027=EDGE_CURVE('',#3933,#3932,#3530,.T.);
#5028=EDGE_CURVE('',#3936,#3961,#3531,.T.);
#5029=EDGE_CURVE('',#3961,#3937,#531,.T.);
#5030=EDGE_CURVE('',#3962,#3935,#3532,.T.);
#5031=EDGE_CURVE('',#3962,#3961,#532,.T.);
#5032=EDGE_CURVE('',#3960,#3963,#533,.T.);
#5033=EDGE_CURVE('',#3963,#3964,#3533,.T.);
#5034=EDGE_CURVE('',#3964,#3962,#534,.T.);
#5035=EDGE_CURVE('',#3965,#3959,#1212,.T.);
#5036=EDGE_CURVE('',#3966,#3965,#535,.T.);
#5037=EDGE_CURVE('',#3966,#3963,#1213,.T.);
#5038=EDGE_CURVE('',#3967,#3951,#3534,.T.);
#5039=EDGE_CURVE('',#3965,#3967,#536,.T.);
#5040=EDGE_CURVE('',#3968,#3969,#3535,.T.);
#5041=EDGE_CURVE('',#3969,#3970,#537,.T.);
#5042=EDGE_CURVE('',#3970,#3971,#3536,.T.);
#5043=EDGE_CURVE('',#3971,#3968,#538,.T.);
#5044=EDGE_CURVE('',#3972,#3973,#3537,.T.);
#5045=EDGE_CURVE('',#3973,#3969,#539,.T.);
#5046=EDGE_CURVE('',#3972,#3968,#476,.T.);
#5047=EDGE_CURVE('',#3970,#3974,#477,.T.);
#5048=EDGE_CURVE('',#3974,#3971,#3538,.T.);
#5049=EDGE_CURVE('',#3975,#3972,#478,.T.);
#5050=EDGE_CURVE('',#3975,#3976,#3539,.T.);
#5051=EDGE_CURVE('',#3976,#3973,#479,.T.);
#5052=EDGE_CURVE('',#3977,#3978,#540,.T.);
#5053=EDGE_CURVE('',#3978,#3976,#541,.T.);
#5054=EDGE_CURVE('',#3975,#3977,#1214,.T.);
#5055=EDGE_CURVE('',#3973,#3979,#542,.T.);
#5056=EDGE_CURVE('',#3979,#3980,#3540,.T.);
#5057=EDGE_CURVE('',#3980,#3970,#543,.T.);
#5058=EDGE_CURVE('',#3978,#3981,#544,.T.);
#5059=EDGE_CURVE('',#3981,#3982,#545,.T.);
#5060=EDGE_CURVE('',#3982,#3983,#546,.T.);
#5061=EDGE_CURVE('',#3984,#3983,#1215,.T.);
#5062=EDGE_CURVE('',#3985,#3984,#547,.F.);
#5063=EDGE_CURVE('',#3985,#3986,#548,.T.);
#5064=EDGE_CURVE('',#3986,#3979,#3541,.T.);
#5065=EDGE_CURVE('',#3974,#3987,#549,.T.);
#5066=EDGE_CURVE('',#3987,#3988,#3542,.T.);
#5067=EDGE_CURVE('',#3988,#3975,#550,.T.);
#5068=EDGE_CURVE('',#3989,#3990,#3543,.F.);
#5069=EDGE_CURVE('',#3991,#3990,#3544,.T.);
#5070=EDGE_CURVE('',#3991,#3992,#3545,.T.);
#5071=EDGE_CURVE('',#3992,#3989,#551,.T.);
#5072=EDGE_CURVE('',#3993,#3994,#3546,.T.);
#5073=EDGE_CURVE('',#3994,#3995,#552,.T.);
#5074=EDGE_CURVE('',#3995,#3996,#3547,.T.);
#5075=EDGE_CURVE('',#3996,#3993,#553,.T.);
#5076=EDGE_CURVE('',#3997,#3998,#3548,.T.);
#5077=EDGE_CURVE('',#3998,#3996,#554,.T.);
#5078=EDGE_CURVE('',#3995,#3997,#555,.T.);
#5079=EDGE_CURVE('',#3993,#3992,#556,.T.);
#5080=EDGE_CURVE('',#3991,#3994,#557,.T.);
#5081=EDGE_CURVE('',#3999,#3987,#3549,.T.);
#5082=EDGE_CURVE('',#3987,#3998,#3550,.T.);
#5083=EDGE_CURVE('',#3997,#3999,#480,.T.);
#5084=EDGE_CURVE('',#3999,#3988,#3551,.T.);
#5085=EDGE_CURVE('',#3998,#3974,#1216,.T.);
#5086=EDGE_CURVE('',#4000,#3988,#558,.T.);
#5087=EDGE_CURVE('',#3977,#4000,#559,.T.);
#5088=EDGE_CURVE('',#3999,#4001,#560,.T.);
#5089=EDGE_CURVE('',#4001,#4002,#3552,.T.);
#5090=EDGE_CURVE('',#4002,#4000,#561,.T.);
#5091=EDGE_CURVE('',#3995,#4003,#562,.T.);
#5092=EDGE_CURVE('',#4003,#4001,#563,.T.);
#5093=EDGE_CURVE('',#4004,#3994,#1217,.T.);
#5094=EDGE_CURVE('',#4004,#4003,#3553,.T.);
#5095=EDGE_CURVE('',#3992,#3986,#1218,.T.);
#5096=EDGE_CURVE('',#3990,#4005,#1219,.T.);
#5097=EDGE_CURVE('',#4004,#4005,#564,.F.);
#5098=EDGE_CURVE('',#4006,#4007,#3554,.T.);
#5099=EDGE_CURVE('',#4007,#3957,#1220,.T.);
#5100=EDGE_CURVE('',#3956,#4006,#1221,.T.);
#5101=EDGE_CURVE('',#3938,#3941,#565,.T.);
#5102=EDGE_CURVE('',#3928,#4006,#566,.T.);
#5103=EDGE_CURVE('',#4008,#4009,#3555,.T.);
#5104=EDGE_CURVE('',#4009,#4010,#567,.T.);
#5105=EDGE_CURVE('',#4010,#4011,#3556,.T.);
#5106=EDGE_CURVE('',#4011,#4012,#568,.T.);
#5107=EDGE_CURVE('',#4008,#4012,#569,.T.);
#5108=EDGE_CURVE('',#4013,#4014,#3557,.T.);
#5109=EDGE_CURVE('',#4014,#4011,#570,.T.);
#5110=EDGE_CURVE('',#4010,#4013,#571,.T.);
#5111=EDGE_CURVE('',#4015,#4008,#572,.F.);
#5112=EDGE_CURVE('',#4015,#4009,#573,.T.);
#5113=EDGE_CURVE('',#4016,#3910,#574,.T.);
#5114=EDGE_CURVE('',#3910,#4017,#575,.T.);
#5115=EDGE_CURVE('',#4017,#4018,#576,.T.);
#5116=EDGE_CURVE('',#4018,#4016,#3558,.T.);
#5117=EDGE_CURVE('',#4018,#4014,#577,.T.);
#5118=EDGE_CURVE('',#4013,#4016,#578,.T.);
#5119=EDGE_CURVE('',#4012,#4019,#579,.F.);
#5120=EDGE_CURVE('',#3907,#4011,#3559,.T.);
#5121=EDGE_CURVE('',#3908,#4019,#580,.T.);
#5122=EDGE_CURVE('',#4014,#3909,#3560,.T.);
#5123=EDGE_CURVE('',#4015,#4020,#581,.T.);
#5124=EDGE_CURVE('',#4020,#4021,#582,.T.);
#5125=EDGE_CURVE('',#4021,#4022,#583,.T.);
#5126=EDGE_CURVE('',#4022,#4015,#584,.T.);
#5127=EDGE_CURVE('',#4023,#4024,#3561,.T.);
#5128=EDGE_CURVE('',#4024,#4025,#585,.T.);
#5129=EDGE_CURVE('',#4025,#4026,#3562,.T.);
#5130=EDGE_CURVE('',#4026,#4023,#586,.T.);
#5131=EDGE_CURVE('',#4023,#3912,#587,.T.);
#5132=EDGE_CURVE('',#3912,#4027,#3563,.T.);
#5133=EDGE_CURVE('',#4027,#4024,#588,.T.);
#5134=EDGE_CURVE('',#4028,#4029,#3564,.T.);
#5135=EDGE_CURVE('',#4029,#4026,#3565,.T.);
#5136=EDGE_CURVE('',#4025,#4028,#3566,.T.);
#5137=EDGE_CURVE('',#4030,#3911,#589,.F.);
#5138=EDGE_CURVE('',#4030,#4027,#590,.T.);
#5139=EDGE_CURVE('',#4031,#4032,#3567,.T.);
#5140=EDGE_CURVE('',#4032,#4029,#591,.T.);
#5141=EDGE_CURVE('',#4028,#4031,#592,.T.);
#5142=EDGE_CURVE('',#4033,#4034,#593,.T.);
#5143=EDGE_CURVE('',#4033,#4032,#594,.T.);
#5144=EDGE_CURVE('',#4031,#4035,#595,.T.);
#5145=EDGE_CURVE('',#4034,#4035,#596,.T.);
#5146=EDGE_CURVE('',#4026,#4036,#3568,.T.);
#5147=EDGE_CURVE('',#4036,#3913,#1222,.T.);
#5148=EDGE_CURVE('',#3901,#4032,#3569,.T.);
#5149=EDGE_CURVE('',#3901,#4036,#3570,.T.);
#5150=EDGE_CURVE('',#3900,#4033,#481,.T.);
#5151=EDGE_CURVE('',#4034,#3902,#597,.T.);
#5152=EDGE_CURVE('',#4037,#4036,#598,.T.);
#5153=EDGE_CURVE('',#3915,#4037,#599,.T.);
#5154=EDGE_CURVE('',#3905,#4037,#3571,.T.);
#5155=EDGE_CURVE('',#3903,#4035,#600,.F.);
#5156=EDGE_CURVE('',#3989,#4038,#1223,.T.);
#5157=EDGE_CURVE('',#4038,#4039,#3572,.T.);
#5158=EDGE_CURVE('',#4039,#3990,#1224,.T.);
#5159=EDGE_CURVE('',#4040,#4041,#3573,.T.);
#5160=EDGE_CURVE('',#4041,#4042,#601,.T.);
#5161=EDGE_CURVE('',#4042,#4043,#3574,.T.);
#5162=EDGE_CURVE('',#4043,#4040,#602,.T.);
#5163=EDGE_CURVE('',#4042,#4044,#603,.T.);
#5164=EDGE_CURVE('',#4044,#4045,#3575,.T.);
#5165=EDGE_CURVE('',#4045,#4043,#604,.T.);
#5166=EDGE_CURVE('',#4046,#4047,#3576,.T.);
#5167=EDGE_CURVE('',#4047,#4041,#605,.T.);
#5168=EDGE_CURVE('',#4040,#4046,#606,.T.);
#5169=EDGE_CURVE('',#4044,#4039,#607,.T.);
#5170=EDGE_CURVE('',#4038,#4045,#608,.T.);
#5171=EDGE_CURVE('',#4048,#4049,#609,.T.);
#5172=EDGE_CURVE('',#4049,#4047,#610,.T.);
#5173=EDGE_CURVE('',#4046,#4048,#3577,.T.);
#5174=EDGE_CURVE('',#4050,#4041,#482,.T.);
#5175=EDGE_CURVE('',#4051,#4050,#611,.T.);
#5176=EDGE_CURVE('',#4052,#4051,#612,.T.);
#5177=EDGE_CURVE('',#4042,#4052,#1225,.T.);
#5178=EDGE_CURVE('',#4049,#4050,#3578,.T.);
#5179=EDGE_CURVE('',#4048,#4053,#613,.T.);
#5180=EDGE_CURVE('',#4053,#4054,#3579,.T.);
#5181=EDGE_CURVE('',#4054,#4049,#614,.T.);
#5182=EDGE_CURVE('',#4055,#4046,#1226,.T.);
#5183=EDGE_CURVE('',#4053,#4055,#3580,.T.);
#5184=EDGE_CURVE('',#4056,#4045,#1227,.T.);
#5185=EDGE_CURVE('',#4057,#4056,#615,.T.);
#5186=EDGE_CURVE('',#4058,#4057,#616,.T.);
#5187=EDGE_CURVE('',#4055,#4058,#617,.T.);
#5188=EDGE_CURVE('',#4028,#4059,#618,.T.);
#5189=EDGE_CURVE('',#4059,#4060,#3581,.T.);
#5190=EDGE_CURVE('',#4060,#3903,#619,.T.);
#5191=EDGE_CURVE('',#3965,#4061,#3582,.T.);
#5192=EDGE_CURVE('',#4061,#4062,#620,.T.);
#5193=EDGE_CURVE('',#4062,#3966,#3583,.T.);
#5194=EDGE_CURVE('',#4062,#4060,#621,.T.);
#5195=EDGE_CURVE('',#4059,#3966,#622,.T.);
#5196=EDGE_CURVE('',#3958,#3967,#3584,.T.);
#5197=EDGE_CURVE('',#3958,#4061,#623,.T.);
#5198=EDGE_CURVE('',#4063,#4060,#1228,.T.);
#5199=EDGE_CURVE('',#3904,#4063,#624,.T.);
#5200=EDGE_CURVE('',#4064,#3985,#1229,.T.);
#5201=EDGE_CURVE('',#4065,#4064,#1230,.T.);
#5202=EDGE_CURVE('',#4066,#4065,#3585,.T.);
#5203=EDGE_CURVE('',#4067,#4066,#625,.T.);
#5204=EDGE_CURVE('',#4063,#4067,#483,.T.);
#5205=EDGE_CURVE('',#4068,#3957,#1231,.T.);
#5206=EDGE_CURVE('',#4069,#4068,#626,.T.);
#5207=EDGE_CURVE('',#4069,#4056,#1232,.T.);
#5208=EDGE_CURVE('',#4070,#4070,#3586,.T.);
#5209=EDGE_CURVE('',#4071,#4071,#3587,.T.);
#5210=EDGE_CURVE('',#4072,#4072,#3588,.T.);
#5211=EDGE_CURVE('',#4073,#4073,#3589,.T.);
#5212=EDGE_CURVE('',#3984,#4074,#1233,.T.);
#5213=EDGE_CURVE('',#4074,#4064,#3590,.T.);
#5214=EDGE_CURVE('',#4075,#4074,#3591,.T.);
#5215=EDGE_CURVE('',#4074,#4076,#1234,.T.);
#5216=EDGE_CURVE('',#4076,#4077,#3592,.T.);
#5217=EDGE_CURVE('',#4077,#4075,#1235,.T.);
#5218=EDGE_CURVE('',#3982,#4078,#1236,.T.);
#5219=EDGE_CURVE('',#4078,#4076,#3593,.T.);
#5220=EDGE_CURVE('',#4076,#3983,#1237,.T.);
#5221=EDGE_CURVE('',#4078,#4077,#3594,.T.);
#5222=EDGE_CURVE('',#4075,#4064,#3595,.T.);
#5223=EDGE_CURVE('',#4075,#4079,#1238,.T.);
#5224=EDGE_CURVE('',#4079,#4065,#3596,.T.);
#5225=EDGE_CURVE('',#4080,#4077,#1239,.T.);
#5226=EDGE_CURVE('',#4080,#4081,#627,.T.);
#5227=EDGE_CURVE('',#4079,#4081,#1240,.T.);
#5228=EDGE_CURVE('',#4078,#4022,#1241,.T.);
#5229=EDGE_CURVE('',#4021,#4080,#628,.T.);
#5230=EDGE_CURVE('',#4082,#4083,#629,.T.);
#5231=EDGE_CURVE('',#4083,#4084,#630,.T.);
#5232=EDGE_CURVE('',#4084,#4085,#631,.T.);
#5233=EDGE_CURVE('',#4085,#4086,#1242,.T.);
#5234=EDGE_CURVE('',#4087,#4086,#632,.T.);
#5235=EDGE_CURVE('',#4087,#4088,#633,.F.);
#5236=EDGE_CURVE('',#4088,#4089,#1243,.T.);
#5237=EDGE_CURVE('',#4090,#4089,#634,.T.);
#5238=EDGE_CURVE('',#4090,#4007,#1244,.T.);
#5239=EDGE_CURVE('',#4007,#3961,#1245,.T.);
#5240=EDGE_CURVE('',#4091,#3964,#635,.T.);
#5241=EDGE_CURVE('',#4091,#4016,#1246,.T.);
#5242=EDGE_CURVE('',#3981,#4005,#1247,.T.);
#5243=EDGE_CURVE('',#4005,#4092,#1248,.T.);
#5244=EDGE_CURVE('',#4092,#4052,#636,.T.);
#5245=EDGE_CURVE('',#4051,#4082,#637,.T.);
#5246=EDGE_CURVE('',#4093,#4093,#3597,.T.);
#5247=EDGE_CURVE('',#4094,#4094,#3598,.T.);
#5248=EDGE_CURVE('',#4095,#4095,#3599,.T.);
#5249=EDGE_CURVE('',#4096,#4096,#3600,.T.);
#5250=EDGE_CURVE('',#4097,#4066,#3601,.T.);
#5251=EDGE_CURVE('',#4079,#4097,#3602,.T.);
#5252=EDGE_CURVE('',#4098,#4067,#3603,.T.);
#5253=EDGE_CURVE('',#4097,#4098,#638,.T.);
#5254=EDGE_CURVE('',#4063,#4099,#3604,.T.);
#5255=EDGE_CURVE('',#4099,#4100,#639,.T.);
#5256=EDGE_CURVE('',#4100,#3904,#3605,.T.);
#5257=EDGE_CURVE('',#4098,#4099,#484,.T.);
#5258=EDGE_CURVE('',#4101,#3905,#3606,.T.);
#5259=EDGE_CURVE('',#4100,#4101,#485,.T.);
#5260=EDGE_CURVE('',#4101,#4037,#3607,.T.);
#5261=EDGE_CURVE('',#4102,#4097,#1249,.T.);
#5262=EDGE_CURVE('',#4098,#4102,#640,.T.);
#5263=EDGE_CURVE('',#4081,#4102,#3608,.T.);
#5264=EDGE_CURVE('',#4101,#4103,#641,.T.);
#5265=EDGE_CURVE('',#4019,#4103,#642,.F.);
#5266=EDGE_CURVE('',#4030,#4091,#3609,.T.);
#5267=EDGE_CURVE('',#4091,#4104,#3610,.T.);
#5268=EDGE_CURVE('',#4104,#4024,#643,.T.);
#5269=EDGE_CURVE('',#3963,#4104,#644,.T.);
#5270=EDGE_CURVE('',#4105,#4106,#645,.T.);
#5271=EDGE_CURVE('',#4106,#4107,#1250,.T.);
#5272=EDGE_CURVE('',#4107,#4108,#646,.T.);
#5273=EDGE_CURVE('',#4108,#4069,#647,.T.);
#5274=EDGE_CURVE('',#4068,#4090,#1251,.T.);
#5275=EDGE_CURVE('',#4089,#4105,#648,.T.);
#5276=EDGE_CURVE('',#4105,#4088,#1252,.T.);
#5277=EDGE_CURVE('',#4087,#4109,#649,.T.);
#5278=EDGE_CURVE('',#4106,#4109,#3611,.T.);
#5279=EDGE_CURVE('',#4056,#4108,#3612,.T.);
#5280=EDGE_CURVE('',#4109,#4110,#1253,.T.);
#5281=EDGE_CURVE('',#4110,#4107,#3613,.T.);
#5282=EDGE_CURVE('',#4110,#4057,#650,.T.);
#5283=EDGE_CURVE('',#4086,#4111,#651,.T.);
#5284=EDGE_CURVE('',#4112,#4111,#3614,.T.);
#5285=EDGE_CURVE('',#4112,#4109,#3615,.T.);
#5286=EDGE_CURVE('',#4111,#4113,#486,.T.);
#5287=EDGE_CURVE('',#4113,#4114,#3616,.T.);
#5288=EDGE_CURVE('',#4114,#4112,#3617,.T.);
#5289=EDGE_CURVE('',#4083,#4115,#652,.T.);
#5290=EDGE_CURVE('',#4115,#4116,#653,.T.);
#5291=EDGE_CURVE('',#4116,#4117,#3618,.T.);
#5292=EDGE_CURVE('',#4117,#4118,#654,.T.);
#5293=EDGE_CURVE('',#4118,#4084,#3619,.T.);
#5294=EDGE_CURVE('',#4118,#4085,#655,.T.);
#5295=EDGE_CURVE('',#4116,#4119,#3620,.T.);
#5296=EDGE_CURVE('',#4119,#4117,#3621,.T.);
#5297=EDGE_CURVE('',#4119,#4114,#487,.T.);
#5298=EDGE_CURVE('',#4113,#4117,#488,.T.);
#5299=EDGE_CURVE('',#4116,#4054,#656,.T.);
#5300=EDGE_CURVE('',#4120,#4054,#3622,.T.);
#5301=EDGE_CURVE('',#4120,#4119,#657,.T.);
#5302=EDGE_CURVE('',#4049,#4082,#1254,.T.);
#5303=EDGE_CURVE('',#4092,#4039,#1255,.T.);
#5304=EDGE_CURVE('',#4110,#4121,#658,.T.);
#5305=EDGE_CURVE('',#4121,#4058,#3623,.T.);
#5306=EDGE_CURVE('',#4122,#4055,#3624,.T.);
#5307=EDGE_CURVE('',#4121,#4122,#659,.T.);
#5308=EDGE_CURVE('',#4120,#4053,#3625,.T.);
#5309=EDGE_CURVE('',#4122,#4120,#489,.T.);
#5310=EDGE_CURVE('',#4121,#4112,#660,.T.);
#5311=EDGE_CURVE('',#4113,#4118,#1256,.T.);
#5312=EDGE_CURVE('',#4002,#3977,#1257,.T.);
#5313=EDGE_CURVE('',#4073,#4093,#1258,.T.);
#5314=EDGE_CURVE('',#4072,#4094,#1259,.T.);
#5315=EDGE_CURVE('',#4071,#4095,#1260,.T.);
#5316=EDGE_CURVE('',#4070,#4096,#1261,.T.);
#5317=EDGE_CURVE('',#4123,#4124,#1262,.T.);
#5318=EDGE_CURVE('',#4124,#4125,#1263,.T.);
#5319=EDGE_CURVE('',#4125,#4126,#1264,.T.);
#5320=EDGE_CURVE('',#4123,#4126,#1265,.T.);
#5321=EDGE_CURVE('',#4124,#4127,#1266,.T.);
#5322=EDGE_CURVE('',#4127,#4128,#1267,.T.);
#5323=EDGE_CURVE('',#4128,#4125,#1268,.T.);
#5324=EDGE_CURVE('',#4127,#4129,#1269,.T.);
#5325=EDGE_CURVE('',#4129,#4130,#1270,.T.);
#5326=EDGE_CURVE('',#4130,#4128,#1271,.T.);
#5327=EDGE_CURVE('',#4129,#4131,#1272,.T.);
#5328=EDGE_CURVE('',#4131,#4132,#1273,.T.);
#5329=EDGE_CURVE('',#4132,#4130,#1274,.T.);
#5330=EDGE_CURVE('',#4131,#4133,#1275,.T.);
#5331=EDGE_CURVE('',#4133,#4134,#1276,.T.);
#5332=EDGE_CURVE('',#4134,#4132,#1277,.T.);
#5333=EDGE_CURVE('',#4135,#4134,#1278,.T.);
#5334=EDGE_CURVE('',#4133,#4136,#1279,.T.);
#5335=EDGE_CURVE('',#4136,#4135,#1280,.T.);
#5336=EDGE_CURVE('',#4137,#4135,#1281,.T.);
#5337=EDGE_CURVE('',#4136,#4138,#1282,.T.);
#5338=EDGE_CURVE('',#4138,#4137,#1283,.T.);
#5339=EDGE_CURVE('',#4126,#4137,#1284,.T.);
#5340=EDGE_CURVE('',#4138,#4123,#1285,.T.);
#5341=EDGE_CURVE('',#4139,#4135,#1286,.T.);
#5342=EDGE_CURVE('',#4140,#4139,#1287,.T.);
#5343=EDGE_CURVE('',#4140,#4134,#1288,.T.);
#5344=EDGE_CURVE('',#4141,#4137,#1289,.T.);
#5345=EDGE_CURVE('',#4139,#4141,#1290,.T.);
#5346=EDGE_CURVE('',#4142,#4126,#1291,.T.);
#5347=EDGE_CURVE('',#4141,#4142,#1292,.T.);
#5348=EDGE_CURVE('',#4143,#4125,#1293,.T.);
#5349=EDGE_CURVE('',#4142,#4143,#1294,.T.);
#5350=EDGE_CURVE('',#4144,#4145,#1295,.T.);
#5351=EDGE_CURVE('',#4145,#4146,#1296,.T.);
#5352=EDGE_CURVE('',#4146,#4147,#1297,.T.);
#5353=EDGE_CURVE('',#4147,#4148,#1298,.T.);
#5354=EDGE_CURVE('',#4148,#4149,#1299,.T.);
#5355=EDGE_CURVE('',#4149,#4150,#1300,.T.);
#5356=EDGE_CURVE('',#4150,#4151,#1301,.T.);
#5357=EDGE_CURVE('',#4151,#4152,#1302,.T.);
#5358=EDGE_CURVE('',#4152,#4153,#1303,.T.);
#5359=EDGE_CURVE('',#4153,#4154,#1304,.T.);
#5360=EDGE_CURVE('',#4154,#4155,#1305,.T.);
#5361=EDGE_CURVE('',#4155,#4144,#1306,.T.);
#5362=EDGE_CURVE('',#4156,#4156,#3626,.T.);
#5363=EDGE_CURVE('',#4157,#4157,#3627,.T.);
#5364=EDGE_CURVE('',#4158,#4158,#3628,.T.);
#5365=EDGE_CURVE('',#4159,#4159,#3629,.T.);
#5366=EDGE_CURVE('',#4160,#4160,#3630,.T.);
#5367=EDGE_CURVE('',#4161,#4161,#3631,.T.);
#5368=EDGE_CURVE('',#4162,#4163,#1307,.T.);
#5369=EDGE_CURVE('',#4163,#4163,#3632,.T.);
#5370=EDGE_CURVE('',#4163,#4164,#1308,.T.);
#5371=EDGE_CURVE('',#4164,#4164,#3633,.T.);
#5372=EDGE_CURVE('',#4164,#4161,#1309,.T.);
#5373=EDGE_CURVE('',#4165,#4166,#1310,.T.);
#5374=EDGE_CURVE('',#4166,#4166,#3634,.T.);
#5375=EDGE_CURVE('',#4166,#4167,#1311,.T.);
#5376=EDGE_CURVE('',#4167,#4167,#3635,.T.);
#5377=EDGE_CURVE('',#4167,#4160,#1312,.T.);
#5378=EDGE_CURVE('',#4168,#4169,#1313,.T.);
#5379=EDGE_CURVE('',#4169,#4169,#3636,.T.);
#5380=EDGE_CURVE('',#4169,#4170,#1314,.T.);
#5381=EDGE_CURVE('',#4170,#4170,#3637,.T.);
#5382=EDGE_CURVE('',#4170,#4159,#1315,.T.);
#5383=EDGE_CURVE('',#4171,#4172,#1316,.T.);
#5384=EDGE_CURVE('',#4172,#4172,#3638,.T.);
#5385=EDGE_CURVE('',#4172,#4173,#1317,.T.);
#5386=EDGE_CURVE('',#4173,#4173,#3639,.T.);
#5387=EDGE_CURVE('',#4173,#4158,#1318,.T.);
#5388=EDGE_CURVE('',#4174,#4175,#1319,.T.);
#5389=EDGE_CURVE('',#4175,#4175,#3640,.T.);
#5390=EDGE_CURVE('',#4175,#4176,#1320,.T.);
#5391=EDGE_CURVE('',#4176,#4176,#3641,.T.);
#5392=EDGE_CURVE('',#4177,#4178,#1321,.T.);
#5393=EDGE_CURVE('',#4178,#4178,#3642,.T.);
#5394=EDGE_CURVE('',#4178,#4179,#1322,.T.);
#5395=EDGE_CURVE('',#4179,#4179,#3643,.T.);
#5396=EDGE_CURVE('',#4180,#4180,#3644,.T.);
#5397=EDGE_CURVE('',#4180,#4157,#1323,.T.);
#5398=EDGE_CURVE('',#4181,#4181,#3645,.T.);
#5399=EDGE_CURVE('',#4181,#4156,#1324,.T.);
#5400=EDGE_CURVE('',#4182,#4182,#3646,.T.);
#5401=EDGE_CURVE('',#4182,#4183,#1325,.T.);
#5402=EDGE_CURVE('',#4183,#4183,#3647,.T.);
#5403=EDGE_CURVE('',#4144,#4184,#1326,.T.);
#5404=EDGE_CURVE('',#4184,#4185,#1327,.T.);
#5405=EDGE_CURVE('',#4145,#4185,#1328,.T.);
#5406=EDGE_CURVE('',#4155,#4186,#1329,.T.);
#5407=EDGE_CURVE('',#4186,#4184,#1330,.T.);
#5408=EDGE_CURVE('',#4154,#4187,#1331,.T.);
#5409=EDGE_CURVE('',#4187,#4186,#1332,.T.);
#5410=EDGE_CURVE('',#4153,#4188,#1333,.T.);
#5411=EDGE_CURVE('',#4188,#4187,#1334,.T.);
#5412=EDGE_CURVE('',#4152,#4189,#1335,.T.);
#5413=EDGE_CURVE('',#4189,#4188,#1336,.T.);
#5414=EDGE_CURVE('',#4151,#4190,#1337,.T.);
#5415=EDGE_CURVE('',#4190,#4189,#1338,.T.);
#5416=EDGE_CURVE('',#4150,#4191,#1339,.T.);
#5417=EDGE_CURVE('',#4191,#4190,#1340,.T.);
#5418=EDGE_CURVE('',#4149,#4192,#1341,.T.);
#5419=EDGE_CURVE('',#4192,#4191,#1342,.T.);
#5420=EDGE_CURVE('',#4148,#4193,#1343,.T.);
#5421=EDGE_CURVE('',#4193,#4192,#1344,.T.);
#5422=EDGE_CURVE('',#4147,#4194,#1345,.T.);
#5423=EDGE_CURVE('',#4194,#4193,#1346,.T.);
#5424=EDGE_CURVE('',#4146,#4195,#1347,.T.);
#5425=EDGE_CURVE('',#4195,#4194,#1348,.T.);
#5426=EDGE_CURVE('',#4185,#4195,#1349,.T.);
#5427=EDGE_CURVE('',#4196,#4128,#1350,.T.);
#5428=EDGE_CURVE('',#4143,#4196,#1351,.T.);
#5429=EDGE_CURVE('',#4197,#4130,#1352,.T.);
#5430=EDGE_CURVE('',#4196,#4197,#1353,.T.);
#5431=EDGE_CURVE('',#4198,#4132,#1354,.T.);
#5432=EDGE_CURVE('',#4197,#4198,#1355,.T.);
#5433=EDGE_CURVE('',#4198,#4140,#1356,.T.);
#5434=EDGE_CURVE('',#4199,#4200,#3648,.T.);
#5435=EDGE_CURVE('',#4200,#4201,#1357,.T.);
#5436=EDGE_CURVE('',#4201,#4202,#3649,.T.);
#5437=EDGE_CURVE('',#4202,#4199,#1358,.T.);
#5438=EDGE_CURVE('',#4203,#4200,#1359,.T.);
#5439=EDGE_CURVE('',#4204,#4203,#1360,.T.);
#5440=EDGE_CURVE('',#4201,#4204,#1361,.T.);
#5441=EDGE_CURVE('',#4205,#4206,#3650,.T.);
#5442=EDGE_CURVE('',#4206,#4207,#1362,.T.);
#5443=EDGE_CURVE('',#4207,#4208,#3651,.T.);
#5444=EDGE_CURVE('',#4208,#4205,#1363,.T.);
#5445=EDGE_CURVE('',#4207,#4202,#1364,.T.);
#5446=EDGE_CURVE('',#4199,#4206,#1365,.T.);
#5447=EDGE_CURVE('',#4203,#4209,#3652,.T.);
#5448=EDGE_CURVE('',#4209,#4210,#1366,.T.);
#5449=EDGE_CURVE('',#4210,#4204,#3653,.T.);
#5450=EDGE_CURVE('',#4211,#4209,#1367,.T.);
#5451=EDGE_CURVE('',#4212,#4211,#1368,.T.);
#5452=EDGE_CURVE('',#4210,#4212,#1369,.T.);
#5453=EDGE_CURVE('',#4211,#4213,#3654,.T.);
#5454=EDGE_CURVE('',#4213,#4214,#1370,.T.);
#5455=EDGE_CURVE('',#4214,#4212,#3655,.T.);
#5456=EDGE_CURVE('',#4214,#4208,#1371,.T.);
#5457=EDGE_CURVE('',#4205,#4213,#1372,.T.);
#5458=EDGE_CURVE('',#4215,#4216,#3656,.T.);
#5459=EDGE_CURVE('',#4216,#4217,#1373,.T.);
#5460=EDGE_CURVE('',#4217,#4218,#3657,.T.);
#5461=EDGE_CURVE('',#4218,#4215,#1374,.T.);
#5462=EDGE_CURVE('',#4219,#4216,#1375,.T.);
#5463=EDGE_CURVE('',#4220,#4219,#1376,.T.);
#5464=EDGE_CURVE('',#4217,#4220,#1377,.T.);
#5465=EDGE_CURVE('',#4221,#4222,#3658,.T.);
#5466=EDGE_CURVE('',#4222,#4223,#1378,.T.);
#5467=EDGE_CURVE('',#4223,#4224,#3659,.T.);
#5468=EDGE_CURVE('',#4224,#4221,#1379,.T.);
#5469=EDGE_CURVE('',#4223,#4218,#1380,.T.);
#5470=EDGE_CURVE('',#4215,#4222,#1381,.T.);
#5471=EDGE_CURVE('',#4219,#4225,#3660,.T.);
#5472=EDGE_CURVE('',#4225,#4226,#1382,.T.);
#5473=EDGE_CURVE('',#4226,#4220,#3661,.T.);
#5474=EDGE_CURVE('',#4227,#4225,#1383,.T.);
#5475=EDGE_CURVE('',#4228,#4227,#1384,.T.);
#5476=EDGE_CURVE('',#4226,#4228,#1385,.T.);
#5477=EDGE_CURVE('',#4227,#4229,#3662,.T.);
#5478=EDGE_CURVE('',#4229,#4230,#1386,.T.);
#5479=EDGE_CURVE('',#4230,#4228,#3663,.T.);
#5480=EDGE_CURVE('',#4230,#4224,#1387,.T.);
#5481=EDGE_CURVE('',#4221,#4229,#1388,.T.);
#5482=EDGE_CURVE('',#4231,#4232,#3664,.T.);
#5483=EDGE_CURVE('',#4232,#4233,#1389,.T.);
#5484=EDGE_CURVE('',#4233,#4234,#3665,.T.);
#5485=EDGE_CURVE('',#4234,#4231,#1390,.T.);
#5486=EDGE_CURVE('',#4235,#4232,#1391,.T.);
#5487=EDGE_CURVE('',#4236,#4235,#1392,.T.);
#5488=EDGE_CURVE('',#4233,#4236,#1393,.T.);
#5489=EDGE_CURVE('',#4237,#4238,#3666,.T.);
#5490=EDGE_CURVE('',#4238,#4239,#1394,.T.);
#5491=EDGE_CURVE('',#4239,#4240,#3667,.T.);
#5492=EDGE_CURVE('',#4240,#4237,#1395,.T.);
#5493=EDGE_CURVE('',#4239,#4234,#1396,.T.);
#5494=EDGE_CURVE('',#4231,#4238,#1397,.T.);
#5495=EDGE_CURVE('',#4235,#4241,#3668,.T.);
#5496=EDGE_CURVE('',#4241,#4242,#1398,.T.);
#5497=EDGE_CURVE('',#4242,#4236,#3669,.T.);
#5498=EDGE_CURVE('',#4243,#4241,#1399,.T.);
#5499=EDGE_CURVE('',#4244,#4243,#1400,.T.);
#5500=EDGE_CURVE('',#4242,#4244,#1401,.T.);
#5501=EDGE_CURVE('',#4243,#4245,#3670,.T.);
#5502=EDGE_CURVE('',#4245,#4246,#1402,.T.);
#5503=EDGE_CURVE('',#4246,#4244,#3671,.T.);
#5504=EDGE_CURVE('',#4246,#4240,#1403,.T.);
#5505=EDGE_CURVE('',#4237,#4245,#1404,.T.);
#5506=EDGE_CURVE('',#4247,#4247,#3672,.T.);
#5507=EDGE_CURVE('',#4247,#4248,#1405,.T.);
#5508=EDGE_CURVE('',#4248,#4248,#3673,.T.);
#5509=EDGE_CURVE('',#4249,#4249,#3674,.T.);
#5510=EDGE_CURVE('',#4249,#4250,#1406,.T.);
#5511=EDGE_CURVE('',#4250,#4250,#3675,.T.);
#5512=EDGE_CURVE('',#4251,#4251,#3676,.T.);
#5513=EDGE_CURVE('',#4251,#4252,#1407,.T.);
#5514=EDGE_CURVE('',#4252,#4252,#3677,.T.);
#5515=EDGE_CURVE('',#4253,#4253,#3678,.T.);
#5516=EDGE_CURVE('',#4253,#4254,#1408,.T.);
#5517=EDGE_CURVE('',#4254,#4254,#3679,.T.);
#5518=EDGE_CURVE('',#4255,#4255,#3680,.T.);
#5519=EDGE_CURVE('',#4255,#4256,#1409,.T.);
#5520=EDGE_CURVE('',#4256,#4256,#3681,.T.);
#5521=EDGE_CURVE('',#4257,#4257,#3682,.T.);
#5522=EDGE_CURVE('',#4257,#4258,#1410,.T.);
#5523=EDGE_CURVE('',#4258,#4258,#3683,.T.);
#5524=EDGE_CURVE('',#4259,#4260,#1411,.T.);
#5525=EDGE_CURVE('',#4259,#4261,#1412,.T.);
#5526=EDGE_CURVE('',#4262,#4261,#1413,.T.);
#5527=EDGE_CURVE('',#4260,#4262,#1414,.T.);
#5528=EDGE_CURVE('',#4260,#4263,#1415,.T.);
#5529=EDGE_CURVE('',#4264,#4262,#1416,.T.);
#5530=EDGE_CURVE('',#4263,#4264,#1417,.T.);
#5531=EDGE_CURVE('',#4263,#4265,#1418,.T.);
#5532=EDGE_CURVE('',#4266,#4264,#1419,.T.);
#5533=EDGE_CURVE('',#4265,#4266,#1420,.T.);
#5534=EDGE_CURVE('',#4265,#4267,#1421,.T.);
#5535=EDGE_CURVE('',#4268,#4266,#1422,.T.);
#5536=EDGE_CURVE('',#4267,#4268,#1423,.T.);
#5537=EDGE_CURVE('',#4267,#4269,#1424,.T.);
#5538=EDGE_CURVE('',#4270,#4268,#1425,.T.);
#5539=EDGE_CURVE('',#4269,#4270,#1426,.T.);
#5540=EDGE_CURVE('',#4269,#4271,#1427,.T.);
#5541=EDGE_CURVE('',#4272,#4270,#1428,.T.);
#5542=EDGE_CURVE('',#4271,#4272,#1429,.T.);
#5543=EDGE_CURVE('',#4271,#4273,#1430,.T.);
#5544=EDGE_CURVE('',#4274,#4272,#1431,.T.);
#5545=EDGE_CURVE('',#4273,#4274,#1432,.T.);
#5546=EDGE_CURVE('',#4273,#4259,#1433,.T.);
#5547=EDGE_CURVE('',#4261,#4274,#1434,.T.);
#5548=EDGE_CURVE('',#4275,#4276,#1435,.T.);
#5549=EDGE_CURVE('',#4276,#4277,#1436,.T.);
#5550=EDGE_CURVE('',#4277,#4278,#1437,.T.);
#5551=EDGE_CURVE('',#4275,#4278,#1438,.T.);
#5552=EDGE_CURVE('',#4276,#4279,#1439,.T.);
#5553=EDGE_CURVE('',#4279,#4280,#1440,.T.);
#5554=EDGE_CURVE('',#4280,#4277,#1441,.T.);
#5555=EDGE_CURVE('',#4279,#4281,#1442,.T.);
#5556=EDGE_CURVE('',#4281,#4282,#1443,.T.);
#5557=EDGE_CURVE('',#4282,#4280,#1444,.T.);
#5558=EDGE_CURVE('',#4281,#4283,#1445,.T.);
#5559=EDGE_CURVE('',#4283,#4284,#1446,.T.);
#5560=EDGE_CURVE('',#4284,#4282,#1447,.T.);
#5561=EDGE_CURVE('',#4285,#4284,#1448,.T.);
#5562=EDGE_CURVE('',#4283,#4286,#1449,.T.);
#5563=EDGE_CURVE('',#4286,#4285,#1450,.T.);
#5564=EDGE_CURVE('',#4278,#4285,#1451,.T.);
#5565=EDGE_CURVE('',#4286,#4275,#1452,.T.);
#5566=EDGE_CURVE('',#4287,#4285,#1453,.T.);
#5567=EDGE_CURVE('',#4287,#4288,#1454,.T.);
#5568=EDGE_CURVE('',#4288,#4284,#1455,.T.);
#5569=EDGE_CURVE('',#4289,#4278,#1456,.T.);
#5570=EDGE_CURVE('',#4289,#4287,#1457,.T.);
#5571=EDGE_CURVE('',#4290,#4277,#1458,.T.);
#5572=EDGE_CURVE('',#4290,#4289,#1459,.T.);
#5573=EDGE_CURVE('',#4291,#4291,#3684,.T.);
#5574=EDGE_CURVE('',#4292,#4292,#3685,.T.);
#5575=EDGE_CURVE('',#4293,#4293,#3686,.T.);
#5576=EDGE_CURVE('',#4294,#4294,#3687,.T.);
#5577=EDGE_CURVE('',#4295,#4295,#3688,.T.);
#5578=EDGE_CURVE('',#4295,#4294,#1460,.T.);
#5579=EDGE_CURVE('',#4296,#4296,#3689,.T.);
#5580=EDGE_CURVE('',#4296,#4293,#1461,.T.);
#5581=EDGE_CURVE('',#4297,#4297,#3690,.T.);
#5582=EDGE_CURVE('',#4297,#4292,#1462,.T.);
#5583=EDGE_CURVE('',#4298,#4298,#3691,.T.);
#5584=EDGE_CURVE('',#4298,#4291,#1463,.T.);
#5585=EDGE_CURVE('',#4299,#4280,#1464,.T.);
#5586=EDGE_CURVE('',#4299,#4290,#1465,.T.);
#5587=EDGE_CURVE('',#4300,#4282,#1466,.T.);
#5588=EDGE_CURVE('',#4300,#4299,#1467,.T.);
#5589=EDGE_CURVE('',#4288,#4300,#1468,.T.);
#5590=EDGE_CURVE('',#4301,#4301,#3692,.T.);
#5591=EDGE_CURVE('',#4302,#4303,#3693,.T.);
#5592=EDGE_CURVE('',#4303,#4304,#661,.T.);
#5593=EDGE_CURVE('',#4304,#4305,#662,.T.);
#5594=EDGE_CURVE('',#4305,#4306,#663,.T.);
#5595=EDGE_CURVE('',#4306,#4307,#664,.T.);
#5596=EDGE_CURVE('',#4307,#4308,#665,.T.);
#5597=EDGE_CURVE('',#4308,#4309,#666,.T.);
#5598=EDGE_CURVE('',#4309,#4310,#667,.T.);
#5599=EDGE_CURVE('',#4310,#4311,#668,.T.);
#5600=EDGE_CURVE('',#4311,#4312,#669,.T.);
#5601=EDGE_CURVE('',#4312,#4313,#670,.T.);
#5602=EDGE_CURVE('',#4313,#4314,#671,.T.);
#5603=EDGE_CURVE('',#4314,#4315,#672,.T.);
#5604=EDGE_CURVE('',#4315,#4316,#673,.T.);
#5605=EDGE_CURVE('',#4316,#4317,#674,.T.);
#5606=EDGE_CURVE('',#4317,#4318,#675,.T.);
#5607=EDGE_CURVE('',#4318,#4319,#676,.T.);
#5608=EDGE_CURVE('',#4319,#4320,#677,.T.);
#5609=EDGE_CURVE('',#4320,#4321,#678,.T.);
#5610=EDGE_CURVE('',#4321,#4322,#679,.T.);
#5611=EDGE_CURVE('',#4322,#4323,#680,.T.);
#5612=EDGE_CURVE('',#4323,#4324,#681,.T.);
#5613=EDGE_CURVE('',#4324,#4325,#682,.T.);
#5614=EDGE_CURVE('',#4325,#4326,#683,.T.);
#5615=EDGE_CURVE('',#4326,#4327,#684,.T.);
#5616=EDGE_CURVE('',#4327,#4328,#685,.T.);
#5617=EDGE_CURVE('',#4328,#4329,#686,.T.);
#5618=EDGE_CURVE('',#4329,#4330,#687,.T.);
#5619=EDGE_CURVE('',#4330,#4331,#688,.T.);
#5620=EDGE_CURVE('',#4331,#4332,#689,.T.);
#5621=EDGE_CURVE('',#4332,#4333,#690,.T.);
#5622=EDGE_CURVE('',#4333,#4334,#691,.T.);
#5623=EDGE_CURVE('',#4334,#4335,#692,.T.);
#5624=EDGE_CURVE('',#4335,#4336,#693,.T.);
#5625=EDGE_CURVE('',#4336,#4337,#694,.T.);
#5626=EDGE_CURVE('',#4337,#4338,#695,.T.);
#5627=EDGE_CURVE('',#4338,#4339,#696,.T.);
#5628=EDGE_CURVE('',#4339,#4340,#697,.T.);
#5629=EDGE_CURVE('',#4340,#4341,#698,.T.);
#5630=EDGE_CURVE('',#4341,#4342,#699,.T.);
#5631=EDGE_CURVE('',#4342,#4343,#700,.T.);
#5632=EDGE_CURVE('',#4343,#4344,#701,.T.);
#5633=EDGE_CURVE('',#4344,#4345,#702,.T.);
#5634=EDGE_CURVE('',#4345,#4346,#703,.T.);
#5635=EDGE_CURVE('',#4346,#4347,#704,.T.);
#5636=EDGE_CURVE('',#4347,#4348,#705,.T.);
#5637=EDGE_CURVE('',#4348,#4349,#706,.T.);
#5638=EDGE_CURVE('',#4349,#4350,#707,.T.);
#5639=EDGE_CURVE('',#4350,#4351,#708,.T.);
#5640=EDGE_CURVE('',#4351,#4352,#709,.T.);
#5641=EDGE_CURVE('',#4352,#4353,#710,.T.);
#5642=EDGE_CURVE('',#4353,#4354,#711,.T.);
#5643=EDGE_CURVE('',#4354,#4355,#712,.T.);
#5644=EDGE_CURVE('',#4355,#4356,#713,.T.);
#5645=EDGE_CURVE('',#4356,#4357,#714,.T.);
#5646=EDGE_CURVE('',#4357,#4358,#715,.T.);
#5647=EDGE_CURVE('',#4358,#4359,#716,.T.);
#5648=EDGE_CURVE('',#4359,#4360,#717,.T.);
#5649=EDGE_CURVE('',#4360,#4361,#718,.T.);
#5650=EDGE_CURVE('',#4361,#4362,#719,.T.);
#5651=EDGE_CURVE('',#4362,#4363,#720,.T.);
#5652=EDGE_CURVE('',#4363,#4364,#721,.T.);
#5653=EDGE_CURVE('',#4364,#4365,#722,.T.);
#5654=EDGE_CURVE('',#4365,#4366,#723,.T.);
#5655=EDGE_CURVE('',#4366,#4367,#724,.T.);
#5656=EDGE_CURVE('',#4367,#4368,#725,.T.);
#5657=EDGE_CURVE('',#4368,#4369,#726,.T.);
#5658=EDGE_CURVE('',#4369,#4370,#727,.T.);
#5659=EDGE_CURVE('',#4370,#4371,#728,.T.);
#5660=EDGE_CURVE('',#4371,#4372,#729,.T.);
#5661=EDGE_CURVE('',#4372,#4373,#730,.T.);
#5662=EDGE_CURVE('',#4373,#4374,#731,.T.);
#5663=EDGE_CURVE('',#4374,#4375,#732,.T.);
#5664=EDGE_CURVE('',#4375,#4376,#733,.T.);
#5665=EDGE_CURVE('',#4376,#4377,#734,.T.);
#5666=EDGE_CURVE('',#4377,#4378,#3694,.T.);
#5667=EDGE_CURVE('',#4378,#4379,#735,.T.);
#5668=EDGE_CURVE('',#4379,#4380,#736,.T.);
#5669=EDGE_CURVE('',#4380,#4381,#737,.T.);
#5670=EDGE_CURVE('',#4381,#4382,#738,.T.);
#5671=EDGE_CURVE('',#4382,#4383,#739,.T.);
#5672=EDGE_CURVE('',#4383,#4384,#740,.T.);
#5673=EDGE_CURVE('',#4384,#4385,#741,.T.);
#5674=EDGE_CURVE('',#4385,#4386,#742,.T.);
#5675=EDGE_CURVE('',#4386,#4387,#743,.T.);
#5676=EDGE_CURVE('',#4387,#4388,#744,.T.);
#5677=EDGE_CURVE('',#4388,#4389,#745,.T.);
#5678=EDGE_CURVE('',#4389,#4390,#746,.T.);
#5679=EDGE_CURVE('',#4390,#4391,#747,.T.);
#5680=EDGE_CURVE('',#4391,#4392,#748,.T.);
#5681=EDGE_CURVE('',#4392,#4393,#749,.T.);
#5682=EDGE_CURVE('',#4393,#4394,#750,.T.);
#5683=EDGE_CURVE('',#4394,#4395,#751,.T.);
#5684=EDGE_CURVE('',#4395,#4396,#752,.T.);
#5685=EDGE_CURVE('',#4396,#4397,#753,.T.);
#5686=EDGE_CURVE('',#4397,#4398,#754,.T.);
#5687=EDGE_CURVE('',#4398,#4399,#755,.T.);
#5688=EDGE_CURVE('',#4399,#4400,#756,.T.);
#5689=EDGE_CURVE('',#4400,#4401,#757,.T.);
#5690=EDGE_CURVE('',#4401,#4402,#758,.T.);
#5691=EDGE_CURVE('',#4402,#4403,#759,.T.);
#5692=EDGE_CURVE('',#4403,#4404,#760,.T.);
#5693=EDGE_CURVE('',#4404,#4405,#761,.T.);
#5694=EDGE_CURVE('',#4405,#4406,#762,.T.);
#5695=EDGE_CURVE('',#4406,#4407,#763,.T.);
#5696=EDGE_CURVE('',#4407,#4408,#764,.T.);
#5697=EDGE_CURVE('',#4408,#4409,#765,.T.);
#5698=EDGE_CURVE('',#4409,#4410,#766,.T.);
#5699=EDGE_CURVE('',#4410,#4411,#767,.T.);
#5700=EDGE_CURVE('',#4411,#4412,#768,.T.);
#5701=EDGE_CURVE('',#4412,#4413,#769,.T.);
#5702=EDGE_CURVE('',#4413,#4414,#770,.T.);
#5703=EDGE_CURVE('',#4414,#4415,#771,.T.);
#5704=EDGE_CURVE('',#4415,#4416,#772,.T.);
#5705=EDGE_CURVE('',#4416,#4417,#773,.T.);
#5706=EDGE_CURVE('',#4417,#4418,#774,.T.);
#5707=EDGE_CURVE('',#4418,#4419,#775,.T.);
#5708=EDGE_CURVE('',#4419,#4420,#776,.T.);
#5709=EDGE_CURVE('',#4420,#4421,#777,.T.);
#5710=EDGE_CURVE('',#4421,#4422,#778,.T.);
#5711=EDGE_CURVE('',#4422,#4423,#779,.T.);
#5712=EDGE_CURVE('',#4423,#4424,#780,.T.);
#5713=EDGE_CURVE('',#4424,#4425,#781,.T.);
#5714=EDGE_CURVE('',#4425,#4426,#782,.T.);
#5715=EDGE_CURVE('',#4426,#4427,#783,.T.);
#5716=EDGE_CURVE('',#4427,#4428,#784,.T.);
#5717=EDGE_CURVE('',#4428,#4429,#785,.T.);
#5718=EDGE_CURVE('',#4429,#4430,#786,.T.);
#5719=EDGE_CURVE('',#4430,#4431,#787,.T.);
#5720=EDGE_CURVE('',#4431,#4432,#788,.T.);
#5721=EDGE_CURVE('',#4432,#4433,#789,.T.);
#5722=EDGE_CURVE('',#4433,#4434,#790,.T.);
#5723=EDGE_CURVE('',#4434,#4435,#791,.T.);
#5724=EDGE_CURVE('',#4435,#4436,#792,.T.);
#5725=EDGE_CURVE('',#4436,#4437,#793,.T.);
#5726=EDGE_CURVE('',#4437,#4438,#794,.T.);
#5727=EDGE_CURVE('',#4438,#4439,#795,.T.);
#5728=EDGE_CURVE('',#4439,#4440,#796,.T.);
#5729=EDGE_CURVE('',#4440,#4441,#797,.T.);
#5730=EDGE_CURVE('',#4441,#4442,#798,.T.);
#5731=EDGE_CURVE('',#4442,#4443,#799,.T.);
#5732=EDGE_CURVE('',#4443,#4444,#800,.T.);
#5733=EDGE_CURVE('',#4444,#4445,#801,.T.);
#5734=EDGE_CURVE('',#4445,#4446,#802,.T.);
#5735=EDGE_CURVE('',#4446,#4447,#803,.T.);
#5736=EDGE_CURVE('',#4447,#4448,#804,.T.);
#5737=EDGE_CURVE('',#4448,#4449,#805,.T.);
#5738=EDGE_CURVE('',#4449,#4450,#806,.T.);
#5739=EDGE_CURVE('',#4450,#4451,#807,.T.);
#5740=EDGE_CURVE('',#4451,#4302,#808,.T.);
#5741=EDGE_CURVE('',#4452,#4452,#3695,.F.);
#5742=EDGE_CURVE('',#4453,#4454,#809,.T.);
#5743=EDGE_CURVE('',#4455,#4454,#3696,.T.);
#5744=EDGE_CURVE('',#4456,#4455,#810,.T.);
#5745=EDGE_CURVE('',#4457,#4456,#811,.F.);
#5746=EDGE_CURVE('',#4458,#4457,#812,.T.);
#5747=EDGE_CURVE('',#4459,#4458,#813,.F.);
#5748=EDGE_CURVE('',#4460,#4459,#814,.T.);
#5749=EDGE_CURVE('',#4461,#4460,#815,.F.);
#5750=EDGE_CURVE('',#4462,#4461,#816,.F.);
#5751=EDGE_CURVE('',#4463,#4462,#817,.F.);
#5752=EDGE_CURVE('',#4464,#4463,#818,.F.);
#5753=EDGE_CURVE('',#4465,#4464,#819,.F.);
#5754=EDGE_CURVE('',#4466,#4465,#820,.F.);
#5755=EDGE_CURVE('',#4467,#4466,#821,.F.);
#5756=EDGE_CURVE('',#4468,#4467,#822,.F.);
#5757=EDGE_CURVE('',#4469,#4468,#823,.T.);
#5758=EDGE_CURVE('',#4470,#4469,#824,.F.);
#5759=EDGE_CURVE('',#4471,#4470,#825,.F.);
#5760=EDGE_CURVE('',#4472,#4471,#826,.F.);
#5761=EDGE_CURVE('',#4473,#4472,#827,.F.);
#5762=EDGE_CURVE('',#4474,#4473,#828,.F.);
#5763=EDGE_CURVE('',#4475,#4474,#829,.F.);
#5764=EDGE_CURVE('',#4476,#4475,#830,.F.);
#5765=EDGE_CURVE('',#4477,#4476,#831,.F.);
#5766=EDGE_CURVE('',#4478,#4477,#832,.T.);
#5767=EDGE_CURVE('',#4479,#4478,#833,.F.);
#5768=EDGE_CURVE('',#4480,#4479,#834,.F.);
#5769=EDGE_CURVE('',#4481,#4480,#835,.F.);
#5770=EDGE_CURVE('',#4482,#4481,#836,.F.);
#5771=EDGE_CURVE('',#4483,#4482,#837,.F.);
#5772=EDGE_CURVE('',#4484,#4483,#838,.F.);
#5773=EDGE_CURVE('',#4485,#4484,#839,.F.);
#5774=EDGE_CURVE('',#4486,#4485,#840,.F.);
#5775=EDGE_CURVE('',#4487,#4486,#841,.T.);
#5776=EDGE_CURVE('',#4488,#4487,#842,.F.);
#5777=EDGE_CURVE('',#4489,#4488,#843,.F.);
#5778=EDGE_CURVE('',#4490,#4489,#844,.F.);
#5779=EDGE_CURVE('',#4491,#4490,#845,.F.);
#5780=EDGE_CURVE('',#4492,#4491,#846,.F.);
#5781=EDGE_CURVE('',#4493,#4492,#847,.F.);
#5782=EDGE_CURVE('',#4494,#4493,#848,.F.);
#5783=EDGE_CURVE('',#4495,#4494,#849,.T.);
#5784=EDGE_CURVE('',#4496,#4495,#3697,.T.);
#5785=EDGE_CURVE('',#4496,#4497,#850,.T.);
#5786=EDGE_CURVE('',#4497,#4498,#851,.T.);
#5787=EDGE_CURVE('',#4498,#4499,#852,.T.);
#5788=EDGE_CURVE('',#4499,#4500,#853,.T.);
#5789=EDGE_CURVE('',#4500,#4501,#854,.T.);
#5790=EDGE_CURVE('',#4501,#4502,#855,.T.);
#5791=EDGE_CURVE('',#4502,#4503,#856,.T.);
#5792=EDGE_CURVE('',#4503,#4504,#857,.T.);
#5793=EDGE_CURVE('',#4504,#4505,#858,.T.);
#5794=EDGE_CURVE('',#4505,#4506,#859,.T.);
#5795=EDGE_CURVE('',#4506,#4507,#860,.T.);
#5796=EDGE_CURVE('',#4507,#4508,#861,.T.);
#5797=EDGE_CURVE('',#4508,#4509,#862,.T.);
#5798=EDGE_CURVE('',#4509,#4510,#863,.T.);
#5799=EDGE_CURVE('',#4510,#4511,#864,.T.);
#5800=EDGE_CURVE('',#4511,#4512,#865,.T.);
#5801=EDGE_CURVE('',#4512,#4513,#866,.T.);
#5802=EDGE_CURVE('',#4513,#4514,#867,.T.);
#5803=EDGE_CURVE('',#4514,#4515,#868,.T.);
#5804=EDGE_CURVE('',#4515,#4516,#869,.T.);
#5805=EDGE_CURVE('',#4516,#4517,#870,.T.);
#5806=EDGE_CURVE('',#4517,#4518,#871,.T.);
#5807=EDGE_CURVE('',#4518,#4519,#872,.T.);
#5808=EDGE_CURVE('',#4519,#4520,#873,.T.);
#5809=EDGE_CURVE('',#4520,#4521,#874,.T.);
#5810=EDGE_CURVE('',#4521,#4522,#875,.T.);
#5811=EDGE_CURVE('',#4522,#4523,#876,.T.);
#5812=EDGE_CURVE('',#4523,#4524,#877,.T.);
#5813=EDGE_CURVE('',#4524,#4525,#878,.T.);
#5814=EDGE_CURVE('',#4525,#4526,#879,.T.);
#5815=EDGE_CURVE('',#4526,#4527,#880,.T.);
#5816=EDGE_CURVE('',#4527,#4528,#881,.T.);
#5817=EDGE_CURVE('',#4528,#4529,#882,.T.);
#5818=EDGE_CURVE('',#4529,#4530,#883,.T.);
#5819=EDGE_CURVE('',#4530,#4531,#884,.T.);
#5820=EDGE_CURVE('',#4531,#4532,#885,.T.);
#5821=EDGE_CURVE('',#4532,#4533,#886,.T.);
#5822=EDGE_CURVE('',#4533,#4534,#887,.T.);
#5823=EDGE_CURVE('',#4534,#4535,#888,.T.);
#5824=EDGE_CURVE('',#4535,#4453,#889,.T.);
#5825=EDGE_CURVE('',#4536,#4537,#1469,.T.);
#5826=EDGE_CURVE('',#4536,#4538,#1470,.T.);
#5827=EDGE_CURVE('',#4538,#4539,#1471,.T.);
#5828=EDGE_CURVE('',#4537,#4539,#1472,.T.);
#5829=EDGE_CURVE('',#4540,#4536,#1473,.T.);
#5830=EDGE_CURVE('',#4540,#4541,#1474,.T.);
#5831=EDGE_CURVE('',#4541,#4538,#1475,.T.);
#5832=EDGE_CURVE('',#4542,#4540,#1476,.T.);
#5833=EDGE_CURVE('',#4542,#4543,#1477,.T.);
#5834=EDGE_CURVE('',#4543,#4541,#1478,.T.);
#5835=EDGE_CURVE('',#4544,#4542,#1479,.T.);
#5836=EDGE_CURVE('',#4544,#4545,#1480,.T.);
#5837=EDGE_CURVE('',#4545,#4543,#1481,.T.);
#5838=EDGE_CURVE('',#4546,#4544,#1482,.T.);
#5839=EDGE_CURVE('',#4546,#4547,#1483,.T.);
#5840=EDGE_CURVE('',#4547,#4545,#1484,.T.);
#5841=EDGE_CURVE('',#4537,#4546,#1485,.T.);
#5842=EDGE_CURVE('',#4539,#4547,#1486,.T.);
#5843=EDGE_CURVE('',#4302,#4455,#890,.T.);
#5844=EDGE_CURVE('',#4454,#4548,#891,.T.);
#5845=EDGE_CURVE('',#4548,#4303,#892,.T.);
#5846=EDGE_CURVE('',#4495,#4378,#893,.T.);
#5847=EDGE_CURVE('',#4377,#4496,#894,.T.);
#5848=EDGE_CURVE('',#4549,#4549,#3698,.T.);
#5849=EDGE_CURVE('',#4301,#4549,#1487,.T.);
#5850=EDGE_CURVE('',#4452,#4550,#1488,.T.);
#5851=EDGE_CURVE('',#4550,#4550,#3699,.T.);
#5852=EDGE_CURVE('',#4551,#4552,#3700,.T.);
#5853=EDGE_CURVE('',#4552,#4553,#1489,.T.);
#5854=EDGE_CURVE('',#4553,#4554,#3701,.T.);
#5855=EDGE_CURVE('',#4554,#4555,#1490,.T.);
#5856=EDGE_CURVE('',#4555,#4551,#3702,.F.);
#5857=EDGE_CURVE('',#4551,#4556,#3703,.T.);
#5858=EDGE_CURVE('',#4556,#4552,#1491,.T.);
#5859=EDGE_CURVE('',#4557,#4558,#3704,.T.);
#5860=EDGE_CURVE('',#4559,#4558,#3705,.T.);
#5861=EDGE_CURVE('',#4559,#4560,#1492,.T.);
#5862=EDGE_CURVE('',#4560,#4561,#3706,.T.);
#5863=EDGE_CURVE('',#4561,#4557,#1493,.T.);
#5864=EDGE_CURVE('',#4554,#4560,#1494,.T.);
#5865=EDGE_CURVE('',#4555,#4559,#1495,.T.);
#5866=EDGE_CURVE('',#4562,#4563,#3707,.T.);
#5867=EDGE_CURVE('',#4563,#4564,#1496,.T.);
#5868=EDGE_CURVE('',#4564,#4565,#3708,.T.);
#5869=EDGE_CURVE('',#4565,#4566,#1497,.T.);
#5870=EDGE_CURVE('',#4566,#4562,#3709,.F.);
#5871=EDGE_CURVE('',#4562,#4567,#3710,.T.);
#5872=EDGE_CURVE('',#4567,#4563,#1498,.T.);
#5873=EDGE_CURVE('',#4568,#4569,#3711,.T.);
#5874=EDGE_CURVE('',#4570,#4569,#3712,.T.);
#5875=EDGE_CURVE('',#4570,#4571,#1499,.T.);
#5876=EDGE_CURVE('',#4571,#4572,#3713,.T.);
#5877=EDGE_CURVE('',#4572,#4568,#1500,.T.);
#5878=EDGE_CURVE('',#4565,#4571,#1501,.T.);
#5879=EDGE_CURVE('',#4566,#4570,#1502,.T.);
#5880=EDGE_CURVE('',#4573,#4574,#1503,.T.);
#5881=EDGE_CURVE('',#4574,#4575,#1504,.T.);
#5882=EDGE_CURVE('',#4575,#4576,#1505,.T.);
#5883=EDGE_CURVE('',#4576,#4573,#1506,.T.);
#5884=EDGE_CURVE('',#4573,#4577,#1507,.T.);
#5885=EDGE_CURVE('',#4577,#4578,#1508,.T.);
#5886=EDGE_CURVE('',#4574,#4578,#1509,.T.);
#5887=EDGE_CURVE('',#4576,#4579,#1510,.T.);
#5888=EDGE_CURVE('',#4579,#4577,#1511,.T.);
#5889=EDGE_CURVE('',#4575,#4580,#1512,.T.);
#5890=EDGE_CURVE('',#4580,#4579,#1513,.T.);
#5891=EDGE_CURVE('',#4578,#4580,#1514,.T.);
#5892=EDGE_CURVE('',#4581,#4581,#3714,.T.);
#5893=EDGE_CURVE('',#4581,#4582,#1515,.T.);
#5894=EDGE_CURVE('',#4583,#4582,#895,.T.);
#5895=EDGE_CURVE('',#4584,#4583,#896,.T.);
#5896=EDGE_CURVE('',#4582,#4584,#897,.T.);
#5897=EDGE_CURVE('',#4585,#4586,#898,.T.);
#5898=EDGE_CURVE('',#4586,#4585,#899,.T.);
#5899=EDGE_CURVE('',#4586,#4587,#1516,.T.);
#5900=EDGE_CURVE('',#4587,#4587,#3715,.T.);
#5901=EDGE_CURVE('',#4588,#4588,#3716,.T.);
#5902=EDGE_CURVE('',#4588,#4589,#1517,.T.);
#5903=EDGE_CURVE('',#4590,#4589,#900,.T.);
#5904=EDGE_CURVE('',#4591,#4590,#901,.T.);
#5905=EDGE_CURVE('',#4589,#4591,#902,.T.);
#5906=EDGE_CURVE('',#4592,#4593,#903,.T.);
#5907=EDGE_CURVE('',#4593,#4592,#904,.T.);
#5908=EDGE_CURVE('',#4593,#4594,#1518,.T.);
#5909=EDGE_CURVE('',#4594,#4594,#3717,.T.);
#5910=EDGE_CURVE('',#4595,#4595,#3718,.T.);
#5911=EDGE_CURVE('',#4595,#4589,#1519,.T.);
#5912=EDGE_CURVE('',#4591,#4582,#1520,.T.);
#5913=EDGE_CURVE('',#4584,#4596,#1521,.T.);
#5914=EDGE_CURVE('',#4596,#4596,#3719,.T.);
#5915=EDGE_CURVE('',#4597,#4556,#1522,.T.);
#5916=EDGE_CURVE('',#4598,#4556,#3720,.T.);
#5917=EDGE_CURVE('',#4597,#4598,#3721,.T.);
#5918=EDGE_CURVE('',#4558,#4551,#3722,.T.);
#5919=EDGE_CURVE('',#4599,#4567,#1523,.T.);
#5920=EDGE_CURVE('',#4599,#4567,#3723,.T.);
#5921=EDGE_CURVE('',#4569,#4562,#3724,.T.);
#5922=EDGE_CURVE('',#4600,#4600,#3725,.T.);
#5923=EDGE_CURVE('',#4600,#4598,#1524,.T.);
#5924=EDGE_CURVE('',#4599,#4558,#3726,.T.);
#5925=EDGE_CURVE('',#4597,#4569,#3727,.T.);
#5926=EDGE_CURVE('',#4557,#4599,#1525,.T.);
#5927=EDGE_CURVE('',#4568,#4597,#1526,.T.);
#5928=EDGE_CURVE('',#4561,#4564,#1527,.T.);
#5929=EDGE_CURVE('',#4572,#4553,#1528,.T.);
#5930=EDGE_CURVE('',#4601,#4601,#905,.T.);
#5931=EDGE_CURVE('',#4601,#4602,#906,.T.);
#5932=EDGE_CURVE('',#4602,#4602,#907,.T.);
#5933=EDGE_CURVE('',#4603,#4603,#3728,.T.);
#5934=EDGE_CURVE('',#4603,#4604,#1529,.T.);
#5935=EDGE_CURVE('',#4604,#4604,#3729,.T.);
#5936=EDGE_CURVE('',#4603,#4605,#1530,.T.);
#5937=EDGE_CURVE('',#4605,#4605,#3730,.T.);
#5938=EDGE_CURVE('',#4606,#4606,#3731,.T.);
#5939=EDGE_CURVE('',#4607,#4607,#3732,.T.);
#5940=EDGE_CURVE('',#4607,#4606,#1531,.T.);
#5941=EDGE_CURVE('',#4608,#4608,#3733,.T.);
#5942=EDGE_CURVE('',#4609,#4609,#3734,.T.);
#5943=EDGE_CURVE('',#4609,#4608,#1532,.T.);
#5944=EDGE_CURVE('',#4610,#4610,#3735,.T.);
#5945=EDGE_CURVE('',#4611,#4611,#3736,.T.);
#5946=EDGE_CURVE('',#4611,#4610,#1533,.T.);
#5947=EDGE_CURVE('',#4612,#4612,#3737,.T.);
#5948=EDGE_CURVE('',#4612,#4611,#1534,.T.);
#5949=EDGE_CURVE('',#4612,#4613,#1535,.T.);
#5950=EDGE_CURVE('',#4613,#4613,#3738,.T.);
#5951=EDGE_CURVE('',#4614,#4614,#3739,.T.);
#5952=EDGE_CURVE('',#4615,#4615,#3740,.T.);
#5953=EDGE_CURVE('',#4615,#4614,#1536,.T.);
#5954=EDGE_CURVE('',#4616,#4616,#3741,.T.);
#5955=EDGE_CURVE('',#4617,#4617,#3742,.T.);
#5956=EDGE_CURVE('',#4617,#4616,#1537,.T.);
#5957=EDGE_CURVE('',#4618,#4618,#3743,.T.);
#5958=EDGE_CURVE('',#4604,#4618,#1538,.T.);
#5959=EDGE_CURVE('',#4619,#4620,#1539,.T.);
#5960=EDGE_CURVE('',#4619,#4621,#1540,.T.);
#5961=EDGE_CURVE('',#4622,#4621,#1541,.T.);
#5962=EDGE_CURVE('',#4623,#4622,#1542,.T.);
#5963=EDGE_CURVE('',#4620,#4623,#131,.T.);
#5964=EDGE_CURVE('',#4624,#4625,#1543,.T.);
#5965=EDGE_CURVE('',#4626,#4624,#132,.T.);
#5966=EDGE_CURVE('',#4627,#4626,#1544,.T.);
#5967=EDGE_CURVE('',#4627,#4628,#1545,.T.);
#5968=EDGE_CURVE('',#4628,#4625,#1546,.T.);
#5969=EDGE_CURVE('',#4622,#4627,#1547,.T.);
#5970=EDGE_CURVE('',#4621,#4628,#1548,.T.);
#5971=EDGE_CURVE('',#4625,#4619,#3744,.T.);
#5972=EDGE_CURVE('',#4626,#4629,#3745,.T.);
#5973=EDGE_CURVE('',#4629,#4630,#1549,.T.);
#5974=EDGE_CURVE('',#4630,#4631,#1550,.T.);
#5975=EDGE_CURVE('',#4631,#4632,#1551,.T.);
#5976=EDGE_CURVE('',#4632,#4633,#3746,.T.);
#5977=EDGE_CURVE('',#4633,#4634,#1552,.T.);
#5978=EDGE_CURVE('',#4634,#4635,#1553,.T.);
#5979=EDGE_CURVE('',#4635,#4636,#1554,.T.);
#5980=EDGE_CURVE('',#4636,#4637,#3747,.T.);
#5981=EDGE_CURVE('',#4637,#4638,#1555,.T.);
#5982=EDGE_CURVE('',#4638,#4639,#1556,.T.);
#5983=EDGE_CURVE('',#4639,#4640,#1557,.T.);
#5984=EDGE_CURVE('',#4640,#4641,#3748,.T.);
#5985=EDGE_CURVE('',#4641,#4642,#1558,.T.);
#5986=EDGE_CURVE('',#4642,#4643,#1559,.T.);
#5987=EDGE_CURVE('',#4643,#4644,#1560,.T.);
#5988=EDGE_CURVE('',#4644,#4645,#3749,.T.);
#5989=EDGE_CURVE('',#4645,#4646,#1561,.T.);
#5990=EDGE_CURVE('',#4646,#4647,#1562,.T.);
#5991=EDGE_CURVE('',#4647,#4648,#1563,.T.);
#5992=EDGE_CURVE('',#4648,#4649,#3750,.T.);
#5993=EDGE_CURVE('',#4649,#4650,#1564,.T.);
#5994=EDGE_CURVE('',#4650,#4651,#1565,.T.);
#5995=EDGE_CURVE('',#4651,#4652,#1566,.T.);
#5996=EDGE_CURVE('',#4652,#4653,#3751,.T.);
#5997=EDGE_CURVE('',#4653,#4654,#1567,.T.);
#5998=EDGE_CURVE('',#4654,#4655,#1568,.T.);
#5999=EDGE_CURVE('',#4655,#4656,#1569,.T.);
#6000=EDGE_CURVE('',#4656,#4623,#3752,.T.);
#6001=EDGE_CURVE('',#4657,#4657,#3753,.T.);
#6002=EDGE_CURVE('',#4624,#4658,#3754,.T.);
#6003=EDGE_CURVE('',#4658,#4629,#133,.T.);
#6004=EDGE_CURVE('',#4656,#4659,#134,.T.);
#6005=EDGE_CURVE('',#4659,#4620,#3755,.T.);
#6006=EDGE_CURVE('',#4660,#4661,#1570,.T.);
#6007=EDGE_CURVE('',#4660,#4662,#1571,.T.);
#6008=EDGE_CURVE('',#4654,#4662,#1572,.T.);
#6009=EDGE_CURVE('',#4661,#4653,#135,.T.);
#6010=EDGE_CURVE('',#4659,#4663,#1573,.T.);
#6011=EDGE_CURVE('',#4655,#4664,#1574,.T.);
#6012=EDGE_CURVE('',#4664,#4663,#1575,.T.);
#6013=EDGE_CURVE('',#4662,#4664,#1576,.T.);
#6014=EDGE_CURVE('',#4663,#4660,#3756,.T.);
#6015=EDGE_CURVE('',#4652,#4665,#136,.T.);
#6016=EDGE_CURVE('',#4665,#4661,#3757,.T.);
#6017=EDGE_CURVE('',#4666,#4667,#1577,.T.);
#6018=EDGE_CURVE('',#4666,#4668,#1578,.T.);
#6019=EDGE_CURVE('',#4650,#4668,#1579,.T.);
#6020=EDGE_CURVE('',#4667,#4649,#137,.T.);
#6021=EDGE_CURVE('',#4665,#4669,#1580,.T.);
#6022=EDGE_CURVE('',#4651,#4670,#1581,.T.);
#6023=EDGE_CURVE('',#4670,#4669,#1582,.T.);
#6024=EDGE_CURVE('',#4668,#4670,#1583,.T.);
#6025=EDGE_CURVE('',#4669,#4666,#3758,.T.);
#6026=EDGE_CURVE('',#4648,#4671,#138,.T.);
#6027=EDGE_CURVE('',#4671,#4667,#3759,.T.);
#6028=EDGE_CURVE('',#4672,#4673,#1584,.T.);
#6029=EDGE_CURVE('',#4672,#4674,#1585,.T.);
#6030=EDGE_CURVE('',#4646,#4674,#1586,.T.);
#6031=EDGE_CURVE('',#4673,#4645,#139,.T.);
#6032=EDGE_CURVE('',#4671,#4675,#1587,.T.);
#6033=EDGE_CURVE('',#4647,#4676,#1588,.T.);
#6034=EDGE_CURVE('',#4676,#4675,#1589,.T.);
#6035=EDGE_CURVE('',#4674,#4676,#1590,.T.);
#6036=EDGE_CURVE('',#4675,#4677,#3760,.T.);
#6037=EDGE_CURVE('',#4677,#4672,#3761,.T.);
#6038=EDGE_CURVE('',#4644,#4678,#140,.T.);
#6039=EDGE_CURVE('',#4678,#4673,#3762,.T.);
#6040=EDGE_CURVE('',#4679,#4680,#1591,.T.);
#6041=EDGE_CURVE('',#4679,#4681,#1592,.T.);
#6042=EDGE_CURVE('',#4642,#4681,#1593,.T.);
#6043=EDGE_CURVE('',#4680,#4641,#141,.T.);
#6044=EDGE_CURVE('',#4678,#4682,#1594,.T.);
#6045=EDGE_CURVE('',#4643,#4683,#1595,.T.);
#6046=EDGE_CURVE('',#4683,#4682,#1596,.T.);
#6047=EDGE_CURVE('',#4681,#4683,#1597,.T.);
#6048=EDGE_CURVE('',#4682,#4679,#3763,.T.);
#6049=EDGE_CURVE('',#4640,#4684,#142,.T.);
#6050=EDGE_CURVE('',#4684,#4680,#3764,.T.);
#6051=EDGE_CURVE('',#4685,#4686,#1598,.T.);
#6052=EDGE_CURVE('',#4685,#4687,#1599,.T.);
#6053=EDGE_CURVE('',#4638,#4687,#1600,.T.);
#6054=EDGE_CURVE('',#4686,#4637,#143,.T.);
#6055=EDGE_CURVE('',#4684,#4688,#1601,.T.);
#6056=EDGE_CURVE('',#4639,#4689,#1602,.T.);
#6057=EDGE_CURVE('',#4689,#4688,#1603,.T.);
#6058=EDGE_CURVE('',#4687,#4689,#1604,.T.);
#6059=EDGE_CURVE('',#4688,#4685,#3765,.T.);
#6060=EDGE_CURVE('',#4636,#4690,#144,.T.);
#6061=EDGE_CURVE('',#4690,#4686,#3766,.T.);
#6062=EDGE_CURVE('',#4635,#4691,#1605,.T.);
#6063=EDGE_CURVE('',#4691,#4692,#1606,.T.);
#6064=EDGE_CURVE('',#4690,#4692,#1607,.T.);
#6065=EDGE_CURVE('',#4693,#4633,#145,.T.);
#6066=EDGE_CURVE('',#4694,#4693,#1608,.T.);
#6067=EDGE_CURVE('',#4694,#4695,#1609,.T.);
#6068=EDGE_CURVE('',#4634,#4695,#1610,.T.);
#6069=EDGE_CURVE('',#4695,#4691,#1611,.T.);
#6070=EDGE_CURVE('',#4692,#4694,#3767,.T.);
#6071=EDGE_CURVE('',#4632,#4696,#146,.T.);
#6072=EDGE_CURVE('',#4696,#4693,#3768,.T.);
#6073=EDGE_CURVE('',#4631,#4697,#1612,.T.);
#6074=EDGE_CURVE('',#4697,#4698,#1613,.T.);
#6075=EDGE_CURVE('',#4696,#4698,#1614,.T.);
#6076=EDGE_CURVE('',#4699,#4658,#1615,.T.);
#6077=EDGE_CURVE('',#4699,#4700,#1616,.T.);
#6078=EDGE_CURVE('',#4630,#4700,#1617,.T.);
#6079=EDGE_CURVE('',#4700,#4697,#1618,.T.);
#6080=EDGE_CURVE('',#4698,#4699,#3769,.T.);
#6081=EDGE_CURVE('',#4701,#4701,#3770,.T.);
#6082=EDGE_CURVE('',#4701,#4702,#1619,.T.);
#6083=EDGE_CURVE('',#4702,#4702,#3771,.T.);
#6084=EDGE_CURVE('',#4703,#4703,#3772,.T.);
#6085=EDGE_CURVE('',#4703,#4704,#1620,.T.);
#6086=EDGE_CURVE('',#4704,#4704,#3773,.T.);
#6087=EDGE_CURVE('',#4705,#4705,#3774,.T.);
#6088=EDGE_CURVE('',#4677,#4705,#1621,.T.);
#6089=EDGE_CURVE('',#4706,#4706,#3775,.T.);
#6090=EDGE_CURVE('',#4706,#4657,#1622,.T.);
#6091=EDGE_CURVE('',#4707,#4708,#1623,.T.);
#6092=EDGE_CURVE('',#4707,#4709,#1624,.T.);
#6093=EDGE_CURVE('',#4709,#4710,#1625,.T.);
#6094=EDGE_CURVE('',#4708,#4710,#1626,.T.);
#6095=EDGE_CURVE('',#4711,#4712,#1627,.T.);
#6096=EDGE_CURVE('',#4713,#4711,#1628,.T.);
#6097=EDGE_CURVE('',#4714,#4713,#1629,.T.);
#6098=EDGE_CURVE('',#4714,#4712,#1630,.T.);
#6099=EDGE_CURVE('',#4709,#4714,#1631,.T.);
#6100=EDGE_CURVE('',#4710,#4713,#1632,.T.);
#6101=EDGE_CURVE('',#4711,#4708,#3776,.T.);
#6102=EDGE_CURVE('',#4715,#4715,#3777,.T.);
#6103=EDGE_CURVE('',#4716,#4716,#3778,.T.);
#6104=EDGE_CURVE('',#4716,#4715,#1633,.T.);
#6105=EDGE_CURVE('',#4712,#4707,#3779,.T.);
#6106=EDGE_CURVE('',#4717,#4717,#3780,.T.);
#6107=EDGE_CURVE('',#4717,#4718,#1634,.T.);
#6108=EDGE_CURVE('',#4718,#4718,#3781,.T.);
#6109=EDGE_CURVE('',#4717,#4719,#1635,.T.);
#6110=EDGE_CURVE('',#4719,#4719,#3782,.T.);
#6111=EDGE_CURVE('',#4720,#4720,#3783,.T.);
#6112=EDGE_CURVE('',#4721,#4721,#3784,.T.);
#6113=EDGE_CURVE('',#4721,#4720,#1636,.T.);
#6114=EDGE_CURVE('',#4722,#4722,#3785,.T.);
#6115=EDGE_CURVE('',#4723,#4723,#3786,.T.);
#6116=EDGE_CURVE('',#4723,#4722,#1637,.T.);
#6117=EDGE_CURVE('',#4724,#4724,#3787,.T.);
#6118=EDGE_CURVE('',#4725,#4725,#3788,.T.);
#6119=EDGE_CURVE('',#4725,#4724,#1638,.T.);
#6120=EDGE_CURVE('',#4726,#4726,#3789,.T.);
#6121=EDGE_CURVE('',#4726,#4725,#1639,.T.);
#6122=EDGE_CURVE('',#4726,#4727,#1640,.T.);
#6123=EDGE_CURVE('',#4727,#4727,#3790,.T.);
#6124=EDGE_CURVE('',#4728,#4728,#3791,.T.);
#6125=EDGE_CURVE('',#4729,#4729,#3792,.T.);
#6126=EDGE_CURVE('',#4729,#4728,#1641,.T.);
#6127=EDGE_CURVE('',#4730,#4730,#3793,.T.);
#6128=EDGE_CURVE('',#4731,#4731,#3794,.T.);
#6129=EDGE_CURVE('',#4731,#4730,#1642,.T.);
#6130=EDGE_CURVE('',#4732,#4732,#3795,.T.);
#6131=EDGE_CURVE('',#4718,#4732,#1643,.T.);
#6132=EDGE_CURVE('',#4733,#4733,#3796,.T.);
#6133=EDGE_CURVE('',#4733,#4734,#1644,.T.);
#6134=EDGE_CURVE('',#4734,#4734,#3797,.T.);
#6135=EDGE_CURVE('',#4733,#4735,#1645,.T.);
#6136=EDGE_CURVE('',#4735,#4735,#3798,.T.);
#6137=EDGE_CURVE('',#4736,#4736,#3799,.T.);
#6138=EDGE_CURVE('',#4737,#4737,#3800,.T.);
#6139=EDGE_CURVE('',#4737,#4736,#1646,.T.);
#6140=EDGE_CURVE('',#4738,#4738,#3801,.T.);
#6141=EDGE_CURVE('',#4738,#4737,#1647,.T.);
#6142=EDGE_CURVE('',#4738,#4739,#1648,.T.);
#6143=EDGE_CURVE('',#4739,#4739,#3802,.T.);
#6144=EDGE_CURVE('',#4740,#4740,#3803,.T.);
#6145=EDGE_CURVE('',#4734,#4740,#1649,.T.);
#6146=EDGE_CURVE('',#4741,#4741,#3804,.T.);
#6147=EDGE_CURVE('',#4742,#4742,#3805,.T.);
#6148=EDGE_CURVE('',#4742,#4741,#1650,.T.);
#6149=EDGE_CURVE('',#4743,#4743,#3806,.T.);
#6150=EDGE_CURVE('',#4743,#4742,#1651,.T.);
#6151=EDGE_CURVE('',#4744,#4744,#3807,.T.);
#6152=EDGE_CURVE('',#4745,#4745,#3808,.T.);
#6153=EDGE_CURVE('',#4745,#4744,#1652,.T.);
#6154=EDGE_CURVE('',#4746,#4746,#3809,.T.);
#6155=EDGE_CURVE('',#4747,#4747,#3810,.T.);
#6156=EDGE_CURVE('',#4747,#4746,#1653,.T.);
#6157=EDGE_CURVE('',#4747,#4748,#1654,.T.);
#6158=EDGE_CURVE('',#4748,#4748,#3811,.T.);
#6159=EDGE_CURVE('',#4749,#4749,#3812,.T.);
#6160=EDGE_CURVE('',#4750,#4750,#3813,.T.);
#6161=EDGE_CURVE('',#4750,#4749,#1655,.T.);
#6162=EDGE_CURVE('',#4751,#4751,#3814,.T.);
#6163=EDGE_CURVE('',#4751,#4750,#1656,.T.);
#6164=EDGE_CURVE('',#4752,#4752,#3815,.T.);
#6165=EDGE_CURVE('',#4753,#4753,#3816,.T.);
#6166=EDGE_CURVE('',#4753,#4752,#1657,.T.);
#6167=EDGE_CURVE('',#4754,#4754,#3817,.T.);
#6168=EDGE_CURVE('',#4755,#4755,#3818,.T.);
#6169=EDGE_CURVE('',#4755,#4754,#1658,.T.);
#6170=EDGE_CURVE('',#4755,#4756,#1659,.T.);
#6171=EDGE_CURVE('',#4756,#4756,#3819,.T.);
#6172=EDGE_CURVE('',#4757,#4757,#3820,.T.);
#6173=EDGE_CURVE('',#4757,#4758,#3821,.T.);
#6174=EDGE_CURVE('',#4758,#4758,#3822,.T.);
#6175=EDGE_CURVE('',#4758,#4759,#1660,.T.);
#6176=EDGE_CURVE('',#4759,#4759,#3823,.T.);
#6177=EDGE_CURVE('',#4760,#4760,#3824,.T.);
#6178=EDGE_CURVE('',#4759,#4760,#1661,.T.);
#6179=EDGE_CURVE('',#4761,#4762,#1662,.T.);
#6180=EDGE_CURVE('',#4763,#4761,#908,.T.);
#6181=EDGE_CURVE('',#4764,#4763,#3825,.T.);
#6182=EDGE_CURVE('',#4764,#4762,#909,.T.);
#6183=EDGE_CURVE('',#4765,#4766,#1663,.T.);
#6184=EDGE_CURVE('',#4767,#4765,#910,.T.);
#6185=EDGE_CURVE('',#4761,#4767,#911,.T.);
#6186=EDGE_CURVE('',#4762,#4768,#912,.T.);
#6187=EDGE_CURVE('',#4768,#4766,#913,.T.);
#6188=EDGE_CURVE('',#4769,#4770,#1664,.T.);
#6189=EDGE_CURVE('',#4771,#4769,#914,.T.);
#6190=EDGE_CURVE('',#4765,#4771,#915,.T.);
#6191=EDGE_CURVE('',#4766,#4770,#916,.T.);
#6192=EDGE_CURVE('',#4772,#4773,#1665,.T.);
#6193=EDGE_CURVE('',#4774,#4772,#917,.T.);
#6194=EDGE_CURVE('',#4769,#4774,#918,.T.);
#6195=EDGE_CURVE('',#4770,#4775,#919,.T.);
#6196=EDGE_CURVE('',#4775,#4773,#920,.T.);
#6197=EDGE_CURVE('',#4776,#4777,#1666,.T.);
#6198=EDGE_CURVE('',#4778,#4776,#921,.T.);
#6199=EDGE_CURVE('',#4772,#4778,#922,.T.);
#6200=EDGE_CURVE('',#4773,#4777,#923,.T.);
#6201=EDGE_CURVE('',#4779,#4780,#1667,.T.);
#6202=EDGE_CURVE('',#4781,#4779,#924,.T.);
#6203=EDGE_CURVE('',#4776,#4781,#925,.T.);
#6204=EDGE_CURVE('',#4777,#4782,#926,.T.);
#6205=EDGE_CURVE('',#4782,#4780,#927,.T.);
#6206=EDGE_CURVE('',#4783,#4784,#1668,.T.);
#6207=EDGE_CURVE('',#4785,#4783,#928,.T.);
#6208=EDGE_CURVE('',#4779,#4785,#929,.T.);
#6209=EDGE_CURVE('',#4780,#4784,#930,.T.);
#6210=EDGE_CURVE('',#4786,#4787,#1669,.T.);
#6211=EDGE_CURVE('',#4788,#4786,#931,.T.);
#6212=EDGE_CURVE('',#4783,#4788,#932,.T.);
#6213=EDGE_CURVE('',#4784,#4789,#933,.T.);
#6214=EDGE_CURVE('',#4789,#4787,#934,.T.);
#6215=EDGE_CURVE('',#4790,#4791,#1670,.T.);
#6216=EDGE_CURVE('',#4792,#4790,#935,.T.);
#6217=EDGE_CURVE('',#4786,#4792,#936,.T.);
#6218=EDGE_CURVE('',#4787,#4791,#937,.T.);
#6219=EDGE_CURVE('',#4793,#4794,#1671,.T.);
#6220=EDGE_CURVE('',#4795,#4793,#938,.T.);
#6221=EDGE_CURVE('',#4790,#4795,#939,.T.);
#6222=EDGE_CURVE('',#4791,#4796,#940,.T.);
#6223=EDGE_CURVE('',#4796,#4794,#941,.T.);
#6224=EDGE_CURVE('',#4797,#4798,#1672,.T.);
#6225=EDGE_CURVE('',#4799,#4797,#942,.T.);
#6226=EDGE_CURVE('',#4793,#4799,#943,.T.);
#6227=EDGE_CURVE('',#4794,#4798,#944,.T.);
#6228=EDGE_CURVE('',#4800,#4801,#1673,.T.);
#6229=EDGE_CURVE('',#4802,#4800,#945,.T.);
#6230=EDGE_CURVE('',#4797,#4802,#946,.T.);
#6231=EDGE_CURVE('',#4798,#4803,#947,.T.);
#6232=EDGE_CURVE('',#4803,#4801,#948,.T.);
#6233=EDGE_CURVE('',#4804,#4805,#1674,.T.);
#6234=EDGE_CURVE('',#4806,#4804,#949,.T.);
#6235=EDGE_CURVE('',#4800,#4806,#950,.T.);
#6236=EDGE_CURVE('',#4801,#4805,#951,.T.);
#6237=EDGE_CURVE('',#4807,#4808,#1675,.T.);
#6238=EDGE_CURVE('',#4809,#4807,#952,.T.);
#6239=EDGE_CURVE('',#4804,#4809,#953,.T.);
#6240=EDGE_CURVE('',#4805,#4810,#954,.T.);
#6241=EDGE_CURVE('',#4810,#4808,#955,.T.);
#6242=EDGE_CURVE('',#4811,#4812,#956,.T.);
#6243=EDGE_CURVE('',#4812,#4813,#3826,.T.);
#6244=EDGE_CURVE('',#4813,#4814,#957,.T.);
#6245=EDGE_CURVE('',#4814,#4815,#958,.T.);
#6246=EDGE_CURVE('',#4815,#4816,#959,.T.);
#6247=EDGE_CURVE('',#4816,#4817,#960,.T.);
#6248=EDGE_CURVE('',#4817,#4818,#961,.T.);
#6249=EDGE_CURVE('',#4818,#4819,#962,.T.);
#6250=EDGE_CURVE('',#4819,#4820,#963,.T.);
#6251=EDGE_CURVE('',#4820,#4821,#964,.T.);
#6252=EDGE_CURVE('',#4821,#4822,#965,.T.);
#6253=EDGE_CURVE('',#4822,#4823,#966,.T.);
#6254=EDGE_CURVE('',#4823,#4824,#967,.T.);
#6255=EDGE_CURVE('',#4824,#4825,#968,.T.);
#6256=EDGE_CURVE('',#4825,#4826,#969,.T.);
#6257=EDGE_CURVE('',#4826,#4827,#970,.T.);
#6258=EDGE_CURVE('',#4827,#4828,#971,.T.);
#6259=EDGE_CURVE('',#4829,#4828,#3827,.T.);
#6260=EDGE_CURVE('',#4829,#4830,#972,.T.);
#6261=EDGE_CURVE('',#4830,#4831,#973,.T.);
#6262=EDGE_CURVE('',#4831,#4832,#974,.T.);
#6263=EDGE_CURVE('',#4832,#4833,#975,.T.);
#6264=EDGE_CURVE('',#4833,#4834,#976,.T.);
#6265=EDGE_CURVE('',#4834,#4835,#977,.T.);
#6266=EDGE_CURVE('',#4835,#4836,#978,.T.);
#6267=EDGE_CURVE('',#4836,#4837,#979,.T.);
#6268=EDGE_CURVE('',#4837,#4838,#980,.T.);
#6269=EDGE_CURVE('',#4838,#4839,#981,.T.);
#6270=EDGE_CURVE('',#4839,#4840,#982,.T.);
#6271=EDGE_CURVE('',#4840,#4841,#983,.T.);
#6272=EDGE_CURVE('',#4841,#4842,#984,.T.);
#6273=EDGE_CURVE('',#4842,#4811,#985,.T.);
#6274=EDGE_CURVE('',#4808,#4843,#986,.T.);
#6275=EDGE_CURVE('',#4843,#4844,#987,.T.);
#6276=EDGE_CURVE('',#4845,#4844,#3828,.T.);
#6277=EDGE_CURVE('',#4846,#4845,#988,.T.);
#6278=EDGE_CURVE('',#4807,#4846,#989,.T.);
#6279=EDGE_CURVE('',#4828,#4845,#990,.T.);
#6280=EDGE_CURVE('',#4763,#4813,#991,.T.);
#6281=EDGE_CURVE('',#4813,#4847,#3829,.T.);
#6282=EDGE_CURVE('',#4847,#4848,#3830,.T.);
#6283=EDGE_CURVE('',#4848,#4764,#992,.T.);
#6284=EDGE_CURVE('',#4844,#4829,#993,.T.);
#6285=EDGE_CURVE('',#4848,#4812,#994,.T.);
#6286=EDGE_CURVE('',#4849,#4850,#147,.T.);
#6287=EDGE_CURVE('',#4850,#4849,#3831,.T.);
#6288=EDGE_CURVE('',#4851,#4852,#148,.T.);
#6289=EDGE_CURVE('',#4852,#4851,#3832,.T.);
#6290=EDGE_CURVE('',#4853,#4854,#149,.T.);
#6291=EDGE_CURVE('',#4854,#4853,#3833,.T.);
#6292=EDGE_CURVE('',#4855,#4856,#150,.T.);
#6293=EDGE_CURVE('',#4856,#4855,#3834,.T.);
#6294=EDGE_CURVE('',#4857,#4858,#151,.T.);
#6295=EDGE_CURVE('',#4859,#4857,#3835,.T.);
#6296=EDGE_CURVE('',#4858,#4859,#3836,.T.);
#6297=EDGE_CURVE('',#4860,#4861,#152,.T.);
#6298=EDGE_CURVE('',#4861,#4860,#3837,.T.);
#6299=EDGE_CURVE('',#4859,#4862,#3838,.T.);
#6300=EDGE_CURVE('',#4862,#4862,#3839,.T.);
#6301=EDGE_CURVE('',#4857,#4863,#3840,.T.);
#6302=EDGE_CURVE('',#4863,#4856,#3841,.T.);
#6303=EDGE_CURVE('',#4855,#4864,#3842,.T.);
#6304=EDGE_CURVE('',#4864,#4854,#3843,.T.);
#6305=EDGE_CURVE('',#4853,#4865,#3844,.T.);
#6306=EDGE_CURVE('',#4865,#4850,#3845,.T.);
#6307=EDGE_CURVE('',#4849,#4866,#3846,.T.);
#6308=EDGE_CURVE('',#4866,#4852,#3847,.T.);
#6309=EDGE_CURVE('',#4851,#4867,#3848,.T.);
#6310=EDGE_CURVE('',#4867,#4861,#3849,.T.);
#6311=EDGE_CURVE('',#4860,#4868,#3850,.T.);
#6312=EDGE_CURVE('',#4868,#4858,#3851,.T.);
#6313=EDGE_CURVE('',#4869,#4870,#1676,.T.);
#6314=EDGE_CURVE('',#4870,#4870,#3852,.T.);
#6315=EDGE_CURVE('',#4867,#4871,#1677,.T.);
#6316=EDGE_CURVE('',#4871,#4872,#1678,.T.);
#6317=EDGE_CURVE('',#4868,#4872,#1679,.T.);
#6318=EDGE_CURVE('',#4872,#4873,#1680,.T.);
#6319=EDGE_CURVE('',#4863,#4873,#1681,.T.);
#6320=EDGE_CURVE('',#4873,#4874,#1682,.T.);
#6321=EDGE_CURVE('',#4864,#4874,#1683,.T.);
#6322=EDGE_CURVE('',#4874,#4875,#1684,.T.);
#6323=EDGE_CURVE('',#4865,#4875,#1685,.T.);
#6324=EDGE_CURVE('',#4866,#4876,#1686,.T.);
#6325=EDGE_CURVE('',#4876,#4871,#1687,.T.);
#6326=EDGE_CURVE('',#4875,#4876,#1688,.T.);
#6327=EDGE_CURVE('',#4877,#4877,#3853,.T.);
#6328=EDGE_CURVE('',#4847,#4877,#1689,.T.);
#6329=EDGE_CURVE('',#4878,#4878,#3854,.T.);
#6330=EDGE_CURVE('',#4862,#4878,#1690,.T.);
#6331=EDGE_CURVE('',#4879,#4880,#1691,.T.);
#6332=EDGE_CURVE('',#4881,#4879,#1692,.T.);
#6333=EDGE_CURVE('',#4882,#4881,#1693,.T.);
#6334=EDGE_CURVE('',#4880,#4882,#1694,.T.);
#6335=EDGE_CURVE('',#4883,#4884,#1695,.T.);
#6336=EDGE_CURVE('',#4885,#4883,#1696,.T.);
#6337=EDGE_CURVE('',#4886,#4885,#1697,.T.);
#6338=EDGE_CURVE('',#4884,#4886,#1698,.T.);
#6339=EDGE_CURVE('',#4887,#4888,#1699,.T.);
#6340=EDGE_CURVE('',#4889,#4887,#1700,.T.);
#6341=EDGE_CURVE('',#4890,#4889,#1701,.T.);
#6342=EDGE_CURVE('',#4888,#4890,#1702,.T.);
#6343=EDGE_CURVE('',#4891,#4892,#1703,.T.);
#6344=EDGE_CURVE('',#4893,#4891,#1704,.T.);
#6345=EDGE_CURVE('',#4894,#4893,#1705,.T.);
#6346=EDGE_CURVE('',#4892,#4894,#1706,.T.);
#6347=EDGE_CURVE('',#4895,#4885,#3855,.T.);
#6348=EDGE_CURVE('',#4896,#4895,#1707,.T.);
#6349=EDGE_CURVE('',#4896,#4886,#3856,.T.);
#6350=EDGE_CURVE('',#4884,#4897,#3857,.T.);
#6351=EDGE_CURVE('',#4897,#4898,#1708,.T.);
#6352=EDGE_CURVE('',#4883,#4898,#3858,.T.);
#6353=EDGE_CURVE('',#4899,#4893,#3859,.T.);
#6354=EDGE_CURVE('',#4900,#4899,#1709,.T.);
#6355=EDGE_CURVE('',#4900,#4894,#3860,.T.);
#6356=EDGE_CURVE('',#4892,#4901,#3861,.T.);
#6357=EDGE_CURVE('',#4901,#4902,#1710,.T.);
#6358=EDGE_CURVE('',#4891,#4902,#3862,.T.);
#6359=EDGE_CURVE('',#4888,#4900,#3863,.T.);
#6360=EDGE_CURVE('',#4887,#4899,#3864,.T.);
#6361=EDGE_CURVE('',#4903,#4896,#3865,.T.);
#6362=EDGE_CURVE('',#4904,#4903,#3866,.T.);
#6363=EDGE_CURVE('',#4901,#4904,#3867,.T.);
#6364=EDGE_CURVE('',#4881,#4890,#3868,.T.);
#6365=EDGE_CURVE('',#4897,#4879,#3869,.T.);
#6366=EDGE_CURVE('',#4898,#4880,#3870,.T.);
#6367=EDGE_CURVE('',#4905,#4895,#3871,.T.);
#6368=EDGE_CURVE('',#4903,#4905,#1711,.T.);
#6369=EDGE_CURVE('',#4906,#4905,#3872,.T.);
#6370=EDGE_CURVE('',#4904,#4906,#1712,.T.);
#6371=EDGE_CURVE('',#4902,#4906,#3873,.T.);
#6372=EDGE_CURVE('',#4882,#4889,#3874,.T.);
#6373=EDGE_CURVE('',#4907,#4908,#1713,.T.);
#6374=EDGE_CURVE('',#4909,#4907,#1714,.T.);
#6375=EDGE_CURVE('',#4910,#4909,#1715,.T.);
#6376=EDGE_CURVE('',#4908,#4910,#1716,.T.);
#6377=EDGE_CURVE('',#4911,#4912,#1717,.T.);
#6378=EDGE_CURVE('',#4913,#4911,#1718,.T.);
#6379=EDGE_CURVE('',#4914,#4913,#1719,.T.);
#6380=EDGE_CURVE('',#4912,#4914,#1720,.T.);
#6381=EDGE_CURVE('',#4915,#4916,#1721,.T.);
#6382=EDGE_CURVE('',#4917,#4915,#1722,.T.);
#6383=EDGE_CURVE('',#4918,#4917,#1723,.T.);
#6384=EDGE_CURVE('',#4916,#4918,#1724,.T.);
#6385=EDGE_CURVE('',#4919,#4920,#1725,.T.);
#6386=EDGE_CURVE('',#4921,#4919,#1726,.T.);
#6387=EDGE_CURVE('',#4922,#4921,#1727,.T.);
#6388=EDGE_CURVE('',#4920,#4922,#1728,.T.);
#6389=EDGE_CURVE('',#4923,#4913,#3875,.T.);
#6390=EDGE_CURVE('',#4924,#4923,#1729,.T.);
#6391=EDGE_CURVE('',#4924,#4914,#3876,.T.);
#6392=EDGE_CURVE('',#4912,#4925,#3877,.T.);
#6393=EDGE_CURVE('',#4925,#4926,#1730,.T.);
#6394=EDGE_CURVE('',#4911,#4926,#3878,.T.);
#6395=EDGE_CURVE('',#4927,#4921,#3879,.T.);
#6396=EDGE_CURVE('',#4928,#4927,#1731,.T.);
#6397=EDGE_CURVE('',#4928,#4922,#3880,.T.);
#6398=EDGE_CURVE('',#4920,#4929,#3881,.T.);
#6399=EDGE_CURVE('',#4929,#4930,#1732,.T.);
#6400=EDGE_CURVE('',#4919,#4930,#3882,.T.);
#6401=EDGE_CURVE('',#4916,#4928,#3883,.T.);
#6402=EDGE_CURVE('',#4915,#4927,#3884,.T.);
#6403=EDGE_CURVE('',#4931,#4924,#3885,.T.);
#6404=EDGE_CURVE('',#4932,#4931,#3886,.T.);
#6405=EDGE_CURVE('',#4929,#4932,#3887,.T.);
#6406=EDGE_CURVE('',#4909,#4918,#3888,.T.);
#6407=EDGE_CURVE('',#4925,#4907,#3889,.T.);
#6408=EDGE_CURVE('',#4926,#4908,#3890,.T.);
#6409=EDGE_CURVE('',#4933,#4923,#3891,.T.);
#6410=EDGE_CURVE('',#4931,#4933,#1733,.T.);
#6411=EDGE_CURVE('',#4934,#4933,#3892,.T.);
#6412=EDGE_CURVE('',#4932,#4934,#1734,.T.);
#6413=EDGE_CURVE('',#4930,#4934,#3893,.T.);
#6414=EDGE_CURVE('',#4910,#4917,#3894,.T.);
#6415=ORIENTED_EDGE('',*,*,#4935,.T.);
#6416=ORIENTED_EDGE('',*,*,#4936,.T.);
#6417=ORIENTED_EDGE('',*,*,#4937,.T.);
#6418=ORIENTED_EDGE('',*,*,#4936,.F.);
#6419=ORIENTED_EDGE('',*,*,#4938,.T.);
#6420=ORIENTED_EDGE('',*,*,#4935,.F.);
#6421=ORIENTED_EDGE('',*,*,#4939,.T.);
#6422=ORIENTED_EDGE('',*,*,#4940,.F.);
#6423=ORIENTED_EDGE('',*,*,#4941,.F.);
#6424=ORIENTED_EDGE('',*,*,#4939,.F.);
#6425=ORIENTED_EDGE('',*,*,#4938,.F.);
#6426=ORIENTED_EDGE('',*,*,#4942,.F.);
#6427=ORIENTED_EDGE('',*,*,#4943,.F.);
#6428=ORIENTED_EDGE('',*,*,#4944,.F.);
#6429=ORIENTED_EDGE('',*,*,#4945,.F.);
#6430=ORIENTED_EDGE('',*,*,#4946,.F.);
#6431=ORIENTED_EDGE('',*,*,#4947,.F.);
#6432=ORIENTED_EDGE('',*,*,#4937,.F.);
#6433=ORIENTED_EDGE('',*,*,#4948,.T.);
#6434=ORIENTED_EDGE('',*,*,#4949,.T.);
#6435=ORIENTED_EDGE('',*,*,#4940,.T.);
#6436=ORIENTED_EDGE('',*,*,#4941,.T.);
#6437=ORIENTED_EDGE('',*,*,#4949,.F.);
#6438=ORIENTED_EDGE('',*,*,#4950,.F.);
#6439=ORIENTED_EDGE('',*,*,#4951,.F.);
#6440=ORIENTED_EDGE('',*,*,#4952,.F.);
#6441=ORIENTED_EDGE('',*,*,#4953,.F.);
#6442=ORIENTED_EDGE('',*,*,#4954,.F.);
#6443=ORIENTED_EDGE('',*,*,#4955,.F.);
#6444=ORIENTED_EDGE('',*,*,#4956,.T.);
#6445=ORIENTED_EDGE('',*,*,#4957,.T.);
#6446=ORIENTED_EDGE('',*,*,#4958,.F.);
#6447=ORIENTED_EDGE('',*,*,#4948,.F.);
#6448=ORIENTED_EDGE('',*,*,#4959,.T.);
#6449=ORIENTED_EDGE('',*,*,#4960,.T.);
#6450=ORIENTED_EDGE('',*,*,#4961,.T.);
#6451=ORIENTED_EDGE('',*,*,#4960,.F.);
#6452=ORIENTED_EDGE('',*,*,#4962,.T.);
#6453=ORIENTED_EDGE('',*,*,#4959,.F.);
#6454=ORIENTED_EDGE('',*,*,#4963,.T.);
#6455=ORIENTED_EDGE('',*,*,#4964,.F.);
#6456=ORIENTED_EDGE('',*,*,#4965,.F.);
#6457=ORIENTED_EDGE('',*,*,#4963,.F.);
#6458=ORIENTED_EDGE('',*,*,#4962,.F.);
#6459=ORIENTED_EDGE('',*,*,#4966,.F.);
#6460=ORIENTED_EDGE('',*,*,#4967,.F.);
#6461=ORIENTED_EDGE('',*,*,#4968,.T.);
#6462=ORIENTED_EDGE('',*,*,#4969,.F.);
#6463=ORIENTED_EDGE('',*,*,#4970,.F.);
#6464=ORIENTED_EDGE('',*,*,#4961,.F.);
#6465=ORIENTED_EDGE('',*,*,#4971,.T.);
#6466=ORIENTED_EDGE('',*,*,#4972,.T.);
#6467=ORIENTED_EDGE('',*,*,#4964,.T.);
#6468=ORIENTED_EDGE('',*,*,#4965,.T.);
#6469=ORIENTED_EDGE('',*,*,#4972,.F.);
#6470=ORIENTED_EDGE('',*,*,#4973,.F.);
#6471=ORIENTED_EDGE('',*,*,#4974,.F.);
#6472=ORIENTED_EDGE('',*,*,#4975,.T.);
#6473=ORIENTED_EDGE('',*,*,#4976,.F.);
#6474=ORIENTED_EDGE('',*,*,#4977,.F.);
#6475=ORIENTED_EDGE('',*,*,#4978,.F.);
#6476=ORIENTED_EDGE('',*,*,#4979,.F.);
#6477=ORIENTED_EDGE('',*,*,#4980,.F.);
#6478=ORIENTED_EDGE('',*,*,#4981,.F.);
#6479=ORIENTED_EDGE('',*,*,#4982,.F.);
#6480=ORIENTED_EDGE('',*,*,#4983,.T.);
#6481=ORIENTED_EDGE('',*,*,#4971,.F.);
#6482=ORIENTED_EDGE('',*,*,#4974,.T.);
#6483=ORIENTED_EDGE('',*,*,#4984,.F.);
#6484=ORIENTED_EDGE('',*,*,#4985,.T.);
#6485=ORIENTED_EDGE('',*,*,#4986,.T.);
#6486=ORIENTED_EDGE('',*,*,#4987,.T.);
#6487=ORIENTED_EDGE('',*,*,#4988,.F.);
#6488=ORIENTED_EDGE('',*,*,#4966,.T.);
#6489=ORIENTED_EDGE('',*,*,#4989,.T.);
#6490=ORIENTED_EDGE('',*,*,#4990,.T.);
#6491=ORIENTED_EDGE('',*,*,#4989,.F.);
#6492=ORIENTED_EDGE('',*,*,#4991,.T.);
#6493=ORIENTED_EDGE('',*,*,#4986,.F.);
#6494=ORIENTED_EDGE('',*,*,#4987,.F.);
#6495=ORIENTED_EDGE('',*,*,#4992,.F.);
#6496=ORIENTED_EDGE('',*,*,#4993,.F.);
#6497=ORIENTED_EDGE('',*,*,#4994,.F.);
#6498=ORIENTED_EDGE('',*,*,#4995,.F.);
#6499=ORIENTED_EDGE('',*,*,#4996,.F.);
#6500=ORIENTED_EDGE('',*,*,#4997,.F.);
#6501=ORIENTED_EDGE('',*,*,#4975,.F.);
#6502=ORIENTED_EDGE('',*,*,#4991,.F.);
#6503=ORIENTED_EDGE('',*,*,#4970,.T.);
#6504=ORIENTED_EDGE('',*,*,#4998,.T.);
#6505=ORIENTED_EDGE('',*,*,#4992,.T.);
#6506=ORIENTED_EDGE('',*,*,#4999,.T.);
#6507=ORIENTED_EDGE('',*,*,#5000,.T.);
#6508=ORIENTED_EDGE('',*,*,#5001,.T.);
#6509=ORIENTED_EDGE('',*,*,#5002,.T.);
#6510=ORIENTED_EDGE('',*,*,#4969,.T.);
#6511=ORIENTED_EDGE('',*,*,#4999,.F.);
#6512=ORIENTED_EDGE('',*,*,#5003,.T.);
#6513=ORIENTED_EDGE('',*,*,#5002,.F.);
#6514=ORIENTED_EDGE('',*,*,#5004,.T.);
#6515=ORIENTED_EDGE('',*,*,#4998,.F.);
#6516=ORIENTED_EDGE('',*,*,#5004,.F.);
#6517=ORIENTED_EDGE('',*,*,#5005,.T.);
#6518=ORIENTED_EDGE('',*,*,#5006,.F.);
#6519=ORIENTED_EDGE('',*,*,#4993,.T.);
#6520=ORIENTED_EDGE('',*,*,#5003,.F.);
#6521=ORIENTED_EDGE('',*,*,#5001,.F.);
#6522=ORIENTED_EDGE('',*,*,#5007,.T.);
#6523=ORIENTED_EDGE('',*,*,#5008,.F.);
#6524=ORIENTED_EDGE('',*,*,#5005,.F.);
#6525=ORIENTED_EDGE('',*,*,#5009,.T.);
#6526=ORIENTED_EDGE('',*,*,#4995,.T.);
#6527=ORIENTED_EDGE('',*,*,#5010,.T.);
#6528=ORIENTED_EDGE('',*,*,#5011,.T.);
#6529=ORIENTED_EDGE('',*,*,#5012,.T.);
#6530=ORIENTED_EDGE('',*,*,#4996,.T.);
#6531=ORIENTED_EDGE('',*,*,#5009,.F.);
#6532=ORIENTED_EDGE('',*,*,#5013,.T.);
#6533=ORIENTED_EDGE('',*,*,#5010,.F.);
#6534=ORIENTED_EDGE('',*,*,#4994,.T.);
#6535=ORIENTED_EDGE('',*,*,#5006,.T.);
#6536=ORIENTED_EDGE('',*,*,#5014,.T.);
#6537=ORIENTED_EDGE('',*,*,#4976,.T.);
#6538=ORIENTED_EDGE('',*,*,#4997,.T.);
#6539=ORIENTED_EDGE('',*,*,#5012,.F.);
#6540=ORIENTED_EDGE('',*,*,#5015,.T.);
#6541=ORIENTED_EDGE('',*,*,#5014,.F.);
#6542=ORIENTED_EDGE('',*,*,#5008,.T.);
#6543=ORIENTED_EDGE('',*,*,#5016,.T.);
#6544=ORIENTED_EDGE('',*,*,#5017,.T.);
#6545=ORIENTED_EDGE('',*,*,#5000,.F.);
#6546=ORIENTED_EDGE('',*,*,#4968,.F.);
#6547=ORIENTED_EDGE('',*,*,#5018,.F.);
#6548=ORIENTED_EDGE('',*,*,#5019,.F.);
#6549=ORIENTED_EDGE('',*,*,#5020,.T.);
#6550=ORIENTED_EDGE('',*,*,#5021,.F.);
#6551=ORIENTED_EDGE('',*,*,#5011,.F.);
#6552=ORIENTED_EDGE('',*,*,#5017,.F.);
#6553=ORIENTED_EDGE('',*,*,#5022,.T.);
#6554=ORIENTED_EDGE('',*,*,#5023,.T.);
#6555=ORIENTED_EDGE('',*,*,#5013,.F.);
#6556=ORIENTED_EDGE('',*,*,#5023,.F.);
#6557=ORIENTED_EDGE('',*,*,#5024,.T.);
#6558=ORIENTED_EDGE('',*,*,#5025,.T.);
#6559=ORIENTED_EDGE('',*,*,#5015,.F.);
#6560=ORIENTED_EDGE('',*,*,#5025,.F.);
#6561=ORIENTED_EDGE('',*,*,#5026,.T.);
#6562=ORIENTED_EDGE('',*,*,#4979,.T.);
#6563=ORIENTED_EDGE('',*,*,#5027,.T.);
#6564=ORIENTED_EDGE('',*,*,#4977,.T.);
#6565=ORIENTED_EDGE('',*,*,#4978,.T.);
#6566=ORIENTED_EDGE('',*,*,#5027,.F.);
#6567=ORIENTED_EDGE('',*,*,#4982,.T.);
#6568=ORIENTED_EDGE('',*,*,#5028,.T.);
#6569=ORIENTED_EDGE('',*,*,#5029,.T.);
#6570=ORIENTED_EDGE('',*,*,#4981,.T.);
#6571=ORIENTED_EDGE('',*,*,#5030,.F.);
#6572=ORIENTED_EDGE('',*,*,#5031,.T.);
#6573=ORIENTED_EDGE('',*,*,#5028,.F.);
#6574=ORIENTED_EDGE('',*,*,#4980,.T.);
#6575=ORIENTED_EDGE('',*,*,#5026,.F.);
#6576=ORIENTED_EDGE('',*,*,#5032,.T.);
#6577=ORIENTED_EDGE('',*,*,#5033,.T.);
#6578=ORIENTED_EDGE('',*,*,#5034,.T.);
#6579=ORIENTED_EDGE('',*,*,#5030,.T.);
#6580=ORIENTED_EDGE('',*,*,#5024,.F.);
#6581=ORIENTED_EDGE('',*,*,#5035,.F.);
#6582=ORIENTED_EDGE('',*,*,#5036,.F.);
#6583=ORIENTED_EDGE('',*,*,#5037,.T.);
#6584=ORIENTED_EDGE('',*,*,#5032,.F.);
#6585=ORIENTED_EDGE('',*,*,#5022,.F.);
#6586=ORIENTED_EDGE('',*,*,#5016,.F.);
#6587=ORIENTED_EDGE('',*,*,#5038,.F.);
#6588=ORIENTED_EDGE('',*,*,#5039,.F.);
#6589=ORIENTED_EDGE('',*,*,#5035,.T.);
#6590=ORIENTED_EDGE('',*,*,#5040,.T.);
#6591=ORIENTED_EDGE('',*,*,#5041,.T.);
#6592=ORIENTED_EDGE('',*,*,#5042,.T.);
#6593=ORIENTED_EDGE('',*,*,#5043,.T.);
#6594=ORIENTED_EDGE('',*,*,#5044,.T.);
#6595=ORIENTED_EDGE('',*,*,#5045,.T.);
#6596=ORIENTED_EDGE('',*,*,#5040,.F.);
#6597=ORIENTED_EDGE('',*,*,#5046,.F.);
#6598=ORIENTED_EDGE('',*,*,#5042,.F.);
#6599=ORIENTED_EDGE('',*,*,#5047,.T.);
#6600=ORIENTED_EDGE('',*,*,#5048,.T.);
#6601=ORIENTED_EDGE('',*,*,#5044,.F.);
#6602=ORIENTED_EDGE('',*,*,#5049,.F.);
#6603=ORIENTED_EDGE('',*,*,#5050,.T.);
#6604=ORIENTED_EDGE('',*,*,#5051,.T.);
#6605=ORIENTED_EDGE('',*,*,#5052,.T.);
#6606=ORIENTED_EDGE('',*,*,#5053,.T.);
#6607=ORIENTED_EDGE('',*,*,#5050,.F.);
#6608=ORIENTED_EDGE('',*,*,#5054,.T.);
#6609=ORIENTED_EDGE('',*,*,#5045,.F.);
#6610=ORIENTED_EDGE('',*,*,#5055,.T.);
#6611=ORIENTED_EDGE('',*,*,#5056,.T.);
#6612=ORIENTED_EDGE('',*,*,#5057,.T.);
#6613=ORIENTED_EDGE('',*,*,#5041,.F.);
#6614=ORIENTED_EDGE('',*,*,#5053,.F.);
#6615=ORIENTED_EDGE('',*,*,#5058,.T.);
#6616=ORIENTED_EDGE('',*,*,#5059,.T.);
#6617=ORIENTED_EDGE('',*,*,#5060,.T.);
#6618=ORIENTED_EDGE('',*,*,#5061,.F.);
#6619=ORIENTED_EDGE('',*,*,#5062,.F.);
#6620=ORIENTED_EDGE('',*,*,#5063,.T.);
#6621=ORIENTED_EDGE('',*,*,#5064,.T.);
#6622=ORIENTED_EDGE('',*,*,#5055,.F.);
#6623=ORIENTED_EDGE('',*,*,#5051,.F.);
#6624=ORIENTED_EDGE('',*,*,#5048,.F.);
#6625=ORIENTED_EDGE('',*,*,#5065,.T.);
#6626=ORIENTED_EDGE('',*,*,#5066,.T.);
#6627=ORIENTED_EDGE('',*,*,#5067,.T.);
#6628=ORIENTED_EDGE('',*,*,#5049,.T.);
#6629=ORIENTED_EDGE('',*,*,#5046,.T.);
#6630=ORIENTED_EDGE('',*,*,#5043,.F.);
#6631=ORIENTED_EDGE('',*,*,#5068,.T.);
#6632=ORIENTED_EDGE('',*,*,#5069,.F.);
#6633=ORIENTED_EDGE('',*,*,#5070,.T.);
#6634=ORIENTED_EDGE('',*,*,#5071,.T.);
#6635=ORIENTED_EDGE('',*,*,#5072,.T.);
#6636=ORIENTED_EDGE('',*,*,#5073,.T.);
#6637=ORIENTED_EDGE('',*,*,#5074,.T.);
#6638=ORIENTED_EDGE('',*,*,#5075,.T.);
#6639=ORIENTED_EDGE('',*,*,#5076,.T.);
#6640=ORIENTED_EDGE('',*,*,#5077,.T.);
#6641=ORIENTED_EDGE('',*,*,#5074,.F.);
#6642=ORIENTED_EDGE('',*,*,#5078,.T.);
#6643=ORIENTED_EDGE('',*,*,#5072,.F.);
#6644=ORIENTED_EDGE('',*,*,#5079,.T.);
#6645=ORIENTED_EDGE('',*,*,#5070,.F.);
#6646=ORIENTED_EDGE('',*,*,#5080,.T.);
#6647=ORIENTED_EDGE('',*,*,#5081,.T.);
#6648=ORIENTED_EDGE('',*,*,#5082,.T.);
#6649=ORIENTED_EDGE('',*,*,#5076,.F.);
#6650=ORIENTED_EDGE('',*,*,#5083,.T.);
#6651=ORIENTED_EDGE('',*,*,#5081,.F.);
#6652=ORIENTED_EDGE('',*,*,#5084,.T.);
#6653=ORIENTED_EDGE('',*,*,#5066,.F.);
#6654=ORIENTED_EDGE('',*,*,#5082,.F.);
#6655=ORIENTED_EDGE('',*,*,#5065,.F.);
#6656=ORIENTED_EDGE('',*,*,#5085,.F.);
#6657=ORIENTED_EDGE('',*,*,#5067,.F.);
#6658=ORIENTED_EDGE('',*,*,#5086,.F.);
#6659=ORIENTED_EDGE('',*,*,#5087,.F.);
#6660=ORIENTED_EDGE('',*,*,#5054,.F.);
#6661=ORIENTED_EDGE('',*,*,#5084,.F.);
#6662=ORIENTED_EDGE('',*,*,#5088,.T.);
#6663=ORIENTED_EDGE('',*,*,#5089,.T.);
#6664=ORIENTED_EDGE('',*,*,#5090,.T.);
#6665=ORIENTED_EDGE('',*,*,#5086,.T.);
#6666=ORIENTED_EDGE('',*,*,#5083,.F.);
#6667=ORIENTED_EDGE('',*,*,#5078,.F.);
#6668=ORIENTED_EDGE('',*,*,#5091,.T.);
#6669=ORIENTED_EDGE('',*,*,#5092,.T.);
#6670=ORIENTED_EDGE('',*,*,#5088,.F.);
#6671=ORIENTED_EDGE('',*,*,#5073,.F.);
#6672=ORIENTED_EDGE('',*,*,#5093,.F.);
#6673=ORIENTED_EDGE('',*,*,#5094,.T.);
#6674=ORIENTED_EDGE('',*,*,#5091,.F.);
#6675=ORIENTED_EDGE('',*,*,#5056,.F.);
#6676=ORIENTED_EDGE('',*,*,#5064,.F.);
#6677=ORIENTED_EDGE('',*,*,#5095,.F.);
#6678=ORIENTED_EDGE('',*,*,#5079,.F.);
#6679=ORIENTED_EDGE('',*,*,#5075,.F.);
#6680=ORIENTED_EDGE('',*,*,#5077,.F.);
#6681=ORIENTED_EDGE('',*,*,#5085,.T.);
#6682=ORIENTED_EDGE('',*,*,#5047,.F.);
#6683=ORIENTED_EDGE('',*,*,#5057,.F.);
#6684=ORIENTED_EDGE('',*,*,#5080,.F.);
#6685=ORIENTED_EDGE('',*,*,#5069,.T.);
#6686=ORIENTED_EDGE('',*,*,#5096,.T.);
#6687=ORIENTED_EDGE('',*,*,#5097,.F.);
#6688=ORIENTED_EDGE('',*,*,#5093,.T.);
#6689=ORIENTED_EDGE('',*,*,#5098,.T.);
#6690=ORIENTED_EDGE('',*,*,#5099,.T.);
#6691=ORIENTED_EDGE('',*,*,#5019,.T.);
#6692=ORIENTED_EDGE('',*,*,#5100,.T.);
#6693=ORIENTED_EDGE('',*,*,#5100,.F.);
#6694=ORIENTED_EDGE('',*,*,#5018,.T.);
#6695=ORIENTED_EDGE('',*,*,#4967,.T.);
#6696=ORIENTED_EDGE('',*,*,#4988,.T.);
#6697=ORIENTED_EDGE('',*,*,#5101,.F.);
#6698=ORIENTED_EDGE('',*,*,#4984,.T.);
#6699=ORIENTED_EDGE('',*,*,#4973,.T.);
#6700=ORIENTED_EDGE('',*,*,#5102,.T.);
#6701=ORIENTED_EDGE('',*,*,#5103,.T.);
#6702=ORIENTED_EDGE('',*,*,#5104,.T.);
#6703=ORIENTED_EDGE('',*,*,#5105,.T.);
#6704=ORIENTED_EDGE('',*,*,#5106,.T.);
#6705=ORIENTED_EDGE('',*,*,#5107,.F.);
#6706=ORIENTED_EDGE('',*,*,#5108,.T.);
#6707=ORIENTED_EDGE('',*,*,#5109,.T.);
#6708=ORIENTED_EDGE('',*,*,#5105,.F.);
#6709=ORIENTED_EDGE('',*,*,#5110,.T.);
#6710=ORIENTED_EDGE('',*,*,#5103,.F.);
#6711=ORIENTED_EDGE('',*,*,#5111,.F.);
#6712=ORIENTED_EDGE('',*,*,#5112,.T.);
#6713=ORIENTED_EDGE('',*,*,#5113,.T.);
#6714=ORIENTED_EDGE('',*,*,#5114,.T.);
#6715=ORIENTED_EDGE('',*,*,#5115,.T.);
#6716=ORIENTED_EDGE('',*,*,#5116,.T.);
#6717=ORIENTED_EDGE('',*,*,#5116,.F.);
#6718=ORIENTED_EDGE('',*,*,#5117,.T.);
#6719=ORIENTED_EDGE('',*,*,#5108,.F.);
#6720=ORIENTED_EDGE('',*,*,#5118,.T.);
#6721=ORIENTED_EDGE('',*,*,#5119,.F.);
#6722=ORIENTED_EDGE('',*,*,#5106,.F.);
#6723=ORIENTED_EDGE('',*,*,#5120,.F.);
#6724=ORIENTED_EDGE('',*,*,#4950,.T.);
#6725=ORIENTED_EDGE('',*,*,#5121,.T.);
#6726=ORIENTED_EDGE('',*,*,#5109,.F.);
#6727=ORIENTED_EDGE('',*,*,#5122,.T.);
#6728=ORIENTED_EDGE('',*,*,#4951,.T.);
#6729=ORIENTED_EDGE('',*,*,#5120,.T.);
#6730=ORIENTED_EDGE('',*,*,#5117,.F.);
#6731=ORIENTED_EDGE('',*,*,#5115,.F.);
#6732=ORIENTED_EDGE('',*,*,#5114,.F.);
#6733=ORIENTED_EDGE('',*,*,#4952,.T.);
#6734=ORIENTED_EDGE('',*,*,#5122,.F.);
#6735=ORIENTED_EDGE('',*,*,#5123,.T.);
#6736=ORIENTED_EDGE('',*,*,#5124,.T.);
#6737=ORIENTED_EDGE('',*,*,#5125,.T.);
#6738=ORIENTED_EDGE('',*,*,#5126,.T.);
#6739=ORIENTED_EDGE('',*,*,#5127,.T.);
#6740=ORIENTED_EDGE('',*,*,#5128,.T.);
#6741=ORIENTED_EDGE('',*,*,#5129,.T.);
#6742=ORIENTED_EDGE('',*,*,#5130,.T.);
#6743=ORIENTED_EDGE('',*,*,#5127,.F.);
#6744=ORIENTED_EDGE('',*,*,#5131,.T.);
#6745=ORIENTED_EDGE('',*,*,#5132,.T.);
#6746=ORIENTED_EDGE('',*,*,#5133,.T.);
#6747=ORIENTED_EDGE('',*,*,#5134,.T.);
#6748=ORIENTED_EDGE('',*,*,#5135,.T.);
#6749=ORIENTED_EDGE('',*,*,#5129,.F.);
#6750=ORIENTED_EDGE('',*,*,#5136,.T.);
#6751=ORIENTED_EDGE('',*,*,#5137,.F.);
#6752=ORIENTED_EDGE('',*,*,#5138,.T.);
#6753=ORIENTED_EDGE('',*,*,#5132,.F.);
#6754=ORIENTED_EDGE('',*,*,#4954,.T.);
#6755=ORIENTED_EDGE('',*,*,#5139,.T.);
#6756=ORIENTED_EDGE('',*,*,#5140,.T.);
#6757=ORIENTED_EDGE('',*,*,#5134,.F.);
#6758=ORIENTED_EDGE('',*,*,#5141,.T.);
#6759=ORIENTED_EDGE('',*,*,#5142,.F.);
#6760=ORIENTED_EDGE('',*,*,#5143,.T.);
#6761=ORIENTED_EDGE('',*,*,#5139,.F.);
#6762=ORIENTED_EDGE('',*,*,#5144,.T.);
#6763=ORIENTED_EDGE('',*,*,#5145,.F.);
#6764=ORIENTED_EDGE('',*,*,#5131,.F.);
#6765=ORIENTED_EDGE('',*,*,#5130,.F.);
#6766=ORIENTED_EDGE('',*,*,#5146,.T.);
#6767=ORIENTED_EDGE('',*,*,#5147,.T.);
#6768=ORIENTED_EDGE('',*,*,#4955,.T.);
#6769=ORIENTED_EDGE('',*,*,#5135,.F.);
#6770=ORIENTED_EDGE('',*,*,#5140,.F.);
#6771=ORIENTED_EDGE('',*,*,#5148,.F.);
#6772=ORIENTED_EDGE('',*,*,#5149,.T.);
#6773=ORIENTED_EDGE('',*,*,#5146,.F.);
#6774=ORIENTED_EDGE('',*,*,#5143,.F.);
#6775=ORIENTED_EDGE('',*,*,#5150,.F.);
#6776=ORIENTED_EDGE('',*,*,#4942,.T.);
#6777=ORIENTED_EDGE('',*,*,#5148,.T.);
#6778=ORIENTED_EDGE('',*,*,#5142,.T.);
#6779=ORIENTED_EDGE('',*,*,#5151,.T.);
#6780=ORIENTED_EDGE('',*,*,#4943,.T.);
#6781=ORIENTED_EDGE('',*,*,#5150,.T.);
#6782=ORIENTED_EDGE('',*,*,#5147,.F.);
#6783=ORIENTED_EDGE('',*,*,#5152,.F.);
#6784=ORIENTED_EDGE('',*,*,#5153,.F.);
#6785=ORIENTED_EDGE('',*,*,#4957,.F.);
#6786=ORIENTED_EDGE('',*,*,#4956,.F.);
#6787=ORIENTED_EDGE('',*,*,#5149,.F.);
#6788=ORIENTED_EDGE('',*,*,#4947,.T.);
#6789=ORIENTED_EDGE('',*,*,#5154,.T.);
#6790=ORIENTED_EDGE('',*,*,#5152,.T.);
#6791=ORIENTED_EDGE('',*,*,#5145,.T.);
#6792=ORIENTED_EDGE('',*,*,#5155,.F.);
#6793=ORIENTED_EDGE('',*,*,#4944,.T.);
#6794=ORIENTED_EDGE('',*,*,#5151,.F.);
#6795=ORIENTED_EDGE('',*,*,#5156,.T.);
#6796=ORIENTED_EDGE('',*,*,#5157,.T.);
#6797=ORIENTED_EDGE('',*,*,#5158,.T.);
#6798=ORIENTED_EDGE('',*,*,#5068,.F.);
#6799=ORIENTED_EDGE('',*,*,#5159,.T.);
#6800=ORIENTED_EDGE('',*,*,#5160,.T.);
#6801=ORIENTED_EDGE('',*,*,#5161,.T.);
#6802=ORIENTED_EDGE('',*,*,#5162,.T.);
#6803=ORIENTED_EDGE('',*,*,#5161,.F.);
#6804=ORIENTED_EDGE('',*,*,#5163,.T.);
#6805=ORIENTED_EDGE('',*,*,#5164,.T.);
#6806=ORIENTED_EDGE('',*,*,#5165,.T.);
#6807=ORIENTED_EDGE('',*,*,#5166,.T.);
#6808=ORIENTED_EDGE('',*,*,#5167,.T.);
#6809=ORIENTED_EDGE('',*,*,#5159,.F.);
#6810=ORIENTED_EDGE('',*,*,#5168,.T.);
#6811=ORIENTED_EDGE('',*,*,#5164,.F.);
#6812=ORIENTED_EDGE('',*,*,#5169,.T.);
#6813=ORIENTED_EDGE('',*,*,#5157,.F.);
#6814=ORIENTED_EDGE('',*,*,#5170,.T.);
#6815=ORIENTED_EDGE('',*,*,#5171,.T.);
#6816=ORIENTED_EDGE('',*,*,#5172,.T.);
#6817=ORIENTED_EDGE('',*,*,#5166,.F.);
#6818=ORIENTED_EDGE('',*,*,#5173,.T.);
#6819=ORIENTED_EDGE('',*,*,#5160,.F.);
#6820=ORIENTED_EDGE('',*,*,#5174,.F.);
#6821=ORIENTED_EDGE('',*,*,#5175,.F.);
#6822=ORIENTED_EDGE('',*,*,#5176,.F.);
#6823=ORIENTED_EDGE('',*,*,#5177,.F.);
#6824=ORIENTED_EDGE('',*,*,#5167,.F.);
#6825=ORIENTED_EDGE('',*,*,#5172,.F.);
#6826=ORIENTED_EDGE('',*,*,#5178,.T.);
#6827=ORIENTED_EDGE('',*,*,#5174,.T.);
#6828=ORIENTED_EDGE('',*,*,#5171,.F.);
#6829=ORIENTED_EDGE('',*,*,#5179,.T.);
#6830=ORIENTED_EDGE('',*,*,#5180,.T.);
#6831=ORIENTED_EDGE('',*,*,#5181,.T.);
#6832=ORIENTED_EDGE('',*,*,#5173,.F.);
#6833=ORIENTED_EDGE('',*,*,#5182,.F.);
#6834=ORIENTED_EDGE('',*,*,#5183,.F.);
#6835=ORIENTED_EDGE('',*,*,#5179,.F.);
#6836=ORIENTED_EDGE('',*,*,#5168,.F.);
#6837=ORIENTED_EDGE('',*,*,#5162,.F.);
#6838=ORIENTED_EDGE('',*,*,#5165,.F.);
#6839=ORIENTED_EDGE('',*,*,#5184,.F.);
#6840=ORIENTED_EDGE('',*,*,#5185,.F.);
#6841=ORIENTED_EDGE('',*,*,#5186,.F.);
#6842=ORIENTED_EDGE('',*,*,#5187,.F.);
#6843=ORIENTED_EDGE('',*,*,#5182,.T.);
#6844=ORIENTED_EDGE('',*,*,#5141,.F.);
#6845=ORIENTED_EDGE('',*,*,#5188,.T.);
#6846=ORIENTED_EDGE('',*,*,#5189,.T.);
#6847=ORIENTED_EDGE('',*,*,#5190,.T.);
#6848=ORIENTED_EDGE('',*,*,#5155,.T.);
#6849=ORIENTED_EDGE('',*,*,#5144,.F.);
#6850=ORIENTED_EDGE('',*,*,#5191,.T.);
#6851=ORIENTED_EDGE('',*,*,#5192,.T.);
#6852=ORIENTED_EDGE('',*,*,#5193,.T.);
#6853=ORIENTED_EDGE('',*,*,#5036,.T.);
#6854=ORIENTED_EDGE('',*,*,#5193,.F.);
#6855=ORIENTED_EDGE('',*,*,#5194,.T.);
#6856=ORIENTED_EDGE('',*,*,#5189,.F.);
#6857=ORIENTED_EDGE('',*,*,#5195,.T.);
#6858=ORIENTED_EDGE('',*,*,#5007,.F.);
#6859=ORIENTED_EDGE('',*,*,#5021,.T.);
#6860=ORIENTED_EDGE('',*,*,#5196,.T.);
#6861=ORIENTED_EDGE('',*,*,#5038,.T.);
#6862=ORIENTED_EDGE('',*,*,#5196,.F.);
#6863=ORIENTED_EDGE('',*,*,#5197,.T.);
#6864=ORIENTED_EDGE('',*,*,#5191,.F.);
#6865=ORIENTED_EDGE('',*,*,#5039,.T.);
#6866=ORIENTED_EDGE('',*,*,#5190,.F.);
#6867=ORIENTED_EDGE('',*,*,#5198,.F.);
#6868=ORIENTED_EDGE('',*,*,#5199,.F.);
#6869=ORIENTED_EDGE('',*,*,#4945,.T.);
#6870=ORIENTED_EDGE('',*,*,#5071,.F.);
#6871=ORIENTED_EDGE('',*,*,#5095,.T.);
#6872=ORIENTED_EDGE('',*,*,#5063,.F.);
#6873=ORIENTED_EDGE('',*,*,#5200,.F.);
#6874=ORIENTED_EDGE('',*,*,#5201,.F.);
#6875=ORIENTED_EDGE('',*,*,#5202,.F.);
#6876=ORIENTED_EDGE('',*,*,#5203,.F.);
#6877=ORIENTED_EDGE('',*,*,#5204,.F.);
#6878=ORIENTED_EDGE('',*,*,#5198,.T.);
#6879=ORIENTED_EDGE('',*,*,#5194,.F.);
#6880=ORIENTED_EDGE('',*,*,#5192,.F.);
#6881=ORIENTED_EDGE('',*,*,#5197,.F.);
#6882=ORIENTED_EDGE('',*,*,#5020,.F.);
#6883=ORIENTED_EDGE('',*,*,#5205,.F.);
#6884=ORIENTED_EDGE('',*,*,#5206,.F.);
#6885=ORIENTED_EDGE('',*,*,#5207,.T.);
#6886=ORIENTED_EDGE('',*,*,#5184,.T.);
#6887=ORIENTED_EDGE('',*,*,#5170,.F.);
#6888=ORIENTED_EDGE('',*,*,#5156,.F.);
#6889=ORIENTED_EDGE('',*,*,#5208,.F.);
#6890=ORIENTED_EDGE('',*,*,#5209,.F.);
#6891=ORIENTED_EDGE('',*,*,#5210,.F.);
#6892=ORIENTED_EDGE('',*,*,#5211,.F.);
#6893=ORIENTED_EDGE('',*,*,#5062,.T.);
#6894=ORIENTED_EDGE('',*,*,#5212,.T.);
#6895=ORIENTED_EDGE('',*,*,#5213,.T.);
#6896=ORIENTED_EDGE('',*,*,#5200,.T.);
#6897=ORIENTED_EDGE('',*,*,#5214,.T.);
#6898=ORIENTED_EDGE('',*,*,#5215,.T.);
#6899=ORIENTED_EDGE('',*,*,#5216,.T.);
#6900=ORIENTED_EDGE('',*,*,#5217,.T.);
#6901=ORIENTED_EDGE('',*,*,#5060,.F.);
#6902=ORIENTED_EDGE('',*,*,#5218,.T.);
#6903=ORIENTED_EDGE('',*,*,#5219,.T.);
#6904=ORIENTED_EDGE('',*,*,#5220,.T.);
#6905=ORIENTED_EDGE('',*,*,#5219,.F.);
#6906=ORIENTED_EDGE('',*,*,#5221,.T.);
#6907=ORIENTED_EDGE('',*,*,#5216,.F.);
#6908=ORIENTED_EDGE('',*,*,#5214,.F.);
#6909=ORIENTED_EDGE('',*,*,#5222,.T.);
#6910=ORIENTED_EDGE('',*,*,#5213,.F.);
#6911=ORIENTED_EDGE('',*,*,#5222,.F.);
#6912=ORIENTED_EDGE('',*,*,#5223,.T.);
#6913=ORIENTED_EDGE('',*,*,#5224,.T.);
#6914=ORIENTED_EDGE('',*,*,#5201,.T.);
#6915=ORIENTED_EDGE('',*,*,#5217,.F.);
#6916=ORIENTED_EDGE('',*,*,#5225,.F.);
#6917=ORIENTED_EDGE('',*,*,#5226,.T.);
#6918=ORIENTED_EDGE('',*,*,#5227,.F.);
#6919=ORIENTED_EDGE('',*,*,#5223,.F.);
#6920=ORIENTED_EDGE('',*,*,#5221,.F.);
#6921=ORIENTED_EDGE('',*,*,#5228,.T.);
#6922=ORIENTED_EDGE('',*,*,#5125,.F.);
#6923=ORIENTED_EDGE('',*,*,#5229,.T.);
#6924=ORIENTED_EDGE('',*,*,#5225,.T.);
#6925=ORIENTED_EDGE('',*,*,#5230,.T.);
#6926=ORIENTED_EDGE('',*,*,#5231,.T.);
#6927=ORIENTED_EDGE('',*,*,#5232,.T.);
#6928=ORIENTED_EDGE('',*,*,#5233,.T.);
#6929=ORIENTED_EDGE('',*,*,#5234,.F.);
#6930=ORIENTED_EDGE('',*,*,#5235,.T.);
#6931=ORIENTED_EDGE('',*,*,#5236,.T.);
#6932=ORIENTED_EDGE('',*,*,#5237,.F.);
#6933=ORIENTED_EDGE('',*,*,#5238,.T.);
#6934=ORIENTED_EDGE('',*,*,#5239,.T.);
#6935=ORIENTED_EDGE('',*,*,#5031,.F.);
#6936=ORIENTED_EDGE('',*,*,#5034,.F.);
#6937=ORIENTED_EDGE('',*,*,#5240,.F.);
#6938=ORIENTED_EDGE('',*,*,#5241,.T.);
#6939=ORIENTED_EDGE('',*,*,#5118,.F.);
#6940=ORIENTED_EDGE('',*,*,#5110,.F.);
#6941=ORIENTED_EDGE('',*,*,#5104,.F.);
#6942=ORIENTED_EDGE('',*,*,#5112,.F.);
#6943=ORIENTED_EDGE('',*,*,#5126,.F.);
#6944=ORIENTED_EDGE('',*,*,#5228,.F.);
#6945=ORIENTED_EDGE('',*,*,#5218,.F.);
#6946=ORIENTED_EDGE('',*,*,#5059,.F.);
#6947=ORIENTED_EDGE('',*,*,#5242,.T.);
#6948=ORIENTED_EDGE('',*,*,#5243,.T.);
#6949=ORIENTED_EDGE('',*,*,#5244,.T.);
#6950=ORIENTED_EDGE('',*,*,#5176,.T.);
#6951=ORIENTED_EDGE('',*,*,#5245,.T.);
#6952=ORIENTED_EDGE('',*,*,#5246,.T.);
#6953=ORIENTED_EDGE('',*,*,#5247,.T.);
#6954=ORIENTED_EDGE('',*,*,#5248,.T.);
#6955=ORIENTED_EDGE('',*,*,#5249,.T.);
#6956=ORIENTED_EDGE('',*,*,#5250,.T.);
#6957=ORIENTED_EDGE('',*,*,#5202,.T.);
#6958=ORIENTED_EDGE('',*,*,#5224,.F.);
#6959=ORIENTED_EDGE('',*,*,#5251,.T.);
#6960=ORIENTED_EDGE('',*,*,#5252,.T.);
#6961=ORIENTED_EDGE('',*,*,#5203,.T.);
#6962=ORIENTED_EDGE('',*,*,#5250,.F.);
#6963=ORIENTED_EDGE('',*,*,#5253,.T.);
#6964=ORIENTED_EDGE('',*,*,#5254,.T.);
#6965=ORIENTED_EDGE('',*,*,#5255,.T.);
#6966=ORIENTED_EDGE('',*,*,#5256,.T.);
#6967=ORIENTED_EDGE('',*,*,#5199,.T.);
#6968=ORIENTED_EDGE('',*,*,#5254,.F.);
#6969=ORIENTED_EDGE('',*,*,#5204,.T.);
#6970=ORIENTED_EDGE('',*,*,#5252,.F.);
#6971=ORIENTED_EDGE('',*,*,#5257,.T.);
#6972=ORIENTED_EDGE('',*,*,#5258,.T.);
#6973=ORIENTED_EDGE('',*,*,#4946,.T.);
#6974=ORIENTED_EDGE('',*,*,#5256,.F.);
#6975=ORIENTED_EDGE('',*,*,#5259,.T.);
#6976=ORIENTED_EDGE('',*,*,#5258,.F.);
#6977=ORIENTED_EDGE('',*,*,#5260,.T.);
#6978=ORIENTED_EDGE('',*,*,#5154,.F.);
#6979=ORIENTED_EDGE('',*,*,#5253,.F.);
#6980=ORIENTED_EDGE('',*,*,#5261,.F.);
#6981=ORIENTED_EDGE('',*,*,#5262,.F.);
#6982=ORIENTED_EDGE('',*,*,#5251,.F.);
#6983=ORIENTED_EDGE('',*,*,#5227,.T.);
#6984=ORIENTED_EDGE('',*,*,#5263,.T.);
#6985=ORIENTED_EDGE('',*,*,#5261,.T.);
#6986=ORIENTED_EDGE('',*,*,#5212,.F.);
#6987=ORIENTED_EDGE('',*,*,#5061,.T.);
#6988=ORIENTED_EDGE('',*,*,#5220,.F.);
#6989=ORIENTED_EDGE('',*,*,#5215,.F.);
#6990=ORIENTED_EDGE('',*,*,#5260,.F.);
#6991=ORIENTED_EDGE('',*,*,#5264,.T.);
#6992=ORIENTED_EDGE('',*,*,#5265,.F.);
#6993=ORIENTED_EDGE('',*,*,#5121,.F.);
#6994=ORIENTED_EDGE('',*,*,#4958,.T.);
#6995=ORIENTED_EDGE('',*,*,#5153,.T.);
#6996=ORIENTED_EDGE('',*,*,#5257,.F.);
#6997=ORIENTED_EDGE('',*,*,#5262,.T.);
#6998=ORIENTED_EDGE('',*,*,#5263,.F.);
#6999=ORIENTED_EDGE('',*,*,#5226,.F.);
#7000=ORIENTED_EDGE('',*,*,#5229,.F.);
#7001=ORIENTED_EDGE('',*,*,#5124,.F.);
#7002=ORIENTED_EDGE('',*,*,#5123,.F.);
#7003=ORIENTED_EDGE('',*,*,#5111,.T.);
#7004=ORIENTED_EDGE('',*,*,#5107,.T.);
#7005=ORIENTED_EDGE('',*,*,#5119,.T.);
#7006=ORIENTED_EDGE('',*,*,#5265,.T.);
#7007=ORIENTED_EDGE('',*,*,#5264,.F.);
#7008=ORIENTED_EDGE('',*,*,#5259,.F.);
#7009=ORIENTED_EDGE('',*,*,#5255,.F.);
#7010=ORIENTED_EDGE('',*,*,#5138,.F.);
#7011=ORIENTED_EDGE('',*,*,#5266,.T.);
#7012=ORIENTED_EDGE('',*,*,#5267,.T.);
#7013=ORIENTED_EDGE('',*,*,#5268,.T.);
#7014=ORIENTED_EDGE('',*,*,#5133,.F.);
#7015=ORIENTED_EDGE('',*,*,#5267,.F.);
#7016=ORIENTED_EDGE('',*,*,#5240,.T.);
#7017=ORIENTED_EDGE('',*,*,#5033,.F.);
#7018=ORIENTED_EDGE('',*,*,#5269,.T.);
#7019=ORIENTED_EDGE('',*,*,#5029,.F.);
#7020=ORIENTED_EDGE('',*,*,#5239,.F.);
#7021=ORIENTED_EDGE('',*,*,#5098,.F.);
#7022=ORIENTED_EDGE('',*,*,#5102,.F.);
#7023=ORIENTED_EDGE('',*,*,#4983,.F.);
#7024=ORIENTED_EDGE('',*,*,#5113,.F.);
#7025=ORIENTED_EDGE('',*,*,#5241,.F.);
#7026=ORIENTED_EDGE('',*,*,#5266,.F.);
#7027=ORIENTED_EDGE('',*,*,#5137,.T.);
#7028=ORIENTED_EDGE('',*,*,#4953,.T.);
#7029=ORIENTED_EDGE('',*,*,#5270,.T.);
#7030=ORIENTED_EDGE('',*,*,#5271,.T.);
#7031=ORIENTED_EDGE('',*,*,#5272,.T.);
#7032=ORIENTED_EDGE('',*,*,#5273,.T.);
#7033=ORIENTED_EDGE('',*,*,#5206,.T.);
#7034=ORIENTED_EDGE('',*,*,#5274,.T.);
#7035=ORIENTED_EDGE('',*,*,#5237,.T.);
#7036=ORIENTED_EDGE('',*,*,#5275,.T.);
#7037=ORIENTED_EDGE('',*,*,#5270,.F.);
#7038=ORIENTED_EDGE('',*,*,#5276,.T.);
#7039=ORIENTED_EDGE('',*,*,#5235,.F.);
#7040=ORIENTED_EDGE('',*,*,#5277,.T.);
#7041=ORIENTED_EDGE('',*,*,#5278,.F.);
#7042=ORIENTED_EDGE('',*,*,#5273,.F.);
#7043=ORIENTED_EDGE('',*,*,#5279,.F.);
#7044=ORIENTED_EDGE('',*,*,#5207,.F.);
#7045=ORIENTED_EDGE('',*,*,#5275,.F.);
#7046=ORIENTED_EDGE('',*,*,#5236,.F.);
#7047=ORIENTED_EDGE('',*,*,#5276,.F.);
#7048=ORIENTED_EDGE('',*,*,#5099,.F.);
#7049=ORIENTED_EDGE('',*,*,#5238,.F.);
#7050=ORIENTED_EDGE('',*,*,#5274,.F.);
#7051=ORIENTED_EDGE('',*,*,#5205,.T.);
#7052=ORIENTED_EDGE('',*,*,#5271,.F.);
#7053=ORIENTED_EDGE('',*,*,#5278,.T.);
#7054=ORIENTED_EDGE('',*,*,#5280,.T.);
#7055=ORIENTED_EDGE('',*,*,#5281,.T.);
#7056=ORIENTED_EDGE('',*,*,#5272,.F.);
#7057=ORIENTED_EDGE('',*,*,#5281,.F.);
#7058=ORIENTED_EDGE('',*,*,#5282,.T.);
#7059=ORIENTED_EDGE('',*,*,#5185,.T.);
#7060=ORIENTED_EDGE('',*,*,#5279,.T.);
#7061=ORIENTED_EDGE('',*,*,#5277,.F.);
#7062=ORIENTED_EDGE('',*,*,#5234,.T.);
#7063=ORIENTED_EDGE('',*,*,#5283,.T.);
#7064=ORIENTED_EDGE('',*,*,#5284,.F.);
#7065=ORIENTED_EDGE('',*,*,#5285,.T.);
#7066=ORIENTED_EDGE('',*,*,#5284,.T.);
#7067=ORIENTED_EDGE('',*,*,#5286,.T.);
#7068=ORIENTED_EDGE('',*,*,#5287,.T.);
#7069=ORIENTED_EDGE('',*,*,#5288,.T.);
#7070=ORIENTED_EDGE('',*,*,#5231,.F.);
#7071=ORIENTED_EDGE('',*,*,#5289,.T.);
#7072=ORIENTED_EDGE('',*,*,#5290,.T.);
#7073=ORIENTED_EDGE('',*,*,#5291,.T.);
#7074=ORIENTED_EDGE('',*,*,#5292,.T.);
#7075=ORIENTED_EDGE('',*,*,#5293,.T.);
#7076=ORIENTED_EDGE('',*,*,#5232,.F.);
#7077=ORIENTED_EDGE('',*,*,#5293,.F.);
#7078=ORIENTED_EDGE('',*,*,#5294,.T.);
#7079=ORIENTED_EDGE('',*,*,#5291,.F.);
#7080=ORIENTED_EDGE('',*,*,#5295,.T.);
#7081=ORIENTED_EDGE('',*,*,#5296,.T.);
#7082=ORIENTED_EDGE('',*,*,#5296,.F.);
#7083=ORIENTED_EDGE('',*,*,#5297,.T.);
#7084=ORIENTED_EDGE('',*,*,#5287,.F.);
#7085=ORIENTED_EDGE('',*,*,#5298,.T.);
#7086=ORIENTED_EDGE('',*,*,#5295,.F.);
#7087=ORIENTED_EDGE('',*,*,#5299,.T.);
#7088=ORIENTED_EDGE('',*,*,#5300,.F.);
#7089=ORIENTED_EDGE('',*,*,#5301,.T.);
#7090=ORIENTED_EDGE('',*,*,#5290,.F.);
#7091=ORIENTED_EDGE('',*,*,#5289,.F.);
#7092=ORIENTED_EDGE('',*,*,#5230,.F.);
#7093=ORIENTED_EDGE('',*,*,#5302,.F.);
#7094=ORIENTED_EDGE('',*,*,#5181,.F.);
#7095=ORIENTED_EDGE('',*,*,#5299,.F.);
#7096=ORIENTED_EDGE('',*,*,#5245,.F.);
#7097=ORIENTED_EDGE('',*,*,#5175,.T.);
#7098=ORIENTED_EDGE('',*,*,#5178,.F.);
#7099=ORIENTED_EDGE('',*,*,#5302,.T.);
#7100=ORIENTED_EDGE('',*,*,#5163,.F.);
#7101=ORIENTED_EDGE('',*,*,#5177,.T.);
#7102=ORIENTED_EDGE('',*,*,#5244,.F.);
#7103=ORIENTED_EDGE('',*,*,#5303,.T.);
#7104=ORIENTED_EDGE('',*,*,#5169,.F.);
#7105=ORIENTED_EDGE('',*,*,#5282,.F.);
#7106=ORIENTED_EDGE('',*,*,#5304,.T.);
#7107=ORIENTED_EDGE('',*,*,#5305,.T.);
#7108=ORIENTED_EDGE('',*,*,#5186,.T.);
#7109=ORIENTED_EDGE('',*,*,#5306,.T.);
#7110=ORIENTED_EDGE('',*,*,#5187,.T.);
#7111=ORIENTED_EDGE('',*,*,#5305,.F.);
#7112=ORIENTED_EDGE('',*,*,#5307,.T.);
#7113=ORIENTED_EDGE('',*,*,#5308,.T.);
#7114=ORIENTED_EDGE('',*,*,#5183,.T.);
#7115=ORIENTED_EDGE('',*,*,#5306,.F.);
#7116=ORIENTED_EDGE('',*,*,#5309,.T.);
#7117=ORIENTED_EDGE('',*,*,#5308,.F.);
#7118=ORIENTED_EDGE('',*,*,#5300,.T.);
#7119=ORIENTED_EDGE('',*,*,#5180,.F.);
#7120=ORIENTED_EDGE('',*,*,#5297,.F.);
#7121=ORIENTED_EDGE('',*,*,#5301,.F.);
#7122=ORIENTED_EDGE('',*,*,#5309,.F.);
#7123=ORIENTED_EDGE('',*,*,#5307,.F.);
#7124=ORIENTED_EDGE('',*,*,#5310,.T.);
#7125=ORIENTED_EDGE('',*,*,#5288,.F.);
#7126=ORIENTED_EDGE('',*,*,#5280,.F.);
#7127=ORIENTED_EDGE('',*,*,#5285,.F.);
#7128=ORIENTED_EDGE('',*,*,#5310,.F.);
#7129=ORIENTED_EDGE('',*,*,#5304,.F.);
#7130=ORIENTED_EDGE('',*,*,#5283,.F.);
#7131=ORIENTED_EDGE('',*,*,#5233,.F.);
#7132=ORIENTED_EDGE('',*,*,#5294,.F.);
#7133=ORIENTED_EDGE('',*,*,#5311,.F.);
#7134=ORIENTED_EDGE('',*,*,#5286,.F.);
#7135=ORIENTED_EDGE('',*,*,#5096,.F.);
#7136=ORIENTED_EDGE('',*,*,#5158,.F.);
#7137=ORIENTED_EDGE('',*,*,#5303,.F.);
#7138=ORIENTED_EDGE('',*,*,#5243,.F.);
#7139=ORIENTED_EDGE('',*,*,#5089,.F.);
#7140=ORIENTED_EDGE('',*,*,#5092,.F.);
#7141=ORIENTED_EDGE('',*,*,#5094,.F.);
#7142=ORIENTED_EDGE('',*,*,#5097,.T.);
#7143=ORIENTED_EDGE('',*,*,#5242,.F.);
#7144=ORIENTED_EDGE('',*,*,#5058,.F.);
#7145=ORIENTED_EDGE('',*,*,#5052,.F.);
#7146=ORIENTED_EDGE('',*,*,#5312,.F.);
#7147=ORIENTED_EDGE('',*,*,#5128,.F.);
#7148=ORIENTED_EDGE('',*,*,#5268,.F.);
#7149=ORIENTED_EDGE('',*,*,#5269,.F.);
#7150=ORIENTED_EDGE('',*,*,#5037,.F.);
#7151=ORIENTED_EDGE('',*,*,#5195,.F.);
#7152=ORIENTED_EDGE('',*,*,#5188,.F.);
#7153=ORIENTED_EDGE('',*,*,#5136,.F.);
#7154=ORIENTED_EDGE('',*,*,#5211,.T.);
#7155=ORIENTED_EDGE('',*,*,#5313,.T.);
#7156=ORIENTED_EDGE('',*,*,#5246,.F.);
#7157=ORIENTED_EDGE('',*,*,#5313,.F.);
#7158=ORIENTED_EDGE('',*,*,#5210,.T.);
#7159=ORIENTED_EDGE('',*,*,#5314,.T.);
#7160=ORIENTED_EDGE('',*,*,#5247,.F.);
#7161=ORIENTED_EDGE('',*,*,#5314,.F.);
#7162=ORIENTED_EDGE('',*,*,#5209,.T.);
#7163=ORIENTED_EDGE('',*,*,#5315,.T.);
#7164=ORIENTED_EDGE('',*,*,#5248,.F.);
#7165=ORIENTED_EDGE('',*,*,#5315,.F.);
#7166=ORIENTED_EDGE('',*,*,#5208,.T.);
#7167=ORIENTED_EDGE('',*,*,#5316,.T.);
#7168=ORIENTED_EDGE('',*,*,#5249,.F.);
#7169=ORIENTED_EDGE('',*,*,#5316,.F.);
#7170=ORIENTED_EDGE('',*,*,#5090,.F.);
#7171=ORIENTED_EDGE('',*,*,#5312,.T.);
#7172=ORIENTED_EDGE('',*,*,#5087,.T.);
#7173=ORIENTED_EDGE('',*,*,#4985,.F.);
#7174=ORIENTED_EDGE('',*,*,#5101,.T.);
#7175=ORIENTED_EDGE('',*,*,#4990,.F.);
#7176=ORIENTED_EDGE('',*,*,#5298,.F.);
#7177=ORIENTED_EDGE('',*,*,#5311,.T.);
#7178=ORIENTED_EDGE('',*,*,#5292,.F.);
#7179=ORIENTED_EDGE('',*,*,#5317,.T.);
#7180=ORIENTED_EDGE('',*,*,#5318,.T.);
#7181=ORIENTED_EDGE('',*,*,#5319,.T.);
#7182=ORIENTED_EDGE('',*,*,#5320,.F.);
#7183=ORIENTED_EDGE('',*,*,#5321,.T.);
#7184=ORIENTED_EDGE('',*,*,#5322,.T.);
#7185=ORIENTED_EDGE('',*,*,#5323,.T.);
#7186=ORIENTED_EDGE('',*,*,#5318,.F.);
#7187=ORIENTED_EDGE('',*,*,#5324,.T.);
#7188=ORIENTED_EDGE('',*,*,#5325,.T.);
#7189=ORIENTED_EDGE('',*,*,#5326,.T.);
#7190=ORIENTED_EDGE('',*,*,#5322,.F.);
#7191=ORIENTED_EDGE('',*,*,#5327,.T.);
#7192=ORIENTED_EDGE('',*,*,#5328,.T.);
#7193=ORIENTED_EDGE('',*,*,#5329,.T.);
#7194=ORIENTED_EDGE('',*,*,#5325,.F.);
#7195=ORIENTED_EDGE('',*,*,#5330,.T.);
#7196=ORIENTED_EDGE('',*,*,#5331,.T.);
#7197=ORIENTED_EDGE('',*,*,#5332,.T.);
#7198=ORIENTED_EDGE('',*,*,#5328,.F.);
#7199=ORIENTED_EDGE('',*,*,#5333,.T.);
#7200=ORIENTED_EDGE('',*,*,#5331,.F.);
#7201=ORIENTED_EDGE('',*,*,#5334,.T.);
#7202=ORIENTED_EDGE('',*,*,#5335,.T.);
#7203=ORIENTED_EDGE('',*,*,#5336,.T.);
#7204=ORIENTED_EDGE('',*,*,#5335,.F.);
#7205=ORIENTED_EDGE('',*,*,#5337,.T.);
#7206=ORIENTED_EDGE('',*,*,#5338,.T.);
#7207=ORIENTED_EDGE('',*,*,#5339,.T.);
#7208=ORIENTED_EDGE('',*,*,#5338,.F.);
#7209=ORIENTED_EDGE('',*,*,#5340,.T.);
#7210=ORIENTED_EDGE('',*,*,#5320,.T.);
#7211=ORIENTED_EDGE('',*,*,#5333,.F.);
#7212=ORIENTED_EDGE('',*,*,#5341,.F.);
#7213=ORIENTED_EDGE('',*,*,#5342,.F.);
#7214=ORIENTED_EDGE('',*,*,#5343,.T.);
#7215=ORIENTED_EDGE('',*,*,#5336,.F.);
#7216=ORIENTED_EDGE('',*,*,#5344,.F.);
#7217=ORIENTED_EDGE('',*,*,#5345,.F.);
#7218=ORIENTED_EDGE('',*,*,#5341,.T.);
#7219=ORIENTED_EDGE('',*,*,#5339,.F.);
#7220=ORIENTED_EDGE('',*,*,#5346,.F.);
#7221=ORIENTED_EDGE('',*,*,#5347,.F.);
#7222=ORIENTED_EDGE('',*,*,#5344,.T.);
#7223=ORIENTED_EDGE('',*,*,#5319,.F.);
#7224=ORIENTED_EDGE('',*,*,#5348,.F.);
#7225=ORIENTED_EDGE('',*,*,#5349,.F.);
#7226=ORIENTED_EDGE('',*,*,#5346,.T.);
#7227=ORIENTED_EDGE('',*,*,#5317,.F.);
#7228=ORIENTED_EDGE('',*,*,#5340,.F.);
#7229=ORIENTED_EDGE('',*,*,#5337,.F.);
#7230=ORIENTED_EDGE('',*,*,#5334,.F.);
#7231=ORIENTED_EDGE('',*,*,#5330,.F.);
#7232=ORIENTED_EDGE('',*,*,#5327,.F.);
#7233=ORIENTED_EDGE('',*,*,#5324,.F.);
#7234=ORIENTED_EDGE('',*,*,#5321,.F.);
#7235=ORIENTED_EDGE('',*,*,#5350,.T.);
#7236=ORIENTED_EDGE('',*,*,#5351,.T.);
#7237=ORIENTED_EDGE('',*,*,#5352,.T.);
#7238=ORIENTED_EDGE('',*,*,#5353,.T.);
#7239=ORIENTED_EDGE('',*,*,#5354,.T.);
#7240=ORIENTED_EDGE('',*,*,#5355,.T.);
#7241=ORIENTED_EDGE('',*,*,#5356,.T.);
#7242=ORIENTED_EDGE('',*,*,#5357,.T.);
#7243=ORIENTED_EDGE('',*,*,#5358,.T.);
#7244=ORIENTED_EDGE('',*,*,#5359,.T.);
#7245=ORIENTED_EDGE('',*,*,#5360,.T.);
#7246=ORIENTED_EDGE('',*,*,#5361,.T.);
#7247=ORIENTED_EDGE('',*,*,#5362,.T.);
#7248=ORIENTED_EDGE('',*,*,#5363,.T.);
#7249=ORIENTED_EDGE('',*,*,#5364,.T.);
#7250=ORIENTED_EDGE('',*,*,#5365,.T.);
#7251=ORIENTED_EDGE('',*,*,#5366,.T.);
#7252=ORIENTED_EDGE('',*,*,#5367,.T.);
#7253=ORIENTED_EDGE('',*,*,#5368,.T.);
#7254=ORIENTED_EDGE('',*,*,#5369,.T.);
#7255=ORIENTED_EDGE('',*,*,#5368,.F.);
#7256=ORIENTED_EDGE('',*,*,#5369,.F.);
#7257=ORIENTED_EDGE('',*,*,#5370,.T.);
#7258=ORIENTED_EDGE('',*,*,#5371,.T.);
#7259=ORIENTED_EDGE('',*,*,#5370,.F.);
#7260=ORIENTED_EDGE('',*,*,#5371,.F.);
#7261=ORIENTED_EDGE('',*,*,#5372,.T.);
#7262=ORIENTED_EDGE('',*,*,#5367,.F.);
#7263=ORIENTED_EDGE('',*,*,#5372,.F.);
#7264=ORIENTED_EDGE('',*,*,#5373,.T.);
#7265=ORIENTED_EDGE('',*,*,#5374,.T.);
#7266=ORIENTED_EDGE('',*,*,#5373,.F.);
#7267=ORIENTED_EDGE('',*,*,#5374,.F.);
#7268=ORIENTED_EDGE('',*,*,#5375,.T.);
#7269=ORIENTED_EDGE('',*,*,#5376,.T.);
#7270=ORIENTED_EDGE('',*,*,#5375,.F.);
#7271=ORIENTED_EDGE('',*,*,#5376,.F.);
#7272=ORIENTED_EDGE('',*,*,#5377,.T.);
#7273=ORIENTED_EDGE('',*,*,#5366,.F.);
#7274=ORIENTED_EDGE('',*,*,#5377,.F.);
#7275=ORIENTED_EDGE('',*,*,#5378,.T.);
#7276=ORIENTED_EDGE('',*,*,#5379,.T.);
#7277=ORIENTED_EDGE('',*,*,#5378,.F.);
#7278=ORIENTED_EDGE('',*,*,#5379,.F.);
#7279=ORIENTED_EDGE('',*,*,#5380,.T.);
#7280=ORIENTED_EDGE('',*,*,#5381,.T.);
#7281=ORIENTED_EDGE('',*,*,#5380,.F.);
#7282=ORIENTED_EDGE('',*,*,#5381,.F.);
#7283=ORIENTED_EDGE('',*,*,#5382,.T.);
#7284=ORIENTED_EDGE('',*,*,#5365,.F.);
#7285=ORIENTED_EDGE('',*,*,#5382,.F.);
#7286=ORIENTED_EDGE('',*,*,#5383,.T.);
#7287=ORIENTED_EDGE('',*,*,#5384,.T.);
#7288=ORIENTED_EDGE('',*,*,#5383,.F.);
#7289=ORIENTED_EDGE('',*,*,#5384,.F.);
#7290=ORIENTED_EDGE('',*,*,#5385,.T.);
#7291=ORIENTED_EDGE('',*,*,#5386,.T.);
#7292=ORIENTED_EDGE('',*,*,#5385,.F.);
#7293=ORIENTED_EDGE('',*,*,#5386,.F.);
#7294=ORIENTED_EDGE('',*,*,#5387,.T.);
#7295=ORIENTED_EDGE('',*,*,#5364,.F.);
#7296=ORIENTED_EDGE('',*,*,#5387,.F.);
#7297=ORIENTED_EDGE('',*,*,#5388,.T.);
#7298=ORIENTED_EDGE('',*,*,#5389,.T.);
#7299=ORIENTED_EDGE('',*,*,#5388,.F.);
#7300=ORIENTED_EDGE('',*,*,#5389,.F.);
#7301=ORIENTED_EDGE('',*,*,#5390,.T.);
#7302=ORIENTED_EDGE('',*,*,#5391,.F.);
#7303=ORIENTED_EDGE('',*,*,#5390,.F.);
#7304=ORIENTED_EDGE('',*,*,#5392,.T.);
#7305=ORIENTED_EDGE('',*,*,#5393,.T.);
#7306=ORIENTED_EDGE('',*,*,#5392,.F.);
#7307=ORIENTED_EDGE('',*,*,#5393,.F.);
#7308=ORIENTED_EDGE('',*,*,#5394,.T.);
#7309=ORIENTED_EDGE('',*,*,#5395,.F.);
#7310=ORIENTED_EDGE('',*,*,#5394,.F.);
#7311=ORIENTED_EDGE('',*,*,#5396,.F.);
#7312=ORIENTED_EDGE('',*,*,#5397,.T.);
#7313=ORIENTED_EDGE('',*,*,#5363,.F.);
#7314=ORIENTED_EDGE('',*,*,#5397,.F.);
#7315=ORIENTED_EDGE('',*,*,#5398,.F.);
#7316=ORIENTED_EDGE('',*,*,#5399,.T.);
#7317=ORIENTED_EDGE('',*,*,#5362,.F.);
#7318=ORIENTED_EDGE('',*,*,#5399,.F.);
#7319=ORIENTED_EDGE('',*,*,#5400,.F.);
#7320=ORIENTED_EDGE('',*,*,#5401,.T.);
#7321=ORIENTED_EDGE('',*,*,#5402,.F.);
#7322=ORIENTED_EDGE('',*,*,#5401,.F.);
#7323=ORIENTED_EDGE('',*,*,#5350,.F.);
#7324=ORIENTED_EDGE('',*,*,#5403,.T.);
#7325=ORIENTED_EDGE('',*,*,#5404,.T.);
#7326=ORIENTED_EDGE('',*,*,#5405,.F.);
#7327=ORIENTED_EDGE('',*,*,#5361,.F.);
#7328=ORIENTED_EDGE('',*,*,#5406,.T.);
#7329=ORIENTED_EDGE('',*,*,#5407,.T.);
#7330=ORIENTED_EDGE('',*,*,#5403,.F.);
#7331=ORIENTED_EDGE('',*,*,#5360,.F.);
#7332=ORIENTED_EDGE('',*,*,#5408,.T.);
#7333=ORIENTED_EDGE('',*,*,#5409,.T.);
#7334=ORIENTED_EDGE('',*,*,#5406,.F.);
#7335=ORIENTED_EDGE('',*,*,#5359,.F.);
#7336=ORIENTED_EDGE('',*,*,#5410,.T.);
#7337=ORIENTED_EDGE('',*,*,#5411,.T.);
#7338=ORIENTED_EDGE('',*,*,#5408,.F.);
#7339=ORIENTED_EDGE('',*,*,#5402,.T.);
#7340=ORIENTED_EDGE('',*,*,#5358,.F.);
#7341=ORIENTED_EDGE('',*,*,#5412,.T.);
#7342=ORIENTED_EDGE('',*,*,#5413,.T.);
#7343=ORIENTED_EDGE('',*,*,#5410,.F.);
#7344=ORIENTED_EDGE('',*,*,#5357,.F.);
#7345=ORIENTED_EDGE('',*,*,#5414,.T.);
#7346=ORIENTED_EDGE('',*,*,#5415,.T.);
#7347=ORIENTED_EDGE('',*,*,#5412,.F.);
#7348=ORIENTED_EDGE('',*,*,#5356,.F.);
#7349=ORIENTED_EDGE('',*,*,#5416,.T.);
#7350=ORIENTED_EDGE('',*,*,#5417,.T.);
#7351=ORIENTED_EDGE('',*,*,#5414,.F.);
#7352=ORIENTED_EDGE('',*,*,#5355,.F.);
#7353=ORIENTED_EDGE('',*,*,#5418,.T.);
#7354=ORIENTED_EDGE('',*,*,#5419,.T.);
#7355=ORIENTED_EDGE('',*,*,#5416,.F.);
#7356=ORIENTED_EDGE('',*,*,#5354,.F.);
#7357=ORIENTED_EDGE('',*,*,#5420,.T.);
#7358=ORIENTED_EDGE('',*,*,#5421,.T.);
#7359=ORIENTED_EDGE('',*,*,#5418,.F.);
#7360=ORIENTED_EDGE('',*,*,#5353,.F.);
#7361=ORIENTED_EDGE('',*,*,#5422,.T.);
#7362=ORIENTED_EDGE('',*,*,#5423,.T.);
#7363=ORIENTED_EDGE('',*,*,#5420,.F.);
#7364=ORIENTED_EDGE('',*,*,#5352,.F.);
#7365=ORIENTED_EDGE('',*,*,#5424,.T.);
#7366=ORIENTED_EDGE('',*,*,#5425,.T.);
#7367=ORIENTED_EDGE('',*,*,#5422,.F.);
#7368=ORIENTED_EDGE('',*,*,#5351,.F.);
#7369=ORIENTED_EDGE('',*,*,#5405,.T.);
#7370=ORIENTED_EDGE('',*,*,#5426,.T.);
#7371=ORIENTED_EDGE('',*,*,#5424,.F.);
#7372=ORIENTED_EDGE('',*,*,#5426,.F.);
#7373=ORIENTED_EDGE('',*,*,#5404,.F.);
#7374=ORIENTED_EDGE('',*,*,#5407,.F.);
#7375=ORIENTED_EDGE('',*,*,#5409,.F.);
#7376=ORIENTED_EDGE('',*,*,#5411,.F.);
#7377=ORIENTED_EDGE('',*,*,#5413,.F.);
#7378=ORIENTED_EDGE('',*,*,#5415,.F.);
#7379=ORIENTED_EDGE('',*,*,#5417,.F.);
#7380=ORIENTED_EDGE('',*,*,#5419,.F.);
#7381=ORIENTED_EDGE('',*,*,#5421,.F.);
#7382=ORIENTED_EDGE('',*,*,#5423,.F.);
#7383=ORIENTED_EDGE('',*,*,#5425,.F.);
#7384=ORIENTED_EDGE('',*,*,#5323,.F.);
#7385=ORIENTED_EDGE('',*,*,#5427,.F.);
#7386=ORIENTED_EDGE('',*,*,#5428,.F.);
#7387=ORIENTED_EDGE('',*,*,#5348,.T.);
#7388=ORIENTED_EDGE('',*,*,#5326,.F.);
#7389=ORIENTED_EDGE('',*,*,#5429,.F.);
#7390=ORIENTED_EDGE('',*,*,#5430,.F.);
#7391=ORIENTED_EDGE('',*,*,#5427,.T.);
#7392=ORIENTED_EDGE('',*,*,#5400,.T.);
#7393=ORIENTED_EDGE('',*,*,#5329,.F.);
#7394=ORIENTED_EDGE('',*,*,#5431,.F.);
#7395=ORIENTED_EDGE('',*,*,#5432,.F.);
#7396=ORIENTED_EDGE('',*,*,#5429,.T.);
#7397=ORIENTED_EDGE('',*,*,#5332,.F.);
#7398=ORIENTED_EDGE('',*,*,#5343,.F.);
#7399=ORIENTED_EDGE('',*,*,#5433,.F.);
#7400=ORIENTED_EDGE('',*,*,#5431,.T.);
#7401=ORIENTED_EDGE('',*,*,#5433,.T.);
#7402=ORIENTED_EDGE('',*,*,#5342,.T.);
#7403=ORIENTED_EDGE('',*,*,#5345,.T.);
#7404=ORIENTED_EDGE('',*,*,#5347,.T.);
#7405=ORIENTED_EDGE('',*,*,#5349,.T.);
#7406=ORIENTED_EDGE('',*,*,#5428,.T.);
#7407=ORIENTED_EDGE('',*,*,#5430,.T.);
#7408=ORIENTED_EDGE('',*,*,#5432,.T.);
#7409=ORIENTED_EDGE('',*,*,#5391,.T.);
#7410=ORIENTED_EDGE('',*,*,#5395,.T.);
#7411=ORIENTED_EDGE('',*,*,#5396,.T.);
#7412=ORIENTED_EDGE('',*,*,#5398,.T.);
#7413=ORIENTED_EDGE('',*,*,#5434,.T.);
#7414=ORIENTED_EDGE('',*,*,#5435,.T.);
#7415=ORIENTED_EDGE('',*,*,#5436,.T.);
#7416=ORIENTED_EDGE('',*,*,#5437,.T.);
#7417=ORIENTED_EDGE('',*,*,#5435,.F.);
#7418=ORIENTED_EDGE('',*,*,#5438,.F.);
#7419=ORIENTED_EDGE('',*,*,#5439,.F.);
#7420=ORIENTED_EDGE('',*,*,#5440,.F.);
#7421=ORIENTED_EDGE('',*,*,#5441,.T.);
#7422=ORIENTED_EDGE('',*,*,#5442,.T.);
#7423=ORIENTED_EDGE('',*,*,#5443,.T.);
#7424=ORIENTED_EDGE('',*,*,#5444,.T.);
#7425=ORIENTED_EDGE('',*,*,#5437,.F.);
#7426=ORIENTED_EDGE('',*,*,#5445,.F.);
#7427=ORIENTED_EDGE('',*,*,#5442,.F.);
#7428=ORIENTED_EDGE('',*,*,#5446,.F.);
#7429=ORIENTED_EDGE('',*,*,#5447,.T.);
#7430=ORIENTED_EDGE('',*,*,#5448,.T.);
#7431=ORIENTED_EDGE('',*,*,#5449,.T.);
#7432=ORIENTED_EDGE('',*,*,#5439,.T.);
#7433=ORIENTED_EDGE('',*,*,#5448,.F.);
#7434=ORIENTED_EDGE('',*,*,#5450,.F.);
#7435=ORIENTED_EDGE('',*,*,#5451,.F.);
#7436=ORIENTED_EDGE('',*,*,#5452,.F.);
#7437=ORIENTED_EDGE('',*,*,#5453,.T.);
#7438=ORIENTED_EDGE('',*,*,#5454,.T.);
#7439=ORIENTED_EDGE('',*,*,#5455,.T.);
#7440=ORIENTED_EDGE('',*,*,#5451,.T.);
#7441=ORIENTED_EDGE('',*,*,#5444,.F.);
#7442=ORIENTED_EDGE('',*,*,#5456,.F.);
#7443=ORIENTED_EDGE('',*,*,#5454,.F.);
#7444=ORIENTED_EDGE('',*,*,#5457,.F.);
#7445=ORIENTED_EDGE('',*,*,#5458,.T.);
#7446=ORIENTED_EDGE('',*,*,#5459,.T.);
#7447=ORIENTED_EDGE('',*,*,#5460,.T.);
#7448=ORIENTED_EDGE('',*,*,#5461,.T.);
#7449=ORIENTED_EDGE('',*,*,#5459,.F.);
#7450=ORIENTED_EDGE('',*,*,#5462,.F.);
#7451=ORIENTED_EDGE('',*,*,#5463,.F.);
#7452=ORIENTED_EDGE('',*,*,#5464,.F.);
#7453=ORIENTED_EDGE('',*,*,#5465,.T.);
#7454=ORIENTED_EDGE('',*,*,#5466,.T.);
#7455=ORIENTED_EDGE('',*,*,#5467,.T.);
#7456=ORIENTED_EDGE('',*,*,#5468,.T.);
#7457=ORIENTED_EDGE('',*,*,#5461,.F.);
#7458=ORIENTED_EDGE('',*,*,#5469,.F.);
#7459=ORIENTED_EDGE('',*,*,#5466,.F.);
#7460=ORIENTED_EDGE('',*,*,#5470,.F.);
#7461=ORIENTED_EDGE('',*,*,#5471,.T.);
#7462=ORIENTED_EDGE('',*,*,#5472,.T.);
#7463=ORIENTED_EDGE('',*,*,#5473,.T.);
#7464=ORIENTED_EDGE('',*,*,#5463,.T.);
#7465=ORIENTED_EDGE('',*,*,#5472,.F.);
#7466=ORIENTED_EDGE('',*,*,#5474,.F.);
#7467=ORIENTED_EDGE('',*,*,#5475,.F.);
#7468=ORIENTED_EDGE('',*,*,#5476,.F.);
#7469=ORIENTED_EDGE('',*,*,#5477,.T.);
#7470=ORIENTED_EDGE('',*,*,#5478,.T.);
#7471=ORIENTED_EDGE('',*,*,#5479,.T.);
#7472=ORIENTED_EDGE('',*,*,#5475,.T.);
#7473=ORIENTED_EDGE('',*,*,#5468,.F.);
#7474=ORIENTED_EDGE('',*,*,#5480,.F.);
#7475=ORIENTED_EDGE('',*,*,#5478,.F.);
#7476=ORIENTED_EDGE('',*,*,#5481,.F.);
#7477=ORIENTED_EDGE('',*,*,#5482,.T.);
#7478=ORIENTED_EDGE('',*,*,#5483,.T.);
#7479=ORIENTED_EDGE('',*,*,#5484,.T.);
#7480=ORIENTED_EDGE('',*,*,#5485,.T.);
#7481=ORIENTED_EDGE('',*,*,#5483,.F.);
#7482=ORIENTED_EDGE('',*,*,#5486,.F.);
#7483=ORIENTED_EDGE('',*,*,#5487,.F.);
#7484=ORIENTED_EDGE('',*,*,#5488,.F.);
#7485=ORIENTED_EDGE('',*,*,#5489,.T.);
#7486=ORIENTED_EDGE('',*,*,#5490,.T.);
#7487=ORIENTED_EDGE('',*,*,#5491,.T.);
#7488=ORIENTED_EDGE('',*,*,#5492,.T.);
#7489=ORIENTED_EDGE('',*,*,#5485,.F.);
#7490=ORIENTED_EDGE('',*,*,#5493,.F.);
#7491=ORIENTED_EDGE('',*,*,#5490,.F.);
#7492=ORIENTED_EDGE('',*,*,#5494,.F.);
#7493=ORIENTED_EDGE('',*,*,#5495,.T.);
#7494=ORIENTED_EDGE('',*,*,#5496,.T.);
#7495=ORIENTED_EDGE('',*,*,#5497,.T.);
#7496=ORIENTED_EDGE('',*,*,#5487,.T.);
#7497=ORIENTED_EDGE('',*,*,#5496,.F.);
#7498=ORIENTED_EDGE('',*,*,#5498,.F.);
#7499=ORIENTED_EDGE('',*,*,#5499,.F.);
#7500=ORIENTED_EDGE('',*,*,#5500,.F.);
#7501=ORIENTED_EDGE('',*,*,#5501,.T.);
#7502=ORIENTED_EDGE('',*,*,#5502,.T.);
#7503=ORIENTED_EDGE('',*,*,#5503,.T.);
#7504=ORIENTED_EDGE('',*,*,#5499,.T.);
#7505=ORIENTED_EDGE('',*,*,#5492,.F.);
#7506=ORIENTED_EDGE('',*,*,#5504,.F.);
#7507=ORIENTED_EDGE('',*,*,#5502,.F.);
#7508=ORIENTED_EDGE('',*,*,#5505,.F.);
#7509=ORIENTED_EDGE('',*,*,#5506,.F.);
#7510=ORIENTED_EDGE('',*,*,#5507,.T.);
#7511=ORIENTED_EDGE('',*,*,#5508,.F.);
#7512=ORIENTED_EDGE('',*,*,#5507,.F.);
#7513=ORIENTED_EDGE('',*,*,#5509,.F.);
#7514=ORIENTED_EDGE('',*,*,#5510,.T.);
#7515=ORIENTED_EDGE('',*,*,#5511,.F.);
#7516=ORIENTED_EDGE('',*,*,#5510,.F.);
#7517=ORIENTED_EDGE('',*,*,#5512,.F.);
#7518=ORIENTED_EDGE('',*,*,#5513,.T.);
#7519=ORIENTED_EDGE('',*,*,#5514,.F.);
#7520=ORIENTED_EDGE('',*,*,#5513,.F.);
#7521=ORIENTED_EDGE('',*,*,#5515,.F.);
#7522=ORIENTED_EDGE('',*,*,#5516,.T.);
#7523=ORIENTED_EDGE('',*,*,#5517,.F.);
#7524=ORIENTED_EDGE('',*,*,#5516,.F.);
#7525=ORIENTED_EDGE('',*,*,#5518,.F.);
#7526=ORIENTED_EDGE('',*,*,#5519,.T.);
#7527=ORIENTED_EDGE('',*,*,#5520,.F.);
#7528=ORIENTED_EDGE('',*,*,#5519,.F.);
#7529=ORIENTED_EDGE('',*,*,#5521,.F.);
#7530=ORIENTED_EDGE('',*,*,#5522,.T.);
#7531=ORIENTED_EDGE('',*,*,#5523,.F.);
#7532=ORIENTED_EDGE('',*,*,#5522,.F.);
#7533=ORIENTED_EDGE('',*,*,#5524,.F.);
#7534=ORIENTED_EDGE('',*,*,#5525,.T.);
#7535=ORIENTED_EDGE('',*,*,#5526,.F.);
#7536=ORIENTED_EDGE('',*,*,#5527,.F.);
#7537=ORIENTED_EDGE('',*,*,#5528,.F.);
#7538=ORIENTED_EDGE('',*,*,#5527,.T.);
#7539=ORIENTED_EDGE('',*,*,#5529,.F.);
#7540=ORIENTED_EDGE('',*,*,#5530,.F.);
#7541=ORIENTED_EDGE('',*,*,#5531,.F.);
#7542=ORIENTED_EDGE('',*,*,#5530,.T.);
#7543=ORIENTED_EDGE('',*,*,#5532,.F.);
#7544=ORIENTED_EDGE('',*,*,#5533,.F.);
#7545=ORIENTED_EDGE('',*,*,#5534,.F.);
#7546=ORIENTED_EDGE('',*,*,#5533,.T.);
#7547=ORIENTED_EDGE('',*,*,#5535,.F.);
#7548=ORIENTED_EDGE('',*,*,#5536,.F.);
#7549=ORIENTED_EDGE('',*,*,#5537,.F.);
#7550=ORIENTED_EDGE('',*,*,#5536,.T.);
#7551=ORIENTED_EDGE('',*,*,#5538,.F.);
#7552=ORIENTED_EDGE('',*,*,#5539,.F.);
#7553=ORIENTED_EDGE('',*,*,#5540,.F.);
#7554=ORIENTED_EDGE('',*,*,#5539,.T.);
#7555=ORIENTED_EDGE('',*,*,#5541,.F.);
#7556=ORIENTED_EDGE('',*,*,#5542,.F.);
#7557=ORIENTED_EDGE('',*,*,#5543,.F.);
#7558=ORIENTED_EDGE('',*,*,#5542,.T.);
#7559=ORIENTED_EDGE('',*,*,#5544,.F.);
#7560=ORIENTED_EDGE('',*,*,#5545,.F.);
#7561=ORIENTED_EDGE('',*,*,#5546,.F.);
#7562=ORIENTED_EDGE('',*,*,#5545,.T.);
#7563=ORIENTED_EDGE('',*,*,#5547,.F.);
#7564=ORIENTED_EDGE('',*,*,#5525,.F.);
#7565=ORIENTED_EDGE('',*,*,#5547,.T.);
#7566=ORIENTED_EDGE('',*,*,#5544,.T.);
#7567=ORIENTED_EDGE('',*,*,#5541,.T.);
#7568=ORIENTED_EDGE('',*,*,#5538,.T.);
#7569=ORIENTED_EDGE('',*,*,#5535,.T.);
#7570=ORIENTED_EDGE('',*,*,#5532,.T.);
#7571=ORIENTED_EDGE('',*,*,#5529,.T.);
#7572=ORIENTED_EDGE('',*,*,#5526,.T.);
#7573=ORIENTED_EDGE('',*,*,#5508,.T.);
#7574=ORIENTED_EDGE('',*,*,#5511,.T.);
#7575=ORIENTED_EDGE('',*,*,#5514,.T.);
#7576=ORIENTED_EDGE('',*,*,#5517,.T.);
#7577=ORIENTED_EDGE('',*,*,#5520,.T.);
#7578=ORIENTED_EDGE('',*,*,#5523,.T.);
#7579=ORIENTED_EDGE('',*,*,#5452,.T.);
#7580=ORIENTED_EDGE('',*,*,#5455,.F.);
#7581=ORIENTED_EDGE('',*,*,#5456,.T.);
#7582=ORIENTED_EDGE('',*,*,#5443,.F.);
#7583=ORIENTED_EDGE('',*,*,#5445,.T.);
#7584=ORIENTED_EDGE('',*,*,#5436,.F.);
#7585=ORIENTED_EDGE('',*,*,#5440,.T.);
#7586=ORIENTED_EDGE('',*,*,#5449,.F.);
#7587=ORIENTED_EDGE('',*,*,#5476,.T.);
#7588=ORIENTED_EDGE('',*,*,#5479,.F.);
#7589=ORIENTED_EDGE('',*,*,#5480,.T.);
#7590=ORIENTED_EDGE('',*,*,#5467,.F.);
#7591=ORIENTED_EDGE('',*,*,#5469,.T.);
#7592=ORIENTED_EDGE('',*,*,#5460,.F.);
#7593=ORIENTED_EDGE('',*,*,#5464,.T.);
#7594=ORIENTED_EDGE('',*,*,#5473,.F.);
#7595=ORIENTED_EDGE('',*,*,#5500,.T.);
#7596=ORIENTED_EDGE('',*,*,#5503,.F.);
#7597=ORIENTED_EDGE('',*,*,#5504,.T.);
#7598=ORIENTED_EDGE('',*,*,#5491,.F.);
#7599=ORIENTED_EDGE('',*,*,#5493,.T.);
#7600=ORIENTED_EDGE('',*,*,#5484,.F.);
#7601=ORIENTED_EDGE('',*,*,#5488,.T.);
#7602=ORIENTED_EDGE('',*,*,#5497,.F.);
#7603=ORIENTED_EDGE('',*,*,#5546,.T.);
#7604=ORIENTED_EDGE('',*,*,#5524,.T.);
#7605=ORIENTED_EDGE('',*,*,#5528,.T.);
#7606=ORIENTED_EDGE('',*,*,#5531,.T.);
#7607=ORIENTED_EDGE('',*,*,#5534,.T.);
#7608=ORIENTED_EDGE('',*,*,#5537,.T.);
#7609=ORIENTED_EDGE('',*,*,#5540,.T.);
#7610=ORIENTED_EDGE('',*,*,#5543,.T.);
#7611=ORIENTED_EDGE('',*,*,#5506,.T.);
#7612=ORIENTED_EDGE('',*,*,#5509,.T.);
#7613=ORIENTED_EDGE('',*,*,#5512,.T.);
#7614=ORIENTED_EDGE('',*,*,#5515,.T.);
#7615=ORIENTED_EDGE('',*,*,#5518,.T.);
#7616=ORIENTED_EDGE('',*,*,#5521,.T.);
#7617=ORIENTED_EDGE('',*,*,#5450,.T.);
#7618=ORIENTED_EDGE('',*,*,#5447,.F.);
#7619=ORIENTED_EDGE('',*,*,#5438,.T.);
#7620=ORIENTED_EDGE('',*,*,#5434,.F.);
#7621=ORIENTED_EDGE('',*,*,#5446,.T.);
#7622=ORIENTED_EDGE('',*,*,#5441,.F.);
#7623=ORIENTED_EDGE('',*,*,#5457,.T.);
#7624=ORIENTED_EDGE('',*,*,#5453,.F.);
#7625=ORIENTED_EDGE('',*,*,#5474,.T.);
#7626=ORIENTED_EDGE('',*,*,#5471,.F.);
#7627=ORIENTED_EDGE('',*,*,#5462,.T.);
#7628=ORIENTED_EDGE('',*,*,#5458,.F.);
#7629=ORIENTED_EDGE('',*,*,#5470,.T.);
#7630=ORIENTED_EDGE('',*,*,#5465,.F.);
#7631=ORIENTED_EDGE('',*,*,#5481,.T.);
#7632=ORIENTED_EDGE('',*,*,#5477,.F.);
#7633=ORIENTED_EDGE('',*,*,#5498,.T.);
#7634=ORIENTED_EDGE('',*,*,#5495,.F.);
#7635=ORIENTED_EDGE('',*,*,#5486,.T.);
#7636=ORIENTED_EDGE('',*,*,#5482,.F.);
#7637=ORIENTED_EDGE('',*,*,#5494,.T.);
#7638=ORIENTED_EDGE('',*,*,#5489,.F.);
#7639=ORIENTED_EDGE('',*,*,#5505,.T.);
#7640=ORIENTED_EDGE('',*,*,#5501,.F.);
#7641=ORIENTED_EDGE('',*,*,#5548,.T.);
#7642=ORIENTED_EDGE('',*,*,#5549,.T.);
#7643=ORIENTED_EDGE('',*,*,#5550,.T.);
#7644=ORIENTED_EDGE('',*,*,#5551,.F.);
#7645=ORIENTED_EDGE('',*,*,#5552,.T.);
#7646=ORIENTED_EDGE('',*,*,#5553,.T.);
#7647=ORIENTED_EDGE('',*,*,#5554,.T.);
#7648=ORIENTED_EDGE('',*,*,#5549,.F.);
#7649=ORIENTED_EDGE('',*,*,#5555,.T.);
#7650=ORIENTED_EDGE('',*,*,#5556,.T.);
#7651=ORIENTED_EDGE('',*,*,#5557,.T.);
#7652=ORIENTED_EDGE('',*,*,#5553,.F.);
#7653=ORIENTED_EDGE('',*,*,#5558,.T.);
#7654=ORIENTED_EDGE('',*,*,#5559,.T.);
#7655=ORIENTED_EDGE('',*,*,#5560,.T.);
#7656=ORIENTED_EDGE('',*,*,#5556,.F.);
#7657=ORIENTED_EDGE('',*,*,#5561,.T.);
#7658=ORIENTED_EDGE('',*,*,#5559,.F.);
#7659=ORIENTED_EDGE('',*,*,#5562,.T.);
#7660=ORIENTED_EDGE('',*,*,#5563,.T.);
#7661=ORIENTED_EDGE('',*,*,#5564,.T.);
#7662=ORIENTED_EDGE('',*,*,#5563,.F.);
#7663=ORIENTED_EDGE('',*,*,#5565,.T.);
#7664=ORIENTED_EDGE('',*,*,#5551,.T.);
#7665=ORIENTED_EDGE('',*,*,#5561,.F.);
#7666=ORIENTED_EDGE('',*,*,#5566,.F.);
#7667=ORIENTED_EDGE('',*,*,#5567,.T.);
#7668=ORIENTED_EDGE('',*,*,#5568,.T.);
#7669=ORIENTED_EDGE('',*,*,#5564,.F.);
#7670=ORIENTED_EDGE('',*,*,#5569,.F.);
#7671=ORIENTED_EDGE('',*,*,#5570,.T.);
#7672=ORIENTED_EDGE('',*,*,#5566,.T.);
#7673=ORIENTED_EDGE('',*,*,#5550,.F.);
#7674=ORIENTED_EDGE('',*,*,#5571,.F.);
#7675=ORIENTED_EDGE('',*,*,#5572,.T.);
#7676=ORIENTED_EDGE('',*,*,#5569,.T.);
#7677=ORIENTED_EDGE('',*,*,#5548,.F.);
#7678=ORIENTED_EDGE('',*,*,#5565,.F.);
#7679=ORIENTED_EDGE('',*,*,#5562,.F.);
#7680=ORIENTED_EDGE('',*,*,#5558,.F.);
#7681=ORIENTED_EDGE('',*,*,#5555,.F.);
#7682=ORIENTED_EDGE('',*,*,#5552,.F.);
#7683=ORIENTED_EDGE('',*,*,#5573,.T.);
#7684=ORIENTED_EDGE('',*,*,#5574,.T.);
#7685=ORIENTED_EDGE('',*,*,#5575,.T.);
#7686=ORIENTED_EDGE('',*,*,#5576,.T.);
#7687=ORIENTED_EDGE('',*,*,#5577,.F.);
#7688=ORIENTED_EDGE('',*,*,#5578,.T.);
#7689=ORIENTED_EDGE('',*,*,#5576,.F.);
#7690=ORIENTED_EDGE('',*,*,#5578,.F.);
#7691=ORIENTED_EDGE('',*,*,#5579,.F.);
#7692=ORIENTED_EDGE('',*,*,#5580,.T.);
#7693=ORIENTED_EDGE('',*,*,#5575,.F.);
#7694=ORIENTED_EDGE('',*,*,#5580,.F.);
#7695=ORIENTED_EDGE('',*,*,#5581,.F.);
#7696=ORIENTED_EDGE('',*,*,#5582,.T.);
#7697=ORIENTED_EDGE('',*,*,#5574,.F.);
#7698=ORIENTED_EDGE('',*,*,#5582,.F.);
#7699=ORIENTED_EDGE('',*,*,#5583,.F.);
#7700=ORIENTED_EDGE('',*,*,#5584,.T.);
#7701=ORIENTED_EDGE('',*,*,#5573,.F.);
#7702=ORIENTED_EDGE('',*,*,#5584,.F.);
#7703=ORIENTED_EDGE('',*,*,#5554,.F.);
#7704=ORIENTED_EDGE('',*,*,#5585,.F.);
#7705=ORIENTED_EDGE('',*,*,#5586,.T.);
#7706=ORIENTED_EDGE('',*,*,#5571,.T.);
#7707=ORIENTED_EDGE('',*,*,#5557,.F.);
#7708=ORIENTED_EDGE('',*,*,#5587,.F.);
#7709=ORIENTED_EDGE('',*,*,#5588,.T.);
#7710=ORIENTED_EDGE('',*,*,#5585,.T.);
#7711=ORIENTED_EDGE('',*,*,#5560,.F.);
#7712=ORIENTED_EDGE('',*,*,#5568,.F.);
#7713=ORIENTED_EDGE('',*,*,#5589,.T.);
#7714=ORIENTED_EDGE('',*,*,#5587,.T.);
#7715=ORIENTED_EDGE('',*,*,#5589,.F.);
#7716=ORIENTED_EDGE('',*,*,#5567,.F.);
#7717=ORIENTED_EDGE('',*,*,#5570,.F.);
#7718=ORIENTED_EDGE('',*,*,#5572,.F.);
#7719=ORIENTED_EDGE('',*,*,#5586,.F.);
#7720=ORIENTED_EDGE('',*,*,#5588,.F.);
#7721=ORIENTED_EDGE('',*,*,#5577,.T.);
#7722=ORIENTED_EDGE('',*,*,#5579,.T.);
#7723=ORIENTED_EDGE('',*,*,#5581,.T.);
#7724=ORIENTED_EDGE('',*,*,#5583,.T.);
#7725=ORIENTED_EDGE('',*,*,#5590,.T.);
#7726=ORIENTED_EDGE('',*,*,#5591,.T.);
#7727=ORIENTED_EDGE('',*,*,#5592,.T.);
#7728=ORIENTED_EDGE('',*,*,#5593,.T.);
#7729=ORIENTED_EDGE('',*,*,#5594,.T.);
#7730=ORIENTED_EDGE('',*,*,#5595,.T.);
#7731=ORIENTED_EDGE('',*,*,#5596,.T.);
#7732=ORIENTED_EDGE('',*,*,#5597,.T.);
#7733=ORIENTED_EDGE('',*,*,#5598,.T.);
#7734=ORIENTED_EDGE('',*,*,#5599,.T.);
#7735=ORIENTED_EDGE('',*,*,#5600,.T.);
#7736=ORIENTED_EDGE('',*,*,#5601,.T.);
#7737=ORIENTED_EDGE('',*,*,#5602,.T.);
#7738=ORIENTED_EDGE('',*,*,#5603,.T.);
#7739=ORIENTED_EDGE('',*,*,#5604,.T.);
#7740=ORIENTED_EDGE('',*,*,#5605,.T.);
#7741=ORIENTED_EDGE('',*,*,#5606,.T.);
#7742=ORIENTED_EDGE('',*,*,#5607,.T.);
#7743=ORIENTED_EDGE('',*,*,#5608,.T.);
#7744=ORIENTED_EDGE('',*,*,#5609,.T.);
#7745=ORIENTED_EDGE('',*,*,#5610,.T.);
#7746=ORIENTED_EDGE('',*,*,#5611,.T.);
#7747=ORIENTED_EDGE('',*,*,#5612,.T.);
#7748=ORIENTED_EDGE('',*,*,#5613,.T.);
#7749=ORIENTED_EDGE('',*,*,#5614,.T.);
#7750=ORIENTED_EDGE('',*,*,#5615,.T.);
#7751=ORIENTED_EDGE('',*,*,#5616,.T.);
#7752=ORIENTED_EDGE('',*,*,#5617,.T.);
#7753=ORIENTED_EDGE('',*,*,#5618,.T.);
#7754=ORIENTED_EDGE('',*,*,#5619,.T.);
#7755=ORIENTED_EDGE('',*,*,#5620,.T.);
#7756=ORIENTED_EDGE('',*,*,#5621,.T.);
#7757=ORIENTED_EDGE('',*,*,#5622,.T.);
#7758=ORIENTED_EDGE('',*,*,#5623,.T.);
#7759=ORIENTED_EDGE('',*,*,#5624,.T.);
#7760=ORIENTED_EDGE('',*,*,#5625,.T.);
#7761=ORIENTED_EDGE('',*,*,#5626,.T.);
#7762=ORIENTED_EDGE('',*,*,#5627,.T.);
#7763=ORIENTED_EDGE('',*,*,#5628,.T.);
#7764=ORIENTED_EDGE('',*,*,#5629,.T.);
#7765=ORIENTED_EDGE('',*,*,#5630,.T.);
#7766=ORIENTED_EDGE('',*,*,#5631,.T.);
#7767=ORIENTED_EDGE('',*,*,#5632,.T.);
#7768=ORIENTED_EDGE('',*,*,#5633,.T.);
#7769=ORIENTED_EDGE('',*,*,#5634,.T.);
#7770=ORIENTED_EDGE('',*,*,#5635,.T.);
#7771=ORIENTED_EDGE('',*,*,#5636,.T.);
#7772=ORIENTED_EDGE('',*,*,#5637,.T.);
#7773=ORIENTED_EDGE('',*,*,#5638,.T.);
#7774=ORIENTED_EDGE('',*,*,#5639,.T.);
#7775=ORIENTED_EDGE('',*,*,#5640,.T.);
#7776=ORIENTED_EDGE('',*,*,#5641,.T.);
#7777=ORIENTED_EDGE('',*,*,#5642,.T.);
#7778=ORIENTED_EDGE('',*,*,#5643,.T.);
#7779=ORIENTED_EDGE('',*,*,#5644,.T.);
#7780=ORIENTED_EDGE('',*,*,#5645,.T.);
#7781=ORIENTED_EDGE('',*,*,#5646,.T.);
#7782=ORIENTED_EDGE('',*,*,#5647,.T.);
#7783=ORIENTED_EDGE('',*,*,#5648,.T.);
#7784=ORIENTED_EDGE('',*,*,#5649,.T.);
#7785=ORIENTED_EDGE('',*,*,#5650,.T.);
#7786=ORIENTED_EDGE('',*,*,#5651,.T.);
#7787=ORIENTED_EDGE('',*,*,#5652,.T.);
#7788=ORIENTED_EDGE('',*,*,#5653,.T.);
#7789=ORIENTED_EDGE('',*,*,#5654,.T.);
#7790=ORIENTED_EDGE('',*,*,#5655,.T.);
#7791=ORIENTED_EDGE('',*,*,#5656,.T.);
#7792=ORIENTED_EDGE('',*,*,#5657,.T.);
#7793=ORIENTED_EDGE('',*,*,#5658,.T.);
#7794=ORIENTED_EDGE('',*,*,#5659,.T.);
#7795=ORIENTED_EDGE('',*,*,#5660,.T.);
#7796=ORIENTED_EDGE('',*,*,#5661,.T.);
#7797=ORIENTED_EDGE('',*,*,#5662,.T.);
#7798=ORIENTED_EDGE('',*,*,#5663,.T.);
#7799=ORIENTED_EDGE('',*,*,#5664,.T.);
#7800=ORIENTED_EDGE('',*,*,#5665,.T.);
#7801=ORIENTED_EDGE('',*,*,#5666,.T.);
#7802=ORIENTED_EDGE('',*,*,#5667,.T.);
#7803=ORIENTED_EDGE('',*,*,#5668,.T.);
#7804=ORIENTED_EDGE('',*,*,#5669,.T.);
#7805=ORIENTED_EDGE('',*,*,#5670,.T.);
#7806=ORIENTED_EDGE('',*,*,#5671,.T.);
#7807=ORIENTED_EDGE('',*,*,#5672,.T.);
#7808=ORIENTED_EDGE('',*,*,#5673,.T.);
#7809=ORIENTED_EDGE('',*,*,#5674,.T.);
#7810=ORIENTED_EDGE('',*,*,#5675,.T.);
#7811=ORIENTED_EDGE('',*,*,#5676,.T.);
#7812=ORIENTED_EDGE('',*,*,#5677,.T.);
#7813=ORIENTED_EDGE('',*,*,#5678,.T.);
#7814=ORIENTED_EDGE('',*,*,#5679,.T.);
#7815=ORIENTED_EDGE('',*,*,#5680,.T.);
#7816=ORIENTED_EDGE('',*,*,#5681,.T.);
#7817=ORIENTED_EDGE('',*,*,#5682,.T.);
#7818=ORIENTED_EDGE('',*,*,#5683,.T.);
#7819=ORIENTED_EDGE('',*,*,#5684,.T.);
#7820=ORIENTED_EDGE('',*,*,#5685,.T.);
#7821=ORIENTED_EDGE('',*,*,#5686,.T.);
#7822=ORIENTED_EDGE('',*,*,#5687,.T.);
#7823=ORIENTED_EDGE('',*,*,#5688,.T.);
#7824=ORIENTED_EDGE('',*,*,#5689,.T.);
#7825=ORIENTED_EDGE('',*,*,#5690,.T.);
#7826=ORIENTED_EDGE('',*,*,#5691,.T.);
#7827=ORIENTED_EDGE('',*,*,#5692,.T.);
#7828=ORIENTED_EDGE('',*,*,#5693,.T.);
#7829=ORIENTED_EDGE('',*,*,#5694,.T.);
#7830=ORIENTED_EDGE('',*,*,#5695,.T.);
#7831=ORIENTED_EDGE('',*,*,#5696,.T.);
#7832=ORIENTED_EDGE('',*,*,#5697,.T.);
#7833=ORIENTED_EDGE('',*,*,#5698,.T.);
#7834=ORIENTED_EDGE('',*,*,#5699,.T.);
#7835=ORIENTED_EDGE('',*,*,#5700,.T.);
#7836=ORIENTED_EDGE('',*,*,#5701,.T.);
#7837=ORIENTED_EDGE('',*,*,#5702,.T.);
#7838=ORIENTED_EDGE('',*,*,#5703,.T.);
#7839=ORIENTED_EDGE('',*,*,#5704,.T.);
#7840=ORIENTED_EDGE('',*,*,#5705,.T.);
#7841=ORIENTED_EDGE('',*,*,#5706,.T.);
#7842=ORIENTED_EDGE('',*,*,#5707,.T.);
#7843=ORIENTED_EDGE('',*,*,#5708,.T.);
#7844=ORIENTED_EDGE('',*,*,#5709,.T.);
#7845=ORIENTED_EDGE('',*,*,#5710,.T.);
#7846=ORIENTED_EDGE('',*,*,#5711,.T.);
#7847=ORIENTED_EDGE('',*,*,#5712,.T.);
#7848=ORIENTED_EDGE('',*,*,#5713,.T.);
#7849=ORIENTED_EDGE('',*,*,#5714,.T.);
#7850=ORIENTED_EDGE('',*,*,#5715,.T.);
#7851=ORIENTED_EDGE('',*,*,#5716,.T.);
#7852=ORIENTED_EDGE('',*,*,#5717,.T.);
#7853=ORIENTED_EDGE('',*,*,#5718,.T.);
#7854=ORIENTED_EDGE('',*,*,#5719,.T.);
#7855=ORIENTED_EDGE('',*,*,#5720,.T.);
#7856=ORIENTED_EDGE('',*,*,#5721,.T.);
#7857=ORIENTED_EDGE('',*,*,#5722,.T.);
#7858=ORIENTED_EDGE('',*,*,#5723,.T.);
#7859=ORIENTED_EDGE('',*,*,#5724,.T.);
#7860=ORIENTED_EDGE('',*,*,#5725,.T.);
#7861=ORIENTED_EDGE('',*,*,#5726,.T.);
#7862=ORIENTED_EDGE('',*,*,#5727,.T.);
#7863=ORIENTED_EDGE('',*,*,#5728,.T.);
#7864=ORIENTED_EDGE('',*,*,#5729,.T.);
#7865=ORIENTED_EDGE('',*,*,#5730,.T.);
#7866=ORIENTED_EDGE('',*,*,#5731,.T.);
#7867=ORIENTED_EDGE('',*,*,#5732,.T.);
#7868=ORIENTED_EDGE('',*,*,#5733,.T.);
#7869=ORIENTED_EDGE('',*,*,#5734,.T.);
#7870=ORIENTED_EDGE('',*,*,#5735,.T.);
#7871=ORIENTED_EDGE('',*,*,#5736,.T.);
#7872=ORIENTED_EDGE('',*,*,#5737,.T.);
#7873=ORIENTED_EDGE('',*,*,#5738,.T.);
#7874=ORIENTED_EDGE('',*,*,#5739,.T.);
#7875=ORIENTED_EDGE('',*,*,#5740,.T.);
#7876=ORIENTED_EDGE('',*,*,#5741,.F.);
#7877=ORIENTED_EDGE('',*,*,#5742,.T.);
#7878=ORIENTED_EDGE('',*,*,#5743,.F.);
#7879=ORIENTED_EDGE('',*,*,#5744,.F.);
#7880=ORIENTED_EDGE('',*,*,#5745,.F.);
#7881=ORIENTED_EDGE('',*,*,#5746,.F.);
#7882=ORIENTED_EDGE('',*,*,#5747,.F.);
#7883=ORIENTED_EDGE('',*,*,#5748,.F.);
#7884=ORIENTED_EDGE('',*,*,#5749,.F.);
#7885=ORIENTED_EDGE('',*,*,#5750,.F.);
#7886=ORIENTED_EDGE('',*,*,#5751,.F.);
#7887=ORIENTED_EDGE('',*,*,#5752,.F.);
#7888=ORIENTED_EDGE('',*,*,#5753,.F.);
#7889=ORIENTED_EDGE('',*,*,#5754,.F.);
#7890=ORIENTED_EDGE('',*,*,#5755,.F.);
#7891=ORIENTED_EDGE('',*,*,#5756,.F.);
#7892=ORIENTED_EDGE('',*,*,#5757,.F.);
#7893=ORIENTED_EDGE('',*,*,#5758,.F.);
#7894=ORIENTED_EDGE('',*,*,#5759,.F.);
#7895=ORIENTED_EDGE('',*,*,#5760,.F.);
#7896=ORIENTED_EDGE('',*,*,#5761,.F.);
#7897=ORIENTED_EDGE('',*,*,#5762,.F.);
#7898=ORIENTED_EDGE('',*,*,#5763,.F.);
#7899=ORIENTED_EDGE('',*,*,#5764,.F.);
#7900=ORIENTED_EDGE('',*,*,#5765,.F.);
#7901=ORIENTED_EDGE('',*,*,#5766,.F.);
#7902=ORIENTED_EDGE('',*,*,#5767,.F.);
#7903=ORIENTED_EDGE('',*,*,#5768,.F.);
#7904=ORIENTED_EDGE('',*,*,#5769,.F.);
#7905=ORIENTED_EDGE('',*,*,#5770,.F.);
#7906=ORIENTED_EDGE('',*,*,#5771,.F.);
#7907=ORIENTED_EDGE('',*,*,#5772,.F.);
#7908=ORIENTED_EDGE('',*,*,#5773,.F.);
#7909=ORIENTED_EDGE('',*,*,#5774,.F.);
#7910=ORIENTED_EDGE('',*,*,#5775,.F.);
#7911=ORIENTED_EDGE('',*,*,#5776,.F.);
#7912=ORIENTED_EDGE('',*,*,#5777,.F.);
#7913=ORIENTED_EDGE('',*,*,#5778,.F.);
#7914=ORIENTED_EDGE('',*,*,#5779,.F.);
#7915=ORIENTED_EDGE('',*,*,#5780,.F.);
#7916=ORIENTED_EDGE('',*,*,#5781,.F.);
#7917=ORIENTED_EDGE('',*,*,#5782,.F.);
#7918=ORIENTED_EDGE('',*,*,#5783,.F.);
#7919=ORIENTED_EDGE('',*,*,#5784,.F.);
#7920=ORIENTED_EDGE('',*,*,#5785,.T.);
#7921=ORIENTED_EDGE('',*,*,#5786,.T.);
#7922=ORIENTED_EDGE('',*,*,#5787,.T.);
#7923=ORIENTED_EDGE('',*,*,#5788,.T.);
#7924=ORIENTED_EDGE('',*,*,#5789,.T.);
#7925=ORIENTED_EDGE('',*,*,#5790,.T.);
#7926=ORIENTED_EDGE('',*,*,#5791,.T.);
#7927=ORIENTED_EDGE('',*,*,#5792,.T.);
#7928=ORIENTED_EDGE('',*,*,#5793,.T.);
#7929=ORIENTED_EDGE('',*,*,#5794,.T.);
#7930=ORIENTED_EDGE('',*,*,#5795,.T.);
#7931=ORIENTED_EDGE('',*,*,#5796,.T.);
#7932=ORIENTED_EDGE('',*,*,#5797,.T.);
#7933=ORIENTED_EDGE('',*,*,#5798,.T.);
#7934=ORIENTED_EDGE('',*,*,#5799,.T.);
#7935=ORIENTED_EDGE('',*,*,#5800,.T.);
#7936=ORIENTED_EDGE('',*,*,#5801,.T.);
#7937=ORIENTED_EDGE('',*,*,#5802,.T.);
#7938=ORIENTED_EDGE('',*,*,#5803,.T.);
#7939=ORIENTED_EDGE('',*,*,#5804,.T.);
#7940=ORIENTED_EDGE('',*,*,#5805,.T.);
#7941=ORIENTED_EDGE('',*,*,#5806,.T.);
#7942=ORIENTED_EDGE('',*,*,#5807,.T.);
#7943=ORIENTED_EDGE('',*,*,#5808,.T.);
#7944=ORIENTED_EDGE('',*,*,#5809,.T.);
#7945=ORIENTED_EDGE('',*,*,#5810,.T.);
#7946=ORIENTED_EDGE('',*,*,#5811,.T.);
#7947=ORIENTED_EDGE('',*,*,#5812,.T.);
#7948=ORIENTED_EDGE('',*,*,#5813,.T.);
#7949=ORIENTED_EDGE('',*,*,#5814,.T.);
#7950=ORIENTED_EDGE('',*,*,#5815,.T.);
#7951=ORIENTED_EDGE('',*,*,#5816,.T.);
#7952=ORIENTED_EDGE('',*,*,#5817,.T.);
#7953=ORIENTED_EDGE('',*,*,#5818,.T.);
#7954=ORIENTED_EDGE('',*,*,#5819,.T.);
#7955=ORIENTED_EDGE('',*,*,#5820,.T.);
#7956=ORIENTED_EDGE('',*,*,#5821,.T.);
#7957=ORIENTED_EDGE('',*,*,#5822,.T.);
#7958=ORIENTED_EDGE('',*,*,#5823,.T.);
#7959=ORIENTED_EDGE('',*,*,#5824,.T.);
#7960=ORIENTED_EDGE('',*,*,#5825,.F.);
#7961=ORIENTED_EDGE('',*,*,#5826,.T.);
#7962=ORIENTED_EDGE('',*,*,#5827,.T.);
#7963=ORIENTED_EDGE('',*,*,#5828,.F.);
#7964=ORIENTED_EDGE('',*,*,#5829,.F.);
#7965=ORIENTED_EDGE('',*,*,#5830,.T.);
#7966=ORIENTED_EDGE('',*,*,#5831,.T.);
#7967=ORIENTED_EDGE('',*,*,#5826,.F.);
#7968=ORIENTED_EDGE('',*,*,#5832,.F.);
#7969=ORIENTED_EDGE('',*,*,#5833,.T.);
#7970=ORIENTED_EDGE('',*,*,#5834,.T.);
#7971=ORIENTED_EDGE('',*,*,#5830,.F.);
#7972=ORIENTED_EDGE('',*,*,#5835,.F.);
#7973=ORIENTED_EDGE('',*,*,#5836,.T.);
#7974=ORIENTED_EDGE('',*,*,#5837,.T.);
#7975=ORIENTED_EDGE('',*,*,#5833,.F.);
#7976=ORIENTED_EDGE('',*,*,#5838,.F.);
#7977=ORIENTED_EDGE('',*,*,#5839,.T.);
#7978=ORIENTED_EDGE('',*,*,#5840,.T.);
#7979=ORIENTED_EDGE('',*,*,#5836,.F.);
#7980=ORIENTED_EDGE('',*,*,#5841,.F.);
#7981=ORIENTED_EDGE('',*,*,#5828,.T.);
#7982=ORIENTED_EDGE('',*,*,#5842,.T.);
#7983=ORIENTED_EDGE('',*,*,#5839,.F.);
#7984=ORIENTED_EDGE('',*,*,#5842,.F.);
#7985=ORIENTED_EDGE('',*,*,#5827,.F.);
#7986=ORIENTED_EDGE('',*,*,#5831,.F.);
#7987=ORIENTED_EDGE('',*,*,#5834,.F.);
#7988=ORIENTED_EDGE('',*,*,#5837,.F.);
#7989=ORIENTED_EDGE('',*,*,#5840,.F.);
#7990=ORIENTED_EDGE('',*,*,#5591,.F.);
#7991=ORIENTED_EDGE('',*,*,#5843,.T.);
#7992=ORIENTED_EDGE('',*,*,#5743,.T.);
#7993=ORIENTED_EDGE('',*,*,#5844,.T.);
#7994=ORIENTED_EDGE('',*,*,#5845,.T.);
#7995=ORIENTED_EDGE('',*,*,#5843,.F.);
#7996=ORIENTED_EDGE('',*,*,#5740,.F.);
#7997=ORIENTED_EDGE('',*,*,#5739,.F.);
#7998=ORIENTED_EDGE('',*,*,#5738,.F.);
#7999=ORIENTED_EDGE('',*,*,#5737,.F.);
#8000=ORIENTED_EDGE('',*,*,#5736,.F.);
#8001=ORIENTED_EDGE('',*,*,#5735,.F.);
#8002=ORIENTED_EDGE('',*,*,#5734,.F.);
#8003=ORIENTED_EDGE('',*,*,#5733,.F.);
#8004=ORIENTED_EDGE('',*,*,#5732,.F.);
#8005=ORIENTED_EDGE('',*,*,#5731,.F.);
#8006=ORIENTED_EDGE('',*,*,#5730,.F.);
#8007=ORIENTED_EDGE('',*,*,#5729,.F.);
#8008=ORIENTED_EDGE('',*,*,#5728,.F.);
#8009=ORIENTED_EDGE('',*,*,#5727,.F.);
#8010=ORIENTED_EDGE('',*,*,#5726,.F.);
#8011=ORIENTED_EDGE('',*,*,#5725,.F.);
#8012=ORIENTED_EDGE('',*,*,#5724,.F.);
#8013=ORIENTED_EDGE('',*,*,#5723,.F.);
#8014=ORIENTED_EDGE('',*,*,#5722,.F.);
#8015=ORIENTED_EDGE('',*,*,#5721,.F.);
#8016=ORIENTED_EDGE('',*,*,#5720,.F.);
#8017=ORIENTED_EDGE('',*,*,#5719,.F.);
#8018=ORIENTED_EDGE('',*,*,#5718,.F.);
#8019=ORIENTED_EDGE('',*,*,#5717,.F.);
#8020=ORIENTED_EDGE('',*,*,#5716,.F.);
#8021=ORIENTED_EDGE('',*,*,#5715,.F.);
#8022=ORIENTED_EDGE('',*,*,#5714,.F.);
#8023=ORIENTED_EDGE('',*,*,#5713,.F.);
#8024=ORIENTED_EDGE('',*,*,#5712,.F.);
#8025=ORIENTED_EDGE('',*,*,#5711,.F.);
#8026=ORIENTED_EDGE('',*,*,#5710,.F.);
#8027=ORIENTED_EDGE('',*,*,#5709,.F.);
#8028=ORIENTED_EDGE('',*,*,#5708,.F.);
#8029=ORIENTED_EDGE('',*,*,#5707,.F.);
#8030=ORIENTED_EDGE('',*,*,#5706,.F.);
#8031=ORIENTED_EDGE('',*,*,#5705,.F.);
#8032=ORIENTED_EDGE('',*,*,#5704,.F.);
#8033=ORIENTED_EDGE('',*,*,#5703,.F.);
#8034=ORIENTED_EDGE('',*,*,#5702,.F.);
#8035=ORIENTED_EDGE('',*,*,#5701,.F.);
#8036=ORIENTED_EDGE('',*,*,#5700,.F.);
#8037=ORIENTED_EDGE('',*,*,#5699,.F.);
#8038=ORIENTED_EDGE('',*,*,#5698,.F.);
#8039=ORIENTED_EDGE('',*,*,#5697,.F.);
#8040=ORIENTED_EDGE('',*,*,#5696,.F.);
#8041=ORIENTED_EDGE('',*,*,#5695,.F.);
#8042=ORIENTED_EDGE('',*,*,#5694,.F.);
#8043=ORIENTED_EDGE('',*,*,#5693,.F.);
#8044=ORIENTED_EDGE('',*,*,#5692,.F.);
#8045=ORIENTED_EDGE('',*,*,#5691,.F.);
#8046=ORIENTED_EDGE('',*,*,#5690,.F.);
#8047=ORIENTED_EDGE('',*,*,#5689,.F.);
#8048=ORIENTED_EDGE('',*,*,#5688,.F.);
#8049=ORIENTED_EDGE('',*,*,#5687,.F.);
#8050=ORIENTED_EDGE('',*,*,#5686,.F.);
#8051=ORIENTED_EDGE('',*,*,#5685,.F.);
#8052=ORIENTED_EDGE('',*,*,#5684,.F.);
#8053=ORIENTED_EDGE('',*,*,#5683,.F.);
#8054=ORIENTED_EDGE('',*,*,#5682,.F.);
#8055=ORIENTED_EDGE('',*,*,#5681,.F.);
#8056=ORIENTED_EDGE('',*,*,#5680,.F.);
#8057=ORIENTED_EDGE('',*,*,#5679,.F.);
#8058=ORIENTED_EDGE('',*,*,#5678,.F.);
#8059=ORIENTED_EDGE('',*,*,#5677,.F.);
#8060=ORIENTED_EDGE('',*,*,#5676,.F.);
#8061=ORIENTED_EDGE('',*,*,#5675,.F.);
#8062=ORIENTED_EDGE('',*,*,#5674,.F.);
#8063=ORIENTED_EDGE('',*,*,#5673,.F.);
#8064=ORIENTED_EDGE('',*,*,#5672,.F.);
#8065=ORIENTED_EDGE('',*,*,#5671,.F.);
#8066=ORIENTED_EDGE('',*,*,#5670,.F.);
#8067=ORIENTED_EDGE('',*,*,#5669,.F.);
#8068=ORIENTED_EDGE('',*,*,#5668,.F.);
#8069=ORIENTED_EDGE('',*,*,#5667,.F.);
#8070=ORIENTED_EDGE('',*,*,#5846,.F.);
#8071=ORIENTED_EDGE('',*,*,#5783,.T.);
#8072=ORIENTED_EDGE('',*,*,#5782,.T.);
#8073=ORIENTED_EDGE('',*,*,#5781,.T.);
#8074=ORIENTED_EDGE('',*,*,#5780,.T.);
#8075=ORIENTED_EDGE('',*,*,#5779,.T.);
#8076=ORIENTED_EDGE('',*,*,#5778,.T.);
#8077=ORIENTED_EDGE('',*,*,#5777,.T.);
#8078=ORIENTED_EDGE('',*,*,#5776,.T.);
#8079=ORIENTED_EDGE('',*,*,#5775,.T.);
#8080=ORIENTED_EDGE('',*,*,#5774,.T.);
#8081=ORIENTED_EDGE('',*,*,#5773,.T.);
#8082=ORIENTED_EDGE('',*,*,#5772,.T.);
#8083=ORIENTED_EDGE('',*,*,#5771,.T.);
#8084=ORIENTED_EDGE('',*,*,#5770,.T.);
#8085=ORIENTED_EDGE('',*,*,#5769,.T.);
#8086=ORIENTED_EDGE('',*,*,#5768,.T.);
#8087=ORIENTED_EDGE('',*,*,#5767,.T.);
#8088=ORIENTED_EDGE('',*,*,#5766,.T.);
#8089=ORIENTED_EDGE('',*,*,#5765,.T.);
#8090=ORIENTED_EDGE('',*,*,#5764,.T.);
#8091=ORIENTED_EDGE('',*,*,#5763,.T.);
#8092=ORIENTED_EDGE('',*,*,#5762,.T.);
#8093=ORIENTED_EDGE('',*,*,#5761,.T.);
#8094=ORIENTED_EDGE('',*,*,#5760,.T.);
#8095=ORIENTED_EDGE('',*,*,#5759,.T.);
#8096=ORIENTED_EDGE('',*,*,#5758,.T.);
#8097=ORIENTED_EDGE('',*,*,#5757,.T.);
#8098=ORIENTED_EDGE('',*,*,#5756,.T.);
#8099=ORIENTED_EDGE('',*,*,#5755,.T.);
#8100=ORIENTED_EDGE('',*,*,#5754,.T.);
#8101=ORIENTED_EDGE('',*,*,#5753,.T.);
#8102=ORIENTED_EDGE('',*,*,#5752,.T.);
#8103=ORIENTED_EDGE('',*,*,#5751,.T.);
#8104=ORIENTED_EDGE('',*,*,#5750,.T.);
#8105=ORIENTED_EDGE('',*,*,#5749,.T.);
#8106=ORIENTED_EDGE('',*,*,#5748,.T.);
#8107=ORIENTED_EDGE('',*,*,#5747,.T.);
#8108=ORIENTED_EDGE('',*,*,#5746,.T.);
#8109=ORIENTED_EDGE('',*,*,#5745,.T.);
#8110=ORIENTED_EDGE('',*,*,#5744,.T.);
#8111=ORIENTED_EDGE('',*,*,#5666,.F.);
#8112=ORIENTED_EDGE('',*,*,#5847,.T.);
#8113=ORIENTED_EDGE('',*,*,#5784,.T.);
#8114=ORIENTED_EDGE('',*,*,#5846,.T.);
#8115=ORIENTED_EDGE('',*,*,#5845,.F.);
#8116=ORIENTED_EDGE('',*,*,#5844,.F.);
#8117=ORIENTED_EDGE('',*,*,#5742,.F.);
#8118=ORIENTED_EDGE('',*,*,#5824,.F.);
#8119=ORIENTED_EDGE('',*,*,#5823,.F.);
#8120=ORIENTED_EDGE('',*,*,#5822,.F.);
#8121=ORIENTED_EDGE('',*,*,#5821,.F.);
#8122=ORIENTED_EDGE('',*,*,#5820,.F.);
#8123=ORIENTED_EDGE('',*,*,#5819,.F.);
#8124=ORIENTED_EDGE('',*,*,#5818,.F.);
#8125=ORIENTED_EDGE('',*,*,#5817,.F.);
#8126=ORIENTED_EDGE('',*,*,#5816,.F.);
#8127=ORIENTED_EDGE('',*,*,#5815,.F.);
#8128=ORIENTED_EDGE('',*,*,#5814,.F.);
#8129=ORIENTED_EDGE('',*,*,#5813,.F.);
#8130=ORIENTED_EDGE('',*,*,#5812,.F.);
#8131=ORIENTED_EDGE('',*,*,#5811,.F.);
#8132=ORIENTED_EDGE('',*,*,#5810,.F.);
#8133=ORIENTED_EDGE('',*,*,#5809,.F.);
#8134=ORIENTED_EDGE('',*,*,#5808,.F.);
#8135=ORIENTED_EDGE('',*,*,#5807,.F.);
#8136=ORIENTED_EDGE('',*,*,#5806,.F.);
#8137=ORIENTED_EDGE('',*,*,#5805,.F.);
#8138=ORIENTED_EDGE('',*,*,#5804,.F.);
#8139=ORIENTED_EDGE('',*,*,#5803,.F.);
#8140=ORIENTED_EDGE('',*,*,#5802,.F.);
#8141=ORIENTED_EDGE('',*,*,#5801,.F.);
#8142=ORIENTED_EDGE('',*,*,#5800,.F.);
#8143=ORIENTED_EDGE('',*,*,#5799,.F.);
#8144=ORIENTED_EDGE('',*,*,#5798,.F.);
#8145=ORIENTED_EDGE('',*,*,#5797,.F.);
#8146=ORIENTED_EDGE('',*,*,#5796,.F.);
#8147=ORIENTED_EDGE('',*,*,#5795,.F.);
#8148=ORIENTED_EDGE('',*,*,#5794,.F.);
#8149=ORIENTED_EDGE('',*,*,#5793,.F.);
#8150=ORIENTED_EDGE('',*,*,#5792,.F.);
#8151=ORIENTED_EDGE('',*,*,#5791,.F.);
#8152=ORIENTED_EDGE('',*,*,#5790,.F.);
#8153=ORIENTED_EDGE('',*,*,#5789,.F.);
#8154=ORIENTED_EDGE('',*,*,#5788,.F.);
#8155=ORIENTED_EDGE('',*,*,#5787,.F.);
#8156=ORIENTED_EDGE('',*,*,#5786,.F.);
#8157=ORIENTED_EDGE('',*,*,#5785,.F.);
#8158=ORIENTED_EDGE('',*,*,#5847,.F.);
#8159=ORIENTED_EDGE('',*,*,#5665,.F.);
#8160=ORIENTED_EDGE('',*,*,#5664,.F.);
#8161=ORIENTED_EDGE('',*,*,#5663,.F.);
#8162=ORIENTED_EDGE('',*,*,#5662,.F.);
#8163=ORIENTED_EDGE('',*,*,#5661,.F.);
#8164=ORIENTED_EDGE('',*,*,#5660,.F.);
#8165=ORIENTED_EDGE('',*,*,#5659,.F.);
#8166=ORIENTED_EDGE('',*,*,#5658,.F.);
#8167=ORIENTED_EDGE('',*,*,#5657,.F.);
#8168=ORIENTED_EDGE('',*,*,#5656,.F.);
#8169=ORIENTED_EDGE('',*,*,#5655,.F.);
#8170=ORIENTED_EDGE('',*,*,#5654,.F.);
#8171=ORIENTED_EDGE('',*,*,#5653,.F.);
#8172=ORIENTED_EDGE('',*,*,#5652,.F.);
#8173=ORIENTED_EDGE('',*,*,#5651,.F.);
#8174=ORIENTED_EDGE('',*,*,#5650,.F.);
#8175=ORIENTED_EDGE('',*,*,#5649,.F.);
#8176=ORIENTED_EDGE('',*,*,#5648,.F.);
#8177=ORIENTED_EDGE('',*,*,#5647,.F.);
#8178=ORIENTED_EDGE('',*,*,#5646,.F.);
#8179=ORIENTED_EDGE('',*,*,#5645,.F.);
#8180=ORIENTED_EDGE('',*,*,#5644,.F.);
#8181=ORIENTED_EDGE('',*,*,#5643,.F.);
#8182=ORIENTED_EDGE('',*,*,#5642,.F.);
#8183=ORIENTED_EDGE('',*,*,#5641,.F.);
#8184=ORIENTED_EDGE('',*,*,#5640,.F.);
#8185=ORIENTED_EDGE('',*,*,#5639,.F.);
#8186=ORIENTED_EDGE('',*,*,#5638,.F.);
#8187=ORIENTED_EDGE('',*,*,#5637,.F.);
#8188=ORIENTED_EDGE('',*,*,#5636,.F.);
#8189=ORIENTED_EDGE('',*,*,#5635,.F.);
#8190=ORIENTED_EDGE('',*,*,#5634,.F.);
#8191=ORIENTED_EDGE('',*,*,#5633,.F.);
#8192=ORIENTED_EDGE('',*,*,#5632,.F.);
#8193=ORIENTED_EDGE('',*,*,#5631,.F.);
#8194=ORIENTED_EDGE('',*,*,#5630,.F.);
#8195=ORIENTED_EDGE('',*,*,#5629,.F.);
#8196=ORIENTED_EDGE('',*,*,#5628,.F.);
#8197=ORIENTED_EDGE('',*,*,#5627,.F.);
#8198=ORIENTED_EDGE('',*,*,#5626,.F.);
#8199=ORIENTED_EDGE('',*,*,#5625,.F.);
#8200=ORIENTED_EDGE('',*,*,#5624,.F.);
#8201=ORIENTED_EDGE('',*,*,#5623,.F.);
#8202=ORIENTED_EDGE('',*,*,#5622,.F.);
#8203=ORIENTED_EDGE('',*,*,#5621,.F.);
#8204=ORIENTED_EDGE('',*,*,#5620,.F.);
#8205=ORIENTED_EDGE('',*,*,#5619,.F.);
#8206=ORIENTED_EDGE('',*,*,#5618,.F.);
#8207=ORIENTED_EDGE('',*,*,#5617,.F.);
#8208=ORIENTED_EDGE('',*,*,#5616,.F.);
#8209=ORIENTED_EDGE('',*,*,#5615,.F.);
#8210=ORIENTED_EDGE('',*,*,#5614,.F.);
#8211=ORIENTED_EDGE('',*,*,#5613,.F.);
#8212=ORIENTED_EDGE('',*,*,#5612,.F.);
#8213=ORIENTED_EDGE('',*,*,#5611,.F.);
#8214=ORIENTED_EDGE('',*,*,#5610,.F.);
#8215=ORIENTED_EDGE('',*,*,#5609,.F.);
#8216=ORIENTED_EDGE('',*,*,#5608,.F.);
#8217=ORIENTED_EDGE('',*,*,#5607,.F.);
#8218=ORIENTED_EDGE('',*,*,#5606,.F.);
#8219=ORIENTED_EDGE('',*,*,#5605,.F.);
#8220=ORIENTED_EDGE('',*,*,#5604,.F.);
#8221=ORIENTED_EDGE('',*,*,#5603,.F.);
#8222=ORIENTED_EDGE('',*,*,#5602,.F.);
#8223=ORIENTED_EDGE('',*,*,#5601,.F.);
#8224=ORIENTED_EDGE('',*,*,#5600,.F.);
#8225=ORIENTED_EDGE('',*,*,#5599,.F.);
#8226=ORIENTED_EDGE('',*,*,#5598,.F.);
#8227=ORIENTED_EDGE('',*,*,#5597,.F.);
#8228=ORIENTED_EDGE('',*,*,#5596,.F.);
#8229=ORIENTED_EDGE('',*,*,#5595,.F.);
#8230=ORIENTED_EDGE('',*,*,#5594,.F.);
#8231=ORIENTED_EDGE('',*,*,#5593,.F.);
#8232=ORIENTED_EDGE('',*,*,#5592,.F.);
#8233=ORIENTED_EDGE('',*,*,#5848,.F.);
#8234=ORIENTED_EDGE('',*,*,#5590,.F.);
#8235=ORIENTED_EDGE('',*,*,#5849,.T.);
#8236=ORIENTED_EDGE('',*,*,#5848,.T.);
#8237=ORIENTED_EDGE('',*,*,#5849,.F.);
#8238=ORIENTED_EDGE('',*,*,#5741,.T.);
#8239=ORIENTED_EDGE('',*,*,#5850,.T.);
#8240=ORIENTED_EDGE('',*,*,#5851,.F.);
#8241=ORIENTED_EDGE('',*,*,#5850,.F.);
#8242=ORIENTED_EDGE('',*,*,#5851,.T.);
#8243=ORIENTED_EDGE('',*,*,#5825,.T.);
#8244=ORIENTED_EDGE('',*,*,#5841,.T.);
#8245=ORIENTED_EDGE('',*,*,#5838,.T.);
#8246=ORIENTED_EDGE('',*,*,#5835,.T.);
#8247=ORIENTED_EDGE('',*,*,#5832,.T.);
#8248=ORIENTED_EDGE('',*,*,#5829,.T.);
#8249=ORIENTED_EDGE('',*,*,#5852,.T.);
#8250=ORIENTED_EDGE('',*,*,#5853,.T.);
#8251=ORIENTED_EDGE('',*,*,#5854,.T.);
#8252=ORIENTED_EDGE('',*,*,#5855,.T.);
#8253=ORIENTED_EDGE('',*,*,#5856,.T.);
#8254=ORIENTED_EDGE('',*,*,#5852,.F.);
#8255=ORIENTED_EDGE('',*,*,#5857,.T.);
#8256=ORIENTED_EDGE('',*,*,#5858,.T.);
#8257=ORIENTED_EDGE('',*,*,#5859,.T.);
#8258=ORIENTED_EDGE('',*,*,#5860,.F.);
#8259=ORIENTED_EDGE('',*,*,#5861,.T.);
#8260=ORIENTED_EDGE('',*,*,#5862,.T.);
#8261=ORIENTED_EDGE('',*,*,#5863,.T.);
#8262=ORIENTED_EDGE('',*,*,#5855,.F.);
#8263=ORIENTED_EDGE('',*,*,#5864,.T.);
#8264=ORIENTED_EDGE('',*,*,#5861,.F.);
#8265=ORIENTED_EDGE('',*,*,#5865,.F.);
#8266=ORIENTED_EDGE('',*,*,#5866,.T.);
#8267=ORIENTED_EDGE('',*,*,#5867,.T.);
#8268=ORIENTED_EDGE('',*,*,#5868,.T.);
#8269=ORIENTED_EDGE('',*,*,#5869,.T.);
#8270=ORIENTED_EDGE('',*,*,#5870,.T.);
#8271=ORIENTED_EDGE('',*,*,#5866,.F.);
#8272=ORIENTED_EDGE('',*,*,#5871,.T.);
#8273=ORIENTED_EDGE('',*,*,#5872,.T.);
#8274=ORIENTED_EDGE('',*,*,#5873,.T.);
#8275=ORIENTED_EDGE('',*,*,#5874,.F.);
#8276=ORIENTED_EDGE('',*,*,#5875,.T.);
#8277=ORIENTED_EDGE('',*,*,#5876,.T.);
#8278=ORIENTED_EDGE('',*,*,#5877,.T.);
#8279=ORIENTED_EDGE('',*,*,#5869,.F.);
#8280=ORIENTED_EDGE('',*,*,#5878,.T.);
#8281=ORIENTED_EDGE('',*,*,#5875,.F.);
#8282=ORIENTED_EDGE('',*,*,#5879,.F.);
#8283=ORIENTED_EDGE('',*,*,#5880,.T.);
#8284=ORIENTED_EDGE('',*,*,#5881,.T.);
#8285=ORIENTED_EDGE('',*,*,#5882,.T.);
#8286=ORIENTED_EDGE('',*,*,#5883,.T.);
#8287=ORIENTED_EDGE('',*,*,#5880,.F.);
#8288=ORIENTED_EDGE('',*,*,#5884,.T.);
#8289=ORIENTED_EDGE('',*,*,#5885,.T.);
#8290=ORIENTED_EDGE('',*,*,#5886,.F.);
#8291=ORIENTED_EDGE('',*,*,#5883,.F.);
#8292=ORIENTED_EDGE('',*,*,#5887,.T.);
#8293=ORIENTED_EDGE('',*,*,#5888,.T.);
#8294=ORIENTED_EDGE('',*,*,#5884,.F.);
#8295=ORIENTED_EDGE('',*,*,#5882,.F.);
#8296=ORIENTED_EDGE('',*,*,#5889,.T.);
#8297=ORIENTED_EDGE('',*,*,#5890,.T.);
#8298=ORIENTED_EDGE('',*,*,#5887,.F.);
#8299=ORIENTED_EDGE('',*,*,#5881,.F.);
#8300=ORIENTED_EDGE('',*,*,#5886,.T.);
#8301=ORIENTED_EDGE('',*,*,#5891,.T.);
#8302=ORIENTED_EDGE('',*,*,#5889,.F.);
#8303=ORIENTED_EDGE('',*,*,#5891,.F.);
#8304=ORIENTED_EDGE('',*,*,#5885,.F.);
#8305=ORIENTED_EDGE('',*,*,#5888,.F.);
#8306=ORIENTED_EDGE('',*,*,#5890,.F.);
#8307=ORIENTED_EDGE('',*,*,#5892,.F.);
#8308=ORIENTED_EDGE('',*,*,#5893,.T.);
#8309=ORIENTED_EDGE('',*,*,#5894,.F.);
#8310=ORIENTED_EDGE('',*,*,#5895,.F.);
#8311=ORIENTED_EDGE('',*,*,#5896,.F.);
#8312=ORIENTED_EDGE('',*,*,#5893,.F.);
#8313=ORIENTED_EDGE('',*,*,#5897,.F.);
#8314=ORIENTED_EDGE('',*,*,#5898,.F.);
#8315=ORIENTED_EDGE('',*,*,#5899,.T.);
#8316=ORIENTED_EDGE('',*,*,#5900,.F.);
#8317=ORIENTED_EDGE('',*,*,#5899,.F.);
#8318=ORIENTED_EDGE('',*,*,#5901,.F.);
#8319=ORIENTED_EDGE('',*,*,#5902,.T.);
#8320=ORIENTED_EDGE('',*,*,#5903,.F.);
#8321=ORIENTED_EDGE('',*,*,#5904,.F.);
#8322=ORIENTED_EDGE('',*,*,#5905,.F.);
#8323=ORIENTED_EDGE('',*,*,#5902,.F.);
#8324=ORIENTED_EDGE('',*,*,#5906,.F.);
#8325=ORIENTED_EDGE('',*,*,#5907,.F.);
#8326=ORIENTED_EDGE('',*,*,#5908,.T.);
#8327=ORIENTED_EDGE('',*,*,#5909,.F.);
#8328=ORIENTED_EDGE('',*,*,#5908,.F.);
#8329=ORIENTED_EDGE('',*,*,#5910,.F.);
#8330=ORIENTED_EDGE('',*,*,#5911,.T.);
#8331=ORIENTED_EDGE('',*,*,#5905,.T.);
#8332=ORIENTED_EDGE('',*,*,#5912,.T.);
#8333=ORIENTED_EDGE('',*,*,#5896,.T.);
#8334=ORIENTED_EDGE('',*,*,#5913,.T.);
#8335=ORIENTED_EDGE('',*,*,#5914,.F.);
#8336=ORIENTED_EDGE('',*,*,#5913,.F.);
#8337=ORIENTED_EDGE('',*,*,#5895,.T.);
#8338=ORIENTED_EDGE('',*,*,#5894,.T.);
#8339=ORIENTED_EDGE('',*,*,#5912,.F.);
#8340=ORIENTED_EDGE('',*,*,#5904,.T.);
#8341=ORIENTED_EDGE('',*,*,#5903,.T.);
#8342=ORIENTED_EDGE('',*,*,#5911,.F.);
#8343=ORIENTED_EDGE('',*,*,#5897,.T.);
#8344=ORIENTED_EDGE('',*,*,#5898,.T.);
#8345=ORIENTED_EDGE('',*,*,#5906,.T.);
#8346=ORIENTED_EDGE('',*,*,#5907,.T.);
#8347=ORIENTED_EDGE('',*,*,#5915,.T.);
#8348=ORIENTED_EDGE('',*,*,#5916,.F.);
#8349=ORIENTED_EDGE('',*,*,#5917,.F.);
#8350=ORIENTED_EDGE('',*,*,#5865,.T.);
#8351=ORIENTED_EDGE('',*,*,#5860,.T.);
#8352=ORIENTED_EDGE('',*,*,#5918,.T.);
#8353=ORIENTED_EDGE('',*,*,#5856,.F.);
#8354=ORIENTED_EDGE('',*,*,#5919,.T.);
#8355=ORIENTED_EDGE('',*,*,#5920,.F.);
#8356=ORIENTED_EDGE('',*,*,#5879,.T.);
#8357=ORIENTED_EDGE('',*,*,#5874,.T.);
#8358=ORIENTED_EDGE('',*,*,#5921,.T.);
#8359=ORIENTED_EDGE('',*,*,#5870,.F.);
#8360=ORIENTED_EDGE('',*,*,#5922,.F.);
#8361=ORIENTED_EDGE('',*,*,#5923,.T.);
#8362=ORIENTED_EDGE('',*,*,#5916,.T.);
#8363=ORIENTED_EDGE('',*,*,#5857,.F.);
#8364=ORIENTED_EDGE('',*,*,#5918,.F.);
#8365=ORIENTED_EDGE('',*,*,#5924,.F.);
#8366=ORIENTED_EDGE('',*,*,#5920,.T.);
#8367=ORIENTED_EDGE('',*,*,#5871,.F.);
#8368=ORIENTED_EDGE('',*,*,#5921,.F.);
#8369=ORIENTED_EDGE('',*,*,#5925,.F.);
#8370=ORIENTED_EDGE('',*,*,#5917,.T.);
#8371=ORIENTED_EDGE('',*,*,#5923,.F.);
#8372=ORIENTED_EDGE('',*,*,#5922,.T.);
#8373=ORIENTED_EDGE('',*,*,#5910,.T.);
#8374=ORIENTED_EDGE('',*,*,#5859,.F.);
#8375=ORIENTED_EDGE('',*,*,#5926,.T.);
#8376=ORIENTED_EDGE('',*,*,#5924,.T.);
#8377=ORIENTED_EDGE('',*,*,#5873,.F.);
#8378=ORIENTED_EDGE('',*,*,#5927,.T.);
#8379=ORIENTED_EDGE('',*,*,#5925,.T.);
#8380=ORIENTED_EDGE('',*,*,#5863,.F.);
#8381=ORIENTED_EDGE('',*,*,#5928,.T.);
#8382=ORIENTED_EDGE('',*,*,#5867,.F.);
#8383=ORIENTED_EDGE('',*,*,#5872,.F.);
#8384=ORIENTED_EDGE('',*,*,#5919,.F.);
#8385=ORIENTED_EDGE('',*,*,#5926,.F.);
#8386=ORIENTED_EDGE('',*,*,#5900,.T.);
#8387=ORIENTED_EDGE('',*,*,#5909,.T.);
#8388=ORIENTED_EDGE('',*,*,#5853,.F.);
#8389=ORIENTED_EDGE('',*,*,#5858,.F.);
#8390=ORIENTED_EDGE('',*,*,#5915,.F.);
#8391=ORIENTED_EDGE('',*,*,#5927,.F.);
#8392=ORIENTED_EDGE('',*,*,#5877,.F.);
#8393=ORIENTED_EDGE('',*,*,#5929,.T.);
#8394=ORIENTED_EDGE('',*,*,#5892,.T.);
#8395=ORIENTED_EDGE('',*,*,#5901,.T.);
#8396=ORIENTED_EDGE('',*,*,#5854,.F.);
#8397=ORIENTED_EDGE('',*,*,#5929,.F.);
#8398=ORIENTED_EDGE('',*,*,#5876,.F.);
#8399=ORIENTED_EDGE('',*,*,#5878,.F.);
#8400=ORIENTED_EDGE('',*,*,#5868,.F.);
#8401=ORIENTED_EDGE('',*,*,#5928,.F.);
#8402=ORIENTED_EDGE('',*,*,#5862,.F.);
#8403=ORIENTED_EDGE('',*,*,#5864,.F.);
#8404=ORIENTED_EDGE('',*,*,#5914,.T.);
#8405=ORIENTED_EDGE('',*,*,#5930,.T.);
#8406=ORIENTED_EDGE('',*,*,#5931,.T.);
#8407=ORIENTED_EDGE('',*,*,#5932,.F.);
#8408=ORIENTED_EDGE('',*,*,#5931,.F.);
#8409=ORIENTED_EDGE('',*,*,#5932,.T.);
#8410=ORIENTED_EDGE('',*,*,#5930,.F.);
#8411=ORIENTED_EDGE('',*,*,#5933,.F.);
#8412=ORIENTED_EDGE('',*,*,#5934,.T.);
#8413=ORIENTED_EDGE('',*,*,#5935,.T.);
#8414=ORIENTED_EDGE('',*,*,#5934,.F.);
#8415=ORIENTED_EDGE('',*,*,#5933,.T.);
#8416=ORIENTED_EDGE('',*,*,#5936,.T.);
#8417=ORIENTED_EDGE('',*,*,#5937,.F.);
#8418=ORIENTED_EDGE('',*,*,#5936,.F.);
#8419=ORIENTED_EDGE('',*,*,#5938,.F.);
#8420=ORIENTED_EDGE('',*,*,#5937,.T.);
#8421=ORIENTED_EDGE('',*,*,#5939,.F.);
#8422=ORIENTED_EDGE('',*,*,#5940,.T.);
#8423=ORIENTED_EDGE('',*,*,#5938,.T.);
#8424=ORIENTED_EDGE('',*,*,#5940,.F.);
#8425=ORIENTED_EDGE('',*,*,#5941,.F.);
#8426=ORIENTED_EDGE('',*,*,#5939,.T.);
#8427=ORIENTED_EDGE('',*,*,#5942,.F.);
#8428=ORIENTED_EDGE('',*,*,#5943,.T.);
#8429=ORIENTED_EDGE('',*,*,#5941,.T.);
#8430=ORIENTED_EDGE('',*,*,#5943,.F.);
#8431=ORIENTED_EDGE('',*,*,#5944,.F.);
#8432=ORIENTED_EDGE('',*,*,#5942,.T.);
#8433=ORIENTED_EDGE('',*,*,#5945,.F.);
#8434=ORIENTED_EDGE('',*,*,#5946,.T.);
#8435=ORIENTED_EDGE('',*,*,#5944,.T.);
#8436=ORIENTED_EDGE('',*,*,#5946,.F.);
#8437=ORIENTED_EDGE('',*,*,#5947,.F.);
#8438=ORIENTED_EDGE('',*,*,#5948,.T.);
#8439=ORIENTED_EDGE('',*,*,#5945,.T.);
#8440=ORIENTED_EDGE('',*,*,#5948,.F.);
#8441=ORIENTED_EDGE('',*,*,#5947,.T.);
#8442=ORIENTED_EDGE('',*,*,#5949,.T.);
#8443=ORIENTED_EDGE('',*,*,#5950,.F.);
#8444=ORIENTED_EDGE('',*,*,#5949,.F.);
#8445=ORIENTED_EDGE('',*,*,#5950,.T.);
#8446=ORIENTED_EDGE('',*,*,#5951,.F.);
#8447=ORIENTED_EDGE('',*,*,#5952,.F.);
#8448=ORIENTED_EDGE('',*,*,#5953,.T.);
#8449=ORIENTED_EDGE('',*,*,#5951,.T.);
#8450=ORIENTED_EDGE('',*,*,#5953,.F.);
#8451=ORIENTED_EDGE('',*,*,#5952,.T.);
#8452=ORIENTED_EDGE('',*,*,#5954,.F.);
#8453=ORIENTED_EDGE('',*,*,#5955,.F.);
#8454=ORIENTED_EDGE('',*,*,#5956,.T.);
#8455=ORIENTED_EDGE('',*,*,#5954,.T.);
#8456=ORIENTED_EDGE('',*,*,#5956,.F.);
#8457=ORIENTED_EDGE('',*,*,#5955,.T.);
#8458=ORIENTED_EDGE('',*,*,#5957,.F.);
#8459=ORIENTED_EDGE('',*,*,#5935,.F.);
#8460=ORIENTED_EDGE('',*,*,#5958,.T.);
#8461=ORIENTED_EDGE('',*,*,#5957,.T.);
#8462=ORIENTED_EDGE('',*,*,#5958,.F.);
#8463=ORIENTED_EDGE('',*,*,#5959,.F.);
#8464=ORIENTED_EDGE('',*,*,#5960,.T.);
#8465=ORIENTED_EDGE('',*,*,#5961,.F.);
#8466=ORIENTED_EDGE('',*,*,#5962,.F.);
#8467=ORIENTED_EDGE('',*,*,#5963,.F.);
#8468=ORIENTED_EDGE('',*,*,#5964,.F.);
#8469=ORIENTED_EDGE('',*,*,#5965,.F.);
#8470=ORIENTED_EDGE('',*,*,#5966,.F.);
#8471=ORIENTED_EDGE('',*,*,#5967,.T.);
#8472=ORIENTED_EDGE('',*,*,#5968,.T.);
#8473=ORIENTED_EDGE('',*,*,#5969,.F.);
#8474=ORIENTED_EDGE('',*,*,#5961,.T.);
#8475=ORIENTED_EDGE('',*,*,#5970,.T.);
#8476=ORIENTED_EDGE('',*,*,#5967,.F.);
#8477=ORIENTED_EDGE('',*,*,#5971,.F.);
#8478=ORIENTED_EDGE('',*,*,#5968,.F.);
#8479=ORIENTED_EDGE('',*,*,#5970,.F.);
#8480=ORIENTED_EDGE('',*,*,#5960,.F.);
#8481=ORIENTED_EDGE('',*,*,#5962,.T.);
#8482=ORIENTED_EDGE('',*,*,#5969,.T.);
#8483=ORIENTED_EDGE('',*,*,#5966,.T.);
#8484=ORIENTED_EDGE('',*,*,#5972,.T.);
#8485=ORIENTED_EDGE('',*,*,#5973,.T.);
#8486=ORIENTED_EDGE('',*,*,#5974,.T.);
#8487=ORIENTED_EDGE('',*,*,#5975,.T.);
#8488=ORIENTED_EDGE('',*,*,#5976,.T.);
#8489=ORIENTED_EDGE('',*,*,#5977,.T.);
#8490=ORIENTED_EDGE('',*,*,#5978,.T.);
#8491=ORIENTED_EDGE('',*,*,#5979,.T.);
#8492=ORIENTED_EDGE('',*,*,#5980,.T.);
#8493=ORIENTED_EDGE('',*,*,#5981,.T.);
#8494=ORIENTED_EDGE('',*,*,#5982,.T.);
#8495=ORIENTED_EDGE('',*,*,#5983,.T.);
#8496=ORIENTED_EDGE('',*,*,#5984,.T.);
#8497=ORIENTED_EDGE('',*,*,#5985,.T.);
#8498=ORIENTED_EDGE('',*,*,#5986,.T.);
#8499=ORIENTED_EDGE('',*,*,#5987,.T.);
#8500=ORIENTED_EDGE('',*,*,#5988,.T.);
#8501=ORIENTED_EDGE('',*,*,#5989,.T.);
#8502=ORIENTED_EDGE('',*,*,#5990,.T.);
#8503=ORIENTED_EDGE('',*,*,#5991,.T.);
#8504=ORIENTED_EDGE('',*,*,#5992,.T.);
#8505=ORIENTED_EDGE('',*,*,#5993,.T.);
#8506=ORIENTED_EDGE('',*,*,#5994,.T.);
#8507=ORIENTED_EDGE('',*,*,#5995,.T.);
#8508=ORIENTED_EDGE('',*,*,#5996,.T.);
#8509=ORIENTED_EDGE('',*,*,#5997,.T.);
#8510=ORIENTED_EDGE('',*,*,#5998,.T.);
#8511=ORIENTED_EDGE('',*,*,#5999,.T.);
#8512=ORIENTED_EDGE('',*,*,#6000,.T.);
#8513=ORIENTED_EDGE('',*,*,#6001,.F.);
#8514=ORIENTED_EDGE('',*,*,#5965,.T.);
#8515=ORIENTED_EDGE('',*,*,#6002,.T.);
#8516=ORIENTED_EDGE('',*,*,#6003,.T.);
#8517=ORIENTED_EDGE('',*,*,#5972,.F.);
#8518=ORIENTED_EDGE('',*,*,#5963,.T.);
#8519=ORIENTED_EDGE('',*,*,#6000,.F.);
#8520=ORIENTED_EDGE('',*,*,#6004,.T.);
#8521=ORIENTED_EDGE('',*,*,#6005,.T.);
#8522=ORIENTED_EDGE('',*,*,#6006,.F.);
#8523=ORIENTED_EDGE('',*,*,#6007,.T.);
#8524=ORIENTED_EDGE('',*,*,#6008,.F.);
#8525=ORIENTED_EDGE('',*,*,#5997,.F.);
#8526=ORIENTED_EDGE('',*,*,#6009,.F.);
#8527=ORIENTED_EDGE('',*,*,#6010,.F.);
#8528=ORIENTED_EDGE('',*,*,#6004,.F.);
#8529=ORIENTED_EDGE('',*,*,#5999,.F.);
#8530=ORIENTED_EDGE('',*,*,#6011,.T.);
#8531=ORIENTED_EDGE('',*,*,#6012,.T.);
#8532=ORIENTED_EDGE('',*,*,#5998,.F.);
#8533=ORIENTED_EDGE('',*,*,#6008,.T.);
#8534=ORIENTED_EDGE('',*,*,#6013,.T.);
#8535=ORIENTED_EDGE('',*,*,#6011,.F.);
#8536=ORIENTED_EDGE('',*,*,#6014,.F.);
#8537=ORIENTED_EDGE('',*,*,#6012,.F.);
#8538=ORIENTED_EDGE('',*,*,#6013,.F.);
#8539=ORIENTED_EDGE('',*,*,#6007,.F.);
#8540=ORIENTED_EDGE('',*,*,#6009,.T.);
#8541=ORIENTED_EDGE('',*,*,#5996,.F.);
#8542=ORIENTED_EDGE('',*,*,#6015,.T.);
#8543=ORIENTED_EDGE('',*,*,#6016,.T.);
#8544=ORIENTED_EDGE('',*,*,#6017,.F.);
#8545=ORIENTED_EDGE('',*,*,#6018,.T.);
#8546=ORIENTED_EDGE('',*,*,#6019,.F.);
#8547=ORIENTED_EDGE('',*,*,#5993,.F.);
#8548=ORIENTED_EDGE('',*,*,#6020,.F.);
#8549=ORIENTED_EDGE('',*,*,#6021,.F.);
#8550=ORIENTED_EDGE('',*,*,#6015,.F.);
#8551=ORIENTED_EDGE('',*,*,#5995,.F.);
#8552=ORIENTED_EDGE('',*,*,#6022,.T.);
#8553=ORIENTED_EDGE('',*,*,#6023,.T.);
#8554=ORIENTED_EDGE('',*,*,#5994,.F.);
#8555=ORIENTED_EDGE('',*,*,#6019,.T.);
#8556=ORIENTED_EDGE('',*,*,#6024,.T.);
#8557=ORIENTED_EDGE('',*,*,#6022,.F.);
#8558=ORIENTED_EDGE('',*,*,#6025,.F.);
#8559=ORIENTED_EDGE('',*,*,#6023,.F.);
#8560=ORIENTED_EDGE('',*,*,#6024,.F.);
#8561=ORIENTED_EDGE('',*,*,#6018,.F.);
#8562=ORIENTED_EDGE('',*,*,#6020,.T.);
#8563=ORIENTED_EDGE('',*,*,#5992,.F.);
#8564=ORIENTED_EDGE('',*,*,#6026,.T.);
#8565=ORIENTED_EDGE('',*,*,#6027,.T.);
#8566=ORIENTED_EDGE('',*,*,#6028,.F.);
#8567=ORIENTED_EDGE('',*,*,#6029,.T.);
#8568=ORIENTED_EDGE('',*,*,#6030,.F.);
#8569=ORIENTED_EDGE('',*,*,#5989,.F.);
#8570=ORIENTED_EDGE('',*,*,#6031,.F.);
#8571=ORIENTED_EDGE('',*,*,#6032,.F.);
#8572=ORIENTED_EDGE('',*,*,#6026,.F.);
#8573=ORIENTED_EDGE('',*,*,#5991,.F.);
#8574=ORIENTED_EDGE('',*,*,#6033,.T.);
#8575=ORIENTED_EDGE('',*,*,#6034,.T.);
#8576=ORIENTED_EDGE('',*,*,#5990,.F.);
#8577=ORIENTED_EDGE('',*,*,#6030,.T.);
#8578=ORIENTED_EDGE('',*,*,#6035,.T.);
#8579=ORIENTED_EDGE('',*,*,#6033,.F.);
#8580=ORIENTED_EDGE('',*,*,#6036,.F.);
#8581=ORIENTED_EDGE('',*,*,#6034,.F.);
#8582=ORIENTED_EDGE('',*,*,#6035,.F.);
#8583=ORIENTED_EDGE('',*,*,#6029,.F.);
#8584=ORIENTED_EDGE('',*,*,#6037,.F.);
#8585=ORIENTED_EDGE('',*,*,#6031,.T.);
#8586=ORIENTED_EDGE('',*,*,#5988,.F.);
#8587=ORIENTED_EDGE('',*,*,#6038,.T.);
#8588=ORIENTED_EDGE('',*,*,#6039,.T.);
#8589=ORIENTED_EDGE('',*,*,#6040,.F.);
#8590=ORIENTED_EDGE('',*,*,#6041,.T.);
#8591=ORIENTED_EDGE('',*,*,#6042,.F.);
#8592=ORIENTED_EDGE('',*,*,#5985,.F.);
#8593=ORIENTED_EDGE('',*,*,#6043,.F.);
#8594=ORIENTED_EDGE('',*,*,#6044,.F.);
#8595=ORIENTED_EDGE('',*,*,#6038,.F.);
#8596=ORIENTED_EDGE('',*,*,#5987,.F.);
#8597=ORIENTED_EDGE('',*,*,#6045,.T.);
#8598=ORIENTED_EDGE('',*,*,#6046,.T.);
#8599=ORIENTED_EDGE('',*,*,#5986,.F.);
#8600=ORIENTED_EDGE('',*,*,#6042,.T.);
#8601=ORIENTED_EDGE('',*,*,#6047,.T.);
#8602=ORIENTED_EDGE('',*,*,#6045,.F.);
#8603=ORIENTED_EDGE('',*,*,#6048,.F.);
#8604=ORIENTED_EDGE('',*,*,#6046,.F.);
#8605=ORIENTED_EDGE('',*,*,#6047,.F.);
#8606=ORIENTED_EDGE('',*,*,#6041,.F.);
#8607=ORIENTED_EDGE('',*,*,#6043,.T.);
#8608=ORIENTED_EDGE('',*,*,#5984,.F.);
#8609=ORIENTED_EDGE('',*,*,#6049,.T.);
#8610=ORIENTED_EDGE('',*,*,#6050,.T.);
#8611=ORIENTED_EDGE('',*,*,#6051,.F.);
#8612=ORIENTED_EDGE('',*,*,#6052,.T.);
#8613=ORIENTED_EDGE('',*,*,#6053,.F.);
#8614=ORIENTED_EDGE('',*,*,#5981,.F.);
#8615=ORIENTED_EDGE('',*,*,#6054,.F.);
#8616=ORIENTED_EDGE('',*,*,#6055,.F.);
#8617=ORIENTED_EDGE('',*,*,#6049,.F.);
#8618=ORIENTED_EDGE('',*,*,#5983,.F.);
#8619=ORIENTED_EDGE('',*,*,#6056,.T.);
#8620=ORIENTED_EDGE('',*,*,#6057,.T.);
#8621=ORIENTED_EDGE('',*,*,#5982,.F.);
#8622=ORIENTED_EDGE('',*,*,#6053,.T.);
#8623=ORIENTED_EDGE('',*,*,#6058,.T.);
#8624=ORIENTED_EDGE('',*,*,#6056,.F.);
#8625=ORIENTED_EDGE('',*,*,#6059,.F.);
#8626=ORIENTED_EDGE('',*,*,#6057,.F.);
#8627=ORIENTED_EDGE('',*,*,#6058,.F.);
#8628=ORIENTED_EDGE('',*,*,#6052,.F.);
#8629=ORIENTED_EDGE('',*,*,#6054,.T.);
#8630=ORIENTED_EDGE('',*,*,#5980,.F.);
#8631=ORIENTED_EDGE('',*,*,#6060,.T.);
#8632=ORIENTED_EDGE('',*,*,#6061,.T.);
#8633=ORIENTED_EDGE('',*,*,#6060,.F.);
#8634=ORIENTED_EDGE('',*,*,#5979,.F.);
#8635=ORIENTED_EDGE('',*,*,#6062,.T.);
#8636=ORIENTED_EDGE('',*,*,#6063,.T.);
#8637=ORIENTED_EDGE('',*,*,#6064,.F.);
#8638=ORIENTED_EDGE('',*,*,#6065,.F.);
#8639=ORIENTED_EDGE('',*,*,#6066,.F.);
#8640=ORIENTED_EDGE('',*,*,#6067,.T.);
#8641=ORIENTED_EDGE('',*,*,#6068,.F.);
#8642=ORIENTED_EDGE('',*,*,#5977,.F.);
#8643=ORIENTED_EDGE('',*,*,#5978,.F.);
#8644=ORIENTED_EDGE('',*,*,#6068,.T.);
#8645=ORIENTED_EDGE('',*,*,#6069,.T.);
#8646=ORIENTED_EDGE('',*,*,#6062,.F.);
#8647=ORIENTED_EDGE('',*,*,#6070,.F.);
#8648=ORIENTED_EDGE('',*,*,#6063,.F.);
#8649=ORIENTED_EDGE('',*,*,#6069,.F.);
#8650=ORIENTED_EDGE('',*,*,#6067,.F.);
#8651=ORIENTED_EDGE('',*,*,#6065,.T.);
#8652=ORIENTED_EDGE('',*,*,#5976,.F.);
#8653=ORIENTED_EDGE('',*,*,#6071,.T.);
#8654=ORIENTED_EDGE('',*,*,#6072,.T.);
#8655=ORIENTED_EDGE('',*,*,#6071,.F.);
#8656=ORIENTED_EDGE('',*,*,#5975,.F.);
#8657=ORIENTED_EDGE('',*,*,#6073,.T.);
#8658=ORIENTED_EDGE('',*,*,#6074,.T.);
#8659=ORIENTED_EDGE('',*,*,#6075,.F.);
#8660=ORIENTED_EDGE('',*,*,#6003,.F.);
#8661=ORIENTED_EDGE('',*,*,#6076,.F.);
#8662=ORIENTED_EDGE('',*,*,#6077,.T.);
#8663=ORIENTED_EDGE('',*,*,#6078,.F.);
#8664=ORIENTED_EDGE('',*,*,#5973,.F.);
#8665=ORIENTED_EDGE('',*,*,#5974,.F.);
#8666=ORIENTED_EDGE('',*,*,#6078,.T.);
#8667=ORIENTED_EDGE('',*,*,#6079,.T.);
#8668=ORIENTED_EDGE('',*,*,#6073,.F.);
#8669=ORIENTED_EDGE('',*,*,#6080,.F.);
#8670=ORIENTED_EDGE('',*,*,#6074,.F.);
#8671=ORIENTED_EDGE('',*,*,#6079,.F.);
#8672=ORIENTED_EDGE('',*,*,#6077,.F.);
#8673=ORIENTED_EDGE('',*,*,#6081,.F.);
#8674=ORIENTED_EDGE('',*,*,#6082,.T.);
#8675=ORIENTED_EDGE('',*,*,#6083,.T.);
#8676=ORIENTED_EDGE('',*,*,#6082,.F.);
#8677=ORIENTED_EDGE('',*,*,#6083,.F.);
#8678=ORIENTED_EDGE('',*,*,#6084,.F.);
#8679=ORIENTED_EDGE('',*,*,#6084,.T.);
#8680=ORIENTED_EDGE('',*,*,#6085,.T.);
#8681=ORIENTED_EDGE('',*,*,#6086,.T.);
#8682=ORIENTED_EDGE('',*,*,#6085,.F.);
#8683=ORIENTED_EDGE('',*,*,#6087,.F.);
#8684=ORIENTED_EDGE('',*,*,#6081,.T.);
#8685=ORIENTED_EDGE('',*,*,#6036,.T.);
#8686=ORIENTED_EDGE('',*,*,#6088,.T.);
#8687=ORIENTED_EDGE('',*,*,#6087,.T.);
#8688=ORIENTED_EDGE('',*,*,#6088,.F.);
#8689=ORIENTED_EDGE('',*,*,#6037,.T.);
#8690=ORIENTED_EDGE('',*,*,#6028,.T.);
#8691=ORIENTED_EDGE('',*,*,#6039,.F.);
#8692=ORIENTED_EDGE('',*,*,#6044,.T.);
#8693=ORIENTED_EDGE('',*,*,#6048,.T.);
#8694=ORIENTED_EDGE('',*,*,#6040,.T.);
#8695=ORIENTED_EDGE('',*,*,#6050,.F.);
#8696=ORIENTED_EDGE('',*,*,#6055,.T.);
#8697=ORIENTED_EDGE('',*,*,#6059,.T.);
#8698=ORIENTED_EDGE('',*,*,#6051,.T.);
#8699=ORIENTED_EDGE('',*,*,#6061,.F.);
#8700=ORIENTED_EDGE('',*,*,#6064,.T.);
#8701=ORIENTED_EDGE('',*,*,#6070,.T.);
#8702=ORIENTED_EDGE('',*,*,#6066,.T.);
#8703=ORIENTED_EDGE('',*,*,#6072,.F.);
#8704=ORIENTED_EDGE('',*,*,#6075,.T.);
#8705=ORIENTED_EDGE('',*,*,#6080,.T.);
#8706=ORIENTED_EDGE('',*,*,#6076,.T.);
#8707=ORIENTED_EDGE('',*,*,#6002,.F.);
#8708=ORIENTED_EDGE('',*,*,#5964,.T.);
#8709=ORIENTED_EDGE('',*,*,#5971,.T.);
#8710=ORIENTED_EDGE('',*,*,#5959,.T.);
#8711=ORIENTED_EDGE('',*,*,#6005,.F.);
#8712=ORIENTED_EDGE('',*,*,#6010,.T.);
#8713=ORIENTED_EDGE('',*,*,#6014,.T.);
#8714=ORIENTED_EDGE('',*,*,#6006,.T.);
#8715=ORIENTED_EDGE('',*,*,#6016,.F.);
#8716=ORIENTED_EDGE('',*,*,#6021,.T.);
#8717=ORIENTED_EDGE('',*,*,#6025,.T.);
#8718=ORIENTED_EDGE('',*,*,#6017,.T.);
#8719=ORIENTED_EDGE('',*,*,#6027,.F.);
#8720=ORIENTED_EDGE('',*,*,#6032,.T.);
#8721=ORIENTED_EDGE('',*,*,#6089,.F.);
#8722=ORIENTED_EDGE('',*,*,#6090,.T.);
#8723=ORIENTED_EDGE('',*,*,#6001,.T.);
#8724=ORIENTED_EDGE('',*,*,#6090,.F.);
#8725=ORIENTED_EDGE('',*,*,#6089,.T.);
#8726=ORIENTED_EDGE('',*,*,#6086,.F.);
#8727=ORIENTED_EDGE('',*,*,#6091,.F.);
#8728=ORIENTED_EDGE('',*,*,#6092,.T.);
#8729=ORIENTED_EDGE('',*,*,#6093,.T.);
#8730=ORIENTED_EDGE('',*,*,#6094,.F.);
#8731=ORIENTED_EDGE('',*,*,#6095,.F.);
#8732=ORIENTED_EDGE('',*,*,#6096,.F.);
#8733=ORIENTED_EDGE('',*,*,#6097,.F.);
#8734=ORIENTED_EDGE('',*,*,#6098,.T.);
#8735=ORIENTED_EDGE('',*,*,#6099,.T.);
#8736=ORIENTED_EDGE('',*,*,#6097,.T.);
#8737=ORIENTED_EDGE('',*,*,#6100,.F.);
#8738=ORIENTED_EDGE('',*,*,#6093,.F.);
#8739=ORIENTED_EDGE('',*,*,#6101,.T.);
#8740=ORIENTED_EDGE('',*,*,#6094,.T.);
#8741=ORIENTED_EDGE('',*,*,#6100,.T.);
#8742=ORIENTED_EDGE('',*,*,#6096,.T.);
#8743=ORIENTED_EDGE('',*,*,#6102,.T.);
#8744=ORIENTED_EDGE('',*,*,#6103,.T.);
#8745=ORIENTED_EDGE('',*,*,#6104,.T.);
#8746=ORIENTED_EDGE('',*,*,#6102,.F.);
#8747=ORIENTED_EDGE('',*,*,#6104,.F.);
#8748=ORIENTED_EDGE('',*,*,#6091,.T.);
#8749=ORIENTED_EDGE('',*,*,#6101,.F.);
#8750=ORIENTED_EDGE('',*,*,#6095,.T.);
#8751=ORIENTED_EDGE('',*,*,#6105,.T.);
#8752=ORIENTED_EDGE('',*,*,#6105,.F.);
#8753=ORIENTED_EDGE('',*,*,#6098,.F.);
#8754=ORIENTED_EDGE('',*,*,#6099,.F.);
#8755=ORIENTED_EDGE('',*,*,#6092,.F.);
#8756=ORIENTED_EDGE('',*,*,#6103,.F.);
#8757=ORIENTED_EDGE('',*,*,#6106,.F.);
#8758=ORIENTED_EDGE('',*,*,#6107,.T.);
#8759=ORIENTED_EDGE('',*,*,#6108,.T.);
#8760=ORIENTED_EDGE('',*,*,#6107,.F.);
#8761=ORIENTED_EDGE('',*,*,#6106,.T.);
#8762=ORIENTED_EDGE('',*,*,#6109,.T.);
#8763=ORIENTED_EDGE('',*,*,#6110,.F.);
#8764=ORIENTED_EDGE('',*,*,#6109,.F.);
#8765=ORIENTED_EDGE('',*,*,#6111,.F.);
#8766=ORIENTED_EDGE('',*,*,#6110,.T.);
#8767=ORIENTED_EDGE('',*,*,#6112,.F.);
#8768=ORIENTED_EDGE('',*,*,#6113,.T.);
#8769=ORIENTED_EDGE('',*,*,#6111,.T.);
#8770=ORIENTED_EDGE('',*,*,#6113,.F.);
#8771=ORIENTED_EDGE('',*,*,#6114,.F.);
#8772=ORIENTED_EDGE('',*,*,#6112,.T.);
#8773=ORIENTED_EDGE('',*,*,#6115,.F.);
#8774=ORIENTED_EDGE('',*,*,#6116,.T.);
#8775=ORIENTED_EDGE('',*,*,#6114,.T.);
#8776=ORIENTED_EDGE('',*,*,#6116,.F.);
#8777=ORIENTED_EDGE('',*,*,#6117,.F.);
#8778=ORIENTED_EDGE('',*,*,#6115,.T.);
#8779=ORIENTED_EDGE('',*,*,#6118,.F.);
#8780=ORIENTED_EDGE('',*,*,#6119,.T.);
#8781=ORIENTED_EDGE('',*,*,#6117,.T.);
#8782=ORIENTED_EDGE('',*,*,#6119,.F.);
#8783=ORIENTED_EDGE('',*,*,#6120,.F.);
#8784=ORIENTED_EDGE('',*,*,#6121,.T.);
#8785=ORIENTED_EDGE('',*,*,#6118,.T.);
#8786=ORIENTED_EDGE('',*,*,#6121,.F.);
#8787=ORIENTED_EDGE('',*,*,#6120,.T.);
#8788=ORIENTED_EDGE('',*,*,#6122,.T.);
#8789=ORIENTED_EDGE('',*,*,#6123,.F.);
#8790=ORIENTED_EDGE('',*,*,#6122,.F.);
#8791=ORIENTED_EDGE('',*,*,#6123,.T.);
#8792=ORIENTED_EDGE('',*,*,#6124,.F.);
#8793=ORIENTED_EDGE('',*,*,#6125,.F.);
#8794=ORIENTED_EDGE('',*,*,#6126,.T.);
#8795=ORIENTED_EDGE('',*,*,#6124,.T.);
#8796=ORIENTED_EDGE('',*,*,#6126,.F.);
#8797=ORIENTED_EDGE('',*,*,#6125,.T.);
#8798=ORIENTED_EDGE('',*,*,#6127,.F.);
#8799=ORIENTED_EDGE('',*,*,#6128,.F.);
#8800=ORIENTED_EDGE('',*,*,#6129,.T.);
#8801=ORIENTED_EDGE('',*,*,#6127,.T.);
#8802=ORIENTED_EDGE('',*,*,#6129,.F.);
#8803=ORIENTED_EDGE('',*,*,#6128,.T.);
#8804=ORIENTED_EDGE('',*,*,#6130,.F.);
#8805=ORIENTED_EDGE('',*,*,#6108,.F.);
#8806=ORIENTED_EDGE('',*,*,#6131,.T.);
#8807=ORIENTED_EDGE('',*,*,#6130,.T.);
#8808=ORIENTED_EDGE('',*,*,#6131,.F.);
#8809=ORIENTED_EDGE('',*,*,#6132,.F.);
#8810=ORIENTED_EDGE('',*,*,#6133,.T.);
#8811=ORIENTED_EDGE('',*,*,#6134,.T.);
#8812=ORIENTED_EDGE('',*,*,#6133,.F.);
#8813=ORIENTED_EDGE('',*,*,#6132,.T.);
#8814=ORIENTED_EDGE('',*,*,#6135,.T.);
#8815=ORIENTED_EDGE('',*,*,#6136,.F.);
#8816=ORIENTED_EDGE('',*,*,#6135,.F.);
#8817=ORIENTED_EDGE('',*,*,#6137,.F.);
#8818=ORIENTED_EDGE('',*,*,#6136,.T.);
#8819=ORIENTED_EDGE('',*,*,#6138,.F.);
#8820=ORIENTED_EDGE('',*,*,#6139,.T.);
#8821=ORIENTED_EDGE('',*,*,#6137,.T.);
#8822=ORIENTED_EDGE('',*,*,#6139,.F.);
#8823=ORIENTED_EDGE('',*,*,#6140,.F.);
#8824=ORIENTED_EDGE('',*,*,#6141,.T.);
#8825=ORIENTED_EDGE('',*,*,#6138,.T.);
#8826=ORIENTED_EDGE('',*,*,#6141,.F.);
#8827=ORIENTED_EDGE('',*,*,#6140,.T.);
#8828=ORIENTED_EDGE('',*,*,#6142,.T.);
#8829=ORIENTED_EDGE('',*,*,#6143,.F.);
#8830=ORIENTED_EDGE('',*,*,#6142,.F.);
#8831=ORIENTED_EDGE('',*,*,#6143,.T.);
#8832=ORIENTED_EDGE('',*,*,#6144,.F.);
#8833=ORIENTED_EDGE('',*,*,#6134,.F.);
#8834=ORIENTED_EDGE('',*,*,#6145,.T.);
#8835=ORIENTED_EDGE('',*,*,#6144,.T.);
#8836=ORIENTED_EDGE('',*,*,#6145,.F.);
#8837=ORIENTED_EDGE('',*,*,#6146,.F.);
#8838=ORIENTED_EDGE('',*,*,#6147,.F.);
#8839=ORIENTED_EDGE('',*,*,#6148,.T.);
#8840=ORIENTED_EDGE('',*,*,#6146,.T.);
#8841=ORIENTED_EDGE('',*,*,#6148,.F.);
#8842=ORIENTED_EDGE('',*,*,#6149,.F.);
#8843=ORIENTED_EDGE('',*,*,#6150,.T.);
#8844=ORIENTED_EDGE('',*,*,#6147,.T.);
#8845=ORIENTED_EDGE('',*,*,#6150,.F.);
#8846=ORIENTED_EDGE('',*,*,#6149,.T.);
#8847=ORIENTED_EDGE('',*,*,#6151,.F.);
#8848=ORIENTED_EDGE('',*,*,#6152,.F.);
#8849=ORIENTED_EDGE('',*,*,#6153,.T.);
#8850=ORIENTED_EDGE('',*,*,#6151,.T.);
#8851=ORIENTED_EDGE('',*,*,#6153,.F.);
#8852=ORIENTED_EDGE('',*,*,#6154,.F.);
#8853=ORIENTED_EDGE('',*,*,#6152,.T.);
#8854=ORIENTED_EDGE('',*,*,#6155,.F.);
#8855=ORIENTED_EDGE('',*,*,#6156,.T.);
#8856=ORIENTED_EDGE('',*,*,#6154,.T.);
#8857=ORIENTED_EDGE('',*,*,#6156,.F.);
#8858=ORIENTED_EDGE('',*,*,#6155,.T.);
#8859=ORIENTED_EDGE('',*,*,#6157,.T.);
#8860=ORIENTED_EDGE('',*,*,#6158,.F.);
#8861=ORIENTED_EDGE('',*,*,#6157,.F.);
#8862=ORIENTED_EDGE('',*,*,#6158,.T.);
#8863=ORIENTED_EDGE('',*,*,#6159,.F.);
#8864=ORIENTED_EDGE('',*,*,#6160,.F.);
#8865=ORIENTED_EDGE('',*,*,#6161,.T.);
#8866=ORIENTED_EDGE('',*,*,#6159,.T.);
#8867=ORIENTED_EDGE('',*,*,#6161,.F.);
#8868=ORIENTED_EDGE('',*,*,#6162,.F.);
#8869=ORIENTED_EDGE('',*,*,#6163,.T.);
#8870=ORIENTED_EDGE('',*,*,#6160,.T.);
#8871=ORIENTED_EDGE('',*,*,#6163,.F.);
#8872=ORIENTED_EDGE('',*,*,#6162,.T.);
#8873=ORIENTED_EDGE('',*,*,#6164,.F.);
#8874=ORIENTED_EDGE('',*,*,#6165,.F.);
#8875=ORIENTED_EDGE('',*,*,#6166,.T.);
#8876=ORIENTED_EDGE('',*,*,#6164,.T.);
#8877=ORIENTED_EDGE('',*,*,#6166,.F.);
#8878=ORIENTED_EDGE('',*,*,#6167,.F.);
#8879=ORIENTED_EDGE('',*,*,#6165,.T.);
#8880=ORIENTED_EDGE('',*,*,#6168,.F.);
#8881=ORIENTED_EDGE('',*,*,#6169,.T.);
#8882=ORIENTED_EDGE('',*,*,#6167,.T.);
#8883=ORIENTED_EDGE('',*,*,#6169,.F.);
#8884=ORIENTED_EDGE('',*,*,#6168,.T.);
#8885=ORIENTED_EDGE('',*,*,#6170,.T.);
#8886=ORIENTED_EDGE('',*,*,#6171,.F.);
#8887=ORIENTED_EDGE('',*,*,#6170,.F.);
#8888=ORIENTED_EDGE('',*,*,#6171,.T.);
#8889=ORIENTED_EDGE('',*,*,#6172,.T.);
#8890=ORIENTED_EDGE('',*,*,#6173,.T.);
#8891=ORIENTED_EDGE('',*,*,#6174,.T.);
#8892=ORIENTED_EDGE('',*,*,#6173,.F.);
#8893=ORIENTED_EDGE('',*,*,#6174,.F.);
#8894=ORIENTED_EDGE('',*,*,#6175,.T.);
#8895=ORIENTED_EDGE('',*,*,#6176,.T.);
#8896=ORIENTED_EDGE('',*,*,#6175,.F.);
#8897=ORIENTED_EDGE('',*,*,#6172,.F.);
#8898=ORIENTED_EDGE('',*,*,#6177,.F.);
#8899=ORIENTED_EDGE('',*,*,#6176,.F.);
#8900=ORIENTED_EDGE('',*,*,#6178,.T.);
#8901=ORIENTED_EDGE('',*,*,#6177,.T.);
#8902=ORIENTED_EDGE('',*,*,#6178,.F.);
#8903=ORIENTED_EDGE('',*,*,#6179,.F.);
#8904=ORIENTED_EDGE('',*,*,#6180,.F.);
#8905=ORIENTED_EDGE('',*,*,#6181,.F.);
#8906=ORIENTED_EDGE('',*,*,#6182,.T.);
#8907=ORIENTED_EDGE('',*,*,#6183,.F.);
#8908=ORIENTED_EDGE('',*,*,#6184,.F.);
#8909=ORIENTED_EDGE('',*,*,#6185,.F.);
#8910=ORIENTED_EDGE('',*,*,#6179,.T.);
#8911=ORIENTED_EDGE('',*,*,#6186,.T.);
#8912=ORIENTED_EDGE('',*,*,#6187,.T.);
#8913=ORIENTED_EDGE('',*,*,#6188,.F.);
#8914=ORIENTED_EDGE('',*,*,#6189,.F.);
#8915=ORIENTED_EDGE('',*,*,#6190,.F.);
#8916=ORIENTED_EDGE('',*,*,#6183,.T.);
#8917=ORIENTED_EDGE('',*,*,#6191,.T.);
#8918=ORIENTED_EDGE('',*,*,#6192,.F.);
#8919=ORIENTED_EDGE('',*,*,#6193,.F.);
#8920=ORIENTED_EDGE('',*,*,#6194,.F.);
#8921=ORIENTED_EDGE('',*,*,#6188,.T.);
#8922=ORIENTED_EDGE('',*,*,#6195,.T.);
#8923=ORIENTED_EDGE('',*,*,#6196,.T.);
#8924=ORIENTED_EDGE('',*,*,#6197,.F.);
#8925=ORIENTED_EDGE('',*,*,#6198,.F.);
#8926=ORIENTED_EDGE('',*,*,#6199,.F.);
#8927=ORIENTED_EDGE('',*,*,#6192,.T.);
#8928=ORIENTED_EDGE('',*,*,#6200,.T.);
#8929=ORIENTED_EDGE('',*,*,#6201,.F.);
#8930=ORIENTED_EDGE('',*,*,#6202,.F.);
#8931=ORIENTED_EDGE('',*,*,#6203,.F.);
#8932=ORIENTED_EDGE('',*,*,#6197,.T.);
#8933=ORIENTED_EDGE('',*,*,#6204,.T.);
#8934=ORIENTED_EDGE('',*,*,#6205,.T.);
#8935=ORIENTED_EDGE('',*,*,#6206,.F.);
#8936=ORIENTED_EDGE('',*,*,#6207,.F.);
#8937=ORIENTED_EDGE('',*,*,#6208,.F.);
#8938=ORIENTED_EDGE('',*,*,#6201,.T.);
#8939=ORIENTED_EDGE('',*,*,#6209,.T.);
#8940=ORIENTED_EDGE('',*,*,#6210,.F.);
#8941=ORIENTED_EDGE('',*,*,#6211,.F.);
#8942=ORIENTED_EDGE('',*,*,#6212,.F.);
#8943=ORIENTED_EDGE('',*,*,#6206,.T.);
#8944=ORIENTED_EDGE('',*,*,#6213,.T.);
#8945=ORIENTED_EDGE('',*,*,#6214,.T.);
#8946=ORIENTED_EDGE('',*,*,#6215,.F.);
#8947=ORIENTED_EDGE('',*,*,#6216,.F.);
#8948=ORIENTED_EDGE('',*,*,#6217,.F.);
#8949=ORIENTED_EDGE('',*,*,#6210,.T.);
#8950=ORIENTED_EDGE('',*,*,#6218,.T.);
#8951=ORIENTED_EDGE('',*,*,#6219,.F.);
#8952=ORIENTED_EDGE('',*,*,#6220,.F.);
#8953=ORIENTED_EDGE('',*,*,#6221,.F.);
#8954=ORIENTED_EDGE('',*,*,#6215,.T.);
#8955=ORIENTED_EDGE('',*,*,#6222,.T.);
#8956=ORIENTED_EDGE('',*,*,#6223,.T.);
#8957=ORIENTED_EDGE('',*,*,#6224,.F.);
#8958=ORIENTED_EDGE('',*,*,#6225,.F.);
#8959=ORIENTED_EDGE('',*,*,#6226,.F.);
#8960=ORIENTED_EDGE('',*,*,#6219,.T.);
#8961=ORIENTED_EDGE('',*,*,#6227,.T.);
#8962=ORIENTED_EDGE('',*,*,#6228,.F.);
#8963=ORIENTED_EDGE('',*,*,#6229,.F.);
#8964=ORIENTED_EDGE('',*,*,#6230,.F.);
#8965=ORIENTED_EDGE('',*,*,#6224,.T.);
#8966=ORIENTED_EDGE('',*,*,#6231,.T.);
#8967=ORIENTED_EDGE('',*,*,#6232,.T.);
#8968=ORIENTED_EDGE('',*,*,#6233,.F.);
#8969=ORIENTED_EDGE('',*,*,#6234,.F.);
#8970=ORIENTED_EDGE('',*,*,#6235,.F.);
#8971=ORIENTED_EDGE('',*,*,#6228,.T.);
#8972=ORIENTED_EDGE('',*,*,#6236,.T.);
#8973=ORIENTED_EDGE('',*,*,#6237,.F.);
#8974=ORIENTED_EDGE('',*,*,#6238,.F.);
#8975=ORIENTED_EDGE('',*,*,#6239,.F.);
#8976=ORIENTED_EDGE('',*,*,#6233,.T.);
#8977=ORIENTED_EDGE('',*,*,#6240,.T.);
#8978=ORIENTED_EDGE('',*,*,#6241,.T.);
#8979=ORIENTED_EDGE('',*,*,#6242,.T.);
#8980=ORIENTED_EDGE('',*,*,#6243,.T.);
#8981=ORIENTED_EDGE('',*,*,#6244,.T.);
#8982=ORIENTED_EDGE('',*,*,#6245,.T.);
#8983=ORIENTED_EDGE('',*,*,#6246,.T.);
#8984=ORIENTED_EDGE('',*,*,#6247,.T.);
#8985=ORIENTED_EDGE('',*,*,#6248,.T.);
#8986=ORIENTED_EDGE('',*,*,#6249,.T.);
#8987=ORIENTED_EDGE('',*,*,#6250,.T.);
#8988=ORIENTED_EDGE('',*,*,#6251,.T.);
#8989=ORIENTED_EDGE('',*,*,#6252,.T.);
#8990=ORIENTED_EDGE('',*,*,#6253,.T.);
#8991=ORIENTED_EDGE('',*,*,#6254,.T.);
#8992=ORIENTED_EDGE('',*,*,#6255,.T.);
#8993=ORIENTED_EDGE('',*,*,#6256,.T.);
#8994=ORIENTED_EDGE('',*,*,#6257,.T.);
#8995=ORIENTED_EDGE('',*,*,#6258,.T.);
#8996=ORIENTED_EDGE('',*,*,#6259,.F.);
#8997=ORIENTED_EDGE('',*,*,#6260,.T.);
#8998=ORIENTED_EDGE('',*,*,#6261,.T.);
#8999=ORIENTED_EDGE('',*,*,#6262,.T.);
#9000=ORIENTED_EDGE('',*,*,#6263,.T.);
#9001=ORIENTED_EDGE('',*,*,#6264,.T.);
#9002=ORIENTED_EDGE('',*,*,#6265,.T.);
#9003=ORIENTED_EDGE('',*,*,#6266,.T.);
#9004=ORIENTED_EDGE('',*,*,#6267,.T.);
#9005=ORIENTED_EDGE('',*,*,#6268,.T.);
#9006=ORIENTED_EDGE('',*,*,#6269,.T.);
#9007=ORIENTED_EDGE('',*,*,#6270,.T.);
#9008=ORIENTED_EDGE('',*,*,#6271,.T.);
#9009=ORIENTED_EDGE('',*,*,#6272,.T.);
#9010=ORIENTED_EDGE('',*,*,#6273,.T.);
#9011=ORIENTED_EDGE('',*,*,#6237,.T.);
#9012=ORIENTED_EDGE('',*,*,#6274,.T.);
#9013=ORIENTED_EDGE('',*,*,#6275,.T.);
#9014=ORIENTED_EDGE('',*,*,#6276,.F.);
#9015=ORIENTED_EDGE('',*,*,#6277,.F.);
#9016=ORIENTED_EDGE('',*,*,#6278,.F.);
#9017=ORIENTED_EDGE('',*,*,#6279,.F.);
#9018=ORIENTED_EDGE('',*,*,#6258,.F.);
#9019=ORIENTED_EDGE('',*,*,#6257,.F.);
#9020=ORIENTED_EDGE('',*,*,#6256,.F.);
#9021=ORIENTED_EDGE('',*,*,#6255,.F.);
#9022=ORIENTED_EDGE('',*,*,#6254,.F.);
#9023=ORIENTED_EDGE('',*,*,#6253,.F.);
#9024=ORIENTED_EDGE('',*,*,#6252,.F.);
#9025=ORIENTED_EDGE('',*,*,#6251,.F.);
#9026=ORIENTED_EDGE('',*,*,#6250,.F.);
#9027=ORIENTED_EDGE('',*,*,#6249,.F.);
#9028=ORIENTED_EDGE('',*,*,#6248,.F.);
#9029=ORIENTED_EDGE('',*,*,#6247,.F.);
#9030=ORIENTED_EDGE('',*,*,#6246,.F.);
#9031=ORIENTED_EDGE('',*,*,#6245,.F.);
#9032=ORIENTED_EDGE('',*,*,#6244,.F.);
#9033=ORIENTED_EDGE('',*,*,#6280,.F.);
#9034=ORIENTED_EDGE('',*,*,#6180,.T.);
#9035=ORIENTED_EDGE('',*,*,#6185,.T.);
#9036=ORIENTED_EDGE('',*,*,#6184,.T.);
#9037=ORIENTED_EDGE('',*,*,#6190,.T.);
#9038=ORIENTED_EDGE('',*,*,#6189,.T.);
#9039=ORIENTED_EDGE('',*,*,#6194,.T.);
#9040=ORIENTED_EDGE('',*,*,#6193,.T.);
#9041=ORIENTED_EDGE('',*,*,#6199,.T.);
#9042=ORIENTED_EDGE('',*,*,#6198,.T.);
#9043=ORIENTED_EDGE('',*,*,#6203,.T.);
#9044=ORIENTED_EDGE('',*,*,#6202,.T.);
#9045=ORIENTED_EDGE('',*,*,#6208,.T.);
#9046=ORIENTED_EDGE('',*,*,#6207,.T.);
#9047=ORIENTED_EDGE('',*,*,#6212,.T.);
#9048=ORIENTED_EDGE('',*,*,#6211,.T.);
#9049=ORIENTED_EDGE('',*,*,#6217,.T.);
#9050=ORIENTED_EDGE('',*,*,#6216,.T.);
#9051=ORIENTED_EDGE('',*,*,#6221,.T.);
#9052=ORIENTED_EDGE('',*,*,#6220,.T.);
#9053=ORIENTED_EDGE('',*,*,#6226,.T.);
#9054=ORIENTED_EDGE('',*,*,#6225,.T.);
#9055=ORIENTED_EDGE('',*,*,#6230,.T.);
#9056=ORIENTED_EDGE('',*,*,#6229,.T.);
#9057=ORIENTED_EDGE('',*,*,#6235,.T.);
#9058=ORIENTED_EDGE('',*,*,#6234,.T.);
#9059=ORIENTED_EDGE('',*,*,#6239,.T.);
#9060=ORIENTED_EDGE('',*,*,#6238,.T.);
#9061=ORIENTED_EDGE('',*,*,#6278,.T.);
#9062=ORIENTED_EDGE('',*,*,#6277,.T.);
#9063=ORIENTED_EDGE('',*,*,#6281,.T.);
#9064=ORIENTED_EDGE('',*,*,#6282,.T.);
#9065=ORIENTED_EDGE('',*,*,#6283,.T.);
#9066=ORIENTED_EDGE('',*,*,#6181,.T.);
#9067=ORIENTED_EDGE('',*,*,#6280,.T.);
#9068=ORIENTED_EDGE('',*,*,#6284,.F.);
#9069=ORIENTED_EDGE('',*,*,#6275,.F.);
#9070=ORIENTED_EDGE('',*,*,#6274,.F.);
#9071=ORIENTED_EDGE('',*,*,#6241,.F.);
#9072=ORIENTED_EDGE('',*,*,#6240,.F.);
#9073=ORIENTED_EDGE('',*,*,#6236,.F.);
#9074=ORIENTED_EDGE('',*,*,#6232,.F.);
#9075=ORIENTED_EDGE('',*,*,#6231,.F.);
#9076=ORIENTED_EDGE('',*,*,#6227,.F.);
#9077=ORIENTED_EDGE('',*,*,#6223,.F.);
#9078=ORIENTED_EDGE('',*,*,#6222,.F.);
#9079=ORIENTED_EDGE('',*,*,#6218,.F.);
#9080=ORIENTED_EDGE('',*,*,#6214,.F.);
#9081=ORIENTED_EDGE('',*,*,#6213,.F.);
#9082=ORIENTED_EDGE('',*,*,#6209,.F.);
#9083=ORIENTED_EDGE('',*,*,#6205,.F.);
#9084=ORIENTED_EDGE('',*,*,#6204,.F.);
#9085=ORIENTED_EDGE('',*,*,#6200,.F.);
#9086=ORIENTED_EDGE('',*,*,#6196,.F.);
#9087=ORIENTED_EDGE('',*,*,#6195,.F.);
#9088=ORIENTED_EDGE('',*,*,#6191,.F.);
#9089=ORIENTED_EDGE('',*,*,#6187,.F.);
#9090=ORIENTED_EDGE('',*,*,#6186,.F.);
#9091=ORIENTED_EDGE('',*,*,#6182,.F.);
#9092=ORIENTED_EDGE('',*,*,#6283,.F.);
#9093=ORIENTED_EDGE('',*,*,#6285,.T.);
#9094=ORIENTED_EDGE('',*,*,#6242,.F.);
#9095=ORIENTED_EDGE('',*,*,#6273,.F.);
#9096=ORIENTED_EDGE('',*,*,#6272,.F.);
#9097=ORIENTED_EDGE('',*,*,#6271,.F.);
#9098=ORIENTED_EDGE('',*,*,#6270,.F.);
#9099=ORIENTED_EDGE('',*,*,#6269,.F.);
#9100=ORIENTED_EDGE('',*,*,#6268,.F.);
#9101=ORIENTED_EDGE('',*,*,#6267,.F.);
#9102=ORIENTED_EDGE('',*,*,#6266,.F.);
#9103=ORIENTED_EDGE('',*,*,#6265,.F.);
#9104=ORIENTED_EDGE('',*,*,#6264,.F.);
#9105=ORIENTED_EDGE('',*,*,#6263,.F.);
#9106=ORIENTED_EDGE('',*,*,#6262,.F.);
#9107=ORIENTED_EDGE('',*,*,#6261,.F.);
#9108=ORIENTED_EDGE('',*,*,#6260,.F.);
#9109=ORIENTED_EDGE('',*,*,#6286,.F.);
#9110=ORIENTED_EDGE('',*,*,#6287,.F.);
#9111=ORIENTED_EDGE('',*,*,#6288,.F.);
#9112=ORIENTED_EDGE('',*,*,#6289,.F.);
#9113=ORIENTED_EDGE('',*,*,#6290,.F.);
#9114=ORIENTED_EDGE('',*,*,#6291,.F.);
#9115=ORIENTED_EDGE('',*,*,#6292,.F.);
#9116=ORIENTED_EDGE('',*,*,#6293,.F.);
#9117=ORIENTED_EDGE('',*,*,#6294,.F.);
#9118=ORIENTED_EDGE('',*,*,#6295,.F.);
#9119=ORIENTED_EDGE('',*,*,#6296,.F.);
#9120=ORIENTED_EDGE('',*,*,#6297,.F.);
#9121=ORIENTED_EDGE('',*,*,#6298,.F.);
#9122=ORIENTED_EDGE('',*,*,#6296,.T.);
#9123=ORIENTED_EDGE('',*,*,#6299,.T.);
#9124=ORIENTED_EDGE('',*,*,#6300,.T.);
#9125=ORIENTED_EDGE('',*,*,#6299,.F.);
#9126=ORIENTED_EDGE('',*,*,#6295,.T.);
#9127=ORIENTED_EDGE('',*,*,#6301,.T.);
#9128=ORIENTED_EDGE('',*,*,#6302,.T.);
#9129=ORIENTED_EDGE('',*,*,#6293,.T.);
#9130=ORIENTED_EDGE('',*,*,#6303,.T.);
#9131=ORIENTED_EDGE('',*,*,#6304,.T.);
#9132=ORIENTED_EDGE('',*,*,#6291,.T.);
#9133=ORIENTED_EDGE('',*,*,#6305,.T.);
#9134=ORIENTED_EDGE('',*,*,#6306,.T.);
#9135=ORIENTED_EDGE('',*,*,#6287,.T.);
#9136=ORIENTED_EDGE('',*,*,#6307,.T.);
#9137=ORIENTED_EDGE('',*,*,#6308,.T.);
#9138=ORIENTED_EDGE('',*,*,#6289,.T.);
#9139=ORIENTED_EDGE('',*,*,#6309,.T.);
#9140=ORIENTED_EDGE('',*,*,#6310,.T.);
#9141=ORIENTED_EDGE('',*,*,#6298,.T.);
#9142=ORIENTED_EDGE('',*,*,#6311,.T.);
#9143=ORIENTED_EDGE('',*,*,#6312,.T.);
#9144=ORIENTED_EDGE('',*,*,#6313,.T.);
#9145=ORIENTED_EDGE('',*,*,#6314,.F.);
#9146=ORIENTED_EDGE('',*,*,#6313,.F.);
#9147=ORIENTED_EDGE('',*,*,#6297,.T.);
#9148=ORIENTED_EDGE('',*,*,#6310,.F.);
#9149=ORIENTED_EDGE('',*,*,#6315,.T.);
#9150=ORIENTED_EDGE('',*,*,#6316,.T.);
#9151=ORIENTED_EDGE('',*,*,#6317,.F.);
#9152=ORIENTED_EDGE('',*,*,#6311,.F.);
#9153=ORIENTED_EDGE('',*,*,#6294,.T.);
#9154=ORIENTED_EDGE('',*,*,#6312,.F.);
#9155=ORIENTED_EDGE('',*,*,#6317,.T.);
#9156=ORIENTED_EDGE('',*,*,#6318,.T.);
#9157=ORIENTED_EDGE('',*,*,#6319,.F.);
#9158=ORIENTED_EDGE('',*,*,#6301,.F.);
#9159=ORIENTED_EDGE('',*,*,#6292,.T.);
#9160=ORIENTED_EDGE('',*,*,#6302,.F.);
#9161=ORIENTED_EDGE('',*,*,#6319,.T.);
#9162=ORIENTED_EDGE('',*,*,#6320,.T.);
#9163=ORIENTED_EDGE('',*,*,#6321,.F.);
#9164=ORIENTED_EDGE('',*,*,#6303,.F.);
#9165=ORIENTED_EDGE('',*,*,#6290,.T.);
#9166=ORIENTED_EDGE('',*,*,#6304,.F.);
#9167=ORIENTED_EDGE('',*,*,#6321,.T.);
#9168=ORIENTED_EDGE('',*,*,#6322,.T.);
#9169=ORIENTED_EDGE('',*,*,#6323,.F.);
#9170=ORIENTED_EDGE('',*,*,#6305,.F.);
#9171=ORIENTED_EDGE('',*,*,#6288,.T.);
#9172=ORIENTED_EDGE('',*,*,#6308,.F.);
#9173=ORIENTED_EDGE('',*,*,#6324,.T.);
#9174=ORIENTED_EDGE('',*,*,#6325,.T.);
#9175=ORIENTED_EDGE('',*,*,#6315,.F.);
#9176=ORIENTED_EDGE('',*,*,#6309,.F.);
#9177=ORIENTED_EDGE('',*,*,#6286,.T.);
#9178=ORIENTED_EDGE('',*,*,#6306,.F.);
#9179=ORIENTED_EDGE('',*,*,#6323,.T.);
#9180=ORIENTED_EDGE('',*,*,#6326,.T.);
#9181=ORIENTED_EDGE('',*,*,#6324,.F.);
#9182=ORIENTED_EDGE('',*,*,#6307,.F.);
#9183=ORIENTED_EDGE('',*,*,#6326,.F.);
#9184=ORIENTED_EDGE('',*,*,#6322,.F.);
#9185=ORIENTED_EDGE('',*,*,#6320,.F.);
#9186=ORIENTED_EDGE('',*,*,#6318,.F.);
#9187=ORIENTED_EDGE('',*,*,#6316,.F.);
#9188=ORIENTED_EDGE('',*,*,#6325,.F.);
#9189=ORIENTED_EDGE('',*,*,#6314,.T.);
#9190=ORIENTED_EDGE('',*,*,#6327,.F.);
#9191=ORIENTED_EDGE('',*,*,#6285,.F.);
#9192=ORIENTED_EDGE('',*,*,#6282,.F.);
#9193=ORIENTED_EDGE('',*,*,#6328,.T.);
#9194=ORIENTED_EDGE('',*,*,#6327,.T.);
#9195=ORIENTED_EDGE('',*,*,#6328,.F.);
#9196=ORIENTED_EDGE('',*,*,#6281,.F.);
#9197=ORIENTED_EDGE('',*,*,#6243,.F.);
#9198=ORIENTED_EDGE('',*,*,#6329,.F.);
#9199=ORIENTED_EDGE('',*,*,#6259,.T.);
#9200=ORIENTED_EDGE('',*,*,#6279,.T.);
#9201=ORIENTED_EDGE('',*,*,#6276,.T.);
#9202=ORIENTED_EDGE('',*,*,#6284,.T.);
#9203=ORIENTED_EDGE('',*,*,#6300,.F.);
#9204=ORIENTED_EDGE('',*,*,#6330,.T.);
#9205=ORIENTED_EDGE('',*,*,#6329,.T.);
#9206=ORIENTED_EDGE('',*,*,#6330,.F.);
#9207=ORIENTED_EDGE('',*,*,#6331,.F.);
#9208=ORIENTED_EDGE('',*,*,#6332,.F.);
#9209=ORIENTED_EDGE('',*,*,#6333,.F.);
#9210=ORIENTED_EDGE('',*,*,#6334,.F.);
#9211=ORIENTED_EDGE('',*,*,#6335,.F.);
#9212=ORIENTED_EDGE('',*,*,#6336,.F.);
#9213=ORIENTED_EDGE('',*,*,#6337,.F.);
#9214=ORIENTED_EDGE('',*,*,#6338,.F.);
#9215=ORIENTED_EDGE('',*,*,#6339,.F.);
#9216=ORIENTED_EDGE('',*,*,#6340,.F.);
#9217=ORIENTED_EDGE('',*,*,#6341,.F.);
#9218=ORIENTED_EDGE('',*,*,#6342,.F.);
#9219=ORIENTED_EDGE('',*,*,#6343,.F.);
#9220=ORIENTED_EDGE('',*,*,#6344,.F.);
#9221=ORIENTED_EDGE('',*,*,#6345,.F.);
#9222=ORIENTED_EDGE('',*,*,#6346,.F.);
#9223=ORIENTED_EDGE('',*,*,#6337,.T.);
#9224=ORIENTED_EDGE('',*,*,#6347,.F.);
#9225=ORIENTED_EDGE('',*,*,#6348,.F.);
#9226=ORIENTED_EDGE('',*,*,#6349,.T.);
#9227=ORIENTED_EDGE('',*,*,#6335,.T.);
#9228=ORIENTED_EDGE('',*,*,#6350,.T.);
#9229=ORIENTED_EDGE('',*,*,#6351,.T.);
#9230=ORIENTED_EDGE('',*,*,#6352,.F.);
#9231=ORIENTED_EDGE('',*,*,#6345,.T.);
#9232=ORIENTED_EDGE('',*,*,#6353,.F.);
#9233=ORIENTED_EDGE('',*,*,#6354,.F.);
#9234=ORIENTED_EDGE('',*,*,#6355,.T.);
#9235=ORIENTED_EDGE('',*,*,#6343,.T.);
#9236=ORIENTED_EDGE('',*,*,#6356,.T.);
#9237=ORIENTED_EDGE('',*,*,#6357,.T.);
#9238=ORIENTED_EDGE('',*,*,#6358,.F.);
#9239=ORIENTED_EDGE('',*,*,#6339,.T.);
#9240=ORIENTED_EDGE('',*,*,#6359,.T.);
#9241=ORIENTED_EDGE('',*,*,#6354,.T.);
#9242=ORIENTED_EDGE('',*,*,#6360,.F.);
#9243=ORIENTED_EDGE('',*,*,#6338,.T.);
#9244=ORIENTED_EDGE('',*,*,#6349,.F.);
#9245=ORIENTED_EDGE('',*,*,#6361,.F.);
#9246=ORIENTED_EDGE('',*,*,#6362,.F.);
#9247=ORIENTED_EDGE('',*,*,#6363,.F.);
#9248=ORIENTED_EDGE('',*,*,#6356,.F.);
#9249=ORIENTED_EDGE('',*,*,#6346,.T.);
#9250=ORIENTED_EDGE('',*,*,#6355,.F.);
#9251=ORIENTED_EDGE('',*,*,#6359,.F.);
#9252=ORIENTED_EDGE('',*,*,#6342,.T.);
#9253=ORIENTED_EDGE('',*,*,#6364,.F.);
#9254=ORIENTED_EDGE('',*,*,#6332,.T.);
#9255=ORIENTED_EDGE('',*,*,#6365,.F.);
#9256=ORIENTED_EDGE('',*,*,#6350,.F.);
#9257=ORIENTED_EDGE('',*,*,#6331,.T.);
#9258=ORIENTED_EDGE('',*,*,#6366,.F.);
#9259=ORIENTED_EDGE('',*,*,#6351,.F.);
#9260=ORIENTED_EDGE('',*,*,#6365,.T.);
#9261=ORIENTED_EDGE('',*,*,#6361,.T.);
#9262=ORIENTED_EDGE('',*,*,#6348,.T.);
#9263=ORIENTED_EDGE('',*,*,#6367,.F.);
#9264=ORIENTED_EDGE('',*,*,#6368,.F.);
#9265=ORIENTED_EDGE('',*,*,#6362,.T.);
#9266=ORIENTED_EDGE('',*,*,#6368,.T.);
#9267=ORIENTED_EDGE('',*,*,#6369,.F.);
#9268=ORIENTED_EDGE('',*,*,#6370,.F.);
#9269=ORIENTED_EDGE('',*,*,#6363,.T.);
#9270=ORIENTED_EDGE('',*,*,#6370,.T.);
#9271=ORIENTED_EDGE('',*,*,#6371,.F.);
#9272=ORIENTED_EDGE('',*,*,#6357,.F.);
#9273=ORIENTED_EDGE('',*,*,#6333,.T.);
#9274=ORIENTED_EDGE('',*,*,#6364,.T.);
#9275=ORIENTED_EDGE('',*,*,#6341,.T.);
#9276=ORIENTED_EDGE('',*,*,#6372,.F.);
#9277=ORIENTED_EDGE('',*,*,#6336,.T.);
#9278=ORIENTED_EDGE('',*,*,#6352,.T.);
#9279=ORIENTED_EDGE('',*,*,#6366,.T.);
#9280=ORIENTED_EDGE('',*,*,#6334,.T.);
#9281=ORIENTED_EDGE('',*,*,#6372,.T.);
#9282=ORIENTED_EDGE('',*,*,#6340,.T.);
#9283=ORIENTED_EDGE('',*,*,#6360,.T.);
#9284=ORIENTED_EDGE('',*,*,#6353,.T.);
#9285=ORIENTED_EDGE('',*,*,#6344,.T.);
#9286=ORIENTED_EDGE('',*,*,#6358,.T.);
#9287=ORIENTED_EDGE('',*,*,#6371,.T.);
#9288=ORIENTED_EDGE('',*,*,#6369,.T.);
#9289=ORIENTED_EDGE('',*,*,#6367,.T.);
#9290=ORIENTED_EDGE('',*,*,#6347,.T.);
#9291=ORIENTED_EDGE('',*,*,#6373,.F.);
#9292=ORIENTED_EDGE('',*,*,#6374,.F.);
#9293=ORIENTED_EDGE('',*,*,#6375,.F.);
#9294=ORIENTED_EDGE('',*,*,#6376,.F.);
#9295=ORIENTED_EDGE('',*,*,#6377,.F.);
#9296=ORIENTED_EDGE('',*,*,#6378,.F.);
#9297=ORIENTED_EDGE('',*,*,#6379,.F.);
#9298=ORIENTED_EDGE('',*,*,#6380,.F.);
#9299=ORIENTED_EDGE('',*,*,#6381,.F.);
#9300=ORIENTED_EDGE('',*,*,#6382,.F.);
#9301=ORIENTED_EDGE('',*,*,#6383,.F.);
#9302=ORIENTED_EDGE('',*,*,#6384,.F.);
#9303=ORIENTED_EDGE('',*,*,#6385,.F.);
#9304=ORIENTED_EDGE('',*,*,#6386,.F.);
#9305=ORIENTED_EDGE('',*,*,#6387,.F.);
#9306=ORIENTED_EDGE('',*,*,#6388,.F.);
#9307=ORIENTED_EDGE('',*,*,#6379,.T.);
#9308=ORIENTED_EDGE('',*,*,#6389,.F.);
#9309=ORIENTED_EDGE('',*,*,#6390,.F.);
#9310=ORIENTED_EDGE('',*,*,#6391,.T.);
#9311=ORIENTED_EDGE('',*,*,#6377,.T.);
#9312=ORIENTED_EDGE('',*,*,#6392,.T.);
#9313=ORIENTED_EDGE('',*,*,#6393,.T.);
#9314=ORIENTED_EDGE('',*,*,#6394,.F.);
#9315=ORIENTED_EDGE('',*,*,#6387,.T.);
#9316=ORIENTED_EDGE('',*,*,#6395,.F.);
#9317=ORIENTED_EDGE('',*,*,#6396,.F.);
#9318=ORIENTED_EDGE('',*,*,#6397,.T.);
#9319=ORIENTED_EDGE('',*,*,#6385,.T.);
#9320=ORIENTED_EDGE('',*,*,#6398,.T.);
#9321=ORIENTED_EDGE('',*,*,#6399,.T.);
#9322=ORIENTED_EDGE('',*,*,#6400,.F.);
#9323=ORIENTED_EDGE('',*,*,#6381,.T.);
#9324=ORIENTED_EDGE('',*,*,#6401,.T.);
#9325=ORIENTED_EDGE('',*,*,#6396,.T.);
#9326=ORIENTED_EDGE('',*,*,#6402,.F.);
#9327=ORIENTED_EDGE('',*,*,#6380,.T.);
#9328=ORIENTED_EDGE('',*,*,#6391,.F.);
#9329=ORIENTED_EDGE('',*,*,#6403,.F.);
#9330=ORIENTED_EDGE('',*,*,#6404,.F.);
#9331=ORIENTED_EDGE('',*,*,#6405,.F.);
#9332=ORIENTED_EDGE('',*,*,#6398,.F.);
#9333=ORIENTED_EDGE('',*,*,#6388,.T.);
#9334=ORIENTED_EDGE('',*,*,#6397,.F.);
#9335=ORIENTED_EDGE('',*,*,#6401,.F.);
#9336=ORIENTED_EDGE('',*,*,#6384,.T.);
#9337=ORIENTED_EDGE('',*,*,#6406,.F.);
#9338=ORIENTED_EDGE('',*,*,#6374,.T.);
#9339=ORIENTED_EDGE('',*,*,#6407,.F.);
#9340=ORIENTED_EDGE('',*,*,#6392,.F.);
#9341=ORIENTED_EDGE('',*,*,#6373,.T.);
#9342=ORIENTED_EDGE('',*,*,#6408,.F.);
#9343=ORIENTED_EDGE('',*,*,#6393,.F.);
#9344=ORIENTED_EDGE('',*,*,#6407,.T.);
#9345=ORIENTED_EDGE('',*,*,#6403,.T.);
#9346=ORIENTED_EDGE('',*,*,#6390,.T.);
#9347=ORIENTED_EDGE('',*,*,#6409,.F.);
#9348=ORIENTED_EDGE('',*,*,#6410,.F.);
#9349=ORIENTED_EDGE('',*,*,#6404,.T.);
#9350=ORIENTED_EDGE('',*,*,#6410,.T.);
#9351=ORIENTED_EDGE('',*,*,#6411,.F.);
#9352=ORIENTED_EDGE('',*,*,#6412,.F.);
#9353=ORIENTED_EDGE('',*,*,#6405,.T.);
#9354=ORIENTED_EDGE('',*,*,#6412,.T.);
#9355=ORIENTED_EDGE('',*,*,#6413,.F.);
#9356=ORIENTED_EDGE('',*,*,#6399,.F.);
#9357=ORIENTED_EDGE('',*,*,#6375,.T.);
#9358=ORIENTED_EDGE('',*,*,#6406,.T.);
#9359=ORIENTED_EDGE('',*,*,#6383,.T.);
#9360=ORIENTED_EDGE('',*,*,#6414,.F.);
#9361=ORIENTED_EDGE('',*,*,#6378,.T.);
#9362=ORIENTED_EDGE('',*,*,#6394,.T.);
#9363=ORIENTED_EDGE('',*,*,#6408,.T.);
#9364=ORIENTED_EDGE('',*,*,#6376,.T.);
#9365=ORIENTED_EDGE('',*,*,#6414,.T.);
#9366=ORIENTED_EDGE('',*,*,#6382,.T.);
#9367=ORIENTED_EDGE('',*,*,#6402,.T.);
#9368=ORIENTED_EDGE('',*,*,#6395,.T.);
#9369=ORIENTED_EDGE('',*,*,#6386,.T.);
#9370=ORIENTED_EDGE('',*,*,#6400,.T.);
#9371=ORIENTED_EDGE('',*,*,#6413,.T.);
#9372=ORIENTED_EDGE('',*,*,#6411,.T.);
#9373=ORIENTED_EDGE('',*,*,#6409,.T.);
#9374=ORIENTED_EDGE('',*,*,#6389,.T.);
#9375=TOROIDAL_SURFACE('',#10100,1.45,0.1);
#9376=TOROIDAL_SURFACE('',#10110,1.45,0.1);
#9377=TOROIDAL_SURFACE('',#10114,1.45,0.1);
#9378=TOROIDAL_SURFACE('',#10123,1.45,0.1);
#9379=TOROIDAL_SURFACE('',#10778,0.2,0.1);
#9380=ADVANCED_FACE('',(#2402),#9375,.T.);
#9381=ADVANCED_FACE('',(#2403),#2271,.F.);
#9382=ADVANCED_FACE('',(#2404,#386),#995,.F.);
#9383=ADVANCED_FACE('',(#2405),#9376,.T.);
#9384=ADVANCED_FACE('',(#2406,#387),#996,.T.);
#9385=ADVANCED_FACE('',(#2407),#9377,.T.);
#9386=ADVANCED_FACE('',(#2408),#2272,.F.);
#9387=ADVANCED_FACE('',(#2409,#388),#997,.F.);
#9388=ADVANCED_FACE('',(#2410),#9378,.T.);
#9389=ADVANCED_FACE('',(#2411,#389),#998,.T.);
#9390=ADVANCED_FACE('',(#2412),#280,.F.);
#9391=ADVANCED_FACE('',(#2413),#2273,.T.);
#9392=ADVANCED_FACE('',(#2414),#270,.T.);
#9393=ADVANCED_FACE('',(#2415),#281,.T.);
#9394=ADVANCED_FACE('',(#2416),#282,.F.);
#9395=ADVANCED_FACE('',(#2417),#283,.F.);
#9396=ADVANCED_FACE('',(#2418),#284,.F.);
#9397=ADVANCED_FACE('',(#2419),#271,.T.);
#9398=ADVANCED_FACE('',(#2420),#285,.F.);
#9399=ADVANCED_FACE('',(#2421),#286,.T.);
#9400=ADVANCED_FACE('',(#2422),#287,.F.);
#9401=ADVANCED_FACE('',(#2423),#288,.F.);
#9402=ADVANCED_FACE('',(#2424),#289,.F.);
#9403=ADVANCED_FACE('',(#2425),#290,.F.);
#9404=ADVANCED_FACE('',(#2426),#291,.T.);
#9405=ADVANCED_FACE('',(#2427),#2274,.T.);
#9406=ADVANCED_FACE('',(#2428),#292,.T.);
#9407=ADVANCED_FACE('',(#2429),#293,.T.);
#9408=ADVANCED_FACE('',(#2430),#294,.T.);
#9409=ADVANCED_FACE('',(#2431),#295,.T.);
#9410=ADVANCED_FACE('',(#2432),#296,.F.);
#9411=ADVANCED_FACE('',(#2433),#297,.F.);
#9412=ADVANCED_FACE('',(#2434),#298,.F.);
#9413=ADVANCED_FACE('',(#2435),#299,.T.);
#9414=ADVANCED_FACE('',(#2436),#300,.T.);
#9415=ADVANCED_FACE('',(#2437),#301,.T.);
#9416=ADVANCED_FACE('',(#2438),#302,.T.);
#9417=ADVANCED_FACE('',(#2439),#303,.T.);
#9418=ADVANCED_FACE('',(#2440),#304,.T.);
#9419=ADVANCED_FACE('',(#2441),#305,.T.);
#9420=ADVANCED_FACE('',(#2442),#306,.F.);
#9421=ADVANCED_FACE('',(#2443),#307,.T.);
#9422=ADVANCED_FACE('',(#2444),#308,.F.);
#9423=ADVANCED_FACE('',(#2445),#309,.F.);
#9424=ADVANCED_FACE('',(#2446),#310,.F.);
#9425=ADVANCED_FACE('',(#2447),#311,.F.);
#9426=ADVANCED_FACE('',(#2448),#312,.F.);
#9427=ADVANCED_FACE('',(#2449),#313,.F.);
#9428=ADVANCED_FACE('',(#2450),#272,.T.);
#9429=ADVANCED_FACE('',(#2451),#999,.F.);
#9430=ADVANCED_FACE('',(#2452),#314,.T.);
#9431=ADVANCED_FACE('',(#2453),#315,.F.);
#9432=ADVANCED_FACE('',(#2454),#316,.T.);
#9433=ADVANCED_FACE('',(#2455),#317,.T.);
#9434=ADVANCED_FACE('',(#2456),#2275,.T.);
#9435=ADVANCED_FACE('',(#2457),#318,.T.);
#9436=ADVANCED_FACE('',(#2458),#2276,.F.);
#9437=ADVANCED_FACE('',(#2459),#319,.T.);
#9438=ADVANCED_FACE('',(#2460),#320,.F.);
#9439=ADVANCED_FACE('',(#2461),#321,.F.);
#9440=ADVANCED_FACE('',(#2462),#322,.F.);
#9441=ADVANCED_FACE('',(#2463),#323,.F.);
#9442=ADVANCED_FACE('',(#2464),#324,.F.);
#9443=ADVANCED_FACE('',(#2465),#325,.T.);
#9444=ADVANCED_FACE('',(#2466),#326,.T.);
#9445=ADVANCED_FACE('',(#2467),#327,.T.);
#9446=ADVANCED_FACE('',(#2468),#328,.T.);
#9447=ADVANCED_FACE('',(#2469),#329,.T.);
#9448=ADVANCED_FACE('',(#2470),#330,.T.);
#9449=ADVANCED_FACE('',(#2471),#331,.T.);
#9450=ADVANCED_FACE('',(#2472),#332,.T.);
#9451=ADVANCED_FACE('',(#2473),#333,.T.);
#9452=ADVANCED_FACE('',(#2474),#334,.T.);
#9453=ADVANCED_FACE('',(#2475),#335,.F.);
#9454=ADVANCED_FACE('',(#2476),#273,.T.);
#9455=ADVANCED_FACE('',(#2477),#2277,.T.);
#9456=ADVANCED_FACE('',(#2478),#336,.T.);
#9457=ADVANCED_FACE('',(#2479),#337,.T.);
#9458=ADVANCED_FACE('',(#2480),#338,.F.);
#9459=ADVANCED_FACE('',(#2481),#1000,.T.);
#9460=ADVANCED_FACE('',(#2482),#2278,.T.);
#9461=ADVANCED_FACE('',(#2483),#339,.F.);
#9462=ADVANCED_FACE('',(#2484),#340,.F.);
#9463=ADVANCED_FACE('',(#2485),#341,.F.);
#9464=ADVANCED_FACE('',(#2486),#342,.F.);
#9465=ADVANCED_FACE('',(#2487),#343,.F.);
#9466=ADVANCED_FACE('',(#2488),#344,.T.);
#9467=ADVANCED_FACE('',(#2489),#345,.T.);
#9468=ADVANCED_FACE('',(#2490),#346,.F.);
#9469=ADVANCED_FACE('',(#2491),#1001,.F.);
#9470=ADVANCED_FACE('',(#2492),#2279,.T.);
#9471=ADVANCED_FACE('',(#2493),#347,.F.);
#9472=ADVANCED_FACE('',(#2494),#348,.F.);
#9473=ADVANCED_FACE('',(#2495),#349,.F.);
#9474=ADVANCED_FACE('',(#2496),#350,.F.);
#9475=ADVANCED_FACE('',(#2497),#351,.F.);
#9476=ADVANCED_FACE('',(#2498),#2280,.T.);
#9477=ADVANCED_FACE('',(#2499,#390,#391,#392,#393),#1002,.F.);
#9478=ADVANCED_FACE('',(#2500),#2281,.T.);
#9479=ADVANCED_FACE('',(#2501),#2282,.T.);
#9480=ADVANCED_FACE('',(#2502),#2283,.T.);
#9481=ADVANCED_FACE('',(#2503),#274,.T.);
#9482=ADVANCED_FACE('',(#2504),#275,.T.);
#9483=ADVANCED_FACE('',(#2505),#2284,.T.);
#9484=ADVANCED_FACE('',(#2506),#1003,.T.);
#9485=ADVANCED_FACE('',(#2507),#2285,.T.);
#9486=ADVANCED_FACE('',(#2508,#394,#395,#396,#397),#1004,.T.);
#9487=ADVANCED_FACE('',(#2509),#352,.F.);
#9488=ADVANCED_FACE('',(#2510),#353,.F.);
#9489=ADVANCED_FACE('',(#2511),#354,.F.);
#9490=ADVANCED_FACE('',(#2512),#355,.F.);
#9491=ADVANCED_FACE('',(#2513),#356,.F.);
#9492=ADVANCED_FACE('',(#2514),#276,.T.);
#9493=ADVANCED_FACE('',(#2515),#357,.T.);
#9494=ADVANCED_FACE('',(#2516),#2286,.F.);
#9495=ADVANCED_FACE('',(#2517),#1005,.T.);
#9496=ADVANCED_FACE('',(#2518),#358,.F.);
#9497=ADVANCED_FACE('',(#2519),#359,.T.);
#9498=ADVANCED_FACE('',(#2520),#360,.F.);
#9499=ADVANCED_FACE('',(#2521),#361,.F.);
#9500=ADVANCED_FACE('',(#2522),#2287,.F.);
#9501=ADVANCED_FACE('',(#2523),#2288,.F.);
#9502=ADVANCED_FACE('',(#2524),#362,.F.);
#9503=ADVANCED_FACE('',(#2525),#363,.T.);
#9504=ADVANCED_FACE('',(#2526),#1006,.T.);
#9505=ADVANCED_FACE('',(#2527),#1007,.T.);
#9506=ADVANCED_FACE('',(#2528),#1008,.T.);
#9507=ADVANCED_FACE('',(#2529),#364,.T.);
#9508=ADVANCED_FACE('',(#2530),#365,.T.);
#9509=ADVANCED_FACE('',(#2531),#366,.F.);
#9510=ADVANCED_FACE('',(#2532),#367,.F.);
#9511=ADVANCED_FACE('',(#2533),#368,.F.);
#9512=ADVANCED_FACE('',(#2534),#369,.F.);
#9513=ADVANCED_FACE('',(#2535),#277,.T.);
#9514=ADVANCED_FACE('',(#2536),#370,.F.);
#9515=ADVANCED_FACE('',(#2537),#371,.F.);
#9516=ADVANCED_FACE('',(#2538),#372,.T.);
#9517=ADVANCED_FACE('',(#2539),#373,.T.);
#9518=ADVANCED_FACE('',(#2540),#374,.T.);
#9519=ADVANCED_FACE('',(#2541),#375,.F.);
#9520=ADVANCED_FACE('',(#2542),#376,.F.);
#9521=ADVANCED_FACE('',(#2543),#377,.F.);
#9522=ADVANCED_FACE('',(#2544),#278,.T.);
#9523=ADVANCED_FACE('',(#2545),#378,.T.);
#9524=ADVANCED_FACE('',(#2546),#379,.T.);
#9525=ADVANCED_FACE('',(#2547),#2289,.F.);
#9526=ADVANCED_FACE('',(#2548),#1009,.T.);
#9527=ADVANCED_FACE('',(#2549),#2290,.F.);
#9528=ADVANCED_FACE('',(#2550),#380,.T.);
#9529=ADVANCED_FACE('',(#2551),#2291,.F.);
#9530=ADVANCED_FACE('',(#2552),#2292,.F.);
#9531=ADVANCED_FACE('',(#2553),#2293,.F.);
#9532=ADVANCED_FACE('',(#2554),#2294,.F.);
#9533=ADVANCED_FACE('',(#2555),#1010,.T.);
#9534=ADVANCED_FACE('',(#2556),#1011,.T.);
#9535=ADVANCED_FACE('',(#2557),#1012,.T.);
#9536=ADVANCED_FACE('',(#2558),#1013,.T.);
#9537=ADVANCED_FACE('',(#2559),#1014,.T.);
#9538=ADVANCED_FACE('',(#2560),#1015,.T.);
#9539=ADVANCED_FACE('',(#2561),#1016,.T.);
#9540=ADVANCED_FACE('',(#2562),#1017,.T.);
#9541=ADVANCED_FACE('',(#2563),#1018,.T.);
#9542=ADVANCED_FACE('',(#2564),#1019,.T.);
#9543=ADVANCED_FACE('',(#2565),#1020,.T.);
#9544=ADVANCED_FACE('',(#2566),#1021,.T.);
#9545=ADVANCED_FACE('',(#2567),#1022,.T.);
#9546=ADVANCED_FACE('',(#2568),#1023,.T.);
#9547=ADVANCED_FACE('',(#2569),#1024,.T.);
#9548=ADVANCED_FACE('',(#2570,#398,#399,#400,#401,#402,#403,#404),#1025,
 .T.);
#9549=ADVANCED_FACE('',(#2571),#153,.F.);
#9550=ADVANCED_FACE('',(#2572),#2295,.F.);
#9551=ADVANCED_FACE('',(#2573),#154,.F.);
#9552=ADVANCED_FACE('',(#2574),#155,.F.);
#9553=ADVANCED_FACE('',(#2575),#2296,.F.);
#9554=ADVANCED_FACE('',(#2576),#156,.F.);
#9555=ADVANCED_FACE('',(#2577),#157,.F.);
#9556=ADVANCED_FACE('',(#2578),#2297,.F.);
#9557=ADVANCED_FACE('',(#2579),#158,.F.);
#9558=ADVANCED_FACE('',(#2580),#159,.F.);
#9559=ADVANCED_FACE('',(#2581),#2298,.F.);
#9560=ADVANCED_FACE('',(#2582),#160,.F.);
#9561=ADVANCED_FACE('',(#2583),#161,.F.);
#9562=ADVANCED_FACE('',(#2584),#2299,.F.);
#9563=ADVANCED_FACE('',(#2585),#162,.F.);
#9564=ADVANCED_FACE('',(#2586),#2300,.F.);
#9565=ADVANCED_FACE('',(#2587),#2301,.F.);
#9566=ADVANCED_FACE('',(#2588),#2302,.F.);
#9567=ADVANCED_FACE('',(#2589),#2303,.F.);
#9568=ADVANCED_FACE('',(#2590),#1026,.F.);
#9569=ADVANCED_FACE('',(#2591),#1027,.F.);
#9570=ADVANCED_FACE('',(#2592),#1028,.F.);
#9571=ADVANCED_FACE('',(#2593,#405),#1029,.F.);
#9572=ADVANCED_FACE('',(#2594),#1030,.F.);
#9573=ADVANCED_FACE('',(#2595),#1031,.F.);
#9574=ADVANCED_FACE('',(#2596),#1032,.F.);
#9575=ADVANCED_FACE('',(#2597),#1033,.F.);
#9576=ADVANCED_FACE('',(#2598),#1034,.F.);
#9577=ADVANCED_FACE('',(#2599),#1035,.F.);
#9578=ADVANCED_FACE('',(#2600),#1036,.F.);
#9579=ADVANCED_FACE('',(#2601),#1037,.F.);
#9580=ADVANCED_FACE('',(#2602),#1038,.F.);
#9581=ADVANCED_FACE('',(#2603),#1039,.T.);
#9582=ADVANCED_FACE('',(#2604,#406),#1040,.T.);
#9583=ADVANCED_FACE('',(#2605),#1041,.T.);
#9584=ADVANCED_FACE('',(#2606),#1042,.T.);
#9585=ADVANCED_FACE('',(#2607,#407,#408,#409,#410),#1043,.F.);
#9586=ADVANCED_FACE('',(#2608),#2304,.F.);
#9587=ADVANCED_FACE('',(#2609),#1044,.F.);
#9588=ADVANCED_FACE('',(#2610),#2305,.F.);
#9589=ADVANCED_FACE('',(#2611),#1045,.F.);
#9590=ADVANCED_FACE('',(#2612),#2306,.F.);
#9591=ADVANCED_FACE('',(#2613),#1046,.F.);
#9592=ADVANCED_FACE('',(#2614),#2307,.F.);
#9593=ADVANCED_FACE('',(#2615),#1047,.F.);
#9594=ADVANCED_FACE('',(#2616),#2308,.F.);
#9595=ADVANCED_FACE('',(#2617),#1048,.F.);
#9596=ADVANCED_FACE('',(#2618),#2309,.F.);
#9597=ADVANCED_FACE('',(#2619),#1049,.F.);
#9598=ADVANCED_FACE('',(#2620),#2310,.F.);
#9599=ADVANCED_FACE('',(#2621),#1050,.F.);
#9600=ADVANCED_FACE('',(#2622),#2311,.F.);
#9601=ADVANCED_FACE('',(#2623),#1051,.F.);
#9602=ADVANCED_FACE('',(#2624),#2312,.F.);
#9603=ADVANCED_FACE('',(#2625),#1052,.F.);
#9604=ADVANCED_FACE('',(#2626),#2313,.F.);
#9605=ADVANCED_FACE('',(#2627),#1053,.F.);
#9606=ADVANCED_FACE('',(#2628),#2314,.F.);
#9607=ADVANCED_FACE('',(#2629),#1054,.F.);
#9608=ADVANCED_FACE('',(#2630),#2315,.F.);
#9609=ADVANCED_FACE('',(#2631),#1055,.F.);
#9610=ADVANCED_FACE('',(#2632),#2316,.F.);
#9611=ADVANCED_FACE('',(#2633),#2317,.F.);
#9612=ADVANCED_FACE('',(#2634),#2318,.F.);
#9613=ADVANCED_FACE('',(#2635),#2319,.F.);
#9614=ADVANCED_FACE('',(#2636),#2320,.F.);
#9615=ADVANCED_FACE('',(#2637),#2321,.F.);
#9616=ADVANCED_FACE('',(#2638),#1056,.T.);
#9617=ADVANCED_FACE('',(#2639),#1057,.T.);
#9618=ADVANCED_FACE('',(#2640),#1058,.T.);
#9619=ADVANCED_FACE('',(#2641),#1059,.T.);
#9620=ADVANCED_FACE('',(#2642),#1060,.T.);
#9621=ADVANCED_FACE('',(#2643),#1061,.T.);
#9622=ADVANCED_FACE('',(#2644),#1062,.T.);
#9623=ADVANCED_FACE('',(#2645),#1063,.T.);
#9624=ADVANCED_FACE('',(#2646,#411,#412,#413,#414,#415,#416,#417,#418,#419),
#1064,.T.);
#9625=ADVANCED_FACE('',(#2647,#420,#421,#422,#423,#424,#425,#426,#427,#428),
#1065,.F.);
#9626=ADVANCED_FACE('',(#2648),#1066,.T.);
#9627=ADVANCED_FACE('',(#2649),#1067,.T.);
#9628=ADVANCED_FACE('',(#2650),#1068,.T.);
#9629=ADVANCED_FACE('',(#2651),#1069,.T.);
#9630=ADVANCED_FACE('',(#2652),#1070,.T.);
#9631=ADVANCED_FACE('',(#2653),#1071,.T.);
#9632=ADVANCED_FACE('',(#2654),#1072,.T.);
#9633=ADVANCED_FACE('',(#2655),#1073,.T.);
#9634=ADVANCED_FACE('',(#2656),#1074,.T.);
#9635=ADVANCED_FACE('',(#2657,#429,#430,#431,#432),#1075,.T.);
#9636=ADVANCED_FACE('',(#2658),#2322,.F.);
#9637=ADVANCED_FACE('',(#2659),#2323,.F.);
#9638=ADVANCED_FACE('',(#2660),#2324,.F.);
#9639=ADVANCED_FACE('',(#2661),#2325,.F.);
#9640=ADVANCED_FACE('',(#2662),#1076,.T.);
#9641=ADVANCED_FACE('',(#2663),#1077,.T.);
#9642=ADVANCED_FACE('',(#2664),#1078,.T.);
#9643=ADVANCED_FACE('',(#2665,#433,#434,#435,#436),#1079,.T.);
#9644=ADVANCED_FACE('',(#2666,#437,#438),#2326,.T.);
#9645=ADVANCED_FACE('',(#2667),#2327,.T.);
#9646=ADVANCED_FACE('',(#2668),#1080,.F.);
#9647=ADVANCED_FACE('',(#2669),#1081,.F.);
#9648=ADVANCED_FACE('',(#2670),#1082,.F.);
#9649=ADVANCED_FACE('',(#2671),#1083,.F.);
#9650=ADVANCED_FACE('',(#2672),#1084,.F.);
#9651=ADVANCED_FACE('',(#2673),#1085,.F.);
#9652=ADVANCED_FACE('',(#2674),#1086,.F.);
#9653=ADVANCED_FACE('',(#2675),#1087,.F.);
#9654=ADVANCED_FACE('',(#2676),#381,.F.);
#9655=ADVANCED_FACE('',(#2677),#1088,.T.);
#9656=ADVANCED_FACE('',(#2678),#382,.F.);
#9657=ADVANCED_FACE('',(#2679),#1089,.T.);
#9658=ADVANCED_FACE('',(#2680),#163,.T.);
#9659=ADVANCED_FACE('',(#2681),#164,.T.);
#9660=ADVANCED_FACE('',(#2682,#439),#1090,.T.);
#9661=ADVANCED_FACE('',(#2683),#2328,.T.);
#9662=ADVANCED_FACE('',(#2684),#1091,.T.);
#9663=ADVANCED_FACE('',(#2685),#2329,.T.);
#9664=ADVANCED_FACE('',(#2686),#1092,.T.);
#9665=ADVANCED_FACE('',(#2687),#2330,.T.);
#9666=ADVANCED_FACE('',(#2688),#1093,.T.);
#9667=ADVANCED_FACE('',(#2689),#2331,.T.);
#9668=ADVANCED_FACE('',(#2690,#440),#1094,.T.);
#9669=ADVANCED_FACE('',(#2691),#1095,.F.);
#9670=ADVANCED_FACE('',(#2692),#1096,.F.);
#9671=ADVANCED_FACE('',(#2693),#1097,.F.);
#9672=ADVANCED_FACE('',(#2694),#1098,.F.);
#9673=ADVANCED_FACE('',(#2695),#1099,.F.);
#9674=ADVANCED_FACE('',(#2696),#2332,.F.);
#9675=ADVANCED_FACE('',(#2697),#2333,.F.);
#9676=ADVANCED_FACE('',(#2698),#2334,.F.);
#9677=ADVANCED_FACE('',(#2699),#2335,.F.);
#9678=ADVANCED_FACE('',(#2700,#441,#442),#2336,.F.);
#9679=ADVANCED_FACE('',(#2701),#1100,.F.);
#9680=ADVANCED_FACE('',(#2702),#1101,.F.);
#9681=ADVANCED_FACE('',(#2703),#1102,.F.);
#9682=ADVANCED_FACE('',(#2704),#1103,.F.);
#9683=ADVANCED_FACE('',(#2705),#2337,.T.);
#9684=ADVANCED_FACE('',(#2706,#443),#1104,.T.);
#9685=ADVANCED_FACE('',(#2707),#1105,.T.);
#9686=ADVANCED_FACE('',(#2708),#1106,.T.);
#9687=ADVANCED_FACE('',(#2709,#444,#445),#1107,.T.);
#9688=ADVANCED_FACE('',(#2710,#446,#447),#1108,.T.);
#9689=ADVANCED_FACE('',(#2711,#448),#1109,.F.);
#9690=ADVANCED_FACE('',(#2712),#383,.T.);
#9691=ADVANCED_FACE('',(#2713),#1110,.T.);
#9692=ADVANCED_FACE('',(#2714),#1111,.F.);
#9693=ADVANCED_FACE('',(#2715),#2338,.F.);
#9694=ADVANCED_FACE('',(#2716),#165,.F.);
#9695=ADVANCED_FACE('',(#2717,#449),#1112,.T.);
#9696=ADVANCED_FACE('',(#2718),#2339,.T.);
#9697=ADVANCED_FACE('',(#2719,#450),#1113,.T.);
#9698=ADVANCED_FACE('',(#2720),#2340,.F.);
#9699=ADVANCED_FACE('',(#2721,#451),#1114,.T.);
#9700=ADVANCED_FACE('',(#2722),#166,.T.);
#9701=ADVANCED_FACE('',(#2723),#2341,.T.);
#9702=ADVANCED_FACE('',(#2724),#167,.T.);
#9703=ADVANCED_FACE('',(#2725,#452),#1115,.T.);
#9704=ADVANCED_FACE('',(#2726),#2342,.F.);
#9705=ADVANCED_FACE('',(#2727,#453),#1116,.T.);
#9706=ADVANCED_FACE('',(#2728),#2343,.T.);
#9707=ADVANCED_FACE('',(#2729,#454),#1117,.T.);
#9708=ADVANCED_FACE('',(#2730),#168,.F.);
#9709=ADVANCED_FACE('',(#2731),#1118,.F.);
#9710=ADVANCED_FACE('',(#2732),#1119,.F.);
#9711=ADVANCED_FACE('',(#2733),#1120,.F.);
#9712=ADVANCED_FACE('',(#2734),#1121,.F.);
#9713=ADVANCED_FACE('',(#2735,#455),#1122,.T.);
#9714=ADVANCED_FACE('',(#2736),#169,.T.);
#9715=ADVANCED_FACE('',(#2737),#170,.T.);
#9716=ADVANCED_FACE('',(#2738),#1123,.F.);
#9717=ADVANCED_FACE('',(#2739),#1124,.F.);
#9718=ADVANCED_FACE('',(#2740),#1125,.F.);
#9719=ADVANCED_FACE('',(#2741),#1126,.F.);
#9720=ADVANCED_FACE('',(#2742),#171,.T.);
#9721=ADVANCED_FACE('',(#2743),#1127,.F.);
#9722=ADVANCED_FACE('',(#2744),#1128,.F.);
#9723=ADVANCED_FACE('',(#2745),#1129,.F.);
#9724=ADVANCED_FACE('',(#2746),#1130,.F.);
#9725=ADVANCED_FACE('',(#2747),#172,.T.);
#9726=ADVANCED_FACE('',(#2748),#1131,.F.);
#9727=ADVANCED_FACE('',(#2749),#1132,.F.);
#9728=ADVANCED_FACE('',(#2750),#1133,.F.);
#9729=ADVANCED_FACE('',(#2751),#1134,.F.);
#9730=ADVANCED_FACE('',(#2752),#173,.T.);
#9731=ADVANCED_FACE('',(#2753),#1135,.F.);
#9732=ADVANCED_FACE('',(#2754),#1136,.F.);
#9733=ADVANCED_FACE('',(#2755),#1137,.F.);
#9734=ADVANCED_FACE('',(#2756),#1138,.F.);
#9735=ADVANCED_FACE('',(#2757),#174,.T.);
#9736=ADVANCED_FACE('',(#2758),#1139,.F.);
#9737=ADVANCED_FACE('',(#2759),#1140,.F.);
#9738=ADVANCED_FACE('',(#2760),#1141,.F.);
#9739=ADVANCED_FACE('',(#2761),#1142,.F.);
#9740=ADVANCED_FACE('',(#2762),#175,.T.);
#9741=ADVANCED_FACE('',(#2763),#1143,.F.);
#9742=ADVANCED_FACE('',(#2764),#1144,.F.);
#9743=ADVANCED_FACE('',(#2765),#1145,.F.);
#9744=ADVANCED_FACE('',(#2766),#1146,.F.);
#9745=ADVANCED_FACE('',(#2767),#176,.T.);
#9746=ADVANCED_FACE('',(#2768),#1147,.F.);
#9747=ADVANCED_FACE('',(#2769),#1148,.F.);
#9748=ADVANCED_FACE('',(#2770),#1149,.F.);
#9749=ADVANCED_FACE('',(#2771),#1150,.F.);
#9750=ADVANCED_FACE('',(#2772),#2344,.F.);
#9751=ADVANCED_FACE('',(#2773,#456),#1151,.F.);
#9752=ADVANCED_FACE('',(#2774),#2345,.F.);
#9753=ADVANCED_FACE('',(#2775,#457),#1152,.T.);
#9754=ADVANCED_FACE('',(#2776),#2346,.T.);
#9755=ADVANCED_FACE('',(#2777),#2347,.F.);
#9756=ADVANCED_FACE('',(#2778,#458),#1153,.T.);
#9757=ADVANCED_FACE('',(#2779),#1154,.T.);
#9758=ADVANCED_FACE('',(#2780),#1155,.T.);
#9759=ADVANCED_FACE('',(#2781),#1156,.T.);
#9760=ADVANCED_FACE('',(#2782,#459),#1157,.T.);
#9761=ADVANCED_FACE('',(#2783),#2348,.F.);
#9762=ADVANCED_FACE('',(#2784),#2349,.T.);
#9763=ADVANCED_FACE('',(#2785,#460),#1158,.F.);
#9764=ADVANCED_FACE('',(#2786),#2350,.F.);
#9765=ADVANCED_FACE('',(#2787),#177,.F.);
#9766=ADVANCED_FACE('',(#2788,#461),#1159,.T.);
#9767=ADVANCED_FACE('',(#2789),#2351,.T.);
#9768=ADVANCED_FACE('',(#2790,#462),#1160,.T.);
#9769=ADVANCED_FACE('',(#2791),#2352,.F.);
#9770=ADVANCED_FACE('',(#2792,#463),#1161,.T.);
#9771=ADVANCED_FACE('',(#2793),#178,.T.);
#9772=ADVANCED_FACE('',(#2794),#2353,.T.);
#9773=ADVANCED_FACE('',(#2795),#179,.T.);
#9774=ADVANCED_FACE('',(#2796,#464),#1162,.T.);
#9775=ADVANCED_FACE('',(#2797),#2354,.F.);
#9776=ADVANCED_FACE('',(#2798,#465),#1163,.T.);
#9777=ADVANCED_FACE('',(#2799),#2355,.T.);
#9778=ADVANCED_FACE('',(#2800,#466),#1164,.T.);
#9779=ADVANCED_FACE('',(#2801),#180,.F.);
#9780=ADVANCED_FACE('',(#2802),#2356,.F.);
#9781=ADVANCED_FACE('',(#2803),#181,.F.);
#9782=ADVANCED_FACE('',(#2804,#467),#1165,.T.);
#9783=ADVANCED_FACE('',(#2805),#182,.T.);
#9784=ADVANCED_FACE('',(#2806),#2357,.T.);
#9785=ADVANCED_FACE('',(#2807),#183,.T.);
#9786=ADVANCED_FACE('',(#2808,#468),#1166,.T.);
#9787=ADVANCED_FACE('',(#2809),#184,.F.);
#9788=ADVANCED_FACE('',(#2810),#1167,.T.);
#9789=ADVANCED_FACE('',(#2811),#185,.T.);
#9790=ADVANCED_FACE('',(#2812),#2358,.T.);
#9791=ADVANCED_FACE('',(#2813,#469),#1168,.T.);
#9792=ADVANCED_FACE('',(#2814),#2359,.T.);
#9793=ADVANCED_FACE('',(#2815,#470),#1169,.T.);
#9794=ADVANCED_FACE('',(#2816),#2360,.T.);
#9795=ADVANCED_FACE('',(#2817),#186,.T.);
#9796=ADVANCED_FACE('',(#2818),#1170,.T.);
#9797=ADVANCED_FACE('',(#2819),#1171,.T.);
#9798=ADVANCED_FACE('',(#2820),#187,.T.);
#9799=ADVANCED_FACE('',(#2821),#2361,.T.);
#9800=ADVANCED_FACE('',(#2822,#471),#1172,.T.);
#9801=ADVANCED_FACE('',(#2823),#2362,.T.);
#9802=ADVANCED_FACE('',(#2824,#472),#1173,.T.);
#9803=ADVANCED_FACE('',(#2825),#2363,.T.);
#9804=ADVANCED_FACE('',(#2826),#188,.T.);
#9805=ADVANCED_FACE('',(#2827),#1174,.T.);
#9806=ADVANCED_FACE('',(#2828),#9379,.T.);
#9807=ADVANCED_FACE('',(#2829),#2364,.T.);
#9808=ADVANCED_FACE('',(#2830),#1175,.T.);
#9809=ADVANCED_FACE('',(#2831),#1176,.T.);
#9810=ADVANCED_FACE('',(#2832),#189,.T.);
#9811=ADVANCED_FACE('',(#2833),#2365,.T.);
#9812=ADVANCED_FACE('',(#2834),#2366,.T.);
#9813=ADVANCED_FACE('',(#2835),#2367,.T.);
#9814=ADVANCED_FACE('',(#2836),#2368,.T.);
#9815=ADVANCED_FACE('',(#2837),#2369,.T.);
#9816=ADVANCED_FACE('',(#2838),#2370,.T.);
#9817=ADVANCED_FACE('',(#2839),#2371,.T.);
#9818=ADVANCED_FACE('',(#2840),#2372,.T.);
#9819=ADVANCED_FACE('',(#2841),#2373,.T.);
#9820=ADVANCED_FACE('',(#2842),#2374,.T.);
#9821=ADVANCED_FACE('',(#2843),#2375,.T.);
#9822=ADVANCED_FACE('',(#2844),#2376,.T.);
#9823=ADVANCED_FACE('',(#2845),#2377,.T.);
#9824=ADVANCED_FACE('',(#2846),#2378,.T.);
#9825=ADVANCED_FACE('',(#2847),#2379,.T.);
#9826=ADVANCED_FACE('',(#2848),#2380,.T.);
#9827=ADVANCED_FACE('',(#2849),#384,.F.);
#9828=ADVANCED_FACE('',(#2850),#1177,.T.);
#9829=ADVANCED_FACE('',(#2851),#385,.F.);
#9830=ADVANCED_FACE('',(#2852),#190,.F.);
#9831=ADVANCED_FACE('',(#2853),#191,.F.);
#9832=ADVANCED_FACE('',(#2854),#192,.F.);
#9833=ADVANCED_FACE('',(#2855),#193,.F.);
#9834=ADVANCED_FACE('',(#2856),#194,.F.);
#9835=ADVANCED_FACE('',(#2857),#195,.F.);
#9836=ADVANCED_FACE('',(#2858),#279,.T.);
#9837=ADVANCED_FACE('',(#2859),#196,.F.);
#9838=ADVANCED_FACE('',(#2860),#1178,.F.);
#9839=ADVANCED_FACE('',(#2861),#1179,.F.);
#9840=ADVANCED_FACE('',(#2862),#1180,.F.);
#9841=ADVANCED_FACE('',(#2863),#1181,.F.);
#9842=ADVANCED_FACE('',(#2864),#1182,.F.);
#9843=ADVANCED_FACE('',(#2865),#1183,.F.);
#9844=ADVANCED_FACE('',(#2866,#473),#1184,.F.);
#9845=ADVANCED_FACE('',(#2867),#1185,.T.);
#9846=ADVANCED_FACE('',(#2868),#197,.T.);
#9847=ADVANCED_FACE('',(#2869,#474),#1186,.T.);
#9848=ADVANCED_FACE('',(#2870),#2381,.T.);
#9849=ADVANCED_FACE('',(#2871),#1187,.F.);
#9850=ADVANCED_FACE('',(#2872),#1188,.F.);
#9851=ADVANCED_FACE('',(#2873),#1189,.F.);
#9852=ADVANCED_FACE('',(#2874),#1190,.F.);
#9853=ADVANCED_FACE('',(#2875),#2382,.T.);
#9854=ADVANCED_FACE('',(#2876),#2383,.T.);
#9855=ADVANCED_FACE('',(#2877),#2384,.T.);
#9856=ADVANCED_FACE('',(#2878),#2385,.T.);
#9857=ADVANCED_FACE('',(#2879),#2386,.F.);
#9858=ADVANCED_FACE('',(#2880),#1191,.F.);
#9859=ADVANCED_FACE('',(#2881),#2387,.F.);
#9860=ADVANCED_FACE('',(#2882),#2388,.F.);
#9861=ADVANCED_FACE('',(#2883),#2389,.T.);
#9862=ADVANCED_FACE('',(#2884),#2390,.F.);
#9863=ADVANCED_FACE('',(#2885),#2391,.T.);
#9864=ADVANCED_FACE('',(#2886),#1192,.T.);
#9865=ADVANCED_FACE('',(#2887),#1193,.F.);
#9866=ADVANCED_FACE('',(#2888),#1194,.F.);
#9867=ADVANCED_FACE('',(#2889),#1195,.F.);
#9868=ADVANCED_FACE('',(#2890),#1196,.F.);
#9869=ADVANCED_FACE('',(#2891),#2392,.T.);
#9870=ADVANCED_FACE('',(#2892),#2393,.T.);
#9871=ADVANCED_FACE('',(#2893),#2394,.T.);
#9872=ADVANCED_FACE('',(#2894),#2395,.T.);
#9873=ADVANCED_FACE('',(#2895),#2396,.F.);
#9874=ADVANCED_FACE('',(#2896),#1197,.F.);
#9875=ADVANCED_FACE('',(#2897),#2397,.F.);
#9876=ADVANCED_FACE('',(#2898),#2398,.F.);
#9877=ADVANCED_FACE('',(#2899),#2399,.T.);
#9878=ADVANCED_FACE('',(#2900),#2400,.F.);
#9879=ADVANCED_FACE('',(#2901),#2401,.T.);
#9880=ADVANCED_FACE('',(#2902),#1198,.T.);
#9881=CLOSED_SHELL('',(#9380,#9381,#9382,#9383,#9384,#9385,#9386,#9387,
#9388,#9389,#9390,#9391,#9392,#9393,#9394,#9395,#9396,#9397,#9398,#9399,
#9400,#9401,#9402,#9403,#9404,#9405,#9406,#9407,#9408,#9409,#9410,#9411,
#9412,#9413,#9414,#9415,#9416,#9417,#9418,#9419,#9420,#9421,#9422,#9423,
#9424,#9425,#9426,#9427,#9428,#9429,#9430,#9431,#9432,#9433,#9434,#9435,
#9436,#9437,#9438,#9439,#9440,#9441,#9442,#9443,#9444,#9445,#9446,#9447,
#9448,#9449,#9450,#9451,#9452,#9453,#9454,#9455,#9456,#9457,#9458,#9459,
#9460,#9461,#9462,#9463,#9464,#9465,#9466,#9467,#9468,#9469,#9470,#9471,
#9472,#9473,#9474,#9475,#9476,#9477,#9478,#9479,#9480,#9481,#9482,#9483,
#9484,#9485,#9486,#9487,#9488,#9489,#9490,#9491,#9492,#9493,#9494,#9495,
#9496,#9497,#9498,#9499,#9500,#9501,#9502,#9503,#9504,#9505,#9506,#9507,
#9508,#9509,#9510,#9511,#9512,#9513,#9514,#9515,#9516,#9517,#9518,#9519,
#9520,#9521,#9522,#9523,#9524,#9525,#9526,#9527,#9528,#9529,#9530,#9531,
#9532,#9533,#9534,#9535));
#9882=CLOSED_SHELL('',(#9536,#9537,#9538,#9539,#9540,#9541,#9542,#9543,
#9544,#9545,#9546,#9547,#9548,#9549,#9550,#9551,#9552,#9553,#9554,#9555,
#9556,#9557,#9558,#9559,#9560,#9561,#9562,#9563,#9564,#9565,#9566,#9567,
#9568,#9569,#9570,#9571,#9572,#9573,#9574,#9575,#9576,#9577,#9578,#9579,
#9580,#9581,#9582,#9583,#9584,#9585));
#9883=CLOSED_SHELL('',(#9586,#9587,#9588,#9589,#9590,#9591,#9592,#9593,
#9594,#9595,#9596,#9597,#9598,#9599,#9600,#9601,#9602,#9603,#9604,#9605,
#9606,#9607,#9608,#9609,#9610,#9611,#9612,#9613,#9614,#9615,#9616,#9617,
#9618,#9619,#9620,#9621,#9622,#9623,#9624,#9625));
#9884=CLOSED_SHELL('',(#9626,#9627,#9628,#9629,#9630,#9631,#9632,#9633,
#9634,#9635,#9636,#9637,#9638,#9639,#9640,#9641,#9642,#9643));
#9885=CLOSED_SHELL('',(#9644,#9645,#9646,#9647,#9648,#9649,#9650,#9651,
#9652,#9653,#9654,#9655,#9656,#9657,#9658,#9659,#9660));
#9886=CLOSED_SHELL('',(#9661,#9662,#9663,#9664,#9665,#9666,#9667,#9668,
#9669,#9670,#9671,#9672,#9673,#9674,#9675,#9676,#9677,#9678,#9679,#9680,
#9681,#9682,#9683,#9684,#9685,#9686,#9687,#9688,#9689));
#9887=CLOSED_SHELL('',(#9690,#9691,#9692));
#9888=CLOSED_SHELL('',(#9693,#9694,#9695,#9696,#9697,#9698,#9699,#9700,
#9701,#9702,#9703,#9704,#9705,#9706,#9707,#9708));
#9889=CLOSED_SHELL('',(#9709,#9710,#9711,#9712,#9713,#9714,#9715,#9716,
#9717,#9718,#9719,#9720,#9721,#9722,#9723,#9724,#9725,#9726,#9727,#9728,
#9729,#9730,#9731,#9732,#9733,#9734,#9735,#9736,#9737,#9738,#9739,#9740,
#9741,#9742,#9743,#9744,#9745,#9746,#9747,#9748,#9749,#9750,#9751,#9752,
#9753,#9754,#9755,#9756));
#9890=CLOSED_SHELL('',(#9757,#9758,#9759,#9760,#9761,#9762,#9763));
#9891=CLOSED_SHELL('',(#9764,#9765,#9766,#9767,#9768,#9769,#9770,#9771,
#9772,#9773,#9774,#9775,#9776,#9777,#9778,#9779));
#9892=CLOSED_SHELL('',(#9780,#9781,#9782,#9783,#9784,#9785,#9786,#9787));
#9893=CLOSED_SHELL('',(#9788,#9789,#9790,#9791,#9792,#9793,#9794,#9795,
#9796));
#9894=CLOSED_SHELL('',(#9797,#9798,#9799,#9800,#9801,#9802,#9803,#9804,
#9805));
#9895=CLOSED_SHELL('',(#9806,#9807,#9808,#9809,#9810));
#9896=CLOSED_SHELL('',(#9811,#9812,#9813,#9814,#9815,#9816,#9817,#9818,
#9819,#9820,#9821,#9822,#9823,#9824,#9825,#9826,#9827,#9828,#9829,#9830,
#9831,#9832,#9833,#9834,#9835,#9836,#9837,#9838,#9839,#9840,#9841,#9842,
#9843,#9844,#9845,#9846,#9847,#9848));
#9897=CLOSED_SHELL('',(#9849,#9850,#9851,#9852,#9853,#9854,#9855,#9856,
#9857,#9858,#9859,#9860,#9861,#9862,#9863,#9864));
#9898=CLOSED_SHELL('',(#9865,#9866,#9867,#9868,#9869,#9870,#9871,#9872,
#9873,#9874,#9875,#9876,#9877,#9878,#9879,#9880));
#9899=DERIVED_UNIT_ELEMENT(#9935,1.);
#9900=DERIVED_UNIT_ELEMENT(#85791,-3.);
#9901=DERIVED_UNIT_ELEMENT(#9935,1.);
#9902=DERIVED_UNIT_ELEMENT(#85791,-3.);
#9903=DERIVED_UNIT_ELEMENT(#9935,1.);
#9904=DERIVED_UNIT_ELEMENT(#85791,-3.);
#9905=DERIVED_UNIT_ELEMENT(#9935,1.);
#9906=DERIVED_UNIT_ELEMENT(#85791,-3.);
#9907=DERIVED_UNIT_ELEMENT(#9935,1.);
#9908=DERIVED_UNIT_ELEMENT(#85791,-3.);
#9909=DERIVED_UNIT_ELEMENT(#9935,1.);
#9910=DERIVED_UNIT_ELEMENT(#85791,-3.);
#9911=DERIVED_UNIT_ELEMENT(#9935,1.);
#9912=DERIVED_UNIT_ELEMENT(#85791,-3.);
#9913=DERIVED_UNIT_ELEMENT(#9935,1.);
#9914=DERIVED_UNIT_ELEMENT(#85791,-3.);
#9915=DERIVED_UNIT_ELEMENT(#9935,1.);
#9916=DERIVED_UNIT_ELEMENT(#85791,-3.);
#9917=DERIVED_UNIT_ELEMENT(#9935,1.);
#9918=DERIVED_UNIT_ELEMENT(#85791,-3.);
#9919=DERIVED_UNIT_ELEMENT(#9935,1.);
#9920=DERIVED_UNIT_ELEMENT(#85791,-3.);
#9921=DERIVED_UNIT_ELEMENT(#9935,1.);
#9922=DERIVED_UNIT_ELEMENT(#85791,-3.);
#9923=DERIVED_UNIT_ELEMENT(#9935,1.);
#9924=DERIVED_UNIT_ELEMENT(#85791,-3.);
#9925=DERIVED_UNIT_ELEMENT(#9935,1.);
#9926=DERIVED_UNIT_ELEMENT(#85791,-3.);
#9927=DERIVED_UNIT_ELEMENT(#9935,1.);
#9928=DERIVED_UNIT_ELEMENT(#85791,-3.);
#9929=DERIVED_UNIT_ELEMENT(#9935,1.);
#9930=DERIVED_UNIT_ELEMENT(#85791,-3.);
#9931=DERIVED_UNIT_ELEMENT(#9935,1.);
#9932=DERIVED_UNIT_ELEMENT(#85791,-3.);
#9933=DERIVED_UNIT_ELEMENT(#9935,1.);
#9934=DERIVED_UNIT_ELEMENT(#85791,-3.);
#9935=(
MASS_UNIT()
NAMED_UNIT(*)
SI_UNIT(.KILO.,.GRAM.)
);
#9936=DERIVED_UNIT((#9899,#9900));
#9937=DERIVED_UNIT((#9901,#9902));
#9938=DERIVED_UNIT((#9903,#9904));
#9939=DERIVED_UNIT((#9905,#9906));
#9940=DERIVED_UNIT((#9907,#9908));
#9941=DERIVED_UNIT((#9909,#9910));
#9942=DERIVED_UNIT((#9911,#9912));
#9943=DERIVED_UNIT((#9913,#9914));
#9944=DERIVED_UNIT((#9915,#9916));
#9945=DERIVED_UNIT((#9917,#9918));
#9946=DERIVED_UNIT((#9919,#9920));
#9947=DERIVED_UNIT((#9921,#9922));
#9948=DERIVED_UNIT((#9923,#9924));
#9949=DERIVED_UNIT((#9925,#9926));
#9950=DERIVED_UNIT((#9927,#9928));
#9951=DERIVED_UNIT((#9929,#9930));
#9952=DERIVED_UNIT((#9931,#9932));
#9953=DERIVED_UNIT((#9933,#9934));
#9954=MEASURE_REPRESENTATION_ITEM('density measure',
POSITIVE_RATIO_MEASURE(7850.),#9936);
#9955=MEASURE_REPRESENTATION_ITEM('density measure',
POSITIVE_RATIO_MEASURE(2670.),#9937);
#9956=MEASURE_REPRESENTATION_ITEM('density measure',
POSITIVE_RATIO_MEASURE(8000.),#9938);
#9957=MEASURE_REPRESENTATION_ITEM('density measure',
POSITIVE_RATIO_MEASURE(7850.),#9939);
#9958=MEASURE_REPRESENTATION_ITEM('density measure',
POSITIVE_RATIO_MEASURE(7850.),#9940);
#9959=MEASURE_REPRESENTATION_ITEM('density measure',
POSITIVE_RATIO_MEASURE(2670.),#9941);
#9960=MEASURE_REPRESENTATION_ITEM('density measure',
POSITIVE_RATIO_MEASURE(7865.),#9942);
#9961=MEASURE_REPRESENTATION_ITEM('density measure',
POSITIVE_RATIO_MEASURE(7810.),#9943);
#9962=MEASURE_REPRESENTATION_ITEM('density measure',
POSITIVE_RATIO_MEASURE(1130.),#9944);
#9963=MEASURE_REPRESENTATION_ITEM('density measure',
POSITIVE_RATIO_MEASURE(8000.),#9945);
#9964=MEASURE_REPRESENTATION_ITEM('density measure',
POSITIVE_RATIO_MEASURE(7810.),#9946);
#9965=MEASURE_REPRESENTATION_ITEM('density measure',
POSITIVE_RATIO_MEASURE(7810.),#9947);
#9966=MEASURE_REPRESENTATION_ITEM('density measure',
POSITIVE_RATIO_MEASURE(7810.),#9948);
#9967=MEASURE_REPRESENTATION_ITEM('density measure',
POSITIVE_RATIO_MEASURE(7810.),#9949);
#9968=MEASURE_REPRESENTATION_ITEM('density measure',
POSITIVE_RATIO_MEASURE(7810.),#9950);
#9969=MEASURE_REPRESENTATION_ITEM('density measure',
POSITIVE_RATIO_MEASURE(8000.),#9951);
#9970=MEASURE_REPRESENTATION_ITEM('density measure',
POSITIVE_RATIO_MEASURE(7850.),#9952);
#9971=MEASURE_REPRESENTATION_ITEM('density measure',
POSITIVE_RATIO_MEASURE(7850.),#9953);
#9972=PROPERTY_DEFINITION_REPRESENTATION(#10062,#10008);
#9973=PROPERTY_DEFINITION_REPRESENTATION(#10063,#10009);
#9974=PROPERTY_DEFINITION_REPRESENTATION(#10064,#10010);
#9975=PROPERTY_DEFINITION_REPRESENTATION(#10065,#10011);
#9976=PROPERTY_DEFINITION_REPRESENTATION(#10066,#10012);
#9977=PROPERTY_DEFINITION_REPRESENTATION(#10067,#10013);
#9978=PROPERTY_DEFINITION_REPRESENTATION(#10068,#10014);
#9979=PROPERTY_DEFINITION_REPRESENTATION(#10069,#10015);
#9980=PROPERTY_DEFINITION_REPRESENTATION(#10070,#10016);
#9981=PROPERTY_DEFINITION_REPRESENTATION(#10071,#10017);
#9982=PROPERTY_DEFINITION_REPRESENTATION(#10072,#10018);
#9983=PROPERTY_DEFINITION_REPRESENTATION(#10073,#10019);
#9984=PROPERTY_DEFINITION_REPRESENTATION(#10074,#10020);
#9985=PROPERTY_DEFINITION_REPRESENTATION(#10075,#10021);
#9986=PROPERTY_DEFINITION_REPRESENTATION(#10076,#10022);
#9987=PROPERTY_DEFINITION_REPRESENTATION(#10077,#10023);
#9988=PROPERTY_DEFINITION_REPRESENTATION(#10078,#10024);
#9989=PROPERTY_DEFINITION_REPRESENTATION(#10079,#10025);
#9990=PROPERTY_DEFINITION_REPRESENTATION(#10080,#10026);
#9991=PROPERTY_DEFINITION_REPRESENTATION(#10081,#10027);
#9992=PROPERTY_DEFINITION_REPRESENTATION(#10082,#10028);
#9993=PROPERTY_DEFINITION_REPRESENTATION(#10083,#10029);
#9994=PROPERTY_DEFINITION_REPRESENTATION(#10084,#10030);
#9995=PROPERTY_DEFINITION_REPRESENTATION(#10085,#10031);
#9996=PROPERTY_DEFINITION_REPRESENTATION(#10086,#10032);
#9997=PROPERTY_DEFINITION_REPRESENTATION(#10087,#10033);
#9998=PROPERTY_DEFINITION_REPRESENTATION(#10088,#10034);
#9999=PROPERTY_DEFINITION_REPRESENTATION(#10089,#10035);
#10000=PROPERTY_DEFINITION_REPRESENTATION(#10090,#10036);
#10001=PROPERTY_DEFINITION_REPRESENTATION(#10091,#10037);
#10002=PROPERTY_DEFINITION_REPRESENTATION(#10092,#10038);
#10003=PROPERTY_DEFINITION_REPRESENTATION(#10093,#10039);
#10004=PROPERTY_DEFINITION_REPRESENTATION(#10094,#10040);
#10005=PROPERTY_DEFINITION_REPRESENTATION(#10095,#10041);
#10006=PROPERTY_DEFINITION_REPRESENTATION(#10096,#10042);
#10007=PROPERTY_DEFINITION_REPRESENTATION(#10097,#10043);
#10008=REPRESENTATION('material name',(#10044),#85771);
#10009=REPRESENTATION('density',(#9954),#85771);
#10010=REPRESENTATION('material name',(#10045),#85772);
#10011=REPRESENTATION('density',(#9955),#85772);
#10012=REPRESENTATION('material name',(#10046),#85773);
#10013=REPRESENTATION('density',(#9956),#85773);
#10014=REPRESENTATION('material name',(#10047),#85774);
#10015=REPRESENTATION('density',(#9957),#85774);
#10016=REPRESENTATION('material name',(#10048),#85775);
#10017=REPRESENTATION('density',(#9958),#85775);
#10018=REPRESENTATION('material name',(#10049),#85776);
#10019=REPRESENTATION('density',(#9959),#85776);
#10020=REPRESENTATION('material name',(#10050),#85777);
#10021=REPRESENTATION('density',(#9960),#85777);
#10022=REPRESENTATION('material name',(#10051),#85778);
#10023=REPRESENTATION('density',(#9961),#85778);
#10024=REPRESENTATION('material name',(#10052),#85779);
#10025=REPRESENTATION('density',(#9962),#85779);
#10026=REPRESENTATION('material name',(#10053),#85780);
#10027=REPRESENTATION('density',(#9963),#85780);
#10028=REPRESENTATION('material name',(#10054),#85781);
#10029=REPRESENTATION('density',(#9964),#85781);
#10030=REPRESENTATION('material name',(#10055),#85782);
#10031=REPRESENTATION('density',(#9965),#85782);
#10032=REPRESENTATION('material name',(#10056),#85783);
#10033=REPRESENTATION('density',(#9966),#85783);
#10034=REPRESENTATION('material name',(#10057),#85784);
#10035=REPRESENTATION('density',(#9967),#85784);
#10036=REPRESENTATION('material name',(#10058),#85785);
#10037=REPRESENTATION('density',(#9968),#85785);
#10038=REPRESENTATION('material name',(#10059),#85786);
#10039=REPRESENTATION('density',(#9969),#85786);
#10040=REPRESENTATION('material name',(#10060),#85787);
#10041=REPRESENTATION('density',(#9970),#85787);
#10042=REPRESENTATION('material name',(#10061),#85788);
#10043=REPRESENTATION('density',(#9971),#85788);
#10044=DESCRIPTIVE_REPRESENTATION_ITEM('Steel AISI 1045 450 QT',
'Steel AISI 1045 450 QT');
#10045=DESCRIPTIVE_REPRESENTATION_ITEM('Aluminum A356 T6',
'Aluminum A356 T6');
#10046=DESCRIPTIVE_REPRESENTATION_ITEM('Stainless Steel AISI 304',
'Stainless Steel AISI 304');
#10047=DESCRIPTIVE_REPRESENTATION_ITEM('Steel, Mild','Steel, Mild');
#10048=DESCRIPTIVE_REPRESENTATION_ITEM('Steel AISI 4340 350A QT',
'Steel AISI 4340 350A QT');
#10049=DESCRIPTIVE_REPRESENTATION_ITEM('Aluminum A356 T6',
'Aluminum A356 T6');
#10050=DESCRIPTIVE_REPRESENTATION_ITEM('Steel AISI 9262 271 QT',
'Steel AISI 9262 271 QT');
#10051=DESCRIPTIVE_REPRESENTATION_ITEM('Steel AISI 5210 517 H',
'Steel AISI 5210 517 H');
#10052=DESCRIPTIVE_REPRESENTATION_ITEM('Nylon 6/6','Nylon 6/6');
#10053=DESCRIPTIVE_REPRESENTATION_ITEM('Stainless Steel AISI 302',
'Stainless Steel AISI 302');
#10054=DESCRIPTIVE_REPRESENTATION_ITEM('Steel AISI 5210 517 H',
'Steel AISI 5210 517 H');
#10055=DESCRIPTIVE_REPRESENTATION_ITEM('Steel AISI 5210 517 H',
'Steel AISI 5210 517 H');
#10056=DESCRIPTIVE_REPRESENTATION_ITEM('Steel AISI 5210 517 H',
'Steel AISI 5210 517 H');
#10057=DESCRIPTIVE_REPRESENTATION_ITEM('Steel AISI 5210 517 H',
'Steel AISI 5210 517 H');
#10058=DESCRIPTIVE_REPRESENTATION_ITEM('Steel AISI 5210 517 H',
'Steel AISI 5210 517 H');
#10059=DESCRIPTIVE_REPRESENTATION_ITEM('Stainless Steel AISI 304',
'Stainless Steel AISI 304');
#10060=DESCRIPTIVE_REPRESENTATION_ITEM('Steel AISI 1060',
'Steel AISI 1060');
#10061=DESCRIPTIVE_REPRESENTATION_ITEM('Steel AISI 1060',
'Steel AISI 1060');
#10062=PROPERTY_DEFINITION('material property','material name',#85883);
#10063=PROPERTY_DEFINITION('material property','density of part',#85883);
#10064=PROPERTY_DEFINITION('material property','material name',#85884);
#10065=PROPERTY_DEFINITION('material property','density of part',#85884);
#10066=PROPERTY_DEFINITION('material property','material name',#85885);
#10067=PROPERTY_DEFINITION('material property','density of part',#85885);
#10068=PROPERTY_DEFINITION('material property','material name',#85886);
#10069=PROPERTY_DEFINITION('material property','density of part',#85886);
#10070=PROPERTY_DEFINITION('material property','material name',#85887);
#10071=PROPERTY_DEFINITION('material property','density of part',#85887);
#10072=PROPERTY_DEFINITION('material property','material name',#85888);
#10073=PROPERTY_DEFINITION('material property','density of part',#85888);
#10074=PROPERTY_DEFINITION('material property','material name',#85889);
#10075=PROPERTY_DEFINITION('material property','density of part',#85889);
#10076=PROPERTY_DEFINITION('material property','material name',#85890);
#10077=PROPERTY_DEFINITION('material property','density of part',#85890);
#10078=PROPERTY_DEFINITION('material property','material name',#85891);
#10079=PROPERTY_DEFINITION('material property','density of part',#85891);
#10080=PROPERTY_DEFINITION('material property','material name',#85892);
#10081=PROPERTY_DEFINITION('material property','density of part',#85892);
#10082=PROPERTY_DEFINITION('material property','material name',#85893);
#10083=PROPERTY_DEFINITION('material property','density of part',#85893);
#10084=PROPERTY_DEFINITION('material property','material name',#85894);
#10085=PROPERTY_DEFINITION('material property','density of part',#85894);
#10086=PROPERTY_DEFINITION('material property','material name',#85895);
#10087=PROPERTY_DEFINITION('material property','density of part',#85895);
#10088=PROPERTY_DEFINITION('material property','material name',#85896);
#10089=PROPERTY_DEFINITION('material property','density of part',#85896);
#10090=PROPERTY_DEFINITION('material property','material name',#85897);
#10091=PROPERTY_DEFINITION('material property','density of part',#85897);
#10092=PROPERTY_DEFINITION('material property','material name',#85898);
#10093=PROPERTY_DEFINITION('material property','density of part',#85898);
#10094=PROPERTY_DEFINITION('material property','material name',#85899);
#10095=PROPERTY_DEFINITION('material property','density of part',#85899);
#10096=PROPERTY_DEFINITION('material property','material name',#85900);
#10097=PROPERTY_DEFINITION('material property','density of part',#85900);
#10098=AXIS2_PLACEMENT_3D('',#13217,#10959,#10960);
#10099=AXIS2_PLACEMENT_3D('',#13218,#10961,#10962);
#10100=AXIS2_PLACEMENT_3D('',#13219,#10963,#10964);
#10101=AXIS2_PLACEMENT_3D('',#13222,#10965,#10966);
#10102=AXIS2_PLACEMENT_3D('',#13224,#10967,#10968);
#10103=AXIS2_PLACEMENT_3D('',#13225,#10969,#10970);
#10104=AXIS2_PLACEMENT_3D('',#13226,#10971,#10972);
#10105=AXIS2_PLACEMENT_3D('',#13227,#10973,#10974);
#10106=AXIS2_PLACEMENT_3D('',#13231,#10976,#10977);
#10107=AXIS2_PLACEMENT_3D('',#13232,#10978,#10979);
#10108=AXIS2_PLACEMENT_3D('',#13233,#10980,#10981);
#10109=AXIS2_PLACEMENT_3D('',#13247,#10985,#10986);
#10110=AXIS2_PLACEMENT_3D('',#13282,#10987,#10988);
#10111=AXIS2_PLACEMENT_3D('',#13284,#10989,#10990);
#10112=AXIS2_PLACEMENT_3D('',#13285,#10991,#10992);
#10113=AXIS2_PLACEMENT_3D('',#13286,#10993,#10994);
#10114=AXIS2_PLACEMENT_3D('',#13404,#10996,#10997);
#10115=AXIS2_PLACEMENT_3D('',#13407,#10998,#10999);
#10116=AXIS2_PLACEMENT_3D('',#13409,#11000,#11001);
#10117=AXIS2_PLACEMENT_3D('',#13410,#11002,#11003);
#10118=AXIS2_PLACEMENT_3D('',#13411,#11004,#11005);
#10119=AXIS2_PLACEMENT_3D('',#13412,#11006,#11007);
#10120=AXIS2_PLACEMENT_3D('',#13416,#11009,#11010);
#10121=AXIS2_PLACEMENT_3D('',#13417,#11011,#11012);
#10122=AXIS2_PLACEMENT_3D('',#13418,#11013,#11014);
#10123=AXIS2_PLACEMENT_3D('',#13472,#11017,#11018);
#10124=AXIS2_PLACEMENT_3D('',#13474,#11019,#11020);
#10125=AXIS2_PLACEMENT_3D('',#13475,#11021,#11022);
#10126=AXIS2_PLACEMENT_3D('',#13476,#11023,#11024);
#10127=AXIS2_PLACEMENT_3D('',#13664,#11027,#11028);
#10128=AXIS2_PLACEMENT_3D('',#13666,#11030,#11031);
#10129=AXIS2_PLACEMENT_3D('',#13696,#11032,#11033);
#10130=AXIS2_PLACEMENT_3D('',#13698,#11035,#11036);
#10131=AXIS2_PLACEMENT_3D('',#13699,#11037,#11038);
#10132=AXIS2_PLACEMENT_3D('',#14266,#11039,#11040);
#10133=AXIS2_PLACEMENT_3D('',#14273,#11041,#11042);
#10134=AXIS2_PLACEMENT_3D('',#14274,#11043,#11044);
#10135=AXIS2_PLACEMENT_3D('',#14450,#11045,#11046);
#10136=AXIS2_PLACEMENT_3D('',#14476,#11047,#11048);
#10137=AXIS2_PLACEMENT_3D('',#14524,#11049,#11050);
#10138=AXIS2_PLACEMENT_3D('',#14538,#11051,#11052);
#10139=AXIS2_PLACEMENT_3D('',#14539,#11053,#11054);
#10140=AXIS2_PLACEMENT_3D('',#14597,#11055,#11056);
#10141=AXIS2_PLACEMENT_3D('',#14635,#11057,#11058);
#10142=AXIS2_PLACEMENT_3D('',#14657,#11059,#11060);
#10143=AXIS2_PLACEMENT_3D('',#14659,#11061,#11062);
#10144=AXIS2_PLACEMENT_3D('',#14688,#11063,#11064);
#10145=AXIS2_PLACEMENT_3D('',#14713,#11065,#11066);
#10146=AXIS2_PLACEMENT_3D('',#14795,#11067,#11068);
#10147=AXIS2_PLACEMENT_3D('',#14796,#11069,#11070);
#10148=AXIS2_PLACEMENT_3D('',#14797,#11071,#11072);
#10149=AXIS2_PLACEMENT_3D('',#14822,#11073,#11074);
#10150=AXIS2_PLACEMENT_3D('',#14854,#11076,#11077);
#10151=AXIS2_PLACEMENT_3D('',#14880,#11078,#11079);
#10152=AXIS2_PLACEMENT_3D('',#14930,#11080,#11081);
#10153=AXIS2_PLACEMENT_3D('',#14968,#11082,#11083);
#10154=AXIS2_PLACEMENT_3D('',#14990,#11084,#11085);
#10155=AXIS2_PLACEMENT_3D('',#15325,#11086,#11087);
#10156=AXIS2_PLACEMENT_3D('',#15797,#11090,#11091);
#10157=AXIS2_PLACEMENT_3D('',#15828,#11092,#11093);
#10158=AXIS2_PLACEMENT_3D('',#15837,#11094,#11095);
#10159=AXIS2_PLACEMENT_3D('',#15878,#11096,#11097);
#10160=AXIS2_PLACEMENT_3D('',#15883,#11098,#11099);
#10161=AXIS2_PLACEMENT_3D('',#15909,#11100,#11101);
#10162=AXIS2_PLACEMENT_3D('',#15910,#11102,#11103);
#10163=AXIS2_PLACEMENT_3D('',#15928,#11104,#11105);
#10164=AXIS2_PLACEMENT_3D('',#15930,#11106,#11107);
#10165=AXIS2_PLACEMENT_3D('',#15931,#11108,#11109);
#10166=AXIS2_PLACEMENT_3D('',#16012,#11111,#11112);
#10167=AXIS2_PLACEMENT_3D('',#16650,#11114,#11115);
#10168=AXIS2_PLACEMENT_3D('',#16767,#11116,#11117);
#10169=AXIS2_PLACEMENT_3D('',#16967,#11118,#11119);
#10170=AXIS2_PLACEMENT_3D('',#16969,#11120,#11121);
#10171=AXIS2_PLACEMENT_3D('',#16971,#11122,#11123);
#10172=AXIS2_PLACEMENT_3D('',#16999,#11124,#11125);
#10173=AXIS2_PLACEMENT_3D('',#17006,#11126,#11127);
#10174=AXIS2_PLACEMENT_3D('',#17033,#11128,#11129);
#10175=AXIS2_PLACEMENT_3D('',#17091,#11130,#11131);
#10176=AXIS2_PLACEMENT_3D('',#17092,#11132,#11133);
#10177=AXIS2_PLACEMENT_3D('',#17093,#11134,#11135);
#10178=AXIS2_PLACEMENT_3D('',#17094,#11136,#11137);
#10179=AXIS2_PLACEMENT_3D('',#17095,#11138,#11139);
#10180=AXIS2_PLACEMENT_3D('',#17096,#11140,#11141);
#10181=AXIS2_PLACEMENT_3D('',#17197,#11143,#11144);
#10182=AXIS2_PLACEMENT_3D('',#17754,#11146,#11147);
#10183=AXIS2_PLACEMENT_3D('',#17755,#11148,#11149);
#10184=AXIS2_PLACEMENT_3D('',#17779,#11152,#11153);
#10185=AXIS2_PLACEMENT_3D('',#17782,#11154,#11155);
#10186=AXIS2_PLACEMENT_3D('',#18333,#11158,#11159);
#10187=AXIS2_PLACEMENT_3D('',#18340,#11160,#11161);
#10188=AXIS2_PLACEMENT_3D('',#18368,#11162,#11163);
#10189=AXIS2_PLACEMENT_3D('',#18451,#11164,#11165);
#10190=AXIS2_PLACEMENT_3D('',#18499,#11166,#11167);
#10191=AXIS2_PLACEMENT_3D('',#18522,#11168,#11169);
#10192=AXIS2_PLACEMENT_3D('',#18674,#11170,#11171);
#10193=AXIS2_PLACEMENT_3D('',#18681,#11172,#11173);
#10194=AXIS2_PLACEMENT_3D('',#18717,#11174,#11175);
#10195=AXIS2_PLACEMENT_3D('',#18744,#11176,#11177);
#10196=AXIS2_PLACEMENT_3D('',#18745,#11178,#11179);
#10197=AXIS2_PLACEMENT_3D('',#18746,#11180,#11181);
#10198=AXIS2_PLACEMENT_3D('',#18834,#11182,#11183);
#10199=AXIS2_PLACEMENT_3D('',#18903,#11184,#11185);
#10200=AXIS2_PLACEMENT_3D('',#18905,#11187,#11188);
#10201=AXIS2_PLACEMENT_3D('',#18906,#11189,#11190);
#10202=AXIS2_PLACEMENT_3D('',#18907,#11191,#11192);
#10203=AXIS2_PLACEMENT_3D('',#18908,#11193,#11194);
#10204=AXIS2_PLACEMENT_3D('',#18909,#11195,#11196);
#10205=AXIS2_PLACEMENT_3D('',#20164,#11197,#11198);
#10206=AXIS2_PLACEMENT_3D('',#20165,#11199,#11200);
#10207=AXIS2_PLACEMENT_3D('',#20172,#11201,#11202);
#10208=AXIS2_PLACEMENT_3D('',#20176,#11204,#11205);
#10209=AXIS2_PLACEMENT_3D('',#20200,#11207,#11208);
#10210=AXIS2_PLACEMENT_3D('',#20207,#11209,#11210);
#10211=AXIS2_PLACEMENT_3D('',#20238,#11211,#11212);
#10212=AXIS2_PLACEMENT_3D('',#20265,#11213,#11214);
#10213=AXIS2_PLACEMENT_3D('',#20381,#11215,#11216);
#10214=AXIS2_PLACEMENT_3D('',#20431,#11217,#11218);
#10215=AXIS2_PLACEMENT_3D('',#20462,#11220,#11221);
#10216=AXIS2_PLACEMENT_3D('',#20585,#11222,#11223);
#10217=AXIS2_PLACEMENT_3D('',#20758,#11224,#11225);
#10218=AXIS2_PLACEMENT_3D('',#20761,#11227,#11228);
#10219=AXIS2_PLACEMENT_3D('',#20762,#11229,#11230);
#10220=AXIS2_PLACEMENT_3D('',#20811,#11232,#11233);
#10221=AXIS2_PLACEMENT_3D('',#20922,#11234,#11235);
#10222=AXIS2_PLACEMENT_3D('',#20945,#11236,#11237);
#10223=AXIS2_PLACEMENT_3D('',#20994,#11238,#11239);
#10224=AXIS2_PLACEMENT_3D('',#21019,#11240,#11241);
#10225=AXIS2_PLACEMENT_3D('',#21028,#11243,#11244);
#10226=AXIS2_PLACEMENT_3D('',#21034,#11247,#11248);
#10227=AXIS2_PLACEMENT_3D('',#21040,#11249,#11250);
#10228=AXIS2_PLACEMENT_3D('',#21051,#11253,#11254);
#10229=AXIS2_PLACEMENT_3D('',#21053,#11255,#11256);
#10230=AXIS2_PLACEMENT_3D('',#21055,#11257,#11258);
#10231=AXIS2_PLACEMENT_3D('',#21057,#11259,#11260);
#10232=AXIS2_PLACEMENT_3D('',#21058,#11261,#11262);
#10233=AXIS2_PLACEMENT_3D('',#21061,#11264,#11265);
#10234=AXIS2_PLACEMENT_3D('',#21062,#11266,#11267);
#10235=AXIS2_PLACEMENT_3D('',#21064,#11268,#11269);
#10236=AXIS2_PLACEMENT_3D('',#21068,#11271,#11272);
#10237=AXIS2_PLACEMENT_3D('',#21070,#11274,#11275);
#10238=AXIS2_PLACEMENT_3D('',#21073,#11277,#11278);
#10239=AXIS2_PLACEMENT_3D('',#21075,#11280,#11281);
#10240=AXIS2_PLACEMENT_3D('',#21076,#11282,#11283);
#10241=AXIS2_PLACEMENT_3D('',#21077,#11284,#11285);
#10242=AXIS2_PLACEMENT_3D('',#21078,#11286,#11287);
#10243=AXIS2_PLACEMENT_3D('',#21079,#11288,#11289);
#10244=AXIS2_PLACEMENT_3D('',#21082,#11291,#11292);
#10245=AXIS2_PLACEMENT_3D('',#21083,#11293,#11294);
#10246=AXIS2_PLACEMENT_3D('',#21096,#11297,#11298);
#10247=AXIS2_PLACEMENT_3D('',#21112,#11300,#11301);
#10248=AXIS2_PLACEMENT_3D('',#21192,#11309,#11310);
#10249=AXIS2_PLACEMENT_3D('',#21194,#11311,#11312);
#10250=AXIS2_PLACEMENT_3D('',#21196,#11313,#11314);
#10251=AXIS2_PLACEMENT_3D('',#21198,#11315,#11316);
#10252=AXIS2_PLACEMENT_3D('',#21220,#11317,#11318);
#10253=AXIS2_PLACEMENT_3D('',#21221,#11319,#11320);
#10254=AXIS2_PLACEMENT_3D('',#21243,#11321,#11322);
#10255=AXIS2_PLACEMENT_3D('',#21279,#11323,#11324);
#10256=AXIS2_PLACEMENT_3D('',#21287,#11325,#11326);
#10257=AXIS2_PLACEMENT_3D('',#21308,#11327,#11328);
#10258=AXIS2_PLACEMENT_3D('',#21326,#11329,#11330);
#10259=AXIS2_PLACEMENT_3D('',#21327,#11331,#11332);
#10260=AXIS2_PLACEMENT_3D('',#21328,#11333,#11334);
#10261=AXIS2_PLACEMENT_3D('',#21329,#11335,#11336);
#10262=AXIS2_PLACEMENT_3D('',#21857,#11338,#11339);
#10263=AXIS2_PLACEMENT_3D('',#21858,#11340,#11341);
#10264=AXIS2_PLACEMENT_3D('',#21859,#11342,#11343);
#10265=AXIS2_PLACEMENT_3D('',#21976,#11344,#11345);
#10266=AXIS2_PLACEMENT_3D('',#21978,#11346,#11347);
#10267=AXIS2_PLACEMENT_3D('',#22007,#11348,#11349);
#10268=AXIS2_PLACEMENT_3D('',#22008,#11350,#11351);
#10269=AXIS2_PLACEMENT_3D('',#22100,#11355,#11356);
#10270=AXIS2_PLACEMENT_3D('',#22101,#11357,#11358);
#10271=AXIS2_PLACEMENT_3D('',#22102,#11359,#11360);
#10272=AXIS2_PLACEMENT_3D('',#22103,#11361,#11362);
#10273=AXIS2_PLACEMENT_3D('',#22104,#11363,#11364);
#10274=AXIS2_PLACEMENT_3D('',#22117,#11366,#11367);
#10275=AXIS2_PLACEMENT_3D('',#22180,#11368,#11369);
#10276=AXIS2_PLACEMENT_3D('',#22181,#11370,#11371);
#10277=AXIS2_PLACEMENT_3D('',#22203,#11372,#11373);
#10278=AXIS2_PLACEMENT_3D('',#22205,#11374,#11375);
#10279=AXIS2_PLACEMENT_3D('',#22206,#11376,#11377);
#10280=AXIS2_PLACEMENT_3D('',#22480,#11378,#11379);
#10281=AXIS2_PLACEMENT_3D('',#22502,#11380,#11381);
#10282=AXIS2_PLACEMENT_3D('',#22523,#11382,#11383);
#10283=AXIS2_PLACEMENT_3D('',#22525,#11384,#11385);
#10284=AXIS2_PLACEMENT_3D('',#22526,#11386,#11387);
#10285=AXIS2_PLACEMENT_3D('',#22547,#11388,#11389);
#10286=AXIS2_PLACEMENT_3D('',#22548,#11390,#11391);
#10287=AXIS2_PLACEMENT_3D('',#22570,#11392,#11393);
#10288=AXIS2_PLACEMENT_3D('',#22676,#11396,#11397);
#10289=AXIS2_PLACEMENT_3D('',#22698,#11398,#11399);
#10290=AXIS2_PLACEMENT_3D('',#22723,#11400,#11401);
#10291=AXIS2_PLACEMENT_3D('',#22724,#11402,#11403);
#10292=AXIS2_PLACEMENT_3D('',#22725,#11404,#11405);
#10293=AXIS2_PLACEMENT_3D('',#22794,#11406,#11407);
#10294=AXIS2_PLACEMENT_3D('',#22796,#11409,#11410);
#10295=AXIS2_PLACEMENT_3D('',#22797,#11411,#11412);
#10296=AXIS2_PLACEMENT_3D('',#23319,#11414,#11415);
#10297=AXIS2_PLACEMENT_3D('',#23321,#11417,#11418);
#10298=AXIS2_PLACEMENT_3D('',#23323,#11420,#11421);
#10299=AXIS2_PLACEMENT_3D('',#23325,#11423,#11424);
#10300=AXIS2_PLACEMENT_3D('',#23327,#11426,#11427);
#10301=AXIS2_PLACEMENT_3D('',#23328,#11428,#11429);
#10302=AXIS2_PLACEMENT_3D('',#23329,#11430,#11431);
#10303=AXIS2_PLACEMENT_3D('',#23330,#11432,#11433);
#10304=AXIS2_PLACEMENT_3D('',#23331,#11434,#11435);
#10305=AXIS2_PLACEMENT_3D('',#23340,#11440,#11441);
#10306=AXIS2_PLACEMENT_3D('',#23346,#11445,#11446);
#10307=AXIS2_PLACEMENT_3D('',#23352,#11450,#11451);
#10308=AXIS2_PLACEMENT_3D('',#23358,#11455,#11456);
#10309=AXIS2_PLACEMENT_3D('',#23364,#11460,#11461);
#10310=AXIS2_PLACEMENT_3D('',#23370,#11465,#11466);
#10311=AXIS2_PLACEMENT_3D('',#23376,#11470,#11471);
#10312=AXIS2_PLACEMENT_3D('',#23379,#11474,#11475);
#10313=AXIS2_PLACEMENT_3D('',#23385,#11479,#11480);
#10314=AXIS2_PLACEMENT_3D('',#23389,#11483,#11484);
#10315=AXIS2_PLACEMENT_3D('',#23393,#11487,#11488);
#10316=AXIS2_PLACEMENT_3D('',#23397,#11491,#11492);
#10317=AXIS2_PLACEMENT_3D('',#23423,#11505,#11506);
#10318=AXIS2_PLACEMENT_3D('',#23425,#11507,#11508);
#10319=AXIS2_PLACEMENT_3D('',#23427,#11509,#11510);
#10320=AXIS2_PLACEMENT_3D('',#23429,#11511,#11512);
#10321=AXIS2_PLACEMENT_3D('',#23431,#11513,#11514);
#10322=AXIS2_PLACEMENT_3D('',#23433,#11515,#11516);
#10323=AXIS2_PLACEMENT_3D('',#23434,#11517,#11518);
#10324=AXIS2_PLACEMENT_3D('',#23438,#11520,#11521);
#10325=AXIS2_PLACEMENT_3D('',#23439,#11522,#11523);
#10326=AXIS2_PLACEMENT_3D('',#23442,#11525,#11526);
#10327=AXIS2_PLACEMENT_3D('',#23443,#11527,#11528);
#10328=AXIS2_PLACEMENT_3D('',#23445,#11530,#11531);
#10329=AXIS2_PLACEMENT_3D('',#23449,#11533,#11534);
#10330=AXIS2_PLACEMENT_3D('',#23450,#11535,#11536);
#10331=AXIS2_PLACEMENT_3D('',#23453,#11538,#11539);
#10332=AXIS2_PLACEMENT_3D('',#23454,#11540,#11541);
#10333=AXIS2_PLACEMENT_3D('',#23456,#11543,#11544);
#10334=AXIS2_PLACEMENT_3D('',#23460,#11546,#11547);
#10335=AXIS2_PLACEMENT_3D('',#23461,#11548,#11549);
#10336=AXIS2_PLACEMENT_3D('',#23464,#11551,#11552);
#10337=AXIS2_PLACEMENT_3D('',#23465,#11553,#11554);
#10338=AXIS2_PLACEMENT_3D('',#23467,#11556,#11557);
#10339=AXIS2_PLACEMENT_3D('',#23471,#11559,#11560);
#10340=AXIS2_PLACEMENT_3D('',#23472,#11561,#11562);
#10341=AXIS2_PLACEMENT_3D('',#23475,#11564,#11565);
#10342=AXIS2_PLACEMENT_3D('',#23476,#11566,#11567);
#10343=AXIS2_PLACEMENT_3D('',#23478,#11569,#11570);
#10344=AXIS2_PLACEMENT_3D('',#23482,#11572,#11573);
#10345=AXIS2_PLACEMENT_3D('',#23483,#11574,#11575);
#10346=AXIS2_PLACEMENT_3D('',#23486,#11577,#11578);
#10347=AXIS2_PLACEMENT_3D('',#23487,#11579,#11580);
#10348=AXIS2_PLACEMENT_3D('',#23491,#11582,#11583);
#10349=AXIS2_PLACEMENT_3D('',#23492,#11584,#11585);
#10350=AXIS2_PLACEMENT_3D('',#23495,#11587,#11588);
#10351=AXIS2_PLACEMENT_3D('',#23496,#11589,#11590);
#10352=AXIS2_PLACEMENT_3D('',#23498,#11591,#11592);
#10353=AXIS2_PLACEMENT_3D('',#23500,#11594,#11595);
#10354=AXIS2_PLACEMENT_3D('',#23502,#11596,#11597);
#10355=AXIS2_PLACEMENT_3D('',#23504,#11599,#11600);
#10356=AXIS2_PLACEMENT_3D('',#23506,#11601,#11602);
#10357=AXIS2_PLACEMENT_3D('',#23509,#11604,#11605);
#10358=AXIS2_PLACEMENT_3D('',#23510,#11606,#11607);
#10359=AXIS2_PLACEMENT_3D('',#23516,#11611,#11612);
#10360=AXIS2_PLACEMENT_3D('',#23520,#11615,#11616);
#10361=AXIS2_PLACEMENT_3D('',#23524,#11619,#11620);
#10362=AXIS2_PLACEMENT_3D('',#23528,#11623,#11624);
#10363=AXIS2_PLACEMENT_3D('',#23532,#11627,#11628);
#10364=AXIS2_PLACEMENT_3D('',#23536,#11631,#11632);
#10365=AXIS2_PLACEMENT_3D('',#23540,#11635,#11636);
#10366=AXIS2_PLACEMENT_3D('',#23544,#11639,#11640);
#10367=AXIS2_PLACEMENT_3D('',#23548,#11643,#11644);
#10368=AXIS2_PLACEMENT_3D('',#23552,#11647,#11648);
#10369=AXIS2_PLACEMENT_3D('',#23556,#11651,#11652);
#10370=AXIS2_PLACEMENT_3D('',#23558,#11654,#11655);
#10371=AXIS2_PLACEMENT_3D('',#23559,#11656,#11657);
#10372=AXIS2_PLACEMENT_3D('',#23563,#11660,#11661);
#10373=AXIS2_PLACEMENT_3D('',#23567,#11664,#11665);
#10374=AXIS2_PLACEMENT_3D('',#23571,#11668,#11669);
#10375=AXIS2_PLACEMENT_3D('',#23573,#11671,#11672);
#10376=AXIS2_PLACEMENT_3D('',#23574,#11673,#11674);
#10377=AXIS2_PLACEMENT_3D('',#23575,#11675,#11676);
#10378=AXIS2_PLACEMENT_3D('',#23578,#11677,#11678);
#10379=AXIS2_PLACEMENT_3D('',#23582,#11680,#11681);
#10380=AXIS2_PLACEMENT_3D('',#23584,#11683,#11684);
#10381=AXIS2_PLACEMENT_3D('',#23590,#11688,#11689);
#10382=AXIS2_PLACEMENT_3D('',#23593,#11690,#11691);
#10383=AXIS2_PLACEMENT_3D('',#23597,#11693,#11694);
#10384=AXIS2_PLACEMENT_3D('',#23599,#11696,#11697);
#10385=AXIS2_PLACEMENT_3D('',#23602,#11700,#11701);
#10386=AXIS2_PLACEMENT_3D('',#23604,#11702,#11703);
#10387=AXIS2_PLACEMENT_3D('',#23607,#11705,#11706);
#10388=AXIS2_PLACEMENT_3D('',#23608,#11707,#11708);
#10389=AXIS2_PLACEMENT_3D('',#23614,#11712,#11713);
#10390=AXIS2_PLACEMENT_3D('',#23616,#11714,#11715);
#10391=AXIS2_PLACEMENT_3D('',#23619,#11717,#11718);
#10392=AXIS2_PLACEMENT_3D('',#23620,#11719,#11720);
#10393=AXIS2_PLACEMENT_3D('',#23623,#11723,#11724);
#10394=AXIS2_PLACEMENT_3D('',#23626,#11725,#11726);
#10395=AXIS2_PLACEMENT_3D('',#23630,#11728,#11729);
#10396=AXIS2_PLACEMENT_3D('',#23632,#11731,#11732);
#10397=AXIS2_PLACEMENT_3D('',#23638,#11736,#11737);
#10398=AXIS2_PLACEMENT_3D('',#23641,#11738,#11739);
#10399=AXIS2_PLACEMENT_3D('',#23645,#11741,#11742);
#10400=AXIS2_PLACEMENT_3D('',#23647,#11744,#11745);
#10401=AXIS2_PLACEMENT_3D('',#23650,#11748,#11749);
#10402=AXIS2_PLACEMENT_3D('',#23652,#11750,#11751);
#10403=AXIS2_PLACEMENT_3D('',#23655,#11753,#11754);
#10404=AXIS2_PLACEMENT_3D('',#23656,#11755,#11756);
#10405=AXIS2_PLACEMENT_3D('',#23662,#11760,#11761);
#10406=AXIS2_PLACEMENT_3D('',#23664,#11762,#11763);
#10407=AXIS2_PLACEMENT_3D('',#23667,#11765,#11766);
#10408=AXIS2_PLACEMENT_3D('',#23668,#11767,#11768);
#10409=AXIS2_PLACEMENT_3D('',#23671,#11771,#11772);
#10410=AXIS2_PLACEMENT_3D('',#23674,#11773,#11774);
#10411=AXIS2_PLACEMENT_3D('',#23678,#11776,#11777);
#10412=AXIS2_PLACEMENT_3D('',#23680,#11779,#11780);
#10413=AXIS2_PLACEMENT_3D('',#23686,#11784,#11785);
#10414=AXIS2_PLACEMENT_3D('',#23689,#11786,#11787);
#10415=AXIS2_PLACEMENT_3D('',#23693,#11789,#11790);
#10416=AXIS2_PLACEMENT_3D('',#23695,#11792,#11793);
#10417=AXIS2_PLACEMENT_3D('',#23698,#11796,#11797);
#10418=AXIS2_PLACEMENT_3D('',#23700,#11798,#11799);
#10419=AXIS2_PLACEMENT_3D('',#23703,#11801,#11802);
#10420=AXIS2_PLACEMENT_3D('',#23704,#11803,#11804);
#10421=AXIS2_PLACEMENT_3D('',#23710,#11808,#11809);
#10422=AXIS2_PLACEMENT_3D('',#23712,#11810,#11811);
#10423=AXIS2_PLACEMENT_3D('',#23715,#11813,#11814);
#10424=AXIS2_PLACEMENT_3D('',#23716,#11815,#11816);
#10425=AXIS2_PLACEMENT_3D('',#23719,#11819,#11820);
#10426=AXIS2_PLACEMENT_3D('',#23721,#11821,#11822);
#10427=AXIS2_PLACEMENT_3D('',#23724,#11824,#11825);
#10428=AXIS2_PLACEMENT_3D('',#23725,#11826,#11827);
#10429=AXIS2_PLACEMENT_3D('',#23727,#11828,#11829);
#10430=AXIS2_PLACEMENT_3D('',#23730,#11831,#11832);
#10431=AXIS2_PLACEMENT_3D('',#23731,#11833,#11834);
#10432=AXIS2_PLACEMENT_3D('',#23733,#11835,#11836);
#10433=AXIS2_PLACEMENT_3D('',#23736,#11838,#11839);
#10434=AXIS2_PLACEMENT_3D('',#23737,#11840,#11841);
#10435=AXIS2_PLACEMENT_3D('',#23739,#11842,#11843);
#10436=AXIS2_PLACEMENT_3D('',#23742,#11845,#11846);
#10437=AXIS2_PLACEMENT_3D('',#23743,#11847,#11848);
#10438=AXIS2_PLACEMENT_3D('',#23745,#11849,#11850);
#10439=AXIS2_PLACEMENT_3D('',#23748,#11852,#11853);
#10440=AXIS2_PLACEMENT_3D('',#23749,#11854,#11855);
#10441=AXIS2_PLACEMENT_3D('',#23751,#11856,#11857);
#10442=AXIS2_PLACEMENT_3D('',#23754,#11859,#11860);
#10443=AXIS2_PLACEMENT_3D('',#23755,#11861,#11862);
#10444=AXIS2_PLACEMENT_3D('',#23764,#11867,#11868);
#10445=AXIS2_PLACEMENT_3D('',#23770,#11872,#11873);
#10446=AXIS2_PLACEMENT_3D('',#23776,#11877,#11878);
#10447=AXIS2_PLACEMENT_3D('',#23782,#11882,#11883);
#10448=AXIS2_PLACEMENT_3D('',#23788,#11887,#11888);
#10449=AXIS2_PLACEMENT_3D('',#23794,#11892,#11893);
#10450=AXIS2_PLACEMENT_3D('',#23800,#11897,#11898);
#10451=AXIS2_PLACEMENT_3D('',#23803,#11901,#11902);
#10452=AXIS2_PLACEMENT_3D('',#23804,#11903,#11904);
#10453=AXIS2_PLACEMENT_3D('',#23805,#11905,#11906);
#10454=AXIS2_PLACEMENT_3D('',#23806,#11907,#11908);
#10455=AXIS2_PLACEMENT_3D('',#23815,#11913,#11914);
#10456=AXIS2_PLACEMENT_3D('',#23821,#11918,#11919);
#10457=AXIS2_PLACEMENT_3D('',#23827,#11923,#11924);
#10458=AXIS2_PLACEMENT_3D('',#23833,#11928,#11929);
#10459=AXIS2_PLACEMENT_3D('',#23839,#11933,#11934);
#10460=AXIS2_PLACEMENT_3D('',#23842,#11937,#11938);
#10461=AXIS2_PLACEMENT_3D('',#23848,#11942,#11943);
#10462=AXIS2_PLACEMENT_3D('',#23852,#11946,#11947);
#10463=AXIS2_PLACEMENT_3D('',#23856,#11950,#11951);
#10464=AXIS2_PLACEMENT_3D('',#23858,#11952,#11953);
#10465=AXIS2_PLACEMENT_3D('',#23860,#11954,#11955);
#10466=AXIS2_PLACEMENT_3D('',#23862,#11956,#11957);
#10467=AXIS2_PLACEMENT_3D('',#23864,#11958,#11959);
#10468=AXIS2_PLACEMENT_3D('',#23865,#11960,#11961);
#10469=AXIS2_PLACEMENT_3D('',#23867,#11962,#11963);
#10470=AXIS2_PLACEMENT_3D('',#23869,#11965,#11966);
#10471=AXIS2_PLACEMENT_3D('',#23871,#11967,#11968);
#10472=AXIS2_PLACEMENT_3D('',#23873,#11970,#11971);
#10473=AXIS2_PLACEMENT_3D('',#23875,#11972,#11973);
#10474=AXIS2_PLACEMENT_3D('',#23877,#11975,#11976);
#10475=AXIS2_PLACEMENT_3D('',#23879,#11977,#11978);
#10476=AXIS2_PLACEMENT_3D('',#23881,#11980,#11981);
#10477=AXIS2_PLACEMENT_3D('',#23885,#11984,#11985);
#10478=AXIS2_PLACEMENT_3D('',#23889,#11988,#11989);
#10479=AXIS2_PLACEMENT_3D('',#23891,#11991,#11992);
#10480=AXIS2_PLACEMENT_3D('',#23892,#11993,#11994);
#10481=AXIS2_PLACEMENT_3D('',#23893,#11995,#11996);
#10482=AXIS2_PLACEMENT_3D('',#23895,#11997,#11998);
#10483=AXIS2_PLACEMENT_3D('',#23898,#11999,#12000);
#10484=AXIS2_PLACEMENT_3D('',#30204,#12001,#12002);
#10485=AXIS2_PLACEMENT_3D('',#36248,#12003,#12004);
#10486=AXIS2_PLACEMENT_3D('',#36249,#12005,#12006);
#10487=AXIS2_PLACEMENT_3D('',#36759,#12007,#12008);
#10488=AXIS2_PLACEMENT_3D('',#54907,#12009,#12010);
#10489=AXIS2_PLACEMENT_3D('',#71754,#12011,#12012);
#10490=AXIS2_PLACEMENT_3D('',#71763,#12017,#12018);
#10491=AXIS2_PLACEMENT_3D('',#71769,#12022,#12023);
#10492=AXIS2_PLACEMENT_3D('',#71775,#12027,#12028);
#10493=AXIS2_PLACEMENT_3D('',#71781,#12032,#12033);
#10494=AXIS2_PLACEMENT_3D('',#71787,#12037,#12038);
#10495=AXIS2_PLACEMENT_3D('',#71790,#12041,#12042);
#10496=AXIS2_PLACEMENT_3D('',#71791,#12043,#12044);
#10497=AXIS2_PLACEMENT_3D('',#73815,#12045,#12046);
#10498=AXIS2_PLACEMENT_3D('',#75715,#12047,#12048);
#10499=AXIS2_PLACEMENT_3D('',#75717,#12049,#12050);
#10500=AXIS2_PLACEMENT_3D('',#75718,#12051,#12052);
#10501=AXIS2_PLACEMENT_3D('',#75720,#12054,#12055);
#10502=AXIS2_PLACEMENT_3D('',#75723,#12057,#12058);
#10503=AXIS2_PLACEMENT_3D('',#75724,#12059,#12060);
#10504=AXIS2_PLACEMENT_3D('',#75725,#12061,#12062);
#10505=AXIS2_PLACEMENT_3D('',#75726,#12063,#12064);
#10506=AXIS2_PLACEMENT_3D('',#75729,#12065,#12066);
#10507=AXIS2_PLACEMENT_3D('',#75733,#12068,#12069);
#10508=AXIS2_PLACEMENT_3D('',#75736,#12071,#12072);
#10509=AXIS2_PLACEMENT_3D('',#75737,#12073,#12074);
#10510=AXIS2_PLACEMENT_3D('',#75739,#12075,#12076);
#10511=AXIS2_PLACEMENT_3D('',#75741,#12078,#12079);
#10512=AXIS2_PLACEMENT_3D('',#75744,#12080,#12081);
#10513=AXIS2_PLACEMENT_3D('',#75746,#12082,#12083);
#10514=AXIS2_PLACEMENT_3D('',#75750,#12085,#12086);
#10515=AXIS2_PLACEMENT_3D('',#75752,#12088,#12089);
#10516=AXIS2_PLACEMENT_3D('',#75755,#12092,#12093);
#10517=AXIS2_PLACEMENT_3D('',#75758,#12094,#12095);
#10518=AXIS2_PLACEMENT_3D('',#75762,#12097,#12098);
#10519=AXIS2_PLACEMENT_3D('',#75765,#12100,#12101);
#10520=AXIS2_PLACEMENT_3D('',#75766,#12102,#12103);
#10521=AXIS2_PLACEMENT_3D('',#75768,#12104,#12105);
#10522=AXIS2_PLACEMENT_3D('',#75770,#12107,#12108);
#10523=AXIS2_PLACEMENT_3D('',#75773,#12109,#12110);
#10524=AXIS2_PLACEMENT_3D('',#75775,#12111,#12112);
#10525=AXIS2_PLACEMENT_3D('',#75779,#12114,#12115);
#10526=AXIS2_PLACEMENT_3D('',#75781,#12117,#12118);
#10527=AXIS2_PLACEMENT_3D('',#75792,#12125,#12126);
#10528=AXIS2_PLACEMENT_3D('',#75798,#12130,#12131);
#10529=AXIS2_PLACEMENT_3D('',#75802,#12134,#12135);
#10530=AXIS2_PLACEMENT_3D('',#75806,#12138,#12139);
#10531=AXIS2_PLACEMENT_3D('',#75808,#12141,#12142);
#10532=AXIS2_PLACEMENT_3D('',#75809,#12143,#12144);
#10533=AXIS2_PLACEMENT_3D('',#75811,#12145,#12146);
#10534=AXIS2_PLACEMENT_3D('',#75862,#12148,#12149);
#10535=AXIS2_PLACEMENT_3D('',#75911,#12151,#12152);
#10536=AXIS2_PLACEMENT_3D('',#75912,#12153,#12154);
#10537=AXIS2_PLACEMENT_3D('',#75914,#12155,#12156);
#10538=AXIS2_PLACEMENT_3D('',#75957,#12158,#12159);
#10539=AXIS2_PLACEMENT_3D('',#75998,#12161,#12162);
#10540=AXIS2_PLACEMENT_3D('',#75999,#12163,#12164);
#10541=AXIS2_PLACEMENT_3D('',#76001,#12165,#12166);
#10542=AXIS2_PLACEMENT_3D('',#76006,#12170,#12171);
#10543=AXIS2_PLACEMENT_3D('',#76007,#12172,#12173);
#10544=AXIS2_PLACEMENT_3D('',#76011,#12175,#12176);
#10545=AXIS2_PLACEMENT_3D('',#76012,#12177,#12178);
#10546=AXIS2_PLACEMENT_3D('',#76013,#12179,#12180);
#10547=AXIS2_PLACEMENT_3D('',#76014,#12181,#12182);
#10548=AXIS2_PLACEMENT_3D('',#76015,#12183,#12184);
#10549=AXIS2_PLACEMENT_3D('',#76018,#12186,#12187);
#10550=AXIS2_PLACEMENT_3D('',#76019,#12188,#12189);
#10551=AXIS2_PLACEMENT_3D('',#76020,#12190,#12191);
#10552=AXIS2_PLACEMENT_3D('',#76021,#12192,#12193);
#10553=AXIS2_PLACEMENT_3D('',#76023,#12194,#12195);
#10554=AXIS2_PLACEMENT_3D('',#76025,#12197,#12198);
#10555=AXIS2_PLACEMENT_3D('',#76026,#12199,#12200);
#10556=AXIS2_PLACEMENT_3D('',#76027,#12201,#12202);
#10557=AXIS2_PLACEMENT_3D('',#76028,#12203,#12204);
#10558=AXIS2_PLACEMENT_3D('',#76030,#12206,#12207);
#10559=AXIS2_PLACEMENT_3D('',#76032,#12209,#12210);
#10560=AXIS2_PLACEMENT_3D('',#76034,#12212,#12213);
#10561=AXIS2_PLACEMENT_3D('',#76036,#12215,#12216);
#10562=AXIS2_PLACEMENT_3D('',#76037,#12217,#12218);
#10563=AXIS2_PLACEMENT_3D('',#77326,#12219,#12220);
#10564=AXIS2_PLACEMENT_3D('',#77327,#12221,#12222);
#10565=AXIS2_PLACEMENT_3D('',#77328,#12223,#12224);
#10566=AXIS2_PLACEMENT_3D('',#77329,#12225,#12226);
#10567=AXIS2_PLACEMENT_3D('',#77331,#12227,#12228);
#10568=AXIS2_PLACEMENT_3D('',#77334,#12230,#12231);
#10569=AXIS2_PLACEMENT_3D('',#77335,#12232,#12233);
#10570=AXIS2_PLACEMENT_3D('',#77338,#12235,#12236);
#10571=AXIS2_PLACEMENT_3D('',#77339,#12237,#12238);
#10572=AXIS2_PLACEMENT_3D('',#77341,#12239,#12240);
#10573=AXIS2_PLACEMENT_3D('',#77342,#12241,#12242);
#10574=AXIS2_PLACEMENT_3D('',#77344,#12243,#12244);
#10575=AXIS2_PLACEMENT_3D('',#77346,#12246,#12247);
#10576=AXIS2_PLACEMENT_3D('',#77348,#12248,#12249);
#10577=AXIS2_PLACEMENT_3D('',#77349,#12250,#12251);
#10578=AXIS2_PLACEMENT_3D('',#77351,#12252,#12253);
#10579=AXIS2_PLACEMENT_3D('',#77353,#12255,#12256);
#10580=AXIS2_PLACEMENT_3D('',#77355,#12257,#12258);
#10581=AXIS2_PLACEMENT_3D('',#77356,#12259,#12260);
#10582=AXIS2_PLACEMENT_3D('',#77358,#12261,#12262);
#10583=AXIS2_PLACEMENT_3D('',#77360,#12264,#12265);
#10584=AXIS2_PLACEMENT_3D('',#77362,#12266,#12267);
#10585=AXIS2_PLACEMENT_3D('',#77364,#12269,#12270);
#10586=AXIS2_PLACEMENT_3D('',#77367,#12272,#12273);
#10587=AXIS2_PLACEMENT_3D('',#77368,#12274,#12275);
#10588=AXIS2_PLACEMENT_3D('',#77370,#12276,#12277);
#10589=AXIS2_PLACEMENT_3D('',#77371,#12278,#12279);
#10590=AXIS2_PLACEMENT_3D('',#77373,#12280,#12281);
#10591=AXIS2_PLACEMENT_3D('',#77375,#12283,#12284);
#10592=AXIS2_PLACEMENT_3D('',#77377,#12285,#12286);
#10593=AXIS2_PLACEMENT_3D('',#77378,#12287,#12288);
#10594=AXIS2_PLACEMENT_3D('',#77380,#12289,#12290);
#10595=AXIS2_PLACEMENT_3D('',#77382,#12292,#12293);
#10596=AXIS2_PLACEMENT_3D('',#77384,#12294,#12295);
#10597=AXIS2_PLACEMENT_3D('',#77385,#12296,#12297);
#10598=AXIS2_PLACEMENT_3D('',#77387,#12299,#12300);
#10599=AXIS2_PLACEMENT_3D('',#77388,#12301,#12302);
#10600=AXIS2_PLACEMENT_3D('',#77401,#12307,#12308);
#10601=AXIS2_PLACEMENT_3D('',#77414,#12313,#12314);
#10602=AXIS2_PLACEMENT_3D('',#77417,#12317,#12318);
#10603=AXIS2_PLACEMENT_3D('',#77418,#12319,#12320);
#10604=AXIS2_PLACEMENT_3D('',#77419,#12321,#12322);
#10605=AXIS2_PLACEMENT_3D('',#77421,#12323,#12324);
#10606=AXIS2_PLACEMENT_3D('',#77429,#12328,#12329);
#10607=AXIS2_PLACEMENT_3D('',#77437,#12333,#12334);
#10608=AXIS2_PLACEMENT_3D('',#77445,#12338,#12339);
#10609=AXIS2_PLACEMENT_3D('',#77453,#12343,#12344);
#10610=AXIS2_PLACEMENT_3D('',#77461,#12348,#12349);
#10611=AXIS2_PLACEMENT_3D('',#77469,#12353,#12354);
#10612=AXIS2_PLACEMENT_3D('',#77476,#12358,#12359);
#10613=AXIS2_PLACEMENT_3D('',#77478,#12360,#12361);
#10614=AXIS2_PLACEMENT_3D('',#77479,#12362,#12363);
#10615=AXIS2_PLACEMENT_3D('',#77481,#12364,#12365);
#10616=AXIS2_PLACEMENT_3D('',#77485,#12366,#12367);
#10617=AXIS2_PLACEMENT_3D('',#77490,#12368,#12369);
#10618=AXIS2_PLACEMENT_3D('',#77491,#12370,#12371);
#10619=AXIS2_PLACEMENT_3D('',#77501,#12375,#12376);
#10620=AXIS2_PLACEMENT_3D('',#77507,#12380,#12381);
#10621=AXIS2_PLACEMENT_3D('',#77509,#12383,#12384);
#10622=AXIS2_PLACEMENT_3D('',#77510,#12385,#12386);
#10623=AXIS2_PLACEMENT_3D('',#77511,#12387,#12388);
#10624=AXIS2_PLACEMENT_3D('',#77516,#12389,#12390);
#10625=AXIS2_PLACEMENT_3D('',#77517,#12391,#12392);
#10626=AXIS2_PLACEMENT_3D('',#77527,#12396,#12397);
#10627=AXIS2_PLACEMENT_3D('',#77533,#12401,#12402);
#10628=AXIS2_PLACEMENT_3D('',#77535,#12404,#12405);
#10629=AXIS2_PLACEMENT_3D('',#77536,#12406,#12407);
#10630=AXIS2_PLACEMENT_3D('',#77537,#12408,#12409);
#10631=AXIS2_PLACEMENT_3D('',#77542,#12410,#12411);
#10632=AXIS2_PLACEMENT_3D('',#77543,#12412,#12413);
#10633=AXIS2_PLACEMENT_3D('',#77553,#12417,#12418);
#10634=AXIS2_PLACEMENT_3D('',#77559,#12422,#12423);
#10635=AXIS2_PLACEMENT_3D('',#77561,#12425,#12426);
#10636=AXIS2_PLACEMENT_3D('',#77563,#12427,#12428);
#10637=AXIS2_PLACEMENT_3D('',#77564,#12429,#12430);
#10638=AXIS2_PLACEMENT_3D('',#77565,#12431,#12432);
#10639=AXIS2_PLACEMENT_3D('',#77570,#12433,#12434);
#10640=AXIS2_PLACEMENT_3D('',#77571,#12435,#12436);
#10641=AXIS2_PLACEMENT_3D('',#77581,#12440,#12441);
#10642=AXIS2_PLACEMENT_3D('',#77587,#12445,#12446);
#10643=AXIS2_PLACEMENT_3D('',#77589,#12448,#12449);
#10644=AXIS2_PLACEMENT_3D('',#77590,#12450,#12451);
#10645=AXIS2_PLACEMENT_3D('',#77591,#12452,#12453);
#10646=AXIS2_PLACEMENT_3D('',#77596,#12454,#12455);
#10647=AXIS2_PLACEMENT_3D('',#77597,#12456,#12457);
#10648=AXIS2_PLACEMENT_3D('',#77607,#12461,#12462);
#10649=AXIS2_PLACEMENT_3D('',#77613,#12466,#12467);
#10650=AXIS2_PLACEMENT_3D('',#77615,#12469,#12470);
#10651=AXIS2_PLACEMENT_3D('',#77616,#12471,#12472);
#10652=AXIS2_PLACEMENT_3D('',#77617,#12473,#12474);
#10653=AXIS2_PLACEMENT_3D('',#77622,#12475,#12476);
#10654=AXIS2_PLACEMENT_3D('',#77623,#12477,#12478);
#10655=AXIS2_PLACEMENT_3D('',#77629,#12482,#12483);
#10656=AXIS2_PLACEMENT_3D('',#77639,#12487,#12488);
#10657=AXIS2_PLACEMENT_3D('',#77641,#12490,#12491);
#10658=AXIS2_PLACEMENT_3D('',#77642,#12492,#12493);
#10659=AXIS2_PLACEMENT_3D('',#77643,#12494,#12495);
#10660=AXIS2_PLACEMENT_3D('',#77648,#12496,#12497);
#10661=AXIS2_PLACEMENT_3D('',#77649,#12498,#12499);
#10662=AXIS2_PLACEMENT_3D('',#77655,#12503,#12504);
#10663=AXIS2_PLACEMENT_3D('',#77661,#12508,#12509);
#10664=AXIS2_PLACEMENT_3D('',#77663,#12511,#12512);
#10665=AXIS2_PLACEMENT_3D('',#77664,#12513,#12514);
#10666=AXIS2_PLACEMENT_3D('',#77665,#12515,#12516);
#10667=AXIS2_PLACEMENT_3D('',#77667,#12517,#12518);
#10668=AXIS2_PLACEMENT_3D('',#77670,#12520,#12521);
#10669=AXIS2_PLACEMENT_3D('',#77671,#12522,#12523);
#10670=AXIS2_PLACEMENT_3D('',#77673,#12524,#12525);
#10671=AXIS2_PLACEMENT_3D('',#77674,#12526,#12527);
#10672=AXIS2_PLACEMENT_3D('',#77677,#12529,#12530);
#10673=AXIS2_PLACEMENT_3D('',#77678,#12531,#12532);
#10674=AXIS2_PLACEMENT_3D('',#77680,#12533,#12534);
#10675=AXIS2_PLACEMENT_3D('',#77681,#12535,#12536);
#10676=AXIS2_PLACEMENT_3D('',#77683,#12538,#12539);
#10677=AXIS2_PLACEMENT_3D('',#77685,#12540,#12541);
#10678=AXIS2_PLACEMENT_3D('',#77687,#12543,#12544);
#10679=AXIS2_PLACEMENT_3D('',#77688,#12545,#12546);
#10680=AXIS2_PLACEMENT_3D('',#77689,#12547,#12548);
#10681=AXIS2_PLACEMENT_3D('',#77698,#12553,#12554);
#10682=AXIS2_PLACEMENT_3D('',#77707,#12559,#12560);
#10683=AXIS2_PLACEMENT_3D('',#77710,#12563,#12564);
#10684=AXIS2_PLACEMENT_3D('',#77711,#12565,#12566);
#10685=AXIS2_PLACEMENT_3D('',#77713,#12567,#12568);
#10686=AXIS2_PLACEMENT_3D('',#77714,#12569,#12570);
#10687=AXIS2_PLACEMENT_3D('',#77716,#12571,#12572);
#10688=AXIS2_PLACEMENT_3D('',#77718,#12574,#12575);
#10689=AXIS2_PLACEMENT_3D('',#77719,#12576,#12577);
#10690=AXIS2_PLACEMENT_3D('',#77720,#12578,#12579);
#10691=AXIS2_PLACEMENT_3D('',#77721,#12580,#12581);
#10692=AXIS2_PLACEMENT_3D('',#77722,#12582,#12583);
#10693=AXIS2_PLACEMENT_3D('',#77724,#12584,#12585);
#10694=AXIS2_PLACEMENT_3D('',#77727,#12587,#12588);
#10695=AXIS2_PLACEMENT_3D('',#77728,#12589,#12590);
#10696=AXIS2_PLACEMENT_3D('',#77731,#12592,#12593);
#10697=AXIS2_PLACEMENT_3D('',#77732,#12594,#12595);
#10698=AXIS2_PLACEMENT_3D('',#77734,#12596,#12597);
#10699=AXIS2_PLACEMENT_3D('',#77735,#12598,#12599);
#10700=AXIS2_PLACEMENT_3D('',#77737,#12600,#12601);
#10701=AXIS2_PLACEMENT_3D('',#77739,#12603,#12604);
#10702=AXIS2_PLACEMENT_3D('',#77741,#12605,#12606);
#10703=AXIS2_PLACEMENT_3D('',#77742,#12607,#12608);
#10704=AXIS2_PLACEMENT_3D('',#77744,#12609,#12610);
#10705=AXIS2_PLACEMENT_3D('',#77746,#12612,#12613);
#10706=AXIS2_PLACEMENT_3D('',#77748,#12614,#12615);
#10707=AXIS2_PLACEMENT_3D('',#77749,#12616,#12617);
#10708=AXIS2_PLACEMENT_3D('',#77751,#12618,#12619);
#10709=AXIS2_PLACEMENT_3D('',#77753,#12621,#12622);
#10710=AXIS2_PLACEMENT_3D('',#77755,#12623,#12624);
#10711=AXIS2_PLACEMENT_3D('',#77757,#12626,#12627);
#10712=AXIS2_PLACEMENT_3D('',#77760,#12629,#12630);
#10713=AXIS2_PLACEMENT_3D('',#77761,#12631,#12632);
#10714=AXIS2_PLACEMENT_3D('',#77763,#12633,#12634);
#10715=AXIS2_PLACEMENT_3D('',#77764,#12635,#12636);
#10716=AXIS2_PLACEMENT_3D('',#77766,#12637,#12638);
#10717=AXIS2_PLACEMENT_3D('',#77768,#12640,#12641);
#10718=AXIS2_PLACEMENT_3D('',#77770,#12642,#12643);
#10719=AXIS2_PLACEMENT_3D('',#77771,#12644,#12645);
#10720=AXIS2_PLACEMENT_3D('',#77773,#12646,#12647);
#10721=AXIS2_PLACEMENT_3D('',#77775,#12649,#12650);
#10722=AXIS2_PLACEMENT_3D('',#77777,#12651,#12652);
#10723=AXIS2_PLACEMENT_3D('',#77778,#12653,#12654);
#10724=AXIS2_PLACEMENT_3D('',#77780,#12656,#12657);
#10725=AXIS2_PLACEMENT_3D('',#77781,#12658,#12659);
#10726=AXIS2_PLACEMENT_3D('',#77783,#12660,#12661);
#10727=AXIS2_PLACEMENT_3D('',#77786,#12663,#12664);
#10728=AXIS2_PLACEMENT_3D('',#77787,#12665,#12666);
#10729=AXIS2_PLACEMENT_3D('',#77790,#12668,#12669);
#10730=AXIS2_PLACEMENT_3D('',#77791,#12670,#12671);
#10731=AXIS2_PLACEMENT_3D('',#77793,#12672,#12673);
#10732=AXIS2_PLACEMENT_3D('',#77794,#12674,#12675);
#10733=AXIS2_PLACEMENT_3D('',#77796,#12676,#12677);
#10734=AXIS2_PLACEMENT_3D('',#77798,#12679,#12680);
#10735=AXIS2_PLACEMENT_3D('',#77800,#12681,#12682);
#10736=AXIS2_PLACEMENT_3D('',#77802,#12684,#12685);
#10737=AXIS2_PLACEMENT_3D('',#77805,#12687,#12688);
#10738=AXIS2_PLACEMENT_3D('',#77806,#12689,#12690);
#10739=AXIS2_PLACEMENT_3D('',#77808,#12691,#12692);
#10740=AXIS2_PLACEMENT_3D('',#77809,#12693,#12694);
#10741=AXIS2_PLACEMENT_3D('',#77811,#12696,#12697);
#10742=AXIS2_PLACEMENT_3D('',#77812,#12698,#12699);
#10743=AXIS2_PLACEMENT_3D('',#77814,#12700,#12701);
#10744=AXIS2_PLACEMENT_3D('',#77815,#12702,#12703);
#10745=AXIS2_PLACEMENT_3D('',#77817,#12704,#12705);
#10746=AXIS2_PLACEMENT_3D('',#77819,#12707,#12708);
#10747=AXIS2_PLACEMENT_3D('',#77821,#12709,#12710);
#10748=AXIS2_PLACEMENT_3D('',#77823,#12712,#12713);
#10749=AXIS2_PLACEMENT_3D('',#77825,#12714,#12715);
#10750=AXIS2_PLACEMENT_3D('',#77826,#12716,#12717);
#10751=AXIS2_PLACEMENT_3D('',#77828,#12718,#12719);
#10752=AXIS2_PLACEMENT_3D('',#77830,#12721,#12722);
#10753=AXIS2_PLACEMENT_3D('',#77832,#12723,#12724);
#10754=AXIS2_PLACEMENT_3D('',#77833,#12725,#12726);
#10755=AXIS2_PLACEMENT_3D('',#77835,#12727,#12728);
#10756=AXIS2_PLACEMENT_3D('',#77837,#12730,#12731);
#10757=AXIS2_PLACEMENT_3D('',#77840,#12733,#12734);
#10758=AXIS2_PLACEMENT_3D('',#77841,#12735,#12736);
#10759=AXIS2_PLACEMENT_3D('',#77842,#12737,#12738);
#10760=AXIS2_PLACEMENT_3D('',#77843,#12739,#12740);
#10761=AXIS2_PLACEMENT_3D('',#77845,#12741,#12742);
#10762=AXIS2_PLACEMENT_3D('',#77846,#12743,#12744);
#10763=AXIS2_PLACEMENT_3D('',#77848,#12745,#12746);
#10764=AXIS2_PLACEMENT_3D('',#77850,#12748,#12749);
#10765=AXIS2_PLACEMENT_3D('',#77852,#12750,#12751);
#10766=AXIS2_PLACEMENT_3D('',#77854,#12753,#12754);
#10767=AXIS2_PLACEMENT_3D('',#77856,#12755,#12756);
#10768=AXIS2_PLACEMENT_3D('',#77857,#12757,#12758);
#10769=AXIS2_PLACEMENT_3D('',#77859,#12759,#12760);
#10770=AXIS2_PLACEMENT_3D('',#77861,#12762,#12763);
#10771=AXIS2_PLACEMENT_3D('',#77863,#12764,#12765);
#10772=AXIS2_PLACEMENT_3D('',#77864,#12766,#12767);
#10773=AXIS2_PLACEMENT_3D('',#77866,#12768,#12769);
#10774=AXIS2_PLACEMENT_3D('',#77868,#12771,#12772);
#10775=AXIS2_PLACEMENT_3D('',#77871,#12774,#12775);
#10776=AXIS2_PLACEMENT_3D('',#77872,#12776,#12777);
#10777=AXIS2_PLACEMENT_3D('',#77873,#12778,#12779);
#10778=AXIS2_PLACEMENT_3D('',#77874,#12780,#12781);
#10779=AXIS2_PLACEMENT_3D('',#77876,#12782,#12783);
#10780=AXIS2_PLACEMENT_3D('',#77878,#12784,#12785);
#10781=AXIS2_PLACEMENT_3D('',#77879,#12786,#12787);
#10782=AXIS2_PLACEMENT_3D('',#77880,#12788,#12789);
#10783=AXIS2_PLACEMENT_3D('',#77883,#12791,#12792);
#10784=AXIS2_PLACEMENT_3D('',#77884,#12793,#12794);
#10785=AXIS2_PLACEMENT_3D('',#77885,#12795,#12796);
#10786=AXIS2_PLACEMENT_3D('',#77887,#12797,#12798);
#10787=AXIS2_PLACEMENT_3D('',#77888,#12799,#12800);
#10788=AXIS2_PLACEMENT_3D('',#77890,#12802,#12803);
#10789=AXIS2_PLACEMENT_3D('',#77891,#12804,#12805);
#10790=AXIS2_PLACEMENT_3D('',#77946,#12807,#12808);
#10791=AXIS2_PLACEMENT_3D('',#77975,#12809,#12810);
#10792=AXIS2_PLACEMENT_3D('',#78243,#12812,#12813);
#10793=AXIS2_PLACEMENT_3D('',#78536,#12815,#12816);
#10794=AXIS2_PLACEMENT_3D('',#78858,#12818,#12819);
#10795=AXIS2_PLACEMENT_3D('',#79155,#12821,#12822);
#10796=AXIS2_PLACEMENT_3D('',#79478,#12824,#12825);
#10797=AXIS2_PLACEMENT_3D('',#79783,#12827,#12828);
#10798=AXIS2_PLACEMENT_3D('',#80090,#12830,#12831);
#10799=AXIS2_PLACEMENT_3D('',#80391,#12833,#12834);
#10800=AXIS2_PLACEMENT_3D('',#80718,#12836,#12837);
#10801=AXIS2_PLACEMENT_3D('',#81013,#12839,#12840);
#10802=AXIS2_PLACEMENT_3D('',#81329,#12842,#12843);
#10803=AXIS2_PLACEMENT_3D('',#81631,#12845,#12846);
#10804=AXIS2_PLACEMENT_3D('',#81860,#12848,#12849);
#10805=AXIS2_PLACEMENT_3D('',#81870,#12850,#12851);
#10806=AXIS2_PLACEMENT_3D('',#82973,#12852,#12853);
#10807=AXIS2_PLACEMENT_3D('',#84375,#12854,#12855);
#10808=AXIS2_PLACEMENT_3D('',#84414,#12856,#12857);
#10809=AXIS2_PLACEMENT_3D('',#84952,#12858,#12859);
#10810=AXIS2_PLACEMENT_3D('',#84954,#12860,#12861);
#10811=AXIS2_PLACEMENT_3D('',#84956,#12862,#12863);
#10812=AXIS2_PLACEMENT_3D('',#85440,#12864,#12865);
#10813=AXIS2_PLACEMENT_3D('',#85446,#12866,#12867);
#10814=AXIS2_PLACEMENT_3D('',#85447,#12868,#12869);
#10815=AXIS2_PLACEMENT_3D('',#85453,#12870,#12871);
#10816=AXIS2_PLACEMENT_3D('',#85454,#12872,#12873);
#10817=AXIS2_PLACEMENT_3D('',#85460,#12874,#12875);
#10818=AXIS2_PLACEMENT_3D('',#85461,#12876,#12877);
#10819=AXIS2_PLACEMENT_3D('',#85467,#12878,#12879);
#10820=AXIS2_PLACEMENT_3D('',#85468,#12880,#12881);
#10821=AXIS2_PLACEMENT_3D('',#85475,#12882,#12883);
#10822=AXIS2_PLACEMENT_3D('',#85476,#12884,#12885);
#10823=AXIS2_PLACEMENT_3D('',#85477,#12886,#12887);
#10824=AXIS2_PLACEMENT_3D('',#85483,#12888,#12889);
#10825=AXIS2_PLACEMENT_3D('',#85484,#12890,#12891);
#10826=AXIS2_PLACEMENT_3D('',#85486,#12892,#12893);
#10827=AXIS2_PLACEMENT_3D('',#85487,#12894,#12895);
#10828=AXIS2_PLACEMENT_3D('',#85489,#12896,#12897);
#10829=AXIS2_PLACEMENT_3D('',#85490,#12898,#12899);
#10830=AXIS2_PLACEMENT_3D('',#85492,#12900,#12901);
#10831=AXIS2_PLACEMENT_3D('',#85493,#12902,#12903);
#10832=AXIS2_PLACEMENT_3D('',#85495,#12904,#12905);
#10833=AXIS2_PLACEMENT_3D('',#85496,#12906,#12907);
#10834=AXIS2_PLACEMENT_3D('',#85498,#12908,#12909);
#10835=AXIS2_PLACEMENT_3D('',#85499,#12910,#12911);
#10836=AXIS2_PLACEMENT_3D('',#85501,#12912,#12913);
#10837=AXIS2_PLACEMENT_3D('',#85502,#12914,#12915);
#10838=AXIS2_PLACEMENT_3D('',#85504,#12916,#12917);
#10839=AXIS2_PLACEMENT_3D('',#85505,#12918,#12919);
#10840=AXIS2_PLACEMENT_3D('',#85506,#12920,#12921);
#10841=AXIS2_PLACEMENT_3D('',#85510,#12923,#12924);
#10842=AXIS2_PLACEMENT_3D('',#85511,#12925,#12926);
#10843=AXIS2_PLACEMENT_3D('',#85517,#12930,#12931);
#10844=AXIS2_PLACEMENT_3D('',#85521,#12934,#12935);
#10845=AXIS2_PLACEMENT_3D('',#85525,#12938,#12939);
#10846=AXIS2_PLACEMENT_3D('',#85529,#12942,#12943);
#10847=AXIS2_PLACEMENT_3D('',#85533,#12946,#12947);
#10848=AXIS2_PLACEMENT_3D('',#85535,#12949,#12950);
#10849=AXIS2_PLACEMENT_3D('',#85536,#12951,#12952);
#10850=AXIS2_PLACEMENT_3D('',#85538,#12953,#12954);
#10851=AXIS2_PLACEMENT_3D('',#85539,#12955,#12956);
#10852=AXIS2_PLACEMENT_3D('',#85541,#12958,#12959);
#10853=AXIS2_PLACEMENT_3D('',#85543,#12960,#12961);
#10854=AXIS2_PLACEMENT_3D('',#85544,#12962,#12963);
#10855=AXIS2_PLACEMENT_3D('',#85546,#12965,#12966);
#10856=AXIS2_PLACEMENT_3D('',#85547,#12967,#12968);
#10857=AXIS2_PLACEMENT_3D('',#85556,#12973,#12974);
#10858=AXIS2_PLACEMENT_3D('',#85565,#12979,#12980);
#10859=AXIS2_PLACEMENT_3D('',#85574,#12985,#12986);
#10860=AXIS2_PLACEMENT_3D('',#85583,#12991,#12992);
#10861=AXIS2_PLACEMENT_3D('',#85585,#12993,#12994);
#10862=AXIS2_PLACEMENT_3D('',#85588,#12996,#12997);
#10863=AXIS2_PLACEMENT_3D('',#85589,#12998,#12999);
#10864=AXIS2_PLACEMENT_3D('',#85591,#13000,#13001);
#10865=AXIS2_PLACEMENT_3D('',#85594,#13003,#13004);
#10866=AXIS2_PLACEMENT_3D('',#85595,#13005,#13006);
#10867=AXIS2_PLACEMENT_3D('',#85597,#13007,#13008);
#10868=AXIS2_PLACEMENT_3D('',#85600,#13010,#13011);
#10869=AXIS2_PLACEMENT_3D('',#85601,#13012,#13013);
#10870=AXIS2_PLACEMENT_3D('',#85603,#13014,#13015);
#10871=AXIS2_PLACEMENT_3D('',#85606,#13017,#13018);
#10872=AXIS2_PLACEMENT_3D('',#85607,#13019,#13020);
#10873=AXIS2_PLACEMENT_3D('',#85608,#13021,#13022);
#10874=AXIS2_PLACEMENT_3D('',#85609,#13023,#13024);
#10875=AXIS2_PLACEMENT_3D('',#85610,#13025,#13026);
#10876=AXIS2_PLACEMENT_3D('',#85612,#13027,#13028);
#10877=AXIS2_PLACEMENT_3D('',#85614,#13029,#13030);
#10878=AXIS2_PLACEMENT_3D('',#85615,#13031,#13032);
#10879=AXIS2_PLACEMENT_3D('',#85616,#13033,#13034);
#10880=AXIS2_PLACEMENT_3D('',#85617,#13035,#13036);
#10881=AXIS2_PLACEMENT_3D('',#85618,#13037,#13038);
#10882=AXIS2_PLACEMENT_3D('',#85619,#13039,#13040);
#10883=AXIS2_PLACEMENT_3D('',#85620,#13041,#13042);
#10884=AXIS2_PLACEMENT_3D('',#85622,#13043,#13044);
#10885=AXIS2_PLACEMENT_3D('',#85624,#13046,#13047);
#10886=AXIS2_PLACEMENT_3D('',#85626,#13048,#13049);
#10887=AXIS2_PLACEMENT_3D('',#85628,#13051,#13052);
#10888=AXIS2_PLACEMENT_3D('',#85629,#13053,#13054);
#10889=AXIS2_PLACEMENT_3D('',#85630,#13055,#13056);
#10890=AXIS2_PLACEMENT_3D('',#85631,#13057,#13058);
#10891=AXIS2_PLACEMENT_3D('',#85632,#13059,#13060);
#10892=AXIS2_PLACEMENT_3D('',#85633,#13061,#13062);
#10893=AXIS2_PLACEMENT_3D('',#85634,#13063,#13064);
#10894=AXIS2_PLACEMENT_3D('',#85643,#13069,#13070);
#10895=AXIS2_PLACEMENT_3D('',#85652,#13075,#13076);
#10896=AXIS2_PLACEMENT_3D('',#85661,#13081,#13082);
#10897=AXIS2_PLACEMENT_3D('',#85670,#13087,#13088);
#10898=AXIS2_PLACEMENT_3D('',#85672,#13089,#13090);
#10899=AXIS2_PLACEMENT_3D('',#85675,#13092,#13093);
#10900=AXIS2_PLACEMENT_3D('',#85676,#13094,#13095);
#10901=AXIS2_PLACEMENT_3D('',#85678,#13096,#13097);
#10902=AXIS2_PLACEMENT_3D('',#85681,#13099,#13100);
#10903=AXIS2_PLACEMENT_3D('',#85682,#13101,#13102);
#10904=AXIS2_PLACEMENT_3D('',#85684,#13103,#13104);
#10905=AXIS2_PLACEMENT_3D('',#85687,#13106,#13107);
#10906=AXIS2_PLACEMENT_3D('',#85688,#13108,#13109);
#10907=AXIS2_PLACEMENT_3D('',#85690,#13110,#13111);
#10908=AXIS2_PLACEMENT_3D('',#85693,#13113,#13114);
#10909=AXIS2_PLACEMENT_3D('',#85694,#13115,#13116);
#10910=AXIS2_PLACEMENT_3D('',#85695,#13117,#13118);
#10911=AXIS2_PLACEMENT_3D('',#85696,#13119,#13120);
#10912=AXIS2_PLACEMENT_3D('',#85697,#13121,#13122);
#10913=AXIS2_PLACEMENT_3D('',#85699,#13123,#13124);
#10914=AXIS2_PLACEMENT_3D('',#85701,#13125,#13126);
#10915=AXIS2_PLACEMENT_3D('',#85702,#13127,#13128);
#10916=AXIS2_PLACEMENT_3D('',#85703,#13129,#13130);
#10917=AXIS2_PLACEMENT_3D('',#85704,#13131,#13132);
#10918=AXIS2_PLACEMENT_3D('',#85705,#13133,#13134);
#10919=AXIS2_PLACEMENT_3D('',#85706,#13135,#13136);
#10920=AXIS2_PLACEMENT_3D('',#85707,#13137,#13138);
#10921=AXIS2_PLACEMENT_3D('',#85709,#13139,#13140);
#10922=AXIS2_PLACEMENT_3D('',#85711,#13142,#13143);
#10923=AXIS2_PLACEMENT_3D('',#85713,#13144,#13145);
#10924=AXIS2_PLACEMENT_3D('',#85715,#13147,#13148);
#10925=AXIS2_PLACEMENT_3D('',#85716,#13149,#13150);
#10926=AXIS2_PLACEMENT_3D('',#85717,#13151,#13152);
#10927=AXIS2_PLACEMENT_3D('',#85718,#13153,#13154);
#10928=AXIS2_PLACEMENT_3D('',#85719,#13155,#13156);
#10929=AXIS2_PLACEMENT_3D('',#85720,#13157,#13158);
#10930=AXIS2_PLACEMENT_3D('',#85721,#13159,#13160);
#10931=AXIS2_PLACEMENT_3D('',#85722,#13161,#13162);
#10932=AXIS2_PLACEMENT_3D('',#85723,#13163,#13164);
#10933=AXIS2_PLACEMENT_3D('',#85724,#13165,#13166);
#10934=AXIS2_PLACEMENT_3D('',#85725,#13167,#13168);
#10935=AXIS2_PLACEMENT_3D('',#85726,#13169,#13170);
#10936=AXIS2_PLACEMENT_3D('',#85727,#13171,#13172);
#10937=AXIS2_PLACEMENT_3D('',#85728,#13173,#13174);
#10938=AXIS2_PLACEMENT_3D('',#85729,#13175,#13176);
#10939=AXIS2_PLACEMENT_3D('',#85730,#13177,#13178);
#10940=AXIS2_PLACEMENT_3D('',#85731,#13179,#13180);
#10941=AXIS2_PLACEMENT_3D('',#85732,#13181,#13182);
#10942=AXIS2_PLACEMENT_3D('',#85733,#13183,#13184);
#10943=AXIS2_PLACEMENT_3D('',#85734,#13185,#13186);
#10944=AXIS2_PLACEMENT_3D('',#85735,#13187,#13188);
#10945=AXIS2_PLACEMENT_3D('',#85736,#13189,#13190);
#10946=AXIS2_PLACEMENT_3D('',#85737,#13191,#13192);
#10947=AXIS2_PLACEMENT_3D('',#85738,#13193,#13194);
#10948=AXIS2_PLACEMENT_3D('',#85739,#13195,#13196);
#10949=AXIS2_PLACEMENT_3D('',#85740,#13197,#13198);
#10950=AXIS2_PLACEMENT_3D('',#85741,#13199,#13200);
#10951=AXIS2_PLACEMENT_3D('',#85742,#13201,#13202);
#10952=AXIS2_PLACEMENT_3D('',#85743,#13203,#13204);
#10953=AXIS2_PLACEMENT_3D('',#85744,#13205,#13206);
#10954=AXIS2_PLACEMENT_3D('',#85745,#13207,#13208);
#10955=AXIS2_PLACEMENT_3D('',#85746,#13209,#13210);
#10956=AXIS2_PLACEMENT_3D('',#85747,#13211,#13212);
#10957=AXIS2_PLACEMENT_3D('',#85748,#13213,#13214);
#10958=AXIS2_PLACEMENT_3D('',#85749,#13215,#13216);
#10959=DIRECTION('axis',(0.,0.,1.));
#10960=DIRECTION('refdir',(1.,0.,0.));
#10961=DIRECTION('axis',(0.,0.,1.));
#10962=DIRECTION('refdir',(1.,0.,0.));
#10963=DIRECTION('center_axis',(0.258819045102521,-0.965925826289068,0.));
#10964=DIRECTION('ref_axis',(0.,0.,-1.));
#10965=DIRECTION('center_axis',(-0.258819045102521,0.965925826289068,0.));
#10966=DIRECTION('ref_axis',(0.965925826289068,0.258819045102521,0.));
#10967=DIRECTION('center_axis',(-0.965925826289068,-0.258819045102521,0.));
#10968=DIRECTION('ref_axis',(0.,0.,1.));
#10969=DIRECTION('center_axis',(0.258819045102521,-0.965925826289068,0.));
#10970=DIRECTION('ref_axis',(0.965925826289068,0.258819045102521,0.));
#10971=DIRECTION('center_axis',(-0.258819045102521,0.965925826289068,0.));
#10972=DIRECTION('ref_axis',(0.965925826289068,0.258819045102521,0.));
#10973=DIRECTION('center_axis',(-0.258819045102521,0.965925826289068,0.));
#10974=DIRECTION('ref_axis',(0.965925826289068,0.258819045102521,0.));
#10975=DIRECTION('',(-0.258819045102521,0.965925826289068,0.));
#10976=DIRECTION('center_axis',(0.258819045102521,-0.965925826289068,0.));
#10977=DIRECTION('ref_axis',(0.965925826289068,0.258819045102521,0.));
#10978=DIRECTION('center_axis',(0.258819045102521,-0.965925826289068,0.));
#10979=DIRECTION('ref_axis',(0.965925826289068,0.258819045102521,0.));
#10980=DIRECTION('center_axis',(-0.258819045102521,0.965925826289068,0.));
#10981=DIRECTION('ref_axis',(0.965925826289068,0.258819045102521,0.));
#10982=DIRECTION('',(0.,0.,1.));
#10983=DIRECTION('',(0.,0.,1.));
#10984=DIRECTION('',(0.,0.,1.));
#10985=DIRECTION('center_axis',(0.258819045102337,-0.965925826289118,-1.46071306349284E-13));
#10986=DIRECTION('ref_axis',(0.177402769042635,0.0475349287001315,-0.982989668353375));
#10987=DIRECTION('center_axis',(0.258819045102521,-0.965925826289068,0.));
#10988=DIRECTION('ref_axis',(0.,0.,-1.));
#10989=DIRECTION('center_axis',(-0.258819045102521,0.965925826289068,0.));
#10990=DIRECTION('ref_axis',(0.965925826289068,0.258819045102521,0.));
#10991=DIRECTION('center_axis',(-0.965925826289068,-0.258819045102521,0.));
#10992=DIRECTION('ref_axis',(0.,0.,1.));
#10993=DIRECTION('center_axis',(-0.258819045102521,0.965925826289068,0.));
#10994=DIRECTION('ref_axis',(0.965925826289068,0.258819045102521,0.));
#10995=DIRECTION('',(0.,0.,-1.));
#10996=DIRECTION('center_axis',(-0.258819045102521,-0.965925826289068,0.));
#10997=DIRECTION('ref_axis',(0.,0.,-1.));
#10998=DIRECTION('center_axis',(0.258819045102521,0.965925826289068,0.));
#10999=DIRECTION('ref_axis',(0.965925826289068,-0.258819045102521,0.));
#11000=DIRECTION('center_axis',(-0.965925826289068,0.258819045102521,0.));
#11001=DIRECTION('ref_axis',(0.,0.,1.));
#11002=DIRECTION('center_axis',(-0.258819045102521,-0.965925826289068,0.));
#11003=DIRECTION('ref_axis',(0.965925826289068,-0.258819045102521,0.));
#11004=DIRECTION('center_axis',(0.258819045102521,0.965925826289068,0.));
#11005=DIRECTION('ref_axis',(0.965925826289068,-0.258819045102521,0.));
#11006=DIRECTION('center_axis',(0.258819045102521,0.965925826289068,0.));
#11007=DIRECTION('ref_axis',(0.965925826289068,-0.258819045102521,0.));
#11008=DIRECTION('',(0.258819045102521,0.965925826289068,0.));
#11009=DIRECTION('center_axis',(-0.258819045102521,-0.965925826289068,0.));
#11010=DIRECTION('ref_axis',(0.965925826289068,-0.258819045102521,0.));
#11011=DIRECTION('center_axis',(-0.258819045102521,-0.965925826289068,0.));
#11012=DIRECTION('ref_axis',(0.965925826289068,-0.258819045102521,0.));
#11013=DIRECTION('center_axis',(0.258819045102521,0.965925826289068,0.));
#11014=DIRECTION('ref_axis',(0.965925826289068,-0.258819045102521,0.));
#11015=DIRECTION('',(0.,0.,-1.));
#11016=DIRECTION('',(0.,0.,1.));
#11017=DIRECTION('center_axis',(-0.258819045102521,-0.965925826289068,0.));
#11018=DIRECTION('ref_axis',(0.,0.,-1.));
#11019=DIRECTION('center_axis',(0.258819045102521,0.965925826289068,0.));
#11020=DIRECTION('ref_axis',(0.965925826289068,-0.258819045102521,0.));
#11021=DIRECTION('center_axis',(-0.965925826289068,0.258819045102521,0.));
#11022=DIRECTION('ref_axis',(0.,0.,1.));
#11023=DIRECTION('center_axis',(0.258819045102521,0.965925826289068,0.));
#11024=DIRECTION('ref_axis',(0.965925826289068,-0.258819045102521,0.));
#11025=DIRECTION('',(0.,0.,-1.));
#11026=DIRECTION('',(-0.258819045102558,-0.965925826289058,0.));
#11027=DIRECTION('center_axis',(0.258819045102522,0.965925826289068,-8.7140221628902E-16));
#11028=DIRECTION('ref_axis',(0.965925826289068,-0.258819045102522,-5.55111512312583E-15));
#11029=DIRECTION('',(0.258819045102527,0.965925826289067,0.));
#11030=DIRECTION('center_axis',(0.,0.,1.));
#11031=DIRECTION('ref_axis',(0.500000000000001,-0.866025403784438,0.));
#11032=DIRECTION('center_axis',(0.,0.,1.));
#11033=DIRECTION('ref_axis',(-0.258819045102521,-0.965925826289068,0.));
#11034=DIRECTION('',(0.,0.,1.));
#11035=DIRECTION('center_axis',(-0.982489324426665,0.175514354454109,0.0625255049415299));
#11036=DIRECTION('ref_axis',(-0.186318886288095,-0.925515297832794,-0.329707000365231));
#11037=DIRECTION('center_axis',(0.338008733858616,-0.0905691672720826,-0.936774957914086));
#11038=DIRECTION('ref_axis',(-0.904855125270071,0.242455200083276,-0.349932390934396));
#11039=DIRECTION('center_axis',(-0.683496777669841,0.180523094083204,0.70727898838971));
#11040=DIRECTION('ref_axis',(-0.620872426437645,0.365761626196878,-0.693351182945011));
#11041=DIRECTION('center_axis',(-0.65831400371426,0.163876138290105,0.734688562462234));
#11042=DIRECTION('ref_axis',(-0.621487514031739,0.432351222926567,-0.653318980235957));
#11043=DIRECTION('center_axis',(-0.653921618105276,0.160745012694953,0.739288548719833));
#11044=DIRECTION('ref_axis',(-0.621897278706049,0.442272360574022,-0.646249900433488));
#11045=DIRECTION('center_axis',(-0.674075235079952,0.180617914877493,-0.716240006057476));
#11046=DIRECTION('ref_axis',(-0.258819045102521,-0.965925826289068,-3.01308868140017E-16));
#11047=DIRECTION('center_axis',(0.617002360972857,-0.165325284213947,-0.769399530123003));
#11048=DIRECTION('ref_axis',(0.286245910019278,-0.863567369973914,0.415108029931454));
#11049=DIRECTION('center_axis',(0.561902904510146,-0.150561429488195,-0.813385752182526));
#11050=DIRECTION('ref_axis',(0.558276694555572,-0.656562293339674,0.507201229573285));
#11051=DIRECTION('center_axis',(0.,0.,1.));
#11052=DIRECTION('ref_axis',(-0.534539664670774,-0.845143388362979,0.));
#11053=DIRECTION('center_axis',(-0.558874237830334,-0.749434485268718,-0.354975405598154));
#11054=DIRECTION('ref_axis',(0.558276694555565,-0.656562293339652,0.50720122957332));
#11055=DIRECTION('center_axis',(0.383424581050413,0.913295599568985,0.137392643377451));
#11056=DIRECTION('ref_axis',(-0.691543692210921,0.185298573858753,0.698163133006319));
#11057=DIRECTION('center_axis',(-0.250167531395729,-0.933637937572942,-0.256391122623056));
#11058=DIRECTION('ref_axis',(-0.965925826289068,0.258819045102521,-2.91742555544839E-17));
#11059=DIRECTION('center_axis',(-0.423012585798295,-0.887904844679767,-0.180790871037337));
#11060=DIRECTION('ref_axis',(0.273913532304164,-0.315488700307649,0.908536326625879));
#11061=DIRECTION('center_axis',(0.395037810900925,0.906269528225027,0.150401696032296));
#11062=DIRECTION('ref_axis',(-0.690739881421107,0.185083193406755,0.699015470310002));
#11063=DIRECTION('center_axis',(-0.428903026584179,-0.883790713143465,-0.186965689762311));
#11064=DIRECTION('ref_axis',(0.226054040298604,-0.305388776659452,0.925006630222249));
#11065=DIRECTION('center_axis',(0.694220983393908,-0.0865158721857753,-0.714543371724579));
#11066=DIRECTION('ref_axis',(-0.642354017365834,0.373397016182184,-0.669295140188703));
#11067=DIRECTION('center_axis',(-0.919731174770121,0.145681409008706,0.364515422479229));
#11068=DIRECTION('ref_axis',(0.303860786783007,-0.323674532104422,0.896048781887792));
#11069=DIRECTION('center_axis',(0.250253996385053,0.933960629306173,0.25512836024113));
#11070=DIRECTION('ref_axis',(0.713893553669226,-4.20541699587671E-15,-0.700254235281389));
#11071=DIRECTION('center_axis',(0.,0.,-1.));
#11072=DIRECTION('ref_axis',(0.,-1.,0.));
#11073=DIRECTION('center_axis',(-0.000608438188569021,-0.999999814768134,
-1.63299973368426E-5));
#11074=DIRECTION('ref_axis',(0.992173749069427,-0.000605715530870061,0.124863464497081));
#11075=DIRECTION('',(0.,0.,1.));
#11076=DIRECTION('center_axis',(0.250649702632458,0.935437425126364,0.249262011231594));
#11077=DIRECTION('ref_axis',(0.705141225886937,-3.98084930332909E-15,-0.709066887927131));
#11078=DIRECTION('center_axis',(0.250754597488213,0.935828898057517,0.247682065154054));
#11079=DIRECTION('ref_axis',(0.702734584093084,-1.83378449178784E-14,-0.711452109645843));
#11080=DIRECTION('center_axis',(0.140540951555781,0.524505971750252,-0.839727173869061));
#11081=DIRECTION('ref_axis',(0.424955852641996,-0.798002955152438,-0.427321666749171));
#11082=DIRECTION('center_axis',(-0.70009646922517,7.77263219592561E-15,
-0.71404827132236));
#11083=DIRECTION('ref_axis',(-0.71404827132236,2.32197393513232E-31,0.70009646922517));
#11084=DIRECTION('center_axis',(0.709066887926615,0.,0.705141225887457));
#11085=DIRECTION('ref_axis',(0.,1.,0.));
#11086=DIRECTION('center_axis',(-0.709066887926423,0.,0.70514122588765));
#11087=DIRECTION('ref_axis',(0.70514122588765,0.,0.709066887926423));
#11088=DIRECTION('',(0.,1.,0.));
#11089=DIRECTION('',(0.,1.,0.));
#11090=DIRECTION('center_axis',(0.709331039883401,-0.115502907144025,-0.695347793768854));
#11091=DIRECTION('ref_axis',(-0.0956309206562688,-0.993131507969492,0.0674131655737816));
#11092=DIRECTION('center_axis',(0.498818539794665,0.780955571567493,0.375883571860768));
#11093=DIRECTION('ref_axis',(-0.769313473215832,0.59870001961531,-0.222968756648148));
#11094=DIRECTION('center_axis',(-0.901161256199291,-0.00205051766332954,
-0.43347916409284));
#11095=DIRECTION('ref_axis',(-0.184974693085487,0.906194417947414,0.380257859614865));
#11096=DIRECTION('center_axis',(0.0190701713654315,0.92873814597838,0.37024557359776));
#11097=DIRECTION('ref_axis',(-0.88093921041517,0.1907406383142,-0.433086730861832));
#11098=DIRECTION('center_axis',(0.000264490323223583,0.341857053068283,
-0.939751927538506));
#11099=DIRECTION('ref_axis',(0.461132353426908,0.833829687993734,0.303455110425305));
#11100=DIRECTION('center_axis',(0.948694400412647,0.154852037999341,-0.275680577758279));
#11101=DIRECTION('ref_axis',(0.31381938810396,-0.354458336717562,0.88083862266676));
#11102=DIRECTION('center_axis',(1.06290398916907E-6,-0.342123200362749,
0.939655104691302));
#11103=DIRECTION('ref_axis',(0.120372757713139,-0.932822607049188,-0.339635662112345));
#11104=DIRECTION('center_axis',(-0.00180337743760444,0.342018865460073,
-0.939691355445617));
#11105=DIRECTION('ref_axis',(0.725796015895035,0.646870608951044,0.234048197143666));
#11106=DIRECTION('center_axis',(0.0160746645957318,0.949410867921572,0.313624949630195));
#11107=DIRECTION('ref_axis',(-0.881483570808126,0.16150693629599,-0.443736660558533));
#11108=DIRECTION('center_axis',(0.998612730749673,0.000484041380214348,
-0.0526533919954209));
#11109=DIRECTION('ref_axis',(0.0174203520886516,0.940611518756013,0.339037611654835));
#11110=DIRECTION('',(0.,0.939692620785908,0.342020143325669));
#11111=DIRECTION('center_axis',(0.08636525163809,0.995922297288841,0.0260733786151215));
#11112=DIRECTION('ref_axis',(0.978828013818433,-0.0799498801240489,-0.188424350953936));
#11113=DIRECTION('',(0.,1.,0.));
#11114=DIRECTION('center_axis',(0.998654787118421,0.0419942023103323,-0.0304155081788857));
#11115=DIRECTION('ref_axis',(0.0410790612416008,-0.998702024996989,-0.0301127214715466));
#11116=DIRECTION('center_axis',(0.0558943316700949,0.341485459772416,-0.93822358979679));
#11117=DIRECTION('ref_axis',(3.15158408626148E-17,-0.939692620785908,-0.34202014332567));
#11118=DIRECTION('center_axis',(-0.999999997425425,-6.29602249007253E-8,
7.1757557210404E-5));
#11119=DIRECTION('ref_axis',(6.29599482845205E-8,-0.999999999999998,-3.87634923658253E-9));
#11120=DIRECTION('center_axis',(0.,-1.,0.));
#11121=DIRECTION('ref_axis',(0.998606857012289,0.,0.0527668942428699));
#11122=DIRECTION('center_axis',(-0.499999999999997,2.40370335797946E-15,
0.866025403784441));
#11123=DIRECTION('ref_axis',(-0.86602540378444,-1.97523375096352E-30,-0.499999999999997));
#11124=DIRECTION('center_axis',(0.052566152876564,0.0871443475070821,-0.994807851933891));
#11125=DIRECTION('ref_axis',(-1.20857617498309E-18,-0.99618513361228,-0.0872649962463973));
#11126=DIRECTION('center_axis',(-0.0468293174424863,-0.283748024629802,
0.957754704267516));
#11127=DIRECTION('ref_axis',(-0.998806810296615,1.84862994057718E-6,-0.0488360082488711));
#11128=DIRECTION('center_axis',(0.26678747535128,-0.329623886957063,0.905633775950857));
#11129=DIRECTION('ref_axis',(-0.963721144476179,-0.0991646056426279,0.247806248261148));
#11130=DIRECTION('center_axis',(0.368750856924727,-0.317917392275649,0.873470856529244));
#11131=DIRECTION('ref_axis',(-0.929514851454483,-0.131167657818318,0.344669677325997));
#11132=DIRECTION('center_axis',(4.77253183189936E-13,-0.939692620785859,
-0.342020143325803));
#11133=DIRECTION('ref_axis',(0.96375164351186,0.0912513137134674,-0.250710923921866));
#11134=DIRECTION('center_axis',(0.0157117490853046,0.93086474670346,0.365025977548701));
#11135=DIRECTION('ref_axis',(0.320465643538016,-0.35050049031928,0.880029077700112));
#11136=DIRECTION('center_axis',(0.,0.,1.));
#11137=DIRECTION('ref_axis',(-0.713843353559374,-0.700305409502959,0.));
#11138=DIRECTION('center_axis',(0.000714845692164799,-0.935248614150113,
-0.353990845539725));
#11139=DIRECTION('ref_axis',(-0.929514851454482,-0.13116765781832,0.344669677325998));
#11140=DIRECTION('center_axis',(0.,0.939692620785908,0.342020143325669));
#11141=DIRECTION('ref_axis',(1.,0.,0.));
#11142=DIRECTION('',(1.,0.,0.));
#11143=DIRECTION('center_axis',(0.185962802483799,-0.914984054098916,-0.358081019934152));
#11144=DIRECTION('ref_axis',(-0.974399049469672,-0.218600131341872,0.0525402224007016));
#11145=DIRECTION('',(0.,-1.,0.));
#11146=DIRECTION('center_axis',(0.998286319297904,0.0169798943930786,0.0560009632867498));
#11147=DIRECTION('ref_axis',(0.0309996601200789,-0.96511714384739,-0.259976767662606));
#11148=DIRECTION('center_axis',(1.,0.,0.));
#11149=DIRECTION('ref_axis',(0.,-1.,0.));
#11150=DIRECTION('',(1.,0.,0.));
#11151=DIRECTION('',(0.,1.,0.));
#11152=DIRECTION('center_axis',(0.,1.,0.));
#11153=DIRECTION('ref_axis',(0.998040925216739,0.,0.0625644594999036));
#11154=DIRECTION('center_axis',(0.00136898756525043,0.999999062261074,3.67426066888223E-5));
#11155=DIRECTION('ref_axis',(0.999999062724686,-0.00136898831953958,2.0511696959745E-5));
#11156=DIRECTION('',(0.,-1.,0.));
#11157=DIRECTION('',(0.,1.,0.));
#11158=DIRECTION('center_axis',(0.0769992342443215,5.53463470572542E-15,
0.997031151933473));
#11159=DIRECTION('ref_axis',(0.372507740406449,0.927583081399946,-0.0287682192334328));
#11160=DIRECTION('center_axis',(-0.108282317724695,0.,-0.994120183714307));
#11161=DIRECTION('ref_axis',(0.,1.,0.));
#11162=DIRECTION('center_axis',(-0.147910770333402,0.,-0.98900070981743));
#11163=DIRECTION('ref_axis',(0.,1.,0.));
#11164=DIRECTION('center_axis',(0.179815697907154,0.,0.983700317569413));
#11165=DIRECTION('ref_axis',(0.191730437229931,0.980821655000061,-0.0350474039346959));
#11166=DIRECTION('center_axis',(-0.0593029104409559,-0.0158901669614693,
-0.998113554365017));
#11167=DIRECTION('ref_axis',(0.25881904510252,-0.965925826289068,2.91618690438022E-17));
#11168=DIRECTION('center_axis',(0.0698168329514292,0.0187073640074283,0.997384401506523));
#11169=DIRECTION('ref_axis',(-0.323156373260713,-0.945484767603846,0.0403548342839344));
#11170=DIRECTION('center_axis',(-0.0660314821081422,0.995510404849706,0.0678150219831547));
#11171=DIRECTION('ref_axis',(0.318920483681049,0.0854544860520815,-0.943921212762072));
#11172=DIRECTION('center_axis',(0.120185456360085,-0.985054343375952,-0.1233831296235));
#11173=DIRECTION('ref_axis',(-0.716328254484438,5.16215345872698E-16,-0.697763449764516));
#11174=DIRECTION('center_axis',(-0.626869024663385,0.756269149073557,-0.187329122341225));
#11175=DIRECTION('ref_axis',(0.401601466608204,0.107608788656578,-0.909470511133815));
#11176=DIRECTION('center_axis',(0.197508325342163,-0.959113442520952,-0.202711286800078));
#11177=DIRECTION('ref_axis',(-0.716238835403652,1.06988830219121E-14,-0.697855236176974));
#11178=DIRECTION('center_axis',(-0.716109385358714,5.87931396607782E-5,
-0.697988069199275));
#11179=DIRECTION('ref_axis',(-0.68756150283332,-0.172259653507989,0.705397612410826));
#11180=DIRECTION('center_axis',(0.716109496908384,-5.89002338248414E-5,
0.697987954744481));
#11181=DIRECTION('ref_axis',(-0.669323575897851,-0.283691166714552,0.686676978407934));
#11182=DIRECTION('center_axis',(0.452203132506872,-0.164412726418077,-0.876630356731243));
#11183=DIRECTION('ref_axis',(-0.554785176563544,0.717736695451074,-0.42079382584388));
#11184=DIRECTION('center_axis',(-0.258819045102521,0.965925826289068,-3.93157553907421E-15));
#11185=DIRECTION('ref_axis',(-0.965925826289068,-0.258819045102521,2.22044604925036E-14));
#11186=DIRECTION('',(-0.258819045102524,0.965925826289068,0.));
#11187=DIRECTION('center_axis',(-0.999923926773649,0.0102397286101005,-0.00687667241892065));
#11188=DIRECTION('ref_axis',(-0.0123345314287038,-0.830104467290876,0.557471463590887));
#11189=DIRECTION('center_axis',(0.,0.,-1.));
#11190=DIRECTION('ref_axis',(0.258819045325331,-0.965925826229366,0.));
#11191=DIRECTION('center_axis',(-0.674252347930799,-0.180665372122846,0.716061306471393));
#11192=DIRECTION('ref_axis',(0.691662109127011,0.185330303575785,0.698037395398328));
#11193=DIRECTION('center_axis',(0.,0.,1.));
#11194=DIRECTION('ref_axis',(-0.500000000000001,-0.866025403784438,0.));
#11195=DIRECTION('center_axis',(-0.695628388101101,0.0314971703251269,-0.717710996104542));
#11196=DIRECTION('ref_axis',(0.716946879324803,-0.03311269790395,-0.696340952022749));
#11197=DIRECTION('center_axis',(0.258111243842629,0.0691606993450251,0.96363654116483));
#11198=DIRECTION('ref_axis',(0.258819045102521,-0.965925826289068,-2.93972626113222E-17));
#11199=DIRECTION('center_axis',(-0.965925826289068,-0.258819045102521,0.));
#11200=DIRECTION('ref_axis',(0.,0.,1.));
#11201=DIRECTION('center_axis',(1.,0.,0.));
#11202=DIRECTION('ref_axis',(0.,-0.707106781186547,-0.707106781186548));
#11203=DIRECTION('',(-1.,0.,0.));
#11204=DIRECTION('center_axis',(1.,0.,0.));
#11205=DIRECTION('ref_axis',(0.,-1.,0.));
#11206=DIRECTION('',(1.,0.,0.));
#11207=DIRECTION('center_axis',(0.0468234603154239,-0.283756854133083,0.95775237472772));
#11208=DIRECTION('ref_axis',(3.26081672821954E-17,-0.958804009877884,-0.284068425985871));
#11209=DIRECTION('center_axis',(-0.0525661528831979,0.0871443475057628,
-0.994807851933656));
#11210=DIRECTION('ref_axis',(0.998606857012238,-6.04578193157126E-18,-0.0527668942438301));
#11211=DIRECTION('center_axis',(-0.499999999999829,-1.34607388046865E-13,
-0.866025403784538));
#11212=DIRECTION('ref_axis',(0.866025403784538,1.92284846106144E-30,-0.499999999999829));
#11213=DIRECTION('center_axis',(-0.266795615085176,-0.329622984395579,0.905631706561489));
#11214=DIRECTION('ref_axis',(-1.17693390083123E-12,-0.939692620785966,-0.342020143325511));
#11215=DIRECTION('center_axis',(-3.84846287078961E-13,-0.939692620785867,
-0.342020143325782));
#11216=DIRECTION('ref_axis',(-0.929470733634111,0.126169814813646,-0.346648717216086));
#11217=DIRECTION('center_axis',(0.998804703166064,1.69786870596043E-5,-0.0488790818763427));
#11218=DIRECTION('ref_axis',(0.0170818764593461,0.936825466105722,0.349379815605343));
#11219=DIRECTION('',(0.,1.,0.));
#11220=DIRECTION('center_axis',(0.0155776059735878,0.947746103906714,0.318645038752805));
#11221=DIRECTION('ref_axis',(-0.846028382887146,0.182343886514573,-0.50098571077439));
#11222=DIRECTION('center_axis',(0.0312572139148635,0.341853023360818,-0.93923346245614));
#11223=DIRECTION('ref_axis',(-4.36812986433843E-19,-0.939692620785908,-0.342020143325669));
#11224=DIRECTION('center_axis',(0.,0.939692620785908,0.342020143325669));
#11225=DIRECTION('ref_axis',(1.,0.,0.));
#11226=DIRECTION('',(1.,0.,0.));
#11227=DIRECTION('center_axis',(4.78283496086397E-13,-0.939692620785863,
-0.342020143325795));
#11228=DIRECTION('ref_axis',(0.971659954583462,0.0808477547528646,-0.222127380595651));
#11229=DIRECTION('center_axis',(1.,0.,0.));
#11230=DIRECTION('ref_axis',(0.,-1.,0.));
#11231=DIRECTION('',(1.,0.,0.));
#11232=DIRECTION('center_axis',(0.700096469223959,-7.77263219591216E-15,
-0.714048271323547));
#11233=DIRECTION('ref_axis',(0.714048271323547,8.33364844194403E-32,0.700096469223959));
#11234=DIRECTION('center_axis',(0.709066887927214,0.,0.705141225886854));
#11235=DIRECTION('ref_axis',(-0.705141225886854,0.,0.709066887927214));
#11236=DIRECTION('center_axis',(-0.709066887925823,0.,0.705141225888253));
#11237=DIRECTION('ref_axis',(0.,-1.,0.));
#11238=DIRECTION('center_axis',(-0.70009646922517,-2.33178965877769E-14,
-0.71404827132236));
#11239=DIRECTION('ref_axis',(3.33066907387548E-14,-1.,4.30601063609922E-29));
#11240=DIRECTION('center_axis',(0.,0.,1.));
#11241=DIRECTION('ref_axis',(0.,-1.,0.));
#11242=DIRECTION('',(0.,0.,1.));
#11243=DIRECTION('center_axis',(0.,1.,0.));
#11244=DIRECTION('ref_axis',(1.,0.,0.));
#11245=DIRECTION('',(-1.,0.,0.));
#11246=DIRECTION('',(0.,0.,-1.));
#11247=DIRECTION('center_axis',(-1.50215510448877E-15,-1.,2.30138252825371E-14));
#11248=DIRECTION('ref_axis',(-0.999999999791142,1.50262546286449E-15,2.04380924802295E-5));
#11249=DIRECTION('center_axis',(-5.46390275282226E-14,-1.,9.03906656443215E-15));
#11250=DIRECTION('ref_axis',(0.410021673945177,-3.0647499209318E-14,-0.912075779140744));
#11251=DIRECTION('',(0.,0.,1.));
#11252=DIRECTION('',(1.,0.,0.));
#11253=DIRECTION('center_axis',(0.,-1.,0.));
#11254=DIRECTION('ref_axis',(1.,0.,0.));
#11255=DIRECTION('center_axis',(0.,-1.,0.));
#11256=DIRECTION('ref_axis',(1.,0.,0.));
#11257=DIRECTION('center_axis',(0.,-1.,0.));
#11258=DIRECTION('ref_axis',(1.,0.,0.));
#11259=DIRECTION('center_axis',(0.,-1.,0.));
#11260=DIRECTION('ref_axis',(1.,0.,0.));
#11261=DIRECTION('center_axis',(1.,0.,0.));
#11262=DIRECTION('ref_axis',(0.,-0.707106781186547,-0.707106781186548));
#11263=DIRECTION('',(1.,0.,0.));
#11264=DIRECTION('center_axis',(-1.,0.,0.));
#11265=DIRECTION('ref_axis',(0.,0.,-1.));
#11266=DIRECTION('center_axis',(0.,1.,0.));
#11267=DIRECTION('ref_axis',(0.707106781186547,0.,-0.707106781186547));
#11268=DIRECTION('center_axis',(0.,1.,0.));
#11269=DIRECTION('ref_axis',(1.,0.,-1.11022302462516E-14));
#11270=DIRECTION('',(0.,1.,0.));
#11271=DIRECTION('center_axis',(0.,-1.,0.));
#11272=DIRECTION('ref_axis',(0.,0.,-1.));
#11273=DIRECTION('',(0.,-1.,0.));
#11274=DIRECTION('center_axis',(-1.,0.,0.));
#11275=DIRECTION('ref_axis',(0.,0.707106781186547,-0.707106781186548));
#11276=DIRECTION('',(1.,0.,0.));
#11277=DIRECTION('center_axis',(-1.,0.,0.));
#11278=DIRECTION('ref_axis',(0.,1.,-1.11022302462516E-14));
#11279=DIRECTION('',(-1.,0.,0.));
#11280=DIRECTION('center_axis',(-0.408248290463859,-0.408248290463862,-0.816496580927729));
#11281=DIRECTION('ref_axis',(0.577350269189625,0.57735026918963,-0.577350269189623));
#11282=DIRECTION('center_axis',(0.,0.,-1.));
#11283=DIRECTION('ref_axis',(0.707106781186549,0.707106781186546,0.));
#11284=DIRECTION('center_axis',(-0.408248290463859,0.408248290463861,-0.816496580927729));
#11285=DIRECTION('ref_axis',(0.577350269189625,-0.577350269189629,-0.577350269189623));
#11286=DIRECTION('center_axis',(0.,0.,-1.));
#11287=DIRECTION('ref_axis',(0.707106781186549,-0.707106781186546,0.));
#11288=DIRECTION('center_axis',(0.,0.,1.));
#11289=DIRECTION('ref_axis',(0.707106781186548,-0.707106781186547,0.));
#11290=DIRECTION('',(0.,0.,1.));
#11291=DIRECTION('center_axis',(0.,0.,-1.));
#11292=DIRECTION('ref_axis',(1.,0.,0.));
#11293=DIRECTION('center_axis',(1.,0.,0.));
#11294=DIRECTION('ref_axis',(0.,0.,-1.));
#11295=DIRECTION('',(0.,0.,-1.));
#11296=DIRECTION('',(0.,1.,0.));
#11297=DIRECTION('center_axis',(0.,0.,-1.));
#11298=DIRECTION('ref_axis',(0.707106781186548,0.707106781186547,0.));
#11299=DIRECTION('',(0.,0.,1.));
#11300=DIRECTION('center_axis',(0.,1.,0.));
#11301=DIRECTION('ref_axis',(1.,0.,0.));
#11302=DIRECTION('',(-1.,0.,0.));
#11303=DIRECTION('',(-1.,0.,0.));
#11304=DIRECTION('',(0.,0.,1.));
#11305=DIRECTION('',(0.,0.,1.));
#11306=DIRECTION('',(0.,0.,-1.));
#11307=DIRECTION('',(-1.,0.,0.));
#11308=DIRECTION('',(-1.,0.,0.));
#11309=DIRECTION('center_axis',(0.,-1.,0.));
#11310=DIRECTION('ref_axis',(1.,0.,0.));
#11311=DIRECTION('center_axis',(0.,-1.,0.));
#11312=DIRECTION('ref_axis',(1.,0.,0.));
#11313=DIRECTION('center_axis',(0.,-1.,0.));
#11314=DIRECTION('ref_axis',(1.,0.,0.));
#11315=DIRECTION('center_axis',(0.,-1.,0.));
#11316=DIRECTION('ref_axis',(1.,0.,0.));
#11317=DIRECTION('center_axis',(-0.124883782089936,0.,-0.99217137681497));
#11318=DIRECTION('ref_axis',(0.99217137681497,0.,-0.124883782089936));
#11319=DIRECTION('center_axis',(0.,1.,0.));
#11320=DIRECTION('ref_axis',(-0.992173928994009,0.,0.124863503973705));
#11321=DIRECTION('center_axis',(-0.215465317990859,0.,-0.97651149340041));
#11322=DIRECTION('ref_axis',(0.97651149340041,-5.55111512312577E-15,-0.215465317990859));
#11323=DIRECTION('center_axis',(0.384746145047863,4.23953194639129E-13,
0.923022428693262));
#11324=DIRECTION('ref_axis',(-3.05311331771915E-12,-1.,1.73194791841523E-12));
#11325=DIRECTION('center_axis',(-0.74869039128462,-0.200610985725532,0.631836949223701));
#11326=DIRECTION('ref_axis',(-0.324728217067871,-0.719949447827078,-0.613371321153351));
#11327=DIRECTION('center_axis',(0.0982582777590185,0.957717020306253,0.270413423978069));
#11328=DIRECTION('ref_axis',(0.127909569660762,-0.281628557964879,0.950959776924251));
#11329=DIRECTION('center_axis',(-0.65684684485648,-0.176001581630224,0.733195516670518));
#11330=DIRECTION('ref_axis',(-0.437553251543722,-0.702943249076073,-0.560729828564426));
#11331=DIRECTION('center_axis',(-0.264383392923062,0.919236580826271,0.291728521089929));
#11332=DIRECTION('ref_axis',(0.07007383801871,-0.283382405581138,0.95644344810991));
#11333=DIRECTION('center_axis',(0.,0.,1.));
#11334=DIRECTION('ref_axis',(1.,0.,0.));
#11335=DIRECTION('center_axis',(0.363488148886145,-0.708643875710738,0.604731529719585));
#11336=DIRECTION('ref_axis',(-0.437553251543735,-0.702943249076031,-0.560729828564468));
#11337=DIRECTION('',(0.,-1.,0.));
#11338=DIRECTION('center_axis',(0.,-1.,0.));
#11339=DIRECTION('ref_axis',(-0.998040925216754,0.,0.0625644594996687));
#11340=DIRECTION('center_axis',(0.163972207190969,0.540732729492925,0.82505831946842));
#11341=DIRECTION('ref_axis',(-0.984161974111908,0.0325543710521824,0.174256769273245));
#11342=DIRECTION('center_axis',(0.,0.,-1.));
#11343=DIRECTION('ref_axis',(-1.,0.,0.));
#11344=DIRECTION('center_axis',(-0.771919959919765,-0.0808086527971774,
-0.630562873241499));
#11345=DIRECTION('ref_axis',(0.0625870122150387,-0.99672963314136,0.0511165757840384));
#11346=DIRECTION('center_axis',(0.700096469223959,1.55452643918243E-14,
-0.714048271323547));
#11347=DIRECTION('ref_axis',(-2.22044604925031E-14,1.,-3.53183321097136E-30));
#11348=DIRECTION('center_axis',(0.,0.,-1.));
#11349=DIRECTION('ref_axis',(0.,-1.,0.));
#11350=DIRECTION('center_axis',(0.,0.,1.));
#11351=DIRECTION('ref_axis',(0.,-1.,0.));
#11352=DIRECTION('',(0.,-1.,-6.48452891646315E-16));
#11353=DIRECTION('',(0.,1.,0.));
#11354=DIRECTION('',(0.447898727755213,0.894084296738994,0.));
#11355=DIRECTION('center_axis',(-1.13908027475977E-11,1.,1.26463314793467E-25));
#11356=DIRECTION('ref_axis',(1.11022302462518E-14,3.05100033046494E-40,
1.));
#11357=DIRECTION('center_axis',(0.,0.,-1.));
#11358=DIRECTION('ref_axis',(-1.,0.,0.));
#11359=DIRECTION('center_axis',(1.76229903791608E-12,9.84552143939818E-13,
-1.));
#11360=DIRECTION('ref_axis',(-0.890482609600958,-0.455017276593172,-2.01698753190003E-12));
#11361=DIRECTION('center_axis',(0.,0.,-1.));
#11362=DIRECTION('ref_axis',(-1.,0.,0.));
#11363=DIRECTION('center_axis',(-1.,0.,0.));
#11364=DIRECTION('ref_axis',(0.,0.,1.));
#11365=DIRECTION('',(0.,-1.,0.));
#11366=DIRECTION('center_axis',(-5.20040241961378E-7,-0.999999999999865,
5.77360650357171E-21));
#11367=DIRECTION('ref_axis',(0.999398340012359,-5.19727354555897E-7,0.0346836846409219));
#11368=DIRECTION('center_axis',(0.0377485314798384,0.276390855786013,-0.960303672391703));
#11369=DIRECTION('ref_axis',(-0.999228297332728,-4.13963359097666E-15,-0.0392786177141947));
#11370=DIRECTION('center_axis',(-0.998948438150501,0.0354752832048574,-0.0290434536205597));
#11371=DIRECTION('ref_axis',(-0.0305542913919211,-0.98741517219653,-0.155169948745348));
#11372=DIRECTION('center_axis',(0.263764010584037,0.923513515076835,0.278480401807835));
#11373=DIRECTION('ref_axis',(0.891000137487118,-0.343866627487043,0.296436329586345));
#11374=DIRECTION('center_axis',(0.169401090369437,-0.337076992361637,0.926111425154705));
#11375=DIRECTION('ref_axis',(4.54657600793298E-17,0.939692620788689,0.342020143318028));
#11376=DIRECTION('center_axis',(-0.554161596073854,-0.802096420655957,-0.222589886130932));
#11377=DIRECTION('ref_axis',(0.831536970603906,-0.545659536114231,-0.103932368232812));
#11378=DIRECTION('center_axis',(0.0310203232622331,0.341855547490705,-0.939240397446009));
#11379=DIRECTION('ref_axis',(-0.999518753973484,0.0106095754081624,-0.0291495688639121));
#11380=DIRECTION('center_axis',(-0.0569607767181947,0.341464845217121,-0.938166951771649));
#11381=DIRECTION('ref_axis',(2.16317518465542E-9,0.939692620828124,0.342020143209682));
#11382=DIRECTION('center_axis',(0.,0.,1.));
#11383=DIRECTION('ref_axis',(-0.736625730662687,0.676300623188876,0.));
#11384=DIRECTION('center_axis',(-0.000471408636173,0.934389008169434,0.356254065501068));
#11385=DIRECTION('ref_axis',(-0.972631522480859,-0.0832049765466535,0.216944355433455));
#11386=DIRECTION('center_axis',(-0.232320635143996,0.332662217771895,-0.913981931633976));
#11387=DIRECTION('ref_axis',(-0.972631522480859,-0.0832049765466558,0.216944355433454));
#11388=DIRECTION('center_axis',(-0.0123951381577513,-0.927528497526217,
-0.373546846897158));
#11389=DIRECTION('ref_axis',(-0.203183137824287,0.368118154650563,-0.907306804074863));
#11390=DIRECTION('center_axis',(8.47652041731572E-13,0.939692620785858,
0.342020143325808));
#11391=DIRECTION('ref_axis',(0.201508985660445,-0.335004169860873,0.920416392114963));
#11392=DIRECTION('center_axis',(0.000457813874219378,-0.9345848157438,-0.355740091341395));
#11393=DIRECTION('ref_axis',(-0.943802615278056,-0.117979263083487,0.308735350869606));
#11394=DIRECTION('',(0.,0.939692620785908,0.342020143325669));
#11395=DIRECTION('',(0.,-1.,0.));
#11396=DIRECTION('center_axis',(-0.0490673383431336,-0.288968791309725,
0.956080244517644));
#11397=DIRECTION('ref_axis',(-0.998685654811338,1.09394001838749E-14,-0.0512539059394343));
#11398=DIRECTION('center_axis',(0.236372695682419,-0.332328136044342,0.913064049631306));
#11399=DIRECTION('ref_axis',(-0.971626941679023,-0.0888766187212934,0.21918492842378));
#11400=DIRECTION('center_axis',(0.33047220550483,-0.322803989289558,0.886896671482941));
#11401=DIRECTION('ref_axis',(-0.943802615278055,-0.117979263083488,0.308735350869608));
#11402=DIRECTION('center_axis',(0.0160970752919315,0.928887250896035,0.370012647472829));
#11403=DIRECTION('ref_axis',(0.286399133952083,-0.358838253610397,0.888375283209375));
#11404=DIRECTION('center_axis',(0.,0.,1.));
#11405=DIRECTION('ref_axis',(-0.710878052583325,-0.703315288014799,0.));
#11406=DIRECTION('center_axis',(1.,0.,0.));
#11407=DIRECTION('ref_axis',(0.,-1.,0.));
#11408=DIRECTION('',(1.,0.,0.));
#11409=DIRECTION('center_axis',(0.,0.,-1.));
#11410=DIRECTION('ref_axis',(-1.,0.,0.));
#11411=DIRECTION('center_axis',(1.,0.,0.));
#11412=DIRECTION('ref_axis',(0.,-1.,0.));
#11413=DIRECTION('',(1.,0.,0.));
#11414=DIRECTION('center_axis',(0.,1.,0.));
#11415=DIRECTION('ref_axis',(1.,0.,0.));
#11416=DIRECTION('',(0.,1.,0.));
#11417=DIRECTION('center_axis',(0.,1.,0.));
#11418=DIRECTION('ref_axis',(1.,0.,0.));
#11419=DIRECTION('',(0.,1.,0.));
#11420=DIRECTION('center_axis',(0.,1.,0.));
#11421=DIRECTION('ref_axis',(1.,0.,0.));
#11422=DIRECTION('',(0.,1.,0.));
#11423=DIRECTION('center_axis',(0.,1.,0.));
#11424=DIRECTION('ref_axis',(1.,0.,0.));
#11425=DIRECTION('',(0.,1.,0.));
#11426=DIRECTION('center_axis',(0.,0.939692620785908,0.342020143325669));
#11427=DIRECTION('ref_axis',(1.,0.,0.));
#11428=DIRECTION('center_axis',(0.965925826289068,-0.258819045102521,0.));
#11429=DIRECTION('ref_axis',(0.,0.,-1.));
#11430=DIRECTION('center_axis',(0.,0.939692620785908,0.342020143325669));
#11431=DIRECTION('ref_axis',(1.,0.,0.));
#11432=DIRECTION('axis',(0.,0.,1.));
#11433=DIRECTION('refdir',(1.,0.,0.));
#11434=DIRECTION('center_axis',(0.662084710881893,0.707106781186549,0.24828176658071));
#11435=DIRECTION('ref_axis',(0.351123441588392,-1.5422241502084E-16,-0.936329177569044));
#11436=DIRECTION('',(-0.351123441588392,0.,0.936329177569044));
#11437=DIRECTION('',(0.577350269189626,-0.692482572856324,0.432590514178192));
#11438=DIRECTION('',(0.351123441588392,0.,-0.936329177569044));
#11439=DIRECTION('',(0.701364677853665,-0.701364677853665,0.127181670528612));
#11440=DIRECTION('center_axis',(0.424264068711928,0.707106781186549,0.565685424949237));
#11441=DIRECTION('ref_axis',(0.8,-1.29618843440069E-16,-0.6));
#11442=DIRECTION('',(-0.8,0.,0.6));
#11443=DIRECTION('',(0.22941573387057,-0.688247201611684,0.688247201611684));
#11444=DIRECTION('',(0.8,0.,-0.6));
#11445=DIRECTION('center_axis',(0.,0.707106781186548,0.707106781186548));
#11446=DIRECTION('ref_axis',(1.,0.,0.));
#11447=DIRECTION('',(-1.,0.,0.));
#11448=DIRECTION('',(-0.229415733870552,-0.688247201611687,0.688247201611687));
#11449=DIRECTION('',(1.,0.,0.));
#11450=DIRECTION('center_axis',(-0.424264068711929,0.707106781186546,0.565685424949239));
#11451=DIRECTION('ref_axis',(0.8,-1.26358053862033E-16,0.6));
#11452=DIRECTION('',(-0.8,0.,-0.6));
#11453=DIRECTION('',(-0.57735026918963,-0.692482572856329,0.43259051417818));
#11454=DIRECTION('',(0.8,0.,0.6));
#11455=DIRECTION('center_axis',(-0.662084710881897,0.707106781186545,0.248281766580712));
#11456=DIRECTION('ref_axis',(0.351123441588392,-1.9741179685392E-16,0.936329177569044));
#11457=DIRECTION('',(-0.351123441588392,0.,-0.936329177569044));
#11458=DIRECTION('',(-0.701364677853667,-0.701364677853667,0.127181670528596));
#11459=DIRECTION('',(0.351123441588392,0.,0.936329177569044));
#11460=DIRECTION('center_axis',(-0.707106781186548,0.707106781186548,0.));
#11461=DIRECTION('ref_axis',(0.,0.,1.));
#11462=DIRECTION('',(0.,0.,1.));
#11463=DIRECTION('',(0.,0.,-1.));
#11464=DIRECTION('',(-0.577350269189626,-0.577350269189623,-0.577350269189629));
#11465=DIRECTION('center_axis',(0.,0.707106781186549,-0.707106781186547));
#11466=DIRECTION('ref_axis',(-1.,0.,0.));
#11467=DIRECTION('',(-1.,0.,0.));
#11468=DIRECTION('',(1.,0.,0.));
#11469=DIRECTION('',(0.577350269189625,-0.577350269189625,-0.577350269189627));
#11470=DIRECTION('center_axis',(0.707106781186548,0.707106781186548,0.));
#11471=DIRECTION('ref_axis',(0.,0.,-1.));
#11472=DIRECTION('',(0.,0.,-1.));
#11473=DIRECTION('',(0.,0.,1.));
#11474=DIRECTION('center_axis',(-1.,0.,0.));
#11475=DIRECTION('ref_axis',(0.,0.,1.));
#11476=DIRECTION('',(0.,1.,0.));
#11477=DIRECTION('',(0.,0.,-1.));
#11478=DIRECTION('',(0.,1.,0.));
#11479=DIRECTION('center_axis',(0.,0.,-1.));
#11480=DIRECTION('ref_axis',(-1.,0.,0.));
#11481=DIRECTION('',(0.,1.,0.));
#11482=DIRECTION('',(1.,0.,0.));
#11483=DIRECTION('center_axis',(1.,0.,0.));
#11484=DIRECTION('ref_axis',(0.,0.,-1.));
#11485=DIRECTION('',(0.,1.,0.));
#11486=DIRECTION('',(0.,0.,1.));
#11487=DIRECTION('center_axis',(0.936329177569044,0.,0.351123441588392));
#11488=DIRECTION('ref_axis',(0.351123441588392,0.,-0.936329177569044));
#11489=DIRECTION('',(0.,1.,0.));
#11490=DIRECTION('',(-0.351123441588392,0.,0.936329177569044));
#11491=DIRECTION('center_axis',(0.,1.,0.));
#11492=DIRECTION('ref_axis',(0.,0.,1.));
#11493=DIRECTION('',(0.,0.,-1.));
#11494=DIRECTION('',(1.,0.,0.));
#11495=DIRECTION('',(0.,0.,-1.));
#11496=DIRECTION('',(1.,0.,0.));
#11497=DIRECTION('',(0.,0.,1.));
#11498=DIRECTION('',(1.,0.,0.));
#11499=DIRECTION('',(0.,0.,1.));
#11500=DIRECTION('',(-1.,0.,0.));
#11501=DIRECTION('',(0.,0.,1.));
#11502=DIRECTION('',(-1.,0.,0.));
#11503=DIRECTION('',(0.,0.,-1.));
#11504=DIRECTION('',(-1.,0.,0.));
#11505=DIRECTION('center_axis',(0.,-1.,0.));
#11506=DIRECTION('ref_axis',(1.,0.,0.));
#11507=DIRECTION('center_axis',(0.,-1.,0.));
#11508=DIRECTION('ref_axis',(1.,0.,0.));
#11509=DIRECTION('center_axis',(0.,-1.,0.));
#11510=DIRECTION('ref_axis',(-1.,0.,0.));
#11511=DIRECTION('center_axis',(0.,-1.,0.));
#11512=DIRECTION('ref_axis',(-1.,0.,0.));
#11513=DIRECTION('center_axis',(0.,-1.,0.));
#11514=DIRECTION('ref_axis',(-1.,0.,0.));
#11515=DIRECTION('center_axis',(0.,-1.,0.));
#11516=DIRECTION('ref_axis',(-1.,0.,0.));
#11517=DIRECTION('center_axis',(0.,1.,0.));
#11518=DIRECTION('ref_axis',(-1.,0.,0.));
#11519=DIRECTION('',(0.85716730070211,0.515038074910058,-1.04972719113862E-16));
#11520=DIRECTION('center_axis',(0.,1.,0.));
#11521=DIRECTION('ref_axis',(1.,0.,0.));
#11522=DIRECTION('center_axis',(0.,1.,0.));
#11523=DIRECTION('ref_axis',(-1.,0.,0.));
#11524=DIRECTION('',(0.,1.,0.));
#11525=DIRECTION('center_axis',(0.,1.,0.));
#11526=DIRECTION('ref_axis',(1.,0.,0.));
#11527=DIRECTION('center_axis',(0.,1.,0.));
#11528=DIRECTION('ref_axis',(-1.,0.,0.));
#11529=DIRECTION('',(0.707106781186546,0.707106781186549,-8.65956056235491E-17));
#11530=DIRECTION('center_axis',(0.,1.,0.));
#11531=DIRECTION('ref_axis',(-1.,0.,0.));
#11532=DIRECTION('',(0.85716730070211,0.515038074910058,-1.04972719113862E-16));
#11533=DIRECTION('center_axis',(0.,1.,0.));
#11534=DIRECTION('ref_axis',(1.,0.,0.));
#11535=DIRECTION('center_axis',(0.,1.,0.));
#11536=DIRECTION('ref_axis',(-1.,0.,0.));
#11537=DIRECTION('',(0.,1.,0.));
#11538=DIRECTION('center_axis',(0.,1.,0.));
#11539=DIRECTION('ref_axis',(1.,0.,0.));
#11540=DIRECTION('center_axis',(0.,1.,0.));
#11541=DIRECTION('ref_axis',(-1.,0.,0.));
#11542=DIRECTION('',(0.707106781186547,0.707106781186548,-8.65956056235493E-17));
#11543=DIRECTION('center_axis',(0.,1.,0.));
#11544=DIRECTION('ref_axis',(-1.,0.,0.));
#11545=DIRECTION('',(0.85716730070211,0.515038074910058,-1.04972719113862E-16));
#11546=DIRECTION('center_axis',(0.,1.,0.));
#11547=DIRECTION('ref_axis',(1.,0.,0.));
#11548=DIRECTION('center_axis',(0.,1.,0.));
#11549=DIRECTION('ref_axis',(-1.,0.,0.));
#11550=DIRECTION('',(0.,1.,0.));
#11551=DIRECTION('center_axis',(0.,1.,0.));
#11552=DIRECTION('ref_axis',(1.,0.,0.));
#11553=DIRECTION('center_axis',(0.,1.,0.));
#11554=DIRECTION('ref_axis',(-1.,0.,0.));
#11555=DIRECTION('',(0.707106781186546,0.707106781186549,-8.65956056235491E-17));
#11556=DIRECTION('center_axis',(0.,1.,0.));
#11557=DIRECTION('ref_axis',(-1.,0.,0.));
#11558=DIRECTION('',(0.85716730070211,0.515038074910058,-1.04972719113862E-16));
#11559=DIRECTION('center_axis',(0.,1.,0.));
#11560=DIRECTION('ref_axis',(1.,0.,0.));
#11561=DIRECTION('center_axis',(0.,1.,0.));
#11562=DIRECTION('ref_axis',(-1.,0.,0.));
#11563=DIRECTION('',(0.,1.,0.));
#11564=DIRECTION('center_axis',(0.,1.,0.));
#11565=DIRECTION('ref_axis',(1.,0.,0.));
#11566=DIRECTION('center_axis',(0.,1.,0.));
#11567=DIRECTION('ref_axis',(-1.,0.,0.));
#11568=DIRECTION('',(0.707106781186547,0.707106781186548,-8.65956056235493E-17));
#11569=DIRECTION('center_axis',(0.,-1.,0.));
#11570=DIRECTION('ref_axis',(1.,0.,0.));
#11571=DIRECTION('',(-0.85716730070211,-0.515038074910058,-1.04972719113862E-16));
#11572=DIRECTION('center_axis',(0.,-1.,0.));
#11573=DIRECTION('ref_axis',(1.,0.,0.));
#11574=DIRECTION('center_axis',(0.,-1.,0.));
#11575=DIRECTION('ref_axis',(1.,0.,0.));
#11576=DIRECTION('',(0.,-1.,0.));
#11577=DIRECTION('center_axis',(0.,1.,0.));
#11578=DIRECTION('ref_axis',(1.,0.,0.));
#11579=DIRECTION('center_axis',(0.,-1.,0.));
#11580=DIRECTION('ref_axis',(1.,0.,0.));
#11581=DIRECTION('',(-0.85716730070211,-0.515038074910058,-1.04972719113862E-16));
#11582=DIRECTION('center_axis',(0.,-1.,0.));
#11583=DIRECTION('ref_axis',(1.,0.,0.));
#11584=DIRECTION('center_axis',(0.,-1.,0.));
#11585=DIRECTION('ref_axis',(1.,0.,0.));
#11586=DIRECTION('',(0.,-1.,0.));
#11587=DIRECTION('center_axis',(0.,1.,0.));
#11588=DIRECTION('ref_axis',(1.,0.,0.));
#11589=DIRECTION('center_axis',(0.,1.,0.));
#11590=DIRECTION('ref_axis',(1.,0.,0.));
#11591=DIRECTION('center_axis',(0.,1.,0.));
#11592=DIRECTION('ref_axis',(1.,0.,0.));
#11593=DIRECTION('',(0.,1.,0.));
#11594=DIRECTION('center_axis',(0.,1.,0.));
#11595=DIRECTION('ref_axis',(1.,0.,0.));
#11596=DIRECTION('center_axis',(0.,1.,0.));
#11597=DIRECTION('ref_axis',(1.,0.,0.));
#11598=DIRECTION('',(0.,1.,0.));
#11599=DIRECTION('center_axis',(0.,0.,-1.));
#11600=DIRECTION('ref_axis',(1.,0.,0.));
#11601=DIRECTION('center_axis',(0.,0.,-1.));
#11602=DIRECTION('ref_axis',(1.,0.,0.));
#11603=DIRECTION('',(0.,0.,-1.));
#11604=DIRECTION('center_axis',(0.,0.,1.));
#11605=DIRECTION('ref_axis',(1.,0.,0.));
#11606=DIRECTION('center_axis',(-1.,0.,0.));
#11607=DIRECTION('ref_axis',(0.,0.,-1.));
#11608=DIRECTION('',(0.,-1.,0.));
#11609=DIRECTION('',(0.,0.,-1.));
#11610=DIRECTION('',(0.,-1.,0.));
#11611=DIRECTION('center_axis',(0.,0.,1.));
#11612=DIRECTION('ref_axis',(-1.,0.,0.));
#11613=DIRECTION('',(0.,-1.,0.));
#11614=DIRECTION('',(-1.,0.,0.));
#11615=DIRECTION('center_axis',(-1.,0.,0.));
#11616=DIRECTION('ref_axis',(0.,0.,-1.));
#11617=DIRECTION('',(0.,-1.,0.));
#11618=DIRECTION('',(0.,0.,-1.));
#11619=DIRECTION('center_axis',(0.,0.,1.));
#11620=DIRECTION('ref_axis',(-1.,0.,0.));
#11621=DIRECTION('',(0.,-1.,0.));
#11622=DIRECTION('',(-1.,0.,0.));
#11623=DIRECTION('center_axis',(1.,0.,0.));
#11624=DIRECTION('ref_axis',(0.,0.,1.));
#11625=DIRECTION('',(0.,-1.,0.));
#11626=DIRECTION('',(0.,0.,1.));
#11627=DIRECTION('center_axis',(0.,0.,1.));
#11628=DIRECTION('ref_axis',(-1.,0.,0.));
#11629=DIRECTION('',(0.,-1.,0.));
#11630=DIRECTION('',(-1.,0.,0.));
#11631=DIRECTION('center_axis',(1.,0.,0.));
#11632=DIRECTION('ref_axis',(0.,0.,1.));
#11633=DIRECTION('',(0.,-1.,0.));
#11634=DIRECTION('',(0.,0.,1.));
#11635=DIRECTION('center_axis',(0.,0.,-1.));
#11636=DIRECTION('ref_axis',(1.,0.,0.));
#11637=DIRECTION('',(0.,-1.,0.));
#11638=DIRECTION('',(1.,0.,0.));
#11639=DIRECTION('center_axis',(1.,0.,0.));
#11640=DIRECTION('ref_axis',(0.,0.,1.));
#11641=DIRECTION('',(0.,-1.,0.));
#11642=DIRECTION('',(0.,0.,1.));
#11643=DIRECTION('center_axis',(0.,0.,-1.));
#11644=DIRECTION('ref_axis',(1.,0.,0.));
#11645=DIRECTION('',(0.,-1.,0.));
#11646=DIRECTION('',(1.,0.,0.));
#11647=DIRECTION('center_axis',(-1.,0.,0.));
#11648=DIRECTION('ref_axis',(0.,0.,-1.));
#11649=DIRECTION('',(0.,-1.,0.));
#11650=DIRECTION('',(0.,0.,-1.));
#11651=DIRECTION('center_axis',(0.,0.,-1.));
#11652=DIRECTION('ref_axis',(1.,0.,0.));
#11653=DIRECTION('',(1.,0.,0.));
#11654=DIRECTION('center_axis',(0.,-1.,0.));
#11655=DIRECTION('ref_axis',(0.,0.,-1.));
#11656=DIRECTION('center_axis',(0.6,0.,0.8));
#11657=DIRECTION('ref_axis',(0.8,0.,-0.6));
#11658=DIRECTION('',(0.,1.,0.));
#11659=DIRECTION('',(-0.8,0.,0.6));
#11660=DIRECTION('center_axis',(0.,0.,1.));
#11661=DIRECTION('ref_axis',(1.,0.,0.));
#11662=DIRECTION('',(0.,1.,0.));
#11663=DIRECTION('',(-1.,0.,0.));
#11664=DIRECTION('center_axis',(-0.6,0.,0.8));
#11665=DIRECTION('ref_axis',(0.8,0.,0.6));
#11666=DIRECTION('',(0.,1.,0.));
#11667=DIRECTION('',(-0.8,0.,-0.6));
#11668=DIRECTION('center_axis',(-0.936329177569044,0.,0.351123441588392));
#11669=DIRECTION('ref_axis',(0.351123441588392,0.,0.936329177569044));
#11670=DIRECTION('',(-0.351123441588392,0.,-0.936329177569044));
#11671=DIRECTION('center_axis',(0.,1.,0.));
#11672=DIRECTION('ref_axis',(1.,0.,0.));
#11673=DIRECTION('axis',(0.,0.,1.));
#11674=DIRECTION('refdir',(1.,0.,0.));
#11675=DIRECTION('center_axis',(0.,1.,0.));
#11676=DIRECTION('ref_axis',(0.707106781186548,0.,0.707106781186548));
#11677=DIRECTION('center_axis',(0.,-1.,0.));
#11678=DIRECTION('ref_axis',(0.707106781186548,0.,0.707106781186548));
#11679=DIRECTION('',(0.,1.,0.));
#11680=DIRECTION('center_axis',(0.,1.,0.));
#11681=DIRECTION('ref_axis',(0.707106781186548,0.,0.707106781186548));
#11682=DIRECTION('',(0.,-1.,0.));
#11683=DIRECTION('center_axis',(0.,0.,1.));
#11684=DIRECTION('ref_axis',(1.,0.,0.));
#11685=DIRECTION('',(1.,0.,0.));
#11686=DIRECTION('',(0.,-1.,0.));
#11687=DIRECTION('',(-1.,0.,0.));
#11688=DIRECTION('center_axis',(0.,1.,0.));
#11689=DIRECTION('ref_axis',(0.707106781186549,0.,-0.707106781186546));
#11690=DIRECTION('center_axis',(0.,-1.,0.));
#11691=DIRECTION('ref_axis',(0.707106781186549,0.,-0.707106781186546));
#11692=DIRECTION('',(0.,1.,0.));
#11693=DIRECTION('center_axis',(0.,1.,0.));
#11694=DIRECTION('ref_axis',(0.707106781186549,0.,-0.707106781186546));
#11695=DIRECTION('',(0.,-1.,0.));
#11696=DIRECTION('center_axis',(1.,0.,0.));
#11697=DIRECTION('ref_axis',(0.,0.,-1.));
#11698=DIRECTION('',(0.,0.,1.));
#11699=DIRECTION('',(0.,0.,-1.));
#11700=DIRECTION('center_axis',(0.,1.,0.));
#11701=DIRECTION('ref_axis',(-0.707106781186548,0.,0.707106781186547));
#11702=DIRECTION('center_axis',(0.,-1.,0.));
#11703=DIRECTION('ref_axis',(-0.707106781186548,0.,0.707106781186547));
#11704=DIRECTION('',(0.,1.,0.));
#11705=DIRECTION('center_axis',(0.,1.,0.));
#11706=DIRECTION('ref_axis',(-0.707106781186548,0.,0.707106781186547));
#11707=DIRECTION('center_axis',(-1.,0.,0.));
#11708=DIRECTION('ref_axis',(0.,0.,1.));
#11709=DIRECTION('',(0.,0.,1.));
#11710=DIRECTION('',(0.,-1.,0.));
#11711=DIRECTION('',(0.,0.,-1.));
#11712=DIRECTION('center_axis',(0.,1.,0.));
#11713=DIRECTION('ref_axis',(-0.707106781186545,0.,-0.70710678118655));
#11714=DIRECTION('center_axis',(0.,-1.,0.));
#11715=DIRECTION('ref_axis',(-0.707106781186545,0.,-0.70710678118655));
#11716=DIRECTION('',(0.,1.,0.));
#11717=DIRECTION('center_axis',(0.,1.,0.));
#11718=DIRECTION('ref_axis',(-0.707106781186545,0.,-0.70710678118655));
#11719=DIRECTION('center_axis',(0.,0.,-1.));
#11720=DIRECTION('ref_axis',(-1.,0.,0.));
#11721=DIRECTION('',(1.,0.,0.));
#11722=DIRECTION('',(-1.,0.,0.));
#11723=DIRECTION('center_axis',(0.,1.,0.));
#11724=DIRECTION('ref_axis',(0.707106781186548,0.,-0.707106781186547));
#11725=DIRECTION('center_axis',(0.,-1.,0.));
#11726=DIRECTION('ref_axis',(0.707106781186548,0.,-0.707106781186547));
#11727=DIRECTION('',(0.,1.,0.));
#11728=DIRECTION('center_axis',(0.,1.,0.));
#11729=DIRECTION('ref_axis',(0.707106781186548,0.,-0.707106781186547));
#11730=DIRECTION('',(0.,-1.,0.));
#11731=DIRECTION('center_axis',(1.,0.,0.));
#11732=DIRECTION('ref_axis',(0.,0.,-1.));
#11733=DIRECTION('',(0.,0.,-1.));
#11734=DIRECTION('',(0.,-1.,0.));
#11735=DIRECTION('',(0.,0.,1.));
#11736=DIRECTION('center_axis',(0.,1.,0.));
#11737=DIRECTION('ref_axis',(-0.707106781186544,0.,-0.707106781186551));
#11738=DIRECTION('center_axis',(0.,-1.,0.));
#11739=DIRECTION('ref_axis',(-0.707106781186544,0.,-0.707106781186551));
#11740=DIRECTION('',(0.,1.,0.));
#11741=DIRECTION('center_axis',(0.,1.,0.));
#11742=DIRECTION('ref_axis',(-0.707106781186544,0.,-0.707106781186551));
#11743=DIRECTION('',(0.,-1.,0.));
#11744=DIRECTION('center_axis',(0.,0.,-1.));
#11745=DIRECTION('ref_axis',(-1.,0.,0.));
#11746=DIRECTION('',(1.,0.,0.));
#11747=DIRECTION('',(-1.,0.,0.));
#11748=DIRECTION('center_axis',(0.,1.,0.));
#11749=DIRECTION('ref_axis',(0.707106781186548,0.,0.707106781186547));
#11750=DIRECTION('center_axis',(0.,-1.,0.));
#11751=DIRECTION('ref_axis',(0.707106781186548,0.,0.707106781186547));
#11752=DIRECTION('',(0.,1.,0.));
#11753=DIRECTION('center_axis',(0.,1.,0.));
#11754=DIRECTION('ref_axis',(0.707106781186548,0.,0.707106781186547));
#11755=DIRECTION('center_axis',(0.,0.,1.));
#11756=DIRECTION('ref_axis',(1.,0.,0.));
#11757=DIRECTION('',(1.,0.,0.));
#11758=DIRECTION('',(0.,-1.,0.));
#11759=DIRECTION('',(-1.,0.,0.));
#11760=DIRECTION('center_axis',(0.,1.,0.));
#11761=DIRECTION('ref_axis',(-0.707106781186549,0.,0.707106781186546));
#11762=DIRECTION('center_axis',(0.,-1.,0.));
#11763=DIRECTION('ref_axis',(-0.707106781186549,0.,0.707106781186546));
#11764=DIRECTION('',(0.,1.,0.));
#11765=DIRECTION('center_axis',(0.,1.,0.));
#11766=DIRECTION('ref_axis',(-0.707106781186549,0.,0.707106781186546));
#11767=DIRECTION('center_axis',(-1.,0.,0.));
#11768=DIRECTION('ref_axis',(0.,0.,1.));
#11769=DIRECTION('',(0.,0.,-1.));
#11770=DIRECTION('',(0.,0.,1.));
#11771=DIRECTION('center_axis',(0.,1.,0.));
#11772=DIRECTION('ref_axis',(0.707106781186549,0.,0.707106781186546));
#11773=DIRECTION('center_axis',(0.,-1.,0.));
#11774=DIRECTION('ref_axis',(0.707106781186549,0.,0.707106781186546));
#11775=DIRECTION('',(0.,1.,0.));
#11776=DIRECTION('center_axis',(0.,1.,0.));
#11777=DIRECTION('ref_axis',(0.707106781186549,0.,0.707106781186546));
#11778=DIRECTION('',(0.,-1.,0.));
#11779=DIRECTION('center_axis',(0.,0.,1.));
#11780=DIRECTION('ref_axis',(1.,0.,0.));
#11781=DIRECTION('',(1.,0.,0.));
#11782=DIRECTION('',(0.,-1.,0.));
#11783=DIRECTION('',(-1.,0.,0.));
#11784=DIRECTION('center_axis',(0.,1.,0.));
#11785=DIRECTION('ref_axis',(0.707106781186549,0.,-0.707106781186546));
#11786=DIRECTION('center_axis',(0.,-1.,0.));
#11787=DIRECTION('ref_axis',(0.707106781186549,0.,-0.707106781186546));
#11788=DIRECTION('',(0.,1.,0.));
#11789=DIRECTION('center_axis',(0.,1.,0.));
#11790=DIRECTION('ref_axis',(0.707106781186549,0.,-0.707106781186546));
#11791=DIRECTION('',(0.,-1.,0.));
#11792=DIRECTION('center_axis',(1.,0.,0.));
#11793=DIRECTION('ref_axis',(0.,0.,-1.));
#11794=DIRECTION('',(0.,0.,1.));
#11795=DIRECTION('',(0.,0.,-1.));
#11796=DIRECTION('center_axis',(0.,1.,0.));
#11797=DIRECTION('ref_axis',(-0.707106781186549,0.,0.707106781186546));
#11798=DIRECTION('center_axis',(0.,-1.,0.));
#11799=DIRECTION('ref_axis',(-0.707106781186549,0.,0.707106781186546));
#11800=DIRECTION('',(0.,1.,0.));
#11801=DIRECTION('center_axis',(0.,1.,0.));
#11802=DIRECTION('ref_axis',(-0.707106781186549,0.,0.707106781186546));
#11803=DIRECTION('center_axis',(-1.,0.,0.));
#11804=DIRECTION('ref_axis',(0.,0.,1.));
#11805=DIRECTION('',(0.,0.,1.));
#11806=DIRECTION('',(0.,-1.,0.));
#11807=DIRECTION('',(0.,0.,-1.));
#11808=DIRECTION('center_axis',(0.,1.,0.));
#11809=DIRECTION('ref_axis',(-0.707106781186546,0.,-0.707106781186549));
#11810=DIRECTION('center_axis',(0.,-1.,0.));
#11811=DIRECTION('ref_axis',(-0.707106781186546,0.,-0.707106781186549));
#11812=DIRECTION('',(0.,1.,0.));
#11813=DIRECTION('center_axis',(0.,1.,0.));
#11814=DIRECTION('ref_axis',(-0.707106781186546,0.,-0.707106781186549));
#11815=DIRECTION('center_axis',(0.,0.,-1.));
#11816=DIRECTION('ref_axis',(-1.,0.,0.));
#11817=DIRECTION('',(1.,0.,0.));
#11818=DIRECTION('',(-1.,0.,0.));
#11819=DIRECTION('center_axis',(0.,1.,0.));
#11820=DIRECTION('ref_axis',(1.,0.,0.));
#11821=DIRECTION('center_axis',(0.,1.,0.));
#11822=DIRECTION('ref_axis',(1.,0.,0.));
#11823=DIRECTION('',(0.,1.,0.));
#11824=DIRECTION('center_axis',(0.,-1.,0.));
#11825=DIRECTION('ref_axis',(1.,0.,0.));
#11826=DIRECTION('center_axis',(0.,1.,0.));
#11827=DIRECTION('ref_axis',(1.,0.,0.));
#11828=DIRECTION('center_axis',(0.,1.,0.));
#11829=DIRECTION('ref_axis',(1.,0.,0.));
#11830=DIRECTION('',(0.,1.,0.));
#11831=DIRECTION('center_axis',(0.,-1.,0.));
#11832=DIRECTION('ref_axis',(1.,0.,0.));
#11833=DIRECTION('center_axis',(0.,1.,0.));
#11834=DIRECTION('ref_axis',(1.,0.,0.));
#11835=DIRECTION('center_axis',(0.,1.,0.));
#11836=DIRECTION('ref_axis',(1.,0.,0.));
#11837=DIRECTION('',(0.,1.,0.));
#11838=DIRECTION('center_axis',(0.,-1.,0.));
#11839=DIRECTION('ref_axis',(1.,0.,0.));
#11840=DIRECTION('center_axis',(0.,1.,0.));
#11841=DIRECTION('ref_axis',(1.,0.,0.));
#11842=DIRECTION('center_axis',(0.,1.,0.));
#11843=DIRECTION('ref_axis',(1.,0.,0.));
#11844=DIRECTION('',(0.,1.,0.));
#11845=DIRECTION('center_axis',(0.,-1.,0.));
#11846=DIRECTION('ref_axis',(1.,0.,0.));
#11847=DIRECTION('center_axis',(0.,1.,0.));
#11848=DIRECTION('ref_axis',(1.,0.,0.));
#11849=DIRECTION('center_axis',(0.,1.,0.));
#11850=DIRECTION('ref_axis',(1.,0.,0.));
#11851=DIRECTION('',(0.,1.,0.));
#11852=DIRECTION('center_axis',(0.,-1.,0.));
#11853=DIRECTION('ref_axis',(1.,0.,0.));
#11854=DIRECTION('center_axis',(0.,1.,0.));
#11855=DIRECTION('ref_axis',(1.,0.,0.));
#11856=DIRECTION('center_axis',(0.,1.,0.));
#11857=DIRECTION('ref_axis',(1.,0.,0.));
#11858=DIRECTION('',(0.,1.,0.));
#11859=DIRECTION('center_axis',(0.,-1.,0.));
#11860=DIRECTION('ref_axis',(1.,0.,0.));
#11861=DIRECTION('center_axis',(-1.,0.,0.));
#11862=DIRECTION('ref_axis',(0.,0.,1.));
#11863=DIRECTION('',(0.,0.,-1.));
#11864=DIRECTION('',(0.,1.,0.));
#11865=DIRECTION('',(0.,0.,1.));
#11866=DIRECTION('',(0.,1.,0.));
#11867=DIRECTION('center_axis',(0.,0.,-1.));
#11868=DIRECTION('ref_axis',(-1.,0.,0.));
#11869=DIRECTION('',(1.,0.,0.));
#11870=DIRECTION('',(-1.,0.,0.));
#11871=DIRECTION('',(0.,1.,0.));
#11872=DIRECTION('center_axis',(1.,0.,0.));
#11873=DIRECTION('ref_axis',(0.,0.,-1.));
#11874=DIRECTION('',(0.,0.,1.));
#11875=DIRECTION('',(0.,0.,-1.));
#11876=DIRECTION('',(0.,1.,0.));
#11877=DIRECTION('center_axis',(0.936329177569044,0.,0.351123441588392));
#11878=DIRECTION('ref_axis',(0.351123441588392,0.,-0.936329177569044));
#11879=DIRECTION('',(-0.351123441588392,0.,0.936329177569044));
#11880=DIRECTION('',(0.351123441588392,0.,-0.936329177569044));
#11881=DIRECTION('',(0.,1.,0.));
#11882=DIRECTION('center_axis',(0.6,0.,0.8));
#11883=DIRECTION('ref_axis',(0.8,0.,-0.6));
#11884=DIRECTION('',(-0.8,0.,0.6));
#11885=DIRECTION('',(0.8,0.,-0.6));
#11886=DIRECTION('',(0.,1.,0.));
#11887=DIRECTION('center_axis',(0.,0.,1.));
#11888=DIRECTION('ref_axis',(1.,0.,0.));
#11889=DIRECTION('',(-1.,0.,0.));
#11890=DIRECTION('',(1.,0.,0.));
#11891=DIRECTION('',(0.,1.,0.));
#11892=DIRECTION('center_axis',(-0.6,0.,0.8));
#11893=DIRECTION('ref_axis',(0.8,0.,0.6));
#11894=DIRECTION('',(-0.8,0.,-0.6));
#11895=DIRECTION('',(0.8,0.,0.6));
#11896=DIRECTION('',(0.,1.,0.));
#11897=DIRECTION('center_axis',(-0.936329177569044,0.,0.351123441588392));
#11898=DIRECTION('ref_axis',(0.351123441588392,0.,0.936329177569044));
#11899=DIRECTION('',(-0.351123441588392,0.,-0.936329177569044));
#11900=DIRECTION('',(0.351123441588392,0.,0.936329177569044));
#11901=DIRECTION('center_axis',(0.,1.,0.));
#11902=DIRECTION('ref_axis',(0.,0.,1.));
#11903=DIRECTION('center_axis',(0.,1.,0.));
#11904=DIRECTION('ref_axis',(1.,0.,0.));
#11905=DIRECTION('axis',(0.,0.,1.));
#11906=DIRECTION('refdir',(1.,0.,0.));
#11907=DIRECTION('center_axis',(0.70710678118655,-0.707106781186545,0.));
#11908=DIRECTION('ref_axis',(0.,0.,-1.));
#11909=DIRECTION('',(0.,0.,-1.));
#11910=DIRECTION('',(0.577350269189622,0.577350269189625,-0.57735026918963));
#11911=DIRECTION('',(0.,0.,1.));
#11912=DIRECTION('',(0.678598344545843,0.678598344545847,0.281084637714829));
#11913=DIRECTION('center_axis',(0.,-0.70710678118655,-0.707106781186545));
#11914=DIRECTION('ref_axis',(-1.,0.,0.));
#11915=DIRECTION('',(-1.,0.,0.));
#11916=DIRECTION('',(-0.577350269189622,0.577350269189625,-0.57735026918963));
#11917=DIRECTION('',(1.,0.,0.));
#11918=DIRECTION('center_axis',(-0.70710678118655,-0.707106781186545,0.));
#11919=DIRECTION('ref_axis',(0.,0.,1.));
#11920=DIRECTION('',(0.,0.,1.));
#11921=DIRECTION('',(-0.678598344545839,0.678598344545844,0.281084637714847));
#11922=DIRECTION('',(0.,0.,-1.));
#11923=DIRECTION('center_axis',(-0.499999999999994,-0.707106781186556,0.499999999999993));
#11924=DIRECTION('ref_axis',(0.707106781186547,-1.66533453693739E-16,0.707106781186548));
#11925=DIRECTION('',(0.707106781186547,0.,0.707106781186548));
#11926=DIRECTION('',(-0.281084637714836,0.678598344545841,0.678598344545847));
#11927=DIRECTION('',(-0.707106781186547,0.,-0.707106781186548));
#11928=DIRECTION('center_axis',(0.,-0.70710678118655,0.707106781186545));
#11929=DIRECTION('ref_axis',(1.,0.,0.));
#11930=DIRECTION('',(-1.,0.,0.));
#11931=DIRECTION('',(1.,0.,0.));
#11932=DIRECTION('',(0.281084637714827,0.678598344545843,0.678598344545848));
#11933=DIRECTION('center_axis',(0.499999999999997,-0.707106781186553,0.499999999999996));
#11934=DIRECTION('ref_axis',(0.707106781186547,1.66533453693763E-16,-0.707106781186548));
#11935=DIRECTION('',(-0.707106781186547,0.,0.707106781186548));
#11936=DIRECTION('',(0.707106781186547,0.,-0.707106781186548));
#11937=DIRECTION('center_axis',(0.,0.,1.));
#11938=DIRECTION('ref_axis',(-1.,0.,0.));
#11939=DIRECTION('',(0.,-1.,0.));
#11940=DIRECTION('',(-1.,0.,0.));
#11941=DIRECTION('',(0.,-1.,0.));
#11942=DIRECTION('center_axis',(0.707106781186548,0.,0.707106781186547));
#11943=DIRECTION('ref_axis',(-0.707106781186547,0.,0.707106781186548));
#11944=DIRECTION('',(0.,-1.,0.));
#11945=DIRECTION('',(-0.707106781186547,0.,0.707106781186548));
#11946=DIRECTION('center_axis',(1.,0.,0.));
#11947=DIRECTION('ref_axis',(0.,0.,1.));
#11948=DIRECTION('',(0.,-1.,0.));
#11949=DIRECTION('',(0.,0.,1.));
#11950=DIRECTION('center_axis',(0.,-1.,0.));
#11951=DIRECTION('ref_axis',(0.,0.,-1.));
#11952=DIRECTION('center_axis',(0.,1.,0.));
#11953=DIRECTION('ref_axis',(1.,0.,0.));
#11954=DIRECTION('center_axis',(0.,1.,0.));
#11955=DIRECTION('ref_axis',(1.,0.,0.));
#11956=DIRECTION('center_axis',(0.,1.,0.));
#11957=DIRECTION('ref_axis',(1.,0.,0.));
#11958=DIRECTION('center_axis',(0.,1.,0.));
#11959=DIRECTION('ref_axis',(1.,0.,0.));
#11960=DIRECTION('center_axis',(0.,-1.,0.));
#11961=DIRECTION('ref_axis',(1.,0.,0.));
#11962=DIRECTION('center_axis',(0.,-1.,0.));
#11963=DIRECTION('ref_axis',(1.,0.,0.));
#11964=DIRECTION('',(0.,-1.,0.));
#11965=DIRECTION('center_axis',(0.,-1.,0.));
#11966=DIRECTION('ref_axis',(1.,0.,0.));
#11967=DIRECTION('center_axis',(0.,-1.,0.));
#11968=DIRECTION('ref_axis',(1.,0.,0.));
#11969=DIRECTION('',(0.,-1.,0.));
#11970=DIRECTION('center_axis',(0.,-1.,0.));
#11971=DIRECTION('ref_axis',(1.,0.,0.));
#11972=DIRECTION('center_axis',(0.,-1.,0.));
#11973=DIRECTION('ref_axis',(1.,0.,0.));
#11974=DIRECTION('',(0.,-1.,0.));
#11975=DIRECTION('center_axis',(0.,-1.,0.));
#11976=DIRECTION('ref_axis',(1.,0.,0.));
#11977=DIRECTION('center_axis',(0.,-1.,0.));
#11978=DIRECTION('ref_axis',(1.,0.,0.));
#11979=DIRECTION('',(0.,-1.,0.));
#11980=DIRECTION('center_axis',(0.,0.,-1.));
#11981=DIRECTION('ref_axis',(1.,0.,0.));
#11982=DIRECTION('',(0.,-1.,0.));
#11983=DIRECTION('',(1.,0.,0.));
#11984=DIRECTION('center_axis',(-1.,0.,0.));
#11985=DIRECTION('ref_axis',(0.,0.,-1.));
#11986=DIRECTION('',(0.,-1.,0.));
#11987=DIRECTION('',(0.,0.,-1.));
#11988=DIRECTION('center_axis',(-0.707106781186548,0.,0.707106781186547));
#11989=DIRECTION('ref_axis',(-0.707106781186547,0.,-0.707106781186548));
#11990=DIRECTION('',(-0.707106781186547,0.,-0.707106781186548));
#11991=DIRECTION('center_axis',(0.,1.,0.));
#11992=DIRECTION('ref_axis',(1.,0.,0.));
#11993=DIRECTION('axis',(0.,0.,1.));
#11994=DIRECTION('refdir',(1.,0.,0.));
#11995=DIRECTION('center_axis',(0.,0.,1.));
#11996=DIRECTION('ref_axis',(1.,0.,0.));
#11997=DIRECTION('center_axis',(0.,0.,1.));
#11998=DIRECTION('ref_axis',(1.,0.,0.));
#11999=DIRECTION('center_axis',(0.,0.,1.));
#12000=DIRECTION('ref_axis',(1.,0.,0.));
#12001=DIRECTION('center_axis',(0.,0.,-1.));
#12002=DIRECTION('ref_axis',(1.,0.,0.));
#12003=DIRECTION('center_axis',(0.,0.,-1.));
#12004=DIRECTION('ref_axis',(1.,0.,0.));
#12005=DIRECTION('center_axis',(0.,0.,1.));
#12006=DIRECTION('ref_axis',(1.,-1.2787674710755E-12,0.));
#12007=DIRECTION('center_axis',(0.,0.,1.));
#12008=DIRECTION('ref_axis',(1.,-1.2787674710755E-12,0.));
#12009=DIRECTION('center_axis',(0.,0.,-1.));
#12010=DIRECTION('ref_axis',(1.,-1.2787674710755E-12,0.));
#12011=DIRECTION('center_axis',(0.866025403784438,0.5,0.));
#12012=DIRECTION('ref_axis',(0.5,-0.866025403784438,0.));
#12013=DIRECTION('',(0.5,-0.866025403784438,0.));
#12014=DIRECTION('',(0.,0.,-1.));
#12015=DIRECTION('',(0.5,-0.866025403784438,0.));
#12016=DIRECTION('',(0.,0.,-1.));
#12017=DIRECTION('center_axis',(0.,1.,0.));
#12018=DIRECTION('ref_axis',(1.,0.,0.));
#12019=DIRECTION('',(1.,0.,0.));
#12020=DIRECTION('',(0.,0.,-1.));
#12021=DIRECTION('',(1.,0.,0.));
#12022=DIRECTION('center_axis',(-0.866025403784438,0.500000000000001,0.));
#12023=DIRECTION('ref_axis',(0.500000000000001,0.866025403784438,0.));
#12024=DIRECTION('',(0.500000000000001,0.866025403784438,0.));
#12025=DIRECTION('',(0.,0.,-1.));
#12026=DIRECTION('',(0.500000000000001,0.866025403784438,0.));
#12027=DIRECTION('center_axis',(-0.866025403784439,-0.499999999999999,0.));
#12028=DIRECTION('ref_axis',(-0.499999999999999,0.866025403784439,0.));
#12029=DIRECTION('',(-0.499999999999999,0.866025403784439,0.));
#12030=DIRECTION('',(0.,0.,-1.));
#12031=DIRECTION('',(-0.499999999999999,0.866025403784439,0.));
#12032=DIRECTION('center_axis',(0.,-1.,0.));
#12033=DIRECTION('ref_axis',(-1.,0.,0.));
#12034=DIRECTION('',(-1.,0.,0.));
#12035=DIRECTION('',(0.,0.,-1.));
#12036=DIRECTION('',(-1.,0.,0.));
#12037=DIRECTION('center_axis',(0.866025403784439,-0.5,0.));
#12038=DIRECTION('ref_axis',(-0.5,-0.866025403784439,0.));
#12039=DIRECTION('',(-0.5,-0.866025403784439,0.));
#12040=DIRECTION('',(-0.5,-0.866025403784439,0.));
#12041=DIRECTION('center_axis',(0.,0.,-1.));
#12042=DIRECTION('ref_axis',(-1.,0.,0.));
#12043=DIRECTION('center_axis',(0.,0.,1.));
#12044=DIRECTION('ref_axis',(1.,0.,0.));
#12045=DIRECTION('center_axis',(0.,0.,1.));
#12046=DIRECTION('ref_axis',(1.,0.,0.));
#12047=DIRECTION('center_axis',(0.,0.,-1.));
#12048=DIRECTION('ref_axis',(-1.,0.,0.));
#12049=DIRECTION('center_axis',(0.,0.,1.));
#12050=DIRECTION('ref_axis',(1.,0.,0.));
#12051=DIRECTION('center_axis',(0.,0.,1.));
#12052=DIRECTION('ref_axis',(1.,0.,0.));
#12053=DIRECTION('',(0.707106781186549,8.65956056235496E-17,-0.707106781186546));
#12054=DIRECTION('center_axis',(0.,0.,-1.));
#12055=DIRECTION('ref_axis',(1.,0.,0.));
#12056=DIRECTION('',(0.70710678118654,-8.65956056235484E-17,0.707106781186556));
#12057=DIRECTION('center_axis',(0.,0.,1.));
#12058=DIRECTION('ref_axis',(1.,0.,0.));
#12059=DIRECTION('center_axis',(0.,0.,1.));
#12060=DIRECTION('ref_axis',(1.,0.,0.));
#12061=DIRECTION('axis',(0.,0.,1.));
#12062=DIRECTION('refdir',(1.,0.,0.));
#12063=DIRECTION('center_axis',(0.,0.,1.));
#12064=DIRECTION('ref_axis',(-0.707106781186546,-0.707106781186549,0.));
#12065=DIRECTION('center_axis',(0.,0.,-1.));
#12066=DIRECTION('ref_axis',(-0.707106781186546,-0.707106781186549,0.));
#12067=DIRECTION('',(0.,0.,-1.));
#12068=DIRECTION('center_axis',(0.,0.,1.));
#12069=DIRECTION('ref_axis',(-0.707106781186546,-0.707106781186549,0.));
#12070=DIRECTION('',(0.,0.,1.));
#12071=DIRECTION('center_axis',(0.,0.,1.));
#12072=DIRECTION('ref_axis',(-0.707106781186546,-0.707106781186549,0.));
#12073=DIRECTION('center_axis',(0.,0.,1.));
#12074=DIRECTION('ref_axis',(1.,0.,0.));
#12075=DIRECTION('center_axis',(0.,0.,-1.));
#12076=DIRECTION('ref_axis',(1.,0.,0.));
#12077=DIRECTION('',(0.,-1.,0.));
#12078=DIRECTION('center_axis',(0.,0.,1.));
#12079=DIRECTION('ref_axis',(0.707106781186546,-0.707106781186549,0.));
#12080=DIRECTION('center_axis',(0.,0.,-1.));
#12081=DIRECTION('ref_axis',(0.707106781186546,-0.707106781186549,0.));
#12082=DIRECTION('center_axis',(0.,0.,1.));
#12083=DIRECTION('ref_axis',(0.707106781186546,-0.707106781186549,0.));
#12084=DIRECTION('',(0.,0.,-1.));
#12085=DIRECTION('center_axis',(0.,0.,1.));
#12086=DIRECTION('ref_axis',(0.707106781186546,-0.707106781186549,0.));
#12087=DIRECTION('',(0.,0.,1.));
#12088=DIRECTION('center_axis',(0.,-1.,0.));
#12089=DIRECTION('ref_axis',(1.,0.,0.));
#12090=DIRECTION('',(1.,0.,0.));
#12091=DIRECTION('',(1.,0.,0.));
#12092=DIRECTION('center_axis',(0.,0.,1.));
#12093=DIRECTION('ref_axis',(0.707106781186546,0.707106781186549,0.));
#12094=DIRECTION('center_axis',(0.,0.,-1.));
#12095=DIRECTION('ref_axis',(0.707106781186546,0.707106781186549,0.));
#12096=DIRECTION('',(0.,0.,-1.));
#12097=DIRECTION('center_axis',(0.,0.,1.));
#12098=DIRECTION('ref_axis',(0.707106781186546,0.707106781186549,0.));
#12099=DIRECTION('',(0.,0.,1.));
#12100=DIRECTION('center_axis',(0.,0.,1.));
#12101=DIRECTION('ref_axis',(0.707106781186546,0.707106781186549,0.));
#12102=DIRECTION('center_axis',(0.,0.,1.));
#12103=DIRECTION('ref_axis',(1.,0.,0.));
#12104=DIRECTION('center_axis',(0.,0.,-1.));
#12105=DIRECTION('ref_axis',(1.,0.,0.));
#12106=DIRECTION('',(0.,1.,0.));
#12107=DIRECTION('center_axis',(0.,0.,1.));
#12108=DIRECTION('ref_axis',(-0.707106781186546,0.707106781186549,0.));
#12109=DIRECTION('center_axis',(0.,0.,-1.));
#12110=DIRECTION('ref_axis',(-0.707106781186546,0.707106781186549,0.));
#12111=DIRECTION('center_axis',(0.,0.,1.));
#12112=DIRECTION('ref_axis',(-0.707106781186546,0.707106781186549,0.));
#12113=DIRECTION('',(0.,0.,-1.));
#12114=DIRECTION('center_axis',(0.,0.,1.));
#12115=DIRECTION('ref_axis',(-0.707106781186546,0.707106781186549,0.));
#12116=DIRECTION('',(0.,0.,1.));
#12117=DIRECTION('center_axis',(0.,1.,0.));
#12118=DIRECTION('ref_axis',(-1.,0.,0.));
#12119=DIRECTION('',(-1.,0.,0.));
#12120=DIRECTION('',(-1.,0.,0.));
#12121=DIRECTION('',(0.,0.,1.));
#12122=DIRECTION('',(-1.,0.,0.));
#12123=DIRECTION('',(0.,0.,-1.));
#12124=DIRECTION('',(1.,0.,0.));
#12125=DIRECTION('center_axis',(1.,0.,0.));
#12126=DIRECTION('ref_axis',(0.,0.,1.));
#12127=DIRECTION('',(0.,-1.,0.));
#12128=DIRECTION('',(0.,0.,1.));
#12129=DIRECTION('',(0.,-1.,0.));
#12130=DIRECTION('center_axis',(0.,0.,-1.));
#12131=DIRECTION('ref_axis',(1.,0.,0.));
#12132=DIRECTION('',(0.,-1.,0.));
#12133=DIRECTION('',(1.,0.,0.));
#12134=DIRECTION('center_axis',(-1.,0.,0.));
#12135=DIRECTION('ref_axis',(0.,0.,-1.));
#12136=DIRECTION('',(0.,-1.,0.));
#12137=DIRECTION('',(0.,0.,-1.));
#12138=DIRECTION('center_axis',(0.,0.,1.));
#12139=DIRECTION('ref_axis',(-1.,0.,0.));
#12140=DIRECTION('',(-1.,0.,0.));
#12141=DIRECTION('center_axis',(0.,-1.,0.));
#12142=DIRECTION('ref_axis',(0.,0.,-1.));
#12143=DIRECTION('center_axis',(1.,0.,0.));
#12144=DIRECTION('ref_axis',(0.,0.,-1.));
#12145=DIRECTION('center_axis',(1.,0.,0.));
#12146=DIRECTION('ref_axis',(0.,0.,-1.));
#12147=DIRECTION('',(1.,0.,0.));
#12148=DIRECTION('center_axis',(1.,0.,0.));
#12149=DIRECTION('ref_axis',(0.,0.,-1.));
#12150=DIRECTION('',(1.,0.,0.));
#12151=DIRECTION('center_axis',(-1.,0.,0.));
#12152=DIRECTION('ref_axis',(0.,0.,-1.));
#12153=DIRECTION('center_axis',(1.,0.,0.));
#12154=DIRECTION('ref_axis',(0.,0.,-1.));
#12155=DIRECTION('center_axis',(1.,0.,0.));
#12156=DIRECTION('ref_axis',(0.,0.,-1.));
#12157=DIRECTION('',(1.,0.,0.));
#12158=DIRECTION('center_axis',(1.,0.,0.));
#12159=DIRECTION('ref_axis',(0.,0.,-1.));
#12160=DIRECTION('',(1.,0.,0.));
#12161=DIRECTION('center_axis',(-1.,0.,0.));
#12162=DIRECTION('ref_axis',(0.,0.,-1.));
#12163=DIRECTION('center_axis',(0.,0.,-1.));
#12164=DIRECTION('ref_axis',(1.,0.,0.));
#12165=DIRECTION('center_axis',(0.,0.,-1.));
#12166=DIRECTION('ref_axis',(1.,0.,0.));
#12167=DIRECTION('',(0.,0.,-1.));
#12168=DIRECTION('',(0.,0.,-1.));
#12169=DIRECTION('',(0.,0.,-1.));
#12170=DIRECTION('center_axis',(0.,0.,1.));
#12171=DIRECTION('ref_axis',(1.,0.,0.));
#12172=DIRECTION('center_axis',(0.,0.,1.));
#12173=DIRECTION('ref_axis',(1.,0.,0.));
#12174=DIRECTION('',(0.,-1.,0.));
#12175=DIRECTION('center_axis',(0.,0.,1.));
#12176=DIRECTION('ref_axis',(1.,0.,0.));
#12177=DIRECTION('center_axis',(0.,0.,1.));
#12178=DIRECTION('ref_axis',(1.,0.,0.));
#12179=DIRECTION('center_axis',(0.,0.,1.));
#12180=DIRECTION('ref_axis',(1.,0.,0.));
#12181=DIRECTION('center_axis',(0.,0.,-1.));
#12182=DIRECTION('ref_axis',(1.,0.,0.));
#12183=DIRECTION('center_axis',(0.,0.,1.));
#12184=DIRECTION('ref_axis',(1.,0.,0.));
#12185=DIRECTION('',(0.,1.,0.));
#12186=DIRECTION('center_axis',(0.,0.,1.));
#12187=DIRECTION('ref_axis',(1.,0.,0.));
#12188=DIRECTION('center_axis',(0.,0.,1.));
#12189=DIRECTION('ref_axis',(1.,0.,0.));
#12190=DIRECTION('center_axis',(0.,0.,-1.));
#12191=DIRECTION('ref_axis',(1.,0.,0.));
#12192=DIRECTION('center_axis',(0.,0.,1.));
#12193=DIRECTION('ref_axis',(1.,0.,0.));
#12194=DIRECTION('center_axis',(0.,0.,1.));
#12195=DIRECTION('ref_axis',(1.,0.,0.));
#12196=DIRECTION('',(0.,0.,-1.));
#12197=DIRECTION('center_axis',(0.,0.,-1.));
#12198=DIRECTION('ref_axis',(1.,0.,0.));
#12199=DIRECTION('center_axis',(0.,0.,-1.));
#12200=DIRECTION('ref_axis',(1.,0.,0.));
#12201=DIRECTION('center_axis',(0.,0.,1.));
#12202=DIRECTION('ref_axis',(1.,0.,0.));
#12203=DIRECTION('center_axis',(0.,0.,1.));
#12204=DIRECTION('ref_axis',(1.,0.,0.));
#12205=DIRECTION('',(0.,1.,0.));
#12206=DIRECTION('center_axis',(0.,0.,1.));
#12207=DIRECTION('ref_axis',(1.,0.,0.));
#12208=DIRECTION('',(0.,-1.,0.));
#12209=DIRECTION('center_axis',(1.,0.,0.));
#12210=DIRECTION('ref_axis',(0.,1.,0.));
#12211=DIRECTION('',(0.,1.,0.));
#12212=DIRECTION('center_axis',(-1.,0.,0.));
#12213=DIRECTION('ref_axis',(0.,-1.,0.));
#12214=DIRECTION('',(0.,-1.,0.));
#12215=DIRECTION('center_axis',(0.,0.,1.));
#12216=DIRECTION('ref_axis',(1.,0.,0.));
#12217=DIRECTION('axis',(0.,0.,1.));
#12218=DIRECTION('refdir',(1.,0.,0.));
#12219=DIRECTION('center_axis',(-0.0185160100832464,-0.994867197984037,
0.0994807305260099));
#12220=DIRECTION('ref_axis',(0.933205561217733,0.0185160101174801,0.358865626497753));
#12221=DIRECTION('center_axis',(0.,1.,0.));
#12222=DIRECTION('ref_axis',(1.,0.,0.));
#12223=DIRECTION('axis',(0.,0.,1.));
#12224=DIRECTION('refdir',(1.,0.,0.));
#12225=DIRECTION('center_axis',(0.,0.,1.));
#12226=DIRECTION('ref_axis',(1.,0.,0.));
#12227=DIRECTION('center_axis',(0.,0.,1.));
#12228=DIRECTION('ref_axis',(1.,0.,0.));
#12229=DIRECTION('',(0.,0.,1.));
#12230=DIRECTION('center_axis',(0.,0.,1.));
#12231=DIRECTION('ref_axis',(1.,0.,0.));
#12232=DIRECTION('center_axis',(0.,0.,-1.));
#12233=DIRECTION('ref_axis',(1.,0.,0.));
#12234=DIRECTION('',(-0.707106781186547,8.65956056235493E-17,-0.707106781186548));
#12235=DIRECTION('center_axis',(0.,0.,1.));
#12236=DIRECTION('ref_axis',(1.,0.,0.));
#12237=DIRECTION('center_axis',(0.,0.,-1.));
#12238=DIRECTION('ref_axis',(-1.,0.,0.));
#12239=DIRECTION('center_axis',(0.,0.,1.));
#12240=DIRECTION('ref_axis',(1.,0.,0.));
#12241=DIRECTION('center_axis',(0.,0.,1.));
#12242=DIRECTION('ref_axis',(1.,0.,0.));
#12243=DIRECTION('center_axis',(0.,0.,1.));
#12244=DIRECTION('ref_axis',(1.,0.,0.));
#12245=DIRECTION('',(0.,0.,-1.));
#12246=DIRECTION('center_axis',(0.,0.,-1.));
#12247=DIRECTION('ref_axis',(-1.,0.,0.));
#12248=DIRECTION('center_axis',(0.,0.,1.));
#12249=DIRECTION('ref_axis',(1.,0.,0.));
#12250=DIRECTION('center_axis',(0.,0.,1.));
#12251=DIRECTION('ref_axis',(1.,0.,0.));
#12252=DIRECTION('center_axis',(0.,0.,1.));
#12253=DIRECTION('ref_axis',(1.,0.,0.));
#12254=DIRECTION('',(0.,0.,1.));
#12255=DIRECTION('center_axis',(0.,0.,-1.));
#12256=DIRECTION('ref_axis',(-1.,0.,0.));
#12257=DIRECTION('center_axis',(0.,0.,1.));
#12258=DIRECTION('ref_axis',(1.,0.,0.));
#12259=DIRECTION('center_axis',(0.,0.,1.));
#12260=DIRECTION('ref_axis',(1.,0.,0.));
#12261=DIRECTION('center_axis',(0.,0.,1.));
#12262=DIRECTION('ref_axis',(1.,0.,0.));
#12263=DIRECTION('',(0.70710678118655,8.65956056235497E-17,-0.707106781186545));
#12264=DIRECTION('center_axis',(0.,0.,1.));
#12265=DIRECTION('ref_axis',(1.,0.,0.));
#12266=DIRECTION('center_axis',(0.,0.,1.));
#12267=DIRECTION('ref_axis',(1.,0.,0.));
#12268=DIRECTION('',(0.,0.,-1.));
#12269=DIRECTION('center_axis',(0.,0.,-1.));
#12270=DIRECTION('ref_axis',(1.,0.,0.));
#12271=DIRECTION('',(0.707106781186552,-8.65956056235498E-17,0.707106781186543));
#12272=DIRECTION('center_axis',(0.,0.,1.));
#12273=DIRECTION('ref_axis',(1.,0.,0.));
#12274=DIRECTION('center_axis',(0.,0.,1.));
#12275=DIRECTION('ref_axis',(1.,0.,0.));
#12276=DIRECTION('center_axis',(0.,0.,1.));
#12277=DIRECTION('ref_axis',(1.,0.,0.));
#12278=DIRECTION('center_axis',(0.,0.,1.));
#12279=DIRECTION('ref_axis',(1.,0.,0.));
#12280=DIRECTION('center_axis',(0.,0.,1.));
#12281=DIRECTION('ref_axis',(1.,0.,0.));
#12282=DIRECTION('',(0.,0.,1.));
#12283=DIRECTION('center_axis',(0.,0.,1.));
#12284=DIRECTION('ref_axis',(1.,0.,0.));
#12285=DIRECTION('center_axis',(0.,0.,1.));
#12286=DIRECTION('ref_axis',(1.,0.,0.));
#12287=DIRECTION('center_axis',(0.,0.,1.));
#12288=DIRECTION('ref_axis',(1.,0.,0.));
#12289=DIRECTION('center_axis',(0.,0.,1.));
#12290=DIRECTION('ref_axis',(1.,0.,0.));
#12291=DIRECTION('',(0.,0.,-1.));
#12292=DIRECTION('center_axis',(0.,0.,1.));
#12293=DIRECTION('ref_axis',(1.,0.,0.));
#12294=DIRECTION('center_axis',(0.,0.,1.));
#12295=DIRECTION('ref_axis',(1.,0.,0.));
#12296=DIRECTION('center_axis',(0.,0.,1.));
#12297=DIRECTION('ref_axis',(1.,0.,0.));
#12298=DIRECTION('',(-0.707106781186548,-8.65956056235494E-17,0.707106781186547));
#12299=DIRECTION('axis',(0.,0.,1.));
#12300=DIRECTION('refdir',(1.,0.,0.));
#12301=DIRECTION('center_axis',(-0.707106781186548,-0.707106781186547,0.));
#12302=DIRECTION('ref_axis',(-0.707106781186547,0.707106781186548,0.));
#12303=DIRECTION('',(0.,0.,1.));
#12304=DIRECTION('',(-0.707106781186547,0.707106781186548,0.));
#12305=DIRECTION('',(0.,0.,-1.));
#12306=DIRECTION('',(-0.707106781186547,0.707106781186548,0.));
#12307=DIRECTION('center_axis',(0.707106781186548,0.707106781186547,0.));
#12308=DIRECTION('ref_axis',(0.707106781186547,-0.707106781186548,0.));
#12309=DIRECTION('',(0.,0.,-1.));
#12310=DIRECTION('',(0.707106781186547,-0.707106781186548,0.));
#12311=DIRECTION('',(0.,0.,-1.));
#12312=DIRECTION('',(0.707106781186547,-0.707106781186548,0.));
#12313=DIRECTION('center_axis',(-0.707106781186547,0.707106781186548,0.));
#12314=DIRECTION('ref_axis',(0.707106781186548,0.707106781186547,0.));
#12315=DIRECTION('',(0.707106781186548,0.707106781186547,0.));
#12316=DIRECTION('',(0.707106781186548,0.707106781186547,0.));
#12317=DIRECTION('center_axis',(0.,0.,-1.));
#12318=DIRECTION('ref_axis',(-0.707106781186547,0.707106781186548,0.));
#12319=DIRECTION('center_axis',(0.,0.,-1.));
#12320=DIRECTION('ref_axis',(1.,0.,0.));
#12321=DIRECTION('center_axis',(0.,0.,1.));
#12322=DIRECTION('ref_axis',(1.,0.,0.));
#12323=DIRECTION('center_axis',(0.,0.,1.));
#12324=DIRECTION('ref_axis',(1.,0.,0.));
#12325=DIRECTION('',(-1.,0.,0.));
#12326=DIRECTION('',(0.,1.,0.));
#12327=DIRECTION('',(1.,0.,0.));
#12328=DIRECTION('center_axis',(0.,0.,1.));
#12329=DIRECTION('ref_axis',(1.,0.,0.));
#12330=DIRECTION('',(-0.707106781186548,-0.707106781186548,0.));
#12331=DIRECTION('',(-0.707106781186548,0.707106781186548,0.));
#12332=DIRECTION('',(0.707106781186548,0.707106781186548,0.));
#12333=DIRECTION('center_axis',(0.,0.,1.));
#12334=DIRECTION('ref_axis',(1.,0.,0.));
#12335=DIRECTION('',(-6.12323399573677E-17,-1.,0.));
#12336=DIRECTION('',(-1.,6.12323399573677E-17,0.));
#12337=DIRECTION('',(6.12323399573677E-17,1.,0.));
#12338=DIRECTION('center_axis',(0.,0.,1.));
#12339=DIRECTION('ref_axis',(1.,0.,0.));
#12340=DIRECTION('',(0.707106781186547,-0.707106781186548,0.));
#12341=DIRECTION('',(-0.707106781186548,-0.707106781186547,0.));
#12342=DIRECTION('',(-0.707106781186547,0.707106781186548,0.));
#12343=DIRECTION('center_axis',(0.,0.,1.));
#12344=DIRECTION('ref_axis',(1.,0.,0.));
#12345=DIRECTION('',(1.,-1.22464679914735E-16,0.));
#12346=DIRECTION('',(-1.22464679914735E-16,-1.,0.));
#12347=DIRECTION('',(-1.,1.22464679914735E-16,0.));
#12348=DIRECTION('center_axis',(0.,0.,1.));
#12349=DIRECTION('ref_axis',(1.,0.,0.));
#12350=DIRECTION('',(0.707106781186548,0.707106781186547,0.));
#12351=DIRECTION('',(0.707106781186547,-0.707106781186548,0.));
#12352=DIRECTION('',(-0.707106781186548,-0.707106781186547,0.));
#12353=DIRECTION('center_axis',(0.,0.,1.));
#12354=DIRECTION('ref_axis',(1.,0.,0.));
#12355=DIRECTION('',(1.83697019872103E-16,1.,0.));
#12356=DIRECTION('',(1.,-1.83697019872103E-16,0.));
#12357=DIRECTION('',(-1.83697019872103E-16,-1.,0.));
#12358=DIRECTION('center_axis',(0.,0.,1.));
#12359=DIRECTION('ref_axis',(1.,0.,0.));
#12360=DIRECTION('center_axis',(0.,0.,1.));
#12361=DIRECTION('ref_axis',(1.,0.,0.));
#12362=DIRECTION('center_axis',(0.,0.,-1.));
#12363=DIRECTION('ref_axis',(1.,0.,0.));
#12364=DIRECTION('center_axis',(0.,0.,1.));
#12365=DIRECTION('ref_axis',(1.,0.,0.));
#12366=DIRECTION('center_axis',(0.,0.,-1.));
#12367=DIRECTION('ref_axis',(1.,0.,0.));
#12368=DIRECTION('center_axis',(0.,0.,1.));
#12369=DIRECTION('ref_axis',(1.,0.,0.));
#12370=DIRECTION('center_axis',(-1.,1.83697019872103E-16,0.));
#12371=DIRECTION('ref_axis',(1.83697019872103E-16,1.,0.));
#12372=DIRECTION('',(0.,0.,1.));
#12373=DIRECTION('',(1.83697019872103E-16,1.,0.));
#12374=DIRECTION('',(0.,0.,-1.));
#12375=DIRECTION('center_axis',(1.,-1.83697019872103E-16,0.));
#12376=DIRECTION('ref_axis',(-1.83697019872103E-16,-1.,0.));
#12377=DIRECTION('',(0.,0.,-1.));
#12378=DIRECTION('',(0.,0.,-1.));
#12379=DIRECTION('',(-1.83697019872103E-16,-1.,0.));
#12380=DIRECTION('center_axis',(1.83697019872103E-16,1.,0.));
#12381=DIRECTION('ref_axis',(1.,-1.83697019872103E-16,0.));
#12382=DIRECTION('',(1.,-1.83697019872103E-16,0.));
#12383=DIRECTION('center_axis',(0.,0.,-1.));
#12384=DIRECTION('ref_axis',(1.83697019872103E-16,1.,0.));
#12385=DIRECTION('center_axis',(0.,0.,-1.));
#12386=DIRECTION('ref_axis',(1.,0.,0.));
#12387=DIRECTION('center_axis',(0.,0.,-1.));
#12388=DIRECTION('ref_axis',(1.,0.,0.));
#12389=DIRECTION('center_axis',(0.,0.,1.));
#12390=DIRECTION('ref_axis',(1.,0.,0.));
#12391=DIRECTION('center_axis',(-0.707106781186547,0.707106781186548,0.));
#12392=DIRECTION('ref_axis',(0.707106781186548,0.707106781186547,0.));
#12393=DIRECTION('',(0.,0.,1.));
#12394=DIRECTION('',(0.707106781186548,0.707106781186547,0.));
#12395=DIRECTION('',(0.,0.,-1.));
#12396=DIRECTION('center_axis',(0.707106781186547,-0.707106781186548,0.));
#12397=DIRECTION('ref_axis',(-0.707106781186548,-0.707106781186547,0.));
#12398=DIRECTION('',(0.,0.,-1.));
#12399=DIRECTION('',(0.,0.,-1.));
#12400=DIRECTION('',(-0.707106781186548,-0.707106781186547,0.));
#12401=DIRECTION('center_axis',(0.707106781186548,0.707106781186547,0.));
#12402=DIRECTION('ref_axis',(0.707106781186547,-0.707106781186548,0.));
#12403=DIRECTION('',(0.707106781186547,-0.707106781186548,0.));
#12404=DIRECTION('center_axis',(0.,0.,-1.));
#12405=DIRECTION('ref_axis',(0.707106781186548,0.707106781186547,0.));
#12406=DIRECTION('center_axis',(0.,0.,-1.));
#12407=DIRECTION('ref_axis',(1.,0.,0.));
#12408=DIRECTION('center_axis',(0.,0.,-1.));
#12409=DIRECTION('ref_axis',(1.,0.,0.));
#12410=DIRECTION('center_axis',(0.,0.,1.));
#12411=DIRECTION('ref_axis',(1.,0.,0.));
#12412=DIRECTION('center_axis',(1.22464679914735E-16,1.,0.));
#12413=DIRECTION('ref_axis',(1.,-1.22464679914735E-16,0.));
#12414=DIRECTION('',(0.,0.,1.));
#12415=DIRECTION('',(1.,-1.22464679914735E-16,0.));
#12416=DIRECTION('',(0.,0.,-1.));
#12417=DIRECTION('center_axis',(-1.22464679914735E-16,-1.,0.));
#12418=DIRECTION('ref_axis',(-1.,1.22464679914735E-16,0.));
#12419=DIRECTION('',(0.,0.,-1.));
#12420=DIRECTION('',(0.,0.,-1.));
#12421=DIRECTION('',(-1.,1.22464679914735E-16,0.));
#12422=DIRECTION('center_axis',(1.,-1.22464679914735E-16,0.));
#12423=DIRECTION('ref_axis',(-1.22464679914735E-16,-1.,0.));
#12424=DIRECTION('',(-1.22464679914735E-16,-1.,0.));
#12425=DIRECTION('center_axis',(0.,0.,-1.));
#12426=DIRECTION('ref_axis',(1.,-1.22464679914735E-16,0.));
#12427=DIRECTION('center_axis',(0.,0.,-1.));
#12428=DIRECTION('ref_axis',(1.,0.,0.));
#12429=DIRECTION('center_axis',(0.,0.,-1.));
#12430=DIRECTION('ref_axis',(1.,0.,0.));
#12431=DIRECTION('center_axis',(0.,0.,-1.));
#12432=DIRECTION('ref_axis',(1.,0.,0.));
#12433=DIRECTION('center_axis',(0.,0.,1.));
#12434=DIRECTION('ref_axis',(1.,0.,0.));
#12435=DIRECTION('center_axis',(0.707106781186548,0.707106781186547,0.));
#12436=DIRECTION('ref_axis',(0.707106781186547,-0.707106781186548,0.));
#12437=DIRECTION('',(0.,0.,1.));
#12438=DIRECTION('',(0.707106781186547,-0.707106781186548,0.));
#12439=DIRECTION('',(0.,0.,-1.));
#12440=DIRECTION('center_axis',(-0.707106781186548,-0.707106781186547,0.));
#12441=DIRECTION('ref_axis',(-0.707106781186547,0.707106781186548,0.));
#12442=DIRECTION('',(0.,0.,-1.));
#12443=DIRECTION('',(0.,0.,-1.));
#12444=DIRECTION('',(-0.707106781186547,0.707106781186548,0.));
#12445=DIRECTION('center_axis',(0.707106781186547,-0.707106781186548,0.));
#12446=DIRECTION('ref_axis',(-0.707106781186548,-0.707106781186547,0.));
#12447=DIRECTION('',(-0.707106781186548,-0.707106781186547,0.));
#12448=DIRECTION('center_axis',(0.,0.,-1.));
#12449=DIRECTION('ref_axis',(0.707106781186547,-0.707106781186548,0.));
#12450=DIRECTION('center_axis',(0.,0.,-1.));
#12451=DIRECTION('ref_axis',(1.,0.,0.));
#12452=DIRECTION('center_axis',(0.,0.,-1.));
#12453=DIRECTION('ref_axis',(1.,0.,0.));
#12454=DIRECTION('center_axis',(0.,0.,1.));
#12455=DIRECTION('ref_axis',(1.,0.,0.));
#12456=DIRECTION('center_axis',(1.,-6.12323399573677E-17,0.));
#12457=DIRECTION('ref_axis',(-6.12323399573677E-17,-1.,0.));
#12458=DIRECTION('',(0.,0.,1.));
#12459=DIRECTION('',(-6.12323399573677E-17,-1.,0.));
#12460=DIRECTION('',(0.,0.,-1.));
#12461=DIRECTION('center_axis',(-1.,6.12323399573677E-17,0.));
#12462=DIRECTION('ref_axis',(6.12323399573677E-17,1.,0.));
#12463=DIRECTION('',(0.,0.,-1.));
#12464=DIRECTION('',(0.,0.,-1.));
#12465=DIRECTION('',(6.12323399573677E-17,1.,0.));
#12466=DIRECTION('center_axis',(-6.12323399573677E-17,-1.,0.));
#12467=DIRECTION('ref_axis',(-1.,6.12323399573677E-17,0.));
#12468=DIRECTION('',(-1.,6.12323399573677E-17,0.));
#12469=DIRECTION('center_axis',(0.,0.,-1.));
#12470=DIRECTION('ref_axis',(-6.12323399573677E-17,-1.,0.));
#12471=DIRECTION('center_axis',(0.,0.,-1.));
#12472=DIRECTION('ref_axis',(1.,0.,0.));
#12473=DIRECTION('center_axis',(0.,0.,-1.));
#12474=DIRECTION('ref_axis',(1.,0.,0.));
#12475=DIRECTION('center_axis',(0.,0.,1.));
#12476=DIRECTION('ref_axis',(1.,0.,0.));
#12477=DIRECTION('center_axis',(-0.707106781186548,0.707106781186548,0.));
#12478=DIRECTION('ref_axis',(0.707106781186548,0.707106781186548,0.));
#12479=DIRECTION('',(0.,0.,-1.));
#12480=DIRECTION('',(0.707106781186548,0.707106781186548,0.));
#12481=DIRECTION('',(0.,0.,-1.));
#12482=DIRECTION('center_axis',(0.707106781186548,-0.707106781186548,0.));
#12483=DIRECTION('ref_axis',(-0.707106781186548,-0.707106781186548,0.));
#12484=DIRECTION('',(0.,0.,1.));
#12485=DIRECTION('',(-0.707106781186548,-0.707106781186548,0.));
#12486=DIRECTION('',(0.,0.,-1.));
#12487=DIRECTION('center_axis',(-0.707106781186548,-0.707106781186548,0.));
#12488=DIRECTION('ref_axis',(-0.707106781186548,0.707106781186548,0.));
#12489=DIRECTION('',(-0.707106781186548,0.707106781186548,0.));
#12490=DIRECTION('center_axis',(0.,0.,-1.));
#12491=DIRECTION('ref_axis',(-0.707106781186548,-0.707106781186548,0.));
#12492=DIRECTION('center_axis',(0.,0.,-1.));
#12493=DIRECTION('ref_axis',(1.,0.,0.));
#12494=DIRECTION('center_axis',(0.,0.,-1.));
#12495=DIRECTION('ref_axis',(1.,0.,0.));
#12496=DIRECTION('center_axis',(0.,0.,1.));
#12497=DIRECTION('ref_axis',(1.,0.,0.));
#12498=DIRECTION('center_axis',(0.,1.,0.));
#12499=DIRECTION('ref_axis',(1.,0.,0.));
#12500=DIRECTION('',(0.,0.,-1.));
#12501=DIRECTION('',(1.,0.,0.));
#12502=DIRECTION('',(0.,0.,-1.));
#12503=DIRECTION('center_axis',(0.,-1.,0.));
#12504=DIRECTION('ref_axis',(-1.,0.,0.));
#12505=DIRECTION('',(0.,0.,1.));
#12506=DIRECTION('',(-1.,0.,0.));
#12507=DIRECTION('',(0.,0.,-1.));
#12508=DIRECTION('center_axis',(-1.,0.,0.));
#12509=DIRECTION('ref_axis',(0.,1.,0.));
#12510=DIRECTION('',(0.,1.,0.));
#12511=DIRECTION('center_axis',(0.,0.,-1.));
#12512=DIRECTION('ref_axis',(-1.,0.,0.));
#12513=DIRECTION('center_axis',(0.,0.,-1.));
#12514=DIRECTION('ref_axis',(1.,0.,0.));
#12515=DIRECTION('center_axis',(0.,0.,1.));
#12516=DIRECTION('ref_axis',(1.,0.,0.));
#12517=DIRECTION('center_axis',(0.,0.,1.));
#12518=DIRECTION('ref_axis',(1.,0.,0.));
#12519=DIRECTION('',(0.,0.,1.));
#12520=DIRECTION('center_axis',(0.,0.,1.));
#12521=DIRECTION('ref_axis',(1.,0.,0.));
#12522=DIRECTION('center_axis',(0.,0.,1.));
#12523=DIRECTION('ref_axis',(1.,0.,0.));
#12524=DIRECTION('center_axis',(0.,0.,-1.));
#12525=DIRECTION('ref_axis',(1.,0.,0.));
#12526=DIRECTION('center_axis',(0.,0.,1.));
#12527=DIRECTION('ref_axis',(1.,0.,0.));
#12528=DIRECTION('',(0.,0.,1.));
#12529=DIRECTION('center_axis',(0.,0.,1.));
#12530=DIRECTION('ref_axis',(1.,0.,0.));
#12531=DIRECTION('center_axis',(0.,0.,-1.));
#12532=DIRECTION('ref_axis',(-1.,0.,0.));
#12533=DIRECTION('center_axis',(0.,0.,1.));
#12534=DIRECTION('ref_axis',(1.,0.,0.));
#12535=DIRECTION('center_axis',(0.,0.,1.));
#12536=DIRECTION('ref_axis',(1.,0.,0.));
#12537=DIRECTION('',(0.,0.,-1.));
#12538=DIRECTION('center_axis',(0.,0.,1.));
#12539=DIRECTION('ref_axis',(1.,0.,0.));
#12540=DIRECTION('center_axis',(0.,0.,1.));
#12541=DIRECTION('ref_axis',(1.,0.,0.));
#12542=DIRECTION('',(0.,0.,1.));
#12543=DIRECTION('center_axis',(0.,0.,1.));
#12544=DIRECTION('ref_axis',(1.,0.,0.));
#12545=DIRECTION('axis',(0.,0.,1.));
#12546=DIRECTION('refdir',(1.,0.,0.));
#12547=DIRECTION('center_axis',(1.,0.,0.));
#12548=DIRECTION('ref_axis',(0.,1.,0.));
#12549=DIRECTION('',(0.,0.,1.));
#12550=DIRECTION('',(0.,1.,0.));
#12551=DIRECTION('',(0.,0.,1.));
#12552=DIRECTION('',(0.,1.,0.));
#12553=DIRECTION('center_axis',(-1.,0.,0.));
#12554=DIRECTION('ref_axis',(0.,-1.,0.));
#12555=DIRECTION('',(0.,0.,-1.));
#12556=DIRECTION('',(0.,-1.,0.));
#12557=DIRECTION('',(0.,0.,1.));
#12558=DIRECTION('',(0.,-1.,0.));
#12559=DIRECTION('center_axis',(0.,1.,0.));
#12560=DIRECTION('ref_axis',(-1.,0.,0.));
#12561=DIRECTION('',(-1.,0.,0.));
#12562=DIRECTION('',(-1.,0.,0.));
#12563=DIRECTION('center_axis',(0.,0.,1.));
#12564=DIRECTION('ref_axis',(1.,0.,0.));
#12565=DIRECTION('center_axis',(0.,0.,1.));
#12566=DIRECTION('ref_axis',(1.,0.,0.));
#12567=DIRECTION('center_axis',(0.,0.,-1.));
#12568=DIRECTION('ref_axis',(1.,0.,0.));
#12569=DIRECTION('center_axis',(0.,0.,1.));
#12570=DIRECTION('ref_axis',(1.,0.,0.));
#12571=DIRECTION('center_axis',(0.,0.,-1.));
#12572=DIRECTION('ref_axis',(1.,0.,0.));
#12573=DIRECTION('',(0.,0.,1.));
#12574=DIRECTION('center_axis',(0.,0.,1.));
#12575=DIRECTION('ref_axis',(6.12323399573677E-17,-1.,0.));
#12576=DIRECTION('center_axis',(0.,0.,1.));
#12577=DIRECTION('ref_axis',(1.,0.,0.));
#12578=DIRECTION('center_axis',(0.,0.,1.));
#12579=DIRECTION('ref_axis',(1.,0.,0.));
#12580=DIRECTION('axis',(0.,0.,1.));
#12581=DIRECTION('refdir',(1.,0.,0.));
#12582=DIRECTION('center_axis',(0.,0.,1.));
#12583=DIRECTION('ref_axis',(1.,0.,0.));
#12584=DIRECTION('center_axis',(0.,0.,1.));
#12585=DIRECTION('ref_axis',(1.,0.,0.));
#12586=DIRECTION('',(0.,0.,1.));
#12587=DIRECTION('center_axis',(0.,0.,1.));
#12588=DIRECTION('ref_axis',(1.,0.,0.));
#12589=DIRECTION('center_axis',(0.,0.,-1.));
#12590=DIRECTION('ref_axis',(1.,0.,0.));
#12591=DIRECTION('',(-0.707106781186547,8.65956056235493E-17,-0.707106781186548));
#12592=DIRECTION('center_axis',(0.,0.,1.));
#12593=DIRECTION('ref_axis',(1.,0.,0.));
#12594=DIRECTION('center_axis',(0.,0.,-1.));
#12595=DIRECTION('ref_axis',(-1.,0.,0.));
#12596=DIRECTION('center_axis',(0.,0.,1.));
#12597=DIRECTION('ref_axis',(1.,0.,0.));
#12598=DIRECTION('center_axis',(0.,0.,1.));
#12599=DIRECTION('ref_axis',(1.,0.,0.));
#12600=DIRECTION('center_axis',(0.,0.,1.));
#12601=DIRECTION('ref_axis',(1.,0.,0.));
#12602=DIRECTION('',(0.,0.,-1.));
#12603=DIRECTION('center_axis',(0.,0.,-1.));
#12604=DIRECTION('ref_axis',(-1.,0.,0.));
#12605=DIRECTION('center_axis',(0.,0.,1.));
#12606=DIRECTION('ref_axis',(1.,0.,0.));
#12607=DIRECTION('center_axis',(0.,0.,1.));
#12608=DIRECTION('ref_axis',(1.,0.,0.));
#12609=DIRECTION('center_axis',(0.,0.,1.));
#12610=DIRECTION('ref_axis',(1.,0.,0.));
#12611=DIRECTION('',(0.,0.,1.));
#12612=DIRECTION('center_axis',(0.,0.,-1.));
#12613=DIRECTION('ref_axis',(-1.,0.,0.));
#12614=DIRECTION('center_axis',(0.,0.,1.));
#12615=DIRECTION('ref_axis',(1.,0.,0.));
#12616=DIRECTION('center_axis',(0.,0.,1.));
#12617=DIRECTION('ref_axis',(1.,0.,0.));
#12618=DIRECTION('center_axis',(0.,0.,1.));
#12619=DIRECTION('ref_axis',(1.,0.,0.));
#12620=DIRECTION('',(0.707106781186548,8.65956056235494E-17,-0.707106781186547));
#12621=DIRECTION('center_axis',(0.,0.,1.));
#12622=DIRECTION('ref_axis',(1.,0.,0.));
#12623=DIRECTION('center_axis',(0.,0.,1.));
#12624=DIRECTION('ref_axis',(1.,0.,0.));
#12625=DIRECTION('',(0.,0.,-1.));
#12626=DIRECTION('center_axis',(0.,0.,-1.));
#12627=DIRECTION('ref_axis',(1.,0.,0.));
#12628=DIRECTION('',(0.707106781186547,-8.65956056235493E-17,0.707106781186548));
#12629=DIRECTION('center_axis',(0.,0.,1.));
#12630=DIRECTION('ref_axis',(1.,0.,0.));
#12631=DIRECTION('center_axis',(0.,0.,1.));
#12632=DIRECTION('ref_axis',(1.,0.,0.));
#12633=DIRECTION('center_axis',(0.,0.,1.));
#12634=DIRECTION('ref_axis',(1.,0.,0.));
#12635=DIRECTION('center_axis',(0.,0.,1.));
#12636=DIRECTION('ref_axis',(1.,0.,0.));
#12637=DIRECTION('center_axis',(0.,0.,1.));
#12638=DIRECTION('ref_axis',(1.,0.,0.));
#12639=DIRECTION('',(0.,0.,1.));
#12640=DIRECTION('center_axis',(0.,0.,1.));
#12641=DIRECTION('ref_axis',(1.,0.,0.));
#12642=DIRECTION('center_axis',(0.,0.,1.));
#12643=DIRECTION('ref_axis',(1.,0.,0.));
#12644=DIRECTION('center_axis',(0.,0.,1.));
#12645=DIRECTION('ref_axis',(1.,0.,0.));
#12646=DIRECTION('center_axis',(0.,0.,1.));
#12647=DIRECTION('ref_axis',(1.,0.,0.));
#12648=DIRECTION('',(0.,0.,-1.));
#12649=DIRECTION('center_axis',(0.,0.,1.));
#12650=DIRECTION('ref_axis',(1.,0.,0.));
#12651=DIRECTION('center_axis',(0.,0.,1.));
#12652=DIRECTION('ref_axis',(1.,0.,0.));
#12653=DIRECTION('center_axis',(0.,0.,1.));
#12654=DIRECTION('ref_axis',(1.,0.,0.));
#12655=DIRECTION('',(-0.707106781186547,-8.65956056235493E-17,0.707106781186548));
#12656=DIRECTION('axis',(0.,0.,1.));
#12657=DIRECTION('refdir',(1.,0.,0.));
#12658=DIRECTION('center_axis',(0.,0.,1.));
#12659=DIRECTION('ref_axis',(1.,0.,0.));
#12660=DIRECTION('center_axis',(0.,0.,1.));
#12661=DIRECTION('ref_axis',(1.,0.,0.));
#12662=DIRECTION('',(0.,0.,1.));
#12663=DIRECTION('center_axis',(0.,0.,1.));
#12664=DIRECTION('ref_axis',(1.,0.,0.));
#12665=DIRECTION('center_axis',(0.,0.,-1.));
#12666=DIRECTION('ref_axis',(1.,0.,0.));
#12667=DIRECTION('',(-0.707106781186547,8.65956056235493E-17,-0.707106781186548));
#12668=DIRECTION('center_axis',(0.,0.,1.));
#12669=DIRECTION('ref_axis',(1.,0.,0.));
#12670=DIRECTION('center_axis',(0.,0.,-1.));
#12671=DIRECTION('ref_axis',(-1.,0.,0.));
#12672=DIRECTION('center_axis',(0.,0.,1.));
#12673=DIRECTION('ref_axis',(1.,0.,0.));
#12674=DIRECTION('center_axis',(0.,0.,1.));
#12675=DIRECTION('ref_axis',(1.,0.,0.));
#12676=DIRECTION('center_axis',(0.,0.,1.));
#12677=DIRECTION('ref_axis',(1.,0.,0.));
#12678=DIRECTION('',(0.707106781186547,8.65956056235493E-17,-0.707106781186548));
#12679=DIRECTION('center_axis',(0.,0.,1.));
#12680=DIRECTION('ref_axis',(1.,0.,0.));
#12681=DIRECTION('center_axis',(0.,0.,1.));
#12682=DIRECTION('ref_axis',(1.,0.,0.));
#12683=DIRECTION('',(0.,0.,-1.));
#12684=DIRECTION('center_axis',(0.,0.,-1.));
#12685=DIRECTION('ref_axis',(1.,0.,0.));
#12686=DIRECTION('',(0.707106781186547,-8.65956056235492E-17,0.707106781186548));
#12687=DIRECTION('center_axis',(0.,0.,1.));
#12688=DIRECTION('ref_axis',(1.,0.,0.));
#12689=DIRECTION('center_axis',(0.,0.,1.));
#12690=DIRECTION('ref_axis',(1.,0.,0.));
#12691=DIRECTION('center_axis',(0.,0.,1.));
#12692=DIRECTION('ref_axis',(1.,0.,0.));
#12693=DIRECTION('center_axis',(0.,0.,1.));
#12694=DIRECTION('ref_axis',(1.,0.,0.));
#12695=DIRECTION('',(-0.707106781186547,-8.65956056235492E-17,0.707106781186548));
#12696=DIRECTION('axis',(0.,0.,1.));
#12697=DIRECTION('refdir',(1.,0.,0.));
#12698=DIRECTION('center_axis',(-1.,0.,0.));
#12699=DIRECTION('ref_axis',(0.,0.,1.));
#12700=DIRECTION('center_axis',(1.,0.,0.));
#12701=DIRECTION('ref_axis',(0.,0.,-1.));
#12702=DIRECTION('center_axis',(1.,0.,0.));
#12703=DIRECTION('ref_axis',(0.,1.,0.));
#12704=DIRECTION('center_axis',(1.,0.,0.));
#12705=DIRECTION('ref_axis',(0.,0.,-1.));
#12706=DIRECTION('',(-0.707106781186547,0.707106781186548,8.65956056235494E-17));
#12707=DIRECTION('center_axis',(1.,0.,0.));
#12708=DIRECTION('ref_axis',(0.,1.,0.));
#12709=DIRECTION('center_axis',(1.,0.,0.));
#12710=DIRECTION('ref_axis',(0.,0.,-1.));
#12711=DIRECTION('',(-1.,0.,0.));
#12712=DIRECTION('center_axis',(1.,0.,0.));
#12713=DIRECTION('ref_axis',(0.,0.,-1.));
#12714=DIRECTION('center_axis',(1.,0.,0.));
#12715=DIRECTION('ref_axis',(0.,0.,-1.));
#12716=DIRECTION('center_axis',(1.,0.,0.));
#12717=DIRECTION('ref_axis',(0.,1.,0.));
#12718=DIRECTION('center_axis',(1.,0.,0.));
#12719=DIRECTION('ref_axis',(0.,0.,-1.));
#12720=DIRECTION('',(-1.,0.,0.));
#12721=DIRECTION('center_axis',(-1.,0.,0.));
#12722=DIRECTION('ref_axis',(0.,0.,1.));
#12723=DIRECTION('center_axis',(1.,0.,0.));
#12724=DIRECTION('ref_axis',(0.,0.,-1.));
#12725=DIRECTION('center_axis',(1.,0.,0.));
#12726=DIRECTION('ref_axis',(0.,1.,0.));
#12727=DIRECTION('center_axis',(1.,0.,0.));
#12728=DIRECTION('ref_axis',(0.,0.,-1.));
#12729=DIRECTION('',(-1.,0.,0.));
#12730=DIRECTION('center_axis',(-1.,0.,0.));
#12731=DIRECTION('ref_axis',(0.,1.,0.));
#12732=DIRECTION('',(0.707106781186551,0.707106781186544,-8.6595605623549E-17));
#12733=DIRECTION('center_axis',(1.,0.,0.));
#12734=DIRECTION('ref_axis',(0.,0.,-1.));
#12735=DIRECTION('center_axis',(1.,0.,0.));
#12736=DIRECTION('ref_axis',(0.,0.,-1.));
#12737=DIRECTION('axis',(0.,0.,1.));
#12738=DIRECTION('refdir',(1.,0.,0.));
#12739=DIRECTION('center_axis',(-1.,0.,0.));
#12740=DIRECTION('ref_axis',(0.,0.,1.));
#12741=DIRECTION('center_axis',(1.,0.,0.));
#12742=DIRECTION('ref_axis',(0.,0.,-1.));
#12743=DIRECTION('center_axis',(1.,0.,0.));
#12744=DIRECTION('ref_axis',(0.,1.,0.));
#12745=DIRECTION('center_axis',(1.,0.,0.));
#12746=DIRECTION('ref_axis',(0.,0.,-1.));
#12747=DIRECTION('',(-0.707106781186546,0.707106781186549,8.65956056235495E-17));
#12748=DIRECTION('center_axis',(1.,0.,0.));
#12749=DIRECTION('ref_axis',(0.,1.,0.));
#12750=DIRECTION('center_axis',(1.,0.,0.));
#12751=DIRECTION('ref_axis',(0.,0.,-1.));
#12752=DIRECTION('',(-1.,0.,0.));
#12753=DIRECTION('center_axis',(1.,0.,0.));
#12754=DIRECTION('ref_axis',(0.,0.,-1.));
#12755=DIRECTION('center_axis',(1.,0.,0.));
#12756=DIRECTION('ref_axis',(0.,0.,-1.));
#12757=DIRECTION('center_axis',(1.,0.,0.));
#12758=DIRECTION('ref_axis',(0.,1.,0.));
#12759=DIRECTION('center_axis',(1.,0.,0.));
#12760=DIRECTION('ref_axis',(0.,0.,-1.));
#12761=DIRECTION('',(-1.,0.,0.));
#12762=DIRECTION('center_axis',(-1.,0.,0.));
#12763=DIRECTION('ref_axis',(0.,0.,1.));
#12764=DIRECTION('center_axis',(1.,0.,0.));
#12765=DIRECTION('ref_axis',(0.,0.,-1.));
#12766=DIRECTION('center_axis',(1.,0.,0.));
#12767=DIRECTION('ref_axis',(0.,1.,0.));
#12768=DIRECTION('center_axis',(1.,0.,0.));
#12769=DIRECTION('ref_axis',(0.,0.,-1.));
#12770=DIRECTION('',(-1.,0.,0.));
#12771=DIRECTION('center_axis',(-1.,0.,0.));
#12772=DIRECTION('ref_axis',(0.,1.,0.));
#12773=DIRECTION('',(0.70710678118655,0.707106781186545,-8.6595605623549E-17));
#12774=DIRECTION('center_axis',(1.,0.,0.));
#12775=DIRECTION('ref_axis',(0.,0.,-1.));
#12776=DIRECTION('center_axis',(1.,0.,0.));
#12777=DIRECTION('ref_axis',(0.,0.,-1.));
#12778=DIRECTION('axis',(0.,0.,1.));
#12779=DIRECTION('refdir',(1.,0.,0.));
#12780=DIRECTION('center_axis',(0.,0.,1.));
#12781=DIRECTION('ref_axis',(1.,0.,0.));
#12782=DIRECTION('center_axis',(0.,0.,-1.));
#12783=DIRECTION('ref_axis',(-1.,1.22464679914735E-16,0.));
#12784=DIRECTION('center_axis',(1.22464679914735E-16,-1.,0.));
#12785=DIRECTION('ref_axis',(-1.,-1.22464679914735E-16,0.));
#12786=DIRECTION('center_axis',(0.,0.,1.));
#12787=DIRECTION('ref_axis',(-1.,1.22464679914735E-16,0.));
#12788=DIRECTION('center_axis',(0.,0.,1.));
#12789=DIRECTION('ref_axis',(1.,0.,0.));
#12790=DIRECTION('',(0.,0.,-1.));
#12791=DIRECTION('center_axis',(0.,0.,1.));
#12792=DIRECTION('ref_axis',(1.,0.,0.));
#12793=DIRECTION('center_axis',(0.,0.,1.));
#12794=DIRECTION('ref_axis',(1.,0.,0.));
#12795=DIRECTION('center_axis',(0.,0.,-1.));
#12796=DIRECTION('ref_axis',(-1.,0.,0.));
#12797=DIRECTION('center_axis',(0.,0.,1.));
#12798=DIRECTION('ref_axis',(1.,0.,0.));
#12799=DIRECTION('center_axis',(0.,0.,1.));
#12800=DIRECTION('ref_axis',(1.,0.,0.));
#12801=DIRECTION('',(0.707106781186547,8.65956056235493E-17,-0.707106781186548));
#12802=DIRECTION('axis',(0.,0.,1.));
#12803=DIRECTION('refdir',(1.,0.,0.));
#12804=DIRECTION('center_axis',(0.,0.,1.));
#12805=DIRECTION('ref_axis',(-0.6579379160252,-0.753072173603843,0.));
#12806=DIRECTION('',(0.,0.,-1.));
#12807=DIRECTION('center_axis',(0.,0.,-1.));
#12808=DIRECTION('ref_axis',(1.,8.51023079448757E-14,0.));
#12809=DIRECTION('center_axis',(0.,0.,1.));
#12810=DIRECTION('ref_axis',(-0.6579379160252,-0.753072173603843,0.));
#12811=DIRECTION('',(0.,0.,-1.));
#12812=DIRECTION('center_axis',(0.,0.,1.));
#12813=DIRECTION('ref_axis',(-0.6579379160252,-0.753072173603843,0.));
#12814=DIRECTION('',(0.,0.,-1.));
#12815=DIRECTION('center_axis',(0.,0.,1.));
#12816=DIRECTION('ref_axis',(-0.6579379160252,-0.753072173603843,0.));
#12817=DIRECTION('',(0.,0.,-1.));
#12818=DIRECTION('center_axis',(0.,0.,1.));
#12819=DIRECTION('ref_axis',(-0.6579379160252,-0.753072173603843,0.));
#12820=DIRECTION('',(0.,0.,-1.));
#12821=DIRECTION('center_axis',(0.,0.,1.));
#12822=DIRECTION('ref_axis',(-0.6579379160252,-0.753072173603843,0.));
#12823=DIRECTION('',(0.,0.,-1.));
#12824=DIRECTION('center_axis',(0.,0.,1.));
#12825=DIRECTION('ref_axis',(-0.6579379160252,-0.753072173603843,0.));
#12826=DIRECTION('',(0.,0.,-1.));
#12827=DIRECTION('center_axis',(0.,0.,1.));
#12828=DIRECTION('ref_axis',(-0.6579379160252,-0.753072173603843,0.));
#12829=DIRECTION('',(0.,0.,-1.));
#12830=DIRECTION('center_axis',(0.,0.,1.));
#12831=DIRECTION('ref_axis',(-0.6579379160252,-0.753072173603843,0.));
#12832=DIRECTION('',(0.,0.,-1.));
#12833=DIRECTION('center_axis',(0.,0.,1.));
#12834=DIRECTION('ref_axis',(-0.6579379160252,-0.753072173603843,0.));
#12835=DIRECTION('',(0.,0.,-1.));
#12836=DIRECTION('center_axis',(0.,0.,1.));
#12837=DIRECTION('ref_axis',(-0.6579379160252,-0.753072173603843,0.));
#12838=DIRECTION('',(0.,0.,-1.));
#12839=DIRECTION('center_axis',(0.,0.,1.));
#12840=DIRECTION('ref_axis',(-0.6579379160252,-0.753072173603843,0.));
#12841=DIRECTION('',(0.,0.,-1.));
#12842=DIRECTION('center_axis',(0.,0.,1.));
#12843=DIRECTION('ref_axis',(-0.6579379160252,-0.753072173603843,0.));
#12844=DIRECTION('',(0.,0.,-1.));
#12845=DIRECTION('center_axis',(0.,0.,1.));
#12846=DIRECTION('ref_axis',(-0.6579379160252,-0.753072173603843,0.));
#12847=DIRECTION('',(0.,0.,-1.));
#12848=DIRECTION('center_axis',(0.,0.,1.));
#12849=DIRECTION('ref_axis',(1.,0.,0.));
#12850=DIRECTION('center_axis',(0.,0.,1.));
#12851=DIRECTION('ref_axis',(1.,0.,0.));
#12852=DIRECTION('center_axis',(0.,0.,1.));
#12853=DIRECTION('ref_axis',(1.,0.,0.));
#12854=DIRECTION('center_axis',(0.,0.,1.));
#12855=DIRECTION('ref_axis',(-0.6579379160252,-0.753072173603843,0.));
#12856=DIRECTION('center_axis',(0.,0.,1.));
#12857=DIRECTION('ref_axis',(1.,8.51023079448757E-14,0.));
#12858=DIRECTION('center_axis',(0.,0.,1.));
#12859=DIRECTION('ref_axis',(1.,0.,0.));
#12860=DIRECTION('center_axis',(0.,0.,1.));
#12861=DIRECTION('ref_axis',(1.,0.,0.));
#12862=DIRECTION('center_axis',(0.,0.,1.));
#12863=DIRECTION('ref_axis',(1.,0.,0.));
#12864=DIRECTION('center_axis',(0.,0.,1.));
#12865=DIRECTION('ref_axis',(1.,0.,0.));
#12866=DIRECTION('center_axis',(0.,0.,-1.));
#12867=DIRECTION('ref_axis',(1.,0.,0.));
#12868=DIRECTION('center_axis',(0.,0.,1.));
#12869=DIRECTION('ref_axis',(1.,0.,0.));
#12870=DIRECTION('center_axis',(0.,0.,-1.));
#12871=DIRECTION('ref_axis',(1.,0.,0.));
#12872=DIRECTION('center_axis',(0.,0.,1.));
#12873=DIRECTION('ref_axis',(1.,0.,0.));
#12874=DIRECTION('center_axis',(0.,0.,-1.));
#12875=DIRECTION('ref_axis',(1.,0.,0.));
#12876=DIRECTION('center_axis',(0.,0.,1.));
#12877=DIRECTION('ref_axis',(1.,0.,0.));
#12878=DIRECTION('center_axis',(0.,0.,-1.));
#12879=DIRECTION('ref_axis',(1.,0.,0.));
#12880=DIRECTION('center_axis',(0.,0.,1.));
#12881=DIRECTION('ref_axis',(-1.,-1.22464679914735E-16,0.));
#12882=DIRECTION('center_axis',(0.,0.,-1.));
#12883=DIRECTION('ref_axis',(1.,0.,0.));
#12884=DIRECTION('center_axis',(0.,0.,-1.));
#12885=DIRECTION('ref_axis',(1.,0.,0.));
#12886=DIRECTION('center_axis',(0.,0.,1.));
#12887=DIRECTION('ref_axis',(1.,0.,0.));
#12888=DIRECTION('center_axis',(0.,0.,-1.));
#12889=DIRECTION('ref_axis',(1.,0.,0.));
#12890=DIRECTION('center_axis',(1.22464679914735E-16,0.,1.));
#12891=DIRECTION('ref_axis',(1.,0.,-1.1686558153949E-16));
#12892=DIRECTION('center_axis',(1.22464679914735E-16,-1.,-7.49879891330929E-33));
#12893=DIRECTION('ref_axis',(-1.,-1.22464679914735E-16,1.1686558153949E-16));
#12894=DIRECTION('center_axis',(0.,0.,1.));
#12895=DIRECTION('ref_axis',(1.,0.,0.));
#12896=DIRECTION('center_axis',(-1.,-1.92296268638356E-16,0.));
#12897=DIRECTION('ref_axis',(0.,0.,-1.));
#12898=DIRECTION('center_axis',(-0.5,0.866025403784439,0.));
#12899=DIRECTION('ref_axis',(0.,0.,-1.));
#12900=DIRECTION('center_axis',(-0.5,0.866025403784439,0.));
#12901=DIRECTION('ref_axis',(0.,0.,-1.));
#12902=DIRECTION('center_axis',(0.5,0.866025403784439,0.));
#12903=DIRECTION('ref_axis',(0.,0.,-1.));
#12904=DIRECTION('center_axis',(0.5,0.866025403784439,0.));
#12905=DIRECTION('ref_axis',(0.,0.,-1.));
#12906=DIRECTION('center_axis',(1.,-3.84592537276713E-16,0.));
#12907=DIRECTION('ref_axis',(0.,0.,1.));
#12908=DIRECTION('center_axis',(1.,-3.84592537276713E-16,0.));
#12909=DIRECTION('ref_axis',(0.,0.,1.));
#12910=DIRECTION('center_axis',(0.5,-0.866025403784439,0.));
#12911=DIRECTION('ref_axis',(0.,0.,1.));
#12912=DIRECTION('center_axis',(0.5,-0.866025403784439,0.));
#12913=DIRECTION('ref_axis',(0.,0.,1.));
#12914=DIRECTION('center_axis',(-0.5,-0.866025403784439,0.));
#12915=DIRECTION('ref_axis',(0.,0.,1.));
#12916=DIRECTION('center_axis',(-0.5,-0.866025403784439,0.));
#12917=DIRECTION('ref_axis',(0.,0.,1.));
#12918=DIRECTION('center_axis',(-1.,-1.92296268638356E-16,0.));
#12919=DIRECTION('ref_axis',(0.,0.,-1.));
#12920=DIRECTION('center_axis',(0.,0.,1.));
#12921=DIRECTION('ref_axis',(1.,0.,0.));
#12922=DIRECTION('',(-0.854074023911687,-1.04593901961835E-16,0.520151479551197));
#12923=DIRECTION('center_axis',(0.,0.,-1.));
#12924=DIRECTION('ref_axis',(1.,0.,0.));
#12925=DIRECTION('center_axis',(-0.5,-0.866025403784439,0.));
#12926=DIRECTION('ref_axis',(-0.866025403784439,0.5,0.));
#12927=DIRECTION('',(0.,0.,-1.));
#12928=DIRECTION('',(-0.866025403784439,0.5,0.));
#12929=DIRECTION('',(0.,0.,-1.));
#12930=DIRECTION('center_axis',(-1.,-1.92296268638356E-16,0.));
#12931=DIRECTION('ref_axis',(-1.92296268638356E-16,1.,0.));
#12932=DIRECTION('',(-1.92296268638356E-16,1.,0.));
#12933=DIRECTION('',(0.,0.,-1.));
#12934=DIRECTION('center_axis',(-0.5,0.866025403784439,0.));
#12935=DIRECTION('ref_axis',(0.866025403784439,0.5,0.));
#12936=DIRECTION('',(0.866025403784439,0.5,0.));
#12937=DIRECTION('',(0.,0.,-1.));
#12938=DIRECTION('center_axis',(0.5,0.866025403784439,0.));
#12939=DIRECTION('ref_axis',(0.866025403784439,-0.5,0.));
#12940=DIRECTION('',(0.866025403784439,-0.5,0.));
#12941=DIRECTION('',(0.,0.,-1.));
#12942=DIRECTION('center_axis',(0.5,-0.866025403784439,0.));
#12943=DIRECTION('ref_axis',(-0.866025403784439,-0.5,0.));
#12944=DIRECTION('',(0.,0.,-1.));
#12945=DIRECTION('',(-0.866025403784439,-0.5,0.));
#12946=DIRECTION('center_axis',(1.,-3.84592537276713E-16,0.));
#12947=DIRECTION('ref_axis',(-3.84592537276713E-16,-1.,0.));
#12948=DIRECTION('',(-3.84592537276713E-16,-1.,0.));
#12949=DIRECTION('center_axis',(0.,0.,-1.));
#12950=DIRECTION('ref_axis',(-1.,0.,0.));
#12951=DIRECTION('center_axis',(0.,0.,-1.));
#12952=DIRECTION('ref_axis',(-1.,0.,0.));
#12953=DIRECTION('center_axis',(0.,0.,1.));
#12954=DIRECTION('ref_axis',(1.,0.,0.));
#12955=DIRECTION('center_axis',(0.,0.,1.));
#12956=DIRECTION('ref_axis',(1.,0.,0.));
#12957=DIRECTION('',(0.707106781186547,8.65956056235493E-17,-0.707106781186548));
#12958=DIRECTION('center_axis',(0.,0.,-1.));
#12959=DIRECTION('ref_axis',(-1.,0.,0.));
#12960=DIRECTION('center_axis',(0.,0.,1.));
#12961=DIRECTION('ref_axis',(1.,0.,0.));
#12962=DIRECTION('center_axis',(0.,0.,1.));
#12963=DIRECTION('ref_axis',(1.,0.,0.));
#12964=DIRECTION('',(0.,0.,-1.));
#12965=DIRECTION('axis',(0.,0.,1.));
#12966=DIRECTION('refdir',(1.,0.,0.));
#12967=DIRECTION('center_axis',(0.,1.,0.));
#12968=DIRECTION('ref_axis',(0.,0.,1.));
#12969=DIRECTION('',(1.,0.,0.));
#12970=DIRECTION('',(0.,0.,1.));
#12971=DIRECTION('',(-1.,0.,0.));
#12972=DIRECTION('',(0.,0.,-1.));
#12973=DIRECTION('center_axis',(0.,1.,0.));
#12974=DIRECTION('ref_axis',(0.,0.,1.));
#12975=DIRECTION('',(-1.,0.,0.));
#12976=DIRECTION('',(0.,0.,-1.));
#12977=DIRECTION('',(1.,0.,0.));
#12978=DIRECTION('',(0.,0.,1.));
#12979=DIRECTION('center_axis',(0.,-1.,0.));
#12980=DIRECTION('ref_axis',(0.,0.,-1.));
#12981=DIRECTION('',(-1.,0.,0.));
#12982=DIRECTION('',(0.,0.,1.));
#12983=DIRECTION('',(1.,0.,0.));
#12984=DIRECTION('',(0.,0.,-1.));
#12985=DIRECTION('center_axis',(0.,-1.,0.));
#12986=DIRECTION('ref_axis',(0.,0.,-1.));
#12987=DIRECTION('',(-1.,0.,0.));
#12988=DIRECTION('',(0.,0.,1.));
#12989=DIRECTION('',(1.,0.,0.));
#12990=DIRECTION('',(0.,0.,-1.));
#12991=DIRECTION('center_axis',(1.,0.,0.));
#12992=DIRECTION('ref_axis',(0.,-0.194892865217565,0.980824536340363));
#12993=DIRECTION('center_axis',(1.,0.,0.));
#12994=DIRECTION('ref_axis',(0.,0.,-1.));
#12995=DIRECTION('',(1.,0.,0.));
#12996=DIRECTION('center_axis',(1.,0.,0.));
#12997=DIRECTION('ref_axis',(0.,0.,-1.));
#12998=DIRECTION('center_axis',(1.,0.,0.));
#12999=DIRECTION('ref_axis',(0.,0.,-1.));
#13000=DIRECTION('center_axis',(1.,0.,0.));
#13001=DIRECTION('ref_axis',(0.,0.,-1.));
#13002=DIRECTION('',(1.,0.,0.));
#13003=DIRECTION('center_axis',(1.,0.,0.));
#13004=DIRECTION('ref_axis',(0.,0.,-1.));
#13005=DIRECTION('center_axis',(1.,0.,0.));
#13006=DIRECTION('ref_axis',(0.,0.,-1.));
#13007=DIRECTION('center_axis',(1.,0.,0.));
#13008=DIRECTION('ref_axis',(0.,0.,-1.));
#13009=DIRECTION('',(1.,0.,0.));
#13010=DIRECTION('center_axis',(1.,0.,0.));
#13011=DIRECTION('ref_axis',(0.,0.,-1.));
#13012=DIRECTION('center_axis',(1.,0.,0.));
#13013=DIRECTION('ref_axis',(0.,0.194892865217571,0.980824536340362));
#13014=DIRECTION('center_axis',(1.,0.,0.));
#13015=DIRECTION('ref_axis',(0.,0.,-1.));
#13016=DIRECTION('',(1.,0.,0.));
#13017=DIRECTION('center_axis',(1.,0.,0.));
#13018=DIRECTION('ref_axis',(0.,0.,-1.));
#13019=DIRECTION('center_axis',(1.,0.,0.));
#13020=DIRECTION('ref_axis',(0.,0.,-1.));
#13021=DIRECTION('center_axis',(-1.,0.,0.));
#13022=DIRECTION('ref_axis',(0.,0.,-1.));
#13023=DIRECTION('center_axis',(-1.,0.,0.));
#13024=DIRECTION('ref_axis',(0.,0.,-1.));
#13025=DIRECTION('center_axis',(1.,0.,0.));
#13026=DIRECTION('ref_axis',(0.,0.,-1.));
#13027=DIRECTION('center_axis',(-1.,0.,0.));
#13028=DIRECTION('ref_axis',(0.,0.,-1.));
#13029=DIRECTION('center_axis',(1.,0.,0.));
#13030=DIRECTION('ref_axis',(0.,0.,-1.));
#13031=DIRECTION('center_axis',(-1.,0.,0.));
#13032=DIRECTION('ref_axis',(0.,0.,-1.));
#13033=DIRECTION('center_axis',(1.,0.,0.));
#13034=DIRECTION('ref_axis',(0.,0.,-1.));
#13035=DIRECTION('center_axis',(-1.,0.,0.));
#13036=DIRECTION('ref_axis',(0.,0.,-1.));
#13037=DIRECTION('center_axis',(1.,0.,0.));
#13038=DIRECTION('ref_axis',(0.,0.,-1.));
#13039=DIRECTION('center_axis',(-1.,0.,0.));
#13040=DIRECTION('ref_axis',(0.,0.,-1.));
#13041=DIRECTION('center_axis',(1.,0.,0.));
#13042=DIRECTION('ref_axis',(0.,0.,-1.));
#13043=DIRECTION('center_axis',(-1.,0.,0.));
#13044=DIRECTION('ref_axis',(0.,0.,-1.));
#13045=DIRECTION('',(1.,0.,0.));
#13046=DIRECTION('center_axis',(1.,0.,0.));
#13047=DIRECTION('ref_axis',(0.,0.,-1.));
#13048=DIRECTION('center_axis',(1.,0.,0.));
#13049=DIRECTION('ref_axis',(0.,0.,-1.));
#13050=DIRECTION('',(1.,0.,0.));
#13051=DIRECTION('center_axis',(1.,0.,0.));
#13052=DIRECTION('ref_axis',(0.,0.,-1.));
#13053=DIRECTION('center_axis',(-1.,0.,0.));
#13054=DIRECTION('ref_axis',(0.,0.,-1.));
#13055=DIRECTION('center_axis',(1.,0.,0.));
#13056=DIRECTION('ref_axis',(0.,1.22464679914735E-16,1.));
#13057=DIRECTION('center_axis',(1.,0.,0.));
#13058=DIRECTION('ref_axis',(0.,0.,-1.));
#13059=DIRECTION('center_axis',(1.,0.,0.));
#13060=DIRECTION('ref_axis',(0.,0.,-1.));
#13061=DIRECTION('axis',(0.,0.,1.));
#13062=DIRECTION('refdir',(1.,0.,0.));
#13063=DIRECTION('center_axis',(0.,1.,0.));
#13064=DIRECTION('ref_axis',(0.,0.,1.));
#13065=DIRECTION('',(1.,0.,0.));
#13066=DIRECTION('',(0.,0.,1.));
#13067=DIRECTION('',(-1.,0.,0.));
#13068=DIRECTION('',(0.,0.,-1.));
#13069=DIRECTION('center_axis',(0.,1.,0.));
#13070=DIRECTION('ref_axis',(0.,0.,1.));
#13071=DIRECTION('',(-1.,0.,0.));
#13072=DIRECTION('',(0.,0.,-1.));
#13073=DIRECTION('',(1.,0.,0.));
#13074=DIRECTION('',(0.,0.,1.));
#13075=DIRECTION('center_axis',(0.,-1.,0.));
#13076=DIRECTION('ref_axis',(0.,0.,-1.));
#13077=DIRECTION('',(-1.,0.,0.));
#13078=DIRECTION('',(0.,0.,1.));
#13079=DIRECTION('',(1.,0.,0.));
#13080=DIRECTION('',(0.,0.,-1.));
#13081=DIRECTION('center_axis',(0.,-1.,0.));
#13082=DIRECTION('ref_axis',(0.,0.,-1.));
#13083=DIRECTION('',(-1.,0.,0.));
#13084=DIRECTION('',(0.,0.,1.));
#13085=DIRECTION('',(1.,0.,0.));
#13086=DIRECTION('',(0.,0.,-1.));
#13087=DIRECTION('center_axis',(1.,0.,0.));
#13088=DIRECTION('ref_axis',(0.,-0.279568819041295,0.960125656057506));
#13089=DIRECTION('center_axis',(1.,0.,0.));
#13090=DIRECTION('ref_axis',(0.,0.,-1.));
#13091=DIRECTION('',(1.,0.,0.));
#13092=DIRECTION('center_axis',(1.,0.,0.));
#13093=DIRECTION('ref_axis',(0.,0.,-1.));
#13094=DIRECTION('center_axis',(1.,0.,0.));
#13095=DIRECTION('ref_axis',(0.,0.,-1.));
#13096=DIRECTION('center_axis',(1.,0.,0.));
#13097=DIRECTION('ref_axis',(0.,0.,-1.));
#13098=DIRECTION('',(1.,0.,0.));
#13099=DIRECTION('center_axis',(1.,0.,0.));
#13100=DIRECTION('ref_axis',(0.,0.,-1.));
#13101=DIRECTION('center_axis',(1.,0.,0.));
#13102=DIRECTION('ref_axis',(0.,0.,-1.));
#13103=DIRECTION('center_axis',(1.,0.,0.));
#13104=DIRECTION('ref_axis',(0.,0.,-1.));
#13105=DIRECTION('',(1.,0.,0.));
#13106=DIRECTION('center_axis',(1.,0.,0.));
#13107=DIRECTION('ref_axis',(0.,0.,-1.));
#13108=DIRECTION('center_axis',(1.,0.,0.));
#13109=DIRECTION('ref_axis',(0.,0.279568819041297,0.960125656057505));
#13110=DIRECTION('center_axis',(1.,0.,0.));
#13111=DIRECTION('ref_axis',(0.,0.,-1.));
#13112=DIRECTION('',(1.,0.,0.));
#13113=DIRECTION('center_axis',(1.,0.,0.));
#13114=DIRECTION('ref_axis',(0.,0.,-1.));
#13115=DIRECTION('center_axis',(1.,0.,0.));
#13116=DIRECTION('ref_axis',(0.,0.,-1.));
#13117=DIRECTION('center_axis',(-1.,0.,0.));
#13118=DIRECTION('ref_axis',(0.,0.,-1.));
#13119=DIRECTION('center_axis',(-1.,0.,0.));
#13120=DIRECTION('ref_axis',(0.,0.,-1.));
#13121=DIRECTION('center_axis',(1.,0.,0.));
#13122=DIRECTION('ref_axis',(0.,0.,-1.));
#13123=DIRECTION('center_axis',(-1.,0.,0.));
#13124=DIRECTION('ref_axis',(0.,0.,-1.));
#13125=DIRECTION('center_axis',(1.,0.,0.));
#13126=DIRECTION('ref_axis',(0.,0.,-1.));
#13127=DIRECTION('center_axis',(-1.,0.,0.));
#13128=DIRECTION('ref_axis',(0.,0.,-1.));
#13129=DIRECTION('center_axis',(1.,0.,0.));
#13130=DIRECTION('ref_axis',(0.,0.,-1.));
#13131=DIRECTION('center_axis',(-1.,0.,0.));
#13132=DIRECTION('ref_axis',(0.,0.,-1.));
#13133=DIRECTION('center_axis',(1.,0.,0.));
#13134=DIRECTION('ref_axis',(0.,0.,-1.));
#13135=DIRECTION('center_axis',(-1.,0.,0.));
#13136=DIRECTION('ref_axis',(0.,0.,-1.));
#13137=DIRECTION('center_axis',(1.,0.,0.));
#13138=DIRECTION('ref_axis',(0.,0.,-1.));
#13139=DIRECTION('center_axis',(-1.,0.,0.));
#13140=DIRECTION('ref_axis',(0.,0.,-1.));
#13141=DIRECTION('',(1.,0.,0.));
#13142=DIRECTION('center_axis',(1.,0.,0.));
#13143=DIRECTION('ref_axis',(0.,0.,-1.));
#13144=DIRECTION('center_axis',(1.,0.,0.));
#13145=DIRECTION('ref_axis',(0.,0.,-1.));
#13146=DIRECTION('',(1.,0.,0.));
#13147=DIRECTION('center_axis',(1.,0.,0.));
#13148=DIRECTION('ref_axis',(0.,0.,-1.));
#13149=DIRECTION('center_axis',(-1.,0.,0.));
#13150=DIRECTION('ref_axis',(0.,0.,-1.));
#13151=DIRECTION('center_axis',(1.,0.,0.));
#13152=DIRECTION('ref_axis',(0.,1.22464679914735E-16,1.));
#13153=DIRECTION('center_axis',(1.,0.,0.));
#13154=DIRECTION('ref_axis',(0.,0.,-1.));
#13155=DIRECTION('center_axis',(1.,0.,0.));
#13156=DIRECTION('ref_axis',(0.,0.,-1.));
#13157=DIRECTION('',(0.,0.,1.));
#13158=DIRECTION('',(1.,0.,0.));
#13159=DIRECTION('',(0.,0.,1.));
#13160=DIRECTION('',(1.,0.,0.));
#13161=DIRECTION('',(0.,0.,1.));
#13162=DIRECTION('',(1.,0.,0.));
#13163=DIRECTION('',(0.,0.,1.));
#13164=DIRECTION('',(1.,0.,0.));
#13165=DIRECTION('',(0.,0.,1.));
#13166=DIRECTION('',(1.,0.,0.));
#13167=DIRECTION('',(0.,0.,1.));
#13168=DIRECTION('',(1.,0.,0.));
#13169=DIRECTION('',(0.,0.,1.));
#13170=DIRECTION('',(1.,0.,0.));
#13171=DIRECTION('',(0.,0.,1.));
#13172=DIRECTION('',(1.,0.,0.));
#13173=DIRECTION('',(1.,0.,0.));
#13174=DIRECTION('',(0.,1.,0.));
#13175=DIRECTION('',(0.,0.,1.));
#13176=DIRECTION('',(1.,0.,0.));
#13177=DIRECTION('',(1.,0.,0.));
#13178=DIRECTION('',(0.,1.,0.));
#13179=DIRECTION('',(0.,0.,1.));
#13180=DIRECTION('',(1.,0.,0.));
#13181=DIRECTION('',(0.,0.,1.));
#13182=DIRECTION('',(1.,0.,0.));
#13183=DIRECTION('',(0.,0.,1.));
#13184=DIRECTION('',(1.,0.,0.));
#13185=DIRECTION('',(0.,1.,0.));
#13186=DIRECTION('',(1.,0.,0.));
#13187=DIRECTION('',(0.,1.,0.));
#13188=DIRECTION('',(1.,0.,0.));
#13189=DIRECTION('',(0.,0.,1.));
#13190=DIRECTION('',(1.,0.,0.));
#13191=DIRECTION('',(0.,0.,1.));
#13192=DIRECTION('',(1.,0.,0.));
#13193=DIRECTION('',(-1.,0.,0.));
#13194=DIRECTION('',(0.,1.,0.));
#13195=DIRECTION('',(-1.,0.,0.));
#13196=DIRECTION('',(0.,1.,0.));
#13197=DIRECTION('',(0.,0.,1.));
#13198=DIRECTION('',(-1.,0.,0.));
#13199=DIRECTION('',(0.,0.,1.));
#13200=DIRECTION('',(-1.,0.,0.));
#13201=DIRECTION('',(0.,1.,0.));
#13202=DIRECTION('',(1.,0.,0.));
#13203=DIRECTION('',(0.,1.,0.));
#13204=DIRECTION('',(1.,0.,0.));
#13205=DIRECTION('',(0.,1.,0.));
#13206=DIRECTION('',(1.,0.,0.));
#13207=DIRECTION('',(0.,1.,0.));
#13208=DIRECTION('',(1.,0.,0.));
#13209=DIRECTION('',(0.,1.,0.));
#13210=DIRECTION('',(1.,0.,0.));
#13211=DIRECTION('',(0.,1.,0.));
#13212=DIRECTION('',(1.,0.,0.));
#13213=DIRECTION('',(0.,0.,1.));
#13214=DIRECTION('',(1.,0.,0.));
#13215=DIRECTION('',(0.,0.,1.));
#13216=DIRECTION('',(1.,0.,0.));
#13217=CARTESIAN_POINT('',(0.,0.,0.));
#13218=CARTESIAN_POINT('',(0.,0.,0.));
#13219=CARTESIAN_POINT('Origin',(5.91049210772187,0.55689895383893,8.58));
#13220=CARTESIAN_POINT('',(4.60649224223163,0.207493242950527,8.58));
#13221=CARTESIAN_POINT('',(5.91049210772187,0.55689895383893,9.93));
#13222=CARTESIAN_POINT('Origin',(5.91049210772187,0.55689895383893,8.58));
#13223=CARTESIAN_POINT('',(5.93637401223212,0.460306371210023,10.03));
#13224=CARTESIAN_POINT('Origin',(5.91049210772187,0.55689895383893,10.03));
#13225=CARTESIAN_POINT('Origin',(5.93637401223212,0.460306371210023,8.58));
#13226=CARTESIAN_POINT('Origin',(5.91049210772187,0.55689895383893,8.58));
#13227=CARTESIAN_POINT('Origin',(5.93637401223212,0.460306371210023,8.58));
#13228=CARTESIAN_POINT('',(4.52884652870087,0.497270990837247,8.58));
#13229=CARTESIAN_POINT('',(4.63237414674188,0.110900660321619,8.58));
#13230=CARTESIAN_POINT('',(5.83284639419111,0.84667670172565,9.93));
#13231=CARTESIAN_POINT('Origin',(5.83284639419111,0.84667670172565,8.58));
#13232=CARTESIAN_POINT('Origin',(5.83284639419111,0.84667670172565,8.58));
#13233=CARTESIAN_POINT('Origin',(6.30001167592482,0.557742789534021,7.49483504398303));
#13234=CARTESIAN_POINT('',(4.41021120669539,0.05137227994804,11.5901922029304));
#13235=CARTESIAN_POINT('',(4.41021120671322,0.0513722799528162,11.7069738861252));
#13236=CARTESIAN_POINT('',(4.41021120669539,0.05137227994804,5.29092677993983));
#13237=CARTESIAN_POINT('',(4.33293714059227,0.0306667563398384,11.6657994729934));
#13238=CARTESIAN_POINT('Ctrl Pts',(4.33293714059226,0.0306667563398384,
11.6657994729934));
#13239=CARTESIAN_POINT('Ctrl Pts',(4.35772155918772,0.0373077212873651,
11.6410754279018));
#13240=CARTESIAN_POINT('Ctrl Pts',(4.38339811720808,0.044187734273338,11.6158676377922));
#13241=CARTESIAN_POINT('Ctrl Pts',(4.41021120669538,0.0513722799480404,
11.5901922029304));
#13242=CARTESIAN_POINT('',(4.33293714061332,0.0306667563454775,11.573751331703));
#13243=CARTESIAN_POINT('',(4.33293714059227,0.0306667563398384,-0.5));
#13244=CARTESIAN_POINT('',(4.33293714059219,0.0306667563398168,3.61523506307464));
#13245=CARTESIAN_POINT('',(4.33293714059227,0.0306667563398384,-0.5));
#13246=CARTESIAN_POINT('',(4.34909964308327,0.0349974858299681,3.59949138964752));
#13247=CARTESIAN_POINT('Origin',(4.27445292104672,0.0149959569426778,3.46653399560907));
#13248=CARTESIAN_POINT('Ctrl Pts',(4.4102112066954,0.0513722799480404,11.706973886163));
#13249=CARTESIAN_POINT('Ctrl Pts',(4.50817751566127,0.0776222733209033,
11.6029328940868));
#13250=CARTESIAN_POINT('Ctrl Pts',(4.70981258666106,0.131650227761089,11.3959302972882));
#13251=CARTESIAN_POINT('Ctrl Pts',(5.04656750998174,0.22188343751207,11.1281422470874));
#13252=CARTESIAN_POINT('Ctrl Pts',(5.37607158806058,0.310173789136056,10.9130750253569));
#13253=CARTESIAN_POINT('Ctrl Pts',(5.62759741836264,0.377569932241062,10.7756758097979));
#13254=CARTESIAN_POINT('Ctrl Pts',(5.92870322026153,0.458250988696196,10.6347886165848));
#13255=CARTESIAN_POINT('Ctrl Pts',(6.23443464884433,0.540171478085771,10.5447321686106));
#13256=CARTESIAN_POINT('Ctrl Pts',(6.60142713036405,0.638506817137273,10.4592774903079));
#13257=CARTESIAN_POINT('Ctrl Pts',(6.86887110582377,0.710168214382273,10.3610377706145));
#13258=CARTESIAN_POINT('Ctrl Pts',(7.10758729640882,0.774132024869772,10.2019978237482));
#13259=CARTESIAN_POINT('Ctrl Pts',(7.37469139866462,0.845702353364252,9.92445780127518));
#13260=CARTESIAN_POINT('Ctrl Pts',(7.64695093531355,0.918654076341007,9.5279070047071));
#13261=CARTESIAN_POINT('Ctrl Pts',(7.87171191954179,0.978878600554987,9.09615331026656));
#13262=CARTESIAN_POINT('Ctrl Pts',(7.97590410013386,1.00679681120227,8.72233320794333));
#13263=CARTESIAN_POINT('Ctrl Pts',(8.02445425036305,1.01980578474859,8.33910068047419));
#13264=CARTESIAN_POINT('Ctrl Pts',(8.03003514943051,1.02130118214676,7.84937648135502));
#13265=CARTESIAN_POINT('Ctrl Pts',(8.10334949970651,1.04094570309683,7.36854474797747));
#13266=CARTESIAN_POINT('Ctrl Pts',(8.17397369844545,1.05986940011502,6.98613553279737));
#13267=CARTESIAN_POINT('Ctrl Pts',(8.19086884853079,1.06439644193639,6.74182415651423));
#13268=CARTESIAN_POINT('Ctrl Pts',(8.15926186591506,1.05592737646932,6.54872190268123));
#13269=CARTESIAN_POINT('Ctrl Pts',(8.08863405403125,1.03700271131187,6.36645372110484));
#13270=CARTESIAN_POINT('Ctrl Pts',(7.8697531842168,0.978353759006469,6.10374129848354));
#13271=CARTESIAN_POINT('Ctrl Pts',(7.59271262743873,0.904120965547118,5.95839742644866));
#13272=CARTESIAN_POINT('Ctrl Pts',(7.24661705601864,0.811384936681117,5.80579085268058));
#13273=CARTESIAN_POINT('Ctrl Pts',(6.8046210773698,0.692952471144354,5.63860904148901));
#13274=CARTESIAN_POINT('Ctrl Pts',(6.26783169213932,0.54912018886625,5.39183749253912));
#13275=CARTESIAN_POINT('Ctrl Pts',(5.76242378203297,0.413696547504953,5.13078873237884));
#13276=CARTESIAN_POINT('Ctrl Pts',(5.39028650561027,0.313982664813972,4.92283216185341));
#13277=CARTESIAN_POINT('Ctrl Pts',(5.0354367362137,0.21890095566979,4.68193520114933));
#13278=CARTESIAN_POINT('Ctrl Pts',(4.72268568825884,0.135099564938299,4.38319469956436));
#13279=CARTESIAN_POINT('Ctrl Pts',(4.48560194249773,0.071573166723062,4.01568874810612));
#13280=CARTESIAN_POINT('Ctrl Pts',(4.38680976101687,0.0451018814767583,
3.74027893176065));
#13281=CARTESIAN_POINT('Ctrl Pts',(4.34909964308327,0.0349974858299679,
3.59949138964752));
#13282=CARTESIAN_POINT('Origin',(5.83284639419111,0.84667670172565,8.58));
#13283=CARTESIAN_POINT('',(5.80696448968086,0.943269284354557,10.03));
#13284=CARTESIAN_POINT('Origin',(5.80696448968086,0.943269284354557,8.58));
#13285=CARTESIAN_POINT('Origin',(5.83284639419111,0.84667670172565,10.03));
#13286=CARTESIAN_POINT('Origin',(6.17060215337356,1.04070570267856,7.49483504398303));
#13287=CARTESIAN_POINT('',(4.13385008609474,0.494959631068776,2.88827625586697));
#13288=CARTESIAN_POINT('',(4.12726177229555,0.493194297692335,2.77093943708514));
#13289=CARTESIAN_POINT('Ctrl Pts',(4.13385008609474,0.494959631068776,2.88827625586696));
#13290=CARTESIAN_POINT('Ctrl Pts',(4.13152685057893,0.49433712198849,2.84917441683306));
#13291=CARTESIAN_POINT('Ctrl Pts',(4.1293392907043,0.493750967086684,2.8100639744616));
#13292=CARTESIAN_POINT('Ctrl Pts',(4.1272652896216,0.493195240171477,2.77094676616559));
#13293=CARTESIAN_POINT('',(4.14655803346906,0.498364715305182,3.0837901291539));
#13294=CARTESIAN_POINT('Ctrl Pts',(4.14655803346906,0.498364715305182,3.0837901291539));
#13295=CARTESIAN_POINT('Ctrl Pts',(4.14199767141828,0.497142769976483,3.01864202972875));
#13296=CARTESIAN_POINT('Ctrl Pts',(4.13772368979234,0.495997560051348,2.95347198278946));
#13297=CARTESIAN_POINT('Ctrl Pts',(4.13385008609474,0.494959631068777,2.88827625586697));
#13298=CARTESIAN_POINT('',(4.20352761804101,0.513629669484373,3.61216526483892));
#13299=CARTESIAN_POINT('Ctrl Pts',(4.20352761804101,0.513629669484373,3.61216526483892));
#13300=CARTESIAN_POINT('Ctrl Pts',(4.20348225943688,0.513617515683026,3.61188189200445));
#13301=CARTESIAN_POINT('Ctrl Pts',(4.20343686017451,0.513605350987338,3.61159855052174));
#13302=CARTESIAN_POINT('Ctrl Pts',(4.17554861335302,0.506132717773207,3.43668170480236));
#13303=CARTESIAN_POINT('Ctrl Pts',(4.15891388414094,0.501675455514513,3.26030247161513));
#13304=CARTESIAN_POINT('Ctrl Pts',(4.14655803346906,0.498364715305183,3.0837901291539));
#13305=CARTESIAN_POINT('',(4.20352736956267,0.513629602904919,11.769453644722));
#13306=CARTESIAN_POINT('',(4.20352761804101,0.513629669484373,6.5));
#13307=CARTESIAN_POINT('',(4.24867452199362,0.525724687915784,11.7797317356146));
#13308=CARTESIAN_POINT('Ctrl Pts',(4.24867356681531,0.525726489999986,11.7797315270537));
#13309=CARTESIAN_POINT('Ctrl Pts',(4.24163096531645,0.523839430615753,11.7763983972512));
#13310=CARTESIAN_POINT('Ctrl Pts',(4.23419172931546,0.521846093338737,11.7739226030364));
#13311=CARTESIAN_POINT('Ctrl Pts',(4.21900017669025,0.517775529081036,11.770542186514));
#13312=CARTESIAN_POINT('Ctrl Pts',(4.21127795560258,0.515706366175067,11.7696614596113));
#13313=CARTESIAN_POINT('Ctrl Pts',(4.2035273694791,0.513629602882414,11.7694536480639));
#13314=CARTESIAN_POINT('',(4.33613465287435,0.549161617378652,11.7628168777948));
#13315=CARTESIAN_POINT('Ctrl Pts',(4.33613465287435,0.549161617378653,11.7628168777948));
#13316=CARTESIAN_POINT('Ctrl Pts',(4.32047051975656,0.544964425559608,11.7794523105961));
#13317=CARTESIAN_POINT('Ctrl Pts',(4.28812302309206,0.536296939951185,11.7920460899797));
#13318=CARTESIAN_POINT('Ctrl Pts',(4.25705519011612,0.527972339194697,11.7836561768042));
#13319=CARTESIAN_POINT('Ctrl Pts',(4.24870939485228,0.525736090093557,11.7797108569314));
#13320=CARTESIAN_POINT('',(4.20352761804101,0.513629669484372,3.08701851589662));
#13321=CARTESIAN_POINT('Ctrl Pts',(4.33613465287435,0.549161617378653,11.7628168777948));
#13322=CARTESIAN_POINT('Ctrl Pts',(4.35205479627536,0.55342740694634,11.7459095600555));
#13323=CARTESIAN_POINT('Ctrl Pts',(4.39438451441832,0.564769620738584,11.7010611784437));
#13324=CARTESIAN_POINT('Ctrl Pts',(4.46445801430387,0.583545758443739,11.6277377103039));
#13325=CARTESIAN_POINT('Ctrl Pts',(4.56524008224957,0.610550232161327,11.5268404604711));
#13326=CARTESIAN_POINT('Ctrl Pts',(4.70129424855043,0.647005836148533,11.4029224160728));
#13327=CARTESIAN_POINT('Ctrl Pts',(4.85646075505348,0.688582576258383,11.2768795166233));
#13328=CARTESIAN_POINT('Ctrl Pts',(5.01695088441627,0.731585776814311,11.1598106424589));
#13329=CARTESIAN_POINT('Ctrl Pts',(5.18020418201412,0.775329366067371,11.051370419133));
#13330=CARTESIAN_POINT('Ctrl Pts',(5.34412061714924,0.819250642488016,10.9511663773825));
#13331=CARTESIAN_POINT('Ctrl Pts',(5.50802499472635,0.863168688095727,10.8599381259735));
#13332=CARTESIAN_POINT('Ctrl Pts',(5.67271528816759,0.907297319224552,10.7795199127532));
#13333=CARTESIAN_POINT('Ctrl Pts',(5.8394939294453,0.951985521469674,10.7114411549111));
#13334=CARTESIAN_POINT('Ctrl Pts',(6.00944121138842,0.997522758422198,10.6558377434042));
#13335=CARTESIAN_POINT('Ctrl Pts',(6.18264944336441,1.04393376430259,10.6103475969888));
#13336=CARTESIAN_POINT('Ctrl Pts',(6.35731808181363,1.0907360849181,10.5687216653907));
#13337=CARTESIAN_POINT('Ctrl Pts',(6.53037102597449,1.13710548155383,10.5222908830264));
#13338=CARTESIAN_POINT('Ctrl Pts',(6.69840611695161,1.18213034848124,10.462050267878));
#13339=CARTESIAN_POINT('Ctrl Pts',(6.85846176969156,1.22501713137695,10.3804015453596));
#13340=CARTESIAN_POINT('Ctrl Pts',(7.00901521774594,1.26535780620084,10.2733319413005));
#13341=CARTESIAN_POINT('Ctrl Pts',(7.15038910771078,1.30323882584776,10.1414720974144));
#13342=CARTESIAN_POINT('Ctrl Pts',(7.2837085682718,1.33896166764044,9.98835756998534));
#13343=CARTESIAN_POINT('Ctrl Pts',(7.4100830632121,1.37282361150359,9.81917361987377));
#13344=CARTESIAN_POINT('Ctrl Pts',(7.52979533329094,1.40490041759531,9.63939026966049));
#13345=CARTESIAN_POINT('Ctrl Pts',(7.64125800723788,1.4347667510656,9.45324999450471));
#13346=CARTESIAN_POINT('Ctrl Pts',(7.7408376555659,1.46144903741767,9.26297089919836));
#13347=CARTESIAN_POINT('Ctrl Pts',(7.82441721291024,1.48384411231184,9.06945407017055));
#13348=CARTESIAN_POINT('Ctrl Pts',(7.88861442185322,1.50104570260444,8.87266947141857));
#13349=CARTESIAN_POINT('Ctrl Pts',(7.93207481020654,1.51269087856646,8.67216210283894));
#13350=CARTESIAN_POINT('Ctrl Pts',(7.9568818673599,1.51933790949729,8.46752658699496));
#13351=CARTESIAN_POINT('Ctrl Pts',(7.96947772195623,1.52271295856436,8.25883677791438));
#13352=CARTESIAN_POINT('Ctrl Pts',(7.97819085477051,1.52504763546549,8.04662057355209));
#13353=CARTESIAN_POINT('Ctrl Pts',(7.99115812626861,1.52852220539144,7.8318867323277));
#13354=CARTESIAN_POINT('Ctrl Pts',(8.01405316627263,1.5346569128712,7.61613341658679));
#13355=CARTESIAN_POINT('Ctrl Pts',(8.04799304870936,1.54375107696133,7.40136016279815));
#13356=CARTESIAN_POINT('Ctrl Pts',(8.08710913224301,1.55423219995524,7.19009032473197));
#13357=CARTESIAN_POINT('Ctrl Pts',(8.12102374647152,1.56331959344938,6.98516923427904));
#13358=CARTESIAN_POINT('Ctrl Pts',(8.13767668870611,1.56778173587274,6.78954489191915));
#13359=CARTESIAN_POINT('Ctrl Pts',(8.12605341309117,1.56466728855831,6.60605451948904));
#13360=CARTESIAN_POINT('Ctrl Pts',(8.07889077726024,1.55203009837449,6.43720976255638));
#13361=CARTESIAN_POINT('Ctrl Pts',(7.99556800549189,1.52970382896804,6.28498018271691));
#13362=CARTESIAN_POINT('Ctrl Pts',(7.88027463155873,1.49881106252999,6.15052660592943));
#13363=CARTESIAN_POINT('Ctrl Pts',(7.73984733045563,1.46118368060413,6.03389995867286));
#13364=CARTESIAN_POINT('Ctrl Pts',(7.58187158370519,1.41885420683865,5.93381436957244));
#13365=CARTESIAN_POINT('Ctrl Pts',(7.41231922357235,1.37342278886626,5.84723737025948));
#13366=CARTESIAN_POINT('Ctrl Pts',(7.23512222452275,1.3259429960697,5.76979878895671));
#13367=CARTESIAN_POINT('Ctrl Pts',(7.05278517393707,1.277085930615,5.69662713609756));
#13368=CARTESIAN_POINT('Ctrl Pts',(6.86668148224273,1.22721959671705,5.62308582598972));
#13369=CARTESIAN_POINT('Ctrl Pts',(6.6774713630728,1.17652089808567,5.54547963906641));
#13370=CARTESIAN_POINT('Ctrl Pts',(6.4854907752383,1.12507985461296,5.46195513100458));
#13371=CARTESIAN_POINT('Ctrl Pts',(6.29101491648524,1.07297020531273,5.37226655127806));
#13372=CARTESIAN_POINT('Ctrl Pts',(6.09444768929516,1.02030017552872,5.27709955371581));
#13373=CARTESIAN_POINT('Ctrl Pts',(5.89654491782883,0.967272287734439,5.17752467829117));
#13374=CARTESIAN_POINT('Ctrl Pts',(5.69860439377644,0.914234284165208,5.07442896098936));
#13375=CARTESIAN_POINT('Ctrl Pts',(5.50271582364677,0.861746099992474,4.96787993373722));
#13376=CARTESIAN_POINT('Ctrl Pts',(5.31184140107964,0.810601452609855,4.85676111532844));
#13377=CARTESIAN_POINT('Ctrl Pts',(5.12937361465137,0.761709356591708,4.73929437247794));
#13378=CARTESIAN_POINT('Ctrl Pts',(4.95878680959194,0.716000759936628,4.61340315498245));
#13379=CARTESIAN_POINT('Ctrl Pts',(4.80324392104458,0.674323168561959,4.47714872481864));
#13380=CARTESIAN_POINT('Ctrl Pts',(4.66524062494947,0.637345296820439,4.32911151507775));
#13381=CARTESIAN_POINT('Ctrl Pts',(4.54618516499875,0.60544448247213,4.16885849319143));
#13382=CARTESIAN_POINT('Ctrl Pts',(4.446442617986,0.578718547549039,3.99681013615577));
#13383=CARTESIAN_POINT('Ctrl Pts',(4.3654670825206,0.557021218214407,3.81399668859083));
#13384=CARTESIAN_POINT('Ctrl Pts',(4.30190073863269,0.539988667703842,3.62185203209172));
#13385=CARTESIAN_POINT('Ctrl Pts',(4.25745603462795,0.528079745157933,3.43759550531468));
#13386=CARTESIAN_POINT('Ctrl Pts',(4.23093262286488,0.520972818395501,3.28931577678263));
#13387=CARTESIAN_POINT('Ctrl Pts',(4.21521358817958,0.516760915745777,3.18044435652352));
#13388=CARTESIAN_POINT('Ctrl Pts',(4.20662995714442,0.514460938741779,3.11273802327794));
#13389=CARTESIAN_POINT('Ctrl Pts',(4.20352761804101,0.513629669484372,3.08701851589662));
#13390=CARTESIAN_POINT('',(4.19355650923267,0.510830172248245,2.99707929452952));
#13391=CARTESIAN_POINT('Ctrl Pts',(4.20352761804066,0.51362966948428,3.0870185158938));
#13392=CARTESIAN_POINT('Ctrl Pts',(4.20154142505499,0.513097470677755,3.07055226141507));
#13393=CARTESIAN_POINT('Ctrl Pts',(4.19944545032181,0.512535855940644,3.05259191451735));
#13394=CARTESIAN_POINT('Ctrl Pts',(4.19741839741691,0.51199270875176,3.03459621555749));
#13395=CARTESIAN_POINT('Ctrl Pts',(4.1954566774867,0.511467067480684,3.01656643638677));
#13396=CARTESIAN_POINT('Ctrl Pts',(4.19355679933009,0.510957996662904,2.99850373251447));
#13397=CARTESIAN_POINT('Ctrl Pts',(4.19340242707872,0.510916632742816,2.99703196752542));
#13398=CARTESIAN_POINT('Ctrl Pts',(4.1272652896216,0.493195240171478,2.77094676616559));
#13399=CARTESIAN_POINT('Ctrl Pts',(4.14396588850096,0.49767015215432,2.79475655535354));
#13400=CARTESIAN_POINT('Ctrl Pts',(4.15972316042568,0.501892300390747,2.83474868902384));
#13401=CARTESIAN_POINT('Ctrl Pts',(4.18183336047469,0.507816710638371,2.91779295323766));
#13402=CARTESIAN_POINT('Ctrl Pts',(4.18947454830694,0.509864160797954,2.95856894798348));
#13403=CARTESIAN_POINT('Ctrl Pts',(4.19349145124426,0.510940486696084,2.99676457959157));
#13404=CARTESIAN_POINT('Origin',(-5.91049210772187,0.556898953838929,8.58));
#13405=CARTESIAN_POINT('',(-7.21449197321211,0.906304664727332,8.58));
#13406=CARTESIAN_POINT('',(-5.91049210772187,0.556898953838929,9.93));
#13407=CARTESIAN_POINT('Origin',(-5.91049210772187,0.556898953838929,8.58));
#13408=CARTESIAN_POINT('',(-5.93637401223212,0.460306371210023,10.03));
#13409=CARTESIAN_POINT('Origin',(-5.91049210772187,0.556898953838929,10.03));
#13410=CARTESIAN_POINT('Origin',(-5.93637401223212,0.460306371210023,8.58));
#13411=CARTESIAN_POINT('Origin',(-5.91049210772187,0.556898953838929,8.58));
#13412=CARTESIAN_POINT('Origin',(-5.93637401223212,0.460306371210023,8.58));
#13413=CARTESIAN_POINT('',(-7.13684625968135,1.19608241261405,8.58));
#13414=CARTESIAN_POINT('',(-7.24037387772236,0.809712082098426,8.58));
#13415=CARTESIAN_POINT('',(-5.83284639419111,0.84667670172565,9.93));
#13416=CARTESIAN_POINT('Origin',(-5.83284639419111,0.84667670172565,8.58));
#13417=CARTESIAN_POINT('Origin',(-5.83284639419111,0.84667670172565,8.58));
#13418=CARTESIAN_POINT('Origin',(-6.30001167592471,0.557742789533991,7.49483504398145));
#13419=CARTESIAN_POINT('',(-4.41021120669539,0.0513722799480398,4.08908175574846));
#13420=CARTESIAN_POINT('',(-4.41021120669539,0.0513722799480399,3.79515655425572));
#13421=CARTESIAN_POINT('',(-4.41021120669539,0.0513722799480398,9.69874330802488));
#13422=CARTESIAN_POINT('',(-4.33293714059227,0.0306667563398384,3.94826261099145));
#13423=CARTESIAN_POINT('Ctrl Pts',(-4.33293714059227,0.0306667563398375,
3.94826261099145));
#13424=CARTESIAN_POINT('Ctrl Pts',(-4.33856564926069,0.0321749106921323,
3.95968497399622));
#13425=CARTESIAN_POINT('Ctrl Pts',(-4.34431878377979,0.0337164584404719,
3.97106471407484));
#13426=CARTESIAN_POINT('Ctrl Pts',(-4.35019991655898,0.0352923032192356,
3.98240125579818));
#13427=CARTESIAN_POINT('Ctrl Pts',(-4.36917645914159,0.0403770524793794,
4.01898066572307));
#13428=CARTESIAN_POINT('Ctrl Pts',(-4.3891749803178,0.0457356400783655,
4.05451189417237));
#13429=CARTESIAN_POINT('Ctrl Pts',(-4.41021120669539,0.0513722799480392,
4.08908175574845));
#13430=CARTESIAN_POINT('',(-4.33293714050842,0.0306667563173706,11.7119910933489));
#13431=CARTESIAN_POINT('',(-4.33293714059227,0.0306667563398384,-0.5));
#13432=CARTESIAN_POINT('',(-4.36526624577324,0.039329313965101,11.7547577775405));
#13433=CARTESIAN_POINT('Ctrl Pts',(-4.36526624577325,0.0393293139651038,
11.7547577775405));
#13434=CARTESIAN_POINT('Ctrl Pts',(-4.35509026165876,0.0366026672394349,
11.7400274737341));
#13435=CARTESIAN_POINT('Ctrl Pts',(-4.34410968865593,0.0336604315708949,
11.7259232172676));
#13436=CARTESIAN_POINT('Ctrl Pts',(-4.33293714047413,0.0306667563081824,
11.7119910933921));
#13437=CARTESIAN_POINT('Ctrl Pts',(-4.41021120669539,0.0513722799480397,
3.79515655425571));
#13438=CARTESIAN_POINT('Ctrl Pts',(-4.45903808887791,0.0644554035977742,
3.93047791113146));
#13439=CARTESIAN_POINT('Ctrl Pts',(-4.582867212341,0.0976353172291641,4.19123490599198));
#13440=CARTESIAN_POINT('Ctrl Pts',(-4.94740819214276,0.195313778375095,
4.6367821770228));
#13441=CARTESIAN_POINT('Ctrl Pts',(-5.46260381387957,0.333360029163525,
4.97227704636915));
#13442=CARTESIAN_POINT('Ctrl Pts',(-6.04190293430869,0.488582760658567,
5.27702023853286));
#13443=CARTESIAN_POINT('Ctrl Pts',(-6.54703332936491,0.623932042086293,
5.5237763509783));
#13444=CARTESIAN_POINT('Ctrl Pts',(-7.06475153359634,0.762654216816996,
5.73854350352349));
#13445=CARTESIAN_POINT('Ctrl Pts',(-7.50199905569102,0.879814337254775,
5.90674273368555));
#13446=CARTESIAN_POINT('Ctrl Pts',(-7.78652969114894,0.956054091247638,
6.07256733032961));
#13447=CARTESIAN_POINT('Ctrl Pts',(-7.93300439915508,0.995301870969469,
6.19198615507442));
#13448=CARTESIAN_POINT('Ctrl Pts',(-8.03020970920239,1.02134795529666,6.29626516002264));
#13449=CARTESIAN_POINT('Ctrl Pts',(-8.10816249423483,1.04223534109386,6.41672618659136));
#13450=CARTESIAN_POINT('Ctrl Pts',(-8.17753074630009,1.06082250821511,6.59727787804477));
#13451=CARTESIAN_POINT('Ctrl Pts',(-8.19098371232079,1.06442721959616,6.8408696776684));
#13452=CARTESIAN_POINT('Ctrl Pts',(-8.14971164745181,1.05336840314455,7.12565705017148));
#13453=CARTESIAN_POINT('Ctrl Pts',(-8.09711272128414,1.03927456335518,7.40937238436613));
#13454=CARTESIAN_POINT('Ctrl Pts',(-8.05552374714506,1.02813083132057,7.6951718595586));
#13455=CARTESIAN_POINT('Ctrl Pts',(-8.02521849097772,1.02001056240412,8.07845955750479));
#13456=CARTESIAN_POINT('Ctrl Pts',(-8.01790604838202,1.0180511993159,8.46573709363457));
#13457=CARTESIAN_POINT('Ctrl Pts',(-7.94784659338026,0.999278824926013,
8.84438522402643));
#13458=CARTESIAN_POINT('Ctrl Pts',(-7.81984691825478,0.964981415344694,
9.20903949392042));
#13459=CARTESIAN_POINT('Ctrl Pts',(-7.58470305177623,0.901974806216633,
9.62563358808958));
#13460=CARTESIAN_POINT('Ctrl Pts',(-7.3194406724111,0.830897965883391,9.99304501740382));
#13461=CARTESIAN_POINT('Ctrl Pts',(-7.07733743840935,0.766026599847657,
10.2205558508687));
#13462=CARTESIAN_POINT('Ctrl Pts',(-6.8418306113212,0.702922735717372,10.3784329123269));
#13463=CARTESIAN_POINT('Ctrl Pts',(-6.60664228072597,0.639904212465156,
10.4553494743371));
#13464=CARTESIAN_POINT('Ctrl Pts',(-6.33491900485657,0.567096180131211,
10.5234765064095));
#13465=CARTESIAN_POINT('Ctrl Pts',(-6.06384344546407,0.494461702904175,
10.5898397099152));
#13466=CARTESIAN_POINT('Ctrl Pts',(-5.70632931912773,0.398666081469635,
10.7280695887413));
#13467=CARTESIAN_POINT('Ctrl Pts',(-5.33566097788268,0.29934579877324,10.9374674705902));
#13468=CARTESIAN_POINT('Ctrl Pts',(-4.98550528234724,0.205521862929361,
11.1722294927876));
#13469=CARTESIAN_POINT('Ctrl Pts',(-4.65974554183767,0.118234803533251,
11.442738806744));
#13470=CARTESIAN_POINT('Ctrl Pts',(-4.462637168512,0.0654197740792256,11.6512961064053));
#13471=CARTESIAN_POINT('Ctrl Pts',(-4.36526624577324,0.0393293139651011,
11.7547577775405));
#13472=CARTESIAN_POINT('Origin',(-5.83284639419111,0.84667670172565,8.58));
#13473=CARTESIAN_POINT('',(-5.80696448968086,0.943269284354557,10.03));
#13474=CARTESIAN_POINT('Origin',(-5.80696448968086,0.943269284354557,8.58));
#13475=CARTESIAN_POINT('Origin',(-5.83284639419111,0.84667670172565,10.03));
#13476=CARTESIAN_POINT('Origin',(-6.17060215337345,1.04070570267853,7.49483504398145));
#13477=CARTESIAN_POINT('',(-4.24038550259138,0.523505709884365,3.72695850307423));
#13478=CARTESIAN_POINT('',(-4.20352761804101,0.513629669484373,3.61216526483895));
#13479=CARTESIAN_POINT('Ctrl Pts',(-4.24038388893983,0.523505277507739,
3.72695930646786));
#13480=CARTESIAN_POINT('Ctrl Pts',(-4.22951847389614,0.520593898321352,
3.6959946199449));
#13481=CARTESIAN_POINT('Ctrl Pts',(-4.21930406783922,0.517856956467237,
3.66463907541042));
#13482=CARTESIAN_POINT('Ctrl Pts',(-4.20969621562989,0.515282540226749,
3.63288801911005));
#13483=CARTESIAN_POINT('Ctrl Pts',(-4.20760920009148,0.514723326098641,
3.62599106166146));
#13484=CARTESIAN_POINT('Ctrl Pts',(-4.20555351635821,0.514172507302417,
3.6190845391588));
#13485=CARTESIAN_POINT('Ctrl Pts',(-4.203527618041,0.513629669484373,3.61216526483892));
#13486=CARTESIAN_POINT('',(-4.35319009416574,0.553731609099237,3.76716196298096));
#13487=CARTESIAN_POINT('Ctrl Pts',(-4.35319009416574,0.553731609099236,
3.76716196298096));
#13488=CARTESIAN_POINT('Ctrl Pts',(-4.34602020468552,0.551810443003191,
3.7472909589409));
#13489=CARTESIAN_POINT('Ctrl Pts',(-4.31557469838348,0.543652594176403,
3.71389681896982));
#13490=CARTESIAN_POINT('Ctrl Pts',(-4.26651510466209,0.530507115657757,
3.71290855827619));
#13491=CARTESIAN_POINT('Ctrl Pts',(-4.24417455750459,0.524520984088436,
3.72454107717024));
#13492=CARTESIAN_POINT('Ctrl Pts',(-4.24038711624293,0.523506142260992,
3.7269576996806));
#13493=CARTESIAN_POINT('',(-4.21983606380434,0.517999504581966,11.8857786587691));
#13494=CARTESIAN_POINT('Ctrl Pts',(-4.35319009416574,0.553731609099237,
3.76716196298096));
#13495=CARTESIAN_POINT('Ctrl Pts',(-4.35641988647835,0.55459702934112,3.77611317712024));
#13496=CARTESIAN_POINT('Ctrl Pts',(-4.37357151210268,0.559192793576042,
3.82283506370591));
#13497=CARTESIAN_POINT('Ctrl Pts',(-4.40695017775135,0.56813658008103,3.9061004919638));
#13498=CARTESIAN_POINT('Ctrl Pts',(-4.46167983075915,0.582801346406506,
4.02309317686375));
#13499=CARTESIAN_POINT('Ctrl Pts',(-4.54618516499859,0.605444482472087,
4.16885849319142));
#13500=CARTESIAN_POINT('Ctrl Pts',(-4.66524062494938,0.637345296820415,
4.32911151507774));
#13501=CARTESIAN_POINT('Ctrl Pts',(-4.80324392104458,0.674323168561958,
4.47714872481861));
#13502=CARTESIAN_POINT('Ctrl Pts',(-4.958786809592,0.716000759936643,4.61340315498244));
#13503=CARTESIAN_POINT('Ctrl Pts',(-5.12937361465147,0.761709356591734,
4.73929437247796));
#13504=CARTESIAN_POINT('Ctrl Pts',(-5.31184140107974,0.810601452609883,
4.8567611153285));
#13505=CARTESIAN_POINT('Ctrl Pts',(-5.50271582364683,0.861746099992491,
4.96787993373728));
#13506=CARTESIAN_POINT('Ctrl Pts',(-5.69860439377643,0.914234284165206,
5.07442896098937));
#13507=CARTESIAN_POINT('Ctrl Pts',(-5.89654491782873,0.967272287734412,
5.17752467829109));
#13508=CARTESIAN_POINT('Ctrl Pts',(-6.09444768929498,1.02030017552868,5.27709955371564));
#13509=CARTESIAN_POINT('Ctrl Pts',(-6.29101491648506,1.07297020531268,5.37226655127787));
#13510=CARTESIAN_POINT('Ctrl Pts',(-6.4854907752382,1.12507985461293,5.46195513100446));
#13511=CARTESIAN_POINT('Ctrl Pts',(-6.67747136307279,1.17652089808567,5.54547963906637));
#13512=CARTESIAN_POINT('Ctrl Pts',(-6.86668148224272,1.22721959671704,5.62308582598972));
#13513=CARTESIAN_POINT('Ctrl Pts',(-7.05278517393693,1.27708593061496,5.69662713609756));
#13514=CARTESIAN_POINT('Ctrl Pts',(-7.23512222452253,1.32594299606964,5.76979878895672));
#13515=CARTESIAN_POINT('Ctrl Pts',(-7.4123192235721,1.37342278886619,5.84723737025949));
#13516=CARTESIAN_POINT('Ctrl Pts',(-7.58187158370505,1.41885420683861,5.93381436957244));
#13517=CARTESIAN_POINT('Ctrl Pts',(-7.73984733045567,1.46118368060414,6.03389995867283));
#13518=CARTESIAN_POINT('Ctrl Pts',(-7.88027463155893,1.49881106253004,6.15052660592937));
#13519=CARTESIAN_POINT('Ctrl Pts',(-7.99556800549214,1.5297038289681,6.28498018271686));
#13520=CARTESIAN_POINT('Ctrl Pts',(-8.0788907772604,1.55203009837453,6.43720976255636));
#13521=CARTESIAN_POINT('Ctrl Pts',(-8.12605341309117,1.56466728855831,6.60605451948903));
#13522=CARTESIAN_POINT('Ctrl Pts',(-8.13767668870588,1.56778173587268,6.78954489191904));
#13523=CARTESIAN_POINT('Ctrl Pts',(-8.12102374647115,1.56331959344928,6.9851692342788));
#13524=CARTESIAN_POINT('Ctrl Pts',(-8.08710913224264,1.55423219995514,7.19009032473164));
#13525=CARTESIAN_POINT('Ctrl Pts',(-8.04799304870916,1.54375107696127,7.40136016279791));
#13526=CARTESIAN_POINT('Ctrl Pts',(-8.01405316627267,1.53465691287121,7.61613341658677));
#13527=CARTESIAN_POINT('Ctrl Pts',(-7.99115812626882,1.5285222053915,7.83188673232793));
#13528=CARTESIAN_POINT('Ctrl Pts',(-7.97819085477082,1.52504763546557,8.04662057355248));
#13529=CARTESIAN_POINT('Ctrl Pts',(-7.96947772195652,1.52271295856444,8.25883677791483));
#13530=CARTESIAN_POINT('Ctrl Pts',(-7.95688186736008,1.51933790949734,8.46752658699528));
#13531=CARTESIAN_POINT('Ctrl Pts',(-7.93207481020656,1.51269087856646,8.67216210283896));
#13532=CARTESIAN_POINT('Ctrl Pts',(-7.88861442185311,1.50104570260441,8.87266947141823));
#13533=CARTESIAN_POINT('Ctrl Pts',(-7.82441721291003,1.48384411231178,9.06945407016992));
#13534=CARTESIAN_POINT('Ctrl Pts',(-7.74083765556568,1.46144903741761,9.26297089919765));
#13535=CARTESIAN_POINT('Ctrl Pts',(-7.6412580072377,1.43476675106555,9.4532499945042));
#13536=CARTESIAN_POINT('Ctrl Pts',(-7.52979533329092,1.4049004175953,9.63939026966035));
#13537=CARTESIAN_POINT('Ctrl Pts',(-7.41008306321222,1.37282361150362,9.81917361987397));
#13538=CARTESIAN_POINT('Ctrl Pts',(-7.28370856827199,1.33896166764049,9.98835756998572));
#13539=CARTESIAN_POINT('Ctrl Pts',(-7.15038910771094,1.30323882584781,10.1414720974148));
#13540=CARTESIAN_POINT('Ctrl Pts',(-7.00901521774607,1.26535780620087,10.2733319413008));
#13541=CARTESIAN_POINT('Ctrl Pts',(-6.85846176969162,1.22501713137696,10.3804015453596));
#13542=CARTESIAN_POINT('Ctrl Pts',(-6.69840611695159,1.18213034848123,10.4620502678778));
#13543=CARTESIAN_POINT('Ctrl Pts',(-6.5303710259744,1.13710548155381,10.522290883026));
#13544=CARTESIAN_POINT('Ctrl Pts',(-6.35731808181357,1.09073608491808,10.5687216653902));
#13545=CARTESIAN_POINT('Ctrl Pts',(-6.18264944336438,1.04393376430258,10.6103475969885));
#13546=CARTESIAN_POINT('Ctrl Pts',(-6.00944121138848,0.997522758422214,
10.6558377434043));
#13547=CARTESIAN_POINT('Ctrl Pts',(-5.83949392944539,0.9519855214697,10.7114411549114));
#13548=CARTESIAN_POINT('Ctrl Pts',(-5.67271528816766,0.907297319224571,
10.7795199127535));
#13549=CARTESIAN_POINT('Ctrl Pts',(-5.5080249947264,0.86316868809574,10.8599381259737));
#13550=CARTESIAN_POINT('Ctrl Pts',(-5.34412061714928,0.819250642488025,
10.9511663773826));
#13551=CARTESIAN_POINT('Ctrl Pts',(-5.18020418201415,0.77532936606738,11.0513704191329));
#13552=CARTESIAN_POINT('Ctrl Pts',(-5.01695088441632,0.731585776814323,
11.1598106424589));
#13553=CARTESIAN_POINT('Ctrl Pts',(-4.85646075505354,0.6885825762584,11.2768795166235));
#13554=CARTESIAN_POINT('Ctrl Pts',(-4.70129424855049,0.64700583614855,11.4029224160731));
#13555=CARTESIAN_POINT('Ctrl Pts',(-4.55372957684968,0.607466001534954,
11.5373242211527));
#13556=CARTESIAN_POINT('Ctrl Pts',(-4.42837559321091,0.573877502850922,
11.6641229448127));
#13557=CARTESIAN_POINT('Ctrl Pts',(-4.33577812365105,0.549066085661191,
11.7630935610003));
#13558=CARTESIAN_POINT('Ctrl Pts',(-4.27132531937695,0.531796008806026,
11.8319171323704));
#13559=CARTESIAN_POINT('Ctrl Pts',(-4.23290575435463,0.52150151738474,11.8721941731916));
#13560=CARTESIAN_POINT('Ctrl Pts',(-4.21983606290434,0.517999504115311,
11.8857786577829));
#13561=CARTESIAN_POINT('',(-4.1874280189678,0.50930672791011,11.9066032159468));
#13562=CARTESIAN_POINT('Ctrl Pts',(-4.18742959608618,0.509316217501841,
11.9066111158145));
#13563=CARTESIAN_POINT('Ctrl Pts',(-4.19350514643691,0.510944156311893,
11.90450243125));
#13564=CARTESIAN_POINT('Ctrl Pts',(-4.19934410120603,0.512508699526892,
11.901643125283));
#13565=CARTESIAN_POINT('Ctrl Pts',(-4.21023945601472,0.515428101049129,
11.8946395116115));
#13566=CARTESIAN_POINT('Ctrl Pts',(-4.21530831280245,0.516786297131982,
11.8904852125323));
#13567=CARTESIAN_POINT('Ctrl Pts',(-4.21983606433895,0.517999504499715,
11.8857786592622));
#13568=CARTESIAN_POINT('',(-4.16769131691124,0.504008073901423,11.877637340138));
#13569=CARTESIAN_POINT('Ctrl Pts',(-4.16763707611828,0.504012827760267,
11.8776857726864));
#13570=CARTESIAN_POINT('Ctrl Pts',(-4.17121106796204,0.504970475988557,
11.8820075339236));
#13571=CARTESIAN_POINT('Ctrl Pts',(-4.17467687370206,0.505899135837717,
11.886562635604));
#13572=CARTESIAN_POINT('Ctrl Pts',(-4.18131563754359,0.507677987247797,
11.8961437713168));
#13573=CARTESIAN_POINT('Ctrl Pts',(-4.18453611370009,0.508540911233175,
11.9012960415207));
#13574=CARTESIAN_POINT('Ctrl Pts',(-4.18742622136955,0.509315313249245,
11.9065959606927));
#13575=CARTESIAN_POINT('',(-4.08479144096579,0.481813289987988,11.8776398161281));
#13576=CARTESIAN_POINT('Ctrl Pts',(-4.08479023695801,0.481814084111799,
11.8776392691564));
#13577=CARTESIAN_POINT('Ctrl Pts',(-4.08706116705159,0.482422577996443,
11.8748861572519));
#13578=CARTESIAN_POINT('Ctrl Pts',(-4.08944735162265,0.48306195422525,11.8721644698882));
#13579=CARTESIAN_POINT('Ctrl Pts',(-4.09704796925229,0.485098533581088,
11.8641214958086));
#13580=CARTESIAN_POINT('Ctrl Pts',(-4.10372042299868,0.486886412173969,
11.8578732851267));
#13581=CARTESIAN_POINT('Ctrl Pts',(-4.11372524923515,0.489567197284444,
11.8523156024532));
#13582=CARTESIAN_POINT('Ctrl Pts',(-4.1165662789659,0.490328448906532,11.8510857204423));
#13583=CARTESIAN_POINT('Ctrl Pts',(-4.12093513745218,0.491499081009779,
11.8499489173249));
#13584=CARTESIAN_POINT('Ctrl Pts',(-4.12235572296345,0.491879725750239,
11.8496888852406));
#13585=CARTESIAN_POINT('Ctrl Pts',(-4.12495943119795,0.492577387269001,
11.8494326147479));
#13586=CARTESIAN_POINT('Ctrl Pts',(-4.12612349683335,0.492889297715944,
11.84939639251));
#13587=CARTESIAN_POINT('Ctrl Pts',(-4.12867719428593,0.493573558886076,
11.8494923231472));
#13588=CARTESIAN_POINT('Ctrl Pts',(-4.1300494846765,0.493941262988009,11.849656558201));
#13589=CARTESIAN_POINT('Ctrl Pts',(-4.13413098098875,0.495034896628787,
11.8504660257216));
#13590=CARTESIAN_POINT('Ctrl Pts',(-4.13674238668242,0.495734620675518,
11.8514172338417));
#13591=CARTESIAN_POINT('Ctrl Pts',(-4.14602007144597,0.498220568815541,
11.8559209100288));
#13592=CARTESIAN_POINT('Ctrl Pts',(-4.15225831333328,0.499892100691434,
11.8612576457903));
#13593=CARTESIAN_POINT('Ctrl Pts',(-4.16089398054571,0.502206020747108,
11.8697337781851));
#13594=CARTESIAN_POINT('Ctrl Pts',(-4.16443685648729,0.503155331494539,
11.8736636802312));
#13595=CARTESIAN_POINT('Ctrl Pts',(-4.16770535281746,0.504031122446673,
11.8776253118062));
#13596=CARTESIAN_POINT('',(-4.07626606489887,0.479531832015509,11.8887931799445));
#13597=CARTESIAN_POINT('Ctrl Pts',(-4.07627028629145,0.479531170211144,
11.8887900280456));
#13598=CARTESIAN_POINT('Ctrl Pts',(-4.0776217174446,0.479893285097256,11.8868801280725));
#13599=CARTESIAN_POINT('Ctrl Pts',(-4.07901087220012,0.480265508002298,
11.8849921870643));
#13600=CARTESIAN_POINT('Ctrl Pts',(-4.08185066713631,0.481026428762121,
11.8812787398917));
#13601=CARTESIAN_POINT('Ctrl Pts',(-4.0833083652902,0.481417017795125,11.8794441008497));
#13602=CARTESIAN_POINT('Ctrl Pts',(-4.08479586226042,0.481815591407038,
11.8776442482011));
#13603=CARTESIAN_POINT('',(-4.08038520490284,0.480637587265309,11.8829275774895));
#13604=CARTESIAN_POINT('Ctrl Pts',(-4.08037603631363,0.48063130261391,11.8829200406371));
#13605=CARTESIAN_POINT('Ctrl Pts',(-4.07969798014178,0.480449618010238,
11.8838896584534));
#13606=CARTESIAN_POINT('Ctrl Pts',(-4.07901808066457,0.480267439494496,
11.88485801079));
#13607=CARTESIAN_POINT('Ctrl Pts',(-4.0776425844075,0.479898876383224,11.8868093475648));
#13608=CARTESIAN_POINT('Ctrl Pts',(-4.07694681683877,0.479712446024951,
11.8877924353392));
#13609=CARTESIAN_POINT('Ctrl Pts',(-4.07624931525263,0.479525551038226,
11.8887740875086));
#13610=CARTESIAN_POINT('',(-4.12427480026047,0.492417973766977,11.8128235778692));
#13611=CARTESIAN_POINT('Ctrl Pts',(-4.12423812645742,0.492384114246278,
11.8127998597806));
#13612=CARTESIAN_POINT('Ctrl Pts',(-4.11801102587266,0.490715567673405,
11.8242536640082));
#13613=CARTESIAN_POINT('Ctrl Pts',(-4.11123809259506,0.488900765674664,
11.8357141226374));
#13614=CARTESIAN_POINT('Ctrl Pts',(-4.0966932732167,0.485003493068176,11.8589805842168));
#13615=CARTESIAN_POINT('Ctrl Pts',(-4.08862759438386,0.482842300935126,
11.8711181616458));
#13616=CARTESIAN_POINT('Ctrl Pts',(-4.0803883880346,0.480634612247568,11.8829292871397));
#13617=CARTESIAN_POINT('',(-4.20352761804114,0.513629669484408,11.6617726299258));
#13618=CARTESIAN_POINT('Ctrl Pts',(-4.20352761804102,0.513629669484374,
11.6617726299262));
#13619=CARTESIAN_POINT('Ctrl Pts',(-4.20343490116772,0.51360482607305,11.6619472559298));
#13620=CARTESIAN_POINT('Ctrl Pts',(-4.20334221118164,0.513579989866137,
11.6621218699999));
#13621=CARTESIAN_POINT('Ctrl Pts',(-4.19007529654029,0.510025130801935,
11.687120248245));
#13622=CARTESIAN_POINT('Ctrl Pts',(-4.17722348491259,0.506581497959521,
11.7121079587146));
#13623=CARTESIAN_POINT('Ctrl Pts',(-4.15123059201542,0.499616723298776,
11.7623137554701));
#13624=CARTESIAN_POINT('Ctrl Pts',(-4.13789818430393,0.496044315714815,
11.7879024491707));
#13625=CARTESIAN_POINT('Ctrl Pts',(-4.12430337644551,0.492401597927895,
11.8128379265828));
#13626=CARTESIAN_POINT('',(-4.20352761804101,0.513629669484372,-0.5));
#13627=CARTESIAN_POINT('Ctrl Pts',(-4.4618940931088,0.148042762057828,3.76716196298096));
#13628=CARTESIAN_POINT('Ctrl Pts',(-4.33144929437701,0.63486937850796,3.76716196298096));
#13629=CARTESIAN_POINT('Ctrl Pts',(-4.45472420362858,0.146121595961783,
3.7472909589409));
#13630=CARTESIAN_POINT('Ctrl Pts',(-4.32427940489679,0.632948212411915,
3.7472909589409));
#13631=CARTESIAN_POINT('Ctrl Pts',(-4.42427869732654,0.137963747134995,
3.71389681896982));
#13632=CARTESIAN_POINT('Ctrl Pts',(-4.29383389859475,0.624790363585127,
3.71389681896982));
#13633=CARTESIAN_POINT('Ctrl Pts',(-4.36342914970185,0.121659159989159,
3.71267106042637));
#13634=CARTESIAN_POINT('Ctrl Pts',(-4.23298435097006,0.608485776439291,
3.71267106042637));
#13635=CARTESIAN_POINT('Ctrl Pts',(-4.32167171841416,0.110470289997625,
3.74751057050733));
#13636=CARTESIAN_POINT('Ctrl Pts',(-4.19122691968237,0.597296906447757,
3.74751057050733));
#13637=CARTESIAN_POINT('Ctrl Pts',(-4.31223161698407,0.107940822442964,
3.77924744726674));
#13638=CARTESIAN_POINT('Ctrl Pts',(-4.18178681825228,0.594767438893096,
3.77924744726674));
#13639=CARTESIAN_POINT('Ctrl Pts',(-4.31223161698407,0.107940822442964,
3.79515655425571));
#13640=CARTESIAN_POINT('Ctrl Pts',(-4.18178681825228,0.594767438893096,
3.79515655425571));
#13641=CARTESIAN_POINT('',(-4.2656293489477,0.281862854502613,3.79515655425571));
#13642=CARTESIAN_POINT('Ctrl Pts',(-4.26562934894771,0.281862854502614,
3.79515655425571));
#13643=CARTESIAN_POINT('Ctrl Pts',(-4.26147271281242,0.297375631748062,
3.78450087317412));
#13644=CARTESIAN_POINT('Ctrl Pts',(-4.25740948502131,0.321025382479211,
3.77380857087543));
#13645=CARTESIAN_POINT('Ctrl Pts',(-4.25373528372325,0.35087999479231,3.76392332459328));
#13646=CARTESIAN_POINT('Ctrl Pts',(-4.25264800923526,0.359714610994202,
3.76099806949206));
#13647=CARTESIAN_POINT('Ctrl Pts',(-4.25159449798474,0.36909250201679,3.75814367226683));
#13648=CARTESIAN_POINT('Ctrl Pts',(-4.25058168579739,0.378963405580522,
3.75538231946777));
#13649=CARTESIAN_POINT('Ctrl Pts',(-4.24992566575775,0.385357000195711,
3.75359373240755));
#13650=CARTESIAN_POINT('Ctrl Pts',(-4.24929705290578,0.391856366095762,
3.75187242351791));
#13651=CARTESIAN_POINT('Ctrl Pts',(-4.2486954070829,0.398435948977368,3.75021886318504));
#13652=CARTESIAN_POINT('Ctrl Pts',(-4.24703988692003,0.416540673899359,
3.74566883995297));
#13653=CARTESIAN_POINT('Ctrl Pts',(-4.24559783322402,0.435254084284691,
3.7416155679197));
#13654=CARTESIAN_POINT('Ctrl Pts',(-4.24432835230835,0.454028466761707,
3.73805391289932));
#13655=CARTESIAN_POINT('Ctrl Pts',(-4.24300172172098,0.473648037048853,
3.73433191878866));
#13656=CARTESIAN_POINT('Ctrl Pts',(-4.24186364941875,0.493334218942247,
3.73114657008713));
#13657=CARTESIAN_POINT('Ctrl Pts',(-4.24091335650253,0.512474244136979,
3.72846116461617));
#13658=CARTESIAN_POINT('Ctrl Pts',(-4.24072970279613,0.516173247368188,
3.72794218287957));
#13659=CARTESIAN_POINT('Ctrl Pts',(-4.24055319140698,0.519851886464871,
3.72744179167473));
#13660=CARTESIAN_POINT('Ctrl Pts',(-4.2403839967245,0.523505786600193,3.72695961362351));
#13661=CARTESIAN_POINT('',(-4.31223161698407,0.107940822442964,3.79515655425571));
#13662=CARTESIAN_POINT('',(-4.2656293489477,0.281862854502613,3.79515655425571));
#13663=CARTESIAN_POINT('',(-4.4618940931088,0.148042762057828,3.76716196298096));
#13664=CARTESIAN_POINT('Origin',(-4.38950568308719,0.128646346051165,3.79515655425571));
#13665=CARTESIAN_POINT('',(-4.4618940931088,0.148042762057828,3.76716196298096));
#13666=CARTESIAN_POINT('Origin',(-4.38950568308719,0.128646346051165,9.69874330802488));
#13667=CARTESIAN_POINT('',(-4.31223161698407,0.107940822442963,3.90484829258838));
#13668=CARTESIAN_POINT('Ctrl Pts',(-4.4102112066954,0.0513722799480405,
4.08908175574846));
#13669=CARTESIAN_POINT('Ctrl Pts',(-4.40715780817639,0.0505541242807026,
4.08406395634642));
#13670=CARTESIAN_POINT('Ctrl Pts',(-4.40410949393389,0.0499312335671429,
4.07899808604622));
#13671=CARTESIAN_POINT('Ctrl Pts',(-4.40108550168694,0.0494888587161251,
4.07391511943208));
#13672=CARTESIAN_POINT('Ctrl Pts',(-4.39811787660674,0.0490547297252024,
4.06892689923374));
#13673=CARTESIAN_POINT('Ctrl Pts',(-4.39516354057751,0.048792963118744,
4.06390522474203));
#13674=CARTESIAN_POINT('Ctrl Pts',(-4.39223708843253,0.0486929882427565,
4.05887466023701));
#13675=CARTESIAN_POINT('Ctrl Pts',(-4.38915212776929,0.0485875983219737,
4.05357161995375));
#13676=CARTESIAN_POINT('Ctrl Pts',(-4.38608814252384,0.0486616553190951,
4.04824149366342));
#13677=CARTESIAN_POINT('Ctrl Pts',(-4.38305987368437,0.0489064467463467,
4.04291033102921));
#13678=CARTESIAN_POINT('Ctrl Pts',(-4.37901299723057,0.0492335777626303,
4.03578594489329));
#13679=CARTESIAN_POINT('Ctrl Pts',(-4.37500939219102,0.0498672890372918,
4.02862330711841));
#13680=CARTESIAN_POINT('Ctrl Pts',(-4.37108271550167,0.0507965273914985,
4.02148538683094));
#13681=CARTESIAN_POINT('Ctrl Pts',(-4.36407440648063,0.0524550264368009,
4.0087456694822));
#13682=CARTESIAN_POINT('Ctrl Pts',(-4.35719229690955,0.0550831201777107,
3.99586222022605));
#13683=CARTESIAN_POINT('Ctrl Pts',(-4.35066738468329,0.0587064677477982,
3.98330174291168));
#13684=CARTESIAN_POINT('Ctrl Pts',(-4.3452914594315,0.0616917716143653,
3.97295306927019));
#13685=CARTESIAN_POINT('Ctrl Pts',(-4.33994121668507,0.0654745878228202,
3.96240228466924));
#13686=CARTESIAN_POINT('Ctrl Pts',(-4.33493714468306,0.0701435073148899,
3.95230898650671));
#13687=CARTESIAN_POINT('Ctrl Pts',(-4.33267033431069,0.0722584958938203,
3.9477367915109));
#13688=CARTESIAN_POINT('Ctrl Pts',(-4.33047389394378,0.0745553153476243,
3.9432588379003));
#13689=CARTESIAN_POINT('Ctrl Pts',(-4.32837457659156,0.0770422006884091,
3.93893808366001));
#13690=CARTESIAN_POINT('Ctrl Pts',(-4.32476766398669,0.0813150077859595,
3.931514440486));
#13691=CARTESIAN_POINT('Ctrl Pts',(-4.32123459484289,0.0864133300397851,
3.9241081537622));
#13692=CARTESIAN_POINT('Ctrl Pts',(-4.31820676396266,0.0923632352188068,
3.91767246460418));
#13693=CARTESIAN_POINT('Ctrl Pts',(-4.31592387475179,0.0968492765058371,
3.91282015748251));
#13694=CARTESIAN_POINT('Ctrl Pts',(-4.31380785765501,0.102058212174025,
3.90826444070493));
#13695=CARTESIAN_POINT('Ctrl Pts',(-4.31223161698407,0.107940822442957,
3.90484829258837));
#13696=CARTESIAN_POINT('Origin',(-4.38950568308719,0.128646346051165,3.79515655425572));
#13697=CARTESIAN_POINT('',(-4.31223161698407,0.107940822442964,9.69874330802488));
#13698=CARTESIAN_POINT('Origin',(-4.38950568308719,0.128646346051165,3.79515655425571));
#13699=CARTESIAN_POINT('Origin',(-4.38950568308719,0.128646346051165,3.79515655425571));
#13700=CARTESIAN_POINT('Ctrl Pts',(-4.48256963531681,-0.527769316435443,
3.08701851589457));
#13701=CARTESIAN_POINT('Ctrl Pts',(-3.91894481913026,1.57570713397942,3.08701851589457));
#13702=CARTESIAN_POINT('Ctrl Pts',(-4.48567197442026,-0.526938047178027,
3.11273802327628));
#13703=CARTESIAN_POINT('Ctrl Pts',(-3.92204715823371,1.57653840323684,3.11273802327628));
#13704=CARTESIAN_POINT('Ctrl Pts',(-4.49425560545544,-0.524638070174025,
3.18044435652227));
#13705=CARTESIAN_POINT('Ctrl Pts',(-3.93063078926889,1.57883838024084,3.18044435652227));
#13706=CARTESIAN_POINT('Ctrl Pts',(-4.50997464014073,-0.520426167524303,
3.28931577678178));
#13707=CARTESIAN_POINT('Ctrl Pts',(-3.94634982395418,1.58305028289056,3.28931577678178));
#13708=CARTESIAN_POINT('Ctrl Pts',(-4.53649805190377,-0.51331924076188,
3.43759550531425));
#13709=CARTESIAN_POINT('Ctrl Pts',(-3.97287323571722,1.59015720965299,3.43759550531425));
#13710=CARTESIAN_POINT('Ctrl Pts',(-4.58094275590847,-0.50141031821598,
3.62185203209171));
#13711=CARTESIAN_POINT('Ctrl Pts',(-4.01731793972192,1.60206613219889,3.62185203209171));
#13712=CARTESIAN_POINT('Ctrl Pts',(-4.64450909979627,-0.484377767705444,
3.81399668859083));
#13713=CARTESIAN_POINT('Ctrl Pts',(-4.08088428360972,1.61909868270942,3.81399668859083));
#13714=CARTESIAN_POINT('Ctrl Pts',(-4.72548463526162,-0.462680438370826,
3.99681013615577));
#13715=CARTESIAN_POINT('Ctrl Pts',(-4.16185981907507,1.64079601204404,3.99681013615577));
#13716=CARTESIAN_POINT('Ctrl Pts',(-4.8252271822744,-0.435954503447729,
4.16885849319142));
#13717=CARTESIAN_POINT('Ctrl Pts',(-4.26160236608785,1.66752194696714,4.16885849319142));
#13718=CARTESIAN_POINT('Ctrl Pts',(-4.94428264222518,-0.404053689099401,
4.32911151507774));
#13719=CARTESIAN_POINT('Ctrl Pts',(-4.38065782603863,1.69942276131547,4.32911151507774));
#13720=CARTESIAN_POINT('Ctrl Pts',(-5.08228593832039,-0.367075817357858,
4.47714872481861));
#13721=CARTESIAN_POINT('Ctrl Pts',(-4.51866112213384,1.73640063305701,4.47714872481861));
#13722=CARTESIAN_POINT('Ctrl Pts',(-5.2378288268678,-0.325398225983173,
4.61340315498244));
#13723=CARTESIAN_POINT('Ctrl Pts',(-4.67420401068125,1.77807822443169,4.61340315498244));
#13724=CARTESIAN_POINT('Ctrl Pts',(-5.40841563192727,-0.279689629328082,
4.73929437247796));
#13725=CARTESIAN_POINT('Ctrl Pts',(-4.84479081574072,1.82378682108679,4.73929437247796));
#13726=CARTESIAN_POINT('Ctrl Pts',(-5.59088341835554,-0.230797533309933,
4.8567611153285));
#13727=CARTESIAN_POINT('Ctrl Pts',(-5.02725860216899,1.87267891710493,4.8567611153285));
#13728=CARTESIAN_POINT('Ctrl Pts',(-5.78175784092263,-0.179652885927325,
4.96787993373728));
#13729=CARTESIAN_POINT('Ctrl Pts',(-5.21813302473608,1.92382356448754,4.96787993373728));
#13730=CARTESIAN_POINT('Ctrl Pts',(-5.97764641105224,-0.127164701754609,
5.07442896098937));
#13731=CARTESIAN_POINT('Ctrl Pts',(-5.41402159486569,1.97631174866026,5.07442896098937));
#13732=CARTESIAN_POINT('Ctrl Pts',(-6.17558693510453,-0.0741266981854037,
5.17752467829109));
#13733=CARTESIAN_POINT('Ctrl Pts',(-5.61196211891798,2.02934975222946,5.17752467829109));
#13734=CARTESIAN_POINT('Ctrl Pts',(-6.37348970657079,-0.0210988103911397,
5.27709955371564));
#13735=CARTESIAN_POINT('Ctrl Pts',(-5.80986489038424,2.08237764002373,5.27709955371564));
#13736=CARTESIAN_POINT('Ctrl Pts',(-6.57005693376087,0.0315712193928662,
5.37226655127787));
#13737=CARTESIAN_POINT('Ctrl Pts',(-6.00643211757432,2.13504766980773,5.37226655127787));
#13738=CARTESIAN_POINT('Ctrl Pts',(-6.764532792514,0.0836808686931177,5.46195513100446));
#13739=CARTESIAN_POINT('Ctrl Pts',(-6.20090797632745,2.18715731910799,5.46195513100446));
#13740=CARTESIAN_POINT('Ctrl Pts',(-6.9565133803486,0.135121912165851,5.54547963906637));
#13741=CARTESIAN_POINT('Ctrl Pts',(-6.39288856416205,2.23859836258072,5.54547963906637));
#13742=CARTESIAN_POINT('Ctrl Pts',(-7.14572349951852,0.185820610797228,
5.62308582598972));
#13743=CARTESIAN_POINT('Ctrl Pts',(-6.58209868333197,2.2892970612121,5.62308582598972));
#13744=CARTESIAN_POINT('Ctrl Pts',(-7.33182719121273,0.235686944695142,
5.69662713609756));
#13745=CARTESIAN_POINT('Ctrl Pts',(-6.76820237502618,2.33916339511001,5.69662713609756));
#13746=CARTESIAN_POINT('Ctrl Pts',(-7.51416424179833,0.284544010149827,
5.76979878895672));
#13747=CARTESIAN_POINT('Ctrl Pts',(-6.95053942561178,2.38802046056469,5.76979878895672));
#13748=CARTESIAN_POINT('Ctrl Pts',(-7.69136124084791,0.332023802946379,
5.84723737025949));
#13749=CARTESIAN_POINT('Ctrl Pts',(-7.12773642466136,2.43550025336125,5.84723737025949));
#13750=CARTESIAN_POINT('Ctrl Pts',(-7.86091360098085,0.377455220918793,
5.93381436957244));
#13751=CARTESIAN_POINT('Ctrl Pts',(-7.2972887847943,2.48093167133366,5.93381436957244));
#13752=CARTESIAN_POINT('Ctrl Pts',(-8.01888934773147,0.419784694684325,
6.03389995867283));
#13753=CARTESIAN_POINT('Ctrl Pts',(-7.45526453154492,2.52326114509919,6.03389995867283));
#13754=CARTESIAN_POINT('Ctrl Pts',(-8.15931664883473,0.457412076610226,
6.15052660592937));
#13755=CARTESIAN_POINT('Ctrl Pts',(-7.59569183264818,2.56088852702509,6.15052660592937));
#13756=CARTESIAN_POINT('Ctrl Pts',(-8.27461002276794,0.488304843048287,
6.28498018271686));
#13757=CARTESIAN_POINT('Ctrl Pts',(-7.71098520658139,2.59178129346315,6.28498018271686));
#13758=CARTESIAN_POINT('Ctrl Pts',(-8.35793279453621,0.510631112454717,
6.43720976255636));
#13759=CARTESIAN_POINT('Ctrl Pts',(-7.79430797834966,2.61410756286958,6.43720976255636));
#13760=CARTESIAN_POINT('Ctrl Pts',(-8.40509543036698,0.523268302638496,
6.60605451948903));
#13761=CARTESIAN_POINT('Ctrl Pts',(-7.84147061418043,2.62674475305336,6.60605451948903));
#13762=CARTESIAN_POINT('Ctrl Pts',(-8.41671870598169,0.526382749952862,
6.78954489191904));
#13763=CARTESIAN_POINT('Ctrl Pts',(-7.85309388979514,2.62985920036773,6.78954489191904));
#13764=CARTESIAN_POINT('Ctrl Pts',(-8.40006576374695,0.521920607529461,
6.9851692342788));
#13765=CARTESIAN_POINT('Ctrl Pts',(-7.8364409475604,2.62539705794433,6.9851692342788));
#13766=CARTESIAN_POINT('Ctrl Pts',(-8.36615114951844,0.512833214035319,
7.19009032473164));
#13767=CARTESIAN_POINT('Ctrl Pts',(-7.80252633333189,2.61630966445019,7.19009032473164));
#13768=CARTESIAN_POINT('Ctrl Pts',(-8.32703506598497,0.502352091041457,
7.40136016279791));
#13769=CARTESIAN_POINT('Ctrl Pts',(-7.76341024979842,2.60582854145632,7.40136016279791));
#13770=CARTESIAN_POINT('Ctrl Pts',(-8.29309518354847,0.49325792695139,7.61613341658677));
#13771=CARTESIAN_POINT('Ctrl Pts',(-7.72947036736192,2.59673437736626,7.61613341658677));
#13772=CARTESIAN_POINT('Ctrl Pts',(-8.27020014354463,0.487123219471682,
7.83188673232793));
#13773=CARTESIAN_POINT('Ctrl Pts',(-7.70657532735808,2.59059966988655,7.83188673232793));
#13774=CARTESIAN_POINT('Ctrl Pts',(-8.25723287204663,0.483648649545758,
8.04662057355248));
#13775=CARTESIAN_POINT('Ctrl Pts',(-7.69360805586008,2.58712509996063,8.04662057355248));
#13776=CARTESIAN_POINT('Ctrl Pts',(-8.24851973923233,0.481313972644621,
8.25883677791483));
#13777=CARTESIAN_POINT('Ctrl Pts',(-7.68489492304578,2.58479042305949,8.25883677791483));
#13778=CARTESIAN_POINT('Ctrl Pts',(-8.23592388463589,0.477938923577525,
8.46752658699528));
#13779=CARTESIAN_POINT('Ctrl Pts',(-7.67229906844934,2.58141537399239,8.46752658699528));
#13780=CARTESIAN_POINT('Ctrl Pts',(-8.21111682748236,0.471291892646646,
8.67216210283896));
#13781=CARTESIAN_POINT('Ctrl Pts',(-7.64749201129581,2.57476834306151,8.67216210283896));
#13782=CARTESIAN_POINT('Ctrl Pts',(-8.16765643912891,0.459646716684596,
8.87266947141823));
#13783=CARTESIAN_POINT('Ctrl Pts',(-7.60403162294236,2.56312316709946,8.87266947141823));
#13784=CARTESIAN_POINT('Ctrl Pts',(-8.10345923018583,0.442445126391965,
9.06945407016992));
#13785=CARTESIAN_POINT('Ctrl Pts',(-7.53983441399928,2.54592157680683,9.06945407016992));
#13786=CARTESIAN_POINT('Ctrl Pts',(-8.01987967284149,0.420050051497798,
9.26297089919765));
#13787=CARTESIAN_POINT('Ctrl Pts',(-7.45625485665494,2.52352650191267,9.26297089919765));
#13788=CARTESIAN_POINT('Ctrl Pts',(-7.9203000245135,0.393367765145738,9.4532499945042));
#13789=CARTESIAN_POINT('Ctrl Pts',(-7.35667520832695,2.49684421556061,9.4532499945042));
#13790=CARTESIAN_POINT('Ctrl Pts',(-7.80883735056672,0.363501431675485,
9.63939026966035));
#13791=CARTESIAN_POINT('Ctrl Pts',(-7.24521253438017,2.46697788209035,9.63939026966035));
#13792=CARTESIAN_POINT('Ctrl Pts',(-7.68912508048803,0.331424625583803,
9.81917361987397));
#13793=CARTESIAN_POINT('Ctrl Pts',(-7.12550026430148,2.43490107599867,9.81917361987397));
#13794=CARTESIAN_POINT('Ctrl Pts',(-7.56275058554779,0.297562681720675,
9.98835756998572));
#13795=CARTESIAN_POINT('Ctrl Pts',(-6.99912576936124,2.40103913213554,9.98835756998572));
#13796=CARTESIAN_POINT('Ctrl Pts',(-7.42943112498675,0.26183983992799,10.1414720974148));
#13797=CARTESIAN_POINT('Ctrl Pts',(-6.8658063088002,2.36531629034286,10.1414720974148));
#13798=CARTESIAN_POINT('Ctrl Pts',(-7.28805723502187,0.223958820281056,
10.2733319413008));
#13799=CARTESIAN_POINT('Ctrl Pts',(-6.72443241883532,2.32743527069592,10.2733319413008));
#13800=CARTESIAN_POINT('Ctrl Pts',(-7.13750378696743,0.183618145457146,
10.3804015453596));
#13801=CARTESIAN_POINT('Ctrl Pts',(-6.57387897078088,2.28709459587201,10.3804015453596));
#13802=CARTESIAN_POINT('Ctrl Pts',(-6.97744813422739,0.140731362561417,
10.4620502678778));
#13803=CARTESIAN_POINT('Ctrl Pts',(-6.41382331804084,2.24420781297628,10.4620502678778));
#13804=CARTESIAN_POINT('Ctrl Pts',(-6.8094130432502,0.0957064956339898,
10.522290883026));
#13805=CARTESIAN_POINT('Ctrl Pts',(-6.24578822706365,2.19918294604886,10.522290883026));
#13806=CARTESIAN_POINT('Ctrl Pts',(-6.63636009908937,0.0493370989982661,
10.5687216653902));
#13807=CARTESIAN_POINT('Ctrl Pts',(-6.07273528290282,2.15281354941313,10.5687216653902));
#13808=CARTESIAN_POINT('Ctrl Pts',(-6.46169146064018,0.00253477838276239,
10.6103475969885));
#13809=CARTESIAN_POINT('Ctrl Pts',(-5.89806664445363,2.10601122879763,10.6103475969885));
#13810=CARTESIAN_POINT('Ctrl Pts',(-6.28848322866428,-0.0438762274976022,
10.6558377434043));
#13811=CARTESIAN_POINT('Ctrl Pts',(-5.72485841247773,2.05960022291727,10.6558377434043));
#13812=CARTESIAN_POINT('Ctrl Pts',(-6.1185359467212,-0.0894134644501156,
10.7114411549114));
#13813=CARTESIAN_POINT('Ctrl Pts',(-5.55491113053465,2.01406298596475,10.7114411549114));
#13814=CARTESIAN_POINT('Ctrl Pts',(-5.95175730544346,-0.134101666695245,
10.7795199127535));
#13815=CARTESIAN_POINT('Ctrl Pts',(-5.38813248925691,1.96937478371962,10.7795199127535));
#13816=CARTESIAN_POINT('Ctrl Pts',(-5.7870670120022,-0.178230297824076,
10.8599381259737));
#13817=CARTESIAN_POINT('Ctrl Pts',(-5.22344219581565,1.92524615259079,10.8599381259737));
#13818=CARTESIAN_POINT('Ctrl Pts',(-5.62316263442508,-0.22214834343179,
10.9511663773826));
#13819=CARTESIAN_POINT('Ctrl Pts',(-5.05953781823853,1.88132810698308,10.9511663773826));
#13820=CARTESIAN_POINT('Ctrl Pts',(-5.45924619928996,-0.266069619852436,
11.0513704191329));
#13821=CARTESIAN_POINT('Ctrl Pts',(-4.89562138310341,1.83740683056243,11.0513704191329));
#13822=CARTESIAN_POINT('Ctrl Pts',(-5.29599290169212,-0.309813209105493,
11.1598106424589));
#13823=CARTESIAN_POINT('Ctrl Pts',(-4.73236808550557,1.79366324130937,11.1598106424589));
#13824=CARTESIAN_POINT('Ctrl Pts',(-5.13550277232935,-0.352816409661416,
11.2768795166235));
#13825=CARTESIAN_POINT('Ctrl Pts',(-4.5718779561428,1.75066004075345,11.2768795166235));
#13826=CARTESIAN_POINT('Ctrl Pts',(-4.9803362658263,-0.394393149771265,
11.4029224160731));
#13827=CARTESIAN_POINT('Ctrl Pts',(-4.41671144963975,1.7090833006436,11.4029224160731));
#13828=CARTESIAN_POINT('Ctrl Pts',(-4.83277159412549,-0.433932984384862,
11.5373242211527));
#13829=CARTESIAN_POINT('Ctrl Pts',(-4.26914677793894,1.66954346603001,11.5373242211527));
#13830=CARTESIAN_POINT('Ctrl Pts',(-4.69404542712503,-0.471104548801699,
11.6776492463597));
#13831=CARTESIAN_POINT('Ctrl Pts',(-4.13042061093848,1.63237190161317,11.6776492463597));
#13832=CARTESIAN_POINT('Ctrl Pts',(-4.5634172640769,-0.506106259599206,
11.8183570873721));
#13833=CARTESIAN_POINT('Ctrl Pts',(-3.99979244789035,1.59737019081566,11.8183570873721));
#13834=CARTESIAN_POINT('Ctrl Pts',(-4.438093400719,-0.539686687578305,11.9514202619522));
#13835=CARTESIAN_POINT('Ctrl Pts',(-3.87446858453245,1.56378976283656,11.9514202619522));
#13836=CARTESIAN_POINT('Ctrl Pts',(-4.31385169054842,-0.572977153484772,
12.0684942936867));
#13837=CARTESIAN_POINT('Ctrl Pts',(-3.75022687436187,1.5304992969301,12.0684942936867));
#13838=CARTESIAN_POINT('Ctrl Pts',(-4.18546338657022,-0.607378695853334,
12.1626050652586));
#13839=CARTESIAN_POINT('Ctrl Pts',(-3.62183857038367,1.49609775456153,12.1626050652586));
#13840=CARTESIAN_POINT('Ctrl Pts',(-4.04719835432938,-0.64442669958373,
12.2301117722809));
#13841=CARTESIAN_POINT('Ctrl Pts',(-3.48357353814283,1.45904975083114,12.2301117722809));
#13842=CARTESIAN_POINT('Ctrl Pts',(-3.89329384649782,-0.685665288168704,
12.2723364229645));
#13843=CARTESIAN_POINT('Ctrl Pts',(-3.32966903031127,1.41781116224616,12.2723364229645));
#13844=CARTESIAN_POINT('Ctrl Pts',(-3.71837239798516,-0.732535349036556,
12.2938762651139));
#13845=CARTESIAN_POINT('Ctrl Pts',(-3.15474758179861,1.37094110137831,12.2938762651139));
#13846=CARTESIAN_POINT('Ctrl Pts',(-3.51787595240156,-0.786258209715991,
12.3010487961981));
#13847=CARTESIAN_POINT('Ctrl Pts',(-2.95425113621501,1.31721824069888,12.3010487961981));
#13848=CARTESIAN_POINT('Ctrl Pts',(-3.28845641826505,-0.847730988615793,
12.300400839059));
#13849=CARTESIAN_POINT('Ctrl Pts',(-2.7248316020785,1.25574546179907,12.300400839059));
#13850=CARTESIAN_POINT('Ctrl Pts',(-3.02847742875917,-0.917392148902953,
12.2969132923574));
#13851=CARTESIAN_POINT('Ctrl Pts',(-2.46485261257262,1.18608430151191,12.2969132923574));
#13852=CARTESIAN_POINT('Ctrl Pts',(-2.7380515440356,-0.995211530175729,
12.2935845551224));
#13853=CARTESIAN_POINT('Ctrl Pts',(-2.17442672784905,1.10826492023914,12.2935845551224));
#13854=CARTESIAN_POINT('Ctrl Pts',(-2.41876039944478,-1.08076533451925,
12.2919684497906));
#13855=CARTESIAN_POINT('Ctrl Pts',(-1.85513558325823,1.02271111589562,12.2919684497906));
#13856=CARTESIAN_POINT('Ctrl Pts',(-2.07346909055444,-1.1732858618899,12.2924280531798));
#13857=CARTESIAN_POINT('Ctrl Pts',(-1.50984427436789,0.930190588524968,
12.2924280531798));
#13858=CARTESIAN_POINT('Ctrl Pts',(-1.70610182774042,-1.27172162328655,
12.2945066442122));
#13859=CARTESIAN_POINT('Ctrl Pts',(-1.14247701155387,0.831754827128318,
12.2945066442122));
#13860=CARTESIAN_POINT('Ctrl Pts',(-1.32143431837074,-1.37479297177665,
12.2972483292773));
#13861=CARTESIAN_POINT('Ctrl Pts',(-0.757809502184194,0.728683478638218,
12.2972483292773));
#13862=CARTESIAN_POINT('Ctrl Pts',(-1.00419011146164,-1.45979830082139,
12.299081889758));
#13863=CARTESIAN_POINT('Ctrl Pts',(-0.440565295275094,0.643678149593478,
12.299081889758));
#13864=CARTESIAN_POINT('Ctrl Pts',(-0.763534432174986,-1.52428179574021,
12.2998330708668));
#13865=CARTESIAN_POINT('Ctrl Pts',(-0.19990961598844,0.579194654674658,
12.2998330708668));
#13866=CARTESIAN_POINT('Ctrl Pts',(-0.602693975746076,-1.56737886615059,
12.2999999999989));
#13867=CARTESIAN_POINT('Ctrl Pts',(-0.0390691595595298,0.536097584264278,
12.2999999999989));
#13868=CARTESIAN_POINT('Ctrl Pts',(-0.522273747531633,-1.58892740135578,
12.3));
#13869=CARTESIAN_POINT('Ctrl Pts',(0.0413510686549131,0.514549049059088,
12.3));
#13870=CARTESIAN_POINT('Ctrl Pts',(-0.441853519317205,-1.61047593656096,
12.3000000000011));
#13871=CARTESIAN_POINT('Ctrl Pts',(0.121771296869341,0.493000513853908,
12.3000000000011));
#13872=CARTESIAN_POINT('Ctrl Pts',(-0.281013062888359,-1.65357300697132,
12.2998330708736));
#13873=CARTESIAN_POINT('Ctrl Pts',(0.282611753298187,0.449903443443548,
12.2998330708736));
#13874=CARTESIAN_POINT('Ctrl Pts',(-0.0403573836016633,-1.71805650189016,
12.2990818897713));
#13875=CARTESIAN_POINT('Ctrl Pts',(0.523267432584883,0.385419948524708,
12.2990818897713));
#13876=CARTESIAN_POINT('Ctrl Pts',(0.276886823307267,-1.80306183093486,
12.2972483292974));
#13877=CARTESIAN_POINT('Ctrl Pts',(0.840511639493813,0.300414619480008,
12.2972483292974));
#13878=CARTESIAN_POINT('Ctrl Pts',(0.661554332676866,-1.90613317942493,
12.2945066442369));
#13879=CARTESIAN_POINT('Ctrl Pts',(1.22517914886341,0.197343270989938,12.2945066442369));
#13880=CARTESIAN_POINT('Ctrl Pts',(1.0289215954908,-2.00456894082156,12.2924280532047));
#13881=CARTESIAN_POINT('Ctrl Pts',(1.59254641167735,0.0989075095933076,
12.2924280532047));
#13882=CARTESIAN_POINT('Ctrl Pts',(1.37421290438113,-2.09708946819221,12.291968449812));
#13883=CARTESIAN_POINT('Ctrl Pts',(1.93783772056768,0.00638698222265788,
12.291968449812));
#13884=CARTESIAN_POINT('Ctrl Pts',(1.693504048972,-2.18264327253574,12.2935845551378));
#13885=CARTESIAN_POINT('Ctrl Pts',(2.25712886515855,-0.0791668221208721,
12.2935845551378));
#13886=CARTESIAN_POINT('Ctrl Pts',(1.98392993369567,-2.26046265380854,12.2969132923658));
#13887=CARTESIAN_POINT('Ctrl Pts',(2.54755474988222,-0.156986203393672,
12.2969132923658));
#13888=CARTESIAN_POINT('Ctrl Pts',(2.24390892320168,-2.33012381409574,12.3004008390612));
#13889=CARTESIAN_POINT('Ctrl Pts',(2.80753373938823,-0.226647363680872,
12.3004008390612));
#13890=CARTESIAN_POINT('Ctrl Pts',(2.47332845733829,-2.39159659299556,12.3010487961961));
#13891=CARTESIAN_POINT('Ctrl Pts',(3.03695327352484,-0.288120142580692,
12.3010487961961));
#13892=CARTESIAN_POINT('Ctrl Pts',(2.67382490292192,-2.44531945367501,12.2938762651102));
#13893=CARTESIAN_POINT('Ctrl Pts',(3.23744971910847,-0.341843003260142,
12.2938762651102));
#13894=CARTESIAN_POINT('Ctrl Pts',(2.84874635143459,-2.49218951454286,12.2723364229612));
#13895=CARTESIAN_POINT('Ctrl Pts',(3.41237116762114,-0.388713064127992,
12.2723364229612));
#13896=CARTESIAN_POINT('Ctrl Pts',(3.0026508592661,-2.53342810312782,12.2301117722792));
#13897=CARTESIAN_POINT('Ctrl Pts',(3.56627567545265,-0.429951652712952,
12.2301117722792));
#13898=CARTESIAN_POINT('Ctrl Pts',(3.14091589150692,-2.57047610685821,12.1626050652587));
#13899=CARTESIAN_POINT('Ctrl Pts',(3.70454070769347,-0.466999656443342,
12.1626050652587));
#13900=CARTESIAN_POINT('Ctrl Pts',(3.26930419548512,-2.60487764922678,12.0684942936878));
#13901=CARTESIAN_POINT('Ctrl Pts',(3.83292901167167,-0.501401198811912,
12.0684942936878));
#13902=CARTESIAN_POINT('Ctrl Pts',(3.39354590565573,-2.63816811513325,11.9514202619535));
#13903=CARTESIAN_POINT('Ctrl Pts',(3.95717072184228,-0.534691664718382,
11.9514202619535));
#13904=CARTESIAN_POINT('Ctrl Pts',(3.51886976901364,-2.67174854311235,11.8183570873731));
#13905=CARTESIAN_POINT('Ctrl Pts',(4.08249458520019,-0.568272092697482,
11.8183570873731));
#13906=CARTESIAN_POINT('Ctrl Pts',(3.64949793206175,-2.70675025390985,11.67764924636));
#13907=CARTESIAN_POINT('Ctrl Pts',(4.2131227482483,-0.603273803494982,11.67764924636));
#13908=CARTESIAN_POINT('Ctrl Pts',(3.78822409906218,-2.74392181832668,11.5373242211525));
#13909=CARTESIAN_POINT('Ctrl Pts',(4.35184891524873,-0.640445367911812,
11.5373242211525));
#13910=CARTESIAN_POINT('Ctrl Pts',(3.93578877076297,-2.78346165294027,11.4029224160728));
#13911=CARTESIAN_POINT('Ctrl Pts',(4.49941358694952,-0.679985202525402,
11.4029224160728));
#13912=CARTESIAN_POINT('Ctrl Pts',(4.09095527726601,-2.82503839305012,11.2768795166233));
#13913=CARTESIAN_POINT('Ctrl Pts',(4.65458009345256,-0.721561942635252,
11.2768795166233));
#13914=CARTESIAN_POINT('Ctrl Pts',(4.25144540662881,-2.86804159360605,11.1598106424589));
#13915=CARTESIAN_POINT('Ctrl Pts',(4.81507022281536,-0.764565143191182,
11.1598106424589));
#13916=CARTESIAN_POINT('Ctrl Pts',(4.41469870422666,-2.91178518285911,11.051370419133));
#13917=CARTESIAN_POINT('Ctrl Pts',(4.97832352041321,-0.808308732444242,
11.051370419133));
#13918=CARTESIAN_POINT('Ctrl Pts',(4.57861513936178,-2.95570645927976,10.9511663773825));
#13919=CARTESIAN_POINT('Ctrl Pts',(5.14223995554833,-0.852230008864892,
10.9511663773825));
#13920=CARTESIAN_POINT('Ctrl Pts',(4.74251951693888,-2.99962450488747,10.8599381259735));
#13921=CARTESIAN_POINT('Ctrl Pts',(5.30614433312543,-0.896148054472602,
10.8599381259735));
#13922=CARTESIAN_POINT('Ctrl Pts',(4.90720981038013,-3.04375313601629,10.7795199127532));
#13923=CARTESIAN_POINT('Ctrl Pts',(5.47083462656668,-0.940276685601422,
10.7795199127532));
#13924=CARTESIAN_POINT('Ctrl Pts',(5.07398845165783,-3.08844133826141,10.7114411549111));
#13925=CARTESIAN_POINT('Ctrl Pts',(5.63761326784438,-0.984964887846542,
10.7114411549111));
#13926=CARTESIAN_POINT('Ctrl Pts',(5.24393573360096,-3.13397857521394,10.6558377434042));
#13927=CARTESIAN_POINT('Ctrl Pts',(5.80756054978751,-1.03050212479907,10.6558377434042));
#13928=CARTESIAN_POINT('Ctrl Pts',(5.41714396557695,-3.18038958109433,10.6103475969888));
#13929=CARTESIAN_POINT('Ctrl Pts',(5.9807687817635,-1.07691313067946,10.6103475969888));
#13930=CARTESIAN_POINT('Ctrl Pts',(5.59181260402617,-3.22719190170984,10.5687216653907));
#13931=CARTESIAN_POINT('Ctrl Pts',(6.15543742021272,-1.12371545129497,10.5687216653907));
#13932=CARTESIAN_POINT('Ctrl Pts',(5.76486554818703,-3.27356129834557,10.5222908830264));
#13933=CARTESIAN_POINT('Ctrl Pts',(6.32849036437358,-1.1700848479307,10.5222908830264));
#13934=CARTESIAN_POINT('Ctrl Pts',(5.93290063916415,-3.31858616527298,10.462050267878));
#13935=CARTESIAN_POINT('Ctrl Pts',(6.4965254553507,-1.21510971485811,10.462050267878));
#13936=CARTESIAN_POINT('Ctrl Pts',(6.0929562919041,-3.36147294816869,10.3804015453596));
#13937=CARTESIAN_POINT('Ctrl Pts',(6.65658110809065,-1.25799649775382,10.3804015453596));
#13938=CARTESIAN_POINT('Ctrl Pts',(6.24350973995848,-3.40181362299258,10.2733319413005));
#13939=CARTESIAN_POINT('Ctrl Pts',(6.80713455614503,-1.29833717257771,10.2733319413005));
#13940=CARTESIAN_POINT('Ctrl Pts',(6.38488362992331,-3.4396946426395,10.1414720974144));
#13941=CARTESIAN_POINT('Ctrl Pts',(6.94850844610986,-1.33621819222463,10.1414720974144));
#13942=CARTESIAN_POINT('Ctrl Pts',(6.51820309048434,-3.47541748443218,9.98835756998534));
#13943=CARTESIAN_POINT('Ctrl Pts',(7.08182790667089,-1.37194103401731,9.98835756998534));
#13944=CARTESIAN_POINT('Ctrl Pts',(6.64457758542464,-3.50927942829533,9.81917361987377));
#13945=CARTESIAN_POINT('Ctrl Pts',(7.20820240161119,-1.40580297788046,9.81917361987377));
#13946=CARTESIAN_POINT('Ctrl Pts',(6.76428985550348,-3.54135623438705,9.63939026966049));
#13947=CARTESIAN_POINT('Ctrl Pts',(7.32791467169003,-1.43787978397218,9.63939026966049));
#13948=CARTESIAN_POINT('Ctrl Pts',(6.87575252945042,-3.57122256785734,9.45324999450471));
#13949=CARTESIAN_POINT('Ctrl Pts',(7.43937734563697,-1.46774611744247,9.45324999450471));
#13950=CARTESIAN_POINT('Ctrl Pts',(6.97533217777844,-3.59790485420941,9.26297089919836));
#13951=CARTESIAN_POINT('Ctrl Pts',(7.53895699396499,-1.49442840379454,9.26297089919836));
#13952=CARTESIAN_POINT('Ctrl Pts',(7.05891173512278,-3.62029992910358,9.06945407017055));
#13953=CARTESIAN_POINT('Ctrl Pts',(7.62253655130933,-1.51682347868871,9.06945407017055));
#13954=CARTESIAN_POINT('Ctrl Pts',(7.12310894406576,-3.63750151939618,8.87266947141857));
#13955=CARTESIAN_POINT('Ctrl Pts',(7.68673376025231,-1.53402506898131,8.87266947141857));
#13956=CARTESIAN_POINT('Ctrl Pts',(7.16656933241908,-3.6491466953582,8.67216210283894));
#13957=CARTESIAN_POINT('Ctrl Pts',(7.73019414860563,-1.54567024494333,8.67216210283894));
#13958=CARTESIAN_POINT('Ctrl Pts',(7.19137638957244,-3.65579372628903,8.46752658699496));
#13959=CARTESIAN_POINT('Ctrl Pts',(7.75500120575899,-1.55231727587416,8.46752658699496));
#13960=CARTESIAN_POINT('Ctrl Pts',(7.20397224416876,-3.6591687753561,8.25883677791438));
#13961=CARTESIAN_POINT('Ctrl Pts',(7.76759706035531,-1.55569232494123,8.25883677791438));
#13962=CARTESIAN_POINT('Ctrl Pts',(7.21268537698305,-3.66150345225723,8.04662057355209));
#13963=CARTESIAN_POINT('Ctrl Pts',(7.7763101931696,-1.55802700184236,8.04662057355209));
#13964=CARTESIAN_POINT('Ctrl Pts',(7.22565264848115,-3.66497802218318,7.8318867323277));
#13965=CARTESIAN_POINT('Ctrl Pts',(7.7892774646677,-1.56150157176831,7.8318867323277));
#13966=CARTESIAN_POINT('Ctrl Pts',(7.24854768848517,-3.67111272966294,7.61613341658679));
#13967=CARTESIAN_POINT('Ctrl Pts',(7.81217250467172,-1.56763627924807,7.61613341658679));
#13968=CARTESIAN_POINT('Ctrl Pts',(7.2824875709219,-3.68020689375307,7.40136016279815));
#13969=CARTESIAN_POINT('Ctrl Pts',(7.84611238710845,-1.5767304433382,7.40136016279815));
#13970=CARTESIAN_POINT('Ctrl Pts',(7.32160365445555,-3.69068801674698,7.19009032473197));
#13971=CARTESIAN_POINT('Ctrl Pts',(7.8852284706421,-1.58721156633211,7.19009032473197));
#13972=CARTESIAN_POINT('Ctrl Pts',(7.35551826868406,-3.69977541024112,6.98516923427904));
#13973=CARTESIAN_POINT('Ctrl Pts',(7.91914308487061,-1.59629895982625,6.98516923427904));
#13974=CARTESIAN_POINT('Ctrl Pts',(7.37217121091865,-3.70423755266448,6.78954489191915));
#13975=CARTESIAN_POINT('Ctrl Pts',(7.9357960271052,-1.60076110224961,6.78954489191915));
#13976=CARTESIAN_POINT('Ctrl Pts',(7.36054793530371,-3.70112310535005,6.60605451948904));
#13977=CARTESIAN_POINT('Ctrl Pts',(7.92417275149026,-1.59764665493518,6.60605451948904));
#13978=CARTESIAN_POINT('Ctrl Pts',(7.31338529947278,-3.68848591516623,6.43720976255638));
#13979=CARTESIAN_POINT('Ctrl Pts',(7.87701011565933,-1.58500946475136,6.43720976255638));
#13980=CARTESIAN_POINT('Ctrl Pts',(7.23006252770443,-3.66615964575978,6.28498018271691));
#13981=CARTESIAN_POINT('Ctrl Pts',(7.79368734389098,-1.56268319534491,6.28498018271691));
#13982=CARTESIAN_POINT('Ctrl Pts',(7.11476915377127,-3.63526687932173,6.15052660592943));
#13983=CARTESIAN_POINT('Ctrl Pts',(7.67839396995782,-1.53179042890686,6.15052660592943));
#13984=CARTESIAN_POINT('Ctrl Pts',(6.97434185266817,-3.59763949739587,6.03389995867286));
#13985=CARTESIAN_POINT('Ctrl Pts',(7.53796666885472,-1.494163046981,6.03389995867286));
#13986=CARTESIAN_POINT('Ctrl Pts',(6.81636610591773,-3.55531002363039,5.93381436957244));
#13987=CARTESIAN_POINT('Ctrl Pts',(7.37999092210428,-1.45183357321552,5.93381436957244));
#13988=CARTESIAN_POINT('Ctrl Pts',(6.64681374578489,-3.509878605658,5.84723737025948));
#13989=CARTESIAN_POINT('Ctrl Pts',(7.21043856197144,-1.40640215524313,5.84723737025948));
#13990=CARTESIAN_POINT('Ctrl Pts',(6.46961674673529,-3.46239881286144,5.76979878895671));
#13991=CARTESIAN_POINT('Ctrl Pts',(7.03324156292184,-1.35892236244657,5.76979878895671));
#13992=CARTESIAN_POINT('Ctrl Pts',(6.28727969614961,-3.41354174740674,5.69662713609756));
#13993=CARTESIAN_POINT('Ctrl Pts',(6.85090451233616,-1.31006529699187,5.69662713609756));
#13994=CARTESIAN_POINT('Ctrl Pts',(6.10117600445527,-3.36367541350879,5.62308582598972));
#13995=CARTESIAN_POINT('Ctrl Pts',(6.66480082064182,-1.26019896309392,5.62308582598972));
#13996=CARTESIAN_POINT('Ctrl Pts',(5.91196588528534,-3.31297671487741,5.54547963906641));
#13997=CARTESIAN_POINT('Ctrl Pts',(6.47559070147189,-1.20950026446254,5.54547963906641));
#13998=CARTESIAN_POINT('Ctrl Pts',(5.71998529745084,-3.2615356714047,5.46195513100458));
#13999=CARTESIAN_POINT('Ctrl Pts',(6.28361011363739,-1.15805922098983,5.46195513100458));
#14000=CARTESIAN_POINT('Ctrl Pts',(5.52550943869778,-3.20942602210447,5.37226655127806));
#14001=CARTESIAN_POINT('Ctrl Pts',(6.08913425488433,-1.1059495716896,5.37226655127806));
#14002=CARTESIAN_POINT('Ctrl Pts',(5.3289422115077,-3.15675599232046,5.27709955371581));
#14003=CARTESIAN_POINT('Ctrl Pts',(5.89256702769425,-1.05327954190559,5.27709955371581));
#14004=CARTESIAN_POINT('Ctrl Pts',(5.13103944004137,-3.10372810452618,5.17752467829117));
#14005=CARTESIAN_POINT('Ctrl Pts',(5.69466425622792,-1.00025165411131,5.17752467829117));
#14006=CARTESIAN_POINT('Ctrl Pts',(4.93309891598898,-3.05069010095695,5.07442896098936));
#14007=CARTESIAN_POINT('Ctrl Pts',(5.49672373217553,-0.947213650542082,
5.07442896098936));
#14008=CARTESIAN_POINT('Ctrl Pts',(4.7372103458593,-2.99820191678422,4.96787993373722));
#14009=CARTESIAN_POINT('Ctrl Pts',(5.30083516204585,-0.894725466369352,
4.96787993373722));
#14010=CARTESIAN_POINT('Ctrl Pts',(4.54633592329218,-2.9470572694016,4.85676111532844));
#14011=CARTESIAN_POINT('Ctrl Pts',(5.10996073947873,-0.843580818986732,
4.85676111532844));
#14012=CARTESIAN_POINT('Ctrl Pts',(4.36386813686391,-2.89816517338345,4.73929437247794));
#14013=CARTESIAN_POINT('Ctrl Pts',(4.92749295305046,-0.794688722968582,
4.73929437247794));
#14014=CARTESIAN_POINT('Ctrl Pts',(4.19328133180448,-2.85245657672837,4.61340315498245));
#14015=CARTESIAN_POINT('Ctrl Pts',(4.75690614799103,-0.748980126313502,
4.61340315498245));
#14016=CARTESIAN_POINT('Ctrl Pts',(4.03773844325712,-2.8107789853537,4.47714872481864));
#14017=CARTESIAN_POINT('Ctrl Pts',(4.60136325944367,-0.707302534938832,
4.47714872481864));
#14018=CARTESIAN_POINT('Ctrl Pts',(3.899735147162,-2.77380111361218,4.32911151507775));
#14019=CARTESIAN_POINT('Ctrl Pts',(4.46335996334855,-0.670324663197312,
4.32911151507775));
#14020=CARTESIAN_POINT('Ctrl Pts',(3.78067968721129,-2.74190029926387,4.16885849319143));
#14021=CARTESIAN_POINT('Ctrl Pts',(4.34430450339784,-0.638423848849002,
4.16885849319143));
#14022=CARTESIAN_POINT('Ctrl Pts',(3.68093714019854,-2.71517436434078,3.99681013615577));
#14023=CARTESIAN_POINT('Ctrl Pts',(4.24456195638509,-0.611697913925912,
3.99681013615577));
#14024=CARTESIAN_POINT('Ctrl Pts',(3.59996160473314,-2.69347703500615,3.81399668859083));
#14025=CARTESIAN_POINT('Ctrl Pts',(4.16358642091969,-0.590000584591282,
3.81399668859083));
#14026=CARTESIAN_POINT('Ctrl Pts',(3.53639526084523,-2.67644448449558,3.62185203209172));
#14027=CARTESIAN_POINT('Ctrl Pts',(4.10002007703178,-0.572968034080712,
3.62185203209172));
#14028=CARTESIAN_POINT('Ctrl Pts',(3.48818717006887,-2.66352716550341,3.42199345348454));
#14029=CARTESIAN_POINT('Ctrl Pts',(4.05181198625542,-0.560050715088542,
3.42199345348454));
#14030=CARTESIAN_POINT('Ctrl Pts',(3.45268796832176,-2.65401518306332,3.21600287470933));
#14031=CARTESIAN_POINT('Ctrl Pts',(4.01631278450831,-0.550538732648452,
3.21600287470933));
#14032=CARTESIAN_POINT('Ctrl Pts',(3.42695681706767,-2.64712054186447,3.00529120729351));
#14033=CARTESIAN_POINT('Ctrl Pts',(3.99058163325422,-0.543644091449602,
3.00529120729351));
#14034=CARTESIAN_POINT('Ctrl Pts',(3.40807807946881,-2.64206199937073,2.7909834104826));
#14035=CARTESIAN_POINT('Ctrl Pts',(3.97170289565536,-0.538585548955862,
2.7909834104826));
#14036=CARTESIAN_POINT('Ctrl Pts',(3.39349547439656,-2.63815460211808,2.57377631141663));
#14037=CARTESIAN_POINT('Ctrl Pts',(3.95712029058311,-0.534678151703212,
2.57377631141663));
#14038=CARTESIAN_POINT('Ctrl Pts',(3.3812915164225,-2.63488456143447,2.35385258470204));
#14039=CARTESIAN_POINT('Ctrl Pts',(3.94491633260905,-0.531408111019602,
2.35385258470204));
#14040=CARTESIAN_POINT('Ctrl Pts',(3.37061031638295,-2.63202254250968,2.13065748555701));
#14041=CARTESIAN_POINT('Ctrl Pts',(3.9342351325695,-0.528546092094812,2.13065748555701));
#14042=CARTESIAN_POINT('Ctrl Pts',(3.36139243871498,-2.62955261963262,1.9033255681334));
#14043=CARTESIAN_POINT('Ctrl Pts',(3.92501725490153,-0.526076169217752,
1.9033255681334));
#14044=CARTESIAN_POINT('Ctrl Pts',(3.35377640719761,-2.62751191013801,1.67142113207676));
#14045=CARTESIAN_POINT('Ctrl Pts',(3.91740122338416,-0.524035459723142,
1.67142113207676));
#14046=CARTESIAN_POINT('Ctrl Pts',(3.34760493989187,-2.62585827045732,1.4355810193293));
#14047=CARTESIAN_POINT('Ctrl Pts',(3.91122975607842,-0.522381820042452,
1.4355810193293));
#14048=CARTESIAN_POINT('Ctrl Pts',(3.34188856653398,-2.62432657283244,1.19819542279832));
#14049=CARTESIAN_POINT('Ctrl Pts',(3.90551338272053,-0.520850122417572,
1.19819542279832));
#14050=CARTESIAN_POINT('Ctrl Pts',(3.33428532937914,-2.62228929157694,0.964078729991153));
#14051=CARTESIAN_POINT('Ctrl Pts',(3.89791014556569,-0.518812841162072,
0.964078729991153));
#14052=CARTESIAN_POINT('Ctrl Pts',(3.32057911187183,-2.61861672166457,0.741129277895168));
#14053=CARTESIAN_POINT('Ctrl Pts',(3.88420392805838,-0.515140271249702,
0.741129277895168));
#14054=CARTESIAN_POINT('Ctrl Pts',(3.29563694769388,-2.6119334889156,0.538436816836329));
#14055=CARTESIAN_POINT('Ctrl Pts',(3.85926176388043,-0.508457038500732,
0.538436816836329));
#14056=CARTESIAN_POINT('Ctrl Pts',(3.25436653279393,-2.60087511457186,0.364350357241537));
#14057=CARTESIAN_POINT('Ctrl Pts',(3.81799134898048,-0.497398664156992,
0.364350357241537));
#14058=CARTESIAN_POINT('Ctrl Pts',(3.19265967747922,-2.58434081252282,0.224659532804428));
#14059=CARTESIAN_POINT('Ctrl Pts',(3.75628449366577,-0.480864362107952,
0.224659532804428));
#14060=CARTESIAN_POINT('Ctrl Pts',(3.10837404726043,-2.56175654597215,0.120497232333236));
#14061=CARTESIAN_POINT('Ctrl Pts',(3.67199886344698,-0.458280095557282,
0.120497232333236));
#14062=CARTESIAN_POINT('Ctrl Pts',(3.00221227044612,-2.5333105836077,0.0470540298718229));
#14063=CARTESIAN_POINT('Ctrl Pts',(3.56583708663267,-0.429834133192832,
0.0470540298718229));
#14064=CARTESIAN_POINT('Ctrl Pts',(2.87822299923539,-2.50008775851666,-0.00118366394786523));
#14065=CARTESIAN_POINT('Ctrl Pts',(3.44184781542194,-0.396611308101792,
-0.00118366394786523));
#14066=CARTESIAN_POINT('Ctrl Pts',(2.74414641495931,-2.46416204603596,-0.0263068037111615));
#14067=CARTESIAN_POINT('Ctrl Pts',(3.30777123114586,-0.360685595621092,
-0.0263068037111615));
#14068=CARTESIAN_POINT('Ctrl Pts',(2.61226182052933,-2.42882367546434,-0.0214179570895094));
#14069=CARTESIAN_POINT('Ctrl Pts',(3.17588663671588,-0.325347225049472,
-0.0214179570895094));
#14070=CARTESIAN_POINT('Ctrl Pts',(2.49578790483729,-2.39761458381537,0.0241851999814078));
#14071=CARTESIAN_POINT('Ctrl Pts',(3.05941272102384,-0.294138133400502,
0.0241851999814078));
#14072=CARTESIAN_POINT('Ctrl Pts',(2.40509129270346,-2.37331249983787,0.119017371327004));
#14073=CARTESIAN_POINT('Ctrl Pts',(2.96871610889001,-0.269836049423002,
0.119017371327004));
#14074=CARTESIAN_POINT('Ctrl Pts',(2.34304142033346,-2.35668628664588,0.262319630540593));
#14075=CARTESIAN_POINT('Ctrl Pts',(2.90666623652001,-0.253209836231012,
0.262319630540593));
#14076=CARTESIAN_POINT('Ctrl Pts',(2.3057679034264,-2.34669887789156,0.444963858672424));
#14077=CARTESIAN_POINT('Ctrl Pts',(2.86939271961295,-0.243222427476692,
0.444963858672424));
#14078=CARTESIAN_POINT('Ctrl Pts',(2.28584564406426,-2.34136072458407,0.65402023086958));
#14079=CARTESIAN_POINT('Ctrl Pts',(2.84947046025081,-0.237884274169202,
0.65402023086958));
#14080=CARTESIAN_POINT('Ctrl Pts',(2.27453624485986,-2.33833038020037,0.875890304828918));
#14081=CARTESIAN_POINT('Ctrl Pts',(2.83816106104641,-0.234853929785502,
0.875890304828918));
#14082=CARTESIAN_POINT('Ctrl Pts',(2.26478646139362,-2.33571793359422,1.10060381648398));
#14083=CARTESIAN_POINT('Ctrl Pts',(2.82841127758017,-0.232241483179352,
1.10060381648398));
#14084=CARTESIAN_POINT('Ctrl Pts',(2.25268204108937,-2.33247456394885,1.32371934078733));
#14085=CARTESIAN_POINT('Ctrl Pts',(2.81630685727592,-0.228998113533982,
1.32371934078733));
#14086=CARTESIAN_POINT('Ctrl Pts',(2.23620043629654,-2.32805833125464,1.54401727992264));
#14087=CARTESIAN_POINT('Ctrl Pts',(2.79982525248309,-0.224581880839772,
1.54401727992264));
#14088=CARTESIAN_POINT('Ctrl Pts',(2.21453882104101,-2.32225411894016,1.76209503442146));
#14089=CARTESIAN_POINT('Ctrl Pts',(2.77816363722756,-0.218777668525292,
1.76209503442146));
#14090=CARTESIAN_POINT('Ctrl Pts',(2.187197906392,-2.31492814293964,1.97856787413951));
#14091=CARTESIAN_POINT('Ctrl Pts',(2.75082272257855,-0.211451692524772,
1.97856787413951));
#14092=CARTESIAN_POINT('Ctrl Pts',(2.15320467528109,-2.30581968411534,2.19251877196071));
#14093=CARTESIAN_POINT('Ctrl Pts',(2.71682949146764,-0.202343233700472,
2.19251877196071));
#14094=CARTESIAN_POINT('Ctrl Pts',(2.11018279685234,-2.29429200653349,2.39962532458029));
#14095=CARTESIAN_POINT('Ctrl Pts',(2.67380761303889,-0.190815556118622,
2.39962532458029));
#14096=CARTESIAN_POINT('Ctrl Pts',(2.05479350671064,-2.27945049097069,2.59347738935741));
#14097=CARTESIAN_POINT('Ctrl Pts',(2.61841832289719,-0.175974040555822,
2.59347738935741));
#14098=CARTESIAN_POINT('Ctrl Pts',(1.98331409228925,-2.26029763960102,2.7672283971178));
#14099=CARTESIAN_POINT('Ctrl Pts',(2.5469389084758,-0.156821189186152,2.7672283971178));
#14100=CARTESIAN_POINT('Ctrl Pts',(1.89216285547678,-2.23587373930803,2.91510580081997));
#14101=CARTESIAN_POINT('Ctrl Pts',(2.45578767166333,-0.132397288893162,
2.91510580081997));
#14102=CARTESIAN_POINT('Ctrl Pts',(1.77845779245372,-2.20540655949567,3.03403241435618));
#14103=CARTESIAN_POINT('Ctrl Pts',(2.34208260864027,-0.101930109080802,
3.03403241435618));
#14104=CARTESIAN_POINT('Ctrl Pts',(1.64052927563717,-2.16844872480145,3.12505646843308));
#14105=CARTESIAN_POINT('Ctrl Pts',(2.20415409182372,-0.0649722743865824,
3.12505646843308));
#14106=CARTESIAN_POINT('Ctrl Pts',(1.477782460992,-2.12484084724654,3.19196918412265));
#14107=CARTESIAN_POINT('Ctrl Pts',(2.04140727717855,-0.0213643968316721,
3.19196918412265));
#14108=CARTESIAN_POINT('Ctrl Pts',(1.29059023976394,-2.07468284273909,3.24001322621211));
#14109=CARTESIAN_POINT('Ctrl Pts',(1.85421505595049,0.0287936076757775,
3.24001322621211));
#14110=CARTESIAN_POINT('Ctrl Pts',(1.08017544120182,-2.01830236738882,3.27464765209773));
#14111=CARTESIAN_POINT('Ctrl Pts',(1.64380025738837,0.0851740830260477,
3.27464765209773));
#14112=CARTESIAN_POINT('Ctrl Pts',(0.84849626609417,-1.95622411951561,3.30006519349576));
#14113=CARTESIAN_POINT('Ctrl Pts',(1.41212108228072,0.147252330899258,3.30006519349576));
#14114=CARTESIAN_POINT('Ctrl Pts',(0.598137797989503,-1.88914077016867,
3.31897283641381));
#14115=CARTESIAN_POINT('Ctrl Pts',(1.16176261417605,0.214335680246198,3.31897283641381));
#14116=CARTESIAN_POINT('Ctrl Pts',(0.332208473855475,-1.81788522252321,
3.33300441174764));
#14117=CARTESIAN_POINT('Ctrl Pts',(0.895833290042021,0.285591227891658,
3.33300441174764));
#14118=CARTESIAN_POINT('Ctrl Pts',(0.0542349483243482,-1.74340244083991,
3.34293392264922));
#14119=CARTESIAN_POINT('Ctrl Pts',(0.617859764510894,0.360074009574958,
3.34293392264922));
#14120=CARTESIAN_POINT('Ctrl Pts',(-0.231942319271813,-1.66672147309537,
3.34897162637417));
#14121=CARTESIAN_POINT('Ctrl Pts',(0.331682496914733,0.436754977319498,
3.34897162637417));
#14122=CARTESIAN_POINT('Ctrl Pts',(-0.522273747531617,-1.58892740135578,
3.35102435732185));
#14123=CARTESIAN_POINT('Ctrl Pts',(0.0413510686549291,0.514549049059088,
3.35102435732185));
#14124=CARTESIAN_POINT('Ctrl Pts',(-0.812605175791414,-1.5111333296162,
3.34897162637426));
#14125=CARTESIAN_POINT('Ctrl Pts',(-0.248980359604868,0.592343120798668,
3.34897162637426));
#14126=CARTESIAN_POINT('Ctrl Pts',(-1.09878244338755,-1.43445236187167,
3.34293392264938));
#14127=CARTESIAN_POINT('Ctrl Pts',(-0.535157627201004,0.669024088543198,
3.34293392264938));
#14128=CARTESIAN_POINT('Ctrl Pts',(-1.37675596891866,-1.35996958018837,
3.33300441174785));
#14129=CARTESIAN_POINT('Ctrl Pts',(-0.813131152732114,0.743506870226498,
3.33300441174785));
#14130=CARTESIAN_POINT('Ctrl Pts',(-1.64268529305271,-1.2887140325429,3.31897283641402));
#14131=CARTESIAN_POINT('Ctrl Pts',(-1.07906047686616,0.814762417871968,
3.31897283641402));
#14132=CARTESIAN_POINT('Ctrl Pts',(-1.8930437611574,-1.22163068319595,3.30006519349591));
#14133=CARTESIAN_POINT('Ctrl Pts',(-1.32941894497085,0.881845767218918,
3.30006519349591));
#14134=CARTESIAN_POINT('Ctrl Pts',(-2.12472293626507,-1.15955243532275,
3.27464765209779));
#14135=CARTESIAN_POINT('Ctrl Pts',(-1.56109812007852,0.943924015092118,
3.27464765209779));
#14136=CARTESIAN_POINT('Ctrl Pts',(-2.33513773482719,-1.10317195997247,
3.24001322621208));
#14137=CARTESIAN_POINT('Ctrl Pts',(-1.77151291864064,1.0003044904424,3.24001322621208));
#14138=CARTESIAN_POINT('Ctrl Pts',(-2.52232995605521,-1.05301395546503,
3.19196918412254));
#14139=CARTESIAN_POINT('Ctrl Pts',(-1.95870513986866,1.05046249494984,3.19196918412254));
#14140=CARTESIAN_POINT('Ctrl Pts',(-2.68507677070033,-1.00940607791014,
3.12505646843295));
#14141=CARTESIAN_POINT('Ctrl Pts',(-2.12145195451378,1.09407037250473,3.12505646843295));
#14142=CARTESIAN_POINT('Ctrl Pts',(-2.82300528751688,-0.972448243215919,
3.03403241435609));
#14143=CARTESIAN_POINT('Ctrl Pts',(-2.25938047133033,1.13102820719895,3.03403241435609));
#14144=CARTESIAN_POINT('Ctrl Pts',(-2.93671035054001,-0.94198106340354,
2.91510580081997));
#14145=CARTESIAN_POINT('Ctrl Pts',(-2.37308553435346,1.16149538701133,2.91510580081997));
#14146=CARTESIAN_POINT('Ctrl Pts',(-3.02786158735262,-0.917557163110504,
2.76722839711793));
#14147=CARTESIAN_POINT('Ctrl Pts',(-2.46423677116607,1.18591928730436,2.76722839711793));
#14148=CARTESIAN_POINT('Ctrl Pts',(-3.09934100177414,-0.898404311740807,
2.59347738935767));
#14149=CARTESIAN_POINT('Ctrl Pts',(-2.53571618558759,1.20507213867406,2.59347738935767));
#14150=CARTESIAN_POINT('Ctrl Pts',(-3.15473029191589,-0.883562796177992,
2.39962532458057));
#14151=CARTESIAN_POINT('Ctrl Pts',(-2.59110547572934,1.21991365423688,2.39962532458057));
#14152=CARTESIAN_POINT('Ctrl Pts',(-3.19775217034456,-0.872035118596162,
2.19251877196088));
#14153=CARTESIAN_POINT('Ctrl Pts',(-2.63412735415801,1.23144133181871,2.19251877196088));
#14154=CARTESIAN_POINT('Ctrl Pts',(-3.23174540145526,-0.862926659771925,
1.97856787413951));
#14155=CARTESIAN_POINT('Ctrl Pts',(-2.66812058526871,1.24054979064294,1.97856787413951));
#14156=CARTESIAN_POINT('Ctrl Pts',(-3.25908631610399,-0.855600683771469,
1.76209503442131));
#14157=CARTESIAN_POINT('Ctrl Pts',(-2.69546149991744,1.2478757666434,1.76209503442131));
#14158=CARTESIAN_POINT('Ctrl Pts',(-3.28074793135931,-0.849796471457051,
1.54401727992238));
#14159=CARTESIAN_POINT('Ctrl Pts',(-2.71712311517276,1.25367997895782,1.54401727992238));
#14160=CARTESIAN_POINT('Ctrl Pts',(-3.29722953615212,-0.84538023876285,
1.32371934078708));
#14161=CARTESIAN_POINT('Ctrl Pts',(-2.73360471996557,1.25809621165202,1.32371934078708));
#14162=CARTESIAN_POINT('Ctrl Pts',(-3.30933395645652,-0.842136869117439,
1.10060381648384));
#14163=CARTESIAN_POINT('Ctrl Pts',(-2.74570914026997,1.26133958129743,1.10060381648384));
#14164=CARTESIAN_POINT('Ctrl Pts',(-3.31908373992304,-0.839524422511207,
0.875890304828914));
#14165=CARTESIAN_POINT('Ctrl Pts',(-2.75545892373649,1.26395202790366,0.875890304828914));
#14166=CARTESIAN_POINT('Ctrl Pts',(-3.3303931391277,-0.836494078127436,
0.654020230869684));
#14167=CARTESIAN_POINT('Ctrl Pts',(-2.76676832294115,1.26698237228743,0.654020230869684));
#14168=CARTESIAN_POINT('Ctrl Pts',(-3.35031539848996,-0.831155924819917,
0.444963858672577));
#14169=CARTESIAN_POINT('Ctrl Pts',(-2.78669058230341,1.27232052559495,0.444963858672577));
#14170=CARTESIAN_POINT('Ctrl Pts',(-3.38758891539696,-0.821168516065618,
0.262319630540737));
#14171=CARTESIAN_POINT('Ctrl Pts',(-2.82396409921041,1.28230793434925,0.262319630540737));
#14172=CARTESIAN_POINT('Ctrl Pts',(-3.4496387877668,-0.804542302873664,
0.11901737132707));
#14173=CARTESIAN_POINT('Ctrl Pts',(-2.88601397158025,1.2989341475412,0.11901737132707));
#14174=CARTESIAN_POINT('Ctrl Pts',(-3.54033539990049,-0.780240218896203,
0.0241851999813871));
#14175=CARTESIAN_POINT('Ctrl Pts',(-2.97671058371394,1.32323623151866,0.0241851999813871));
#14176=CARTESIAN_POINT('Ctrl Pts',(-3.65680931559247,-0.749031127247248,
-0.0214179570895714));
#14177=CARTESIAN_POINT('Ctrl Pts',(-3.09318449940592,1.35444532316762,-0.0214179570895714));
#14178=CARTESIAN_POINT('Ctrl Pts',(-3.78869391002249,-0.713692756675616,
-0.0263068037112043));
#14179=CARTESIAN_POINT('Ctrl Pts',(-3.22506909383594,1.38978369373925,-0.0263068037112043));
#14180=CARTESIAN_POINT('Ctrl Pts',(-3.92277049429866,-0.677767044194892,
-0.00118366394785932));
#14181=CARTESIAN_POINT('Ctrl Pts',(-3.35914567811211,1.42570940621998,-0.00118366394785932));
#14182=CARTESIAN_POINT('Ctrl Pts',(-4.04675976550942,-0.644544219103847,
0.0470540298718583));
#14183=CARTESIAN_POINT('Ctrl Pts',(-3.48313494932287,1.45893223131102,0.0470540298718583));
#14184=CARTESIAN_POINT('Ctrl Pts',(-4.15292154232371,-0.616098256739405,
0.120497232333251));
#14185=CARTESIAN_POINT('Ctrl Pts',(-3.58929672613716,1.48737819367546,0.120497232333251));
#14186=CARTESIAN_POINT('Ctrl Pts',(-4.23720717254246,-0.593513990188742,
0.224659532804408));
#14187=CARTESIAN_POINT('Ctrl Pts',(-3.67358235635591,1.50996246022613,0.224659532804408));
#14188=CARTESIAN_POINT('Ctrl Pts',(-4.29891402785718,-0.576979688139698,
0.364350357241515));
#14189=CARTESIAN_POINT('Ctrl Pts',(-3.73528921167063,1.52649676227517,0.364350357241515));
#14190=CARTESIAN_POINT('Ctrl Pts',(-4.34018444275717,-0.565921313795949,
0.538436816836325));
#14191=CARTESIAN_POINT('Ctrl Pts',(-3.77655962657062,1.53755513661892,0.538436816836325));
#14192=CARTESIAN_POINT('Ctrl Pts',(-4.36512660693517,-0.559238081046971,
0.741129277895169));
#14193=CARTESIAN_POINT('Ctrl Pts',(-3.80150179074862,1.5442383693679,0.741129277895169));
#14194=CARTESIAN_POINT('Ctrl Pts',(-4.37883282444249,-0.555565511134598,
0.964078729991154));
#14195=CARTESIAN_POINT('Ctrl Pts',(-3.81520800825594,1.54791093928027,0.964078729991154));
#14196=CARTESIAN_POINT('Ctrl Pts',(-4.38643606159726,-0.553528229879115,
1.1981954227983));
#14197=CARTESIAN_POINT('Ctrl Pts',(-3.82281124541071,1.54994822053575,1.1981954227983));
#14198=CARTESIAN_POINT('Ctrl Pts',(-4.39215243495502,-0.551996532254268,
1.43558101932923));
#14199=CARTESIAN_POINT('Ctrl Pts',(-3.82852761876847,1.5514799181606,1.43558101932923));
#14200=CARTESIAN_POINT('Ctrl Pts',(-4.39832390226062,-0.550342892573617,
1.67142113207667));
#14201=CARTESIAN_POINT('Ctrl Pts',(-3.83469908607407,1.55313355784125,1.67142113207667));
#14202=CARTESIAN_POINT('Ctrl Pts',(-4.40593993377794,-0.548302183079021,
1.90332556813333));
#14203=CARTESIAN_POINT('Ctrl Pts',(-3.84231511759139,1.55517426733585,1.90332556813333));
#14204=CARTESIAN_POINT('Ctrl Pts',(-4.41515781144595,-0.54583226020195,
2.130657485557));
#14205=CARTESIAN_POINT('Ctrl Pts',(-3.8515329952594,1.55764419021292,2.130657485557));
#14206=CARTESIAN_POINT('Ctrl Pts',(-4.42583901148565,-0.542970241277118,
2.35385258470204));
#14207=CARTESIAN_POINT('Ctrl Pts',(-3.8622141952991,1.56050620913775,2.35385258470204));
#14208=CARTESIAN_POINT('Ctrl Pts',(-4.43804296945989,-0.539700200593456,
2.57377631141659));
#14209=CARTESIAN_POINT('Ctrl Pts',(-3.87441815327334,1.56377624982141,2.57377631141659));
#14210=CARTESIAN_POINT('Ctrl Pts',(-4.45084745128755,-0.536269250028235,
2.76449836272519));
#14211=CARTESIAN_POINT('Ctrl Pts',(-3.887222635101,1.56720720038663,2.76449836272519));
#14212=CARTESIAN_POINT('Ctrl Pts',(-4.46320446802865,-0.532958197371602,
2.91011271894269));
#14213=CARTESIAN_POINT('Ctrl Pts',(-3.8995796518421,1.57051825304327,2.91011271894269));
#14214=CARTESIAN_POINT('Ctrl Pts',(-4.47372590670627,-0.530138986374719,
3.01179023688553));
#14215=CARTESIAN_POINT('Ctrl Pts',(-3.91010109051972,1.57333746404015,3.01179023688553));
#14216=CARTESIAN_POINT('Ctrl Pts',(-4.48058344233111,-0.528301515241974,
3.07055226141567));
#14217=CARTESIAN_POINT('Ctrl Pts',(-3.91695862614456,1.57517493517289,3.07055226141567));
#14218=CARTESIAN_POINT('Ctrl Pts',(-4.48256963531681,-0.527769316435443,
3.08701851589457));
#14219=CARTESIAN_POINT('Ctrl Pts',(-3.91894481913026,1.57570713397942,3.08701851589457));
#14220=CARTESIAN_POINT('',(-4.39990749973883,0.13143350442279,11.8105861003151));
#14221=CARTESIAN_POINT('Ctrl Pts',(-4.39990749973883,0.131433504422787,
11.8105861003151));
#14222=CARTESIAN_POINT('Ctrl Pts',(-4.49754913369766,0.157596501389713,
11.7068367844248));
#14223=CARTESIAN_POINT('Ctrl Pts',(-4.69125400852046,0.209499566168453,
11.5019717467543));
#14224=CARTESIAN_POINT('Ctrl Pts',(-5.00967190543604,0.294819384502599,
11.2375756728753));
#14225=CARTESIAN_POINT('Ctrl Pts',(-5.35454459136527,0.38722774218889,11.0061555791443));
#14226=CARTESIAN_POINT('Ctrl Pts',(-5.71913861942256,0.48492041757205,10.8005509999885));
#14227=CARTESIAN_POINT('Ctrl Pts',(-6.06462842910348,0.577494133069235,
10.66692181492));
#14228=CARTESIAN_POINT('Ctrl Pts',(-6.33148581479284,0.648998354058979,
10.6014247262997));
#14229=CARTESIAN_POINT('Ctrl Pts',(-6.60565152217716,0.722460833944915,
10.5327688098564));
#14230=CARTESIAN_POINT('Ctrl Pts',(-6.85297550359782,0.78873109503543,10.4523928827042));
#14231=CARTESIAN_POINT('Ctrl Pts',(-7.10446088941469,0.856116401073289,
10.2839337584245));
#14232=CARTESIAN_POINT('Ctrl Pts',(-7.35838141384484,0.924154200536037,
10.0446906337461));
#14233=CARTESIAN_POINT('Ctrl Pts',(-7.62832379034323,0.996485042321717,
9.6700018953962));
#14234=CARTESIAN_POINT('Ctrl Pts',(-7.86849512871787,1.0608387584843,9.24528298390541));
#14235=CARTESIAN_POINT('Ctrl Pts',(-8.00203202129173,1.09661986100923,8.8659022538591));
#14236=CARTESIAN_POINT('Ctrl Pts',(-8.07463904021301,1.11607485309402,8.47098152553076));
#14237=CARTESIAN_POINT('Ctrl Pts',(-8.08171248804463,1.11797017772821,8.08076694642368));
#14238=CARTESIAN_POINT('Ctrl Pts',(-8.11167522300546,1.12599866836399,7.7043597380442));
#14239=CARTESIAN_POINT('Ctrl Pts',(-8.15245921105438,1.13692670502582,7.42372739456374));
#14240=CARTESIAN_POINT('Ctrl Pts',(-8.20488040179384,1.15097292075073,7.14034281931128));
#14241=CARTESIAN_POINT('Ctrl Pts',(-8.2477646225197,1.16246371306227,6.84786314045739));
#14242=CARTESIAN_POINT('Ctrl Pts',(-8.2340924899642,1.15880027618521,6.58185725748997));
#14243=CARTESIAN_POINT('Ctrl Pts',(-8.15624193537567,1.1379402829529,6.37882425840707));
#14244=CARTESIAN_POINT('Ctrl Pts',(-8.06959783090691,1.11472406513158,6.24539149037989));
#14245=CARTESIAN_POINT('Ctrl Pts',(-7.96390674795061,1.08640422480626,6.13212489925341));
#14246=CARTESIAN_POINT('Ctrl Pts',(-7.80782708725179,1.04458280576709,6.00502448889162));
#14247=CARTESIAN_POINT('Ctrl Pts',(-7.51121080585291,0.965104712704338,
5.83268998867983));
#14248=CARTESIAN_POINT('Ctrl Pts',(-7.07025856977831,0.846951917147452,
5.6633705113799));
#14249=CARTESIAN_POINT('Ctrl Pts',(-6.55772910172197,0.709620060084601,
5.45056821320793));
#14250=CARTESIAN_POINT('Ctrl Pts',(-6.05533862945534,0.575004938755668,
5.20523396509008));
#14251=CARTESIAN_POINT('Ctrl Pts',(-5.47842644000812,0.420421783489613,
4.90183331737205));
#14252=CARTESIAN_POINT('Ctrl Pts',(-4.97546534076346,0.28565376312274,4.5730826167126));
#14253=CARTESIAN_POINT('Ctrl Pts',(-4.62774205069207,0.192481588358615,
4.14707585774942));
#14254=CARTESIAN_POINT('Ctrl Pts',(-4.50892895738859,0.160645715957704,
3.89751682838105));
#14255=CARTESIAN_POINT('Ctrl Pts',(-4.4618940931088,0.148042762057827,3.76716196298096));
#14256=CARTESIAN_POINT('',(-4.38674149674992,0.152249769835312,11.8181058720863));
#14257=CARTESIAN_POINT('Ctrl Pts',(-4.38674149675009,0.152249769834917,
11.8181058720862));
#14258=CARTESIAN_POINT('Ctrl Pts',(-4.3869775568074,0.151688294341147,11.8180210706515));
#14259=CARTESIAN_POINT('Ctrl Pts',(-4.38748854871073,0.150590557851844,
11.8178062692381));
#14260=CARTESIAN_POINT('Ctrl Pts',(-4.38858693511445,0.14845239833212,11.817285750215));
#14261=CARTESIAN_POINT('Ctrl Pts',(-4.39064941066155,0.144825508674648,
11.8162052857216));
#14262=CARTESIAN_POINT('Ctrl Pts',(-4.39446005348131,0.138892971386962,
11.8140046108773));
#14263=CARTESIAN_POINT('Ctrl Pts',(-4.3978421585968,0.134197554896133,11.8118993900741));
#14264=CARTESIAN_POINT('Ctrl Pts',(-4.39990749973883,0.131433504422785,
11.8105861003151));
#14265=CARTESIAN_POINT('',(-4.34854691846782,0.241356558688882,11.8322728954492));
#14266=CARTESIAN_POINT('Origin',(-1.23271387586545,-1.70581675488325,15.3403250734267));
#14267=CARTESIAN_POINT('',(-4.25518135747447,0.44557426920425,11.8702643430631));
#14268=CARTESIAN_POINT('Ctrl Pts',(-4.25518135747447,0.445574269204249,
11.8702643430631));
#14269=CARTESIAN_POINT('Ctrl Pts',(-4.28743714356257,0.378238787953571,
11.8563818704341));
#14270=CARTESIAN_POINT('Ctrl Pts',(-4.31850684021249,0.310110504419452,
11.8437528706395));
#14271=CARTESIAN_POINT('Ctrl Pts',(-4.34854691846782,0.241356558688883,
11.8322728954492));
#14272=CARTESIAN_POINT('',(-4.2368109319615,0.483558887244307,11.8782524024265));
#14273=CARTESIAN_POINT('Origin',(-1.56538794823573,-1.42563865727917,14.6978241049146));
#14274=CARTESIAN_POINT('Origin',(-1.70912501884918,-1.31404604504918,14.5049189366084));
#14275=CARTESIAN_POINT('Ctrl Pts',(-4.39990749973883,0.131433504422787,
11.8105861003151));
#14276=CARTESIAN_POINT('Ctrl Pts',(-4.49754913369766,0.157596501389713,
11.7068367844248));
#14277=CARTESIAN_POINT('Ctrl Pts',(-4.69125400852046,0.209499566168453,
11.5019717467543));
#14278=CARTESIAN_POINT('Ctrl Pts',(-5.00967190543604,0.294819384502599,
11.2375756728753));
#14279=CARTESIAN_POINT('Ctrl Pts',(-5.35454459136527,0.38722774218889,11.0061555791443));
#14280=CARTESIAN_POINT('Ctrl Pts',(-5.71913861942256,0.48492041757205,10.8005509999885));
#14281=CARTESIAN_POINT('Ctrl Pts',(-6.06462842910348,0.577494133069235,
10.66692181492));
#14282=CARTESIAN_POINT('Ctrl Pts',(-6.33148581479284,0.648998354058979,
10.6014247262997));
#14283=CARTESIAN_POINT('Ctrl Pts',(-6.60565152217716,0.722460833944915,
10.5327688098564));
#14284=CARTESIAN_POINT('Ctrl Pts',(-6.85297550359782,0.78873109503543,10.4523928827042));
#14285=CARTESIAN_POINT('Ctrl Pts',(-7.10446088941469,0.856116401073289,
10.2839337584245));
#14286=CARTESIAN_POINT('Ctrl Pts',(-7.35838141384484,0.924154200536037,
10.0446906337461));
#14287=CARTESIAN_POINT('Ctrl Pts',(-7.62832379034323,0.996485042321717,
9.6700018953962));
#14288=CARTESIAN_POINT('Ctrl Pts',(-7.86849512871787,1.0608387584843,9.24528298390541));
#14289=CARTESIAN_POINT('Ctrl Pts',(-8.00203202129173,1.09661986100923,8.8659022538591));
#14290=CARTESIAN_POINT('Ctrl Pts',(-8.07463904021301,1.11607485309402,8.47098152553076));
#14291=CARTESIAN_POINT('Ctrl Pts',(-8.08171248804463,1.11797017772821,8.08076694642368));
#14292=CARTESIAN_POINT('Ctrl Pts',(-8.11167522300546,1.12599866836399,7.7043597380442));
#14293=CARTESIAN_POINT('Ctrl Pts',(-8.15245921105438,1.13692670502582,7.42372739456374));
#14294=CARTESIAN_POINT('Ctrl Pts',(-8.20488040179384,1.15097292075073,7.14034281931128));
#14295=CARTESIAN_POINT('Ctrl Pts',(-8.2477646225197,1.16246371306227,6.84786314045739));
#14296=CARTESIAN_POINT('Ctrl Pts',(-8.2340924899642,1.15880027618521,6.58185725748997));
#14297=CARTESIAN_POINT('Ctrl Pts',(-8.15624193537567,1.1379402829529,6.37882425840707));
#14298=CARTESIAN_POINT('Ctrl Pts',(-8.06959783090691,1.11472406513158,6.24539149037989));
#14299=CARTESIAN_POINT('Ctrl Pts',(-7.96390674795061,1.08640422480626,6.13212489925341));
#14300=CARTESIAN_POINT('Ctrl Pts',(-7.80782708725179,1.04458280576709,6.00502448889162));
#14301=CARTESIAN_POINT('Ctrl Pts',(-7.51121080585291,0.965104712704338,
5.83268998867983));
#14302=CARTESIAN_POINT('Ctrl Pts',(-7.07025856977831,0.846951917147452,
5.6633705113799));
#14303=CARTESIAN_POINT('Ctrl Pts',(-6.55772910172197,0.709620060084601,
5.45056821320793));
#14304=CARTESIAN_POINT('Ctrl Pts',(-6.05533862945534,0.575004938755668,
5.20523396509008));
#14305=CARTESIAN_POINT('Ctrl Pts',(-5.47842644000812,0.420421783489613,
4.90183331737205));
#14306=CARTESIAN_POINT('Ctrl Pts',(-4.97546534076346,0.28565376312274,4.5730826167126));
#14307=CARTESIAN_POINT('Ctrl Pts',(-4.62774205069207,0.192481588358615,
4.14707585774942));
#14308=CARTESIAN_POINT('Ctrl Pts',(-4.50892895738859,0.160645715957704,
3.89751682838105));
#14309=CARTESIAN_POINT('Ctrl Pts',(-4.4618940931088,0.148042762057827,3.76716196298096));
#14310=CARTESIAN_POINT('Ctrl Pts',(-4.40610257791561,0.10831315791016,11.8105861003151));
#14311=CARTESIAN_POINT('Ctrl Pts',(-4.50374507702499,0.134476386693474,
11.7068358651574));
#14312=CARTESIAN_POINT('Ctrl Pts',(-4.69744752408798,0.186378800955935,
11.5019742817009));
#14313=CARTESIAN_POINT('Ctrl Pts',(-5.01586638212965,0.271698876823038,
11.2375781425806));
#14314=CARTESIAN_POINT('Ctrl Pts',(-5.36073964308098,0.364107388586036,
11.0061565233321));
#14315=CARTESIAN_POINT('Ctrl Pts',(-5.72534334415641,0.461802655846596,
10.8005488998531));
#14316=CARTESIAN_POINT('Ctrl Pts',(-6.07081472117805,0.554371432327612,
10.6669268865357));
#14317=CARTESIAN_POINT('Ctrl Pts',(-6.33766369106806,0.62587339831072,10.6014312575901));
#14318=CARTESIAN_POINT('Ctrl Pts',(-6.61182227957146,0.699333970698262,
10.5327811735249));
#14319=CARTESIAN_POINT('Ctrl Pts',(-6.85916868333988,0.765610239838752,
10.4524004053925));
#14320=CARTESIAN_POINT('Ctrl Pts',(-7.11066195746784,0.832997659543196,
10.2839369025062));
#14321=CARTESIAN_POINT('Ctrl Pts',(-7.36459656854927,0.901039233512779,
10.0446770327022));
#14322=CARTESIAN_POINT('Ctrl Pts',(-7.63451688382228,0.973364164010934,
9.67000537128577));
#14323=CARTESIAN_POINT('Ctrl Pts',(-7.87469455084438,1.0377195759295,9.24528421592605));
#14324=CARTESIAN_POINT('Ctrl Pts',(-8.00823128702896,1.07350063655004,8.86590036282094));
#14325=CARTESIAN_POINT('Ctrl Pts',(-8.08083869530086,1.09295573296102,8.47096393307005));
#14326=CARTESIAN_POINT('Ctrl Pts',(-8.08790913116448,1.09485025054081,8.08075207953364));
#14327=CARTESIAN_POINT('Ctrl Pts',(-8.11787189500846,1.10287874891581,7.70436013759456));
#14328=CARTESIAN_POINT('Ctrl Pts',(-8.15865443057292,1.1138063963856,7.42374345640766));
#14329=CARTESIAN_POINT('Ctrl Pts',(-8.21107842618733,1.12785336367449,7.14036999923671));
#14330=CARTESIAN_POINT('Ctrl Pts',(-8.25396944631471,1.13934597788017,6.84789820200929));
#14331=CARTESIAN_POINT('Ctrl Pts',(-8.24031812870394,1.13568811835075,6.58189724851307));
#14332=CARTESIAN_POINT('Ctrl Pts',(-8.16244596760929,1.11482233567257,6.37880997093398));
#14333=CARTESIAN_POINT('Ctrl Pts',(-8.07579191235616,1.09160345154661,6.24536441066714));
#14334=CARTESIAN_POINT('Ctrl Pts',(-7.97009137637762,1.06328107829162,6.13209608067231));
#14335=CARTESIAN_POINT('Ctrl Pts',(-7.81399260224414,1.02145453782307,6.00498322378118));
#14336=CARTESIAN_POINT('Ctrl Pts',(-7.51738480597013,0.941978718342671,
5.83267352057959));
#14337=CARTESIAN_POINT('Ctrl Pts',(-7.07644541070296,0.823829363469767,
5.66336515001065));
#14338=CARTESIAN_POINT('Ctrl Pts',(-6.56392284376063,0.686499355554842,
5.45056727419079));
#14339=CARTESIAN_POINT('Ctrl Pts',(-6.06153370995061,0.551884592864275,
5.20523328921882));
#14340=CARTESIAN_POINT('Ctrl Pts',(-5.48461630527476,0.397300040181924,
4.90183082421786));
#14341=CARTESIAN_POINT('Ctrl Pts',(-4.98165380025924,0.26253164313988,4.57306922084908));
#14342=CARTESIAN_POINT('Ctrl Pts',(-4.63394385126977,0.169363043107885,
4.14707693759231));
#14343=CARTESIAN_POINT('Ctrl Pts',(-4.51511830855761,0.137523834897972,
3.89750095625433));
#14344=CARTESIAN_POINT('Ctrl Pts',(-4.46808917128558,0.124922415545199,
3.76716196298096));
#14345=CARTESIAN_POINT('Ctrl Pts',(-4.40291516435328,0.0645741697282324,
11.796556443628));
#14346=CARTESIAN_POINT('Ctrl Pts',(-4.50048856350348,0.0907188832332889,
11.6928796307718));
#14347=CARTESIAN_POINT('Ctrl Pts',(-4.69504931294762,0.14285127892564,11.4870859088997));
#14348=CARTESIAN_POINT('Ctrl Pts',(-5.0153119872158,0.228665403861629,11.2211535933451));
#14349=CARTESIAN_POINT('Ctrl Pts',(-5.36151215707251,0.321429459794252,
10.9888940346623));
#14350=CARTESIAN_POINT('Ctrl Pts',(-5.72763036696513,0.419530538469309,
10.7823369202495));
#14351=CARTESIAN_POINT('Ctrl Pts',(-6.0761462566863,0.51291508966951,10.6475498808516));
#14352=CARTESIAN_POINT('Ctrl Pts',(-6.3440656643213,0.584703878581932,10.5818347915591));
#14353=CARTESIAN_POINT('Ctrl Pts',(-6.61761927622536,0.658002347978243,
10.5133104011913));
#14354=CARTESIAN_POINT('Ctrl Pts',(-6.861888253579,0.723454023196128,10.4338049599974));
#14355=CARTESIAN_POINT('Ctrl Pts',(-7.10935635790786,0.789762901903506,
10.2680061458923));
#14356=CARTESIAN_POINT('Ctrl Pts',(-7.36030385820222,0.85700408194999,10.0317153152368));
#14357=CARTESIAN_POINT('Ctrl Pts',(-7.62907538108075,0.929021194453772,
9.65885131647057));
#14358=CARTESIAN_POINT('Ctrl Pts',(-7.86798181564301,0.993035980661329,
9.23617470335927));
#14359=CARTESIAN_POINT('Ctrl Pts',(-8.00012724262594,1.02844424110487,8.86049547284917));
#14360=CARTESIAN_POINT('Ctrl Pts',(-8.07209396647679,1.04772766664262,8.46966777014732));
#14361=CARTESIAN_POINT('Ctrl Pts',(-8.07922818767295,1.04963927545076,8.08019062380329));
#14362=CARTESIAN_POINT('Ctrl Pts',(-8.10927699136119,1.05769082813254,7.70205072960373));
#14363=CARTESIAN_POINT('Ctrl Pts',(-8.15026361671259,1.06867316129593,7.42011617327014));
#14364=CARTESIAN_POINT('Ctrl Pts',(-8.20272880746984,1.08273116679008,7.13664584277076));
#14365=CARTESIAN_POINT('Ctrl Pts',(-8.24520628166168,1.0941129716963,6.84609737205768));
#14366=CARTESIAN_POINT('Ctrl Pts',(-8.23158429149218,1.09046297043107,6.58572297937688));
#14367=CARTESIAN_POINT('Ctrl Pts',(-8.15587046120199,1.07017551074895,6.38835239922954));
#14368=CARTESIAN_POINT('Ctrl Pts',(-8.07141284400203,1.04754516042556,6.258182462026));
#14369=CARTESIAN_POINT('Ctrl Pts',(-7.96785647648126,1.01979731537727,6.14717486337006));
#14370=CARTESIAN_POINT('Ctrl Pts',(-7.81419507107175,0.978623865889961,
6.02200778579695));
#14371=CARTESIAN_POINT('Ctrl Pts',(-7.52061390092899,0.899959028437226,
5.85130334614999));
#14372=CARTESIAN_POINT('Ctrl Pts',(-7.08058961552272,0.782054876512532,
5.68226275410023));
#14373=CARTESIAN_POINT('Ctrl Pts',(-6.56675458224047,0.644373194301734,
5.46896563973939));
#14374=CARTESIAN_POINT('Ctrl Pts',(-6.06367525013762,0.509573493535987,
5.2232740147586));
#14375=CARTESIAN_POINT('Ctrl Pts',(-5.48616446123447,0.354829944029128,
4.91953641642625));
#14376=CARTESIAN_POINT('Ctrl Pts',(-4.9801291599051,0.219238193696283,4.58909349075147));
#14377=CARTESIAN_POINT('Ctrl Pts',(-4.62817642216375,0.124932741844566,
4.15817276994372));
#14378=CARTESIAN_POINT('Ctrl Pts',(-4.50810575167473,0.0927599026523696,
3.90580371045959));
#14379=CARTESIAN_POINT('Ctrl Pts',(-4.46061919574128,0.080035918338667,
3.77419700335406));
#14380=CARTESIAN_POINT('Ctrl Pts',(-4.37768603361793,0.0426571860882519,
11.7672856238756));
#14381=CARTESIAN_POINT('Ctrl Pts',(-4.4751175795493,0.0687638901378774,
11.6637595374443));
#14382=CARTESIAN_POINT('Ctrl Pts',(-4.67146255830039,0.121374368632138,
11.4560302833013));
#14383=CARTESIAN_POINT('Ctrl Pts',(-4.99557465491178,0.208219943176319,
11.1868927865811));
#14384=CARTESIAN_POINT('Ctrl Pts',(-5.34454476327236,0.301726201894137,
10.9528809104907));
#14385=CARTESIAN_POINT('Ctrl Pts',(-5.71384864247256,0.400680878087512,
10.7443346810372));
#14386=CARTESIAN_POINT('Ctrl Pts',(-6.06866716597707,0.495754214920148,
10.6071361653846));
#14387=CARTESIAN_POINT('Ctrl Pts',(-6.33879737818042,0.568135387131283,
10.540967107949));
#14388=CARTESIAN_POINT('Ctrl Pts',(-6.61106975689777,0.641090551129898,
10.4727205567864));
#14389=CARTESIAN_POINT('Ctrl Pts',(-6.84897810060804,0.704837899699691,
10.3950284103723));
#14390=CARTESIAN_POINT('Ctrl Pts',(-7.08806937487797,0.768902213557648,
10.234777368477));
#14391=CARTESIAN_POINT('Ctrl Pts',(-7.3328223793598,0.834483583453643,10.0046362201527));
#14392=CARTESIAN_POINT('Ctrl Pts',(-7.59913811631925,0.905842670103627,
9.63558931371895));
#14393=CARTESIAN_POINT('Ctrl Pts',(-7.83540923585815,0.969151325778873,
9.21717233709717));
#14394=CARTESIAN_POINT('Ctrl Pts',(-7.9646514821359,1.00378168129698,8.84921390584317));
#14395=CARTESIAN_POINT('Ctrl Pts',(-8.03528255322126,1.02270721975485,8.46691646823682));
#14396=CARTESIAN_POINT('Ctrl Pts',(-8.04254179813168,1.02465232856626,8.07897946972552));
#14397=CARTESIAN_POINT('Ctrl Pts',(-8.07277018857148,1.03275200137309,7.69723355728135));
#14398=CARTESIAN_POINT('Ctrl Pts',(-8.11417873287728,1.04384738737958,7.41259133413029));
#14399=CARTESIAN_POINT('Ctrl Pts',(-8.16673737243891,1.0579304324054,7.12894862515868));
#14400=CARTESIAN_POINT('Ctrl Pts',(-8.20837022762595,1.06908592233137,6.8424339710948));
#14401=CARTESIAN_POINT('Ctrl Pts',(-8.19486509106195,1.06546723189537,6.59381175490167));
#14402=CARTESIAN_POINT('Ctrl Pts',(-8.12359651814278,1.04637087533596,6.40822306593102));
#14403=CARTESIAN_POINT('Ctrl Pts',(-8.04369483483858,1.02496128382071,6.28485302475822));
#14404=CARTESIAN_POINT('Ctrl Pts',(-7.94458667955791,0.998405333649918,
6.17855745994456));
#14405=CARTESIAN_POINT('Ctrl Pts',(-7.79595937050461,0.958580766215877,
6.05741667913553));
#14406=CARTESIAN_POINT('Ctrl Pts',(-7.50871550370568,0.88161400407631,5.89012770190778));
#14407=CARTESIAN_POINT('Ctrl Pts',(-7.0706348013897,0.764230633671083,5.72167549359611));
#14408=CARTESIAN_POINT('Ctrl Pts',(-6.5540799556138,0.625820179899048,5.50734861815085));
#14409=CARTESIAN_POINT('Ctrl Pts',(-6.04956420554889,0.490635592100373,
5.26091153351829));
#14410=CARTESIAN_POINT('Ctrl Pts',(-5.47080146025223,0.335556581888915,
4.95646986864331));
#14411=CARTESIAN_POINT('Ctrl Pts',(-4.95835146085607,0.198246018389383,
4.62248995318707));
#14412=CARTESIAN_POINT('Ctrl Pts',(-4.59758244560127,0.101578252097688,
4.18132548363876));
#14413=CARTESIAN_POINT('Ctrl Pts',(-4.47488070480479,0.0687004197413792,
3.92308374120045));
#14414=CARTESIAN_POINT('Ctrl Pts',(-4.42645512791889,0.0557248255217898,
3.78887458266364));
#14415=CARTESIAN_POINT('Ctrl Pts',(-4.36526624577324,0.0393293139651011,
11.7547577775405));
#14416=CARTESIAN_POINT('Ctrl Pts',(-4.462637168512,0.0654197740792256,11.6512961064053));
#14417=CARTESIAN_POINT('Ctrl Pts',(-4.65974554183767,0.118234803533251,
11.442738806744));
#14418=CARTESIAN_POINT('Ctrl Pts',(-4.98550528234724,0.205521862929361,
11.1722294927876));
#14419=CARTESIAN_POINT('Ctrl Pts',(-5.33566097788268,0.29934579877324,10.9374674705902));
#14420=CARTESIAN_POINT('Ctrl Pts',(-5.70632931912773,0.398666081469635,
10.7280695887413));
#14421=CARTESIAN_POINT('Ctrl Pts',(-6.06384344546407,0.494461702904175,
10.5898397099152));
#14422=CARTESIAN_POINT('Ctrl Pts',(-6.33491900485657,0.567096180131211,
10.5234765064095));
#14423=CARTESIAN_POINT('Ctrl Pts',(-6.60664228072597,0.639904212465156,
10.4553494743371));
#14424=CARTESIAN_POINT('Ctrl Pts',(-6.8418306113212,0.702922735717372,10.3784329123269));
#14425=CARTESIAN_POINT('Ctrl Pts',(-7.07733743840935,0.766026599847657,
10.2205558508687));
#14426=CARTESIAN_POINT('Ctrl Pts',(-7.3194406724111,0.830897965883391,9.99304501740382));
#14427=CARTESIAN_POINT('Ctrl Pts',(-7.58470305177623,0.901974806216633,
9.62563358808958));
#14428=CARTESIAN_POINT('Ctrl Pts',(-7.81984691825478,0.964981415344694,
9.20903949392042));
#14429=CARTESIAN_POINT('Ctrl Pts',(-7.94784659338026,0.999278824926013,
8.84438522402643));
#14430=CARTESIAN_POINT('Ctrl Pts',(-8.01790604838202,1.0180511993159,8.46573709363457));
#14431=CARTESIAN_POINT('Ctrl Pts',(-8.02521849097772,1.02001056240412,8.07845955750479));
#14432=CARTESIAN_POINT('Ctrl Pts',(-8.05552374714506,1.02813083132057,7.6951718595586));
#14433=CARTESIAN_POINT('Ctrl Pts',(-8.09711272128414,1.03927456335518,7.40937238436613));
#14434=CARTESIAN_POINT('Ctrl Pts',(-8.14971164745181,1.05336840314455,7.12565705017148));
#14435=CARTESIAN_POINT('Ctrl Pts',(-8.19098371232079,1.06442721959616,6.8408696776684));
#14436=CARTESIAN_POINT('Ctrl Pts',(-8.17753074630009,1.06082250821511,6.59727787804477));
#14437=CARTESIAN_POINT('Ctrl Pts',(-8.10816249423483,1.04223534109386,6.41672618659136));
#14438=CARTESIAN_POINT('Ctrl Pts',(-8.03020970920239,1.02134795529666,6.29626516002264));
#14439=CARTESIAN_POINT('Ctrl Pts',(-7.93300439915508,0.995301870969469,
6.19198615507442));
#14440=CARTESIAN_POINT('Ctrl Pts',(-7.78652969114894,0.956054091247638,
6.07256733032961));
#14441=CARTESIAN_POINT('Ctrl Pts',(-7.50199905569102,0.879814337254775,
5.90674273368555));
#14442=CARTESIAN_POINT('Ctrl Pts',(-7.06475153359634,0.762654216816996,
5.73854350352349));
#14443=CARTESIAN_POINT('Ctrl Pts',(-6.54703332936491,0.623932042086293,
5.5237763509783));
#14444=CARTESIAN_POINT('Ctrl Pts',(-6.04190293430869,0.488582760658567,
5.27702023853286));
#14445=CARTESIAN_POINT('Ctrl Pts',(-5.46260381387957,0.333360029163525,
4.97227704636915));
#14446=CARTESIAN_POINT('Ctrl Pts',(-4.94740819214276,0.195313778375095,
4.6367821770228));
#14447=CARTESIAN_POINT('Ctrl Pts',(-4.582867212341,0.0976353172291641,4.19123490599198));
#14448=CARTESIAN_POINT('Ctrl Pts',(-4.45903808887791,0.0644554035977742,
3.93047791113146));
#14449=CARTESIAN_POINT('Ctrl Pts',(-4.41021120669539,0.0513722799480397,
3.79515655425571));
#14450=CARTESIAN_POINT('Origin',(-4.34456072216504,0.116603380068226,11.7547577775405));
#14451=CARTESIAN_POINT('Ctrl Pts',(-4.26119373042795,0.0145528918841498,
11.638842338191));
#14452=CARTESIAN_POINT('Ctrl Pts',(-4.26125236043256,0.0145635653496478,
11.6390494463487));
#14453=CARTESIAN_POINT('Ctrl Pts',(-4.2613108171609,0.0145742781139868,
11.6392564542239));
#14454=CARTESIAN_POINT('Ctrl Pts',(-4.27313475944305,0.0168564057035511,
11.6811561932301));
#14455=CARTESIAN_POINT('Ctrl Pts',(-4.28208612481729,0.0278778097684391,
11.7209829966278));
#14456=CARTESIAN_POINT('Ctrl Pts',(-4.28908755611092,0.0448598329498131,
11.7564896488273));
#14457=CARTESIAN_POINT('Ctrl Pts',(-4.26119373042795,0.0145528918841498,
11.638842338191));
#14458=CARTESIAN_POINT('Ctrl Pts',(-4.26127828911038,0.0145682856093495,
11.6390223367578));
#14459=CARTESIAN_POINT('Ctrl Pts',(-4.26136364251986,0.0145842788598119,
11.639202913148));
#14460=CARTESIAN_POINT('Ctrl Pts',(-4.27851654506032,0.0177444550235382,
11.675650547572));
#14461=CARTESIAN_POINT('Ctrl Pts',(-4.29379674050307,0.0238869170482415,
11.7114368827851));
#14462=CARTESIAN_POINT('Ctrl Pts',(-4.30450945627382,0.0325071787760864,
11.7471124459761));
#14463=CARTESIAN_POINT('Ctrl Pts',(-4.26119373042795,0.0145528918841498,
11.638842338191));
#14464=CARTESIAN_POINT('Ctrl Pts',(-4.26130467158735,0.0145730884822054,
11.6389946828916));
#14465=CARTESIAN_POINT('Ctrl Pts',(-4.2614161729233,0.0145934983333006,
11.639149772681));
#14466=CARTESIAN_POINT('Ctrl Pts',(-4.28389600361695,0.0186893116053435,
11.6701638807614));
#14467=CARTESIAN_POINT('Ctrl Pts',(-4.30492281676891,0.023383483481463,
11.7014497023147));
#14468=CARTESIAN_POINT('Ctrl Pts',(-4.32325512462864,0.0279667529147067,
11.7334386747809));
#14469=CARTESIAN_POINT('Ctrl Pts',(-4.26119373042795,0.0145528918841498,
11.638842338191));
#14470=CARTESIAN_POINT('Ctrl Pts',(-4.26133114891829,0.0145779086230217,
11.6389687144068));
#14471=CARTESIAN_POINT('Ctrl Pts',(-4.26146855208158,0.014602959314705,
11.639095090611));
#14472=CARTESIAN_POINT('Ctrl Pts',(-4.28927567952828,0.0196775034910065,
11.6647148078266));
#14473=CARTESIAN_POINT('Ctrl Pts',(-4.3154573308492,0.0258092392550238,
11.6915792314772));
#14474=CARTESIAN_POINT('Ctrl Pts',(-4.33960641395499,0.0324815600844758,
11.7196558802127));
#14475=CARTESIAN_POINT('',(-4.28933390296185,0.0388612606170688,11.7451969266016));
#14476=CARTESIAN_POINT('Origin',(-4.31223161686593,0.107940822411309,11.7119910933921));
#14477=CARTESIAN_POINT('',(-4.26119373042794,0.0145528918841489,11.638842338191));
#14478=CARTESIAN_POINT('Ctrl Pts',(-4.33293714046261,0.0306667563050961,
11.7119910933921));
#14479=CARTESIAN_POINT('Ctrl Pts',(-4.31066098923177,0.0246978795758798,
11.6866819998201));
#14480=CARTESIAN_POINT('Ctrl Pts',(-4.28674775885131,0.0192161812931609,
11.6623857426252));
#14481=CARTESIAN_POINT('Ctrl Pts',(-4.26146855208158,0.014602959314705,
11.639095090611));
#14482=CARTESIAN_POINT('Ctrl Pts',(-4.26133114891829,0.0145779086230217,
11.6389687144068));
#14483=CARTESIAN_POINT('Ctrl Pts',(-4.26119373042795,0.0145528918841498,
11.638842338191));
#14484=CARTESIAN_POINT('Ctrl Pts',(-4.26119373042795,0.0145528918841497,
11.638842338191));
#14485=CARTESIAN_POINT('Ctrl Pts',(-4.26125633218466,0.0145642883985241,
11.6390452934056));
#14486=CARTESIAN_POINT('Ctrl Pts',(-4.26131888429506,0.0145758879335255,
11.639248262593));
#14487=CARTESIAN_POINT('Ctrl Pts',(-4.2613813161263,0.0145876766504085,
11.6394510185953));
#14488=CARTESIAN_POINT('Ctrl Pts',(-4.265016010492,0.0152739993480501,11.6512551909948));
#14489=CARTESIAN_POINT('Ctrl Pts',(-4.26847153091007,0.0166441818282242,
11.6629691301088));
#14490=CARTESIAN_POINT('Ctrl Pts',(-4.27169388060566,0.0186106171418232,
11.6744752186442));
#14491=CARTESIAN_POINT('Ctrl Pts',(-4.27431552229403,0.0202104710629102,
11.6838363508068));
#14492=CARTESIAN_POINT('Ctrl Pts',(-4.27678305604313,0.0222047860179351,
11.6930581330534));
#14493=CARTESIAN_POINT('Ctrl Pts',(-4.2790962892493,0.0245559887567339,
11.7021068786235));
#14494=CARTESIAN_POINT('Ctrl Pts',(-4.28076743592503,0.0262545657227037,
11.7086439545391));
#14495=CARTESIAN_POINT('Ctrl Pts',(-4.28235877711272,0.0281396923832335,
11.7150914206716));
#14496=CARTESIAN_POINT('Ctrl Pts',(-4.28387859102004,0.0302000190087009,
11.7214511909726));
#14497=CARTESIAN_POINT('Ctrl Pts',(-4.2848378009235,0.0315003661722649,
11.7254650736113));
#14498=CARTESIAN_POINT('Ctrl Pts',(-4.28576868964866,0.032870535179902,
11.7294443738346));
#14499=CARTESIAN_POINT('Ctrl Pts',(-4.28667443781518,0.0343117715877457,
11.733390025982));
#14500=CARTESIAN_POINT('Ctrl Pts',(-4.28758560787174,0.0357616353664485,
11.7373592971583));
#14501=CARTESIAN_POINT('Ctrl Pts',(-4.28847140705044,0.0372834000391179,
11.741294500388));
#14502=CARTESIAN_POINT('Ctrl Pts',(-4.28933737923093,0.0388717353254243,
11.7451918804009));
#14503=CARTESIAN_POINT('Ctrl Pts',(-4.28933194406438,0.0388554328133947,
11.7451997357866));
#14504=CARTESIAN_POINT('Ctrl Pts',(-4.29334608958886,0.0462195341306841,
11.7632876305128));
#14505=CARTESIAN_POINT('Ctrl Pts',(-4.29689723089593,0.0549276403535255,
11.780184802912));
#14506=CARTESIAN_POINT('Ctrl Pts',(-4.2998985866006,0.0640783966010583,
11.7953338759064));
#14507=CARTESIAN_POINT('Ctrl Pts',(-4.29723383551483,0.0337205660463619,
11.7399663528515));
#14508=CARTESIAN_POINT('Ctrl Pts',(-4.30223892661807,0.0391552689494062,
11.7577758392426));
#14509=CARTESIAN_POINT('Ctrl Pts',(-4.30655480288613,0.0454981284300141,
11.7748811862141));
#14510=CARTESIAN_POINT('Ctrl Pts',(-4.3097492473298,0.0521509621179001,
11.7907366681496));
#14511=CARTESIAN_POINT('Ctrl Pts',(-4.31216328890714,0.0280798242089688,
11.7292060775775));
#14512=CARTESIAN_POINT('Ctrl Pts',(-4.31962072705201,0.0310704426480294,
11.7457834264563));
#14513=CARTESIAN_POINT('Ctrl Pts',(-4.32641873804203,0.0341585077796439,
11.7622236442056));
#14514=CARTESIAN_POINT('Ctrl Pts',(-4.33187469076345,0.0371197035570584,
11.7782343306969));
#14515=CARTESIAN_POINT('Ctrl Pts',(-4.32692885226188,0.0290568403338177,
11.7171552346107));
#14516=CARTESIAN_POINT('Ctrl Pts',(-4.3370622021989,0.0317709139581999,
11.7318804084193));
#14517=CARTESIAN_POINT('Ctrl Pts',(-4.34688041119116,0.0344079488305172,
11.7466859910022));
#14518=CARTESIAN_POINT('Ctrl Pts',(-4.35575691289273,0.0367812958992088,
11.7617986618842));
#14519=CARTESIAN_POINT('Ctrl Pts',(-4.33293714047413,0.0306667563081824,
11.7119910933921));
#14520=CARTESIAN_POINT('Ctrl Pts',(-4.34410968865593,0.0336604315708949,
11.7259232172676));
#14521=CARTESIAN_POINT('Ctrl Pts',(-4.35509026165876,0.0366026672394349,
11.7400274737341));
#14522=CARTESIAN_POINT('Ctrl Pts',(-4.36526624577325,0.0393293139651038,
11.7547577775405));
#14523=CARTESIAN_POINT('',(-4.29989857489109,0.0640783949723723,11.7953338609094));
#14524=CARTESIAN_POINT('Origin',(-4.34456072216505,0.116603380068228,11.7547577775405));
#14525=CARTESIAN_POINT('Ctrl Pts',(-4.28933737992813,0.0388717366042249,
11.7451918835388));
#14526=CARTESIAN_POINT('Ctrl Pts',(-4.2909926879354,0.0419078436176716,
11.7526417353203));
#14527=CARTESIAN_POINT('Ctrl Pts',(-4.2925597985808,0.045175191270237,11.7599143873744));
#14528=CARTESIAN_POINT('Ctrl Pts',(-4.29404906906754,0.048603587745722,
11.7669287724202));
#14529=CARTESIAN_POINT('Ctrl Pts',(-4.29544178305482,0.0518097049472987,
11.773488381472));
#14530=CARTESIAN_POINT('Ctrl Pts',(-4.29676629412499,0.055156301714286,
11.7798217675776));
#14531=CARTESIAN_POINT('Ctrl Pts',(-4.29801615211051,0.0585984518134254,
11.7859058819922));
#14532=CARTESIAN_POINT('Ctrl Pts',(-4.29854849608121,0.0600645446597914,
11.7884972497021));
#14533=CARTESIAN_POINT('Ctrl Pts',(-4.29906711701482,0.061548155517918,
11.791043982633));
#14534=CARTESIAN_POINT('Ctrl Pts',(-4.2995707431049,0.0630465295669297,
11.7935470041674));
#14535=CARTESIAN_POINT('Ctrl Pts',(-4.29968948856959,0.0633998177031627,
11.7941371690954));
#14536=CARTESIAN_POINT('Ctrl Pts',(-4.29980739879513,0.0637539277173913,
11.794724911699));
#14537=CARTESIAN_POINT('Ctrl Pts',(-4.29992448656911,0.0641087544296572,
11.7953102793706));
#14538=CARTESIAN_POINT('Origin',(-4.34456072216505,0.116603380068228,11.7547577775405));
#14539=CARTESIAN_POINT('Origin',(-4.34456072216505,0.116603380068228,11.7547577775405));
#14540=CARTESIAN_POINT('Ctrl Pts',(-4.2998985866006,0.064078396601051,11.7953338759064));
#14541=CARTESIAN_POINT('Ctrl Pts',(-4.29821195997181,0.0679078725578545,
11.7984345883761));
#14542=CARTESIAN_POINT('Ctrl Pts',(-4.29531934379238,0.0747519942657476,
11.8037156359142));
#14543=CARTESIAN_POINT('Ctrl Pts',(-4.2912761668828,0.0857111829491446,
11.8105333018319));
#14544=CARTESIAN_POINT('Ctrl Pts',(-4.28845382290292,0.0942165736780995,
11.8148613164417));
#14545=CARTESIAN_POINT('Ctrl Pts',(-4.2864128668125,0.100856657618271,11.8176056635397));
#14546=CARTESIAN_POINT('Ctrl Pts',(-4.28514086404414,0.105200715903957,
11.8191332343535));
#14547=CARTESIAN_POINT('Ctrl Pts',(-4.28411650287131,0.108864535984662,
11.8201045080524));
#14548=CARTESIAN_POINT('Ctrl Pts',(-4.30795938649042,0.0651995776992974,
11.8056577506247));
#14549=CARTESIAN_POINT('Ctrl Pts',(-4.30631269428566,0.0692259606646627,
11.8084959096106));
#14550=CARTESIAN_POINT('Ctrl Pts',(-4.30347431591841,0.0763856825373679,
11.8133201493039));
#14551=CARTESIAN_POINT('Ctrl Pts',(-4.29949162445147,0.0876978144383768,
11.8194950118656));
#14552=CARTESIAN_POINT('Ctrl Pts',(-4.29671134521685,0.096384223729235,
11.8233849066295));
#14553=CARTESIAN_POINT('Ctrl Pts',(-4.29470323588274,0.103112943879637,
11.8258358009157));
#14554=CARTESIAN_POINT('Ctrl Pts',(-4.29345297485791,0.107492911285536,
11.8271931981825));
#14555=CARTESIAN_POINT('Ctrl Pts',(-4.29244646900149,0.111166126951951,
11.8280516647877));
#14556=CARTESIAN_POINT('Ctrl Pts',(-4.32773770108309,0.071786906985305,
11.8228894198173));
#14557=CARTESIAN_POINT('Ctrl Pts',(-4.32604509607268,0.0760054220053826,
11.8251425773725));
#14558=CARTESIAN_POINT('Ctrl Pts',(-4.32313045108372,0.0834482477498973,
11.8289613255584));
#14559=CARTESIAN_POINT('Ctrl Pts',(-4.31908434704812,0.0948720157954402,
11.8337366208354));
#14560=CARTESIAN_POINT('Ctrl Pts',(-4.31631218946471,0.103451916842004,
11.8366810362039));
#14561=CARTESIAN_POINT('Ctrl Pts',(-4.31434777281709,0.109977688871195,
11.8385003202736));
#14562=CARTESIAN_POINT('Ctrl Pts',(-4.31314270025451,0.114174994801066,
11.8394921390526));
#14563=CARTESIAN_POINT('Ctrl Pts',(-4.31219079724573,0.11764156937273,11.8401081161105));
#14564=CARTESIAN_POINT('Ctrl Pts',(-4.36711540513978,0.0957581984702657,
11.8342768900003));
#14565=CARTESIAN_POINT('Ctrl Pts',(-4.36512365334321,0.0996049620227929,
11.8357058653262));
#14566=CARTESIAN_POINT('Ctrl Pts',(-4.36174755499454,0.106299259541304,
11.838076628538));
#14567=CARTESIAN_POINT('Ctrl Pts',(-4.35740902944085,0.115985641359757,
11.8408395466436));
#14568=CARTESIAN_POINT('Ctrl Pts',(-4.35465467492231,0.122890231767463,
11.8424013451887));
#14569=CARTESIAN_POINT('Ctrl Pts',(-4.35285551426538,0.127878032137172,
11.8432892482311));
#14570=CARTESIAN_POINT('Ctrl Pts',(-4.35182072520549,0.130969600301793,
11.8437365863237));
#14571=CARTESIAN_POINT('Ctrl Pts',(-4.35107864844448,0.133383930697635,
11.8439884456233));
#14572=CARTESIAN_POINT('Ctrl Pts',(-4.39089217151298,0.118900218345273,
11.8228529842754));
#14573=CARTESIAN_POINT('Ctrl Pts',(-4.38876480488994,0.122050896380848,
11.8241142878602));
#14574=CARTESIAN_POINT('Ctrl Pts',(-4.3852578467149,0.127458307394871,11.8261928035957));
#14575=CARTESIAN_POINT('Ctrl Pts',(-4.38105329091733,0.134756486516246,
11.8283977830178));
#14576=CARTESIAN_POINT('Ctrl Pts',(-4.37861013558601,0.139584989063466,
11.8295332346106));
#14577=CARTESIAN_POINT('Ctrl Pts',(-4.37716840812328,0.142775051211099,
11.8301075639033));
#14578=CARTESIAN_POINT('Ctrl Pts',(-4.37641616631218,0.144611204644327,
11.8303632616803));
#14579=CARTESIAN_POINT('Ctrl Pts',(-4.37596057093255,0.14586216270989,11.830479908078));
#14580=CARTESIAN_POINT('Ctrl Pts',(-4.39990749973883,0.131433504422785,
11.8105861003151));
#14581=CARTESIAN_POINT('Ctrl Pts',(-4.3978421585968,0.134197554896133,11.8118993900741));
#14582=CARTESIAN_POINT('Ctrl Pts',(-4.39446005348131,0.138892971386962,
11.8140046108773));
#14583=CARTESIAN_POINT('Ctrl Pts',(-4.39064941066155,0.144825508674648,
11.8162052857216));
#14584=CARTESIAN_POINT('Ctrl Pts',(-4.38858693511445,0.14845239833212,11.817285750215));
#14585=CARTESIAN_POINT('Ctrl Pts',(-4.38748854871073,0.150590557851844,
11.8178062692381));
#14586=CARTESIAN_POINT('Ctrl Pts',(-4.3869775568074,0.151688294341147,11.8180210706515));
#14587=CARTESIAN_POINT('Ctrl Pts',(-4.38674149675009,0.152249769834917,
11.8181058720862));
#14588=CARTESIAN_POINT('',(-4.2841165028712,0.108864535984968,11.8201045080524));
#14589=CARTESIAN_POINT('Ctrl Pts',(-4.2998985866006,0.064078396601051,11.7953338759064));
#14590=CARTESIAN_POINT('Ctrl Pts',(-4.29821195997181,0.0679078725578545,
11.7984345883761));
#14591=CARTESIAN_POINT('Ctrl Pts',(-4.29531934379238,0.0747519942657476,
11.8037156359142));
#14592=CARTESIAN_POINT('Ctrl Pts',(-4.2912761668828,0.0857111829491446,
11.8105333018319));
#14593=CARTESIAN_POINT('Ctrl Pts',(-4.28845382290292,0.0942165736780995,
11.8148613164417));
#14594=CARTESIAN_POINT('Ctrl Pts',(-4.2864128668125,0.100856657618271,11.8176056635397));
#14595=CARTESIAN_POINT('Ctrl Pts',(-4.28514086404414,0.105200715903957,
11.8191332343535));
#14596=CARTESIAN_POINT('Ctrl Pts',(-4.28411650287131,0.108864535984662,
11.8201045080524));
#14597=CARTESIAN_POINT('Origin',(-4.33141800137305,0.137425883926612,11.7622528214458));
#14598=CARTESIAN_POINT('Ctrl Pts',(-4.3311987144153,-0.00670693054967494,
11.638842338191));
#14599=CARTESIAN_POINT('Ctrl Pts',(-4.32865175517181,-0.00423844336129769,
11.6757969496053));
#14600=CARTESIAN_POINT('Ctrl Pts',(-4.32053855991217,0.0128128759699999,
11.7357728410368));
#14601=CARTESIAN_POINT('Ctrl Pts',(-4.30180491658975,0.060867221367586,
11.7992439240354));
#14602=CARTESIAN_POINT('Ctrl Pts',(-4.28926759889689,0.0944043425441492,
11.8171772285701));
#14603=CARTESIAN_POINT('Ctrl Pts',(-4.28411650287131,0.108864535984677,
11.8201045080524));
#14604=CARTESIAN_POINT('Ctrl Pts',(-4.32340379388905,0.000847827738124409,
11.638842338191));
#14605=CARTESIAN_POINT('Ctrl Pts',(-4.31988349734736,0.00359272330750201,
11.6744199079636));
#14606=CARTESIAN_POINT('Ctrl Pts',(-4.31012377341186,0.0204532503036035,
11.7318681580362));
#14607=CARTESIAN_POINT('Ctrl Pts',(-4.28935754019246,0.0661213671384488,
11.7913563224866));
#14608=CARTESIAN_POINT('Ctrl Pts',(-4.2761201452253,0.096359272667129,11.8069169849178));
#14609=CARTESIAN_POINT('Ctrl Pts',(-4.27107064996794,0.108365776698791,
11.8091915396309));
#14610=CARTESIAN_POINT('Ctrl Pts',(-4.30157877347568,0.0147332594892646,
11.638842338191));
#14611=CARTESIAN_POINT('Ctrl Pts',(-4.2953386362925,0.0173336386664227,
11.6716031387927));
#14612=CARTESIAN_POINT('Ctrl Pts',(-4.28103898314758,0.0323127313395658,
11.724213122074));
#14613=CARTESIAN_POINT('Ctrl Pts',(-4.25429940326487,0.0709362647361591,
11.7778555072083));
#14614=CARTESIAN_POINT('Ctrl Pts',(-4.23840934345728,0.0944555394156121,
11.7911968100006));
#14615=CARTESIAN_POINT('Ctrl Pts',(-4.23285157171247,0.102524661495376,
11.7931703698428));
#14616=CARTESIAN_POINT('Ctrl Pts',(-4.27543328147234,0.0171451713454814,
11.638842338191));
#14617=CARTESIAN_POINT('Ctrl Pts',(-4.26664745710568,0.0173596858998116,
11.670251961572));
#14618=CARTESIAN_POINT('Ctrl Pts',(-4.2487117108702,0.0266051976481541,
11.722201613145));
#14619=CARTESIAN_POINT('Ctrl Pts',(-4.2184725963509,0.0562721118852402,
11.7810985911187));
#14620=CARTESIAN_POINT('Ctrl Pts',(-4.20102503055697,0.0781925592767865,
11.8019661605246));
#14621=CARTESIAN_POINT('Ctrl Pts',(-4.19434863166431,0.0884303231042628,
11.8069260082108));
#14622=CARTESIAN_POINT('Ctrl Pts',(-4.26119373042795,0.0145528918841497,
11.638842338191));
#14623=CARTESIAN_POINT('Ctrl Pts',(-4.2515576859341,0.0127986708309713,
11.670082443596));
#14624=CARTESIAN_POINT('Ctrl Pts',(-4.23284451070938,0.0179955453015912,
11.7229716250566));
#14625=CARTESIAN_POINT('Ctrl Pts',(-4.20334790059126,0.0435290176544484,
11.7880179360481));
#14626=CARTESIAN_POINT('Ctrl Pts',(-4.18652333699586,0.0670043771977565,
11.8149459781635));
#14627=CARTESIAN_POINT('Ctrl Pts',(-4.17955578083775,0.0803031880431222,
11.8220868710498));
#14628=CARTESIAN_POINT('',(-4.17955578083768,0.080303188043321,11.8220868710499));
#14629=CARTESIAN_POINT('Ctrl Pts',(-4.26119373042795,0.0145528918841497,
11.638842338191));
#14630=CARTESIAN_POINT('Ctrl Pts',(-4.2515576859341,0.0127986708309713,
11.670082443596));
#14631=CARTESIAN_POINT('Ctrl Pts',(-4.23284451070938,0.0179955453015912,
11.7229716250566));
#14632=CARTESIAN_POINT('Ctrl Pts',(-4.20334819884833,0.0435287594709281,
11.7880172783277));
#14633=CARTESIAN_POINT('Ctrl Pts',(-4.18652393242557,0.0670035463958563,
11.8149450251635));
#14634=CARTESIAN_POINT('Ctrl Pts',(-4.17955652059904,0.0803017760943429,
11.8220861128668));
#14635=CARTESIAN_POINT('Origin',(-4.2368150043693,0.0803031880435051,11.8779561946592));
#14636=CARTESIAN_POINT('Ctrl Pts',(-4.25298213616247,0.198467231410946,
11.8394929583522));
#14637=CARTESIAN_POINT('Ctrl Pts',(-4.2286257884895,0.267808752164977,11.8547475451914));
#14638=CARTESIAN_POINT('Ctrl Pts',(-4.20375550827876,0.336898704931691,
11.8704997107853));
#14639=CARTESIAN_POINT('Ctrl Pts',(-4.17831101056731,0.405641108349178,
11.8866997463764));
#14640=CARTESIAN_POINT('Ctrl Pts',(-4.26764395882653,0.202972445897108,
11.8508559827845));
#14641=CARTESIAN_POINT('Ctrl Pts',(-4.24322404174216,0.272657752950044,
11.8641477704669));
#14642=CARTESIAN_POINT('Ctrl Pts',(-4.21791862804,0.341979351501413,11.8780814874676));
#14643=CARTESIAN_POINT('Ctrl Pts',(-4.19175410711448,0.410851995456146,
11.892562174259));
#14644=CARTESIAN_POINT('Ctrl Pts',(-4.30407807870002,0.216966069077792,
11.862230432717));
#14645=CARTESIAN_POINT('Ctrl Pts',(-4.27759840717805,0.286590344056463,
11.8724273890985));
#14646=CARTESIAN_POINT('Ctrl Pts',(-4.24997131879908,0.355728405406215,
11.8835722239453));
#14647=CARTESIAN_POINT('Ctrl Pts',(-4.22116750718431,0.424212414426285,
11.8957681405415));
#14648=CARTESIAN_POINT('Ctrl Pts',(-4.3369990180675,0.234073734275867,11.8456124354964));
#14649=CARTESIAN_POINT('Ctrl Pts',(-4.3077197084613,0.303022130841672,11.8562178951535));
#14650=CARTESIAN_POINT('Ctrl Pts',(-4.27744040849402,0.371404354559313,
11.8680190687516));
#14651=CARTESIAN_POINT('Ctrl Pts',(-4.24596884413302,0.439041104136474,
11.8809722029021));
#14652=CARTESIAN_POINT('Ctrl Pts',(-4.34855965130146,0.24132741635741,11.8322680295746));
#14653=CARTESIAN_POINT('Ctrl Pts',(-4.31851137785818,0.310100961669604,
11.8437509230397));
#14654=CARTESIAN_POINT('Ctrl Pts',(-4.28743292633124,0.378248514869065,
11.8563834756258));
#14655=CARTESIAN_POINT('Ctrl Pts',(-4.25516769303209,0.445602794179394,
11.8702702241066));
#14656=CARTESIAN_POINT('',(-4.17831869257478,0.405606437847502,11.8867128997031));
#14657=CARTESIAN_POINT('Origin',(-4.20023746323962,0.430852097115001,11.8140111108424));
#14658=CARTESIAN_POINT('',(-4.25297464465416,0.19849748388496,11.8395016149463));
#14659=CARTESIAN_POINT('Origin',(-4.29328772795413,0.226549903216342,11.7763516578244));
#14660=CARTESIAN_POINT('Ctrl Pts',(-4.25297464465415,0.198497483885009,
11.8395016149464));
#14661=CARTESIAN_POINT('Ctrl Pts',(-4.23691634103563,0.244214515550849,
11.8495588444424));
#14662=CARTESIAN_POINT('Ctrl Pts',(-4.22062846601348,0.289815884959662,
11.859850949835));
#14663=CARTESIAN_POINT('Ctrl Pts',(-4.20410226715093,0.335282633479534,
11.8703374283436));
#14664=CARTESIAN_POINT('Ctrl Pts',(-4.19556935771983,0.358758306891982,
11.8757518719255));
#14665=CARTESIAN_POINT('Ctrl Pts',(-4.18697273257692,0.382197862800513,
11.8812189300755));
#14666=CARTESIAN_POINT('Ctrl Pts',(-4.17831110315985,0.405597624417347,
11.8867383703356));
#14667=CARTESIAN_POINT('Ctrl Pts',(-4.17832438065528,0.405613001090449,
11.8866940169724));
#14668=CARTESIAN_POINT('Ctrl Pts',(-4.17353003744589,0.418565725487248,
11.8897464020236));
#14669=CARTESIAN_POINT('Ctrl Pts',(-4.16871489377343,0.431505611461712,
11.8928150545396));
#14670=CARTESIAN_POINT('Ctrl Pts',(-4.16387784115802,0.444431102132758,
11.8959002913408));
#14671=CARTESIAN_POINT('Ctrl Pts',(-4.19176708001533,0.410823686905363,
11.8925562479089));
#14672=CARTESIAN_POINT('Ctrl Pts',(-4.18683712032951,0.423800954990201,
11.8952847659635));
#14673=CARTESIAN_POINT('Ctrl Pts',(-4.18187186452005,0.436758289002851,
11.898043001497));
#14674=CARTESIAN_POINT('Ctrl Pts',(-4.17687624823759,0.449699275767736,
11.9008161302017));
#14675=CARTESIAN_POINT('Ctrl Pts',(-4.22117628298598,0.424185231737969,
11.8957460251486));
#14676=CARTESIAN_POINT('Ctrl Pts',(-4.21574899813179,0.43708928465133,11.8980438924075));
#14677=CARTESIAN_POINT('Ctrl Pts',(-4.21027895401589,0.449969857826206,
11.9003772371141));
#14678=CARTESIAN_POINT('Ctrl Pts',(-4.20476498303276,0.462824517622096,
11.9027501529791));
#14679=CARTESIAN_POINT('Ctrl Pts',(-4.2459821724517,0.439012459536339,11.8809667172436));
#14680=CARTESIAN_POINT('Ctrl Pts',(-4.24005221860176,0.451756844238467,
11.883407410326));
#14681=CARTESIAN_POINT('Ctrl Pts',(-4.23408529886524,0.464475341488486,
11.8858987952752));
#14682=CARTESIAN_POINT('Ctrl Pts',(-4.22806909913246,0.477163666032771,
11.8884288073028));
#14683=CARTESIAN_POINT('Ctrl Pts',(-4.2551813574745,0.445574269204196,11.8702643430631));
#14684=CARTESIAN_POINT('Ctrl Pts',(-4.24910188448058,0.45826545703258,11.8728808695122));
#14685=CARTESIAN_POINT('Ctrl Pts',(-4.24297931347368,0.47092779002261,11.8755428064202));
#14686=CARTESIAN_POINT('Ctrl Pts',(-4.2368109319615,0.483558887244307,11.8782524024265));
#14687=CARTESIAN_POINT('',(-4.16387023623629,0.44442096356818,11.8959309387847));
#14688=CARTESIAN_POINT('Origin',(-4.18196216438191,0.468862204265513,11.821899760923));
#14689=CARTESIAN_POINT('Ctrl Pts',(-4.17832438065528,0.405613001090449,
11.8866940169724));
#14690=CARTESIAN_POINT('Ctrl Pts',(-4.17353003744589,0.418565725487248,
11.8897464020236));
#14691=CARTESIAN_POINT('Ctrl Pts',(-4.16871489377343,0.431505611461712,
11.8928150545396));
#14692=CARTESIAN_POINT('Ctrl Pts',(-4.16387784115802,0.444431102132758,
11.8959002913408));
#14693=CARTESIAN_POINT('Ctrl Pts',(-4.28411650287118,0.108864535985058,
11.8201045080525));
#14694=CARTESIAN_POINT('Ctrl Pts',(-4.27383348446592,0.138789589880342,
11.8264707476279));
#14695=CARTESIAN_POINT('Ctrl Pts',(-4.26345245300614,0.168667789068198,
11.8329394197285));
#14696=CARTESIAN_POINT('Ctrl Pts',(-4.25297464465416,0.198497483884985,
11.8395016149463));
#14697=CARTESIAN_POINT('Ctrl Pts',(-4.30077643513154,0.113467717919639,
11.835998821523));
#14698=CARTESIAN_POINT('Ctrl Pts',(-4.29061215932074,0.143598492746439,
11.841360239256));
#14699=CARTESIAN_POINT('Ctrl Pts',(-4.28023908095909,0.173646869395274,
11.8468941305194));
#14700=CARTESIAN_POINT('Ctrl Pts',(-4.26973042744931,0.203646502026694,
11.8524853083802));
#14701=CARTESIAN_POINT('Ctrl Pts',(-4.34104542870178,0.128332090592554,
11.8495698235112));
#14702=CARTESIAN_POINT('Ctrl Pts',(-4.32996580556451,0.158437379738818,
11.8535197351198));
#14703=CARTESIAN_POINT('Ctrl Pts',(-4.31867086063058,0.18845912219569,11.8576528974894));
#14704=CARTESIAN_POINT('Ctrl Pts',(-4.30715498164588,0.218382296444562,
11.8619899386228));
#14705=CARTESIAN_POINT('Ctrl Pts',(-4.37596057093238,0.145862162710285,
11.8304799080781));
#14706=CARTESIAN_POINT('Ctrl Pts',(-4.36371043865105,0.175725323285883,
11.8346706366403));
#14707=CARTESIAN_POINT('Ctrl Pts',(-4.35128087581798,0.20549030245879,11.8390867979876));
#14708=CARTESIAN_POINT('Ctrl Pts',(-4.33863808356346,0.235139180415304,
11.8437106389784));
#14709=CARTESIAN_POINT('Ctrl Pts',(-4.38674149674992,0.152249769835312,
11.8181058720863));
#14710=CARTESIAN_POINT('Ctrl Pts',(-4.37420531076058,0.182067441230975,
11.8226093301053));
#14711=CARTESIAN_POINT('Ctrl Pts',(-4.36147336656485,0.211771272545564,
11.8273329847674));
#14712=CARTESIAN_POINT('Ctrl Pts',(-4.34854691846783,0.241356558688859,
11.8322728954492));
#14713=CARTESIAN_POINT('Origin',(2.32049299786841,-3.62262617981002,18.6886752212914));
#14714=CARTESIAN_POINT('Ctrl Pts',(-4.16387784115802,0.444431102132757,
11.8959002913408));
#14715=CARTESIAN_POINT('Ctrl Pts',(-4.15828181192265,0.459384717366581,
11.8994696292642));
#14716=CARTESIAN_POINT('Ctrl Pts',(-4.15265646004605,0.474319169743533,
11.9030611537802));
#14717=CARTESIAN_POINT('Ctrl Pts',(-4.14699952201194,0.489230927920841,
11.90667591896));
#14718=CARTESIAN_POINT('Ctrl Pts',(-4.17687624823759,0.449699275767735,
11.9008161302017));
#14719=CARTESIAN_POINT('Ctrl Pts',(-4.17109677528411,0.464670818570484,
11.9040243874894));
#14720=CARTESIAN_POINT('Ctrl Pts',(-4.16526996333276,0.47961431758977,11.9072712243025));
#14721=CARTESIAN_POINT('Ctrl Pts',(-4.15939846344752,0.49453108177116,11.9105424838858));
#14722=CARTESIAN_POINT('Ctrl Pts',(-4.20476498083012,0.462824518205306,
11.9027501451694));
#14723=CARTESIAN_POINT('Ctrl Pts',(-4.19838581870849,0.477696188569049,
11.9054953926599));
#14724=CARTESIAN_POINT('Ctrl Pts',(-4.19194742237,0.492533642599708,11.9082903960795));
#14725=CARTESIAN_POINT('Ctrl Pts',(-4.18544686834643,0.507332016553614,
11.9111411005044));
#14726=CARTESIAN_POINT('Ctrl Pts',(-4.22806909913247,0.477163666032769,
11.8884288073027));
#14727=CARTESIAN_POINT('Ctrl Pts',(-4.221108904099,0.491842901663036,11.8913558007423));
#14728=CARTESIAN_POINT('Ctrl Pts',(-4.21409456216484,0.506484223480552,
11.8943508066784));
#14729=CARTESIAN_POINT('Ctrl Pts',(-4.20701096015312,0.521080619220583,
11.8974040141978));
#14730=CARTESIAN_POINT('Ctrl Pts',(-4.23681093196151,0.483558887244306,
11.8782524024265));
#14731=CARTESIAN_POINT('Ctrl Pts',(-4.22967467647256,0.498171916075573,
11.8813871581699));
#14732=CARTESIAN_POINT('Ctrl Pts',(-4.22247713691368,0.512743255380418,
11.8845856560674));
#14733=CARTESIAN_POINT('Ctrl Pts',(-4.21521271352384,0.527267762951524,
11.8878527735462));
#14734=CARTESIAN_POINT('Ctrl Pts',(-4.16386860738941,0.444418764937274,
11.8959375572369));
#14735=CARTESIAN_POINT('Ctrl Pts',(-4.16391834371126,0.4445411940699,11.8959904740987));
#14736=CARTESIAN_POINT('Ctrl Pts',(-4.163968157019,0.444663693166018,11.8960431989357));
#14737=CARTESIAN_POINT('Ctrl Pts',(-4.16401805752376,0.444786241611601,
11.8960957271683));
#14738=CARTESIAN_POINT('Ctrl Pts',(-4.16561890128454,0.448717683096392,
11.8977808703098));
#14739=CARTESIAN_POINT('Ctrl Pts',(-4.16724284026456,0.452546011395253,
11.899195612021));
#14740=CARTESIAN_POINT('Ctrl Pts',(-4.16886553453554,0.456301479369417,
11.9004052791275));
#14741=CARTESIAN_POINT('Ctrl Pts',(-4.16924869277134,0.457188238205828,
11.9006909114384));
#14742=CARTESIAN_POINT('Ctrl Pts',(-4.16963159810811,0.458070820883551,
11.9009650379668));
#14743=CARTESIAN_POINT('Ctrl Pts',(-4.17001364086649,0.45894930734541,11.9012282802084));
#14744=CARTESIAN_POINT('Ctrl Pts',(-4.17055703829997,0.460198820072074,
11.9016027020638));
#14745=CARTESIAN_POINT('Ctrl Pts',(-4.17109864146052,0.461440173594932,
11.9019550639622));
#14746=CARTESIAN_POINT('Ctrl Pts',(-4.17163327228824,0.46268105659674,11.9022825344791));
#14747=CARTESIAN_POINT('Ctrl Pts',(-4.17269401152293,0.465143041984486,
11.9029322553846));
#14748=CARTESIAN_POINT('Ctrl Pts',(-4.17374475353427,0.467580949994859,
11.9034907549559));
#14749=CARTESIAN_POINT('Ctrl Pts',(-4.17476688820595,0.4700231092791,11.9039700966035));
#14750=CARTESIAN_POINT('Ctrl Pts',(-4.17534733062492,0.471409944968901,
11.9042423016594));
#14751=CARTESIAN_POINT('Ctrl Pts',(-4.17591872561242,0.472797307639367,
11.9044893141433));
#14752=CARTESIAN_POINT('Ctrl Pts',(-4.17647934282577,0.474183601581782,
11.9047162802904));
#14753=CARTESIAN_POINT('Ctrl Pts',(-4.17651181682008,0.47426390325737,11.9047294274025));
#14754=CARTESIAN_POINT('Ctrl Pts',(-4.17654425502559,0.474344199989393,
11.9047425078853));
#14755=CARTESIAN_POINT('Ctrl Pts',(-4.17657665727905,0.474424489992879,
11.9047555221994));
#14756=CARTESIAN_POINT('Ctrl Pts',(-4.17794092023881,0.47780501653376,11.9053034762694));
#14757=CARTESIAN_POINT('Ctrl Pts',(-4.17923643699538,0.48119604508226,11.9057257123795));
#14758=CARTESIAN_POINT('Ctrl Pts',(-4.18044332363875,0.484607579902023,
11.9060319457311));
#14759=CARTESIAN_POINT('Ctrl Pts',(-4.18153051926195,0.487680781303985,
11.9063078088881));
#14760=CARTESIAN_POINT('Ctrl Pts',(-4.1825475622151,0.490770285934714,11.9064918264379));
#14761=CARTESIAN_POINT('Ctrl Pts',(-4.18349249663733,0.493896424319563,
11.9066042613417));
#14762=CARTESIAN_POINT('Ctrl Pts',(-4.18440502081064,0.496915339471953,
11.9067128398475));
#14763=CARTESIAN_POINT('Ctrl Pts',(-4.18524674175396,0.499965615042457,
11.9067514773718));
#14764=CARTESIAN_POINT('Ctrl Pts',(-4.18601047565315,0.503059942136878,
11.9067297730278));
#14765=CARTESIAN_POINT('Ctrl Pts',(-4.18604651909286,0.503205974926828,
11.9067287487192));
#14766=CARTESIAN_POINT('Ctrl Pts',(-4.18608238856455,0.503352107249628,
11.9067275884811));
#14767=CARTESIAN_POINT('Ctrl Pts',(-4.18611808342164,0.50349833985629,11.9067262938402));
#14768=CARTESIAN_POINT('Ctrl Pts',(-4.18637628476887,0.504556124062116,
11.9067169289611));
#14769=CARTESIAN_POINT('Ctrl Pts',(-4.1866253519351,0.505619124128795,11.9067005504272));
#14770=CARTESIAN_POINT('Ctrl Pts',(-4.18686494960606,0.506687549510347,
11.9066776046077));
#14771=CARTESIAN_POINT('Ctrl Pts',(-4.18706148986136,0.507563971206857,
11.9066587823162));
#14772=CARTESIAN_POINT('Ctrl Pts',(-4.18725052829967,0.508439469984838,
11.9066356211609));
#14773=CARTESIAN_POINT('Ctrl Pts',(-4.1874280189678,0.50930672791011,11.9066032159468));
#14774=CARTESIAN_POINT('Ctrl Pts',(-4.28411650287119,0.108864535985059,
11.8201045080525));
#14775=CARTESIAN_POINT('Ctrl Pts',(-4.27608425813253,0.138890274178381,
11.8283607642014));
#14776=CARTESIAN_POINT('Ctrl Pts',(-4.26805801086052,0.168913049189128,
11.8366050116627));
#14777=CARTESIAN_POINT('Ctrl Pts',(-4.26003736024089,0.198935548997806,
11.8448257475953));
#14778=CARTESIAN_POINT('Ctrl Pts',(-4.26672203233337,0.10819952360388,11.8055538834905));
#14779=CARTESIAN_POINT('Ctrl Pts',(-4.25869817607788,0.138222655883494,
11.8138093209203));
#14780=CARTESIAN_POINT('Ctrl Pts',(-4.25068357204439,0.168242310003863,
11.8220515500891));
#14781=CARTESIAN_POINT('Ctrl Pts',(-4.2426781599081,0.198260104377667,11.8302708366033));
#14782=CARTESIAN_POINT('Ctrl Pts',(-4.22594174945398,0.1006372010266,11.793301386559));
#14783=CARTESIAN_POINT('Ctrl Pts',(-4.21793377436576,0.130663341317267,
11.8015463165459));
#14784=CARTESIAN_POINT('Ctrl Pts',(-4.20994143979378,0.160686561995819,
11.8097749635335));
#14785=CARTESIAN_POINT('Ctrl Pts',(-4.20196492133035,0.190709798308366,
11.8179752139256));
#14786=CARTESIAN_POINT('Ctrl Pts',(-4.19065041895756,0.0863985393393625,
11.8107162239207));
#14787=CARTESIAN_POINT('Ctrl Pts',(-4.18264086798039,0.116436218388614,
11.8189393524712));
#14788=CARTESIAN_POINT('Ctrl Pts',(-4.17464603081676,0.146475576888081,
11.8271373943832));
#14789=CARTESIAN_POINT('Ctrl Pts',(-4.16666679209685,0.176519661076779,
11.8352979905427));
#14790=CARTESIAN_POINT('Ctrl Pts',(-4.17955578083765,0.0803031880435048,
11.8220868710499));
#14791=CARTESIAN_POINT('Ctrl Pts',(-4.1715408983818,0.110345789757979,11.8303011452969));
#14792=CARTESIAN_POINT('Ctrl Pts',(-4.1635389344325,0.140392086225485,11.8384867715752));
#14793=CARTESIAN_POINT('Ctrl Pts',(-4.15555007706065,0.170445064553628,
11.8466312332458));
#14794=CARTESIAN_POINT('',(-4.15555007706065,0.170445064553628,11.8466312332458));
#14795=CARTESIAN_POINT('Origin',(-16.9242493907379,13.7717485420172,-25.8067217625208));
#14796=CARTESIAN_POINT('Origin',(-4.21266156135419,0.170445064553628,11.9026515720683));
#14797=CARTESIAN_POINT('Origin',(-4.1,0.9,6.5));
#14798=CARTESIAN_POINT('',(-4.10062628980501,2.179093092077E-7,3.09201395474528));
#14799=CARTESIAN_POINT('Ctrl Pts',(-4.10062628985477,2.17910570921021E-7,
3.09201395473902));
#14800=CARTESIAN_POINT('Ctrl Pts',(-4.10946509570597,6.36863920784053E-6,
3.16223612469626));
#14801=CARTESIAN_POINT('Ctrl Pts',(-4.11980376888638,8.0145983837535E-5,
3.23266996300447));
#14802=CARTESIAN_POINT('Ctrl Pts',(-4.13221833032745,0.000519669739900586,
3.30274456732768));
#14803=CARTESIAN_POINT('Ctrl Pts',(-4.1427684836723,0.000893186198551402,
3.36229542820175));
#14804=CARTESIAN_POINT('Ctrl Pts',(-4.15482146373736,0.00153084307074809,
3.42158490272002));
#14805=CARTESIAN_POINT('Ctrl Pts',(-4.16871245653638,0.0026156074478858,
3.480242356807));
#14806=CARTESIAN_POINT('Ctrl Pts',(-4.17290633342143,0.00294311235072616,
3.49795182828901));
#14807=CARTESIAN_POINT('Ctrl Pts',(-4.17726742698064,0.0033113718635993,
3.51560363027309));
#14808=CARTESIAN_POINT('Ctrl Pts',(-4.18180390848863,0.0037254212262936,
3.53318749645313));
#14809=CARTESIAN_POINT('Ctrl Pts',(-4.19639560025769,0.00505722003710435,
3.58974638574991));
#14810=CARTESIAN_POINT('Ctrl Pts',(-4.21284049567206,0.0068867784862876,
3.64574064454163));
#14811=CARTESIAN_POINT('Ctrl Pts',(-4.23143875004913,0.00963952341296004,
3.70094503351942));
#14812=CARTESIAN_POINT('Ctrl Pts',(-4.24030470587491,0.0109517817800476,
3.72726146430606));
#14813=CARTESIAN_POINT('Ctrl Pts',(-4.24965932888634,0.0124738356593051,
3.75339825043382));
#14814=CARTESIAN_POINT('Ctrl Pts',(-4.25953080556008,0.014251772749529,
3.77933080745784));
#14815=CARTESIAN_POINT('Ctrl Pts',(-4.27693923829638,0.0173871798692027,
3.82506309144671));
#14816=CARTESIAN_POINT('Ctrl Pts',(-4.29591937405777,0.0213206157856711,
3.87005702106385));
#14817=CARTESIAN_POINT('Ctrl Pts',(-4.31656055867041,0.026441281981235,
3.9141641214968));
#14818=CARTESIAN_POINT('Ctrl Pts',(-4.32190785897979,0.0277678405313199,
3.92559049630121));
#14819=CARTESIAN_POINT('Ctrl Pts',(-4.32736638333248,0.0291740764308477,
3.93695744733596));
#14820=CARTESIAN_POINT('Ctrl Pts',(-4.33293714059227,0.0306667563398393,
3.94826261099145));
#14821=CARTESIAN_POINT('',(-4.1,2.23481172803575E-17,3.08202325217327));
#14822=CARTESIAN_POINT('Origin',(-4.18002610983571,4.86909770516006E-5,
3.08202161556327));
#14823=CARTESIAN_POINT('',(-4.1,0.,11.7890187209227));
#14824=CARTESIAN_POINT('',(-4.1,0.,-0.5));
#14825=CARTESIAN_POINT('Ctrl Pts',(-4.26119373042794,0.014552891884149,
11.638842338191));
#14826=CARTESIAN_POINT('Ctrl Pts',(-4.20740273136266,0.00476035687747917,
11.6883109569019));
#14827=CARTESIAN_POINT('Ctrl Pts',(-4.15394513638752,2.66182811039857E-16,
11.7388892266742));
#14828=CARTESIAN_POINT('Ctrl Pts',(-4.1,0.,11.7890187209227));
#14829=CARTESIAN_POINT('Ctrl Pts',(-4.25297464465415,0.198497483885009,
11.8395016149464));
#14830=CARTESIAN_POINT('Ctrl Pts',(-4.23432610916137,0.268350649999046,
11.8586270490361));
#14831=CARTESIAN_POINT('Ctrl Pts',(-4.21571553863559,0.338200359108088,
11.877624289993));
#14832=CARTESIAN_POINT('Ctrl Pts',(-4.19713727273351,0.408083416458755,
11.8963406005087));
#14833=CARTESIAN_POINT('Ctrl Pts',(-4.23780121350118,0.19723139322301,11.8292529191487));
#14834=CARTESIAN_POINT('Ctrl Pts',(-4.2191816325323,0.267079242619096,11.8483714100219));
#14835=CARTESIAN_POINT('Ctrl Pts',(-4.20061568185391,0.336921901139932,
11.8673561360113));
#14836=CARTESIAN_POINT('Ctrl Pts',(-4.18209944631418,0.406793934797266,
11.886058258236));
#14837=CARTESIAN_POINT('Ctrl Pts',(-4.20089925437152,0.190087479799487,
11.8192080583286));
#14838=CARTESIAN_POINT('Ctrl Pts',(-4.1823370650831,0.259947915222703,11.8382842185072));
#14839=CARTESIAN_POINT('Ctrl Pts',(-4.16386011311889,0.329808442959132,
11.8572064988123));
#14840=CARTESIAN_POINT('Ctrl Pts',(-4.14546763523864,0.399706853583148,
11.8758191065186));
#14841=CARTESIAN_POINT('Ctrl Pts',(-4.16755381812912,0.17700436588702,11.8343936873133));
#14842=CARTESIAN_POINT('Ctrl Pts',(-4.14898961110941,0.246909238451779,
11.8533850386243));
#14843=CARTESIAN_POINT('Ctrl Pts',(-4.1305071888592,0.31683856296458,11.8721748641617));
#14844=CARTESIAN_POINT('Ctrl Pts',(-4.11211341232255,0.386829622935632,
11.8906052241705));
#14845=CARTESIAN_POINT('Ctrl Pts',(-4.15555007706064,0.170445064553676,
11.8466312332458));
#14846=CARTESIAN_POINT('Ctrl Pts',(-4.13696158210585,0.240372415866411,
11.8655817887042));
#14847=CARTESIAN_POINT('Ctrl Pts',(-4.11844401855589,0.310335983331864,
11.8843096665637));
#14848=CARTESIAN_POINT('Ctrl Pts',(-4.1,0.380373905065778,11.9026515720683));
#14849=CARTESIAN_POINT('',(-4.1,0.380373905065777,11.9026515720683));
#14850=CARTESIAN_POINT('Ctrl Pts',(-4.15555007706064,0.170445064553676,
11.8466312332458));
#14851=CARTESIAN_POINT('Ctrl Pts',(-4.13696158210585,0.240372415866411,
11.8655817887042));
#14852=CARTESIAN_POINT('Ctrl Pts',(-4.11844401855589,0.310335983331864,
11.8843096665637));
#14853=CARTESIAN_POINT('Ctrl Pts',(-4.1,0.380373905065778,11.9026515720683));
#14854=CARTESIAN_POINT('Origin',(-4.15641129807095,0.380373905065777,11.9593769231025));
#14855=CARTESIAN_POINT('Ctrl Pts',(-4.08957475120669,0.420000000000004,
11.9129846529869));
#14856=CARTESIAN_POINT('Ctrl Pts',(-4.09304720501634,0.406788497264506,
11.9095547476558));
#14857=CARTESIAN_POINT('Ctrl Pts',(-4.09652229439691,0.393579881415503,
11.90611002378));
#14858=CARTESIAN_POINT('Ctrl Pts',(-4.1,0.380373905065779,11.9026515720683));
#14859=CARTESIAN_POINT('Ctrl Pts',(-4.09935159372593,0.425175588381722,
11.9033276075325));
#14860=CARTESIAN_POINT('Ctrl Pts',(-4.10281576552394,0.411971887580064,
11.8998828402856));
#14861=CARTESIAN_POINT('Ctrl Pts',(-4.10628316887034,0.398770707124635,
11.8964240952639));
#14862=CARTESIAN_POINT('Ctrl Pts',(-4.10975331598555,0.385571833991309,
11.892952254123));
#14863=CARTESIAN_POINT('Ctrl Pts',(-4.12472484253256,0.435512908316209,
11.8899576288478));
#14864=CARTESIAN_POINT('Ctrl Pts',(-4.12818546048421,0.422324742310494,
11.886482228227));
#14865=CARTESIAN_POINT('Ctrl Pts',(-4.13164915696943,0.409138427226951,
11.8829942449745));
#14866=CARTESIAN_POINT('Ctrl Pts',(-4.13511596185361,0.395953697471928,
11.8794947521918));
#14867=CARTESIAN_POINT('Ctrl Pts',(-4.15423485006789,0.44280432443085,11.892284208906));
#14868=CARTESIAN_POINT('Ctrl Pts',(-4.15771124289688,0.429624324733392,
11.8887884960684));
#14869=CARTESIAN_POINT('Ctrl Pts',(-4.16118998038772,0.416445694643035,
11.8852813895583));
#14870=CARTESIAN_POINT('Ctrl Pts',(-4.16467098162167,0.403268395711099,
11.8817635071735));
#14871=CARTESIAN_POINT('Ctrl Pts',(-4.16786079472921,0.445145811119343,
11.8972322351616));
#14872=CARTESIAN_POINT('Ctrl Pts',(-4.1713468289151,0.43196686310669,11.8937304736977));
#14873=CARTESIAN_POINT('Ctrl Pts',(-4.17483467940513,0.418789345178509,
11.8902173887752));
#14874=CARTESIAN_POINT('Ctrl Pts',(-4.17832438065533,0.405613001090281,
11.8866940169724));
#14875=CARTESIAN_POINT('',(-4.08957475121441,0.420000000004092,11.9129846529793));
#14876=CARTESIAN_POINT('Ctrl Pts',(-4.1,0.380373905065779,11.9026515720683));
#14877=CARTESIAN_POINT('Ctrl Pts',(-4.09652229439691,0.393579881415503,
11.90611002378));
#14878=CARTESIAN_POINT('Ctrl Pts',(-4.09304720501634,0.406788497264506,
11.9095547476558));
#14879=CARTESIAN_POINT('Ctrl Pts',(-4.08957475120669,0.420000000000004,
11.9129846529869));
#14880=CARTESIAN_POINT('Origin',(-4.14579351793413,0.420000000000002,11.9699008217586));
#14881=CARTESIAN_POINT('Ctrl Pts',(-4.20389723040784,0.448082122854196,
11.9226213021674));
#14882=CARTESIAN_POINT('Ctrl Pts',(-4.20184390702141,0.454587762651284,
11.9239619770498));
#14883=CARTESIAN_POINT('Ctrl Pts',(-4.19793638990807,0.467244934591944,
11.9248776171878));
#14884=CARTESIAN_POINT('Ctrl Pts',(-4.19264636363395,0.486132237432104,
11.9213061489869));
#14885=CARTESIAN_POINT('Ctrl Pts',(-4.18798032404462,0.506067458447531,
11.9109852930588));
#14886=CARTESIAN_POINT('Ctrl Pts',(-4.18528583117895,0.519829640007596,
11.8969505489161));
#14887=CARTESIAN_POINT('Ctrl Pts',(-4.18416745800402,0.52598322777095,11.8885969417624));
#14888=CARTESIAN_POINT('Ctrl Pts',(-4.19174908380885,0.448683750825517,
11.9080492965203));
#14889=CARTESIAN_POINT('Ctrl Pts',(-4.18980989453422,0.453995201447333,
11.9090114292076));
#14890=CARTESIAN_POINT('Ctrl Pts',(-4.18629251150101,0.463929335183028,
11.9094067500189));
#14891=CARTESIAN_POINT('Ctrl Pts',(-4.18220013538096,0.477785316871903,
11.9066119377239));
#14892=CARTESIAN_POINT('Ctrl Pts',(-4.17917348866453,0.493275358206986,
11.899219888217));
#14893=CARTESIAN_POINT('Ctrl Pts',(-4.17754427524001,0.505531647607768,
11.8877547429666));
#14894=CARTESIAN_POINT('Ctrl Pts',(-4.1769096978644,0.511201122881534,11.880578516275));
#14895=CARTESIAN_POINT('Ctrl Pts',(-4.16303328561123,0.445542625831325,
11.890845536232));
#14896=CARTESIAN_POINT('Ctrl Pts',(-4.16100917724248,0.449355522427211,
11.8915365465931));
#14897=CARTESIAN_POINT('Ctrl Pts',(-4.15757466275877,0.455975296164343,
11.8916732129521));
#14898=CARTESIAN_POINT('Ctrl Pts',(-4.15465267900733,0.464139333458313,
11.8899004794177));
#14899=CARTESIAN_POINT('Ctrl Pts',(-4.15404544758576,0.474490462284283,
11.885476111969));
#14900=CARTESIAN_POINT('Ctrl Pts',(-4.15452950414342,0.48467806297157,11.8766922820171));
#14901=CARTESIAN_POINT('Ctrl Pts',(-4.15493036552924,0.489633970339022,
11.8707859261611));
#14902=CARTESIAN_POINT('Ctrl Pts',(-4.11911994815048,0.43335877848646,11.8924222558676));
#14903=CARTESIAN_POINT('Ctrl Pts',(-4.11669542890408,0.437016335410973,
11.8938247509459));
#14904=CARTESIAN_POINT('Ctrl Pts',(-4.11252036702983,0.443826518601221,
11.8952537752929));
#14905=CARTESIAN_POINT('Ctrl Pts',(-4.10893178611961,0.453405904273695,
11.89379446554));
#14906=CARTESIAN_POINT('Ctrl Pts',(-4.10901293703883,0.464398928863795,
11.8871965822423));
#14907=CARTESIAN_POINT('Ctrl Pts',(-4.11127193969944,0.473342094480854,
11.8767538807855));
#14908=CARTESIAN_POINT('Ctrl Pts',(-4.11272151139406,0.477535811726914,
11.8702935234762));
#14909=CARTESIAN_POINT('Ctrl Pts',(-4.09799980361865,0.424459988313498,
11.9046628339601));
#14910=CARTESIAN_POINT('Ctrl Pts',(-4.0953727901903,0.428957878019816,11.9068711895671));
#14911=CARTESIAN_POINT('Ctrl Pts',(-4.09066232230966,0.438065597562857,
11.9096177858811));
#14912=CARTESIAN_POINT('Ctrl Pts',(-4.08582024878189,0.452523147275828,
11.9077859527864));
#14913=CARTESIAN_POINT('Ctrl Pts',(-4.08474695018234,0.467269876710216,
11.8974070840654));
#14914=CARTESIAN_POINT('Ctrl Pts',(-4.08693113570529,0.476307270345706,
11.8837903326451));
#14915=CARTESIAN_POINT('Ctrl Pts',(-4.088504487915,0.480216196086898,11.8760208135731));
#14916=CARTESIAN_POINT('Ctrl Pts',(-4.08957475120669,0.420000000000002,
11.9129846529869));
#14917=CARTESIAN_POINT('Ctrl Pts',(-4.08688537940494,0.425116071352305,
11.9156410715272));
#14918=CARTESIAN_POINT('Ctrl Pts',(-4.08194577754747,0.435809942712488,
11.9190952094536));
#14919=CARTESIAN_POINT('Ctrl Pts',(-4.0763463965552,0.453454331933779,11.9169484279061));
#14920=CARTESIAN_POINT('Ctrl Pts',(-4.07432022781093,0.470721130278274,
11.9042829130981));
#14921=CARTESIAN_POINT('Ctrl Pts',(-4.07611770769293,0.48001701618929,11.888710974919));
#14922=CARTESIAN_POINT('Ctrl Pts',(-4.07758517014024,0.483840236412191,
11.8801119543743));
#14923=CARTESIAN_POINT('Ctrl Pts',(-4.08957475120669,0.420000000000002,
11.9129846529869));
#14924=CARTESIAN_POINT('Ctrl Pts',(-4.08688537940494,0.425116071352305,
11.9156410715272));
#14925=CARTESIAN_POINT('Ctrl Pts',(-4.08194577754747,0.435809942712488,
11.9190952094536));
#14926=CARTESIAN_POINT('Ctrl Pts',(-4.0763463965552,0.453454331933779,11.9169484279061));
#14927=CARTESIAN_POINT('Ctrl Pts',(-4.07457762006514,0.468527660380283,
11.9058918636934));
#14928=CARTESIAN_POINT('Ctrl Pts',(-4.07558957056381,0.476670041956566,
11.8939568640326));
#14929=CARTESIAN_POINT('Ctrl Pts',(-4.07626606489887,0.479531832015509,
11.8887931799445));
#14930=CARTESIAN_POINT('Origin',(-4.11158163835162,0.547680472824379,11.9142976877142));
#14931=CARTESIAN_POINT('Ctrl Pts',(-4.16771789344709,0.504034482698269,
11.8776405136582));
#14932=CARTESIAN_POINT('Ctrl Pts',(-4.16747677218029,0.509230674892329,
11.8710844000372));
#14933=CARTESIAN_POINT('Ctrl Pts',(-4.16740198755876,0.514183898751254,
11.8631601154487));
#14934=CARTESIAN_POINT('Ctrl Pts',(-4.16750381345594,0.518518893325527,
11.8542908886285));
#14935=CARTESIAN_POINT('Ctrl Pts',(-4.15716840981065,0.494162146356706,
11.8732397213383));
#14936=CARTESIAN_POINT('Ctrl Pts',(-4.15737066207015,0.49902515398837,11.8672225409494));
#14937=CARTESIAN_POINT('Ctrl Pts',(-4.15774524939355,0.503761760048647,
11.8598165458383));
#14938=CARTESIAN_POINT('Ctrl Pts',(-4.15827955078225,0.507967835497394,
11.8514452383884));
#14939=CARTESIAN_POINT('Ctrl Pts',(-4.12991591613054,0.479256016633343,
11.8684902470024));
#14940=CARTESIAN_POINT('Ctrl Pts',(-4.13102224542203,0.48352297529437,11.8628269450333));
#14941=CARTESIAN_POINT('Ctrl Pts',(-4.13236454521323,0.487741753406994,
11.8558585890896));
#14942=CARTESIAN_POINT('Ctrl Pts',(-4.13387372265488,0.491526065878086,
11.8479575722917));
#14943=CARTESIAN_POINT('Ctrl Pts',(-4.09886149942541,0.47853885680583,11.8732397213383));
#14944=CARTESIAN_POINT('Ctrl Pts',(-4.10035784041994,0.482395955248883,
11.8663776500601));
#14945=CARTESIAN_POINT('Ctrl Pts',(-4.10225093958688,0.485898763965467,
11.8584280339396));
#14946=CARTESIAN_POINT('Ctrl Pts',(-4.10441543782456,0.488897063406756,
11.8498117164234));
#14947=CARTESIAN_POINT('Ctrl Pts',(-4.08478921042867,0.481813809054108,
11.8776405136582));
#14948=CARTESIAN_POINT('Ctrl Pts',(-4.08624010985666,0.485540704403993,
11.8698834704985));
#14949=CARTESIAN_POINT('Ctrl Pts',(-4.08818793877976,0.488689291789136,
11.861178695302));
#14950=CARTESIAN_POINT('Ctrl Pts',(-4.09047268188156,0.491245759629021,
11.8519547869365));
#14951=CARTESIAN_POINT('Ctrl Pts',(-4.1,0.5,11.7890187209227));
#14952=CARTESIAN_POINT('Ctrl Pts',(-4.13477970278813,0.5,11.7464513530047));
#14953=CARTESIAN_POINT('Ctrl Pts',(-4.16929090131684,0.504455968886619,
11.7035428752933));
#14954=CARTESIAN_POINT('Ctrl Pts',(-4.20352761804122,0.513629669484429,
11.6617726299259));
#14955=CARTESIAN_POINT('Ctrl Pts',(-4.10836665945874,0.5,11.7972219040708));
#14956=CARTESIAN_POINT('Ctrl Pts',(-4.14352422788613,0.500728939428738,
11.754930342142));
#14957=CARTESIAN_POINT('Ctrl Pts',(-4.17822160408369,0.506004692387703,
11.7124031482063));
#14958=CARTESIAN_POINT('Ctrl Pts',(-4.21239479773503,0.516005623122533,
11.6711203195198));
#14959=CARTESIAN_POINT('Ctrl Pts',(-4.1167281686604,0.497385130283631,11.8054200375929));
#14960=CARTESIAN_POINT('Ctrl Pts',(-4.1524905396068,0.49863124735402,11.763403178915));
#14961=CARTESIAN_POINT('Ctrl Pts',(-4.18765174637402,0.504533209103448,
11.7212564005378));
#14962=CARTESIAN_POINT('Ctrl Pts',(-4.22210281883105,0.515209463850521,
11.6804590353039));
#14963=CARTESIAN_POINT('Ctrl Pts',(-4.12430006992852,0.492400711949332,
11.8128439913451));
#14964=CARTESIAN_POINT('Ctrl Pts',(-4.16077688798415,0.493922555267979,
11.7710156405394));
#14965=CARTESIAN_POINT('Ctrl Pts',(-4.19655913075278,0.500206823344764,
11.7291447804131));
#14966=CARTESIAN_POINT('Ctrl Pts',(-4.23152093150711,0.511333924981017,
11.6887010425988));
#14967=CARTESIAN_POINT('',(-4.1,0.5,11.7890187209227));
#14968=CARTESIAN_POINT('Origin',(-4.1,0.42,11.7890187209227));
#14969=CARTESIAN_POINT('Ctrl Pts',(-4.1,0.5,11.7890187209227));
#14970=CARTESIAN_POINT('Ctrl Pts',(-4.13477970278813,0.5,11.7464513530047));
#14971=CARTESIAN_POINT('Ctrl Pts',(-4.16929090131684,0.504455968886619,
11.7035428752933));
#14972=CARTESIAN_POINT('Ctrl Pts',(-4.20352761804122,0.513629669484429,
11.6617726299259));
#14973=CARTESIAN_POINT('Ctrl Pts',(-4.13726390506229,0.480634448429844,
11.8255545258696));
#14974=CARTESIAN_POINT('Ctrl Pts',(-4.11846919910142,0.480634448429844,
11.8447237802385));
#14975=CARTESIAN_POINT('Ctrl Pts',(-4.0995468371381,0.480634448429845,11.8638771748766));
#14976=CARTESIAN_POINT('Ctrl Pts',(-4.08038777665855,0.480634448429845,
11.8829301635628));
#14977=CARTESIAN_POINT('Ctrl Pts',(-4.12700765835792,0.492996832959403,
11.8154986761552));
#14978=CARTESIAN_POINT('Ctrl Pts',(-4.10823910349475,0.492996832959403,
11.8346412582769));
#14979=CARTESIAN_POINT('Ctrl Pts',(-4.08935809686133,0.492996832959405,
11.8537525739076));
#14980=CARTESIAN_POINT('Ctrl Pts',(-4.0702594664804,0.492996832959404,11.872745467059));
#14981=CARTESIAN_POINT('Ctrl Pts',(-4.11353190731664,0.500000000000001,
11.8022862280574));
#14982=CARTESIAN_POINT('Ctrl Pts',(-4.09479778199198,0.500000000000001,
11.821393694515));
#14983=CARTESIAN_POINT('Ctrl Pts',(-4.0759708825117,0.500000000000003,11.8404499526433));
#14984=CARTESIAN_POINT('Ctrl Pts',(-4.05695181209536,0.500000000000002,
11.8593637263041));
#14985=CARTESIAN_POINT('Ctrl Pts',(-4.09999999999997,0.500000000000001,
11.7890187209227));
#14986=CARTESIAN_POINT('Ctrl Pts',(-4.08130046851071,0.500000000000001,
11.8080909041452));
#14987=CARTESIAN_POINT('Ctrl Pts',(-4.06252783272246,0.500000000000003,
11.8270919444204));
#14988=CARTESIAN_POINT('Ctrl Pts',(-4.04358870192888,0.500000000000002,
11.8459262210343));
#14989=CARTESIAN_POINT('',(-4.04358870192886,0.5,11.8459262210343));
#14990=CARTESIAN_POINT('Origin',(-4.04358870192886,0.42,11.8459262210343));
#14991=CARTESIAN_POINT('Ctrl Pts',(-4.04358870192888,0.500000000000002,
11.8459262210343));
#14992=CARTESIAN_POINT('Ctrl Pts',(-4.06252783272246,0.500000000000003,
11.8270919444204));
#14993=CARTESIAN_POINT('Ctrl Pts',(-4.08130046851071,0.500000000000001,
11.8080909041452));
#14994=CARTESIAN_POINT('Ctrl Pts',(-4.09999999999997,0.500000000000001,
11.7890187209227));
#14995=CARTESIAN_POINT('Ctrl Pts',(-4.0999999999998,0.42,11.9026515720685));
#14996=CARTESIAN_POINT('Ctrl Pts',(-4.06432399954019,0.42,11.9381300567181));
#14997=CARTESIAN_POINT('Ctrl Pts',(-3.98818997166498,0.42,12.0113742928463));
#14998=CARTESIAN_POINT('Ctrl Pts',(-3.86894020585271,0.42,12.109102240647));
#14999=CARTESIAN_POINT('Ctrl Pts',(-3.73111144412829,0.42,12.1934025947443));
#15000=CARTESIAN_POINT('Ctrl Pts',(-3.52459207479152,0.42,12.2691713922624));
#15001=CARTESIAN_POINT('Ctrl Pts',(-3.26513732430851,0.42,12.297823424652));
#15002=CARTESIAN_POINT('Ctrl Pts',(-2.86516759113243,0.42,12.3018709397382));
#15003=CARTESIAN_POINT('Ctrl Pts',(-2.37243413007993,0.42,12.2928374209075));
#15004=CARTESIAN_POINT('Ctrl Pts',(-1.18525443737258,0.42,12.2925016573196));
#15005=CARTESIAN_POINT('Ctrl Pts',(0.197222451502637,0.42,12.3061814082829));
#15006=CARTESIAN_POINT('Ctrl Pts',(1.58273499720914,0.42,12.2905377746514));
#15007=CARTESIAN_POINT('Ctrl Pts',(2.37158402949751,0.42,12.2934888460097));
#15008=CARTESIAN_POINT('Ctrl Pts',(2.86495583790509,0.42,12.3017734583628));
#15009=CARTESIAN_POINT('Ctrl Pts',(3.26529661019376,0.42,12.2978358829359));
#15010=CARTESIAN_POINT('Ctrl Pts',(3.52422846912908,0.42,12.2692306735397));
#15011=CARTESIAN_POINT('Ctrl Pts',(3.73122727647141,0.42,12.1933706003979));
#15012=CARTESIAN_POINT('Ctrl Pts',(3.86889495391816,0.42,12.1090059816509));
#15013=CARTESIAN_POINT('Ctrl Pts',(3.98631775211335,0.42,12.0130270377017));
#15014=CARTESIAN_POINT('Ctrl Pts',(4.06432399954022,0.42,11.9381300567193));
#15015=CARTESIAN_POINT('Ctrl Pts',(4.09999999999981,0.42,11.9026515720696));
#15016=CARTESIAN_POINT('Ctrl Pts',(-4.0999999999998,0.443935944027351,11.9026515720685));
#15017=CARTESIAN_POINT('Ctrl Pts',(-4.0643220054189,0.443935944027351,11.9381320397991));
#15018=CARTESIAN_POINT('Ctrl Pts',(-3.98819821833631,0.443935944027351,
12.0113730441545));
#15019=CARTESIAN_POINT('Ctrl Pts',(-3.86894133667588,0.443935944027351,
12.1091109056158));
#15020=CARTESIAN_POINT('Ctrl Pts',(-3.73109426468088,0.443935944027351,
12.1934251234395));
#15021=CARTESIAN_POINT('Ctrl Pts',(-3.52453039533999,0.443935944027351,
12.2692079948208));
#15022=CARTESIAN_POINT('Ctrl Pts',(-3.26508191635705,0.443935944027351,
12.2978445388081));
#15023=CARTESIAN_POINT('Ctrl Pts',(-2.86512840714357,0.443935944027351,
12.301883045595));
#15024=CARTESIAN_POINT('Ctrl Pts',(-2.37242384296456,0.443935944027351,
12.2928403209455));
#15025=CARTESIAN_POINT('Ctrl Pts',(-1.18525600106237,0.443935944027351,
12.2925029665493));
#15026=CARTESIAN_POINT('Ctrl Pts',(0.197225231324838,0.44393594402735,12.306179798813));
#15027=CARTESIAN_POINT('Ctrl Pts',(1.58273129397298,0.443935944027351,12.2905396651414));
#15028=CARTESIAN_POINT('Ctrl Pts',(2.3715789007231,0.443935944027351,12.2934900210802));
#15029=CARTESIAN_POINT('Ctrl Pts',(2.8649096643031,0.443935944027351,12.3017877807429));
#15030=CARTESIAN_POINT('Ctrl Pts',(3.26524130832891,0.443935944027351,12.2978569519032));
#15031=CARTESIAN_POINT('Ctrl Pts',(3.52416578331235,0.443935944027351,12.2692675954058));
#15032=CARTESIAN_POINT('Ctrl Pts',(3.73120989460243,0.443935944027351,12.1933931820489));
#15033=CARTESIAN_POINT('Ctrl Pts',(3.86889576959486,0.443935944027351,12.1090147570509));
#15034=CARTESIAN_POINT('Ctrl Pts',(3.98632566897136,0.443935944027351,12.0130260375901));
#15035=CARTESIAN_POINT('Ctrl Pts',(4.06432200541893,0.443935944027351,11.9381320398003));
#15036=CARTESIAN_POINT('Ctrl Pts',(4.09999999999981,0.443935944027351,11.9026515720696));
#15037=CARTESIAN_POINT('Ctrl Pts',(-4.08582416466455,0.48536014866598,11.8883968170266));
#15038=CARTESIAN_POINT('Ctrl Pts',(-4.05030544143939,0.48536014866598,11.9237188951879));
#15039=CARTESIAN_POINT('Ctrl Pts',(-3.97469565176084,0.48536014866598,11.9964466583217));
#15040=CARTESIAN_POINT('Ctrl Pts',(-3.85709194674926,0.48536014866598,12.0927846652945));
#15041=CARTESIAN_POINT('Ctrl Pts',(-3.72224972003245,0.48536014866598,12.1751942765285));
#15042=CARTESIAN_POINT('Ctrl Pts',(-3.52063687145968,0.48536014866598,12.2492378201496));
#15043=CARTESIAN_POINT('Ctrl Pts',(-3.26439665787152,0.48536014866598,12.2777279953723));
#15044=CARTESIAN_POINT('Ctrl Pts',(-2.86552312724983,0.48536014866598,12.2817557317464));
#15045=CARTESIAN_POINT('Ctrl Pts',(-2.37263653108989,0.48536014866598,12.2727373685992));
#15046=CARTESIAN_POINT('Ctrl Pts',(-1.18492906129251,0.485360148665981,
12.2723917905604));
#15047=CARTESIAN_POINT('Ctrl Pts',(0.19708118789358,0.48536014866598,12.2860843598974));
#15048=CARTESIAN_POINT('Ctrl Pts',(1.58260427556699,0.485360148665981,12.2704294766691));
#15049=CARTESIAN_POINT('Ctrl Pts',(2.37177678789268,0.48536014866598,12.2733912458457));
#15050=CARTESIAN_POINT('Ctrl Pts',(2.86532273287249,0.48536014866598,12.2816545608874));
#15051=CARTESIAN_POINT('Ctrl Pts',(3.26455255367795,0.48536014866598,12.2777416788692));
#15052=CARTESIAN_POINT('Ctrl Pts',(3.5202829538042,0.48536014866598,12.2492936061086));
#15053=CARTESIAN_POINT('Ctrl Pts',(3.72236308599005,0.48536014866598,12.1751634108215));
#15054=CARTESIAN_POINT('Ctrl Pts',(3.85705298820777,0.48536014866598,12.092684991886));
#15055=CARTESIAN_POINT('Ctrl Pts',(3.97284435283825,0.48536014866598,11.9980807271348));
#15056=CARTESIAN_POINT('Ctrl Pts',(4.05030544143941,0.48536014866598,11.9237188951891));
#15057=CARTESIAN_POINT('Ctrl Pts',(4.08582416466454,0.48536014866598,11.8883968170278));
#15058=CARTESIAN_POINT('Ctrl Pts',(-4.05624736761451,0.5,11.8586553600401));
#15059=CARTESIAN_POINT('Ctrl Pts',(-4.02105560774434,0.5,11.893652285039));
#15060=CARTESIAN_POINT('Ctrl Pts',(-3.94654567923738,0.5,11.9653005485802));
#15061=CARTESIAN_POINT('Ctrl Pts',(-3.83237213080353,0.5,12.0587444343159));
#15062=CARTESIAN_POINT('Ctrl Pts',(-3.7037502134039,0.5,12.1372173836306));
#15063=CARTESIAN_POINT('Ctrl Pts',(-3.51234803324907,0.5,12.2076696701355));
#15064=CARTESIAN_POINT('Ctrl Pts',(-3.26281842755994,0.5,12.2358129498859));
#15065=CARTESIAN_POINT('Ctrl Pts',(-2.86624166923353,0.5,12.2397940727743));
#15066=CARTESIAN_POINT('Ctrl Pts',(-2.37305271959604,0.5,12.230801866854));
#15067=CARTESIAN_POINT('Ctrl Pts',(-1.18425111706809,0.500000000000001,
12.2304348675178));
#15068=CARTESIAN_POINT('Ctrl Pts',(0.196788102082843,0.499999999999999,
12.24415244907));
#15069=CARTESIAN_POINT('Ctrl Pts',(1.58232933686155,0.5,12.2284761717562));
#15070=CARTESIAN_POINT('Ctrl Pts',(2.37217591946072,0.499999999999999,12.2314598364887));
#15071=CARTESIAN_POINT('Ctrl Pts',(2.86606082566913,0.5,12.2396865196674));
#15072=CARTESIAN_POINT('Ctrl Pts',(3.26296731319181,0.5,12.2358291628754));
#15073=CARTESIAN_POINT('Ctrl Pts',(3.51201373156969,0.5,12.2077183528994));
#15074=CARTESIAN_POINT('Ctrl Pts',(3.70385831329287,0.5,12.1371889041741));
#15075=CARTESIAN_POINT('Ctrl Pts',(3.83234611589616,0.5,12.0586377025416));
#15076=CARTESIAN_POINT('Ctrl Pts',(3.94473783385368,0.5,11.9668957987984));
#15077=CARTESIAN_POINT('Ctrl Pts',(4.02105560774433,0.5,11.8936522850402));
#15078=CARTESIAN_POINT('Ctrl Pts',(4.05624736761446,0.5,11.8586553600413));
#15079=CARTESIAN_POINT('Ctrl Pts',(-4.04358870192886,0.5,11.8459262210343));
#15080=CARTESIAN_POINT('Ctrl Pts',(-4.00853667496434,0.5,11.8807841867417));
#15081=CARTESIAN_POINT('Ctrl Pts',(-3.9344985330766,0.5,11.9519700993884));
#15082=CARTESIAN_POINT('Ctrl Pts',(-3.82179233596298,0.5,12.0441763410897));
#15083=CARTESIAN_POINT('Ctrl Pts',(-3.69583078434751,0.5,12.120965852524));
#15084=CARTESIAN_POINT('Ctrl Pts',(-3.50879412174487,0.5,12.1898825536479));
#15085=CARTESIAN_POINT('Ctrl Pts',(-3.26213725530659,0.5,12.2178757710291));
#15086=CARTESIAN_POINT('Ctrl Pts',(-2.86654516889356,0.5,12.2218360168654));
#15087=CARTESIAN_POINT('Ctrl Pts',(-2.37322978704452,0.5,12.2128540589361));
#15088=CARTESIAN_POINT('Ctrl Pts',(-1.18396112248055,0.500000000000001,
12.2124777277647));
#15089=CARTESIAN_POINT('Ctrl Pts',(0.196662949368364,0.499999999999999,
12.2262057140885));
#15090=CARTESIAN_POINT('Ctrl Pts',(1.58221128398681,0.5,12.2105206403396));
#15091=CARTESIAN_POINT('Ctrl Pts',(2.37234621736262,0.499999999999999,12.2135136026149));
#15092=CARTESIAN_POINT('Ctrl Pts',(2.86637197383024,0.5,12.2217259602429));
#15093=CARTESIAN_POINT('Ctrl Pts',(3.26228315154647,0.5,12.2178930619748));
#15094=CARTESIAN_POINT('Ctrl Pts',(3.50846811203046,0.5,12.1899282291445));
#15095=CARTESIAN_POINT('Ctrl Pts',(3.69593660956959,0.5,12.1209383998147));
#15096=CARTESIAN_POINT('Ctrl Pts',(3.82177182841876,0.5,12.0440665997448));
#15097=CARTESIAN_POINT('Ctrl Pts',(3.93270925157646,0.5,11.9535487610897));
#15098=CARTESIAN_POINT('Ctrl Pts',(4.00853667496432,0.5,11.8807841867429));
#15099=CARTESIAN_POINT('Ctrl Pts',(4.0435887019288,0.5,11.8459262210355));
#15100=CARTESIAN_POINT('',(4.09999999999981,0.42,11.9026515720696));
#15101=CARTESIAN_POINT('Ctrl Pts',(-4.08957475120668,0.42,11.9129846529869));
#15102=CARTESIAN_POINT('Ctrl Pts',(-4.07070912639531,0.42,11.9316191145701));
#15103=CARTESIAN_POINT('Ctrl Pts',(-4.0512337618078,0.42,11.9504965620406));
#15104=CARTESIAN_POINT('Ctrl Pts',(-4.03136941462863,0.42,11.9691382395571));
#15105=CARTESIAN_POINT('Ctrl Pts',(-4.01968819006244,0.42,11.9801004735231));
#15106=CARTESIAN_POINT('Ctrl Pts',(-4.00787168701817,0.42,11.9909814506739));
#15107=CARTESIAN_POINT('Ctrl Pts',(-3.9959601173972,0.42,12.0016910697278));
#15108=CARTESIAN_POINT('Ctrl Pts',(-3.98877368957404,0.42,12.0081523428256));
#15109=CARTESIAN_POINT('Ctrl Pts',(-3.98155552980581,0.42,12.0145488528393));
#15110=CARTESIAN_POINT('Ctrl Pts',(-3.97430247432981,0.42,12.0208725332347));
#15111=CARTESIAN_POINT('Ctrl Pts',(-3.95549323097764,0.42,12.0372716416975));
#15112=CARTESIAN_POINT('Ctrl Pts',(-3.93643357392197,0.42,12.0531996537834));
#15113=CARTESIAN_POINT('Ctrl Pts',(-3.91688135136191,0.42,12.0686460330885));
#15114=CARTESIAN_POINT('Ctrl Pts',(-3.89958719643529,0.42,12.0823085247022));
#15115=CARTESIAN_POINT('Ctrl Pts',(-3.88190823253498,0.42,12.0955935663832));
#15116=CARTESIAN_POINT('Ctrl Pts',(-3.86365572107541,0.42,12.1084664329205));
#15117=CARTESIAN_POINT('Ctrl Pts',(-3.84554580736162,0.42,12.121238730188));
#15118=CARTESIAN_POINT('Ctrl Pts',(-3.82687067374783,0.42,12.1335981171097));
#15119=CARTESIAN_POINT('Ctrl Pts',(-3.80766293258994,0.42,12.1453574730567));
#15120=CARTESIAN_POINT('Ctrl Pts',(-3.78860525190984,0.42,12.1570249590355));
#15121=CARTESIAN_POINT('Ctrl Pts',(-3.76902255736466,0.42,12.1681009219439));
#15122=CARTESIAN_POINT('Ctrl Pts',(-3.74894872534242,0.42,12.1784597126869));
#15123=CARTESIAN_POINT('Ctrl Pts',(-3.73602631200023,0.42,12.1851281243563));
#15124=CARTESIAN_POINT('Ctrl Pts',(-3.72289678284864,0.42,12.1915021804535));
#15125=CARTESIAN_POINT('Ctrl Pts',(-3.70958667619023,0.42,12.1975557390669));
#15126=CARTESIAN_POINT('Ctrl Pts',(-3.69192772874079,0.42,12.2055871903678));
#15127=CARTESIAN_POINT('Ctrl Pts',(-3.67395508821995,0.42,12.213050119862));
#15128=CARTESIAN_POINT('Ctrl Pts',(-3.65577503211398,0.42,12.2199120405514));
#15129=CARTESIAN_POINT('Ctrl Pts',(-3.63730907646068,0.42,12.2268818718));
#15130=CARTESIAN_POINT('Ctrl Pts',(-3.61862858092384,0.42,12.2332320858495));
#15131=CARTESIAN_POINT('Ctrl Pts',(-3.59987390808581,0.42,12.2389739060236));
#15132=CARTESIAN_POINT('Ctrl Pts',(-3.58812827122212,0.42,12.2425698810258));
#15133=CARTESIAN_POINT('Ctrl Pts',(-3.57635645365837,0.42,12.2459275182189));
#15134=CARTESIAN_POINT('Ctrl Pts',(-3.56459228573084,0.42,12.2490589093387));
#15135=CARTESIAN_POINT('Ctrl Pts',(-3.53640474847592,0.42,12.2565618797478));
#15136=CARTESIAN_POINT('Ctrl Pts',(-3.50822366783652,0.42,12.2627808667959));
#15137=CARTESIAN_POINT('Ctrl Pts',(-3.48006243281124,0.42,12.2680130438463));
#15138=CARTESIAN_POINT('Ctrl Pts',(-3.45179977817908,0.42,12.2732640640098));
#15139=CARTESIAN_POINT('Ctrl Pts',(-3.42355783651323,0.42,12.2775216531967));
#15140=CARTESIAN_POINT('Ctrl Pts',(-3.39537788085669,0.42,12.2810411396377));
#15141=CARTESIAN_POINT('Ctrl Pts',(-3.36659368263903,0.42,12.2846360919002));
#15142=CARTESIAN_POINT('Ctrl Pts',(-3.33787477852993,0.42,12.2874610919638));
#15143=CARTESIAN_POINT('Ctrl Pts',(-3.30928381995259,0.42,12.2897363835961));
#15144=CARTESIAN_POINT('Ctrl Pts',(-3.29376488816646,0.42,12.2909713927525));
#15145=CARTESIAN_POINT('Ctrl Pts',(-3.27828562790243,0.42,12.2920434331052));
#15146=CARTESIAN_POINT('Ctrl Pts',(-3.26285194183848,0.42,12.292981865386));
#15147=CARTESIAN_POINT('Ctrl Pts',(-3.23369857325195,0.42,12.2947545114061));
#15148=CARTESIAN_POINT('Ctrl Pts',(-3.20468141212112,0.42,12.2960551913495));
#15149=CARTESIAN_POINT('Ctrl Pts',(-3.17579045328073,0.42,12.2970396330972));
#15150=CARTESIAN_POINT('Ctrl Pts',(-3.14550795106456,0.42,12.2980714908341));
#15151=CARTESIAN_POINT('Ctrl Pts',(-3.11536462644417,0.42,12.2987553967142));
#15152=CARTESIAN_POINT('Ctrl Pts',(-3.08532794916976,0.42,12.2992169145794));
#15153=CARTESIAN_POINT('Ctrl Pts',(-3.05377633819841,0.42,12.2997017096187));
#15154=CARTESIAN_POINT('Ctrl Pts',(-3.0223429235208,0.42,12.2999404094041));
#15155=CARTESIAN_POINT('Ctrl Pts',(-2.99095908120567,0.42,12.300030121024));
#15156=CARTESIAN_POINT('Ctrl Pts',(-2.97279349404179,0.42,12.3000820478797));
#15157=CARTESIAN_POINT('Ctrl Pts',(-2.95464182185859,0.42,12.3000832384085));
#15158=CARTESIAN_POINT('Ctrl Pts',(-2.93649043054004,0.42,12.3000470713686));
#15159=CARTESIAN_POINT('Ctrl Pts',(-2.89676042107724,0.42,12.2999679084653));
#15160=CARTESIAN_POINT('Ctrl Pts',(-2.85705476098733,0.42,12.2997128386374));
#15161=CARTESIAN_POINT('Ctrl Pts',(-2.81741363626107,0.42,12.2993798909943));
#15162=CARTESIAN_POINT('Ctrl Pts',(-2.77585567983252,0.42,12.2990308437929));
#15163=CARTESIAN_POINT('Ctrl Pts',(-2.73436928668848,0.42,12.2985951218158));
#15164=CARTESIAN_POINT('Ctrl Pts',(-2.69296287950309,0.42,12.2981386342706));
#15165=CARTESIAN_POINT('Ctrl Pts',(-2.65015799313489,0.42,12.2976667291035));
#15166=CARTESIAN_POINT('Ctrl Pts',(-2.60743892093361,0.42,12.2971716744601));
#15167=CARTESIAN_POINT('Ctrl Pts',(-2.56476785938501,0.42,12.2966935956038));
#15168=CARTESIAN_POINT('Ctrl Pts',(-2.52908709297847,0.42,12.29629383475));
#15169=CARTESIAN_POINT('Ctrl Pts',(-2.49343899198747,0.42,12.2959052051901));
#15170=CARTESIAN_POINT('Ctrl Pts',(-2.45777598101278,0.42,12.29554055751));
#15171=CARTESIAN_POINT('Ctrl Pts',(-2.4327936161251,0.42,12.2952851174574));
#15172=CARTESIAN_POINT('Ctrl Pts',(-2.40780344620683,0.42,12.2950412596816));
#15173=CARTESIAN_POINT('Ctrl Pts',(-2.38278265214531,0.42,12.2948116115015));
#15174=CARTESIAN_POINT('Ctrl Pts',(-2.36409688161798,0.42,12.2946401080239));
#15175=CARTESIAN_POINT('Ctrl Pts',(-2.34539571618718,0.42,12.294476523425));
#15176=CARTESIAN_POINT('Ctrl Pts',(-2.3266909260608,0.42,12.2943217432458));
#15177=CARTESIAN_POINT('Ctrl Pts',(-2.27024903989047,0.42,12.2938546925492));
#15178=CARTESIAN_POINT('Ctrl Pts',(-2.21375528545711,0.42,12.2934689635508));
#15179=CARTESIAN_POINT('Ctrl Pts',(-2.15726656535151,0.42,12.2931722059907));
#15180=CARTESIAN_POINT('Ctrl Pts',(-2.09932295136259,0.42,12.2928678052983));
#15181=CARTESIAN_POINT('Ctrl Pts',(-2.04138464776779,0.42,12.2926564220354));
#15182=CARTESIAN_POINT('Ctrl Pts',(-1.98346034243504,0.42,12.2925319928656));
#15183=CARTESIAN_POINT('Ctrl Pts',(-1.92373696814234,0.42,12.2924036990547));
#15184=CARTESIAN_POINT('Ctrl Pts',(-1.86402835174857,0.42,12.2923674602502));
#15185=CARTESIAN_POINT('Ctrl Pts',(-1.80428946616947,0.42,12.2924092102655));
#15186=CARTESIAN_POINT('Ctrl Pts',(-1.78362811703507,0.42,12.2924236499664));
#15187=CARTESIAN_POINT('Ctrl Pts',(-1.76296338243997,0.42,12.2924473754325));
#15188=CARTESIAN_POINT('Ctrl Pts',(-1.74227825988445,0.42,12.2924797416047));
#15189=CARTESIAN_POINT('Ctrl Pts',(-1.66551379267926,0.42,12.2925998555636));
#15190=CARTESIAN_POINT('Ctrl Pts',(-1.58853637524402,0.42,12.2928393894616));
#15191=CARTESIAN_POINT('Ctrl Pts',(-1.51149675923115,0.42,12.2931600654634));
#15192=CARTESIAN_POINT('Ctrl Pts',(-1.43226893428785,0.42,12.2934898498452));
#15193=CARTESIAN_POINT('Ctrl Pts',(-1.35297520958703,0.42,12.2939050013854));
#15194=CARTESIAN_POINT('Ctrl Pts',(-1.27372326985414,0.42,12.2943620060925));
#15195=CARTESIAN_POINT('Ctrl Pts',(-1.19121670263452,0.42,12.2948377785431));
#15196=CARTESIAN_POINT('Ctrl Pts',(-1.10875518516202,0.42,12.2953586061595));
#15197=CARTESIAN_POINT('Ctrl Pts',(-1.02640265123843,0.42,12.2958793155528));
#15198=CARTESIAN_POINT('Ctrl Pts',(-0.939286032192044,0.42,12.2964301479279));
#15199=CARTESIAN_POINT('Ctrl Pts',(-0.852290996877637,0.42,12.2969806094654));
#15200=CARTESIAN_POINT('Ctrl Pts',(-0.765434646151399,0.42,12.2974858650896));
#15201=CARTESIAN_POINT('Ctrl Pts',(-0.671380899427911,0.42,12.2980329889799));
#15202=CARTESIAN_POINT('Ctrl Pts',(-0.57748916422919,0.42,12.2985268001515));
#15203=CARTESIAN_POINT('Ctrl Pts',(-0.483721777843278,0.42,12.2989246112183));
#15204=CARTESIAN_POINT('Ctrl Pts',(-0.371719028569128,0.42,12.2993997863818));
#15205=CARTESIAN_POINT('Ctrl Pts',(-0.259892687853164,0.42,12.2997368001716));
#15206=CARTESIAN_POINT('Ctrl Pts',(-0.148108023827894,0.42,12.2998948321153));
#15207=CARTESIAN_POINT('Ctrl Pts',(-0.0348382015673389,0.42,12.3000549636533));
#15208=CARTESIAN_POINT('Ctrl Pts',(0.0783927177796026,0.42,12.3000304822599));
#15209=CARTESIAN_POINT('Ctrl Pts',(0.191748815331185,0.42,12.299824260992));
#15210=CARTESIAN_POINT('Ctrl Pts',(0.273957475225655,0.42,12.2996747042021));
#15211=CARTESIAN_POINT('Ctrl Pts',(0.356232687434953,0.42,12.2994307737856));
#15212=CARTESIAN_POINT('Ctrl Pts',(0.438626822026294,0.42,12.2991085248334));
#15213=CARTESIAN_POINT('Ctrl Pts',(0.486761625529418,0.42,12.2989202664085));
#15214=CARTESIAN_POINT('Ctrl Pts',(0.534936768026288,0.42,12.2987054934661));
#15215=CARTESIAN_POINT('Ctrl Pts',(0.583159437202681,0.42,12.2984690821935));
#15216=CARTESIAN_POINT('Ctrl Pts',(0.600704406570152,0.42,12.2983830681132));
#15217=CARTESIAN_POINT('Ctrl Pts',(0.61825202790425,0.42,12.2982942177471));
#15218=CARTESIAN_POINT('Ctrl Pts',(0.635793398928577,0.42,12.2982028570652));
#15219=CARTESIAN_POINT('Ctrl Pts',(0.722624179925258,0.42,12.2977506165105));
#15220=CARTESIAN_POINT('Ctrl Pts',(0.809376157106363,0.42,12.2972357585868));
#15221=CARTESIAN_POINT('Ctrl Pts',(0.896142685250265,0.42,12.2966978388299));
#15222=CARTESIAN_POINT('Ctrl Pts',(0.976708017257756,0.42,12.2961983641508));
#15223=CARTESIAN_POINT('Ctrl Pts',(1.05728638072386,0.42,12.2956791514925));
#15224=CARTESIAN_POINT('Ctrl Pts',(1.13791082663924,0.42,12.2951788015391));
#15225=CARTESIAN_POINT('Ctrl Pts',(1.21452814789454,0.42,12.294703319535));
#15226=CARTESIAN_POINT('Ctrl Pts',(1.29118742965583,0.42,12.2942450181282));
#15227=CARTESIAN_POINT('Ctrl Pts',(1.36787207531147,0.42,12.2938415740963));
#15228=CARTESIAN_POINT('Ctrl Pts',(1.44182337776109,0.42,12.2934525104009));
#15229=CARTESIAN_POINT('Ctrl Pts',(1.51579851999178,0.42,12.2931146870792));
#15230=CARTESIAN_POINT('Ctrl Pts',(1.5897353553651,0.42,12.2928636232826));
#15231=CARTESIAN_POINT('Ctrl Pts',(1.64315891931009,0.42,12.2926822154264));
#15232=CARTESIAN_POINT('Ctrl Pts',(1.69656152233123,0.42,12.2925461826626));
#15233=CARTESIAN_POINT('Ctrl Pts',(1.74990250989962,0.42,12.2924682031349));
#15234=CARTESIAN_POINT('Ctrl Pts',(1.81164714531486,0.42,12.2923779382612));
#15235=CARTESIAN_POINT('Ctrl Pts',(1.87329665865665,0.42,12.2923655874348));
#15236=CARTESIAN_POINT('Ctrl Pts',(1.93494398932289,0.42,12.2924476940399));
#15237=CARTESIAN_POINT('Ctrl Pts',(1.99177230648263,0.42,12.2925233823161));
#15238=CARTESIAN_POINT('Ctrl Pts',(2.04859905035996,0.42,12.2926795846011));
#15239=CARTESIAN_POINT('Ctrl Pts',(2.10544947311221,0.42,12.2929245095271));
#15240=CARTESIAN_POINT('Ctrl Pts',(2.16086336245647,0.42,12.2931632455309));
#15241=CARTESIAN_POINT('Ctrl Pts',(2.2162998172383,0.42,12.2934867203752));
#15242=CARTESIAN_POINT('Ctrl Pts',(2.2717345377493,0.42,12.2938928339529));
#15243=CARTESIAN_POINT('Ctrl Pts',(2.30424765863584,0.42,12.2941310243817));
#15244=CARTESIAN_POINT('Ctrl Pts',(2.33675926922426,0.42,12.2943974408816));
#15245=CARTESIAN_POINT('Ctrl Pts',(2.36925649852847,0.42,12.2946888798043));
#15246=CARTESIAN_POINT('Ctrl Pts',(2.38798692621633,0.42,12.2948568564528));
#15247=CARTESIAN_POINT('Ctrl Pts',(2.40670347471599,0.42,12.2950330172923));
#15248=CARTESIAN_POINT('Ctrl Pts',(2.42541331068238,0.42,12.2952163892074));
#15249=CARTESIAN_POINT('Ctrl Pts',(2.46864196476304,0.42,12.295640065882));
#15250=CARTESIAN_POINT('Ctrl Pts',(2.51184253377794,0.42,12.2961032804126));
#15251=CARTESIAN_POINT('Ctrl Pts',(2.55510163816728,0.42,12.2965855577766));
#15252=CARTESIAN_POINT('Ctrl Pts',(2.59710888202152,0.42,12.2970538786797));
#15253=CARTESIAN_POINT('Ctrl Pts',(2.63917124418029,0.42,12.2975407387835));
#15254=CARTESIAN_POINT('Ctrl Pts',(2.68132348844875,0.42,12.298009707522));
#15255=CARTESIAN_POINT('Ctrl Pts',(2.72181559106942,0.42,12.2984602061993));
#15256=CARTESIAN_POINT('Ctrl Pts',(2.76239031938167,0.42,12.2988949370747));
#15257=CARTESIAN_POINT('Ctrl Pts',(2.80303973715188,0.42,12.2992556829302));
#15258=CARTESIAN_POINT('Ctrl Pts',(2.83631806432058,0.42,12.2995510135712));
#15259=CARTESIAN_POINT('Ctrl Pts',(2.86964564495769,0.42,12.2997966701148));
#15260=CARTESIAN_POINT('Ctrl Pts',(2.90300032749941,0.42,12.2999403096602));
#15261=CARTESIAN_POINT('Ctrl Pts',(2.9253128012298,0.42,12.3000363967262));
#15262=CARTESIAN_POINT('Ctrl Pts',(2.94763579581574,0.42,12.3000864441799));
#15263=CARTESIAN_POINT('Ctrl Pts',(2.96996315170153,0.42,12.3000682690189));
#15264=CARTESIAN_POINT('Ctrl Pts',(3.001246560905,0.42,12.3000428033523));
#15265=CARTESIAN_POINT('Ctrl Pts',(3.03255914305104,0.42,12.2998853345777));
#15266=CARTESIAN_POINT('Ctrl Pts',(3.06397042497329,0.42,12.299508487312));
#15267=CARTESIAN_POINT('Ctrl Pts',(3.09387571006892,0.42,12.2991497077835));
#15268=CARTESIAN_POINT('Ctrl Pts',(3.12387002346923,0.42,12.2985926943181));
#15269=CARTESIAN_POINT('Ctrl Pts',(3.15398744202724,0.42,12.2977244393391));
#15270=CARTESIAN_POINT('Ctrl Pts',(3.18152646583026,0.42,12.2969305168957));
#15271=CARTESIAN_POINT('Ctrl Pts',(3.20916793051934,0.42,12.295876467876));
#15272=CARTESIAN_POINT('Ctrl Pts',(3.23692222273258,0.42,12.2944393742418));
#15273=CARTESIAN_POINT('Ctrl Pts',(3.25616037421766,0.42,12.2934432391279));
#15274=CARTESIAN_POINT('Ctrl Pts',(3.275450562525,0.42,12.2922625424322));
#15275=CARTESIAN_POINT('Ctrl Pts',(3.29480672148807,0.42,12.2908428966008));
#15276=CARTESIAN_POINT('Ctrl Pts',(3.32306225045922,0.42,12.2887705410268));
#15277=CARTESIAN_POINT('Ctrl Pts',(3.35144553838964,0.42,12.2861918016504));
#15278=CARTESIAN_POINT('Ctrl Pts',(3.37990572257727,0.42,12.2829011177135));
#15279=CARTESIAN_POINT('Ctrl Pts',(3.40779276483902,0.42,12.2796767028112));
#15280=CARTESIAN_POINT('Ctrl Pts',(3.43575306489468,0.42,12.2757687321118));
#15281=CARTESIAN_POINT('Ctrl Pts',(3.46375142663797,0.42,12.2709352312518));
#15282=CARTESIAN_POINT('Ctrl Pts',(3.49164628247108,0.42,12.2661195991483));
#15283=CARTESIAN_POINT('Ctrl Pts',(3.5195782146669,0.42,12.2603849831845));
#15284=CARTESIAN_POINT('Ctrl Pts',(3.54753465345975,0.42,12.253445044257));
#15285=CARTESIAN_POINT('Ctrl Pts',(3.55922703608369,0.42,12.2505425135761));
#15286=CARTESIAN_POINT('Ctrl Pts',(3.57092593140847,0.42,12.2474280556932));
#15287=CARTESIAN_POINT('Ctrl Pts',(3.582625824136,0.42,12.2440804130704));
#15288=CARTESIAN_POINT('Ctrl Pts',(3.60127037025197,0.42,12.2387457250768));
#15289=CARTESIAN_POINT('Ctrl Pts',(3.61989878758966,0.42,12.232820362843));
#15290=CARTESIAN_POINT('Ctrl Pts',(3.63835640205551,0.42,12.2262827655873));
#15291=CARTESIAN_POINT('Ctrl Pts',(3.65652907738884,0.42,12.2198460923861));
#15292=CARTESIAN_POINT('Ctrl Pts',(3.67453667498046,0.42,12.2128154357668));
#15293=CARTESIAN_POINT('Ctrl Pts',(3.69226143752051,0.42,12.2052109768377));
#15294=CARTESIAN_POINT('Ctrl Pts',(3.70807253769151,0.42,12.1984275369128));
#15295=CARTESIAN_POINT('Ctrl Pts',(3.72365839535628,0.42,12.1911883500437));
#15296=CARTESIAN_POINT('Ctrl Pts',(3.73895335801981,0.42,12.1835382315404));
#15297=CARTESIAN_POINT('Ctrl Pts',(3.75809368978208,0.42,12.1739647654655));
#15298=CARTESIAN_POINT('Ctrl Pts',(3.77678640737143,0.42,12.1637435281572));
#15299=CARTESIAN_POINT('Ctrl Pts',(3.79498734855382,0.42,12.1529840694506));
#15300=CARTESIAN_POINT('Ctrl Pts',(3.80954442722186,0.42,12.1443786745292));
#15301=CARTESIAN_POINT('Ctrl Pts',(3.82378730102014,0.42,12.135430261965));
#15302=CARTESIAN_POINT('Ctrl Pts',(3.83769546581467,0.42,12.1262188936489));
#15303=CARTESIAN_POINT('Ctrl Pts',(3.84723128386294,0.42,12.1199033276821));
#15304=CARTESIAN_POINT('Ctrl Pts',(3.85660972029853,0.42,12.1134646514204));
#15305=CARTESIAN_POINT('Ctrl Pts',(3.86582411962837,0.42,12.106933278707));
#15306=CARTESIAN_POINT('Ctrl Pts',(3.8833908188634,0.42,12.0944816086696));
#15307=CARTESIAN_POINT('Ctrl Pts',(3.90037718862227,0.42,12.0816882444054));
#15308=CARTESIAN_POINT('Ctrl Pts',(3.91703215924884,0.42,12.0685268765388));
#15309=CARTESIAN_POINT('Ctrl Pts',(3.93298261941915,0.42,12.0559222386412));
#15310=CARTESIAN_POINT('Ctrl Pts',(3.94862830275337,0.42,12.0429793468167));
#15311=CARTESIAN_POINT('Ctrl Pts',(3.96417057138444,0.42,12.0296382333238));
#15312=CARTESIAN_POINT('Ctrl Pts',(3.97157392199353,0.42,12.0232833733579));
#15313=CARTESIAN_POINT('Ctrl Pts',(3.97895364133667,0.42,12.0168376559896));
#15314=CARTESIAN_POINT('Ctrl Pts',(3.98633070224374,0.42,12.0102922388325));
#15315=CARTESIAN_POINT('Ctrl Pts',(4.00248995147145,0.42,11.9959546823893));
#15316=CARTESIAN_POINT('Ctrl Pts',(4.01861703151618,0.42,11.9811508058126));
#15317=CARTESIAN_POINT('Ctrl Pts',(4.0345005913335,0.42,11.9661948419058));
#15318=CARTESIAN_POINT('Ctrl Pts',(4.05281961135389,0.42,11.948945648061));
#15319=CARTESIAN_POINT('Ctrl Pts',(4.07081647195516,0.42,11.9314955882412));
#15320=CARTESIAN_POINT('Ctrl Pts',(4.08814786889807,0.42,11.9143933611413));
#15321=CARTESIAN_POINT('Ctrl Pts',(4.09213542393225,0.42,11.9104585328067));
#15322=CARTESIAN_POINT('Ctrl Pts',(4.09608761671172,0.42,11.9065422949265));
#15323=CARTESIAN_POINT('Ctrl Pts',(4.09999999999981,0.42,11.9026515720696));
#15324=CARTESIAN_POINT('',(4.0435887019288,0.5,11.8459262210355));
#15325=CARTESIAN_POINT('Origin',(4.0435887019288,0.42,11.8459262210355));
#15326=CARTESIAN_POINT('Ctrl Pts',(4.0435887019288,0.5,11.8459262210355));
#15327=CARTESIAN_POINT('Ctrl Pts',(4.00853667496432,0.5,11.8807841867429));
#15328=CARTESIAN_POINT('Ctrl Pts',(3.93270925157646,0.5,11.9535487610897));
#15329=CARTESIAN_POINT('Ctrl Pts',(3.82177182841876,0.5,12.0440665997448));
#15330=CARTESIAN_POINT('Ctrl Pts',(3.69593660956959,0.5,12.1209383998147));
#15331=CARTESIAN_POINT('Ctrl Pts',(3.50846811203046,0.5,12.1899282291445));
#15332=CARTESIAN_POINT('Ctrl Pts',(3.26228315154647,0.5,12.2178930619748));
#15333=CARTESIAN_POINT('Ctrl Pts',(2.86637197383024,0.5,12.2217259602429));
#15334=CARTESIAN_POINT('Ctrl Pts',(2.37234621736262,0.499999999999999,12.2135136026149));
#15335=CARTESIAN_POINT('Ctrl Pts',(1.58221128398681,0.5,12.2105206403396));
#15336=CARTESIAN_POINT('Ctrl Pts',(0.196662949368364,0.499999999999999,
12.2262057140885));
#15337=CARTESIAN_POINT('Ctrl Pts',(-1.18396112248055,0.500000000000001,
12.2124777277647));
#15338=CARTESIAN_POINT('Ctrl Pts',(-2.37322978704452,0.5,12.2128540589361));
#15339=CARTESIAN_POINT('Ctrl Pts',(-2.86654516889356,0.5,12.2218360168654));
#15340=CARTESIAN_POINT('Ctrl Pts',(-3.26213725530659,0.5,12.2178757710291));
#15341=CARTESIAN_POINT('Ctrl Pts',(-3.50879412174487,0.5,12.1898825536479));
#15342=CARTESIAN_POINT('Ctrl Pts',(-3.69583078434751,0.5,12.120965852524));
#15343=CARTESIAN_POINT('Ctrl Pts',(-3.82179233596298,0.5,12.0441763410897));
#15344=CARTESIAN_POINT('Ctrl Pts',(-3.9344985330766,0.5,11.9519700993884));
#15345=CARTESIAN_POINT('Ctrl Pts',(-4.00853667496434,0.5,11.8807841867417));
#15346=CARTESIAN_POINT('Ctrl Pts',(-4.04358870192886,0.5,11.8459262210343));
#15347=CARTESIAN_POINT('Ctrl Pts',(-4.0999999999998,0.,11.9026515720685));
#15348=CARTESIAN_POINT('Ctrl Pts',(-4.0999999999998,0.6,11.9026515720685));
#15349=CARTESIAN_POINT('Ctrl Pts',(-4.09081961446015,0.,11.9117811315272));
#15350=CARTESIAN_POINT('Ctrl Pts',(-4.09081961446015,0.6,11.9117811315272));
#15351=CARTESIAN_POINT('Ctrl Pts',(-4.05565687163378,0.,11.9465013108369));
#15352=CARTESIAN_POINT('Ctrl Pts',(-4.05565687163378,0.6,11.9465013108369));
#15353=CARTESIAN_POINT('Ctrl Pts',(-3.99482565231276,0.,12.0046763352293));
#15354=CARTESIAN_POINT('Ctrl Pts',(-3.99482565231276,0.6,12.0046763352293));
#15355=CARTESIAN_POINT('Ctrl Pts',(-3.9081172594404,0.,12.0806818325556));
#15356=CARTESIAN_POINT('Ctrl Pts',(-3.9081172594404,0.6,12.0806818325556));
#15357=CARTESIAN_POINT('Ctrl Pts',(-3.79241297762166,0.,12.1626050652586));
#15358=CARTESIAN_POINT('Ctrl Pts',(-3.79241297762166,0.6,12.1626050652586));
#15359=CARTESIAN_POINT('Ctrl Pts',(-3.64927048315908,0.,12.2301117722809));
#15360=CARTESIAN_POINT('Ctrl Pts',(-3.64927048315908,0.6,12.2301117722809));
#15361=CARTESIAN_POINT('Ctrl Pts',(-3.48993681214334,0.,12.2723364229645));
#15362=CARTESIAN_POINT('Ctrl Pts',(-3.48993681214334,0.6,12.2723364229645));
#15363=CARTESIAN_POINT('Ctrl Pts',(-3.30884480305534,0.,12.2938762651139));
#15364=CARTESIAN_POINT('Ctrl Pts',(-3.30884480305534,0.6,12.2938762651139));
#15365=CARTESIAN_POINT('Ctrl Pts',(-3.10127560868576,0.,12.3010487961981));
#15366=CARTESIAN_POINT('Ctrl Pts',(-3.10127560868576,0.6,12.3010487961981));
#15367=CARTESIAN_POINT('Ctrl Pts',(-2.86376302967345,0.,12.300400839059));
#15368=CARTESIAN_POINT('Ctrl Pts',(-2.86376302967345,0.6,12.300400839059));
#15369=CARTESIAN_POINT('Ctrl Pts',(-2.59461297443094,0.,12.2969132923574));
#15370=CARTESIAN_POINT('Ctrl Pts',(-2.59461297443094,0.6,12.2969132923574));
#15371=CARTESIAN_POINT('Ctrl Pts',(-2.29394197380209,0.,12.2935845551224));
#15372=CARTESIAN_POINT('Ctrl Pts',(-2.29394197380209,0.6,12.2935845551224));
#15373=CARTESIAN_POINT('Ctrl Pts',(-1.96338745719135,0.,12.2919684497906));
#15374=CARTESIAN_POINT('Ctrl Pts',(-1.96338745719135,0.6,12.2919684497906));
#15375=CARTESIAN_POINT('Ctrl Pts',(-1.60591558979456,0.,12.2924280531798));
#15376=CARTESIAN_POINT('Ctrl Pts',(-1.60591558979456,0.6,12.2924280531798));
#15377=CARTESIAN_POINT('Ctrl Pts',(-1.22558901314075,0.,12.2945066442122));
#15378=CARTESIAN_POINT('Ctrl Pts',(-1.22558901314075,0.6,12.2945066442122));
#15379=CARTESIAN_POINT('Ctrl Pts',(-0.827351903312651,0.,12.2972483292773));
#15380=CARTESIAN_POINT('Ctrl Pts',(-0.827351903312651,0.6,12.2972483292773));
#15381=CARTESIAN_POINT('Ctrl Pts',(-0.498916532526571,0.,12.299081889758));
#15382=CARTESIAN_POINT('Ctrl Pts',(-0.498916532526571,0.6,12.299081889758));
#15383=CARTESIAN_POINT('Ctrl Pts',(-0.249771440080693,0.,12.2998330708668));
#15384=CARTESIAN_POINT('Ctrl Pts',(-0.249771440080693,0.6,12.2998330708668));
#15385=CARTESIAN_POINT('Ctrl Pts',(-0.0832571466935557,0.,12.2999999999989));
#15386=CARTESIAN_POINT('Ctrl Pts',(-0.0832571466935557,0.6,12.2999999999989));
#15387=CARTESIAN_POINT('Ctrl Pts',(0.,0.,12.3));
#15388=CARTESIAN_POINT('Ctrl Pts',(0.,0.6,12.3));
#15389=CARTESIAN_POINT('Ctrl Pts',(0.0832571466935396,0.,12.3000000000011));
#15390=CARTESIAN_POINT('Ctrl Pts',(0.0832571466935396,0.6,12.3000000000011));
#15391=CARTESIAN_POINT('Ctrl Pts',(0.24977144008061,0.,12.2998330708736));
#15392=CARTESIAN_POINT('Ctrl Pts',(0.24977144008061,0.6,12.2998330708736));
#15393=CARTESIAN_POINT('Ctrl Pts',(0.498916532526534,0.,12.2990818897713));
#15394=CARTESIAN_POINT('Ctrl Pts',(0.498916532526534,0.6,12.2990818897713));
#15395=CARTESIAN_POINT('Ctrl Pts',(0.827351903312438,0.,12.2972483292974));
#15396=CARTESIAN_POINT('Ctrl Pts',(0.827351903312438,0.6,12.2972483292974));
#15397=CARTESIAN_POINT('Ctrl Pts',(1.22558901314046,0.,12.2945066442369));
#15398=CARTESIAN_POINT('Ctrl Pts',(1.22558901314046,0.6,12.2945066442369));
#15399=CARTESIAN_POINT('Ctrl Pts',(1.60591558979418,0.,12.2924280532047));
#15400=CARTESIAN_POINT('Ctrl Pts',(1.60591558979418,0.6,12.2924280532047));
#15401=CARTESIAN_POINT('Ctrl Pts',(1.96338745719096,0.,12.291968449812));
#15402=CARTESIAN_POINT('Ctrl Pts',(1.96338745719096,0.6,12.291968449812));
#15403=CARTESIAN_POINT('Ctrl Pts',(2.29394197380175,0.,12.2935845551378));
#15404=CARTESIAN_POINT('Ctrl Pts',(2.29394197380175,0.6,12.2935845551378));
#15405=CARTESIAN_POINT('Ctrl Pts',(2.59461297443069,0.,12.2969132923658));
#15406=CARTESIAN_POINT('Ctrl Pts',(2.59461297443069,0.6,12.2969132923658));
#15407=CARTESIAN_POINT('Ctrl Pts',(2.86376302967335,0.,12.3004008390612));
#15408=CARTESIAN_POINT('Ctrl Pts',(2.86376302967335,0.6,12.3004008390612));
#15409=CARTESIAN_POINT('Ctrl Pts',(3.10127560868576,0.,12.3010487961961));
#15410=CARTESIAN_POINT('Ctrl Pts',(3.10127560868576,0.6,12.3010487961961));
#15411=CARTESIAN_POINT('Ctrl Pts',(3.30884480305537,0.,12.2938762651102));
#15412=CARTESIAN_POINT('Ctrl Pts',(3.30884480305537,0.6,12.2938762651102));
#15413=CARTESIAN_POINT('Ctrl Pts',(3.48993681214337,0.,12.2723364229612));
#15414=CARTESIAN_POINT('Ctrl Pts',(3.48993681214337,0.6,12.2723364229612));
#15415=CARTESIAN_POINT('Ctrl Pts',(3.64927048315907,0.,12.2301117722792));
#15416=CARTESIAN_POINT('Ctrl Pts',(3.64927048315907,0.6,12.2301117722792));
#15417=CARTESIAN_POINT('Ctrl Pts',(3.79241297762162,0.,12.1626050652587));
#15418=CARTESIAN_POINT('Ctrl Pts',(3.79241297762162,0.6,12.1626050652587));
#15419=CARTESIAN_POINT('Ctrl Pts',(3.90811725944037,0.,12.0806818325567));
#15420=CARTESIAN_POINT('Ctrl Pts',(3.90811725944037,0.6,12.0806818325567));
#15421=CARTESIAN_POINT('Ctrl Pts',(3.99482565231275,0.,12.0046763352306));
#15422=CARTESIAN_POINT('Ctrl Pts',(3.99482565231275,0.6,12.0046763352306));
#15423=CARTESIAN_POINT('Ctrl Pts',(4.05565687163378,0.,11.9465013108382));
#15424=CARTESIAN_POINT('Ctrl Pts',(4.05565687163378,0.6,11.9465013108382));
#15425=CARTESIAN_POINT('Ctrl Pts',(4.09081961446015,0.,11.9117811315284));
#15426=CARTESIAN_POINT('Ctrl Pts',(4.09081961446015,0.6,11.9117811315284));
#15427=CARTESIAN_POINT('Ctrl Pts',(4.09999999999981,0.,11.9026515720696));
#15428=CARTESIAN_POINT('Ctrl Pts',(4.09999999999981,0.6,11.9026515720696));
#15429=CARTESIAN_POINT('',(-4.09999999999981,0.08,11.9026515720685));
#15430=CARTESIAN_POINT('',(-4.1,0.,11.9026515720683));
#15431=CARTESIAN_POINT('',(4.0999999999999,0.08,11.9026515720696));
#15432=CARTESIAN_POINT('Ctrl Pts',(4.09999999999981,0.08,11.9026515720696));
#15433=CARTESIAN_POINT('Ctrl Pts',(4.08085111799688,0.08,11.9216944386311));
#15434=CARTESIAN_POINT('Ctrl Pts',(4.06101542096552,0.08,11.9410853975879));
#15435=CARTESIAN_POINT('Ctrl Pts',(4.04073585097501,0.08,11.9603045561526));
#15436=CARTESIAN_POINT('Ctrl Pts',(4.02436441134365,0.08,11.97581993909));
#15437=CARTESIAN_POINT('Ctrl Pts',(4.00770239235104,0.08,11.9912224049274));
#15438=CARTESIAN_POINT('Ctrl Pts',(3.99086144408298,0.08,12.0062594906044));
#15439=CARTESIAN_POINT('Ctrl Pts',(3.98153193750382,0.08,12.0145896978778));
#15440=CARTESIAN_POINT('Ctrl Pts',(3.97215358351719,0.08,12.0228031793437));
#15441=CARTESIAN_POINT('Ctrl Pts',(3.96270172391276,0.08,12.0308975945789));
#15442=CARTESIAN_POINT('Ctrl Pts',(3.94584705089436,0.08,12.045331655999));
#15443=CARTESIAN_POINT('Ctrl Pts',(3.92875556290024,0.08,12.0593923164246));
#15444=CARTESIAN_POINT('Ctrl Pts',(3.91125351666559,0.08,12.0730677817931));
#15445=CARTESIAN_POINT('Ctrl Pts',(3.89832363377578,0.08,12.0831707242324));
#15446=CARTESIAN_POINT('Ctrl Pts',(3.8851694742044,0.08,12.0930629305754));
#15447=CARTESIAN_POINT('Ctrl Pts',(3.87171397149225,0.08,12.102730041241));
#15448=CARTESIAN_POINT('Ctrl Pts',(3.8614190416025,0.08,12.1101264372485));
#15449=CARTESIAN_POINT('Ctrl Pts',(3.85094099847984,0.08,12.1173949809926));
#15450=CARTESIAN_POINT('Ctrl Pts',(3.84027953928806,0.08,12.12450190652));
#15451=CARTESIAN_POINT('Ctrl Pts',(3.82175706889362,0.08,12.136848979778));
#15452=CARTESIAN_POINT('Ctrl Pts',(3.80268700852572,0.08,12.1487003513866));
#15453=CARTESIAN_POINT('Ctrl Pts',(3.78310122932964,0.08,12.1598936311512));
#15454=CARTESIAN_POINT('Ctrl Pts',(3.76586254638967,0.08,12.1697455445721));
#15455=CARTESIAN_POINT('Ctrl Pts',(3.74822395968075,0.08,12.1790882008887));
#15456=CARTESIAN_POINT('Ctrl Pts',(3.73021120715776,0.08,12.1878507821834));
#15457=CARTESIAN_POINT('Ctrl Pts',(3.71288220522445,0.08,12.1962807424575));
#15458=CARTESIAN_POINT('Ctrl Pts',(3.69520648253534,0.08,12.2041725145781));
#15459=CARTESIAN_POINT('Ctrl Pts',(3.6772807651628,0.08,12.2114752670303));
#15460=CARTESIAN_POINT('Ctrl Pts',(3.6591356399706,0.08,12.2188674039663));
#15461=CARTESIAN_POINT('Ctrl Pts',(3.64073365439416,0.08,12.2256564236659));
#15462=CARTESIAN_POINT('Ctrl Pts',(3.62219995454964,0.08,12.2318367403961));
#15463=CARTESIAN_POINT('Ctrl Pts',(3.6080919145163,0.08,12.2365412600861));
#15464=CARTESIAN_POINT('Ctrl Pts',(3.59390804694076,0.08,12.2408941383227));
#15465=CARTESIAN_POINT('Ctrl Pts',(3.57971589417065,0.08,12.2449082304703));
#15466=CARTESIAN_POINT('Ctrl Pts',(3.56437379192782,0.08,12.2492475730026));
#15467=CARTESIAN_POINT('Ctrl Pts',(3.54903220918601,0.08,12.2531896473898));
#15468=CARTESIAN_POINT('Ctrl Pts',(3.5336945114111,0.08,12.2567838613074));
#15469=CARTESIAN_POINT('Ctrl Pts',(3.50554417223935,0.08,12.2633805710823));
#15470=CARTESIAN_POINT('Ctrl Pts',(3.47740156491547,0.08,12.2688092691411));
#15471=CARTESIAN_POINT('Ctrl Pts',(3.44929127767962,0.08,12.2733508469725));
#15472=CARTESIAN_POINT('Ctrl Pts',(3.4208806380215,0.08,12.2779409505942));
#15473=CARTESIAN_POINT('Ctrl Pts',(3.39250369100482,0.08,12.2816252157076));
#15474=CARTESIAN_POINT('Ctrl Pts',(3.364210072182,0.08,12.2846455979633));
#15475=CARTESIAN_POINT('Ctrl Pts',(3.34067447290198,0.08,12.2871580551675));
#15476=CARTESIAN_POINT('Ctrl Pts',(3.31719712358888,0.08,12.2892101937693));
#15477=CARTESIAN_POINT('Ctrl Pts',(3.29381437654729,0.08,12.2909154727553));
#15478=CARTESIAN_POINT('Ctrl Pts',(3.26990846383811,0.08,12.2926589056595));
#15479=CARTESIAN_POINT('Ctrl Pts',(3.24611026789158,0.08,12.2940396163213));
#15480=CARTESIAN_POINT('Ctrl Pts',(3.22239636521847,0.08,12.2951574602113));
#15481=CARTESIAN_POINT('Ctrl Pts',(3.19272700000078,0.08,12.2965560372015));
#15482=CARTESIAN_POINT('Ctrl Pts',(3.16319729337309,0.08,12.2975435340936));
#15483=CARTESIAN_POINT('Ctrl Pts',(3.13378818621321,0.08,12.2982614632568));
#15484=CARTESIAN_POINT('Ctrl Pts',(3.10291902762736,0.08,12.2990150348996));
#15485=CARTESIAN_POINT('Ctrl Pts',(3.07218325518306,0.08,12.2994710273203));
#15486=CARTESIAN_POINT('Ctrl Pts',(3.04153322298808,0.08,12.2997413666759));
#15487=CARTESIAN_POINT('Ctrl Pts',(3.01414756926293,0.08,12.2999829135667));
#15488=CARTESIAN_POINT('Ctrl Pts',(2.98683142537097,0.08,12.3000750815676));
#15489=CARTESIAN_POINT('Ctrl Pts',(2.95952635057301,0.08,12.3000718531387));
#15490=CARTESIAN_POINT('Ctrl Pts',(2.92022752887084,0.08,12.3000672066233));
#15491=CARTESIAN_POINT('Ctrl Pts',(2.88094163407949,0.08,12.2998660100441));
#15492=CARTESIAN_POINT('Ctrl Pts',(2.84171310121476,0.08,12.299573016108));
#15493=CARTESIAN_POINT('Ctrl Pts',(2.80046664143214,0.08,12.2992649504803));
#15494=CARTESIAN_POINT('Ctrl Pts',(2.75928426917026,0.08,12.2988543578822));
#15495=CARTESIAN_POINT('Ctrl Pts',(2.71818210888147,0.08,12.2984132059186));
#15496=CARTESIAN_POINT('Ctrl Pts',(2.67559761222298,0.08,12.2979561439494));
#15497=CARTESIAN_POINT('Ctrl Pts',(2.63309961275455,0.08,12.2974652765352));
#15498=CARTESIAN_POINT('Ctrl Pts',(2.59066040545446,0.08,12.2969852179935));
#15499=CARTESIAN_POINT('Ctrl Pts',(2.54700739090149,0.08,12.296491429258));
#15500=CARTESIAN_POINT('Ctrl Pts',(2.50341670354419,0.08,12.2960083404301));
#15501=CARTESIAN_POINT('Ctrl Pts',(2.45980678945122,0.08,12.2955613475654));
#15502=CARTESIAN_POINT('Ctrl Pts',(2.43495747913403,0.08,12.2953066471231));
#15503=CARTESIAN_POINT('Ctrl Pts',(2.41010097941813,0.08,12.2950633182646));
#15504=CARTESIAN_POINT('Ctrl Pts',(2.38521498311308,0.08,12.2948339814447));
#15505=CARTESIAN_POINT('Ctrl Pts',(2.36524312905612,0.08,12.2946499308871));
#15506=CARTESIAN_POINT('Ctrl Pts',(2.3452529798216,0.08,12.2944748786647));
#15507=CARTESIAN_POINT('Ctrl Pts',(2.32525887175618,0.08,12.2943099103763));
#15508=CARTESIAN_POINT('Ctrl Pts',(2.26880377106821,0.08,12.2938441080859));
#15509=CARTESIAN_POINT('Ctrl Pts',(2.21229745148629,0.08,12.2934598053646));
#15510=CARTESIAN_POINT('Ctrl Pts',(2.15579643324432,0.08,12.2931645025908));
#15511=CARTESIAN_POINT('Ctrl Pts',(2.09783882688532,0.08,12.292861586954));
#15512=CARTESIAN_POINT('Ctrl Pts',(2.03988681065597,0.08,12.2926517251859));
#15513=CARTESIAN_POINT('Ctrl Pts',(1.98194864244373,0.08,12.2925287651092));
#15514=CARTESIAN_POINT('Ctrl Pts',(1.92220737766913,0.0800000000000001,
12.292401978386));
#15515=CARTESIAN_POINT('Ctrl Pts',(1.86248071190454,0.08,12.2923672037462));
#15516=CARTESIAN_POINT('Ctrl Pts',(1.80272313765481,0.08,12.2924103227315));
#15517=CARTESIAN_POINT('Ctrl Pts',(1.78236504214316,0.08,12.2924250124245));
#15518=CARTESIAN_POINT('Ctrl Pts',(1.76200320414501,0.08,12.2924487012689));
#15519=CARTESIAN_POINT('Ctrl Pts',(1.74162156320725,0.08,12.292480772058));
#15520=CARTESIAN_POINT('Ctrl Pts',(1.66485073951616,0.08,12.2926015719925));
#15521=CARTESIAN_POINT('Ctrl Pts',(1.5878674439253,0.08,12.2928417064317));
#15522=CARTESIAN_POINT('Ctrl Pts',(1.5108223052039,0.08,12.2931628749459));
#15523=CARTESIAN_POINT('Ctrl Pts',(1.43158637455503,0.08,12.2934931759427));
#15524=CARTESIAN_POINT('Ctrl Pts',(1.35228491570348,0.08,12.2939087355891));
#15525=CARTESIAN_POINT('Ctrl Pts',(1.27302549034632,0.0800000000000001,
12.2943660309377));
#15526=CARTESIAN_POINT('Ctrl Pts',(1.1905078550462,0.0800000000000001,12.2948421248613));
#15527=CARTESIAN_POINT('Ctrl Pts',(1.10803554212318,0.08,12.2953631505531));
#15528=CARTESIAN_POINT('Ctrl Pts',(1.02567235785951,0.08,12.2958839331962));
#15529=CARTESIAN_POINT('Ctrl Pts',(0.938539807628001,0.08,12.2964348725534));
#15530=CARTESIAN_POINT('Ctrl Pts',(0.851529016120771,0.0800000000000001,
12.2969853013965));
#15531=CARTESIAN_POINT('Ctrl Pts',(0.764656942700882,0.0800000000000001,
12.2974903879526));
#15532=CARTESIAN_POINT('Ctrl Pts',(0.670578247057742,0.0800000000000001,
12.2980373748324));
#15533=CARTESIAN_POINT('Ctrl Pts',(0.576661628618322,0.0800000000000001,
12.2985308796243));
#15534=CARTESIAN_POINT('Ctrl Pts',(0.482869249226626,0.0800000000000001,
12.2989282255145));
#15535=CARTESIAN_POINT('Ctrl Pts',(0.370835051600932,0.0800000000000001,
12.2994028517929));
#15536=CARTESIAN_POINT('Ctrl Pts',(0.258977105568546,0.08,12.2997390836903));
#15537=CARTESIAN_POINT('Ctrl Pts',(0.147160428731306,0.08,12.2998961675423));
#15538=CARTESIAN_POINT('Ctrl Pts',(0.0339191259990135,0.08,12.3000552527569));
#15539=CARTESIAN_POINT('Ctrl Pts',(-0.0792837384867833,0.08,12.3000297581724));
#15540=CARTESIAN_POINT('Ctrl Pts',(-0.192612106107584,0.08,12.2998226870296));
#15541=CARTESIAN_POINT('Ctrl Pts',(-0.274803209508849,0.08,12.2996725092226));
#15542=CARTESIAN_POINT('Ctrl Pts',(-0.357061036136113,0.08,12.2994280361329));
#15543=CARTESIAN_POINT('Ctrl Pts',(-0.439437867128799,0.08,12.2991053502863));
#15544=CARTESIAN_POINT('Ctrl Pts',(-0.48787066530124,0.08,12.2989156297265));
#15545=CARTESIAN_POINT('Ctrl Pts',(-0.536344351747438,0.08,12.2986990890481));
#15546=CARTESIAN_POINT('Ctrl Pts',(-0.584866221452301,0.08,12.2984607057927));
#15547=CARTESIAN_POINT('Ctrl Pts',(-0.601617610893425,0.08,12.2983784078357));
#15548=CARTESIAN_POINT('Ctrl Pts',(-0.618370748229175,0.08,12.2982935358771));
#15549=CARTESIAN_POINT('Ctrl Pts',(-0.635118395921561,0.08,12.2982063714116));
#15550=CARTESIAN_POINT('Ctrl Pts',(-0.7219687678754,0.08,12.2977543517373));
#15551=CARTESIAN_POINT('Ctrl Pts',(-0.808739990504138,0.08,12.2972395965865));
#15552=CARTESIAN_POINT('Ctrl Pts',(-0.895525604899384,0.08,12.2967016641001));
#15553=CARTESIAN_POINT('Ctrl Pts',(-0.976102388614265,0.08,12.296202216468));
#15554=CARTESIAN_POINT('Ctrl Pts',(-1.05669206509419,0.08,12.2956829345119));
#15555=CARTESIAN_POINT('Ctrl Pts',(-1.13732782725138,0.08,12.2951824199131));
#15556=CARTESIAN_POINT('Ctrl Pts',(-1.21395246397961,0.08,12.2947068027889));
#15557=CARTESIAN_POINT('Ctrl Pts',(-1.29061906065972,0.08,12.2942482785114));
#15558=CARTESIAN_POINT('Ctrl Pts',(-1.36731114548385,0.08,12.2938445261533));
#15559=CARTESIAN_POINT('Ctrl Pts',(-1.44126731795944,0.08,12.2934551772512));
#15560=CARTESIAN_POINT('Ctrl Pts',(-1.51524744450851,0.08,12.2931169858094));
#15561=CARTESIAN_POINT('Ctrl Pts',(-1.58918949676173,0.08,12.292865478377));
#15562=CARTESIAN_POINT('Ctrl Pts',(-1.64262457071585,0.08,12.2926837236402));
#15563=CARTESIAN_POINT('Ctrl Pts',(-1.69603879964548,0.08,12.2925473178858));
#15564=CARTESIAN_POINT('Ctrl Pts',(-1.74939155466375,0.08,12.2924689518492));
#15565=CARTESIAN_POINT('Ctrl Pts',(-1.81138702877719,0.08,12.2923778911421));
#15566=CARTESIAN_POINT('Ctrl Pts',(-1.87328650735159,0.08,12.292365329224));
#15567=CARTESIAN_POINT('Ctrl Pts',(-1.93518382952162,0.08,12.2924480139311));
#15568=CARTESIAN_POINT('Ctrl Pts',(-1.99201075404425,0.08,12.2925239254156));
#15569=CARTESIAN_POINT('Ctrl Pts',(-2.04883617969711,0.08,12.2926803633538));
#15570=CARTESIAN_POINT('Ctrl Pts',(-2.10568527146238,0.08,12.2929255258877));
#15571=CARTESIAN_POINT('Ctrl Pts',(-2.1610981357588,0.08,12.2931644946697));
#15572=CARTESIAN_POINT('Ctrl Pts',(-2.21653355338608,0.08,12.2934882052722));
#15573=CARTESIAN_POINT('Ctrl Pts',(-2.27196714524091,0.08,12.2938945384932));
#15574=CARTESIAN_POINT('Ctrl Pts',(-2.30462425317035,0.08,12.2941339180356));
#15575=CARTESIAN_POINT('Ctrl Pts',(-2.33727981008809,0.08,12.2944017716056));
#15576=CARTESIAN_POINT('Ctrl Pts',(-2.3699207434827,0.08,12.2946948402871));
#15577=CARTESIAN_POINT('Ctrl Pts',(-2.38860422091697,0.08,12.2948625910689));
#15578=CARTESIAN_POINT('Ctrl Pts',(-2.40727353322535,0.08,12.2950384715363));
#15579=CARTESIAN_POINT('Ctrl Pts',(-2.42593646929677,0.08,12.2952215184717));
#15580=CARTESIAN_POINT('Ctrl Pts',(-2.46915994082182,0.08,12.2956454562686));
#15581=CARTESIAN_POINT('Ctrl Pts',(-2.5123557613935,0.08,12.2961088688924));
#15582=CARTESIAN_POINT('Ctrl Pts',(-2.5556103407381,0.08,12.2965912298652));
#15583=CARTESIAN_POINT('Ctrl Pts',(-2.59761221637401,0.08,12.2970596210944));
#15584=CARTESIAN_POINT('Ctrl Pts',(-2.63966941763936,0.08,12.2975464435437));
#15585=CARTESIAN_POINT('Ctrl Pts',(-2.6818165243447,0.08,12.2980151918792));
#15586=CARTESIAN_POINT('Ctrl Pts',(-2.72230118964439,0.08,12.2984654510063));
#15587=CARTESIAN_POINT('Ctrl Pts',(-2.76286849091756,0.08,12.2988997761342));
#15588=CARTESIAN_POINT('Ctrl Pts',(-2.80351035458597,0.08,12.2992598559852));
#15589=CARTESIAN_POINT('Ctrl Pts',(-2.83665379540435,0.08,12.2995535011125));
#15590=CARTESIAN_POINT('Ctrl Pts',(-2.86984601586543,0.08,12.2997976670906));
#15591=CARTESIAN_POINT('Ctrl Pts',(-2.90306509578608,0.08,12.2999405884475));
#15592=CARTESIAN_POINT('Ctrl Pts',(-2.92537741132963,0.08,12.3000365846769));
#15593=CARTESIAN_POINT('Ctrl Pts',(-2.9477002227499,0.08,12.3000865234911));
#15594=CARTESIAN_POINT('Ctrl Pts',(-2.97002743072866,0.08,12.3000682165033));
#15595=CARTESIAN_POINT('Ctrl Pts',(-3.00130987000378,0.08,12.3000425667564));
#15596=CARTESIAN_POINT('Ctrl Pts',(-3.0326215472723,0.08,12.2998848748288));
#15597=CARTESIAN_POINT('Ctrl Pts',(-3.06403195826998,0.08,12.2995077488028));
#15598=CARTESIAN_POINT('Ctrl Pts',(-3.09393641998059,0.08,12.2991487038095));
#15599=CARTESIAN_POINT('Ctrl Pts',(-3.12392994078988,0.08,12.2985913743274));
#15600=CARTESIAN_POINT('Ctrl Pts',(-3.1540465763897,0.08,12.2977227341565));
#15601=CARTESIAN_POINT('Ctrl Pts',(-3.1815930910073,0.08,12.2969282227947));
#15602=CARTESIAN_POINT('Ctrl Pts',(-3.20924211628561,0.08,12.2958733738442));
#15603=CARTESIAN_POINT('Ctrl Pts',(-3.23700403466603,0.08,12.2944351369897));
#15604=CARTESIAN_POINT('Ctrl Pts',(-3.2562020509982,0.08,12.2934405625427));
#15605=CARTESIAN_POINT('Ctrl Pts',(-3.27545188943979,0.08,12.292262127272));
#15606=CARTESIAN_POINT('Ctrl Pts',(-3.2947674345378,0.08,12.2908457777182));
#15607=CARTESIAN_POINT('Ctrl Pts',(-3.32302318748729,0.08,12.2887738702013));
#15608=CARTESIAN_POINT('Ctrl Pts',(-3.35140672998653,0.08,12.286195650168));
#15609=CARTESIAN_POINT('Ctrl Pts',(-3.37986719282862,0.08,12.2829055722533));
#15610=CARTESIAN_POINT('Ctrl Pts',(-3.40775432368432,0.08,12.2796817724915));
#15611=CARTESIAN_POINT('Ctrl Pts',(-3.43571473452292,0.08,12.2757745092888));
#15612=CARTESIAN_POINT('Ctrl Pts',(-3.46371322028709,0.08,12.2709418264406));
#15613=CARTESIAN_POINT('Ctrl Pts',(-3.49160795780378,0.08,12.2661270510743));
#15614=CARTESIAN_POINT('Ctrl Pts',(-3.51953978424926,0.08,12.2603934176664));
#15615=CARTESIAN_POINT('Ctrl Pts',(-3.54749611690544,0.08,12.2534546098573));
#15616=CARTESIAN_POINT('Ctrl Pts',(-3.55919101099375,0.08,12.2505519178831));
#15617=CARTESIAN_POINT('Ctrl Pts',(-3.57089240832327,0.08,12.2474372356666));
#15618=CARTESIAN_POINT('Ctrl Pts',(-3.58259483305825,0.08,12.2440892798788));
#15619=CARTESIAN_POINT('Ctrl Pts',(-3.60123965610208,0.08,12.2387551679632));
#15620=CARTESIAN_POINT('Ctrl Pts',(-3.61986844142307,0.08,12.2328303885715));
#15621=CARTESIAN_POINT('Ctrl Pts',(-3.63832649186014,0.08,12.2262933590496));
#15622=CARTESIAN_POINT('Ctrl Pts',(-3.65649948761467,0.08,12.2198572833571));
#15623=CARTESIAN_POINT('Ctrl Pts',(-3.67450747348183,0.08,12.2128272165978));
#15624=CARTESIAN_POINT('Ctrl Pts',(-3.69223267685152,0.08,12.2052233154293));
#15625=CARTESIAN_POINT('Ctrl Pts',(-3.7080454670573,0.08,12.1984398167344));
#15626=CARTESIAN_POINT('Ctrl Pts',(-3.72363302436823,0.08,12.1912004677199));
#15627=CARTESIAN_POINT('Ctrl Pts',(-3.73892965687719,0.08,12.1835500857559));
#15628=CARTESIAN_POINT('Ctrl Pts',(-3.75806999941515,0.08,12.1739773297097));
#15629=CARTESIAN_POINT('Ctrl Pts',(-3.77676276852181,0.08,12.1637567909941));
#15630=CARTESIAN_POINT('Ctrl Pts',(-3.79496379833088,0.08,12.1529979906693));
#15631=CARTESIAN_POINT('Ctrl Pts',(-3.80952218159534,0.08,12.144392393061));
#15632=CARTESIAN_POINT('Ctrl Pts',(-3.82376633054058,0.08,12.1354436934871));
#15633=CARTESIAN_POINT('Ctrl Pts',(-3.83767573576978,0.08,12.1262319605201));
#15634=CARTESIAN_POINT('Ctrl Pts',(-3.84721444931906,0.08,12.1199147901871));
#15635=CARTESIAN_POINT('Ctrl Pts',(-3.85659570047497,0.08,12.1134744181737));
#15636=CARTESIAN_POINT('Ctrl Pts',(-3.86581281892743,0.08,12.1069412887918));
#15637=CARTESIAN_POINT('Ctrl Pts',(-3.88337947259145,0.08,12.0944899764009));
#15638=CARTESIAN_POINT('Ctrl Pts',(-3.9003657611309,0.08,12.0816969810865));
#15639=CARTESIAN_POINT('Ctrl Pts',(-3.91702061319308,0.08,12.0685360005523));
#15640=CARTESIAN_POINT('Ctrl Pts',(-3.9329721656094,0.08,12.0559307807606));
#15641=CARTESIAN_POINT('Ctrl Pts',(-3.94861886098581,0.08,12.0429872732068));
#15642=CARTESIAN_POINT('Ctrl Pts',(-3.96416210392647,0.08,12.0296455015386));
#15643=CARTESIAN_POINT('Ctrl Pts',(-3.971565740585,0.08,12.0232904808914));
#15644=CARTESIAN_POINT('Ctrl Pts',(-3.97894573577746,0.08,12.0168445998276));
#15645=CARTESIAN_POINT('Ctrl Pts',(-3.98632307325471,0.08,12.0102990077394));
#15646=CARTESIAN_POINT('Ctrl Pts',(-4.00248188436664,0.08,11.9959619943526));
#15647=CARTESIAN_POINT('Ctrl Pts',(-4.01860857072346,0.08,11.9811586329138));
#15648=CARTESIAN_POINT('Ctrl Pts',(-4.03449178471336,0.08,11.9662031341815));
#15649=CARTESIAN_POINT('Ctrl Pts',(-4.05281046348137,0.08,11.9489544226005));
#15650=CARTESIAN_POINT('Ctrl Pts',(-4.07080704435507,0.08,11.9315047769153));
#15651=CARTESIAN_POINT('Ctrl Pts',(-4.08813823052043,0.08,11.9144028720395));
#15652=CARTESIAN_POINT('Ctrl Pts',(-4.09212905724568,0.08,11.9104648415792));
#15653=CARTESIAN_POINT('Ctrl Pts',(-4.0960844664969,0.08,11.9065454276994));
#15654=CARTESIAN_POINT('Ctrl Pts',(-4.0999999999998,0.08,11.9026515720685));
#15655=CARTESIAN_POINT('',(4.1,0.,11.9026515720695));
#15656=CARTESIAN_POINT('Ctrl Pts',(-4.1,-3.,3.08701851589457));
#15657=CARTESIAN_POINT('Ctrl Pts',(-4.1,4.2,3.08701851589457));
#15658=CARTESIAN_POINT('Ctrl Pts',(-4.10321177777735,-3.,3.11273802327628));
#15659=CARTESIAN_POINT('Ctrl Pts',(-4.10321177777735,4.2,3.11273802327628));
#15660=CARTESIAN_POINT('Ctrl Pts',(-4.1120982065295,-3.,3.18044435652227));
#15661=CARTESIAN_POINT('Ctrl Pts',(-4.1120982065295,4.2,3.18044435652227));
#15662=CARTESIAN_POINT('Ctrl Pts',(-4.12837174871823,-3.,3.28931577678178));
#15663=CARTESIAN_POINT('Ctrl Pts',(-4.12837174871823,4.2,3.28931577678178));
#15664=CARTESIAN_POINT('Ctrl Pts',(-4.1558308051397,-3.,3.43759550531425));
#15665=CARTESIAN_POINT('Ctrl Pts',(-4.1558308051397,4.2,3.43759550531425));
#15666=CARTESIAN_POINT('Ctrl Pts',(-4.20184334854115,-3.,3.62185203209171));
#15667=CARTESIAN_POINT('Ctrl Pts',(-4.20184334854115,4.2,3.62185203209171));
#15668=CARTESIAN_POINT('Ctrl Pts',(-4.26765207024395,-3.,3.81399668859083));
#15669=CARTESIAN_POINT('Ctrl Pts',(-4.26765207024395,4.2,3.81399668859083));
#15670=CARTESIAN_POINT('Ctrl Pts',(-4.35148411330718,-3.,3.99681013615577));
#15671=CARTESIAN_POINT('Ctrl Pts',(-4.35148411330718,4.2,3.99681013615577));
#15672=CARTESIAN_POINT('Ctrl Pts',(-4.45474519640294,-3.,4.16885849319142));
#15673=CARTESIAN_POINT('Ctrl Pts',(-4.45474519640294,4.2,4.16885849319142));
#15674=CARTESIAN_POINT('Ctrl Pts',(-4.57800047823775,-3.,4.32911151507774));
#15675=CARTESIAN_POINT('Ctrl Pts',(-4.57800047823775,4.2,4.32911151507774));
#15676=CARTESIAN_POINT('Ctrl Pts',(-4.7208720035032,-3.,4.47714872481861));
#15677=CARTESIAN_POINT('Ctrl Pts',(-4.7208720035032,4.2,4.47714872481861));
#15678=CARTESIAN_POINT('Ctrl Pts',(-4.88190185104852,-3.,4.61340315498244));
#15679=CARTESIAN_POINT('Ctrl Pts',(-4.88190185104852,4.2,4.61340315498244));
#15680=CARTESIAN_POINT('Ctrl Pts',(-5.05850630701885,-3.,4.73929437247796));
#15681=CARTESIAN_POINT('Ctrl Pts',(-5.05850630701885,4.2,4.73929437247796));
#15682=CARTESIAN_POINT('Ctrl Pts',(-5.24741086000019,-3.,4.8567611153285));
#15683=CARTESIAN_POINT('Ctrl Pts',(-5.24741086000019,4.2,4.8567611153285));
#15684=CARTESIAN_POINT('Ctrl Pts',(-5.44501860313342,-3.,4.96787993373728));
#15685=CARTESIAN_POINT('Ctrl Pts',(-5.44501860313342,4.2,4.96787993373728));
#15686=CARTESIAN_POINT('Ctrl Pts',(-5.64781737380319,-3.,5.07442896098937));
#15687=CARTESIAN_POINT('Ctrl Pts',(-5.64781737380319,4.2,5.07442896098937));
#15688=CARTESIAN_POINT('Ctrl Pts',(-5.85274048349242,-3.,5.17752467829109));
#15689=CARTESIAN_POINT('Ctrl Pts',(-5.85274048349242,4.2,5.17752467829109));
#15690=CARTESIAN_POINT('Ctrl Pts',(-6.05762450882858,-3.,5.27709955371564));
#15691=CARTESIAN_POINT('Ctrl Pts',(-6.05762450882858,4.2,5.27709955371564));
#15692=CARTESIAN_POINT('Ctrl Pts',(-6.26112587698772,-3.,5.37226655127787));
#15693=CARTESIAN_POINT('Ctrl Pts',(-6.26112587698772,4.2,5.37226655127787));
#15694=CARTESIAN_POINT('Ctrl Pts',(-6.46246210121964,-3.,5.46195513100446));
#15695=CARTESIAN_POINT('Ctrl Pts',(-6.46246210121964,4.2,5.46195513100446));
#15696=CARTESIAN_POINT('Ctrl Pts',(-6.66121503090592,-3.,5.54547963906637));
#15697=CARTESIAN_POINT('Ctrl Pts',(-6.66121503090592,4.2,5.54547963906637));
#15698=CARTESIAN_POINT('Ctrl Pts',(-6.8570997603751,-3.,5.62308582598972));
#15699=CARTESIAN_POINT('Ctrl Pts',(-6.8570997603751,4.2,5.62308582598972));
#15700=CARTESIAN_POINT('Ctrl Pts',(-7.04976847947249,-3.,5.69662713609756));
#15701=CARTESIAN_POINT('Ctrl Pts',(-7.04976847947249,4.2,5.69662713609756));
#15702=CARTESIAN_POINT('Ctrl Pts',(-7.23853768475,-3.,5.76979878895672));
#15703=CARTESIAN_POINT('Ctrl Pts',(-7.23853768475,4.2,5.76979878895672));
#15704=CARTESIAN_POINT('Ctrl Pts',(-7.42198551710617,-3.,5.84723737025949));
#15705=CARTESIAN_POINT('Ctrl Pts',(-7.42198551710617,4.2,5.84723737025949));
#15706=CARTESIAN_POINT('Ctrl Pts',(-7.59751903688412,-3.,5.93381436957244));
#15707=CARTESIAN_POINT('Ctrl Pts',(-7.59751903688412,4.2,5.93381436957244));
#15708=CARTESIAN_POINT('Ctrl Pts',(-7.76106756457753,-3.,6.03389995867283));
#15709=CARTESIAN_POINT('Ctrl Pts',(-7.76106756457753,4.2,6.03389995867283));
#15710=CARTESIAN_POINT('Ctrl Pts',(-7.90644860448901,-3.,6.15052660592937));
#15711=CARTESIAN_POINT('Ctrl Pts',(-7.90644860448901,4.2,6.15052660592937));
#15712=CARTESIAN_POINT('Ctrl Pts',(-8.02580908828117,-3.,6.28498018271686));
#15713=CARTESIAN_POINT('Ctrl Pts',(-8.02580908828117,4.2,6.28498018271686));
#15714=CARTESIAN_POINT('Ctrl Pts',(-8.11207116917861,-3.,6.43720976255636));
#15715=CARTESIAN_POINT('Ctrl Pts',(-8.11207116917861,4.2,6.43720976255636));
#15716=CARTESIAN_POINT('Ctrl Pts',(-8.16089752265956,-3.,6.60605451948903));
#15717=CARTESIAN_POINT('Ctrl Pts',(-8.16089752265956,4.2,6.60605451948903));
#15718=CARTESIAN_POINT('Ctrl Pts',(-8.17293082304181,-3.,6.78954489191904));
#15719=CARTESIAN_POINT('Ctrl Pts',(-8.17293082304181,4.2,6.78954489191904));
#15720=CARTESIAN_POINT('Ctrl Pts',(-8.15569042861244,-3.,6.9851692342788));
#15721=CARTESIAN_POINT('Ctrl Pts',(-8.15569042861244,4.2,6.9851692342788));
#15722=CARTESIAN_POINT('Ctrl Pts',(-8.12057943633387,-3.,7.19009032473164));
#15723=CARTESIAN_POINT('Ctrl Pts',(-8.12057943633387,4.2,7.19009032473164));
#15724=CARTESIAN_POINT('Ctrl Pts',(-8.08008348678073,-3.,7.40136016279791));
#15725=CARTESIAN_POINT('Ctrl Pts',(-8.08008348678073,4.2,7.40136016279791));
#15726=CARTESIAN_POINT('Ctrl Pts',(-8.04494633492831,-3.,7.61613341658677));
#15727=CARTESIAN_POINT('Ctrl Pts',(-8.04494633492831,4.2,7.61613341658677));
#15728=CARTESIAN_POINT('Ctrl Pts',(-8.02124364536279,-3.,7.83188673232793));
#15729=CARTESIAN_POINT('Ctrl Pts',(-8.02124364536279,4.2,7.83188673232793));
#15730=CARTESIAN_POINT('Ctrl Pts',(-8.007818938056,-3.,8.04662057355248));
#15731=CARTESIAN_POINT('Ctrl Pts',(-8.007818938056,4.2,8.04662057355248));
#15732=CARTESIAN_POINT('Ctrl Pts',(-7.99879843919661,-3.,8.25883677791483));
#15733=CARTESIAN_POINT('Ctrl Pts',(-7.99879843919661,4.2,8.25883677791483));
#15734=CARTESIAN_POINT('Ctrl Pts',(-7.98575825096101,-3.,8.46752658699528));
#15735=CARTESIAN_POINT('Ctrl Pts',(-7.98575825096101,4.2,8.46752658699528));
#15736=CARTESIAN_POINT('Ctrl Pts',(-7.96007609558389,-3.,8.67216210283896));
#15737=CARTESIAN_POINT('Ctrl Pts',(-7.96007609558389,4.2,8.67216210283896));
#15738=CARTESIAN_POINT('Ctrl Pts',(-7.91508259073019,-3.,8.87266947141823));
#15739=CARTESIAN_POINT('Ctrl Pts',(-7.91508259073019,4.2,8.87266947141823));
#15740=CARTESIAN_POINT('Ctrl Pts',(-7.84862074946261,-3.,9.06945407016992));
#15741=CARTESIAN_POINT('Ctrl Pts',(-7.84862074946261,4.2,9.06945407016992));
#15742=CARTESIAN_POINT('Ctrl Pts',(-7.76209282457479,-3.,9.26297089919765));
#15743=CARTESIAN_POINT('Ctrl Pts',(-7.76209282457479,4.2,9.26297089919765));
#15744=CARTESIAN_POINT('Ctrl Pts',(-7.65900038660722,-3.,9.4532499945042));
#15745=CARTESIAN_POINT('Ctrl Pts',(-7.65900038660722,4.2,9.4532499945042));
#15746=CARTESIAN_POINT('Ctrl Pts',(-7.5436057352653,-3.,9.63939026966035));
#15747=CARTESIAN_POINT('Ctrl Pts',(-7.5436057352653,4.2,9.63939026966035));
#15748=CARTESIAN_POINT('Ctrl Pts',(-7.41967047355001,-3.,9.81917361987397));
#15749=CARTESIAN_POINT('Ctrl Pts',(-7.41967047355001,4.2,9.81917361987397));
#15750=CARTESIAN_POINT('Ctrl Pts',(-7.28883796912703,-3.,9.98835756998572));
#15751=CARTESIAN_POINT('Ctrl Pts',(-7.28883796912703,4.2,9.98835756998572));
#15752=CARTESIAN_POINT('Ctrl Pts',(-7.15081550722306,-3.,10.1414720974148));
#15753=CARTESIAN_POINT('Ctrl Pts',(-7.15081550722306,4.2,10.1414720974148));
#15754=CARTESIAN_POINT('Ctrl Pts',(-7.0044544864105,-3.,10.2733319413008));
#15755=CARTESIAN_POINT('Ctrl Pts',(-7.0044544864105,4.2,10.2733319413008));
#15756=CARTESIAN_POINT('Ctrl Pts',(-6.84859008776113,-3.,10.3804015453596));
#15757=CARTESIAN_POINT('Ctrl Pts',(-6.84859008776113,4.2,10.3804015453596));
#15758=CARTESIAN_POINT('Ctrl Pts',(-6.68288828293938,-3.,10.4620502678778));
#15759=CARTESIAN_POINT('Ctrl Pts',(-6.68288828293938,4.2,10.4620502678778));
#15760=CARTESIAN_POINT('Ctrl Pts',(-6.50892555577766,-3.,10.522290883026));
#15761=CARTESIAN_POINT('Ctrl Pts',(-6.50892555577766,4.2,10.522290883026));
#15762=CARTESIAN_POINT('Ctrl Pts',(-6.32976796473811,-3.,10.5687216653902));
#15763=CARTESIAN_POINT('Ctrl Pts',(-6.32976796473811,4.2,10.5687216653902));
#15764=CARTESIAN_POINT('Ctrl Pts',(-6.14893768388701,-3.,10.6103475969885));
#15765=CARTESIAN_POINT('Ctrl Pts',(-6.14893768388701,4.2,10.6103475969885));
#15766=CARTESIAN_POINT('Ctrl Pts',(-5.96961932707142,-3.,10.6558377434043));
#15767=CARTESIAN_POINT('Ctrl Pts',(-5.96961932707142,4.2,10.6558377434043));
#15768=CARTESIAN_POINT('Ctrl Pts',(-5.79367695415031,-3.,10.7114411549114));
#15769=CARTESIAN_POINT('Ctrl Pts',(-5.79367695415031,4.2,10.7114411549114));
#15770=CARTESIAN_POINT('Ctrl Pts',(-5.62101499943431,-3.,10.7795199127535));
#15771=CARTESIAN_POINT('Ctrl Pts',(-5.62101499943431,4.2,10.7795199127535));
#15772=CARTESIAN_POINT('Ctrl Pts',(-5.45051506148982,-3.,10.8599381259737));
#15773=CARTESIAN_POINT('Ctrl Pts',(-5.45051506148982,4.2,10.8599381259737));
#15774=CARTESIAN_POINT('Ctrl Pts',(-5.28082876351929,-3.,10.9511663773826));
#15775=CARTESIAN_POINT('Ctrl Pts',(-5.28082876351929,4.2,10.9511663773826));
#15776=CARTESIAN_POINT('Ctrl Pts',(-5.11112998264616,-3.,11.0513704191329));
#15777=CARTESIAN_POINT('Ctrl Pts',(-5.11112998264616,4.2,11.0513704191329));
#15778=CARTESIAN_POINT('Ctrl Pts',(-4.94211773226973,-3.,11.1598106424589));
#15779=CARTESIAN_POINT('Ctrl Pts',(-4.94211773226973,4.2,11.1598106424589));
#15780=CARTESIAN_POINT('Ctrl Pts',(-4.77596612414951,-3.,11.2768795166235));
#15781=CARTESIAN_POINT('Ctrl Pts',(-4.77596612414951,4.2,11.2768795166235));
#15782=CARTESIAN_POINT('Ctrl Pts',(-4.61532593596946,-3.,11.4029224160731));
#15783=CARTESIAN_POINT('Ctrl Pts',(-4.61532593596946,4.2,11.4029224160731));
#15784=CARTESIAN_POINT('Ctrl Pts',(-4.46255574628757,-3.,11.5373242211527));
#15785=CARTESIAN_POINT('Ctrl Pts',(-4.46255574628757,4.2,11.5373242211527));
#15786=CARTESIAN_POINT('Ctrl Pts',(-4.3290607566988,-3.,11.6677566212747));
#15787=CARTESIAN_POINT('Ctrl Pts',(-4.3290607566988,4.2,11.6677566212747));
#15788=CARTESIAN_POINT('Ctrl Pts',(-4.22986670297865,-3.,11.7703786717728));
#15789=CARTESIAN_POINT('Ctrl Pts',(-4.22986670297865,4.2,11.7703786717728));
#15790=CARTESIAN_POINT('Ctrl Pts',(-4.15991130277621,-3.,11.842517268501));
#15791=CARTESIAN_POINT('Ctrl Pts',(-4.15991130277621,4.2,11.842517268501));
#15792=CARTESIAN_POINT('Ctrl Pts',(-4.11686402271798,-3.,11.8858809149481));
#15793=CARTESIAN_POINT('Ctrl Pts',(-4.11686402271798,4.2,11.8858809149481));
#15794=CARTESIAN_POINT('Ctrl Pts',(-4.1,-3.,11.9026515720683));
#15795=CARTESIAN_POINT('Ctrl Pts',(-4.1,4.2,11.9026515720683));
#15796=CARTESIAN_POINT('',(-4.15712386170579,0.0799999999999999,11.8450264384607));
#15797=CARTESIAN_POINT('Origin',(-4.01664557121473,1.77216539020708,11.7072473142283));
#15798=CARTESIAN_POINT('Ctrl Pts',(-4.0999999999998,0.08,11.9026515720685));
#15799=CARTESIAN_POINT('Ctrl Pts',(-4.11927627294061,0.08,11.8834820198536));
#15800=CARTESIAN_POINT('Ctrl Pts',(-4.13827843210557,0.08,11.8642474273099));
#15801=CARTESIAN_POINT('Ctrl Pts',(-4.15712386170576,0.08,11.8450264384607));
#15802=CARTESIAN_POINT('Ctrl Pts',(3.98763757557447,0.0893144327047665,
0.904932892569182));
#15803=CARTESIAN_POINT('Ctrl Pts',(3.98203476831165,0.080980516655767,0.901899655408594));
#15804=CARTESIAN_POINT('Ctrl Pts',(3.96967224365401,0.068894102459747,0.897500692078048));
#15805=CARTESIAN_POINT('Ctrl Pts',(3.94855499960848,0.0583913140546653,
0.893678342428863));
#15806=CARTESIAN_POINT('Ctrl Pts',(3.93547774845255,0.055477193409909,0.892617991958012));
#15807=CARTESIAN_POINT('Ctrl Pts',(3.9293765880439,0.0547985738896275,0.892371260600161));
#15808=CARTESIAN_POINT('Ctrl Pts',(3.98243005775679,0.0869928933912105,
0.916663912034212));
#15809=CARTESIAN_POINT('Ctrl Pts',(3.97744058496684,0.0790608728779208,
0.913329286844901));
#15810=CARTESIAN_POINT('Ctrl Pts',(3.96624502189315,0.0673244992554347,
0.908078805155286));
#15811=CARTESIAN_POINT('Ctrl Pts',(3.94633901956984,0.0568639390894838,
0.901649656409215));
#15812=CARTESIAN_POINT('Ctrl Pts',(3.93358166964479,0.0539712488488517,
0.898346678324299));
#15813=CARTESIAN_POINT('Ctrl Pts',(3.92751586915137,0.0536129422494931,
0.896239350875046));
#15814=CARTESIAN_POINT('Ctrl Pts',(3.97972958477838,0.0827272695427162,
0.929109421587075));
#15815=CARTESIAN_POINT('Ctrl Pts',(3.97493957450629,0.0750745480505631,
0.925223897697526));
#15816=CARTESIAN_POINT('Ctrl Pts',(3.96409914923351,0.0637718835013209,
0.918754898918153));
#15817=CARTESIAN_POINT('Ctrl Pts',(3.94450057092466,0.0540981768731819,
0.909481071136272));
#15818=CARTESIAN_POINT('Ctrl Pts',(3.93179086316711,0.0518251218281415,
0.903943073991344));
#15819=CARTESIAN_POINT('Ctrl Pts',(3.92569874356709,0.0520681029751514,
0.900018242283346));
#15820=CARTESIAN_POINT('Ctrl Pts',(3.97984798233949,0.0770101465833284,
0.94083226531257));
#15821=CARTESIAN_POINT('Ctrl Pts',(3.97479328383972,0.0694388470342489,
0.936335429667805));
#15822=CARTESIAN_POINT('Ctrl Pts',(3.96340956460396,0.0585229907363136,
0.928669651644793));
#15823=CARTESIAN_POINT('Ctrl Pts',(3.9431247884684,0.0502165408921483,0.916833416299925));
#15824=CARTESIAN_POINT('Ctrl Pts',(3.93014957889597,0.0490851008089254,
0.909289140537019));
#15825=CARTESIAN_POINT('Ctrl Pts',(3.92395044195663,0.0501855062839886,
0.903655465216232));
#15826=CARTESIAN_POINT('',(3.98750649384402,0.089362716860748,0.904960783852724));
#15827=CARTESIAN_POINT('',(3.97983671972002,0.0769932827027835,0.940822248119245));
#15828=CARTESIAN_POINT('Origin',(4.04916946954199,0.0413995564077306,0.922765214848074));
#15829=CARTESIAN_POINT('',(3.92397049706406,0.0501819523054353,0.903673683563879));
#15830=CARTESIAN_POINT('Ctrl Pts',(3.97983671972021,0.0769932826936726,
0.940822248137924));
#15831=CARTESIAN_POINT('Ctrl Pts',(3.9747831370112,0.0694291188139783,0.936328597068607));
#15832=CARTESIAN_POINT('Ctrl Pts',(3.96340310875481,0.0585203471189109,
0.92866588463502));
#15833=CARTESIAN_POINT('Ctrl Pts',(3.94313104090131,0.0502191012122621,
0.916837064615631));
#15834=CARTESIAN_POINT('Ctrl Pts',(3.93016357755921,0.049086322581369,0.909297279894274));
#15835=CARTESIAN_POINT('Ctrl Pts',(3.92397049706405,0.0501819523054367,
0.903673683563877));
#15836=CARTESIAN_POINT('',(3.929394405843,0.0548135766059198,0.892377353749379));
#15837=CARTESIAN_POINT('Origin',(3.9387684725109,-0.0223136011303559,0.873253054794691));
#15838=CARTESIAN_POINT('Ctrl Pts',(3.929394405843,0.0548135766059198,0.892377353749379));
#15839=CARTESIAN_POINT('Ctrl Pts',(3.93294284341525,0.0552167805124275,
0.892524159568853));
#15840=CARTESIAN_POINT('Ctrl Pts',(3.93664094497026,0.0558681664406091,
0.892761271875184));
#15841=CARTESIAN_POINT('Ctrl Pts',(3.94035177870644,0.0567901148977748,
0.893096851090279));
#15842=CARTESIAN_POINT('Ctrl Pts',(3.9430125834771,0.0574511859743905,0.893337473775081));
#15843=CARTESIAN_POINT('Ctrl Pts',(3.94567955148932,0.0582503453705328,
0.893628363566722));
#15844=CARTESIAN_POINT('Ctrl Pts',(3.94830258562972,0.0591802781982167,
0.89396684560707));
#15845=CARTESIAN_POINT('Ctrl Pts',(3.95411448629012,0.0612407459336948,
0.894716825930824));
#15846=CARTESIAN_POINT('Ctrl Pts',(3.95972301416291,0.0639386192551732,
0.895698385030791));
#15847=CARTESIAN_POINT('Ctrl Pts',(3.96496846008119,0.0672806009961073,
0.896914467460389));
#15848=CARTESIAN_POINT('Ctrl Pts',(3.9653920120109,0.0675504546629755,0.897012661983364));
#15849=CARTESIAN_POINT('Ctrl Pts',(3.96581317192551,0.0678245213626311,
0.897112391282691));
#15850=CARTESIAN_POINT('Ctrl Pts',(3.96623184176758,0.0681028114885871,
0.897213659854605));
#15851=CARTESIAN_POINT('Ctrl Pts',(3.96747264480673,0.0689275741042759,
0.897513787399455));
#15852=CARTESIAN_POINT('Ctrl Pts',(3.9686909782428,0.0697890488164992,0.897827314561264));
#15853=CARTESIAN_POINT('Ctrl Pts',(3.96988312090337,0.0706865001004049,
0.898154007323679));
#15854=CARTESIAN_POINT('Ctrl Pts',(3.97453898522749,0.0741914593251504,
0.899429892524157));
#15855=CARTESIAN_POINT('Ctrl Pts',(3.97879291378003,0.0782485705570666,
0.900907911202756));
#15856=CARTESIAN_POINT('Ctrl Pts',(3.98252105307226,0.0827084187352409,
0.902532503084932));
#15857=CARTESIAN_POINT('Ctrl Pts',(3.98430255563518,0.084839570587914,0.903308819197324));
#15858=CARTESIAN_POINT('Ctrl Pts',(3.98596444849724,0.0870620466537864,
0.904118357281442));
#15859=CARTESIAN_POINT('Ctrl Pts',(3.98749614255641,0.089356831788631,0.90495397253418));
#15860=CARTESIAN_POINT('Ctrl Pts',(3.99995017471379,0.126799874999198,0.918578169368801));
#15861=CARTESIAN_POINT('Ctrl Pts',(3.99944986938898,0.11348851535217,0.913733230679671));
#15862=CARTESIAN_POINT('Ctrl Pts',(3.99505715576901,0.100344093242609,0.90894905228516));
#15863=CARTESIAN_POINT('Ctrl Pts',(3.98762439168473,0.0892955579769557,
0.904927714316222));
#15864=CARTESIAN_POINT('Ctrl Pts',(3.99313598197604,0.122218533523161,0.930421158791107));
#15865=CARTESIAN_POINT('Ctrl Pts',(3.99279640530477,0.109784526212468,0.925839927766699));
#15866=CARTESIAN_POINT('Ctrl Pts',(3.98903809825174,0.0974908830262579,
0.921079001953896));
#15867=CARTESIAN_POINT('Ctrl Pts',(3.98241869839885,0.0869748432979465,
0.916657600142957));
#15868=CARTESIAN_POINT('Ctrl Pts',(3.98984275968184,0.116883323642803,0.943973826544633));
#15869=CARTESIAN_POINT('Ctrl Pts',(3.98959331650047,0.104765282119502,0.939370198048702));
#15870=CARTESIAN_POINT('Ctrl Pts',(3.98607384319811,0.0928557239444475,
0.934253508985834));
#15871=CARTESIAN_POINT('Ctrl Pts',(3.97971891715341,0.0827099677051683,
0.929101291873573));
#15872=CARTESIAN_POINT('Ctrl Pts',(3.99053121895996,0.111540623934062,0.957340198321923));
#15873=CARTESIAN_POINT('Ctrl Pts',(3.99028017432925,0.0991190831119013,
0.952466190557957));
#15874=CARTESIAN_POINT('Ctrl Pts',(3.98654272619743,0.0870307818092068,
0.946785236162934));
#15875=CARTESIAN_POINT('Ctrl Pts',(3.97983671972021,0.0769932826936736,
0.940822248137926));
#15876=CARTESIAN_POINT('',(3.99994696244202,0.126799890819684,0.918578279225942));
#15877=CARTESIAN_POINT('',(3.99053121895996,0.111540623934062,0.957340198321923));
#15878=CARTESIAN_POINT('Origin',(4.07042531154701,0.111540623934061,0.953225107837748));
#15879=CARTESIAN_POINT('Ctrl Pts',(3.99053121895996,0.111540623934062,0.957340198321923));
#15880=CARTESIAN_POINT('Ctrl Pts',(3.99028017432925,0.0991190831119013,
0.952466190557957));
#15881=CARTESIAN_POINT('Ctrl Pts',(3.98654272619743,0.0870307818092068,
0.946785236162934));
#15882=CARTESIAN_POINT('Ctrl Pts',(3.97983671972021,0.0769932826936736,
0.940822248137926));
#15883=CARTESIAN_POINT('Origin',(3.9367321686135,0.121247013319355,0.916540496718191));
#15884=CARTESIAN_POINT('Ctrl Pts',(3.92939607642122,0.0548006123101191,
0.892372580860866));
#15885=CARTESIAN_POINT('Ctrl Pts',(3.92634388981074,0.0544603574102712,
0.892248738205258));
#15886=CARTESIAN_POINT('Ctrl Pts',(3.92326758436874,0.0542854221831822,
0.892185066989672));
#15887=CARTESIAN_POINT('Ctrl Pts',(3.92012020332128,0.0542767513583031,
0.892181911067511));
#15888=CARTESIAN_POINT('Ctrl Pts',(3.92004146981349,0.0542766412926813,
0.892181871006901));
#15889=CARTESIAN_POINT('Ctrl Pts',(3.9199627360209,0.0542766412926813,0.892181871006901));
#15890=CARTESIAN_POINT('Ctrl Pts',(3.92753533006471,0.0536139664579581,
0.896246505841524));
#15891=CARTESIAN_POINT('Ctrl Pts',(3.92511894507891,0.05359185050338,0.894857113199761));
#15892=CARTESIAN_POINT('Ctrl Pts',(3.92263409808172,0.0538017795257374,
0.893523976721591));
#15893=CARTESIAN_POINT('Ctrl Pts',(3.92009002060122,0.0542535960747209,
0.892245667428479));
#15894=CARTESIAN_POINT('Ctrl Pts',(3.92002637871827,0.0542650414753612,
0.892213741243058));
#15895=CARTESIAN_POINT('Ctrl Pts',(3.9199627360209,0.0542766412926813,0.892181871006901));
#15896=CARTESIAN_POINT('Ctrl Pts',(3.92571837401383,0.0520672372167076,
0.900031098340516));
#15897=CARTESIAN_POINT('Ctrl Pts',(3.92389518151557,0.0525997003708216,
0.89742148095101));
#15898=CARTESIAN_POINT('Ctrl Pts',(3.92200062309269,0.0533123669048904,
0.894860812183919));
#15899=CARTESIAN_POINT('Ctrl Pts',(3.92005983815835,0.0542303656386634,
0.892309396431305));
#15900=CARTESIAN_POINT('Ctrl Pts',(3.92001128762305,0.054253441658041,0.892245611479215));
#15901=CARTESIAN_POINT('Ctrl Pts',(3.9199627360209,0.0542766412926813,0.892181871006901));
#15902=CARTESIAN_POINT('Ctrl Pts',(3.92397049706405,0.0501819523054441,
0.903673683563853));
#15903=CARTESIAN_POINT('Ctrl Pts',(3.92267324571416,0.0514837668071902,
0.899940280902761));
#15904=CARTESIAN_POINT('Ctrl Pts',(3.92136717122144,0.0528172498522682,
0.896195564980704));
#15905=CARTESIAN_POINT('Ctrl Pts',(3.92002965606137,0.054207059082659,0.892373097632133));
#15906=CARTESIAN_POINT('Ctrl Pts',(3.91999619652783,0.0542418418407209,
0.892277481715372));
#15907=CARTESIAN_POINT('Ctrl Pts',(3.9199627360209,0.0542766412926813,0.892181871006901));
#15908=CARTESIAN_POINT('',(3.91996276391134,0.0542766409928811,0.892181871823741));
#15909=CARTESIAN_POINT('Origin',(3.89398158889879,0.447015786354718,1.02337823064183));
#15910=CARTESIAN_POINT('Origin',(3.91993477835724,0.128120482093708,0.919068001247204));
#15911=CARTESIAN_POINT('Ctrl Pts',(4.,0.129452050955555,0.919543482472952));
#15912=CARTESIAN_POINT('Ctrl Pts',(4.,0.128568366080467,0.919221847481949));
#15913=CARTESIAN_POINT('Ctrl Pts',(3.99998336677459,0.127682998637521,0.918899600086328));
#15914=CARTESIAN_POINT('Ctrl Pts',(3.99995017471379,0.126799874999197,0.918578169368801));
#15915=CARTESIAN_POINT('Ctrl Pts',(3.99320174100155,0.125572492169931,0.931636190695047));
#15916=CARTESIAN_POINT('Ctrl Pts',(3.99318664336971,0.124450242215544,0.931244569432182));
#15917=CARTESIAN_POINT('Ctrl Pts',(3.99316471933781,0.123330766671213,0.930839013626173));
#15918=CARTESIAN_POINT('Ctrl Pts',(3.99313598197604,0.122218533523161,0.930421158791108));
#15919=CARTESIAN_POINT('Ctrl Pts',(3.98992351495583,0.121055159551916,0.945479161641182));
#15920=CARTESIAN_POINT('Ctrl Pts',(3.98989830405354,0.119653684370202,0.945009099951952));
#15921=CARTESIAN_POINT('Ctrl Pts',(3.98987138440309,0.118261520219538,0.944506745566704));
#15922=CARTESIAN_POINT('Ctrl Pts',(3.98984275968184,0.116883323642802,0.943973826544634));
#15923=CARTESIAN_POINT('Ctrl Pts',(3.99062355969946,0.116531496051876,0.959137393584632));
#15924=CARTESIAN_POINT('Ctrl Pts',(3.99059540935326,0.114850322896056,0.958588165894169));
#15925=CARTESIAN_POINT('Ctrl Pts',(3.9905646125374,0.11318519078342,0.957988531469827));
#15926=CARTESIAN_POINT('Ctrl Pts',(3.99053121895996,0.111540623934061,0.957340198321925));
#15927=CARTESIAN_POINT('',(4.,0.129452050955555,0.919543482472952));
#15928=CARTESIAN_POINT('Origin',(3.92338073148591,0.121553580080691,0.916815722371178));
#15929=CARTESIAN_POINT('',(3.99062355969947,0.116531496051876,0.959137393584632));
#15930=CARTESIAN_POINT('Origin',(4.07051868566465,0.116531496051876,0.955042415317635));
#15931=CARTESIAN_POINT('Origin',(3.98841540917197,0.128777749562786,0.917370672555525));
#15932=CARTESIAN_POINT('Ctrl Pts',(4.,0.524122951685637,1.06319194266973));
#15933=CARTESIAN_POINT('Ctrl Pts',(4.,0.392579508521167,1.01531404484498));
#15934=CARTESIAN_POINT('Ctrl Pts',(4.,0.261012992948574,0.967427749350433));
#15935=CARTESIAN_POINT('Ctrl Pts',(4.,0.129452050955556,0.919543482472952));
#15936=CARTESIAN_POINT('Ctrl Pts',(3.99722173585145,0.521464639036904,1.07150653805471));
#15937=CARTESIAN_POINT('Ctrl Pts',(3.99608172587457,0.389414444976033,1.02512218732467));
#15938=CARTESIAN_POINT('Ctrl Pts',(3.99478956593868,0.257458496604602,0.978440228041136));
#15939=CARTESIAN_POINT('Ctrl Pts',(3.99320174100156,0.125572492169931,0.931636190695047));
#15940=CARTESIAN_POINT('Ctrl Pts',(3.99595792658054,0.518642023625072,1.08027231824298));
#15941=CARTESIAN_POINT('Ctrl Pts',(3.99426602664426,0.385984032905188,1.03565889431257));
#15942=CARTESIAN_POINT('Ctrl Pts',(3.99232735107637,0.253495283774764,0.99057504228606));
#15943=CARTESIAN_POINT('Ctrl Pts',(3.98992351495583,0.121055159551917,0.945479161641181));
#15944=CARTESIAN_POINT('Ctrl Pts',(3.99628184601446,0.515818756594824,1.08898105602234));
#15945=CARTESIAN_POINT('Ctrl Pts',(3.99468731422838,0.38255220960787,1.04611126263635));
#15946=CARTESIAN_POINT('Ctrl Pts',(3.99285055050703,0.249530114845418,1.00258712627989));
#15947=CARTESIAN_POINT('Ctrl Pts',(3.99062355969947,0.116531496051877,0.959137393584631));
#15948=CARTESIAN_POINT('',(4.,0.524122951685637,1.06319194266973));
#15949=CARTESIAN_POINT('',(3.99628071248376,0.515724022809955,1.08895058147547));
#15950=CARTESIAN_POINT('Ctrl Pts',(4.,0.524122951685637,1.06319194266973));
#15951=CARTESIAN_POINT('Ctrl Pts',(3.9986089924126,0.522629326334401,1.06729564459538));
#15952=CARTESIAN_POINT('Ctrl Pts',(3.99759863687363,0.521165724744202,1.07152731239861));
#15953=CARTESIAN_POINT('Ctrl Pts',(3.99697497557878,0.519756336372472,1.07584372036492));
#15954=CARTESIAN_POINT('Ctrl Pts',(3.99635088558503,0.518345979200444,1.08016309538943));
#15955=CARTESIAN_POINT('Ctrl Pts',(3.99611691668579,0.516996538273542,1.084547162494));
#15956=CARTESIAN_POINT('Ctrl Pts',(3.99628071248508,0.515724022802589,1.08895058149858));
#15957=CARTESIAN_POINT('Ctrl Pts',(3.99628071248508,0.515724022802589,1.08895058149858));
#15958=CARTESIAN_POINT('Ctrl Pts',(3.99468644375212,0.382489169567759,1.04609063626742));
#15959=CARTESIAN_POINT('Ctrl Pts',(3.99285002281427,0.249498600387411,1.00257683072353));
#15960=CARTESIAN_POINT('Ctrl Pts',(3.99062355969947,0.116531496051877,0.959137393584631));
#15961=CARTESIAN_POINT('',(4.,0.0542766412926824,0.892181871006898));
#15962=CARTESIAN_POINT('Ctrl Pts',(3.99784434068601,0.000813388873467947,
1.16174107276121));
#15963=CARTESIAN_POINT('Ctrl Pts',(3.99784432727272,0.0008135747227017,
1.16174071881185));
#15964=CARTESIAN_POINT('Ctrl Pts',(3.9958522274879,0.00126345588851946,
1.15121922616146));
#15965=CARTESIAN_POINT('Ctrl Pts',(3.99078965828379,0.00281482454399863,
1.12710950869973));
#15966=CARTESIAN_POINT('Ctrl Pts',(3.98313335463591,0.00589478809278018,
1.0946626330386));
#15967=CARTESIAN_POINT('Ctrl Pts',(3.96225979086675,0.0168110800211123,
1.01686469965838));
#15968=CARTESIAN_POINT('Ctrl Pts',(3.94114259504174,0.0329494505434504,
0.953093833553903));
#15969=CARTESIAN_POINT('Ctrl Pts',(3.92397049706406,0.0501819523054334,
0.903673683563887));
#15970=CARTESIAN_POINT('Ctrl Pts',(3.9982278284976,0.000727245993550886,
1.16376965450937));
#15971=CARTESIAN_POINT('Ctrl Pts',(3.99822932035433,0.00181436044573403,
1.16381581953223));
#15972=CARTESIAN_POINT('Ctrl Pts',(3.99679023674084,0.00394535585146101,
1.15344065726723));
#15973=CARTESIAN_POINT('Ctrl Pts',(3.99313422044013,0.00741388714452286,
1.12958158728165));
#15974=CARTESIAN_POINT('Ctrl Pts',(3.98757564687094,0.0119616813045604,
1.09733717910204));
#15975=CARTESIAN_POINT('Ctrl Pts',(3.97223449897184,0.0244847572237893,
1.01956065811568));
#15976=CARTESIAN_POINT('Ctrl Pts',(3.95599704952542,0.0389933222701742,
0.954854087536785));
#15977=CARTESIAN_POINT('Ctrl Pts',(3.94181237515934,0.0536467548616993,
0.904095794994089));
#15978=CARTESIAN_POINT('Ctrl Pts',(3.99883736539415,0.000553542649297133,
1.16785724348145));
#15979=CARTESIAN_POINT('Ctrl Pts',(3.9988418299182,0.00382806012798106,
1.16799630117926));
#15980=CARTESIAN_POINT('Ctrl Pts',(3.99824607010187,0.00936410973956307,
1.15796429058724));
#15981=CARTESIAN_POINT('Ctrl Pts',(3.99675628178266,0.0169794272648916,
1.1347803839048));
#15982=CARTESIAN_POINT('Ctrl Pts',(3.99453093968089,0.0251577732975947,
1.10326524512036));
#15983=CARTESIAN_POINT('Ctrl Pts',(3.98837066180094,0.0436242941790727,
1.02669421700478));
#15984=CARTESIAN_POINT('Ctrl Pts',(3.98165970299104,0.0589291697315894,
0.961716549736144));
#15985=CARTESIAN_POINT('Ctrl Pts',(3.97502664104943,0.0722507173702981,
0.909843629936585));
#15986=CARTESIAN_POINT('Ctrl Pts',(3.99912832044927,0.000378790238046,1.17197973040507));
#15987=CARTESIAN_POINT('Ctrl Pts',(3.99913571708803,0.00585391903912836,
1.17221224354204));
#15988=CARTESIAN_POINT('Ctrl Pts',(3.99882664657299,0.0148542262907823,
1.16259013266621));
#15989=CARTESIAN_POINT('Ctrl Pts',(3.9980956580057,0.026941094118525,1.14028756032799));
#15990=CARTESIAN_POINT('Ctrl Pts',(3.99704746786599,0.0395222742335762,
1.10990521749973));
#15991=CARTESIAN_POINT('Ctrl Pts',(3.99432345688666,0.0669108953728227,
1.03597240480608));
#15992=CARTESIAN_POINT('Ctrl Pts',(3.99146441961465,0.0882021911235168,
0.973040771868915));
#15993=CARTESIAN_POINT('Ctrl Pts',(3.98866790214921,0.10584241001414,0.922799195037908));
#15994=CARTESIAN_POINT('Ctrl Pts',(3.99919371386846,0.000291414002863247,
1.1740435121275));
#15995=CARTESIAN_POINT('Ctrl Pts',(3.99920256193258,0.00686684929623559,
1.17432275235113));
#15996=CARTESIAN_POINT('Ctrl Pts',(3.99890451851341,0.0175976878297955,
1.16490897998439));
#15997=CARTESIAN_POINT('Ctrl Pts',(3.99819220127434,0.0319198582513071,
1.14305909112717));
#15998=CARTESIAN_POINT('Ctrl Pts',(3.99717818807624,0.0466981217662143,
1.11326101887131));
#15999=CARTESIAN_POINT('Ctrl Pts',(3.99451765518903,0.0785527702394917,
1.0407191721013));
#16000=CARTESIAN_POINT('Ctrl Pts',(3.99178846069233,0.10282206024219,0.978899329348002));
#16001=CARTESIAN_POINT('Ctrl Pts',(3.98904904336713,0.122677505741229,0.929651197081971));
#16002=CARTESIAN_POINT('',(3.99919381669006,0.00037425564854435,1.17404675699404));
#16003=CARTESIAN_POINT('Ctrl Pts',(3.99053162689604,0.111552033777857,0.957344809613607));
#16004=CARTESIAN_POINT('Ctrl Pts',(3.99259503042251,0.0954962439419094,
0.99739900732689));
#16005=CARTESIAN_POINT('Ctrl Pts',(3.99484994314364,0.0745742755413206,
1.04977930513061));
#16006=CARTESIAN_POINT('Ctrl Pts',(3.99717818807624,0.0466981217662143,
1.11326101887131));
#16007=CARTESIAN_POINT('Ctrl Pts',(3.99819220127434,0.0319198582513071,
1.14305909112717));
#16008=CARTESIAN_POINT('Ctrl Pts',(3.99890376983111,0.0176127411724394,
1.16488601461992));
#16009=CARTESIAN_POINT('Ctrl Pts',(3.99920130863952,0.00691194818962238,
1.17428316822488));
#16010=CARTESIAN_POINT('Ctrl Pts',(3.99919381710518,0.000374283339306366,
1.17404677002645));
#16011=CARTESIAN_POINT('',(3.99784430834598,0.000813481663902603,1.16174090062732));
#16012=CARTESIAN_POINT('Origin',(3.91983487919139,0.00718513856492471,1.17675789077508));
#16013=CARTESIAN_POINT('Ctrl Pts',(3.99784427600595,0.000813574454337259,
1.16174072849342));
#16014=CARTESIAN_POINT('Ctrl Pts',(3.99784273578734,0.000813920976441579,
1.16173258218817));
#16015=CARTESIAN_POINT('Ctrl Pts',(3.99784119332941,0.000814267840078317,
1.16172443633252));
#16016=CARTESIAN_POINT('Ctrl Pts',(3.99783965031257,0.000814614752868342,
1.16171629060187));
#16017=CARTESIAN_POINT('Ctrl Pts',(3.99783810729574,0.000814961665658368,
1.16170814487122));
#16018=CARTESIAN_POINT('Ctrl Pts',(3.9978365635392,0.000815308692277274,
1.16169999930219));
#16019=CARTESIAN_POINT('Ctrl Pts',(3.99783501934031,0.000815655834302155,
1.16169185383936));
#16020=CARTESIAN_POINT('Ctrl Pts',(3.99783193094253,0.000816350118351918,
1.16167556291369));
#16021=CARTESIAN_POINT('Ctrl Pts',(3.99782884075641,0.000817044867590349,
1.16165927241632));
#16022=CARTESIAN_POINT('Ctrl Pts',(3.99782574942695,0.000817740093563617,
1.16164298222655));
#16023=CARTESIAN_POINT('Ctrl Pts',(3.99781956676803,0.000819130545510153,
1.161610401847));
#16024=CARTESIAN_POINT('Ctrl Pts',(3.99781337941355,0.00082052164669327,
1.16157782264312));
#16025=CARTESIAN_POINT('Ctrl Pts',(3.99780720576951,0.000821928804838678,
1.16154533134384));
#16026=CARTESIAN_POINT('Ctrl Pts',(3.99779485848145,0.000824743121129494,
1.16148034874528));
#16027=CARTESIAN_POINT('Ctrl Pts',(3.99778250361156,0.000827582818338727,
1.16141539269024));
#16028=CARTESIAN_POINT('Ctrl Pts',(3.99777013683724,0.000830435889113772,
1.1613504218586));
#16029=CARTESIAN_POINT('Ctrl Pts',(3.9977234002965,0.000841218220467512,
1.16110488394862));
#16030=CARTESIAN_POINT('Ctrl Pts',(3.99767648280878,0.000852133710343159,
1.16085906292802));
#16031=CARTESIAN_POINT('Ctrl Pts',(3.99762845973455,0.000863380424841601,
1.16060793645995));
#16032=CARTESIAN_POINT('Ctrl Pts',(3.99756970142126,0.000877141267617072,
1.160300672339));
#16033=CARTESIAN_POINT('Ctrl Pts',(3.99751198108985,0.000890770026660122,
1.15999957986487));
#16034=CARTESIAN_POINT('Ctrl Pts',(3.99745532005822,0.000904237073150987,
1.15970459222681));
#16035=CARTESIAN_POINT('Ctrl Pts',(3.99741296186454,0.000914304658353342,
1.15948406776497));
#16036=CARTESIAN_POINT('Ctrl Pts',(3.99737009284839,0.000924544502561343,
1.1592612178845));
#16037=CARTESIAN_POINT('Ctrl Pts',(3.99732664050266,0.000934975402716219,
1.15903567313117));
#16038=CARTESIAN_POINT('Ctrl Pts',(3.99721602020136,0.00096153022498384,
1.15846148483017));
#16039=CARTESIAN_POINT('Ctrl Pts',(3.99710528340557,0.000988442107634933,
1.15788883833414));
#16040=CARTESIAN_POINT('Ctrl Pts',(3.99699448762094,0.00101568823936224,
1.15731795844143));
#16041=CARTESIAN_POINT('Ctrl Pts',(3.99683542048025,0.00105480492853115,
1.15649835837712));
#16042=CARTESIAN_POINT('Ctrl Pts',(3.99667448325672,0.00109504469120612,
1.15567341858394));
#16043=CARTESIAN_POINT('Ctrl Pts',(3.99651353174244,0.00113600838460423,
1.15485305488917));
#16044=CARTESIAN_POINT('Ctrl Pts',(3.99625082685399,0.00120286928089424,
1.15351405814923));
#16045=CARTESIAN_POINT('Ctrl Pts',(3.99598541481855,0.00127229923616561,
1.15217339875294));
#16046=CARTESIAN_POINT('Ctrl Pts',(3.99571743128359,0.0013449066789999,
1.15083588464134));
#16047=CARTESIAN_POINT('Ctrl Pts',(3.99519502051448,0.00148644862134294,
1.14822851633478));
#16048=CARTESIAN_POINT('Ctrl Pts',(3.99466155494466,0.00164050954618525,
1.1456272130292));
#16049=CARTESIAN_POINT('Ctrl Pts',(3.99411896967372,0.00180574117961086,
1.14303238119294));
#16050=CARTESIAN_POINT('Ctrl Pts',(3.99341629071535,0.00201972559511968,
1.13967192555673));
#16051=CARTESIAN_POINT('Ctrl Pts',(3.99269813258433,0.00225249187749216,
1.13632143548993));
#16052=CARTESIAN_POINT('Ctrl Pts',(3.99196676110863,0.00250303256209103,
1.1329829561429));
#16053=CARTESIAN_POINT('Ctrl Pts',(3.99105452080383,0.00281553218516866,
1.12881886782618));
#16054=CARTESIAN_POINT('Ctrl Pts',(3.99012140143879,0.00315586692512113,
1.12467248508852));
#16055=CARTESIAN_POINT('Ctrl Pts',(3.98917086800784,0.00352214531426548,
1.12054686155091));
#16056=CARTESIAN_POINT('Ctrl Pts',(3.98870515989402,0.00370160119891811,
1.11852553721503));
#16057=CARTESIAN_POINT('Ctrl Pts',(3.98823550683287,0.0038871810438387,
1.11651018939739));
#16058=CARTESIAN_POINT('Ctrl Pts',(3.98775852062678,0.00408030873675932,
1.11448575646417));
#16059=CARTESIAN_POINT('Ctrl Pts',(3.9862084876943,0.00470790400130428,
1.10790708044385));
#16060=CARTESIAN_POINT('Ctrl Pts',(3.98459064329944,0.00541159016947844,
1.10127461612058));
#16061=CARTESIAN_POINT('Ctrl Pts',(3.98292515171806,0.00618848637705155,
1.09466884705581));
#16062=CARTESIAN_POINT('Ctrl Pts',(3.97963238984024,0.0077244498390748,
1.08160890439789));
#16063=CARTESIAN_POINT('Ctrl Pts',(3.97615366065642,0.00954620024828415,
1.06865218726209));
#16064=CARTESIAN_POINT('Ctrl Pts',(3.9725476703773,0.0116345924802287,1.05580609615032));
#16065=CARTESIAN_POINT('Ctrl Pts',(3.96631447912973,0.0152445157395957,
1.03360078318899));
#16066=CARTESIAN_POINT('Ctrl Pts',(3.95970190268761,0.0196489544111943,
1.01172528029353));
#16067=CARTESIAN_POINT('Ctrl Pts',(3.95284326123313,0.024832861200458,0.990102320899307));
#16068=CARTESIAN_POINT('Ctrl Pts',(3.94567549386735,0.0302504119148388,
0.967504792842701));
#16069=CARTESIAN_POINT('Ctrl Pts',(3.93823747405201,0.0365191099549545,
0.945182309268941));
#16070=CARTESIAN_POINT('Ctrl Pts',(3.93065896302406,0.0436712823961812,
0.923055906994704));
#16071=CARTESIAN_POINT('Ctrl Pts',(3.92844049782574,0.0457649450687984,
0.916578822877736));
#16072=CARTESIAN_POINT('Ctrl Pts',(3.92620993731492,0.0479346347022567,
0.910118642894705));
#16073=CARTESIAN_POINT('Ctrl Pts',(3.92397049706406,0.0501819523054339,
0.903673683563887));
#16074=CARTESIAN_POINT('Ctrl Pts',(4.00794703095364,-0.208000000000001,
1.48914872207946));
#16075=CARTESIAN_POINT('Ctrl Pts',(4.00794703095364,0.891200000000001,1.48914872207946));
#16076=CARTESIAN_POINT('Ctrl Pts',(4.00765497692301,-0.208000000000001,
1.47837060024778));
#16077=CARTESIAN_POINT('Ctrl Pts',(4.00765497692301,0.891200000000001,1.47837060024778));
#16078=CARTESIAN_POINT('Ctrl Pts',(4.00609251232828,-0.208000000000001,
1.42037324240448));
#16079=CARTESIAN_POINT('Ctrl Pts',(4.00609251232828,0.891200000000001,1.42037324240448));
#16080=CARTESIAN_POINT('Ctrl Pts',(4.00332489658119,-0.208000000000001,
1.31493320069941));
#16081=CARTESIAN_POINT('Ctrl Pts',(4.00332489658119,0.891200000000001,1.31493320069941));
#16082=CARTESIAN_POINT('Ctrl Pts',(3.99926045685694,-0.208000000000001,
1.16206588280709));
#16083=CARTESIAN_POINT('Ctrl Pts',(3.99926045685694,0.891200000000001,1.16206588280709));
#16084=CARTESIAN_POINT('Ctrl Pts',(3.99260375067002,-0.208000000000001,
0.964078729991153));
#16085=CARTESIAN_POINT('Ctrl Pts',(3.99260375067002,0.891200000000001,0.964078729991153));
#16086=CARTESIAN_POINT('Ctrl Pts',(3.97841403016118,-0.208000000000001,
0.741129277895168));
#16087=CARTESIAN_POINT('Ctrl Pts',(3.97841403016118,0.891200000000001,0.741129277895168));
#16088=CARTESIAN_POINT('Ctrl Pts',(3.95259200169988,-0.208000000000001,
0.538436816836329));
#16089=CARTESIAN_POINT('Ctrl Pts',(3.95259200169988,0.891200000000001,0.538436816836329));
#16090=CARTESIAN_POINT('Ctrl Pts',(3.90986572419832,-0.208000000000001,
0.364350357241537));
#16091=CARTESIAN_POINT('Ctrl Pts',(3.90986572419832,0.891200000000001,0.364350357241537));
#16092=CARTESIAN_POINT('Ctrl Pts',(3.84598208672298,-0.208000000000001,
0.224659532804428));
#16093=CARTESIAN_POINT('Ctrl Pts',(3.84598208672298,0.891200000000001,0.224659532804428));
#16094=CARTESIAN_POINT('Ctrl Pts',(3.75872318140661,-0.208000000000001,
0.120497232333236));
#16095=CARTESIAN_POINT('Ctrl Pts',(3.75872318140661,0.891200000000001,0.120497232333236));
#16096=CARTESIAN_POINT('Ctrl Pts',(3.64881642260075,-0.208000000000001,
0.0470540298718229));
#16097=CARTESIAN_POINT('Ctrl Pts',(3.64881642260075,0.891200000000001,0.0470540298718229));
#16098=CARTESIAN_POINT('Ctrl Pts',(3.52045328348988,-0.208000000000001,
-0.00118366394786523));
#16099=CARTESIAN_POINT('Ctrl Pts',(3.52045328348988,0.891200000000001,-0.00118366394786523));
#16100=CARTESIAN_POINT('Ctrl Pts',(3.3816469894381,-0.208000000000001,-0.0263068037111615));
#16101=CARTESIAN_POINT('Ctrl Pts',(3.3816469894381,0.891200000000001,-0.0263068037111615));
#16102=CARTESIAN_POINT('Ctrl Pts',(3.2451100102617,-0.208000000000001,-0.0214179570895094));
#16103=CARTESIAN_POINT('Ctrl Pts',(3.2451100102617,0.891200000000001,-0.0214179570895094));
#16104=CARTESIAN_POINT('Ctrl Pts',(3.12452733970665,-0.208000000000001,
0.0241851999814078));
#16105=CARTESIAN_POINT('Ctrl Pts',(3.12452733970665,0.891200000000001,0.0241851999814078));
#16106=CARTESIAN_POINT('Ctrl Pts',(3.03063129752059,-0.208000000000001,
0.119017371327004));
#16107=CARTESIAN_POINT('Ctrl Pts',(3.03063129752059,0.891200000000001,0.119017371327004));
#16108=CARTESIAN_POINT('Ctrl Pts',(2.96639254265844,-0.208000000000001,
0.262319630540593));
#16109=CARTESIAN_POINT('Ctrl Pts',(2.96639254265844,0.891200000000001,0.262319630540593));
#16110=CARTESIAN_POINT('Ctrl Pts',(2.92780415844446,-0.208000000000001,
0.444963858672424));
#16111=CARTESIAN_POINT('Ctrl Pts',(2.92780415844446,0.891200000000001,0.444963858672424));
#16112=CARTESIAN_POINT('Ctrl Pts',(2.90717911786689,-0.208000000000001,
0.65402023086958));
#16113=CARTESIAN_POINT('Ctrl Pts',(2.90717911786689,0.891200000000001,0.65402023086958));
#16114=CARTESIAN_POINT('Ctrl Pts',(2.89547076625581,-0.208000000000001,
0.875890304828918));
#16115=CARTESIAN_POINT('Ctrl Pts',(2.89547076625581,0.891200000000001,0.875890304828918));
#16116=CARTESIAN_POINT('Ctrl Pts',(2.88537704766906,-0.208000000000001,
1.10060381648398));
#16117=CARTESIAN_POINT('Ctrl Pts',(2.88537704766906,0.891200000000001,1.10060381648398));
#16118=CARTESIAN_POINT('Ctrl Pts',(2.8728456296504,-0.208000000000001,1.32371934078733));
#16119=CARTESIAN_POINT('Ctrl Pts',(2.8728456296504,0.891200000000001,1.32371934078733));
#16120=CARTESIAN_POINT('Ctrl Pts',(2.85578261679345,-0.208000000000001,
1.54401727992264));
#16121=CARTESIAN_POINT('Ctrl Pts',(2.85578261679345,0.891200000000001,1.54401727992264));
#16122=CARTESIAN_POINT('Ctrl Pts',(2.83335686249019,-0.208000000000001,
1.76209503442146));
#16123=CARTESIAN_POINT('Ctrl Pts',(2.83335686249019,0.891200000000001,1.76209503442146));
#16124=CARTESIAN_POINT('Ctrl Pts',(2.80505146480345,-0.208000000000001,
1.97856787413951));
#16125=CARTESIAN_POINT('Ctrl Pts',(2.80505146480345,0.891200000000001,1.97856787413951));
#16126=CARTESIAN_POINT('Ctrl Pts',(2.76985908233915,-0.208000000000001,
2.19251877196071));
#16127=CARTESIAN_POINT('Ctrl Pts',(2.76985908233915,0.891200000000001,2.19251877196071));
#16128=CARTESIAN_POINT('Ctrl Pts',(2.72531955636536,-0.208000000000001,
2.39962532458029));
#16129=CARTESIAN_POINT('Ctrl Pts',(2.72531955636536,0.891200000000001,2.39962532458029));
#16130=CARTESIAN_POINT('Ctrl Pts',(2.66797634363184,-0.208000000000001,
2.59347738935741));
#16131=CARTESIAN_POINT('Ctrl Pts',(2.66797634363184,0.891200000000001,2.59347738935741));
#16132=CARTESIAN_POINT('Ctrl Pts',(2.59397540849171,-0.208000000000001,
2.7672283971178));
#16133=CARTESIAN_POINT('Ctrl Pts',(2.59397540849171,0.891200000000001,2.7672283971178));
#16134=CARTESIAN_POINT('Ctrl Pts',(2.49960870420485,-0.208000000000001,
2.91510580081997));
#16135=CARTESIAN_POINT('Ctrl Pts',(2.49960870420485,0.891200000000001,2.91510580081997));
#16136=CARTESIAN_POINT('Ctrl Pts',(2.38189256086504,-0.208000000000001,
3.03403241435618));
#16137=CARTESIAN_POINT('Ctrl Pts',(2.38189256086504,0.891200000000001,3.03403241435618));
#16138=CARTESIAN_POINT('Ctrl Pts',(2.23909845280558,-0.208000000000001,
3.12505646843308));
#16139=CARTESIAN_POINT('Ctrl Pts',(2.23909845280558,0.891200000000001,3.12505646843308));
#16140=CARTESIAN_POINT('Ctrl Pts',(2.07061055216582,-0.208000000000001,
3.19196918412265));
#16141=CARTESIAN_POINT('Ctrl Pts',(2.07061055216582,0.891200000000001,3.19196918412265));
#16142=CARTESIAN_POINT('Ctrl Pts',(1.87681490437036,-0.208000000000001,
3.24001322621211));
#16143=CARTESIAN_POINT('Ctrl Pts',(1.87681490437036,0.891200000000001,3.24001322621211));
#16144=CARTESIAN_POINT('Ctrl Pts',(1.65897747541321,-0.208000000000001,
3.27464765209773));
#16145=CARTESIAN_POINT('Ctrl Pts',(1.65897747541321,0.891200000000001,3.27464765209773));
#16146=CARTESIAN_POINT('Ctrl Pts',(1.4191255439272,-0.208000000000001,3.30006519349576));
#16147=CARTESIAN_POINT('Ctrl Pts',(1.4191255439272,0.891200000000001,3.30006519349576));
#16148=CARTESIAN_POINT('Ctrl Pts',(1.15993538533448,-0.208000000000001,
3.31897283641381));
#16149=CARTESIAN_POINT('Ctrl Pts',(1.15993538533448,0.891200000000001,3.31897283641381));
#16150=CARTESIAN_POINT('Ctrl Pts',(0.884625090385968,-0.208000000000001,
3.33300441174764));
#16151=CARTESIAN_POINT('Ctrl Pts',(0.884625090385968,0.891200000000001,
3.33300441174764));
#16152=CARTESIAN_POINT('Ctrl Pts',(0.596845720618978,-0.208000000000001,
3.34293392264922));
#16153=CARTESIAN_POINT('Ctrl Pts',(0.596845720618978,0.891200000000001,
3.34293392264922));
#16154=CARTESIAN_POINT('Ctrl Pts',(0.30057321210183,-0.208000000000001,
3.34897162637417));
#16155=CARTESIAN_POINT('Ctrl Pts',(0.30057321210183,0.891200000000001,3.34897162637417));
#16156=CARTESIAN_POINT('Ctrl Pts',(1.66741620510891E-14,-0.208000000000001,
3.35102435732185));
#16157=CARTESIAN_POINT('Ctrl Pts',(1.66741620510891E-14,0.891200000000001,
3.35102435732185));
#16158=CARTESIAN_POINT('Ctrl Pts',(-0.300573212101791,-0.208000000000001,
3.34897162637426));
#16159=CARTESIAN_POINT('Ctrl Pts',(-0.300573212101791,0.891200000000001,
3.34897162637426));
#16160=CARTESIAN_POINT('Ctrl Pts',(-0.596845720618908,-0.208000000000001,
3.34293392264938));
#16161=CARTESIAN_POINT('Ctrl Pts',(-0.596845720618908,0.891200000000001,
3.34293392264938));
#16162=CARTESIAN_POINT('Ctrl Pts',(-0.884625090385886,-0.208000000000001,
3.33300441174785));
#16163=CARTESIAN_POINT('Ctrl Pts',(-0.884625090385886,0.891200000000001,
3.33300441174785));
#16164=CARTESIAN_POINT('Ctrl Pts',(-1.15993538533442,-0.208000000000001,
3.31897283641402));
#16165=CARTESIAN_POINT('Ctrl Pts',(-1.15993538533442,0.891200000000001,
3.31897283641402));
#16166=CARTESIAN_POINT('Ctrl Pts',(-1.41912554392716,-0.208000000000001,
3.30006519349591));
#16167=CARTESIAN_POINT('Ctrl Pts',(-1.41912554392716,0.891200000000001,
3.30006519349591));
#16168=CARTESIAN_POINT('Ctrl Pts',(-1.65897747541319,-0.208000000000001,
3.27464765209779));
#16169=CARTESIAN_POINT('Ctrl Pts',(-1.65897747541319,0.891200000000001,
3.27464765209779));
#16170=CARTESIAN_POINT('Ctrl Pts',(-1.87681490437034,-0.208000000000001,
3.24001322621208));
#16171=CARTESIAN_POINT('Ctrl Pts',(-1.87681490437034,0.891200000000001,
3.24001322621208));
#16172=CARTESIAN_POINT('Ctrl Pts',(-2.07061055216576,-0.208000000000001,
3.19196918412254));
#16173=CARTESIAN_POINT('Ctrl Pts',(-2.07061055216576,0.891200000000001,
3.19196918412254));
#16174=CARTESIAN_POINT('Ctrl Pts',(-2.23909845280547,-0.208000000000001,
3.12505646843295));
#16175=CARTESIAN_POINT('Ctrl Pts',(-2.23909845280547,0.891200000000001,
3.12505646843295));
#16176=CARTESIAN_POINT('Ctrl Pts',(-2.38189256086493,-0.208000000000001,
3.03403241435609));
#16177=CARTESIAN_POINT('Ctrl Pts',(-2.38189256086493,0.891200000000001,
3.03403241435609));
#16178=CARTESIAN_POINT('Ctrl Pts',(-2.49960870420481,-0.208000000000001,
2.91510580081997));
#16179=CARTESIAN_POINT('Ctrl Pts',(-2.49960870420481,0.891200000000001,
2.91510580081997));
#16180=CARTESIAN_POINT('Ctrl Pts',(-2.59397540849182,-0.208000000000001,
2.76722839711793));
#16181=CARTESIAN_POINT('Ctrl Pts',(-2.59397540849182,0.891200000000001,
2.76722839711793));
#16182=CARTESIAN_POINT('Ctrl Pts',(-2.66797634363209,-0.208000000000001,
2.59347738935767));
#16183=CARTESIAN_POINT('Ctrl Pts',(-2.66797634363209,0.891200000000001,
2.59347738935767));
#16184=CARTESIAN_POINT('Ctrl Pts',(-2.72531955636566,-0.208000000000001,
2.39962532458057));
#16185=CARTESIAN_POINT('Ctrl Pts',(-2.72531955636566,0.891200000000001,
2.39962532458057));
#16186=CARTESIAN_POINT('Ctrl Pts',(-2.76985908233936,-0.208000000000001,
2.19251877196088));
#16187=CARTESIAN_POINT('Ctrl Pts',(-2.76985908233936,0.891200000000001,
2.19251877196088));
#16188=CARTESIAN_POINT('Ctrl Pts',(-2.80505146480344,-0.208000000000001,
1.97856787413951));
#16189=CARTESIAN_POINT('Ctrl Pts',(-2.80505146480344,0.891200000000001,
1.97856787413951));
#16190=CARTESIAN_POINT('Ctrl Pts',(-2.8333568624899,-0.208000000000001,
1.76209503442131));
#16191=CARTESIAN_POINT('Ctrl Pts',(-2.8333568624899,0.891200000000001,1.76209503442131));
#16192=CARTESIAN_POINT('Ctrl Pts',(-2.85578261679294,-0.208000000000001,
1.54401727992238));
#16193=CARTESIAN_POINT('Ctrl Pts',(-2.85578261679294,0.891200000000001,
1.54401727992238));
#16194=CARTESIAN_POINT('Ctrl Pts',(-2.87284562964987,-0.208000000000001,
1.32371934078708));
#16195=CARTESIAN_POINT('Ctrl Pts',(-2.87284562964987,0.891200000000001,
1.32371934078708));
#16196=CARTESIAN_POINT('Ctrl Pts',(-2.88537704766869,-0.208000000000001,
1.10060381648384));
#16197=CARTESIAN_POINT('Ctrl Pts',(-2.88537704766869,0.891200000000001,
1.10060381648384));
#16198=CARTESIAN_POINT('Ctrl Pts',(-2.89547076625573,-0.208000000000001,
0.875890304828914));
#16199=CARTESIAN_POINT('Ctrl Pts',(-2.89547076625573,0.891200000000001,
0.875890304828914));
#16200=CARTESIAN_POINT('Ctrl Pts',(-2.90717911786707,-0.208000000000001,
0.654020230869684));
#16201=CARTESIAN_POINT('Ctrl Pts',(-2.90717911786707,0.891200000000001,
0.654020230869684));
#16202=CARTESIAN_POINT('Ctrl Pts',(-2.92780415844476,-0.208000000000001,
0.444963858672577));
#16203=CARTESIAN_POINT('Ctrl Pts',(-2.92780415844476,0.891200000000001,
0.444963858672577));
#16204=CARTESIAN_POINT('Ctrl Pts',(-2.96639254265869,-0.208000000000001,
0.262319630540737));
#16205=CARTESIAN_POINT('Ctrl Pts',(-2.96639254265869,0.891200000000001,
0.262319630540737));
#16206=CARTESIAN_POINT('Ctrl Pts',(-3.03063129752067,-0.208000000000001,
0.11901737132707));
#16207=CARTESIAN_POINT('Ctrl Pts',(-3.03063129752067,0.891200000000001,
0.11901737132707));
#16208=CARTESIAN_POINT('Ctrl Pts',(-3.12452733970658,-0.208000000000001,
0.0241851999813871));
#16209=CARTESIAN_POINT('Ctrl Pts',(-3.12452733970658,0.891200000000001,
0.0241851999813871));
#16210=CARTESIAN_POINT('Ctrl Pts',(-3.24511001026157,-0.208000000000001,
-0.0214179570895714));
#16211=CARTESIAN_POINT('Ctrl Pts',(-3.24511001026157,0.891200000000001,
-0.0214179570895714));
#16212=CARTESIAN_POINT('Ctrl Pts',(-3.38164698943802,-0.208000000000001,
-0.0263068037112043));
#16213=CARTESIAN_POINT('Ctrl Pts',(-3.38164698943802,0.891200000000001,
-0.0263068037112043));
#16214=CARTESIAN_POINT('Ctrl Pts',(-3.52045328348989,-0.208000000000001,
-0.00118366394785932));
#16215=CARTESIAN_POINT('Ctrl Pts',(-3.52045328348989,0.891200000000001,
-0.00118366394785932));
#16216=CARTESIAN_POINT('Ctrl Pts',(-3.64881642260079,-0.208000000000001,
0.0470540298718583));
#16217=CARTESIAN_POINT('Ctrl Pts',(-3.64881642260079,0.891200000000001,
0.0470540298718583));
#16218=CARTESIAN_POINT('Ctrl Pts',(-3.75872318140663,-0.208000000000001,
0.120497232333251));
#16219=CARTESIAN_POINT('Ctrl Pts',(-3.75872318140663,0.891200000000001,
0.120497232333251));
#16220=CARTESIAN_POINT('Ctrl Pts',(-3.84598208672296,-0.208000000000001,
0.224659532804408));
#16221=CARTESIAN_POINT('Ctrl Pts',(-3.84598208672296,0.891200000000001,
0.224659532804408));
#16222=CARTESIAN_POINT('Ctrl Pts',(-3.9098657241983,-0.208000000000001,
0.364350357241515));
#16223=CARTESIAN_POINT('Ctrl Pts',(-3.9098657241983,0.891200000000001,0.364350357241515));
#16224=CARTESIAN_POINT('Ctrl Pts',(-3.9525920016999,-0.208000000000001,
0.538436816836325));
#16225=CARTESIAN_POINT('Ctrl Pts',(-3.9525920016999,0.891200000000001,0.538436816836325));
#16226=CARTESIAN_POINT('Ctrl Pts',(-3.97841403016126,-0.208000000000001,
0.741129277895169));
#16227=CARTESIAN_POINT('Ctrl Pts',(-3.97841403016126,0.891200000000001,
0.741129277895169));
#16228=CARTESIAN_POINT('Ctrl Pts',(-3.99260375067011,-0.208000000000001,
0.964078729991154));
#16229=CARTESIAN_POINT('Ctrl Pts',(-3.99260375067011,0.891200000000001,
0.964078729991154));
#16230=CARTESIAN_POINT('Ctrl Pts',(-4.00047520099045,-0.208000000000001,
1.1981954227983));
#16231=CARTESIAN_POINT('Ctrl Pts',(-4.00047520099045,0.891200000000001,
1.1981954227983));
#16232=CARTESIAN_POINT('Ctrl Pts',(-4.00639322616607,-0.208000000000001,
1.43558101932923));
#16233=CARTESIAN_POINT('Ctrl Pts',(-4.00639322616607,0.891200000000001,
1.43558101932923));
#16234=CARTESIAN_POINT('Ctrl Pts',(-4.01278239926574,-0.208000000000001,
1.67142113207667));
#16235=CARTESIAN_POINT('Ctrl Pts',(-4.01278239926574,0.891200000000001,
1.67142113207667));
#16236=CARTESIAN_POINT('Ctrl Pts',(-4.02066709528487,-0.208000000000001,
1.90332556813333));
#16237=CARTESIAN_POINT('Ctrl Pts',(-4.02066709528487,0.891200000000001,
1.90332556813333));
#16238=CARTESIAN_POINT('Ctrl Pts',(-4.0302101444685,-0.208000000000001,
2.130657485557));
#16239=CARTESIAN_POINT('Ctrl Pts',(-4.0302101444685,0.891200000000001,2.130657485557));
#16240=CARTESIAN_POINT('Ctrl Pts',(-4.04126813644779,-0.208000000000001,
2.35385258470204));
#16241=CARTESIAN_POINT('Ctrl Pts',(-4.04126813644779,0.891200000000001,
2.35385258470204));
#16242=CARTESIAN_POINT('Ctrl Pts',(-4.05390260344525,-0.208000000000001,
2.57377631141659));
#16243=CARTESIAN_POINT('Ctrl Pts',(-4.05390260344525,0.891200000000001,
2.57377631141659));
#16244=CARTESIAN_POINT('Ctrl Pts',(-4.06899962712502,-0.208000000000001,
2.7909834104825));
#16245=CARTESIAN_POINT('Ctrl Pts',(-4.06899962712502,0.891200000000001,
2.7909834104825));
#16246=CARTESIAN_POINT('Ctrl Pts',(-4.08854433447739,-0.208000000000001,
3.00529120729338));
#16247=CARTESIAN_POINT('Ctrl Pts',(-4.08854433447739,0.891200000000001,
3.00529120729338));
#16248=CARTESIAN_POINT('Ctrl Pts',(-4.11518318246524,-0.208000000000001,
3.21600287470921));
#16249=CARTESIAN_POINT('Ctrl Pts',(-4.11518318246524,0.891200000000001,
3.21600287470921));
#16250=CARTESIAN_POINT('Ctrl Pts',(-4.15193466045748,-0.208000000000001,
3.42199345348447));
#16251=CARTESIAN_POINT('Ctrl Pts',(-4.15193466045748,0.891200000000001,
3.42199345348447));
#16252=CARTESIAN_POINT('Ctrl Pts',(-4.20184334854115,-0.208000000000001,
3.62185203209171));
#16253=CARTESIAN_POINT('Ctrl Pts',(-4.20184334854115,0.891200000000001,
3.62185203209171));
#16254=CARTESIAN_POINT('Ctrl Pts',(-4.26765207024395,-0.208000000000001,
3.81399668859083));
#16255=CARTESIAN_POINT('Ctrl Pts',(-4.26765207024395,0.891200000000001,
3.81399668859083));
#16256=CARTESIAN_POINT('Ctrl Pts',(-4.35148411330718,-0.208000000000001,
3.99681013615577));
#16257=CARTESIAN_POINT('Ctrl Pts',(-4.35148411330718,0.891200000000001,
3.99681013615577));
#16258=CARTESIAN_POINT('Ctrl Pts',(-4.45474519640294,-0.208000000000001,
4.16885849319142));
#16259=CARTESIAN_POINT('Ctrl Pts',(-4.45474519640294,0.891200000000001,
4.16885849319142));
#16260=CARTESIAN_POINT('Ctrl Pts',(-4.57800047823775,-0.208000000000001,
4.32911151507774));
#16261=CARTESIAN_POINT('Ctrl Pts',(-4.57800047823775,0.891200000000001,
4.32911151507774));
#16262=CARTESIAN_POINT('Ctrl Pts',(-4.7208720035032,-0.208000000000001,
4.47714872481861));
#16263=CARTESIAN_POINT('Ctrl Pts',(-4.7208720035032,0.891200000000001,4.47714872481861));
#16264=CARTESIAN_POINT('Ctrl Pts',(-4.88190185104852,-0.208000000000001,
4.61340315498244));
#16265=CARTESIAN_POINT('Ctrl Pts',(-4.88190185104852,0.891200000000001,
4.61340315498244));
#16266=CARTESIAN_POINT('Ctrl Pts',(-5.05850630701885,-0.208000000000001,
4.73929437247796));
#16267=CARTESIAN_POINT('Ctrl Pts',(-5.05850630701885,0.891200000000001,
4.73929437247796));
#16268=CARTESIAN_POINT('Ctrl Pts',(-5.24741086000019,-0.208000000000001,
4.8567611153285));
#16269=CARTESIAN_POINT('Ctrl Pts',(-5.24741086000019,0.891200000000001,
4.8567611153285));
#16270=CARTESIAN_POINT('Ctrl Pts',(-5.44501860313342,-0.208000000000001,
4.96787993373728));
#16271=CARTESIAN_POINT('Ctrl Pts',(-5.44501860313342,0.891200000000001,
4.96787993373728));
#16272=CARTESIAN_POINT('Ctrl Pts',(-5.64781737380319,-0.208000000000001,
5.07442896098937));
#16273=CARTESIAN_POINT('Ctrl Pts',(-5.64781737380319,0.891200000000001,
5.07442896098937));
#16274=CARTESIAN_POINT('Ctrl Pts',(-5.85274048349242,-0.208000000000001,
5.17752467829109));
#16275=CARTESIAN_POINT('Ctrl Pts',(-5.85274048349242,0.891200000000001,
5.17752467829109));
#16276=CARTESIAN_POINT('Ctrl Pts',(-6.05762450882858,-0.208000000000001,
5.27709955371564));
#16277=CARTESIAN_POINT('Ctrl Pts',(-6.05762450882858,0.891200000000001,
5.27709955371564));
#16278=CARTESIAN_POINT('Ctrl Pts',(-6.26112587698772,-0.208000000000001,
5.37226655127787));
#16279=CARTESIAN_POINT('Ctrl Pts',(-6.26112587698772,0.891200000000001,
5.37226655127787));
#16280=CARTESIAN_POINT('Ctrl Pts',(-6.46246210121964,-0.208000000000001,
5.46195513100446));
#16281=CARTESIAN_POINT('Ctrl Pts',(-6.46246210121964,0.891200000000001,
5.46195513100446));
#16282=CARTESIAN_POINT('Ctrl Pts',(-6.66121503090592,-0.208000000000001,
5.54547963906637));
#16283=CARTESIAN_POINT('Ctrl Pts',(-6.66121503090592,0.891200000000001,
5.54547963906637));
#16284=CARTESIAN_POINT('Ctrl Pts',(-6.8570997603751,-0.208000000000001,
5.62308582598972));
#16285=CARTESIAN_POINT('Ctrl Pts',(-6.8570997603751,0.891200000000001,5.62308582598972));
#16286=CARTESIAN_POINT('Ctrl Pts',(-7.04976847947249,-0.208000000000001,
5.69662713609756));
#16287=CARTESIAN_POINT('Ctrl Pts',(-7.04976847947249,0.891200000000001,
5.69662713609756));
#16288=CARTESIAN_POINT('Ctrl Pts',(-7.23853768475,-0.208000000000001,5.76979878895672));
#16289=CARTESIAN_POINT('Ctrl Pts',(-7.23853768475,0.891200000000001,5.76979878895672));
#16290=CARTESIAN_POINT('Ctrl Pts',(-7.42198551710617,-0.208000000000001,
5.84723737025949));
#16291=CARTESIAN_POINT('Ctrl Pts',(-7.42198551710617,0.891200000000001,
5.84723737025949));
#16292=CARTESIAN_POINT('Ctrl Pts',(-7.59751903688412,-0.208000000000001,
5.93381436957244));
#16293=CARTESIAN_POINT('Ctrl Pts',(-7.59751903688412,0.891200000000001,
5.93381436957244));
#16294=CARTESIAN_POINT('Ctrl Pts',(-7.76106756457753,-0.208000000000001,
6.03389995867283));
#16295=CARTESIAN_POINT('Ctrl Pts',(-7.76106756457753,0.891200000000001,
6.03389995867283));
#16296=CARTESIAN_POINT('Ctrl Pts',(-7.90644860448901,-0.208000000000001,
6.15052660592937));
#16297=CARTESIAN_POINT('Ctrl Pts',(-7.90644860448901,0.891200000000001,
6.15052660592937));
#16298=CARTESIAN_POINT('Ctrl Pts',(-8.02580908828117,-0.208000000000001,
6.28498018271686));
#16299=CARTESIAN_POINT('Ctrl Pts',(-8.02580908828117,0.891200000000001,
6.28498018271686));
#16300=CARTESIAN_POINT('Ctrl Pts',(-8.11207116917861,-0.208000000000001,
6.43720976255636));
#16301=CARTESIAN_POINT('Ctrl Pts',(-8.11207116917861,0.891200000000001,
6.43720976255636));
#16302=CARTESIAN_POINT('Ctrl Pts',(-8.16089752265956,-0.208000000000001,
6.60605451948903));
#16303=CARTESIAN_POINT('Ctrl Pts',(-8.16089752265956,0.891200000000001,
6.60605451948903));
#16304=CARTESIAN_POINT('Ctrl Pts',(-8.17293082304181,-0.208000000000001,
6.78954489191904));
#16305=CARTESIAN_POINT('Ctrl Pts',(-8.17293082304181,0.891200000000001,
6.78954489191904));
#16306=CARTESIAN_POINT('Ctrl Pts',(-8.15569042861244,-0.208000000000001,
6.9851692342788));
#16307=CARTESIAN_POINT('Ctrl Pts',(-8.15569042861244,0.891200000000001,
6.9851692342788));
#16308=CARTESIAN_POINT('Ctrl Pts',(-8.12057943633387,-0.208000000000001,
7.19009032473164));
#16309=CARTESIAN_POINT('Ctrl Pts',(-8.12057943633387,0.891200000000001,
7.19009032473164));
#16310=CARTESIAN_POINT('Ctrl Pts',(-8.08008348678073,-0.208000000000001,
7.40136016279791));
#16311=CARTESIAN_POINT('Ctrl Pts',(-8.08008348678073,0.891200000000001,
7.40136016279791));
#16312=CARTESIAN_POINT('Ctrl Pts',(-8.04494633492831,-0.208000000000001,
7.61613341658677));
#16313=CARTESIAN_POINT('Ctrl Pts',(-8.04494633492831,0.891200000000001,
7.61613341658677));
#16314=CARTESIAN_POINT('Ctrl Pts',(-8.02124364536279,-0.208000000000001,
7.83188673232793));
#16315=CARTESIAN_POINT('Ctrl Pts',(-8.02124364536279,0.891200000000001,
7.83188673232793));
#16316=CARTESIAN_POINT('Ctrl Pts',(-8.007818938056,-0.208000000000001,8.04662057355248));
#16317=CARTESIAN_POINT('Ctrl Pts',(-8.007818938056,0.891200000000001,8.04662057355248));
#16318=CARTESIAN_POINT('Ctrl Pts',(-7.99879843919661,-0.208000000000001,
8.25883677791483));
#16319=CARTESIAN_POINT('Ctrl Pts',(-7.99879843919661,0.891200000000001,
8.25883677791483));
#16320=CARTESIAN_POINT('Ctrl Pts',(-7.98575825096101,-0.208000000000001,
8.46752658699528));
#16321=CARTESIAN_POINT('Ctrl Pts',(-7.98575825096101,0.891200000000001,
8.46752658699528));
#16322=CARTESIAN_POINT('Ctrl Pts',(-7.96007609558389,-0.208000000000001,
8.67216210283896));
#16323=CARTESIAN_POINT('Ctrl Pts',(-7.96007609558389,0.891200000000001,
8.67216210283896));
#16324=CARTESIAN_POINT('Ctrl Pts',(-7.91508259073019,-0.208000000000001,
8.87266947141823));
#16325=CARTESIAN_POINT('Ctrl Pts',(-7.91508259073019,0.891200000000001,
8.87266947141823));
#16326=CARTESIAN_POINT('Ctrl Pts',(-7.84862074946261,-0.208000000000001,
9.06945407016992));
#16327=CARTESIAN_POINT('Ctrl Pts',(-7.84862074946261,0.891200000000001,
9.06945407016992));
#16328=CARTESIAN_POINT('Ctrl Pts',(-7.76209282457479,-0.208000000000001,
9.26297089919765));
#16329=CARTESIAN_POINT('Ctrl Pts',(-7.76209282457479,0.891200000000001,
9.26297089919765));
#16330=CARTESIAN_POINT('Ctrl Pts',(-7.65900038660722,-0.208000000000001,
9.4532499945042));
#16331=CARTESIAN_POINT('Ctrl Pts',(-7.65900038660722,0.891200000000001,
9.4532499945042));
#16332=CARTESIAN_POINT('Ctrl Pts',(-7.5436057352653,-0.208000000000001,
9.63939026966035));
#16333=CARTESIAN_POINT('Ctrl Pts',(-7.5436057352653,0.891200000000001,9.63939026966035));
#16334=CARTESIAN_POINT('Ctrl Pts',(-7.41967047355001,-0.208000000000001,
9.81917361987397));
#16335=CARTESIAN_POINT('Ctrl Pts',(-7.41967047355001,0.891200000000001,
9.81917361987397));
#16336=CARTESIAN_POINT('Ctrl Pts',(-7.28883796912703,-0.208000000000001,
9.98835756998572));
#16337=CARTESIAN_POINT('Ctrl Pts',(-7.28883796912703,0.891200000000001,
9.98835756998572));
#16338=CARTESIAN_POINT('Ctrl Pts',(-7.15081550722306,-0.208000000000001,
10.1414720974148));
#16339=CARTESIAN_POINT('Ctrl Pts',(-7.15081550722306,0.891200000000001,
10.1414720974148));
#16340=CARTESIAN_POINT('Ctrl Pts',(-7.0044544864105,-0.208000000000001,
10.2733319413008));
#16341=CARTESIAN_POINT('Ctrl Pts',(-7.0044544864105,0.891200000000001,10.2733319413008));
#16342=CARTESIAN_POINT('Ctrl Pts',(-6.84859008776113,-0.208000000000001,
10.3804015453596));
#16343=CARTESIAN_POINT('Ctrl Pts',(-6.84859008776113,0.891200000000001,
10.3804015453596));
#16344=CARTESIAN_POINT('Ctrl Pts',(-6.68288828293938,-0.208000000000001,
10.4620502678778));
#16345=CARTESIAN_POINT('Ctrl Pts',(-6.68288828293938,0.891200000000001,
10.4620502678778));
#16346=CARTESIAN_POINT('Ctrl Pts',(-6.50892555577766,-0.208000000000001,
10.522290883026));
#16347=CARTESIAN_POINT('Ctrl Pts',(-6.50892555577766,0.891200000000001,
10.522290883026));
#16348=CARTESIAN_POINT('Ctrl Pts',(-6.32976796473811,-0.208000000000001,
10.5687216653902));
#16349=CARTESIAN_POINT('Ctrl Pts',(-6.32976796473811,0.891200000000001,
10.5687216653902));
#16350=CARTESIAN_POINT('Ctrl Pts',(-6.14893768388701,-0.208000000000001,
10.6103475969885));
#16351=CARTESIAN_POINT('Ctrl Pts',(-6.14893768388701,0.891200000000001,
10.6103475969885));
#16352=CARTESIAN_POINT('Ctrl Pts',(-5.96961932707142,-0.208000000000001,
10.6558377434043));
#16353=CARTESIAN_POINT('Ctrl Pts',(-5.96961932707142,0.891200000000001,
10.6558377434043));
#16354=CARTESIAN_POINT('Ctrl Pts',(-5.79367695415031,-0.208000000000001,
10.7114411549114));
#16355=CARTESIAN_POINT('Ctrl Pts',(-5.79367695415031,0.891200000000001,
10.7114411549114));
#16356=CARTESIAN_POINT('Ctrl Pts',(-5.62101499943431,-0.208000000000001,
10.7795199127535));
#16357=CARTESIAN_POINT('Ctrl Pts',(-5.62101499943431,0.891200000000001,
10.7795199127535));
#16358=CARTESIAN_POINT('Ctrl Pts',(-5.45051506148982,-0.208000000000001,
10.8599381259737));
#16359=CARTESIAN_POINT('Ctrl Pts',(-5.45051506148982,0.891200000000001,
10.8599381259737));
#16360=CARTESIAN_POINT('Ctrl Pts',(-5.28082876351929,-0.208000000000001,
10.9511663773826));
#16361=CARTESIAN_POINT('Ctrl Pts',(-5.28082876351929,0.891200000000001,
10.9511663773826));
#16362=CARTESIAN_POINT('Ctrl Pts',(-5.11112998264616,-0.208000000000001,
11.0513704191329));
#16363=CARTESIAN_POINT('Ctrl Pts',(-5.11112998264616,0.891200000000001,
11.0513704191329));
#16364=CARTESIAN_POINT('Ctrl Pts',(-4.94211773226973,-0.208000000000001,
11.1598106424589));
#16365=CARTESIAN_POINT('Ctrl Pts',(-4.94211773226973,0.891200000000001,
11.1598106424589));
#16366=CARTESIAN_POINT('Ctrl Pts',(-4.77596612414951,-0.208000000000001,
11.2768795166235));
#16367=CARTESIAN_POINT('Ctrl Pts',(-4.77596612414951,0.891200000000001,
11.2768795166235));
#16368=CARTESIAN_POINT('Ctrl Pts',(-4.61532593596946,-0.208000000000001,
11.4029224160731));
#16369=CARTESIAN_POINT('Ctrl Pts',(-4.61532593596946,0.891200000000001,
11.4029224160731));
#16370=CARTESIAN_POINT('Ctrl Pts',(-4.46255574628757,-0.208000000000001,
11.5373242211527));
#16371=CARTESIAN_POINT('Ctrl Pts',(-4.46255574628757,0.891200000000001,
11.5373242211527));
#16372=CARTESIAN_POINT('Ctrl Pts',(-4.31893584999241,-0.208000000000001,
11.6776492463597));
#16373=CARTESIAN_POINT('Ctrl Pts',(-4.31893584999241,0.891200000000001,
11.6776492463597));
#16374=CARTESIAN_POINT('Ctrl Pts',(-4.18369962429796,-0.208000000000001,
11.8183570873721));
#16375=CARTESIAN_POINT('Ctrl Pts',(-4.18369962429796,0.891200000000001,
11.8183570873721));
#16376=CARTESIAN_POINT('Ctrl Pts',(-4.05395481372655,-0.208000000000001,
11.9514202619522));
#16377=CARTESIAN_POINT('Ctrl Pts',(-4.05395481372655,0.891200000000001,
11.9514202619522));
#16378=CARTESIAN_POINT('Ctrl Pts',(-3.92533033057354,-0.208000000000001,
12.0684942936867));
#16379=CARTESIAN_POINT('Ctrl Pts',(-3.92533033057354,0.891200000000001,
12.0684942936867));
#16380=CARTESIAN_POINT('Ctrl Pts',(-3.79241297762166,-0.208000000000001,
12.1626050652586));
#16381=CARTESIAN_POINT('Ctrl Pts',(-3.79241297762166,0.891200000000001,
12.1626050652586));
#16382=CARTESIAN_POINT('Ctrl Pts',(-3.64927048315908,-0.208000000000001,
12.2301117722809));
#16383=CARTESIAN_POINT('Ctrl Pts',(-3.64927048315908,0.891200000000001,
12.2301117722809));
#16384=CARTESIAN_POINT('Ctrl Pts',(-3.48993681214334,-0.208000000000001,
12.2723364229645));
#16385=CARTESIAN_POINT('Ctrl Pts',(-3.48993681214334,0.891200000000001,
12.2723364229645));
#16386=CARTESIAN_POINT('Ctrl Pts',(-3.30884480305534,-0.208000000000001,
12.2938762651139));
#16387=CARTESIAN_POINT('Ctrl Pts',(-3.30884480305534,0.891200000000001,
12.2938762651139));
#16388=CARTESIAN_POINT('Ctrl Pts',(-3.10127560868576,-0.208000000000001,
12.3010487961981));
#16389=CARTESIAN_POINT('Ctrl Pts',(-3.10127560868576,0.891200000000001,
12.3010487961981));
#16390=CARTESIAN_POINT('Ctrl Pts',(-2.86376302967345,-0.208000000000001,
12.300400839059));
#16391=CARTESIAN_POINT('Ctrl Pts',(-2.86376302967345,0.891200000000001,
12.300400839059));
#16392=CARTESIAN_POINT('Ctrl Pts',(-2.59461297443094,-0.208000000000001,
12.2969132923574));
#16393=CARTESIAN_POINT('Ctrl Pts',(-2.59461297443094,0.891200000000001,
12.2969132923574));
#16394=CARTESIAN_POINT('Ctrl Pts',(-2.29394197380209,-0.208000000000001,
12.2935845551224));
#16395=CARTESIAN_POINT('Ctrl Pts',(-2.29394197380209,0.891200000000001,
12.2935845551224));
#16396=CARTESIAN_POINT('Ctrl Pts',(-1.96338745719135,-0.208000000000001,
12.2919684497906));
#16397=CARTESIAN_POINT('Ctrl Pts',(-1.96338745719135,0.891200000000001,
12.2919684497906));
#16398=CARTESIAN_POINT('Ctrl Pts',(-1.60591558979456,-0.208000000000001,
12.2924280531798));
#16399=CARTESIAN_POINT('Ctrl Pts',(-1.60591558979456,0.891200000000001,
12.2924280531798));
#16400=CARTESIAN_POINT('Ctrl Pts',(-1.22558901314075,-0.208000000000001,
12.2945066442122));
#16401=CARTESIAN_POINT('Ctrl Pts',(-1.22558901314075,0.891200000000001,
12.2945066442122));
#16402=CARTESIAN_POINT('Ctrl Pts',(-0.827351903312651,-0.208000000000001,
12.2972483292773));
#16403=CARTESIAN_POINT('Ctrl Pts',(-0.827351903312651,0.891200000000001,
12.2972483292773));
#16404=CARTESIAN_POINT('Ctrl Pts',(-0.498916532526571,-0.208000000000001,
12.299081889758));
#16405=CARTESIAN_POINT('Ctrl Pts',(-0.498916532526571,0.891200000000001,
12.299081889758));
#16406=CARTESIAN_POINT('Ctrl Pts',(-0.249771440080693,-0.208000000000001,
12.2998330708668));
#16407=CARTESIAN_POINT('Ctrl Pts',(-0.249771440080693,0.891200000000001,
12.2998330708668));
#16408=CARTESIAN_POINT('Ctrl Pts',(-0.0832571466935557,-0.208000000000001,
12.2999999999989));
#16409=CARTESIAN_POINT('Ctrl Pts',(-0.0832571466935557,0.891200000000001,
12.2999999999989));
#16410=CARTESIAN_POINT('Ctrl Pts',(0.,-0.208000000000001,12.3));
#16411=CARTESIAN_POINT('Ctrl Pts',(0.,0.891200000000001,12.3));
#16412=CARTESIAN_POINT('Ctrl Pts',(0.0832571466935396,-0.208000000000001,
12.3000000000011));
#16413=CARTESIAN_POINT('Ctrl Pts',(0.0832571466935396,0.891200000000001,
12.3000000000011));
#16414=CARTESIAN_POINT('Ctrl Pts',(0.24977144008061,-0.208000000000001,
12.2998330708736));
#16415=CARTESIAN_POINT('Ctrl Pts',(0.24977144008061,0.891200000000001,12.2998330708736));
#16416=CARTESIAN_POINT('Ctrl Pts',(0.498916532526534,-0.208000000000001,
12.2990818897713));
#16417=CARTESIAN_POINT('Ctrl Pts',(0.498916532526534,0.891200000000001,
12.2990818897713));
#16418=CARTESIAN_POINT('Ctrl Pts',(0.827351903312438,-0.208000000000001,
12.2972483292974));
#16419=CARTESIAN_POINT('Ctrl Pts',(0.827351903312438,0.891200000000001,
12.2972483292974));
#16420=CARTESIAN_POINT('Ctrl Pts',(1.22558901314046,-0.208000000000001,
12.2945066442369));
#16421=CARTESIAN_POINT('Ctrl Pts',(1.22558901314046,0.891200000000001,12.2945066442369));
#16422=CARTESIAN_POINT('Ctrl Pts',(1.60591558979418,-0.208000000000001,
12.2924280532047));
#16423=CARTESIAN_POINT('Ctrl Pts',(1.60591558979418,0.891200000000001,12.2924280532047));
#16424=CARTESIAN_POINT('Ctrl Pts',(1.96338745719096,-0.208000000000001,
12.291968449812));
#16425=CARTESIAN_POINT('Ctrl Pts',(1.96338745719096,0.891200000000001,12.291968449812));
#16426=CARTESIAN_POINT('Ctrl Pts',(2.29394197380175,-0.208000000000001,
12.2935845551378));
#16427=CARTESIAN_POINT('Ctrl Pts',(2.29394197380175,0.891200000000001,12.2935845551378));
#16428=CARTESIAN_POINT('Ctrl Pts',(2.59461297443069,-0.208000000000001,
12.2969132923658));
#16429=CARTESIAN_POINT('Ctrl Pts',(2.59461297443069,0.891200000000001,12.2969132923658));
#16430=CARTESIAN_POINT('Ctrl Pts',(2.86376302967335,-0.208000000000001,
12.3004008390612));
#16431=CARTESIAN_POINT('Ctrl Pts',(2.86376302967335,0.891200000000001,12.3004008390612));
#16432=CARTESIAN_POINT('Ctrl Pts',(3.10127560868576,-0.208000000000001,
12.3010487961961));
#16433=CARTESIAN_POINT('Ctrl Pts',(3.10127560868576,0.891200000000001,12.3010487961961));
#16434=CARTESIAN_POINT('Ctrl Pts',(3.30884480305537,-0.208000000000001,
12.2938762651102));
#16435=CARTESIAN_POINT('Ctrl Pts',(3.30884480305537,0.891200000000001,12.2938762651102));
#16436=CARTESIAN_POINT('Ctrl Pts',(3.48993681214337,-0.208000000000001,
12.2723364229612));
#16437=CARTESIAN_POINT('Ctrl Pts',(3.48993681214337,0.891200000000001,12.2723364229612));
#16438=CARTESIAN_POINT('Ctrl Pts',(3.64927048315907,-0.208000000000001,
12.2301117722792));
#16439=CARTESIAN_POINT('Ctrl Pts',(3.64927048315907,0.891200000000001,12.2301117722792));
#16440=CARTESIAN_POINT('Ctrl Pts',(3.79241297762162,-0.208000000000001,
12.1626050652587));
#16441=CARTESIAN_POINT('Ctrl Pts',(3.79241297762162,0.891200000000001,12.1626050652587));
#16442=CARTESIAN_POINT('Ctrl Pts',(3.92533033057351,-0.208000000000001,
12.0684942936878));
#16443=CARTESIAN_POINT('Ctrl Pts',(3.92533033057351,0.891200000000001,12.0684942936878));
#16444=CARTESIAN_POINT('Ctrl Pts',(4.05395481372655,-0.208000000000001,
11.9514202619535));
#16445=CARTESIAN_POINT('Ctrl Pts',(4.05395481372655,0.891200000000001,11.9514202619535));
#16446=CARTESIAN_POINT('Ctrl Pts',(4.18369962429796,-0.208000000000001,
11.8183570873731));
#16447=CARTESIAN_POINT('Ctrl Pts',(4.18369962429796,0.891200000000001,11.8183570873731));
#16448=CARTESIAN_POINT('Ctrl Pts',(4.3189358499924,-0.208000000000001,11.67764924636));
#16449=CARTESIAN_POINT('Ctrl Pts',(4.3189358499924,0.891200000000001,11.67764924636));
#16450=CARTESIAN_POINT('Ctrl Pts',(4.46255574628753,-0.208000000000001,
11.5373242211525));
#16451=CARTESIAN_POINT('Ctrl Pts',(4.46255574628753,0.891200000000001,11.5373242211525));
#16452=CARTESIAN_POINT('Ctrl Pts',(4.61532593596939,-0.208000000000001,
11.4029224160728));
#16453=CARTESIAN_POINT('Ctrl Pts',(4.61532593596939,0.891200000000001,11.4029224160728));
#16454=CARTESIAN_POINT('Ctrl Pts',(4.77596612414944,-0.208000000000001,
11.2768795166233));
#16455=CARTESIAN_POINT('Ctrl Pts',(4.77596612414944,0.891200000000001,11.2768795166233));
#16456=CARTESIAN_POINT('Ctrl Pts',(4.94211773226968,-0.208000000000001,
11.1598106424589));
#16457=CARTESIAN_POINT('Ctrl Pts',(4.94211773226968,0.891200000000001,11.1598106424589));
#16458=CARTESIAN_POINT('Ctrl Pts',(5.11112998264613,-0.208000000000001,
11.051370419133));
#16459=CARTESIAN_POINT('Ctrl Pts',(5.11112998264613,0.891200000000001,11.051370419133));
#16460=CARTESIAN_POINT('Ctrl Pts',(5.28082876351925,-0.208000000000001,
10.9511663773825));
#16461=CARTESIAN_POINT('Ctrl Pts',(5.28082876351925,0.891200000000001,10.9511663773825));
#16462=CARTESIAN_POINT('Ctrl Pts',(5.45051506148977,-0.208000000000001,
10.8599381259735));
#16463=CARTESIAN_POINT('Ctrl Pts',(5.45051506148977,0.891200000000001,10.8599381259735));
#16464=CARTESIAN_POINT('Ctrl Pts',(5.62101499943423,-0.208000000000001,
10.7795199127532));
#16465=CARTESIAN_POINT('Ctrl Pts',(5.62101499943423,0.891200000000001,10.7795199127532));
#16466=CARTESIAN_POINT('Ctrl Pts',(5.7936769541502,-0.208000000000001,10.7114411549111));
#16467=CARTESIAN_POINT('Ctrl Pts',(5.7936769541502,0.891200000000001,10.7114411549111));
#16468=CARTESIAN_POINT('Ctrl Pts',(5.96961932707136,-0.208000000000001,
10.6558377434042));
#16469=CARTESIAN_POINT('Ctrl Pts',(5.96961932707136,0.891200000000001,10.6558377434042));
#16470=CARTESIAN_POINT('Ctrl Pts',(6.14893768388704,-0.208000000000001,
10.6103475969888));
#16471=CARTESIAN_POINT('Ctrl Pts',(6.14893768388704,0.891200000000001,10.6103475969888));
#16472=CARTESIAN_POINT('Ctrl Pts',(6.32976796473819,-0.208000000000001,
10.5687216653907));
#16473=CARTESIAN_POINT('Ctrl Pts',(6.32976796473819,0.891200000000001,10.5687216653907));
#16474=CARTESIAN_POINT('Ctrl Pts',(6.50892555577775,-0.208000000000001,
10.5222908830264));
#16475=CARTESIAN_POINT('Ctrl Pts',(6.50892555577775,0.891200000000001,10.5222908830264));
#16476=CARTESIAN_POINT('Ctrl Pts',(6.68288828293941,-0.208000000000001,
10.462050267878));
#16477=CARTESIAN_POINT('Ctrl Pts',(6.68288828293941,0.891200000000001,10.462050267878));
#16478=CARTESIAN_POINT('Ctrl Pts',(6.84859008776107,-0.208000000000001,
10.3804015453596));
#16479=CARTESIAN_POINT('Ctrl Pts',(6.84859008776107,0.891200000000001,10.3804015453596));
#16480=CARTESIAN_POINT('Ctrl Pts',(7.00445448641038,-0.208000000000001,
10.2733319413005));
#16481=CARTESIAN_POINT('Ctrl Pts',(7.00445448641038,0.891200000000001,10.2733319413005));
#16482=CARTESIAN_POINT('Ctrl Pts',(7.15081550722288,-0.208000000000001,
10.1414720974144));
#16483=CARTESIAN_POINT('Ctrl Pts',(7.15081550722288,0.891200000000001,10.1414720974144));
#16484=CARTESIAN_POINT('Ctrl Pts',(7.28883796912684,-0.208000000000001,
9.98835756998534));
#16485=CARTESIAN_POINT('Ctrl Pts',(7.28883796912684,0.891200000000001,9.98835756998534));
#16486=CARTESIAN_POINT('Ctrl Pts',(7.41967047354988,-0.208000000000001,
9.81917361987377));
#16487=CARTESIAN_POINT('Ctrl Pts',(7.41967047354988,0.891200000000001,9.81917361987377));
#16488=CARTESIAN_POINT('Ctrl Pts',(7.54360573526532,-0.208000000000001,
9.63939026966049));
#16489=CARTESIAN_POINT('Ctrl Pts',(7.54360573526532,0.891200000000001,9.63939026966049));
#16490=CARTESIAN_POINT('Ctrl Pts',(7.6590003866074,-0.208000000000001,9.45324999450471));
#16491=CARTESIAN_POINT('Ctrl Pts',(7.6590003866074,0.891200000000001,9.45324999450471));
#16492=CARTESIAN_POINT('Ctrl Pts',(7.76209282457502,-0.208000000000001,
9.26297089919836));
#16493=CARTESIAN_POINT('Ctrl Pts',(7.76209282457502,0.891200000000001,9.26297089919836));
#16494=CARTESIAN_POINT('Ctrl Pts',(7.84862074946283,-0.208000000000001,
9.06945407017055));
#16495=CARTESIAN_POINT('Ctrl Pts',(7.84862074946283,0.891200000000001,9.06945407017055));
#16496=CARTESIAN_POINT('Ctrl Pts',(7.91508259073031,-0.208000000000001,
8.87266947141857));
#16497=CARTESIAN_POINT('Ctrl Pts',(7.91508259073031,0.891200000000001,8.87266947141857));
#16498=CARTESIAN_POINT('Ctrl Pts',(7.96007609558387,-0.208000000000001,
8.67216210283894));
#16499=CARTESIAN_POINT('Ctrl Pts',(7.96007609558387,0.891200000000001,8.67216210283894));
#16500=CARTESIAN_POINT('Ctrl Pts',(7.98575825096082,-0.208000000000001,
8.46752658699496));
#16501=CARTESIAN_POINT('Ctrl Pts',(7.98575825096082,0.891200000000001,8.46752658699496));
#16502=CARTESIAN_POINT('Ctrl Pts',(7.9987984391963,-0.208000000000001,8.25883677791438));
#16503=CARTESIAN_POINT('Ctrl Pts',(7.9987984391963,0.891200000000001,8.25883677791438));
#16504=CARTESIAN_POINT('Ctrl Pts',(8.00781893805568,-0.208000000000001,
8.04662057355209));
#16505=CARTESIAN_POINT('Ctrl Pts',(8.00781893805568,0.891200000000001,8.04662057355209));
#16506=CARTESIAN_POINT('Ctrl Pts',(8.02124364536257,-0.208000000000001,
7.8318867323277));
#16507=CARTESIAN_POINT('Ctrl Pts',(8.02124364536257,0.891200000000001,7.8318867323277));
#16508=CARTESIAN_POINT('Ctrl Pts',(8.04494633492827,-0.208000000000001,
7.61613341658679));
#16509=CARTESIAN_POINT('Ctrl Pts',(8.04494633492827,0.891200000000001,7.61613341658679));
#16510=CARTESIAN_POINT('Ctrl Pts',(8.08008348678094,-0.208000000000001,
7.40136016279815));
#16511=CARTESIAN_POINT('Ctrl Pts',(8.08008348678094,0.891200000000001,7.40136016279815));
#16512=CARTESIAN_POINT('Ctrl Pts',(8.12057943633426,-0.208000000000001,
7.19009032473197));
#16513=CARTESIAN_POINT('Ctrl Pts',(8.12057943633426,0.891200000000001,7.19009032473197));
#16514=CARTESIAN_POINT('Ctrl Pts',(8.15569042861283,-0.208000000000001,
6.98516923427904));
#16515=CARTESIAN_POINT('Ctrl Pts',(8.15569042861283,0.891200000000001,6.98516923427904));
#16516=CARTESIAN_POINT('Ctrl Pts',(8.17293082304204,-0.208000000000001,
6.78954489191915));
#16517=CARTESIAN_POINT('Ctrl Pts',(8.17293082304204,0.891200000000001,6.78954489191915));
#16518=CARTESIAN_POINT('Ctrl Pts',(8.16089752265956,-0.208000000000001,
6.60605451948904));
#16519=CARTESIAN_POINT('Ctrl Pts',(8.16089752265956,0.891200000000001,6.60605451948904));
#16520=CARTESIAN_POINT('Ctrl Pts',(8.11207116917844,-0.208000000000001,
6.43720976255638));
#16521=CARTESIAN_POINT('Ctrl Pts',(8.11207116917844,0.891200000000001,6.43720976255638));
#16522=CARTESIAN_POINT('Ctrl Pts',(8.02580908828092,-0.208000000000001,
6.28498018271691));
#16523=CARTESIAN_POINT('Ctrl Pts',(8.02580908828092,0.891200000000001,6.28498018271691));
#16524=CARTESIAN_POINT('Ctrl Pts',(7.90644860448881,-0.208000000000001,
6.15052660592943));
#16525=CARTESIAN_POINT('Ctrl Pts',(7.90644860448881,0.891200000000001,6.15052660592943));
#16526=CARTESIAN_POINT('Ctrl Pts',(7.76106756457749,-0.208000000000001,
6.03389995867286));
#16527=CARTESIAN_POINT('Ctrl Pts',(7.76106756457749,0.891200000000001,6.03389995867286));
#16528=CARTESIAN_POINT('Ctrl Pts',(7.59751903688427,-0.208000000000001,
5.93381436957244));
#16529=CARTESIAN_POINT('Ctrl Pts',(7.59751903688427,0.891200000000001,5.93381436957244));
#16530=CARTESIAN_POINT('Ctrl Pts',(7.42198551710643,-0.208000000000001,
5.84723737025948));
#16531=CARTESIAN_POINT('Ctrl Pts',(7.42198551710643,0.891200000000001,5.84723737025948));
#16532=CARTESIAN_POINT('Ctrl Pts',(7.23853768475023,-0.208000000000001,
5.76979878895671));
#16533=CARTESIAN_POINT('Ctrl Pts',(7.23853768475023,0.891200000000001,5.76979878895671));
#16534=CARTESIAN_POINT('Ctrl Pts',(7.04976847947264,-0.208000000000001,
5.69662713609756));
#16535=CARTESIAN_POINT('Ctrl Pts',(7.04976847947264,0.891200000000001,5.69662713609756));
#16536=CARTESIAN_POINT('Ctrl Pts',(6.85709976037512,-0.208000000000001,
5.62308582598972));
#16537=CARTESIAN_POINT('Ctrl Pts',(6.85709976037512,0.891200000000001,5.62308582598972));
#16538=CARTESIAN_POINT('Ctrl Pts',(6.66121503090593,-0.208000000000001,
5.54547963906641));
#16539=CARTESIAN_POINT('Ctrl Pts',(6.66121503090593,0.891200000000001,5.54547963906641));
#16540=CARTESIAN_POINT('Ctrl Pts',(6.46246210121974,-0.208000000000001,
5.46195513100458));
#16541=CARTESIAN_POINT('Ctrl Pts',(6.46246210121974,0.891200000000001,5.46195513100458));
#16542=CARTESIAN_POINT('Ctrl Pts',(6.26112587698791,-0.208000000000001,
5.37226655127806));
#16543=CARTESIAN_POINT('Ctrl Pts',(6.26112587698791,0.891200000000001,5.37226655127806));
#16544=CARTESIAN_POINT('Ctrl Pts',(6.05762450882876,-0.208000000000001,
5.27709955371581));
#16545=CARTESIAN_POINT('Ctrl Pts',(6.05762450882876,0.891200000000001,5.27709955371581));
#16546=CARTESIAN_POINT('Ctrl Pts',(5.85274048349253,-0.208000000000001,
5.17752467829117));
#16547=CARTESIAN_POINT('Ctrl Pts',(5.85274048349253,0.891200000000001,5.17752467829117));
#16548=CARTESIAN_POINT('Ctrl Pts',(5.6478173738032,-0.208000000000001,5.07442896098936));
#16549=CARTESIAN_POINT('Ctrl Pts',(5.6478173738032,0.891200000000001,5.07442896098936));
#16550=CARTESIAN_POINT('Ctrl Pts',(5.44501860313336,-0.208000000000001,
4.96787993373722));
#16551=CARTESIAN_POINT('Ctrl Pts',(5.44501860313336,0.891200000000001,4.96787993373722));
#16552=CARTESIAN_POINT('Ctrl Pts',(5.24741086000008,-0.208000000000001,
4.85676111532844));
#16553=CARTESIAN_POINT('Ctrl Pts',(5.24741086000008,0.891200000000001,4.85676111532844));
#16554=CARTESIAN_POINT('Ctrl Pts',(5.05850630701875,-0.208000000000001,
4.73929437247794));
#16555=CARTESIAN_POINT('Ctrl Pts',(5.05850630701875,0.891200000000001,4.73929437247794));
#16556=CARTESIAN_POINT('Ctrl Pts',(4.88190185104846,-0.208000000000001,
4.61340315498245));
#16557=CARTESIAN_POINT('Ctrl Pts',(4.88190185104846,0.891200000000001,4.61340315498245));
#16558=CARTESIAN_POINT('Ctrl Pts',(4.7208720035032,-0.208000000000001,4.47714872481864));
#16559=CARTESIAN_POINT('Ctrl Pts',(4.7208720035032,0.891200000000001,4.47714872481864));
#16560=CARTESIAN_POINT('Ctrl Pts',(4.57800047823784,-0.208000000000001,
4.32911151507775));
#16561=CARTESIAN_POINT('Ctrl Pts',(4.57800047823784,0.891200000000001,4.32911151507775));
#16562=CARTESIAN_POINT('Ctrl Pts',(4.4547451964031,-0.208000000000001,4.16885849319143));
#16563=CARTESIAN_POINT('Ctrl Pts',(4.4547451964031,0.891200000000001,4.16885849319143));
#16564=CARTESIAN_POINT('Ctrl Pts',(4.35148411330737,-0.208000000000001,
3.99681013615577));
#16565=CARTESIAN_POINT('Ctrl Pts',(4.35148411330737,0.891200000000001,3.99681013615577));
#16566=CARTESIAN_POINT('Ctrl Pts',(4.26765207024408,-0.208000000000001,
3.81399668859083));
#16567=CARTESIAN_POINT('Ctrl Pts',(4.26765207024408,0.891200000000001,3.81399668859083));
#16568=CARTESIAN_POINT('Ctrl Pts',(4.20184334854117,-0.208000000000001,
3.62185203209172));
#16569=CARTESIAN_POINT('Ctrl Pts',(4.20184334854117,0.891200000000001,3.62185203209172));
#16570=CARTESIAN_POINT('Ctrl Pts',(4.15193466045737,-0.208000000000001,
3.42199345348454));
#16571=CARTESIAN_POINT('Ctrl Pts',(4.15193466045737,0.891200000000001,3.42199345348454));
#16572=CARTESIAN_POINT('Ctrl Pts',(4.11518318246501,-0.208000000000001,
3.21600287470933));
#16573=CARTESIAN_POINT('Ctrl Pts',(4.11518318246501,0.891200000000001,3.21600287470933));
#16574=CARTESIAN_POINT('Ctrl Pts',(4.08854433447712,-0.208000000000001,
3.00529120729351));
#16575=CARTESIAN_POINT('Ctrl Pts',(4.08854433447712,0.891200000000001,3.00529120729351));
#16576=CARTESIAN_POINT('Ctrl Pts',(4.06899962712481,-0.208000000000001,
2.7909834104826));
#16577=CARTESIAN_POINT('Ctrl Pts',(4.06899962712481,0.891200000000001,2.7909834104826));
#16578=CARTESIAN_POINT('Ctrl Pts',(4.05390260344518,-0.208000000000001,
2.57377631141663));
#16579=CARTESIAN_POINT('Ctrl Pts',(4.05390260344518,0.891200000000001,2.57377631141663));
#16580=CARTESIAN_POINT('Ctrl Pts',(4.04126813644791,-0.208000000000001,
2.35385258470204));
#16581=CARTESIAN_POINT('Ctrl Pts',(4.04126813644791,0.891200000000001,2.35385258470204));
#16582=CARTESIAN_POINT('Ctrl Pts',(4.03021014446877,-0.208000000000001,
2.13065748555701));
#16583=CARTESIAN_POINT('Ctrl Pts',(4.03021014446877,0.891200000000001,2.13065748555701));
#16584=CARTESIAN_POINT('Ctrl Pts',(4.02110299519686,-0.208000000000001,
1.91370945705801));
#16585=CARTESIAN_POINT('Ctrl Pts',(4.02110299519686,0.891200000000001,1.91370945705801));
#16586=CARTESIAN_POINT('Ctrl Pts',(4.0150839653859,-0.208000000000001,1.73897559179867));
#16587=CARTESIAN_POINT('Ctrl Pts',(4.0150839653859,0.891200000000001,1.73897559179867));
#16588=CARTESIAN_POINT('Ctrl Pts',(4.01123999191373,-0.208000000000001,
1.60904011456728));
#16589=CARTESIAN_POINT('Ctrl Pts',(4.01123999191373,0.891200000000001,1.60904011456728));
#16590=CARTESIAN_POINT('Ctrl Pts',(4.0089337502854,-0.208000000000001,1.52556315247963));
#16591=CARTESIAN_POINT('Ctrl Pts',(4.0089337502854,0.891200000000001,1.52556315247963));
#16592=CARTESIAN_POINT('Ctrl Pts',(4.00794703095364,-0.208000000000001,
1.48914872207946));
#16593=CARTESIAN_POINT('Ctrl Pts',(4.00794703095364,0.891200000000001,1.48914872207946));
#16594=CARTESIAN_POINT('',(4.,0.5,1.2));
#16595=CARTESIAN_POINT('Ctrl Pts',(3.99628071248376,0.515724022809955,1.08895058147551));
#16596=CARTESIAN_POINT('Ctrl Pts',(3.99695111863745,0.510515400451476,1.10697360799751));
#16597=CARTESIAN_POINT('Ctrl Pts',(3.99759476802297,0.506584394748987,1.12533130577593));
#16598=CARTESIAN_POINT('Ctrl Pts',(3.99821367094827,0.503955544636118,1.14388558371581));
#16599=CARTESIAN_POINT('Ctrl Pts',(3.99883257387358,0.501326694523249,1.16243986165569));
#16600=CARTESIAN_POINT('Ctrl Pts',(3.9994268264293,0.5,1.18119071480602));
#16601=CARTESIAN_POINT('Ctrl Pts',(4.,0.5,1.2));
#16602=CARTESIAN_POINT('',(4.00232316926925,0.5,1.28));
#16603=CARTESIAN_POINT('Ctrl Pts',(4.,0.5,1.2));
#16604=CARTESIAN_POINT('Ctrl Pts',(4.00048648979365,0.5,1.21596466714547));
#16605=CARTESIAN_POINT('Ctrl Pts',(4.00095995114739,0.5,1.23195096410174));
#16606=CARTESIAN_POINT('Ctrl Pts',(4.00142258957318,0.5,1.2479547597375));
#16607=CARTESIAN_POINT('Ctrl Pts',(4.00187639644938,0.5,1.26397226336412));
#16608=CARTESIAN_POINT('Ctrl Pts',(4.00232316926925,0.5,1.28));
#16609=CARTESIAN_POINT('',(4.,0.42,1.2));
#16610=CARTESIAN_POINT('Ctrl Pts',(4.00232316926925,0.5,1.28000000000001));
#16611=CARTESIAN_POINT('Ctrl Pts',(4.00230299966747,0.5,1.2792764262932));
#16612=CARTESIAN_POINT('Ctrl Pts',(4.00228281233137,0.499990182776602,1.27855285870449));
#16613=CARTESIAN_POINT('Ctrl Pts',(4.00214695508649,0.499858141613736,1.27368777894256));
#16614=CARTESIAN_POINT('Ctrl Pts',(4.0020311113454,0.499424139669874,1.26956098182442));
#16615=CARTESIAN_POINT('Ctrl Pts',(4.00163265096412,0.496820195244168,1.25544601244678));
#16616=CARTESIAN_POINT('Ctrl Pts',(4.00135768601021,0.493062784524195,1.24585198650422));
#16617=CARTESIAN_POINT('Ctrl Pts',(4.00086839188745,0.482409927602859,1.22901639363533));
#16618=CARTESIAN_POINT('Ctrl Pts',(4.00065589411436,0.475764975074544,1.22182250919509));
#16619=CARTESIAN_POINT('Ctrl Pts',(4.00029434770309,0.459596631686721,1.20969879529552));
#16620=CARTESIAN_POINT('Ctrl Pts',(4.00015547253981,0.450041622442072,1.20511554604908));
#16621=CARTESIAN_POINT('Ctrl Pts',(4.0000256112516,0.433366702909574,1.20083901694649));
#16622=CARTESIAN_POINT('Ctrl Pts',(4.,0.426689213070844,1.2));
#16623=CARTESIAN_POINT('Ctrl Pts',(4.,0.420000000000006,1.2));
#16624=CARTESIAN_POINT('',(4.,0.08,1.2));
#16625=CARTESIAN_POINT('',(4.,0.,1.2));
#16626=CARTESIAN_POINT('',(4.00232316926925,0.,1.28));
#16627=CARTESIAN_POINT('Ctrl Pts',(4.,0.0799999999999845,1.2));
#16628=CARTESIAN_POINT('Ctrl Pts',(4.,0.0712353307855553,1.2));
#16629=CARTESIAN_POINT('Ctrl Pts',(4.00004401876777,0.0625213699048051,
1.20144045396));
#16630=CARTESIAN_POINT('Ctrl Pts',(4.00022068673853,0.0453965107457132,
1.20727262474139));
#16631=CARTESIAN_POINT('Ctrl Pts',(4.00035699792145,0.0371755072686487,
1.21178919233617));
#16632=CARTESIAN_POINT('Ctrl Pts',(4.00068867210099,0.0232931356215582,
1.22293442282227));
#16633=CARTESIAN_POINT('Ctrl Pts',(4.00087563722023,0.0175589585117979,
1.22927281222884));
#16634=CARTESIAN_POINT('Ctrl Pts',(4.0012611591677,0.00894266831347314,
1.24252529496691));
#16635=CARTESIAN_POINT('Ctrl Pts',(4.00145268528988,0.00581567214900459,
1.24917507680124));
#16636=CARTESIAN_POINT('Ctrl Pts',(4.0018273760135,0.00170830451366606,
1.2623297822669));
#16637=CARTESIAN_POINT('Ctrl Pts',(4.00200757811868,0.000536463326316975,
1.26871413063067));
#16638=CARTESIAN_POINT('Ctrl Pts',(4.00221809264031,8.14663303026943E-5,
1.27623581107857));
#16639=CARTESIAN_POINT('Ctrl Pts',(4.00224792817779,3.83285587785669E-5,
1.27730329002437));
#16640=CARTESIAN_POINT('Ctrl Pts',(4.00229289069437,5.52723888419683E-6,
1.27891413388588));
#16641=CARTESIAN_POINT('Ctrl Pts',(4.00230803498764,-4.43319744566652E-17,
1.27945706571897));
#16642=CARTESIAN_POINT('Ctrl Pts',(4.00232316926925,-2.77555756156289E-17,
1.28));
#16643=CARTESIAN_POINT('',(4.,0.,1.2));
#16644=CARTESIAN_POINT('Ctrl Pts',(4.00232316926925,-5.55111512312578E-17,
1.28));
#16645=CARTESIAN_POINT('Ctrl Pts',(4.00187639644938,-5.55111512312578E-17,
1.26397226336412));
#16646=CARTESIAN_POINT('Ctrl Pts',(4.00142258957318,-5.55111512312578E-17,
1.2479547597375));
#16647=CARTESIAN_POINT('Ctrl Pts',(4.00095995114739,-5.55111512312578E-17,
1.23195096410174));
#16648=CARTESIAN_POINT('Ctrl Pts',(4.00048648979365,-5.55111512312578E-17,
1.21596466714547));
#16649=CARTESIAN_POINT('Ctrl Pts',(4.,-5.55111512312578E-17,1.2));
#16650=CARTESIAN_POINT('Origin',(3.96221895354333,0.899296250818234,1.20115091904051));
#16651=CARTESIAN_POINT('Ctrl Pts',(2.8805419932544,0.136565758583769,0.899998731395832));
#16652=CARTESIAN_POINT('Ctrl Pts',(2.88783884470249,0.181143949322972,0.77752115893973));
#16653=CARTESIAN_POINT('Ctrl Pts',(2.8993736353594,0.270316072740132,0.532522763406263));
#16654=CARTESIAN_POINT('Ctrl Pts',(2.9196026767358,0.376119687828295,0.241829720054866));
#16655=CARTESIAN_POINT('Ctrl Pts',(2.9730125063753,0.451017094008355,0.0360507877994292));
#16656=CARTESIAN_POINT('Ctrl Pts',(3.01389049537916,0.482936356580544,-0.0516466653633009));
#16657=CARTESIAN_POINT('Ctrl Pts',(3.05985159914742,0.506141825662096,-0.115403167672718));
#16658=CARTESIAN_POINT('Ctrl Pts',(3.11058052482755,0.52437488961235,-0.165498099163513));
#16659=CARTESIAN_POINT('Ctrl Pts',(3.21732310712232,0.544182531031752,-0.219919146695976));
#16660=CARTESIAN_POINT('Ctrl Pts',(3.35194656845354,0.548863870554337,-0.232781021327076));
#16661=CARTESIAN_POINT('Ctrl Pts',(3.49778753718399,0.541692651427306,-0.213078258705599));
#16662=CARTESIAN_POINT('Ctrl Pts',(3.6265539989599,0.526408247588463,-0.171084704288551));
#16663=CARTESIAN_POINT('Ctrl Pts',(3.73739288004811,0.503000447457269,-0.10677230198899));
#16664=CARTESIAN_POINT('Ctrl Pts',(3.84808202669468,0.46276591626256,0.00377116395081768));
#16665=CARTESIAN_POINT('Ctrl Pts',(3.9204363567822,0.403359946625806,0.166987724108605));
#16666=CARTESIAN_POINT('Ctrl Pts',(3.96110129343823,0.333991249229589,0.357576653821691));
#16667=CARTESIAN_POINT('Ctrl Pts',(3.98904669612228,0.242194739655562,0.60978549106108));
#16668=CARTESIAN_POINT('Ctrl Pts',(3.99598983762634,0.174461093782049,0.795882153635894));
#16669=CARTESIAN_POINT('Ctrl Pts',(4.,0.129452050955555,0.919543482472952));
#16670=CARTESIAN_POINT('Ctrl Pts',(2.8805419932544,0.114073328609723,0.891812156388963));
#16671=CARTESIAN_POINT('Ctrl Pts',(2.88783872593927,0.158650793796348,0.769336577372186));
#16672=CARTESIAN_POINT('Ctrl Pts',(2.89937600566135,0.247822523947933,0.524339262327005));
#16673=CARTESIAN_POINT('Ctrl Pts',(2.9195545062059,0.353605214767559,0.233703707930933));
#16674=CARTESIAN_POINT('Ctrl Pts',(2.97295217221839,0.428508407704055,0.0279088766928571));
#16675=CARTESIAN_POINT('Ctrl Pts',(3.01382111580078,0.460433630477054,-0.0598049519870154));
#16676=CARTESIAN_POINT('Ctrl Pts',(3.05980698983149,0.483652921552891,-0.123599429913622));
#16677=CARTESIAN_POINT('Ctrl Pts',(3.11055009633998,0.501895319408686,-0.173720006099127));
#16678=CARTESIAN_POINT('Ctrl Pts',(3.21736084446955,0.521716087056444,-0.228177117647598));
#16679=CARTESIAN_POINT('Ctrl Pts',(3.35195992956318,0.526387882971129,-0.241012771431496));
#16680=CARTESIAN_POINT('Ctrl Pts',(3.4978195772253,0.519215743708778,-0.221307480759004));
#16681=CARTESIAN_POINT('Ctrl Pts',(3.62657748910597,0.503928259570136,-0.179305463287815));
#16682=CARTESIAN_POINT('Ctrl Pts',(3.73742854793082,0.480515769664525,-0.114980175938938));
#16683=CARTESIAN_POINT('Ctrl Pts',(3.8481659110119,0.440262093407297,-0.00438410937216693));
#16684=CARTESIAN_POINT('Ctrl Pts',(3.92047099581111,0.380857917917725,0.158827521406752));
#16685=CARTESIAN_POINT('Ctrl Pts',(3.96112079679389,0.311492110423669,0.349408511178906));
#16686=CARTESIAN_POINT('Ctrl Pts',(3.98905963354223,0.219691592626807,0.601628360920028));
#16687=CARTESIAN_POINT('Ctrl Pts',(3.99598979363886,0.151969157512326,0.787694222187545));
#16688=CARTESIAN_POINT('Ctrl Pts',(4.,0.106959620981509,0.911356907466082));
#16689=CARTESIAN_POINT('Ctrl Pts',(2.90060526052275,0.0747531580267383,
0.878696094802245));
#16690=CARTESIAN_POINT('Ctrl Pts',(2.90791147887875,0.11938857342105,0.756061298898396));
#16691=CARTESIAN_POINT('Ctrl Pts',(2.91940548593204,0.208587912033988,0.510988130229062));
#16692=CARTESIAN_POINT('Ctrl Pts',(2.93971734293678,0.313973665333152,0.221443152707394));
#16693=CARTESIAN_POINT('Ctrl Pts',(2.99225360162521,0.387510002496177,0.0194037268425803));
#16694=CARTESIAN_POINT('Ctrl Pts',(3.03182463200544,0.418305990574516,-0.0652075550124495));
#16695=CARTESIAN_POINT('Ctrl Pts',(3.07550932869219,0.440350515088388,-0.125774388336927));
#16696=CARTESIAN_POINT('Ctrl Pts',(3.12310116181815,0.457414736169163,-0.172657950436938));
#16697=CARTESIAN_POINT('Ctrl Pts',(3.22253873842663,0.475909198392738,-0.223471067781167));
#16698=CARTESIAN_POINT('Ctrl Pts',(3.35113610177915,0.480513385154656,-0.236120966944487));
#16699=CARTESIAN_POINT('Ctrl Pts',(3.49306055599084,0.473537376896056,-0.216954541776055));
#16700=CARTESIAN_POINT('Ctrl Pts',(3.61818010203025,0.458676526293589,-0.176124690311888));
#16701=CARTESIAN_POINT('Ctrl Pts',(3.72462733520835,0.436152051570704,-0.114239204625684));
#16702=CARTESIAN_POINT('Ctrl Pts',(3.83038111193484,0.397744836296198,-0.00871624791484828));
#16703=CARTESIAN_POINT('Ctrl Pts',(3.9009685656033,0.340106698388871,0.149643234484944));
#16704=CARTESIAN_POINT('Ctrl Pts',(3.94117885677219,0.271582068768333,0.337913107043865));
#16705=CARTESIAN_POINT('Ctrl Pts',(3.96895833352272,0.180412639324759,0.588399055784644));
#16706=CARTESIAN_POINT('Ctrl Pts',(3.97590794636788,0.112784383202069,0.774206162398828));
#16707=CARTESIAN_POINT('Ctrl Pts',(3.97991463942917,0.0678142790554765,
0.897760508092115));
#16708=CARTESIAN_POINT('Ctrl Pts',(2.94249302709539,0.0602041295977449,
0.875896230734658));
#16709=CARTESIAN_POINT('Ctrl Pts',(2.9498187182991,0.104958509222874,0.752934583292915));
#16710=CARTESIAN_POINT('Ctrl Pts',(2.96122932239305,0.194214391674412,0.507706061703817));
#16711=CARTESIAN_POINT('Ctrl Pts',(2.98167866039825,0.298713075662704,0.220598287083263));
#16712=CARTESIAN_POINT('Ctrl Pts',(3.03238256717175,0.369411850319645,0.0263550001302063));
#16713=CARTESIAN_POINT('Ctrl Pts',(3.06921861113533,0.397866861024811,-0.0518244992525782));
#16714=CARTESIAN_POINT('Ctrl Pts',(3.10816802129538,0.417497270910729,-0.105758607148775));
#16715=CARTESIAN_POINT('Ctrl Pts',(3.14922022130347,0.432127742064011,-0.145955496278401));
#16716=CARTESIAN_POINT('Ctrl Pts',(3.23345429671096,0.44788976904434,-0.189261309491687));
#16717=CARTESIAN_POINT('Ctrl Pts',(3.34945338625923,0.452326189141897,-0.201450273532941));
#16718=CARTESIAN_POINT('Ctrl Pts',(3.48321409508734,0.445757094142106,-0.183401833354763));
#16719=CARTESIAN_POINT('Ctrl Pts',(3.60071367717697,0.431778372428901,-0.144995611094893));
#16720=CARTESIAN_POINT('Ctrl Pts',(3.69800063294054,0.411094803582314,-0.0881679727351601));
#16721=CARTESIAN_POINT('Ctrl Pts',(3.79348421490767,0.376489211798969,0.00691010927644513));
#16722=CARTESIAN_POINT('Ctrl Pts',(3.86034830022832,0.322543181908982,0.15512560826841));
#16723=CARTESIAN_POINT('Ctrl Pts',(3.89959878244922,0.255782808716465,0.338548226129213));
#16724=CARTESIAN_POINT('Ctrl Pts',(3.9270272401522,0.165919778027693,0.585444873790373));
#16725=CARTESIAN_POINT('Ctrl Pts',(3.93398126610095,0.0985194096795488,
0.770625863889823));
#16726=CARTESIAN_POINT('Ctrl Pts',(3.9379807468151,0.0536302550833677,0.893957802521238));
#16727=CARTESIAN_POINT('Ctrl Pts',(2.96041691837963,0.0598609284456541,
0.876839168150358));
#16728=CARTESIAN_POINT('Ctrl Pts',(2.96775093160951,0.104666149296221,0.753737835589749));
#16729=CARTESIAN_POINT('Ctrl Pts',(2.97912606655434,0.193946192378553,0.508442933213105));
#16730=CARTESIAN_POINT('Ctrl Pts',(2.99962978200786,0.298063454185075,0.22238310742424));
#16731=CARTESIAN_POINT('Ctrl Pts',(3.04954854909233,0.3675485376204,0.0314744096967656));
#16732=CARTESIAN_POINT('Ctrl Pts',(3.08521348818013,0.395002362532113,-0.0439543543258271));
#16733=CARTESIAN_POINT('Ctrl Pts',(3.12213883760405,0.413600983366687,-0.095053645101818));
#16734=CARTESIAN_POINT('Ctrl Pts',(3.16039395937928,0.427190868210603,-0.132391546843465));
#16735=CARTESIAN_POINT('Ctrl Pts',(3.23812841779038,0.441784834591999,-0.172488139936633));
#16736=CARTESIAN_POINT('Ctrl Pts',(3.34873452432173,0.446148626378716,-0.184477559333837));
#16737=CARTESIAN_POINT('Ctrl Pts',(3.47900358892302,0.439753569654038,-0.166907285386653));
#16738=CARTESIAN_POINT('Ctrl Pts',(3.59324181436642,0.426152042057545,-0.129537395445201));
#16739=CARTESIAN_POINT('Ctrl Pts',(3.68661013453806,0.406255788910909,-0.074872889193063));
#16740=CARTESIAN_POINT('Ctrl Pts',(3.77770331808059,0.373275236268507,0.0157404344730694));
#16741=CARTESIAN_POINT('Ctrl Pts',(3.84296982682103,0.320909227628625,0.15961486075811));
#16742=CARTESIAN_POINT('Ctrl Pts',(3.88180827116063,0.254904039155253,0.340962625655547));
#16743=CARTESIAN_POINT('Ctrl Pts',(3.90908594858962,0.165599667112526,0.586324371301513));
#16744=CARTESIAN_POINT('Ctrl Pts',(3.91604071966527,0.0982977998881255,
0.771234731787688));
#16745=CARTESIAN_POINT('Ctrl Pts',(3.92003711807002,0.053443240348906,0.894471621281276));
#16746=CARTESIAN_POINT('',(2.96041691837963,0.0598609284456542,0.876839168150358));
#16747=CARTESIAN_POINT('Ctrl Pts',(3.91996278980377,0.0542766424889417,
0.892181867720203));
#16748=CARTESIAN_POINT('Ctrl Pts',(3.91598305831422,0.098853560185636,0.769707792919649));
#16749=CARTESIAN_POINT('Ctrl Pts',(3.90900147842788,0.165876213955253,0.585564565095701));
#16750=CARTESIAN_POINT('Ctrl Pts',(3.8818082711687,0.25490403915566,0.340962625654429));
#16751=CARTESIAN_POINT('Ctrl Pts',(3.84296982682819,0.320909227629314,0.159614860756216));
#16752=CARTESIAN_POINT('Ctrl Pts',(3.77770331808652,0.373275236269741,0.0157404344696786));
#16753=CARTESIAN_POINT('Ctrl Pts',(3.68661013454203,0.406255788912611,-0.0748728891977425));
#16754=CARTESIAN_POINT('Ctrl Pts',(3.59324181436885,0.426152042059393,-0.129537395450278));
#16755=CARTESIAN_POINT('Ctrl Pts',(3.47900358892426,0.439753569655855,-0.166907285391647));
#16756=CARTESIAN_POINT('Ctrl Pts',(3.34873452432189,0.446148626380414,-0.184477559338504));
#16757=CARTESIAN_POINT('Ctrl Pts',(3.23812841778915,0.441784834593533,-0.172488139940845));
#16758=CARTESIAN_POINT('Ctrl Pts',(3.16039395937664,0.42719086821175,-0.132391546846618));
#16759=CARTESIAN_POINT('Ctrl Pts',(3.12213883760094,0.413600983367549,-0.0950536451041868));
#16760=CARTESIAN_POINT('Ctrl Pts',(3.0852134881768,0.395002362532705,-0.0439543543274574));
#16761=CARTESIAN_POINT('Ctrl Pts',(3.04954854908906,0.367548537620745,0.0314744096958174));
#16762=CARTESIAN_POINT('Ctrl Pts',(2.99962978200522,0.298063454185146,0.222383107424044));
#16763=CARTESIAN_POINT('Ctrl Pts',(2.97912606655288,0.193946192378579,0.508442933213033));
#16764=CARTESIAN_POINT('Ctrl Pts',(2.96775093160902,0.10466614929623,0.753737835589723));
#16765=CARTESIAN_POINT('Ctrl Pts',(2.96041691837963,0.0598609284456542,
0.876839168150358));
#16766=CARTESIAN_POINT('',(2.88054198318953,0.136565694403419,0.899998899355773));
#16767=CARTESIAN_POINT('Origin',(2.96041691837963,0.135036338108527,0.904200779616412));
#16768=CARTESIAN_POINT('Ctrl Pts',(2.8805419932544,0.136565756430656,0.899998730612164));
#16769=CARTESIAN_POINT('Ctrl Pts',(2.88284752702291,0.150650807367472,0.86130037131219));
#16770=CARTESIAN_POINT('Ctrl Pts',(2.88498553892976,0.164719389055088,0.822647260902508));
#16771=CARTESIAN_POINT('Ctrl Pts',(2.88704880814836,0.178807167502167,0.783941407829676));
#16772=CARTESIAN_POINT('Ctrl Pts',(2.88896759991875,0.19190846960258,0.747945876237076));
#16773=CARTESIAN_POINT('Ctrl Pts',(2.89082106771812,0.205026680469038,0.711903888191579));
#16774=CARTESIAN_POINT('Ctrl Pts',(2.89270923333433,0.218175254353227,0.675778478440476));
#16775=CARTESIAN_POINT('Ctrl Pts',(2.8943613782485,0.229680256501893,0.644168744908261));
#16776=CARTESIAN_POINT('Ctrl Pts',(2.8960399023492,0.241208574106251,0.612494952688007));
#16777=CARTESIAN_POINT('Ctrl Pts',(2.89783714020707,0.252754941297751,0.58077156963465));
#16778=CARTESIAN_POINT('Ctrl Pts',(2.89864412818268,0.25793944119282,0.566527273278611));
#16779=CARTESIAN_POINT('Ctrl Pts',(2.89947544083931,0.263127363552645,0.552273573777938));
#16780=CARTESIAN_POINT('Ctrl Pts',(2.90034147758514,0.268317099136106,0.538014892486267));
#16781=CARTESIAN_POINT('Ctrl Pts',(2.9008098570909,0.271123868940463,0.530303355847108));
#16782=CARTESIAN_POINT('Ctrl Pts',(2.9012883190563,0.273930533419183,0.522592108587758));
#16783=CARTESIAN_POINT('Ctrl Pts',(2.90177824359068,0.276734477144718,0.514888336536346));
#16784=CARTESIAN_POINT('Ctrl Pts',(2.90336905113846,0.285839011678269,0.489873833555445));
#16785=CARTESIAN_POINT('Ctrl Pts',(2.90508092831803,0.294927759204885,0.464902705019619));
#16786=CARTESIAN_POINT('Ctrl Pts',(2.9069985081457,0.304047491932523,0.439846445343648));
#16787=CARTESIAN_POINT('Ctrl Pts',(2.90873365103152,0.312299580911864,0.417174017268099));
#16788=CARTESIAN_POINT('Ctrl Pts',(2.91063698175396,0.320577156553037,0.39443156516467));
#16789=CARTESIAN_POINT('Ctrl Pts',(2.91279212081837,0.328903729190399,0.371554494920593));
#16790=CARTESIAN_POINT('Ctrl Pts',(2.91480972174193,0.336698910912354,0.350137409213762));
#16791=CARTESIAN_POINT('Ctrl Pts',(2.91704780723451,0.344537153750784,0.328602014061762));
#16792=CARTESIAN_POINT('Ctrl Pts',(2.91959741789068,0.352425801447324,0.306928132700273));
#16793=CARTESIAN_POINT('Ctrl Pts',(2.92200870659192,0.359886472751267,0.286430106810531));
#16794=CARTESIAN_POINT('Ctrl Pts',(2.92469846160555,0.367392338442971,0.265807910360929));
#16795=CARTESIAN_POINT('Ctrl Pts',(2.92776715496281,0.374936938954671,0.245079290868043));
#16796=CARTESIAN_POINT('Ctrl Pts',(2.93069401968964,0.382132843707919,0.225308705095369));
#16797=CARTESIAN_POINT('Ctrl Pts',(2.93396547545055,0.389364082820534,0.205441038968201));
#16798=CARTESIAN_POINT('Ctrl Pts',(2.9376928277366,0.39661170582491,0.18552835846838));
#16799=CARTESIAN_POINT('Ctrl Pts',(2.93958647111764,0.400293786904793,0.175411923869907));
#16800=CARTESIAN_POINT('Ctrl Pts',(2.94159818848892,0.403979870729996,0.165284491819052));
#16801=CARTESIAN_POINT('Ctrl Pts',(2.94374529812117,0.407665924548674,0.155157142210448));
#16802=CARTESIAN_POINT('Ctrl Pts',(2.94585156221408,0.411281856723828,0.145222450233562));
#16803=CARTESIAN_POINT('Ctrl Pts',(2.94808951946978,0.414900689447676,0.135279789064636));
#16804=CARTESIAN_POINT('Ctrl Pts',(2.9504855759059,0.418527466733358,0.125315300391463));
#16805=CARTESIAN_POINT('Ctrl Pts',(2.95400177923571,0.423849748035309,0.11069245273051));
#16806=CARTESIAN_POINT('Ctrl Pts',(2.95785705464788,0.429189653995361,0.0960211817194013));
#16807=CARTESIAN_POINT('Ctrl Pts',(2.96215449172343,0.434550976790958,0.0812910684362362));
#16808=CARTESIAN_POINT('Ctrl Pts',(2.96625355726838,0.439664818636796,0.067240903472608));
#16809=CARTESIAN_POINT('Ctrl Pts',(2.97075478982208,0.444798246534775,0.0531369262729893));
#16810=CARTESIAN_POINT('Ctrl Pts',(2.97577209874859,0.449940564089527,0.0390085249421184));
#16811=CARTESIAN_POINT('Ctrl Pts',(2.97918365263398,0.453437118455781,0.0294018207983813));
#16812=CARTESIAN_POINT('Ctrl Pts',(2.9828331038583,0.456936448561027,0.0197874903744428));
#16813=CARTESIAN_POINT('Ctrl Pts',(2.98676781952857,0.460434520497467,0.0101766167408878));
#16814=CARTESIAN_POINT('Ctrl Pts',(2.99149133630772,0.46463385861261,-0.00136096987898278));
#16815=CARTESIAN_POINT('Ctrl Pts',(2.99662739646606,0.468834248967704,-0.012901447504355));
#16816=CARTESIAN_POINT('Ctrl Pts',(3.00229038497435,0.473028530998255,-0.0244251426459792));
#16817=CARTESIAN_POINT('Ctrl Pts',(3.00781030054253,0.477116846318673,-0.0356576966450058));
#16818=CARTESIAN_POINT('Ctrl Pts',(3.01383080706225,0.481199452809662,-0.0468745657640879));
#16819=CARTESIAN_POINT('Ctrl Pts',(3.02048134180172,0.485255100567417,-0.058017366372349));
#16820=CARTESIAN_POINT('Ctrl Pts',(3.0267482302952,0.489076792094842,-0.0685173775222242));
#16821=CARTESIAN_POINT('Ctrl Pts',(3.03357181695739,0.492873280426181,-0.0789481434599518));
#16822=CARTESIAN_POINT('Ctrl Pts',(3.04109585537297,0.49662045126684,-0.0892434107056537));
#16823=CARTESIAN_POINT('Ctrl Pts',(3.04486925792249,0.498499705893495,-0.0944066203448309));
#16824=CARTESIAN_POINT('Ctrl Pts',(3.04881908834144,0.500366209445059,-0.0995347966931213));
#16825=CARTESIAN_POINT('Ctrl Pts',(3.05296508290757,0.502214984022785,-0.104614263086121));
#16826=CARTESIAN_POINT('Ctrl Pts',(3.060391064349,0.505526364557563,-0.113712206309427));
#16827=CARTESIAN_POINT('Ctrl Pts',(3.06845132453832,0.508780407076342,-0.122652614628499));
#16828=CARTESIAN_POINT('Ctrl Pts',(3.07713855153503,0.511902111536166,-0.131229427118859));
#16829=CARTESIAN_POINT('Ctrl Pts',(3.08491334356286,0.514695937800484,-0.138905401673171));
#16830=CARTESIAN_POINT('Ctrl Pts',(3.09319019714925,0.517383779610739,-0.146290186333133));
#16831=CARTESIAN_POINT('Ctrl Pts',(3.10194077335529,0.51992284141446,-0.153266201284675));
#16832=CARTESIAN_POINT('Ctrl Pts',(3.10852358399233,0.521832905695494,-0.158514059750891));
#16833=CARTESIAN_POINT('Ctrl Pts',(3.11537464890556,0.523659162604978,-0.16353165935619));
#16834=CARTESIAN_POINT('Ctrl Pts',(3.12247262936851,0.525387979268932,-0.168281544087149));
#16835=CARTESIAN_POINT('Ctrl Pts',(3.1307377782938,0.527401076834736,-0.173812484174152));
#16836=CARTESIAN_POINT('Ctrl Pts',(3.13933120153844,0.529279332314368,-0.178972948674204));
#16837=CARTESIAN_POINT('Ctrl Pts',(3.14814690854809,0.5310009427641,-0.183703034491738));
#16838=CARTESIAN_POINT('Ctrl Pts',(3.15731996650597,0.532792339916818,-0.188624857699165));
#16839=CARTESIAN_POINT('Ctrl Pts',(3.16673349682595,0.534414126214741,-0.19308067891295));
#16840=CARTESIAN_POINT('Ctrl Pts',(3.17624049743953,0.535859067329586,-0.197050621979487));
#16841=CARTESIAN_POINT('Ctrl Pts',(3.18104129060916,0.5365887257904,-0.199055342114923));
#16842=CARTESIAN_POINT('Ctrl Pts',(3.18586550820414,0.537273559539332,-0.200936907366632));
#16843=CARTESIAN_POINT('Ctrl Pts',(3.19069207830152,0.537914163621228,-0.202696952606885));
#16844=CARTESIAN_POINT('Ctrl Pts',(3.20477225839308,0.539782948422546,-0.207831396622426));
#16845=CARTESIAN_POINT('Ctrl Pts',(3.21888668941886,0.541279553722331,-0.211943285861518));
#16846=CARTESIAN_POINT('Ctrl Pts',(3.232951619864,0.542478223729469,-0.215236604611607));
#16847=CARTESIAN_POINT('Ctrl Pts',(3.24728773102728,0.543700004849358,-0.218593420621578));
#16848=CARTESIAN_POINT('Ctrl Pts',(3.26157252361816,0.544612257958954,-0.22109981541258));
#16849=CARTESIAN_POINT('Ctrl Pts',(3.27574767618657,0.545277946538929,-0.222928779726012));
#16850=CARTESIAN_POINT('Ctrl Pts',(3.29045467092517,0.545968611305745,-0.224826365547746));
#16851=CARTESIAN_POINT('Ctrl Pts',(3.30504387474672,0.546393830448175,-0.225994645510384));
#16852=CARTESIAN_POINT('Ctrl Pts',(3.31947992236691,0.546607405586862,-0.226581438351777));
#16853=CARTESIAN_POINT('Ctrl Pts',(3.32858799458099,0.546742155612456,-0.226951660985751));
#16854=CARTESIAN_POINT('Ctrl Pts',(3.33763568635411,0.54679232725762,-0.22708950642932));
#16855=CARTESIAN_POINT('Ctrl Pts',(3.34661911478556,0.546768383881266,-0.227023722524826));
#16856=CARTESIAN_POINT('Ctrl Pts',(3.35530982102777,0.546745220692298,-0.226960082168163));
#16857=CARTESIAN_POINT('Ctrl Pts',(3.36393308913914,0.546652688354262,-0.22670585164083));
#16858=CARTESIAN_POINT('Ctrl Pts',(3.37248678968118,0.546498757350756,-0.226282929666532));
#16859=CARTESIAN_POINT('Ctrl Pts',(3.38746886531583,0.5462291423548,-0.225542168521652));
#16860=CARTESIAN_POINT('Ctrl Pts',(3.40224291180634,0.545772076519649,-0.224286390428826));
#16861=CARTESIAN_POINT('Ctrl Pts',(3.41684838029837,0.545155788972577,-0.222593154277811));
#16862=CARTESIAN_POINT('Ctrl Pts',(3.43217875145474,0.544508913670987,-0.220815878960379));
#16863=CARTESIAN_POINT('Ctrl Pts',(3.44732409536616,0.543686565379946,-0.218556495566705));
#16864=CARTESIAN_POINT('Ctrl Pts',(3.46234328791778,0.542702696012868,-0.215853336663856));
#16865=CARTESIAN_POINT('Ctrl Pts',(3.47471047134688,0.541892553064698,-0.213627487179962));
#16866=CARTESIAN_POINT('Ctrl Pts',(3.48699354766808,0.540972452748603,-0.211099532310594));
#16867=CARTESIAN_POINT('Ctrl Pts',(3.4992235181442,0.539941812764334,-0.208267872198965));
#16868=CARTESIAN_POINT('Ctrl Pts',(3.51606259294448,0.538522755880987,-0.20436904541751));
#16869=CARTESIAN_POINT('Ctrl Pts',(3.53278579816242,0.536895749242862,-0.19989888138042));
#16870=CARTESIAN_POINT('Ctrl Pts',(3.54937570118406,0.535050013825628,-0.194827764961743));
#16871=CARTESIAN_POINT('Ctrl Pts',(3.56588793090174,0.533212920072418,-0.189780391320013));
#16872=CARTESIAN_POINT('Ctrl Pts',(3.58226861273737,0.531159094717761,-0.184137552497226));
#16873=CARTESIAN_POINT('Ctrl Pts',(3.59849464287997,0.528860502418511,-0.17782222202114));
#16874=CARTESIAN_POINT('Ctrl Pts',(3.61188615228933,0.526963450574455,-0.172610114885227));
#16875=CARTESIAN_POINT('Ctrl Pts',(3.62517276692824,0.524899303618216,-0.166938917701686));
#16876=CARTESIAN_POINT('Ctrl Pts',(3.6383336937211,0.522643621255268,-0.160741481313188));
#16877=CARTESIAN_POINT('Ctrl Pts',(3.65581519087164,0.519647426122431,-0.15250950280048));
#16878=CARTESIAN_POINT('Ctrl Pts',(3.67305736175662,0.516313909635384,-0.143350741483978));
#16879=CARTESIAN_POINT('Ctrl Pts',(3.68980508007049,0.512617597665949,-0.133195207771734));
#16880=CARTESIAN_POINT('Ctrl Pts',(3.70149620034588,0.510037304219394,-0.126105909763166));
#16881=CARTESIAN_POINT('Ctrl Pts',(3.71294709160308,0.507280253568292,-0.118530975326379));
#16882=CARTESIAN_POINT('Ctrl Pts',(3.72408551786322,0.504340318645617,-0.11045357048307));
#16883=CARTESIAN_POINT('Ctrl Pts',(3.73141197837736,0.502406534049653,-0.105140540952761));
#16884=CARTESIAN_POINT('Ctrl Pts',(3.73860597392585,0.500392914616266,-0.0996081670093482));
#16885=CARTESIAN_POINT('Ctrl Pts',(3.74564087975467,0.498301423080776,-0.0938618412238027));
#16886=CARTESIAN_POINT('Ctrl Pts',(3.7558814748348,0.495256873736462,-0.0854970106205085));
#16887=CARTESIAN_POINT('Ctrl Pts',(3.76577710849098,0.49204828623515,-0.0766814888849327));
#16888=CARTESIAN_POINT('Ctrl Pts',(3.77523378380848,0.488702069947446,-0.0674878351664772));
#16889=CARTESIAN_POINT('Ctrl Pts',(3.78430306882689,0.485492930558862,-0.0586707971342026));
#16890=CARTESIAN_POINT('Ctrl Pts',(3.79296886515126,0.482157211977029,-0.0495059856267071));
#16891=CARTESIAN_POINT('Ctrl Pts',(3.8011755061435,0.478730534395561,-0.0400912663216156));
#16892=CARTESIAN_POINT('Ctrl Pts',(3.80703355753486,0.476284508866618,-0.0333708663946939));
#16893=CARTESIAN_POINT('Ctrl Pts',(3.81265712292028,0.473792923732884,-0.0265252924823697));
#16894=CARTESIAN_POINT('Ctrl Pts',(3.81803733335002,0.471271007296339,-0.0195963840004684));
#16895=CARTESIAN_POINT('Ctrl Pts',(3.83298840477383,0.464262851526213,-0.000341634217944583));
#16896=CARTESIAN_POINT('Ctrl Pts',(3.84610260970866,0.457005364869118,0.0195981465464975));
#16897=CARTESIAN_POINT('Ctrl Pts',(3.85774603965601,0.449598868493433,0.0399473281480481));
#16898=CARTESIAN_POINT('Ctrl Pts',(3.86822850312385,0.442930873921912,0.0582674927132378));
#16899=CARTESIAN_POINT('Ctrl Pts',(3.87751904506637,0.43614275421269,0.0769176983817686));
#16900=CARTESIAN_POINT('Ctrl Pts',(3.8858524605855,0.429301526663394,0.0957138166416987));
#16901=CARTESIAN_POINT('Ctrl Pts',(3.89358602033688,0.422952744233937,0.113156953051177));
#16902=CARTESIAN_POINT('Ctrl Pts',(3.90049500946549,0.416558315606917,0.130725501357744));
#16903=CARTESIAN_POINT('Ctrl Pts',(3.90673917358546,0.410161791821601,0.148299806064416));
#16904=CARTESIAN_POINT('Ctrl Pts',(3.91218759686158,0.404580425219352,0.163634484811763));
#16905=CARTESIAN_POINT('Ctrl Pts',(3.91712836591243,0.398998754805198,0.178969998275458));
#16906=CARTESIAN_POINT('Ctrl Pts',(3.92165664060923,0.393431214595175,0.19426668932237));
#16907=CARTESIAN_POINT('Ctrl Pts',(3.92700398270312,0.386856626232525,0.212330222435795));
#16908=CARTESIAN_POINT('Ctrl Pts',(3.93177725325759,0.380301392122174,0.230340580178059));
#16909=CARTESIAN_POINT('Ctrl Pts',(3.93610473145847,0.373771682027175,0.24828081126449));
#16910=CARTESIAN_POINT('Ctrl Pts',(3.94061484429769,0.366966395444824,0.266978182529147));
#16911=CARTESIAN_POINT('Ctrl Pts',(3.94464053769894,0.360188774116983,0.285599544131731));
#16912=CARTESIAN_POINT('Ctrl Pts',(3.94829463739126,0.353429038225082,0.304171765902933));
#16913=CARTESIAN_POINT('Ctrl Pts',(3.95132569513222,0.34782187051561,0.319577332610564));
#16914=CARTESIAN_POINT('Ctrl Pts',(3.95410037541624,0.342226650443178,0.334950073455211));
#16915=CARTESIAN_POINT('Ctrl Pts',(3.95666897647058,0.336630239649571,0.3503260857794));
#16916=CARTESIAN_POINT('Ctrl Pts',(3.95905101066503,0.33144031657685,0.364585282266353));
#16917=CARTESIAN_POINT('Ctrl Pts',(3.9612551996362,0.32624922422557,0.378847691319743));
#16918=CARTESIAN_POINT('Ctrl Pts',(3.96330637589166,0.321063603501971,0.393095067199633));
#16919=CARTESIAN_POINT('Ctrl Pts',(3.96691882338176,0.311930900976914,0.418186961229127));
#16920=CARTESIAN_POINT('Ctrl Pts',(3.97005955397289,0.302813398031445,0.443237094756921));
#16921=CARTESIAN_POINT('Ctrl Pts',(3.97284569678751,0.293717730509341,0.468227235952075));
#16922=CARTESIAN_POINT('Ctrl Pts',(3.97543099278593,0.285277749355281,0.491415893652218));
#16923=CARTESIAN_POINT('Ctrl Pts',(3.97771036641322,0.276856252186037,0.514553767021461));
#16924=CARTESIAN_POINT('Ctrl Pts',(3.97975648063729,0.268447161865253,0.537657552854712));
#16925=CARTESIAN_POINT('Ctrl Pts',(3.98161738897013,0.260799228008218,0.558670078485823));
#16926=CARTESIAN_POINT('Ctrl Pts',(3.98328556717928,0.253158069280994,0.579663989600761));
#16927=CARTESIAN_POINT('Ctrl Pts',(3.98480166079054,0.245527014801487,0.600630139523244));
#16928=CARTESIAN_POINT('Ctrl Pts',(3.98708880152943,0.234014997699602,0.632259146643622));
#16929=CARTESIAN_POINT('Ctrl Pts',(3.98903054474691,0.222528738766917,0.663817383775745));
#16930=CARTESIAN_POINT('Ctrl Pts',(3.99073668214014,0.211074767458993,0.695286911387915));
#16931=CARTESIAN_POINT('Ctrl Pts',(3.99252654604435,0.199058707155059,0.728300765828298));
#16932=CARTESIAN_POINT('Ctrl Pts',(3.99405681992494,0.187078032354012,0.761217399398529));
#16933=CARTESIAN_POINT('Ctrl Pts',(3.99542341045194,0.175123022359742,0.794063519491691));
#16934=CARTESIAN_POINT('Ctrl Pts',(3.99689014952689,0.162291907293772,0.829316718492614));
#16935=CARTESIAN_POINT('Ctrl Pts',(3.99816813525302,0.149490243752837,0.864489000093564));
#16936=CARTESIAN_POINT('Ctrl Pts',(3.99934516717317,0.136688680681622,0.899661005656283));
#16937=CARTESIAN_POINT('Ctrl Pts',(3.99956694488036,0.134276595454529,0.906288155368636));
#16938=CARTESIAN_POINT('Ctrl Pts',(3.99978506111859,0.13186447030226,0.912915414774516));
#16939=CARTESIAN_POINT('Ctrl Pts',(4.,0.129452050955556,0.919543482472952));
#16940=CARTESIAN_POINT('Ctrl Pts',(2.80364725095274,0.0799999999984753,
1.19999999979367));
#16941=CARTESIAN_POINT('Ctrl Pts',(2.81754102919364,0.0799999999984752,
1.19999900193533));
#16942=CARTESIAN_POINT('Ctrl Pts',(2.84544455850609,0.0799999999992679,
1.19257285603888));
#16943=CARTESIAN_POINT('Ctrl Pts',(2.86597664848058,0.08,1.17203236493386));
#16944=CARTESIAN_POINT('Ctrl Pts',(2.87292353761413,0.08,1.16));
#16945=CARTESIAN_POINT('Ctrl Pts',(2.80364725095274,0.0560640559714148,
1.19999999979413));
#16946=CARTESIAN_POINT('Ctrl Pts',(2.81749662686061,0.0560640559714148,
1.19999900512479));
#16947=CARTESIAN_POINT('Ctrl Pts',(2.84542227433267,0.0560640559720564,
1.19253372046443));
#16948=CARTESIAN_POINT('Ctrl Pts',(2.86599884964717,0.0560640559726492,
1.17199391138533));
#16949=CARTESIAN_POINT('Ctrl Pts',(2.87292353761413,0.0560640559726492,
1.16));
#16950=CARTESIAN_POINT('Ctrl Pts',(2.80364869399581,0.0146264256801572,
1.22009235108497));
#16951=CARTESIAN_POINT('Ctrl Pts',(2.82104450402995,0.0146264256801572,
1.22009110170889));
#16952=CARTESIAN_POINT('Ctrl Pts',(2.85594987654874,0.0146264256803497,
1.21081090750893));
#16953=CARTESIAN_POINT('Ctrl Pts',(2.88162611926498,0.0146264256805277,
1.18511138910848));
#16954=CARTESIAN_POINT('Ctrl Pts',(2.8903240242984,0.0146264256805276,1.17004617567119));
#16955=CARTESIAN_POINT('Ctrl Pts',(2.80365170727521,-4.27466544297813E-18,
1.26204804161335));
#16956=CARTESIAN_POINT('Ctrl Pts',(2.8283278847973,-1.21341104992333E-18,
1.26204626935751));
#16957=CARTESIAN_POINT('Ctrl Pts',(2.87787022921565,-1.44254953221807E-16,
1.24886602237777));
#16958=CARTESIAN_POINT('Ctrl Pts',(2.91432062943914,-1.3683229200899E-16,
1.21239421763245));
#16959=CARTESIAN_POINT('Ctrl Pts',(2.92665871822345,-1.79312001105175E-16,
1.19102402098974));
#16960=CARTESIAN_POINT('Ctrl Pts',(2.80365299659412,9.71445146547012E-17,
1.27999999958735));
#16961=CARTESIAN_POINT('Ctrl Pts',(2.8314405530759,1.0015366995025E-16,
1.27999800387066));
#16962=CARTESIAN_POINT('Ctrl Pts',(2.88724761170081,-9.28783814262485E-17,
1.26514571207777));
#16963=CARTESIAN_POINT('Ctrl Pts',(2.92831179164978,-1.37991962040859E-16,
1.22406472986772));
#16964=CARTESIAN_POINT('Ctrl Pts',(2.94220556991688,-1.80411241501588E-16,
1.2));
#16965=CARTESIAN_POINT('',(2.80365299659412,3.70074341541719E-17,1.27999999977075));
#16966=CARTESIAN_POINT('',(2.80364725095274,0.0800000000002712,1.2));
#16967=CARTESIAN_POINT('Origin',(2.80365299155732,0.0800000001034236,1.27999999989746));
#16968=CARTESIAN_POINT('',(2.87292353761412,0.08,1.16));
#16969=CARTESIAN_POINT('Origin',(2.80364150531137,0.08,1.12));
#16970=CARTESIAN_POINT('',(2.94220556991688,0.,1.2));
#16971=CARTESIAN_POINT('Origin',(2.94220556991688,0.08,1.2));
#16972=CARTESIAN_POINT('Ctrl Pts',(2.94220556991688,-1.80411241501588E-16,
1.2));
#16973=CARTESIAN_POINT('Ctrl Pts',(2.92831179164978,-1.37991962040859E-16,
1.22406472986772));
#16974=CARTESIAN_POINT('Ctrl Pts',(2.88724761170081,-9.28783814262485E-17,
1.26514571207777));
#16975=CARTESIAN_POINT('Ctrl Pts',(2.8314405530759,1.0015366995025E-16,
1.27999800387066));
#16976=CARTESIAN_POINT('Ctrl Pts',(2.80365299659412,9.71445146547012E-17,
1.27999999958735));
#16977=CARTESIAN_POINT('Ctrl Pts',(2.97150805818412,0.0370740550288554,
0.944346301619442));
#16978=CARTESIAN_POINT('Ctrl Pts',(2.96893696336745,0.0199732893870456,
1.00206772104214));
#16979=CARTESIAN_POINT('Ctrl Pts',(2.96630502643548,0.00868534462510511,
1.06150700206698));
#16980=CARTESIAN_POINT('Ctrl Pts',(2.96341860243339,0.00343337974894797,
1.12146150337824));
#16981=CARTESIAN_POINT('Ctrl Pts',(2.94780950688205,0.0373896078982158,
0.943281193781355));
#16982=CARTESIAN_POINT('Ctrl Pts',(2.94518931216128,0.0202159191784814,
1.00097915593662));
#16983=CARTESIAN_POINT('Ctrl Pts',(2.94251940811176,0.00887573436834648,
1.06032244794287));
#16984=CARTESIAN_POINT('Ctrl Pts',(2.93958582132594,0.00354285648585825,
1.12021175717441));
#16985=CARTESIAN_POINT('Ctrl Pts',(2.90676713760894,0.0568417110754077,
0.947037633415512));
#16986=CARTESIAN_POINT('Ctrl Pts',(2.90406861189144,0.0400195254220902,
1.00340948853811));
#16987=CARTESIAN_POINT('Ctrl Pts',(2.90132962478988,0.0288803134333534,
1.06138518563746));
#16988=CARTESIAN_POINT('Ctrl Pts',(2.89832135056208,0.0236236998222968,
1.11979038686856));
#16989=CARTESIAN_POINT('Ctrl Pts',(2.89185002996796,0.0967164840794545,
0.958121804096728));
#16990=CARTESIAN_POINT('Ctrl Pts',(2.88922085401446,0.0807642369419484,
1.01185984132483));
#16991=CARTESIAN_POINT('Ctrl Pts',(2.88654630615169,0.0702230541962401,
1.06707171515406));
#16992=CARTESIAN_POINT('Ctrl Pts',(2.88361236102833,0.0652969522996504,
1.1226636989333));
#16993=CARTESIAN_POINT('Ctrl Pts',(2.89160349189832,0.113778583470735,0.963164633118633));
#16994=CARTESIAN_POINT('Ctrl Pts',(2.88903135432334,0.0981978858859783,
1.01577658887176));
#16995=CARTESIAN_POINT('Ctrl Pts',(2.88640501551798,0.0879133139917624,
1.06981306289243));
#16996=CARTESIAN_POINT('Ctrl Pts',(2.8835300538724,0.0831281904379304,1.12422135153853));
#16997=CARTESIAN_POINT('',(2.96341860243339,0.00343337974894797,1.12146150337824));
#16998=CARTESIAN_POINT('',(2.88353005387238,0.0831281904379304,1.12422135153898));
#16999=CARTESIAN_POINT('Origin',(2.96341860243339,0.0831281904379304,1.12844270307795));
#17000=CARTESIAN_POINT('',(2.89160351335905,0.11377873136113,0.96316419414885));
#17001=CARTESIAN_POINT('Ctrl Pts',(2.8835300538724,0.0831281904379304,1.12422135153853));
#17002=CARTESIAN_POINT('Ctrl Pts',(2.88640501551798,0.0879133139917624,
1.06981306289243));
#17003=CARTESIAN_POINT('Ctrl Pts',(2.88903135432334,0.0981978858859783,
1.01577658887176));
#17004=CARTESIAN_POINT('Ctrl Pts',(2.89160349189832,0.113778583470735,0.963164633118633));
#17005=CARTESIAN_POINT('',(2.97150807857098,0.0370741994904978,0.944345814008723));
#17006=CARTESIAN_POINT('Origin',(2.97150805818412,0.113778583470735,0.967071074808825));
#17007=CARTESIAN_POINT('Ctrl Pts',(2.97150805818412,0.0370740550288554,
0.944346301619442));
#17008=CARTESIAN_POINT('Ctrl Pts',(2.96893696336745,0.0199732893870456,
1.00206772104214));
#17009=CARTESIAN_POINT('Ctrl Pts',(2.96630502643548,0.00868534462510511,
1.06150700206698));
#17010=CARTESIAN_POINT('Ctrl Pts',(2.96341860243339,0.00343337974894797,
1.12146150337824));
#17011=CARTESIAN_POINT('Ctrl Pts',(2.89160353535339,0.113778846700823,0.963163744264181));
#17012=CARTESIAN_POINT('Ctrl Pts',(2.89200309459449,0.115874999468036,0.954990934520135));
#17013=CARTESIAN_POINT('Ctrl Pts',(2.89105241294694,0.118516767083136,0.946926805316735));
#17014=CARTESIAN_POINT('Ctrl Pts',(2.8887998347044,0.12151892108873,0.939367876351702));
#17015=CARTESIAN_POINT('Ctrl Pts',(2.89193225405221,0.091029389236732,0.956439946820171));
#17016=CARTESIAN_POINT('Ctrl Pts',(2.89244979273278,0.0933382871392351,
0.947816425216694));
#17017=CARTESIAN_POINT('Ctrl Pts',(2.89143805103303,0.0961424440727286,
0.939168089922756));
#17018=CARTESIAN_POINT('Ctrl Pts',(2.88899324581141,0.0991663031639316,
0.931175208977201));
#17019=CARTESIAN_POINT('Ctrl Pts',(2.91219550748833,0.0516302792459275,
0.945758016401462));
#17020=CARTESIAN_POINT('Ctrl Pts',(2.91287652263897,0.0549833683958626,
0.934311081329529));
#17021=CARTESIAN_POINT('Ctrl Pts',(2.91159668209949,0.0586720092836598,
0.922844854319782));
#17022=CARTESIAN_POINT('Ctrl Pts',(2.90847135897849,0.0624299397708595,
0.91206627137828));
#17023=CARTESIAN_POINT('Ctrl Pts',(2.95373418875325,0.0373110094222872,
0.943546496072754));
#17024=CARTESIAN_POINT('Ctrl Pts',(2.95449085000615,0.0420466727985156,
0.927625463037334));
#17025=CARTESIAN_POINT('Ctrl Pts',(2.95277547249147,0.0472656493538997,
0.911724687618538));
#17026=CARTESIAN_POINT('Ctrl Pts',(2.94868907631857,0.0526474168866845,
0.89665812635227));
#17027=CARTESIAN_POINT('Ctrl Pts',(2.97150810162045,0.0370743439314857,
0.944345326468057));
#17028=CARTESIAN_POINT('Ctrl Pts',(2.97229749829158,0.0423247695708639,
0.926623268322567));
#17029=CARTESIAN_POINT('Ctrl Pts',(2.97039533243128,0.0481773468294725,
0.90893953762639));
#17030=CARTESIAN_POINT('Ctrl Pts',(2.96589752617094,0.0542766837559666,
0.892181754340009));
#17031=CARTESIAN_POINT('',(2.88879983479628,0.121518920962533,0.939367876658545));
#17032=CARTESIAN_POINT('',(2.96589753208429,0.0542766627970602,0.892181811924114));
#17033=CARTESIAN_POINT('Origin',(2.96589752635434,0.129452089417722,0.919543376799038));
#17034=CARTESIAN_POINT('Ctrl Pts',(2.96589754105586,0.0542766635709679,
0.892181809797819));
#17035=CARTESIAN_POINT('Ctrl Pts',(2.97039533662793,0.0481773339172204,
0.908939576641134));
#17036=CARTESIAN_POINT('Ctrl Pts',(2.97229749742078,0.0423247637789863,
0.926623287872219));
#17037=CARTESIAN_POINT('Ctrl Pts',(2.97150810162045,0.0370743439314857,
0.944345326468057));
#17038=CARTESIAN_POINT('Ctrl Pts',(2.89160353535339,0.113778846700823,0.963163744264181));
#17039=CARTESIAN_POINT('Ctrl Pts',(2.89200309458905,0.115874999439544,0.954990934631221));
#17040=CARTESIAN_POINT('Ctrl Pts',(2.89105241297279,0.118516767011321,0.946926805535954));
#17041=CARTESIAN_POINT('Ctrl Pts',(2.88879983479625,0.121518920966312,0.93936787665993));
#17042=CARTESIAN_POINT('Ctrl Pts',(2.87292353761413,0.08,1.16));
#17043=CARTESIAN_POINT('Ctrl Pts',(2.87920815162899,0.0800000000000001,
1.14911472922029));
#17044=CARTESIAN_POINT('Ctrl Pts',(2.88286933791013,0.0809375160872416,
1.13672531827616));
#17045=CARTESIAN_POINT('Ctrl Pts',(2.88353005387235,0.0831281904378509,
1.12422135153943));
#17046=CARTESIAN_POINT('Ctrl Pts',(2.87292353761413,0.0560640559726493,
1.16));
#17047=CARTESIAN_POINT('Ctrl Pts',(2.87947165153049,0.0562707216725976,
1.14867500509237));
#17048=CARTESIAN_POINT('Ctrl Pts',(2.88327482610756,0.057283711013126,1.1353889478833));
#17049=CARTESIAN_POINT('Ctrl Pts',(2.88363979674692,0.0593532062534744,
1.12214448139916));
#17050=CARTESIAN_POINT('Ctrl Pts',(2.89032400439417,0.0146263981036585,
1.17004616417948));
#17051=CARTESIAN_POINT('Ctrl Pts',(2.89862998177407,0.015162040564682,1.15493509506255));
#17052=CARTESIAN_POINT('Ctrl Pts',(2.90339459648587,0.0163044774309504,
1.13733803743769));
#17053=CARTESIAN_POINT('Ctrl Pts',(2.90376961212187,0.0181889922805759,
1.11960219988233));
#17054=CARTESIAN_POINT('Ctrl Pts',(2.92665871822345,1.04444016743217E-16,
1.19102402098974));
#17055=CARTESIAN_POINT('Ctrl Pts',(2.93795081424088,0.000240558124196419,
1.16964064866978));
#17056=CARTESIAN_POINT('Ctrl Pts',(2.94450524794608,0.00132703835077383,
1.14520540513807));
#17057=CARTESIAN_POINT('Ctrl Pts',(2.94554401660275,0.0035154873015423,
1.12052419372636));
#17058=CARTESIAN_POINT('Ctrl Pts',(2.94220556991688,5.55111512312578E-17,
1.2));
#17059=CARTESIAN_POINT('Ctrl Pts',(2.95477479794662,1.89492314713005E-16,
1.17610550316648));
#17060=CARTESIAN_POINT('Ctrl Pts',(2.96209717050889,0.00102898107136256,
1.14890923524034));
#17061=CARTESIAN_POINT('Ctrl Pts',(2.96341860243333,0.00343337974886057,
1.12146150337924));
#17062=CARTESIAN_POINT('Ctrl Pts',(2.96341860243333,0.00343337974886057,
1.12146150337924));
#17063=CARTESIAN_POINT('Ctrl Pts',(2.96209717050889,0.00102898107136256,
1.14890923524034));
#17064=CARTESIAN_POINT('Ctrl Pts',(2.95477479794662,1.89492314713005E-16,
1.17610550316648));
#17065=CARTESIAN_POINT('Ctrl Pts',(2.94220556991688,5.55111512312578E-17,
1.2));
#17066=CARTESIAN_POINT('Ctrl Pts',(2.8729150760721,0.08,1.1599951409471));
#17067=CARTESIAN_POINT('Ctrl Pts',(2.87917356064383,0.0800000000000001,
1.14909663226456));
#17068=CARTESIAN_POINT('Ctrl Pts',(2.88286933791013,0.0809375160872416,
1.13672531827616));
#17069=CARTESIAN_POINT('Ctrl Pts',(2.88353005387235,0.0831281904378509,
1.12422135153943));
#17070=CARTESIAN_POINT('Ctrl Pts',(2.88879983479625,0.121518920966305,0.939367876659928));
#17071=CARTESIAN_POINT('Ctrl Pts',(2.8880324319677,0.122541686734965,0.936792718960852));
#17072=CARTESIAN_POINT('Ctrl Pts',(2.8871159230781,0.123551627030471,0.934256686681854));
#17073=CARTESIAN_POINT('Ctrl Pts',(2.88605564938321,0.124542858554496,0.931774551486074));
#17074=CARTESIAN_POINT('Ctrl Pts',(2.88899324674614,0.0991663025264055,
0.931175212345719));
#17075=CARTESIAN_POINT('Ctrl Pts',(2.88820270097191,0.100171613150583,0.928602454646129));
#17076=CARTESIAN_POINT('Ctrl Pts',(2.887256914194,0.101172190427294,0.926046640793733));
#17077=CARTESIAN_POINT('Ctrl Pts',(2.88617479048184,0.102143858159124,0.923571684284616));
#17078=CARTESIAN_POINT('Ctrl Pts',(2.90847130245117,0.0624298642422617,
0.91206627056425));
#17079=CARTESIAN_POINT('Ctrl Pts',(2.90747172794183,0.0636341682311426,
0.908814316971422));
#17080=CARTESIAN_POINT('Ctrl Pts',(2.90628712830328,0.0648169887234241,
0.905621914364158));
#17081=CARTESIAN_POINT('Ctrl Pts',(2.90492140034315,0.0659768590565696,
0.902493719598966));
#17082=CARTESIAN_POINT('Ctrl Pts',(2.94868907688287,0.0526474135734431,
0.89665813737666));
#17083=CARTESIAN_POINT('Ctrl Pts',(2.94731633955782,0.0543286937237626,
0.892038265656662));
#17084=CARTESIAN_POINT('Ctrl Pts',(2.94567970499161,0.0559838108192925,
0.887492074720039));
#17085=CARTESIAN_POINT('Ctrl Pts',(2.9437870193114,0.0576045375805993,0.883038551101561));
#17086=CARTESIAN_POINT('Ctrl Pts',(2.96589752635434,0.054276679754843,0.892181765332982));
#17087=CARTESIAN_POINT('Ctrl Pts',(2.96436522474194,0.0561698833733057,
0.886980231140826));
#17088=CARTESIAN_POINT('Ctrl Pts',(2.96253475240426,0.0580349143566106,
0.881856100627612));
#17089=CARTESIAN_POINT('Ctrl Pts',(2.96041677700223,0.059860909263175,0.876839220853787));
#17090=CARTESIAN_POINT('',(2.88605571002765,0.124542801858886,0.931774693457122));
#17091=CARTESIAN_POINT('Origin',(2.96041689814401,0.135036214484351,0.904201119271044));
#17092=CARTESIAN_POINT('Origin',(2.81153837945173,0.0396614298686474,0.932336834374758));
#17093=CARTESIAN_POINT('Origin',(2.83103982275571,0.116960654826865,0.953478215069898));
#17094=CARTESIAN_POINT('Origin',(2.96041689814401,0.135036214484351,0.904201119271044));
#17095=CARTESIAN_POINT('Origin',(2.96041689814401,0.135036214484351,0.904201119271044));
#17096=CARTESIAN_POINT('Origin',(3.43968169690401,0.263987455675949,0.316006143873433));
#17097=CARTESIAN_POINT('',(-4.5,0.0542766412926824,0.892181871006898));
#17098=CARTESIAN_POINT('Ctrl Pts',(4.,0.0542766412926824,0.892181871006898));
#17099=CARTESIAN_POINT('Ctrl Pts',(4.,0.618092213764235,1.0973939570023));
#17100=CARTESIAN_POINT('Ctrl Pts',(3.99999413894399,0.0543424242950403,
0.892001133693336));
#17101=CARTESIAN_POINT('Ctrl Pts',(3.99999413894399,0.618157996766593,1.09721321968874));
#17102=CARTESIAN_POINT('Ctrl Pts',(3.99855414331412,0.0704990924696518,
0.84761105270997));
#17103=CARTESIAN_POINT('Ctrl Pts',(3.99855414331412,0.634314664941205,1.05282313870537));
#17104=CARTESIAN_POINT('Ctrl Pts',(3.99545186687381,0.102617065619348,0.759367646722529));
#17105=CARTESIAN_POINT('Ctrl Pts',(3.99545186687381,0.666432638090901,0.96457973271793));
#17106=CARTESIAN_POINT('Ctrl Pts',(3.98977740850449,0.150154761706454,0.628758900150308));
#17107=CARTESIAN_POINT('Ctrl Pts',(3.98977740850449,0.713970334178007,0.833970986145709));
#17108=CARTESIAN_POINT('Ctrl Pts',(3.97841403016118,0.21121967143493,0.460984439550287));
#17109=CARTESIAN_POINT('Ctrl Pts',(3.97841403016118,0.775035243906483,0.666196525545688));
#17110=CARTESIAN_POINT('Ctrl Pts',(3.95259200169988,0.280544576017307,0.270515829604361));
#17111=CARTESIAN_POINT('Ctrl Pts',(3.95259200169988,0.84436014848886,0.475727915599762));
#17112=CARTESIAN_POINT('Ctrl Pts',(3.90986572419832,0.340085651878976,0.10692806814439));
#17113=CARTESIAN_POINT('Ctrl Pts',(3.90986572419832,0.903901224350529,0.312140154139791));
#17114=CARTESIAN_POINT('Ctrl Pts',(3.84598208672298,0.387862727674237,-0.024338368770661));
#17115=CARTESIAN_POINT('Ctrl Pts',(3.84598208672298,0.95167830014579,0.18087371722474));
#17116=CARTESIAN_POINT('Ctrl Pts',(3.75872318140661,0.423488332610525,-0.122218913887524));
#17117=CARTESIAN_POINT('Ctrl Pts',(3.75872318140661,0.987303905082078,0.0829931721078771));
#17118=CARTESIAN_POINT('Ctrl Pts',(3.64881642260075,0.448607387242674,-0.1912329492874));
#17119=CARTESIAN_POINT('Ctrl Pts',(3.64881642260075,1.01242295971423,0.0139791367080011));
#17120=CARTESIAN_POINT('Ctrl Pts',(3.52045328348988,0.465105650196583,-0.236561554213491));
#17121=CARTESIAN_POINT('Ctrl Pts',(3.52045328348988,1.02892122266814,-0.0313494682180899));
#17122=CARTESIAN_POINT('Ctrl Pts',(3.3816469894381,0.473698270059216,-0.260169583260034));
#17123=CARTESIAN_POINT('Ctrl Pts',(3.3816469894381,1.03751384253077,-0.0549574972646329));
#17124=CARTESIAN_POINT('Ctrl Pts',(3.2451100102617,0.472026186036982,-0.255575570165513));
#17125=CARTESIAN_POINT('Ctrl Pts',(3.2451100102617,1.03584175850854,-0.0503634841701119));
#17126=CARTESIAN_POINT('Ctrl Pts',(3.12452733970665,0.456428987719484,-0.212722619981431));
#17127=CARTESIAN_POINT('Ctrl Pts',(3.12452733970665,1.02024456019104,-0.00751053398602988));
#17128=CARTESIAN_POINT('Ctrl Pts',(3.03063129752059,0.423994474883979,-0.12360952835487));
#17129=CARTESIAN_POINT('Ctrl Pts',(3.03063129752059,0.987810047355532,0.0816025576405311));
#17130=CARTESIAN_POINT('Ctrl Pts',(2.96639254265844,0.374982215648855,0.0110505471700891));
#17131=CARTESIAN_POINT('Ctrl Pts',(2.96639254265844,0.938797788120408,0.21626263316549));
#17132=CARTESIAN_POINT('Ctrl Pts',(2.92780415844446,0.3125142105656,0.182679980574709));
#17133=CARTESIAN_POINT('Ctrl Pts',(2.92780415844446,0.876329783037153,0.38789206657011));
#17134=CARTESIAN_POINT('Ctrl Pts',(2.90717911786689,0.241012720183584,0.379128710856649));
#17135=CARTESIAN_POINT('Ctrl Pts',(2.90717911786689,0.804828292655137,0.58434079685205));
#17136=CARTESIAN_POINT('Ctrl Pts',(2.89676647174986,0.173526397310964,0.564545859071197));
#17137=CARTESIAN_POINT('Ctrl Pts',(2.89676647174986,0.737341969782517,0.769757945066598));
#17138=CARTESIAN_POINT('Ctrl Pts',(2.88965455295895,0.120639229722747,0.709852157798736));
#17139=CARTESIAN_POINT('Ctrl Pts',(2.88965455295895,0.6844548021943,0.915064243794137));
#17140=CARTESIAN_POINT('Ctrl Pts',(2.88410012960048,0.0831761921549105,
0.812781007580546));
#17141=CARTESIAN_POINT('Ctrl Pts',(2.88410012960048,0.646991764626463,1.01799309357595));
#17142=CARTESIAN_POINT('Ctrl Pts',(2.88050601962429,0.0610892789569565,
0.873464302857379));
#17143=CARTESIAN_POINT('Ctrl Pts',(2.88050601962429,0.624904851428509,1.07867638885278));
#17144=CARTESIAN_POINT('Ctrl Pts',(2.87936339380802,0.0542766412926821,
0.892181871006899));
#17145=CARTESIAN_POINT('Ctrl Pts',(2.87936339380802,0.618092213764235,1.0973939570023));
#17146=CARTESIAN_POINT('',(2.88019546786692,0.529127141944176,1.04944304294295));
#17147=CARTESIAN_POINT('Ctrl Pts',(2.88019546787498,0.529127141999364,1.04944304281375));
#17148=CARTESIAN_POINT('Ctrl Pts',(2.88033620447493,0.398430560163569,0.999217108032501));
#17149=CARTESIAN_POINT('Ctrl Pts',(2.88044239084245,0.267517984580123,0.949554742349327));
#17150=CARTESIAN_POINT('Ctrl Pts',(2.88054197312457,0.13656563129969,0.899999067707368));
#17151=CARTESIAN_POINT('Ctrl Pts',(4.,0.524122951685637,1.06319194266973));
#17152=CARTESIAN_POINT('Ctrl Pts',(3.99999413894399,0.524188734687995,1.06301120535617));
#17153=CARTESIAN_POINT('Ctrl Pts',(3.99855414331412,0.540345402862606,1.0186211243728));
#17154=CARTESIAN_POINT('Ctrl Pts',(3.99545186687381,0.572463376012303,0.930377718385363));
#17155=CARTESIAN_POINT('Ctrl Pts',(3.98977740850449,0.620001072099409,0.799768971813143));
#17156=CARTESIAN_POINT('Ctrl Pts',(3.97841403016118,0.681065981827884,0.631994511213121));
#17157=CARTESIAN_POINT('Ctrl Pts',(3.95259200169988,0.750390886410261,0.441525901267195));
#17158=CARTESIAN_POINT('Ctrl Pts',(3.90986572419832,0.80993196227193,0.277938139807224));
#17159=CARTESIAN_POINT('Ctrl Pts',(3.84598208672298,0.857709038067191,0.146671702892173));
#17160=CARTESIAN_POINT('Ctrl Pts',(3.75872318140661,0.893334643003479,0.0487911577753098));
#17161=CARTESIAN_POINT('Ctrl Pts',(3.64881642260075,0.918453697635628,-0.0202228776245657));
#17162=CARTESIAN_POINT('Ctrl Pts',(3.52045328348988,0.934951960589537,-0.0655514825506567));
#17163=CARTESIAN_POINT('Ctrl Pts',(3.3816469894381,0.943544580452171,-0.0891595115971992));
#17164=CARTESIAN_POINT('Ctrl Pts',(3.2451100102617,0.941872496429936,-0.0845654985026787));
#17165=CARTESIAN_POINT('Ctrl Pts',(3.12452733970665,0.926275298112438,-0.041712548318597));
#17166=CARTESIAN_POINT('Ctrl Pts',(3.03063129752059,0.893840785276933,0.0474005433079645));
#17167=CARTESIAN_POINT('Ctrl Pts',(2.96639254265844,0.844828526041809,0.182060618832923));
#17168=CARTESIAN_POINT('Ctrl Pts',(2.92780415844446,0.782360520958554,0.353690052237544));
#17169=CARTESIAN_POINT('Ctrl Pts',(2.90717911786689,0.710859030576538,0.550138782519483));
#17170=CARTESIAN_POINT('Ctrl Pts',(2.89692008845523,0.644368326537099,0.732820490471484));
#17171=CARTESIAN_POINT('Ctrl Pts',(2.88992562590405,0.59249855766718,0.875331509193915));
#17172=CARTESIAN_POINT('Ctrl Pts',(2.88454584060419,0.556036094594039,0.975511303145068));
#17173=CARTESIAN_POINT('Ctrl Pts',(2.88115416462358,0.534942607774809,1.03346518187847));
#17174=CARTESIAN_POINT('Ctrl Pts',(2.88019546785078,0.529127141844543,1.04944304320548));
#17175=CARTESIAN_POINT('Ctrl Pts',(2.88605571006501,0.12454279754309,0.931774691915435));
#17176=CARTESIAN_POINT('Ctrl Pts',(2.88491303328969,0.256571286428345,0.978937914242353));
#17177=CARTESIAN_POINT('Ctrl Pts',(2.88378009846091,0.388637587381446,1.02596265267948));
#17178=CARTESIAN_POINT('Ctrl Pts',(2.8826071904062,0.520860744120384,1.07251108028126));
#17179=CARTESIAN_POINT('Ctrl Pts',(2.88179136985247,0.128344716275584,0.921721359700738));
#17180=CARTESIAN_POINT('Ctrl Pts',(2.88137748969615,0.260125811446042,0.969562560736564));
#17181=CARTESIAN_POINT('Ctrl Pts',(2.88096557603236,0.391911191572128,1.01736709873619));
#17182=CARTESIAN_POINT('Ctrl Pts',(2.88054812086471,0.523720986413769,1.06506475118311));
#17183=CARTESIAN_POINT('Ctrl Pts',(2.87989567979058,0.132478313274208,0.910796512238404));
#17184=CARTESIAN_POINT('Ctrl Pts',(2.8798498458325,0.263928703639433,0.959537410055039));
#17185=CARTESIAN_POINT('Ctrl Pts',(2.87979494426834,0.39536106646766,1.00831406088685));
#17186=CARTESIAN_POINT('Ctrl Pts',(2.87973121518385,0.526696991648902,1.05732078078704));
#17187=CARTESIAN_POINT('Ctrl Pts',(2.88054197312457,0.13656563129969,0.899999067707368));
#17188=CARTESIAN_POINT('Ctrl Pts',(2.88044225836535,0.267692194169797,0.949620667653677));
#17189=CARTESIAN_POINT('Ctrl Pts',(2.88033592193784,0.398778873437746,0.999349242698191));
#17190=CARTESIAN_POINT('Ctrl Pts',(2.88019490601393,0.529648748841403,1.04964349671765));
#17191=CARTESIAN_POINT('',(2.88260719040209,0.52086074410776,1.07251108032045));
#17192=CARTESIAN_POINT('Ctrl Pts',(2.88605571002765,0.124542801858885,0.931774693457124));
#17193=CARTESIAN_POINT('Ctrl Pts',(2.884913033265,0.256571289306366,0.978937915267128));
#17194=CARTESIAN_POINT('Ctrl Pts',(2.88378009844813,0.388637588822166,1.02596265318668));
#17195=CARTESIAN_POINT('Ctrl Pts',(2.8826071904062,0.520860744120384,1.07251108028126));
#17196=CARTESIAN_POINT('',(2.88071362092342,0.524122953967611,1.06319194136119));
#17197=CARTESIAN_POINT('Origin',(2.95737828760701,0.541322246857939,1.05905796302752));
#17198=CARTESIAN_POINT('Ctrl Pts',(2.88071362118334,0.524122952384465,1.06319194074971));
#17199=CARTESIAN_POINT('Ctrl Pts',(2.88040468271156,0.524951973935425,1.06091422275821));
#17200=CARTESIAN_POINT('Ctrl Pts',(2.88020636536677,0.525785827271151,1.05862322954717));
#17201=CARTESIAN_POINT('Ctrl Pts',(2.88003298245609,0.527456219186867,1.0540338654771));
#17202=CARTESIAN_POINT('Ctrl Pts',(2.88005791438801,0.528292751084348,1.05173551297811));
#17203=CARTESIAN_POINT('Ctrl Pts',(2.88019546787499,0.529127141988623,1.04944304280962));
#17204=CARTESIAN_POINT('Ctrl Pts',(2.88602210209193,0.123730872767436,0.931375362419385));
#17205=CARTESIAN_POINT('Ctrl Pts',(2.88489031580204,0.256137405346913,0.978701308463558));
#17206=CARTESIAN_POINT('Ctrl Pts',(2.88377139476759,0.388593451583146,1.0259100078282));
#17207=CARTESIAN_POINT('Ctrl Pts',(2.8826044419187,0.521173013031435,1.07262110155611));
#17208=CARTESIAN_POINT('Ctrl Pts',(2.89021809451686,0.120434537356878,0.941383776987583));
#17209=CARTESIAN_POINT('Ctrl Pts',(2.88835152335579,0.253090597695893,0.9880121068955));
#17210=CARTESIAN_POINT('Ctrl Pts',(2.88651642325475,0.385832990043375,1.03444765358277));
#17211=CARTESIAN_POINT('Ctrl Pts',(2.8846060092736,0.518831485782303,1.08003438801855));
#17212=CARTESIAN_POINT('Ctrl Pts',(2.89213808672452,0.116817760728715,0.952233907678371));
#17213=CARTESIAN_POINT('Ctrl Pts',(2.88989822816684,0.249806253739155,0.997944196331249));
#17214=CARTESIAN_POINT('Ctrl Pts',(2.88769856407366,0.382904634727536,1.04342082167946));
#17215=CARTESIAN_POINT('Ctrl Pts',(2.88542850388851,0.516380034734364,1.08773011616922));
#17216=CARTESIAN_POINT('Ctrl Pts',(2.89161299367911,0.113199040068761,0.962970280062921));
#17217=CARTESIAN_POINT('Ctrl Pts',(2.88942220836743,0.246520922365427,1.00778095469082));
#17218=CARTESIAN_POINT('Ctrl Pts',(2.88725277180458,0.379975622201312,1.05231434239752));
#17219=CARTESIAN_POINT('Ctrl Pts',(2.885035153377,0.513928253868178,1.09536424252732));
#17220=CARTESIAN_POINT('',(2.88503519983007,0.513928543448632,1.09536334085845));
#17221=CARTESIAN_POINT('Ctrl Pts',(2.89160353474128,0.113778879042689,0.963163755874196));
#17222=CARTESIAN_POINT('Ctrl Pts',(2.88941597895361,0.246907970065613,1.00790881681038));
#17223=CARTESIAN_POINT('Ctrl Pts',(2.88724961188406,0.380170018768777,1.0523756565061));
#17224=CARTESIAN_POINT('Ctrl Pts',(2.88503519983007,0.513928543448632,1.09536334085845));
#17225=CARTESIAN_POINT('Ctrl Pts',(2.88503519983007,0.513928543448631,1.09536334085845));
#17226=CARTESIAN_POINT('Ctrl Pts',(2.88532122676486,0.515433447174265,1.08981078998296));
#17227=CARTESIAN_POINT('Ctrl Pts',(2.88498244688731,0.517061672225632,1.0842825322267));
#17228=CARTESIAN_POINT('Ctrl Pts',(2.88402831182171,0.518781812731824,1.07886904595466));
#17229=CARTESIAN_POINT('Ctrl Pts',(2.88365018585186,0.519463508458812,1.07672366861689));
#17230=CARTESIAN_POINT('Ctrl Pts',(2.88317616630465,0.520157484227229,1.07460257154214));
#17231=CARTESIAN_POINT('Ctrl Pts',(2.88260719039372,0.520860744100385,1.07251108040514));
#17232=CARTESIAN_POINT('Ctrl Pts',(4.,-0.208000000000001,1.2));
#17233=CARTESIAN_POINT('Ctrl Pts',(4.,0.670547542022765,1.2));
#17234=CARTESIAN_POINT('Ctrl Pts',(3.99999413894399,-0.208000000000001,
1.19980766336825));
#17235=CARTESIAN_POINT('Ctrl Pts',(3.99999413894399,0.670547542022765,1.19980766336825));
#17236=CARTESIAN_POINT('Ctrl Pts',(3.99855414331412,-0.208000000000001,
1.15256872586735));
#17237=CARTESIAN_POINT('Ctrl Pts',(3.99855414331412,0.670547542022765,1.15256872586735));
#17238=CARTESIAN_POINT('Ctrl Pts',(3.99545186687381,-0.208000000000001,
1.05866205464794));
#17239=CARTESIAN_POINT('Ctrl Pts',(3.99545186687381,0.670547542022765,1.05866205464794));
#17240=CARTESIAN_POINT('Ctrl Pts',(3.98977740850449,-0.208000000000001,
0.919671129654847));
#17241=CARTESIAN_POINT('Ctrl Pts',(3.98977740850449,0.670547542022765,0.919671129654847));
#17242=CARTESIAN_POINT('Ctrl Pts',(3.97841403016118,-0.208000000000001,
0.741129277895168));
#17243=CARTESIAN_POINT('Ctrl Pts',(3.97841403016118,0.670547542022765,0.741129277895168));
#17244=CARTESIAN_POINT('Ctrl Pts',(3.95259200169988,-0.208000000000001,
0.538436816836329));
#17245=CARTESIAN_POINT('Ctrl Pts',(3.95259200169988,0.670547542022765,0.538436816836329));
#17246=CARTESIAN_POINT('Ctrl Pts',(3.90986572419832,-0.208000000000001,
0.364350357241537));
#17247=CARTESIAN_POINT('Ctrl Pts',(3.90986572419832,0.670547542022765,0.364350357241537));
#17248=CARTESIAN_POINT('Ctrl Pts',(3.84598208672298,-0.208000000000001,
0.224659532804428));
#17249=CARTESIAN_POINT('Ctrl Pts',(3.84598208672298,0.670547542022765,0.224659532804428));
#17250=CARTESIAN_POINT('Ctrl Pts',(3.75872318140661,-0.208000000000001,
0.120497232333236));
#17251=CARTESIAN_POINT('Ctrl Pts',(3.75872318140661,0.670547542022765,0.120497232333236));
#17252=CARTESIAN_POINT('Ctrl Pts',(3.64881642260075,-0.208000000000001,
0.0470540298718229));
#17253=CARTESIAN_POINT('Ctrl Pts',(3.64881642260075,0.670547542022765,0.0470540298718229));
#17254=CARTESIAN_POINT('Ctrl Pts',(3.52045328348988,-0.208000000000001,
-0.00118366394786523));
#17255=CARTESIAN_POINT('Ctrl Pts',(3.52045328348988,0.670547542022765,-0.00118366394786523));
#17256=CARTESIAN_POINT('Ctrl Pts',(3.3816469894381,-0.208000000000001,-0.0263068037111615));
#17257=CARTESIAN_POINT('Ctrl Pts',(3.3816469894381,0.670547542022765,-0.0263068037111615));
#17258=CARTESIAN_POINT('Ctrl Pts',(3.2451100102617,-0.208000000000001,-0.0214179570895094));
#17259=CARTESIAN_POINT('Ctrl Pts',(3.2451100102617,0.670547542022765,-0.0214179570895094));
#17260=CARTESIAN_POINT('Ctrl Pts',(3.12452733970665,-0.208000000000001,
0.0241851999814078));
#17261=CARTESIAN_POINT('Ctrl Pts',(3.12452733970665,0.670547542022765,0.0241851999814078));
#17262=CARTESIAN_POINT('Ctrl Pts',(3.03063129752059,-0.208000000000001,
0.119017371327004));
#17263=CARTESIAN_POINT('Ctrl Pts',(3.03063129752059,0.670547542022765,0.119017371327004));
#17264=CARTESIAN_POINT('Ctrl Pts',(2.96639254265844,-0.208000000000001,
0.262319630540593));
#17265=CARTESIAN_POINT('Ctrl Pts',(2.96639254265844,0.670547542022765,0.262319630540593));
#17266=CARTESIAN_POINT('Ctrl Pts',(2.92780415844446,-0.208000000000001,
0.444963858672424));
#17267=CARTESIAN_POINT('Ctrl Pts',(2.92780415844446,0.670547542022765,0.444963858672424));
#17268=CARTESIAN_POINT('Ctrl Pts',(2.90717911786689,-0.208000000000001,
0.65402023086958));
#17269=CARTESIAN_POINT('Ctrl Pts',(2.90717911786689,0.670547542022765,0.65402023086958));
#17270=CARTESIAN_POINT('Ctrl Pts',(2.89547076625581,-0.208000000000001,
0.875890304828918));
#17271=CARTESIAN_POINT('Ctrl Pts',(2.89547076625581,0.670547542022765,0.875890304828918));
#17272=CARTESIAN_POINT('Ctrl Pts',(2.88537704766906,-0.208000000000001,
1.10060381648398));
#17273=CARTESIAN_POINT('Ctrl Pts',(2.88537704766906,0.670547542022765,1.10060381648398));
#17274=CARTESIAN_POINT('Ctrl Pts',(2.8728456296504,-0.208000000000001,1.32371934078733));
#17275=CARTESIAN_POINT('Ctrl Pts',(2.8728456296504,0.670547542022765,1.32371934078733));
#17276=CARTESIAN_POINT('Ctrl Pts',(2.85578261679345,-0.208000000000001,
1.54401727992264));
#17277=CARTESIAN_POINT('Ctrl Pts',(2.85578261679345,0.670547542022765,1.54401727992264));
#17278=CARTESIAN_POINT('Ctrl Pts',(2.83335686249019,-0.208000000000001,
1.76209503442146));
#17279=CARTESIAN_POINT('Ctrl Pts',(2.83335686249019,0.670547542022765,1.76209503442146));
#17280=CARTESIAN_POINT('Ctrl Pts',(2.80505146480345,-0.208000000000001,
1.97856787413951));
#17281=CARTESIAN_POINT('Ctrl Pts',(2.80505146480345,0.670547542022765,1.97856787413951));
#17282=CARTESIAN_POINT('Ctrl Pts',(2.76985908233915,-0.208000000000001,
2.19251877196071));
#17283=CARTESIAN_POINT('Ctrl Pts',(2.76985908233915,0.670547542022765,2.19251877196071));
#17284=CARTESIAN_POINT('Ctrl Pts',(2.72531955636536,-0.208000000000001,
2.39962532458029));
#17285=CARTESIAN_POINT('Ctrl Pts',(2.72531955636536,0.670547542022765,2.39962532458029));
#17286=CARTESIAN_POINT('Ctrl Pts',(2.66797634363184,-0.208000000000001,
2.59347738935741));
#17287=CARTESIAN_POINT('Ctrl Pts',(2.66797634363184,0.670547542022765,2.59347738935741));
#17288=CARTESIAN_POINT('Ctrl Pts',(2.59397540849171,-0.208000000000001,
2.7672283971178));
#17289=CARTESIAN_POINT('Ctrl Pts',(2.59397540849171,0.670547542022765,2.7672283971178));
#17290=CARTESIAN_POINT('Ctrl Pts',(2.49960870420485,-0.208000000000001,
2.91510580081997));
#17291=CARTESIAN_POINT('Ctrl Pts',(2.49960870420485,0.670547542022765,2.91510580081997));
#17292=CARTESIAN_POINT('Ctrl Pts',(2.38189256086504,-0.208000000000001,
3.03403241435618));
#17293=CARTESIAN_POINT('Ctrl Pts',(2.38189256086504,0.670547542022765,3.03403241435618));
#17294=CARTESIAN_POINT('Ctrl Pts',(2.23909845280558,-0.208000000000001,
3.12505646843308));
#17295=CARTESIAN_POINT('Ctrl Pts',(2.23909845280558,0.670547542022765,3.12505646843308));
#17296=CARTESIAN_POINT('Ctrl Pts',(2.07061055216582,-0.208000000000001,
3.19196918412265));
#17297=CARTESIAN_POINT('Ctrl Pts',(2.07061055216582,0.670547542022765,3.19196918412265));
#17298=CARTESIAN_POINT('Ctrl Pts',(1.87681490437036,-0.208000000000001,
3.24001322621211));
#17299=CARTESIAN_POINT('Ctrl Pts',(1.87681490437036,0.670547542022765,3.24001322621211));
#17300=CARTESIAN_POINT('Ctrl Pts',(1.65897747541321,-0.208000000000001,
3.27464765209773));
#17301=CARTESIAN_POINT('Ctrl Pts',(1.65897747541321,0.670547542022765,3.27464765209773));
#17302=CARTESIAN_POINT('Ctrl Pts',(1.4191255439272,-0.208000000000001,3.30006519349576));
#17303=CARTESIAN_POINT('Ctrl Pts',(1.4191255439272,0.670547542022765,3.30006519349576));
#17304=CARTESIAN_POINT('Ctrl Pts',(1.15993538533448,-0.208000000000001,
3.31897283641381));
#17305=CARTESIAN_POINT('Ctrl Pts',(1.15993538533448,0.670547542022765,3.31897283641381));
#17306=CARTESIAN_POINT('Ctrl Pts',(0.884625090385968,-0.208000000000001,
3.33300441174764));
#17307=CARTESIAN_POINT('Ctrl Pts',(0.884625090385968,0.670547542022765,
3.33300441174764));
#17308=CARTESIAN_POINT('Ctrl Pts',(0.596845720618978,-0.208000000000001,
3.34293392264922));
#17309=CARTESIAN_POINT('Ctrl Pts',(0.596845720618978,0.670547542022765,
3.34293392264922));
#17310=CARTESIAN_POINT('Ctrl Pts',(0.30057321210183,-0.208000000000001,
3.34897162637417));
#17311=CARTESIAN_POINT('Ctrl Pts',(0.30057321210183,0.670547542022765,3.34897162637417));
#17312=CARTESIAN_POINT('Ctrl Pts',(1.66741620510891E-14,-0.208000000000001,
3.35102435732185));
#17313=CARTESIAN_POINT('Ctrl Pts',(1.66741620510891E-14,0.670547542022765,
3.35102435732185));
#17314=CARTESIAN_POINT('Ctrl Pts',(-0.300573212101791,-0.208000000000001,
3.34897162637426));
#17315=CARTESIAN_POINT('Ctrl Pts',(-0.300573212101791,0.670547542022765,
3.34897162637426));
#17316=CARTESIAN_POINT('Ctrl Pts',(-0.596845720618908,-0.208000000000001,
3.34293392264938));
#17317=CARTESIAN_POINT('Ctrl Pts',(-0.596845720618908,0.670547542022765,
3.34293392264938));
#17318=CARTESIAN_POINT('Ctrl Pts',(-0.884625090385886,-0.208000000000001,
3.33300441174785));
#17319=CARTESIAN_POINT('Ctrl Pts',(-0.884625090385886,0.670547542022765,
3.33300441174785));
#17320=CARTESIAN_POINT('Ctrl Pts',(-1.15993538533442,-0.208000000000001,
3.31897283641402));
#17321=CARTESIAN_POINT('Ctrl Pts',(-1.15993538533442,0.670547542022765,
3.31897283641402));
#17322=CARTESIAN_POINT('Ctrl Pts',(-1.41912554392716,-0.208000000000001,
3.30006519349591));
#17323=CARTESIAN_POINT('Ctrl Pts',(-1.41912554392716,0.670547542022765,
3.30006519349591));
#17324=CARTESIAN_POINT('Ctrl Pts',(-1.65897747541319,-0.208000000000001,
3.27464765209779));
#17325=CARTESIAN_POINT('Ctrl Pts',(-1.65897747541319,0.670547542022765,
3.27464765209779));
#17326=CARTESIAN_POINT('Ctrl Pts',(-1.87681490437034,-0.208000000000001,
3.24001322621208));
#17327=CARTESIAN_POINT('Ctrl Pts',(-1.87681490437034,0.670547542022765,
3.24001322621208));
#17328=CARTESIAN_POINT('Ctrl Pts',(-2.07061055216576,-0.208000000000001,
3.19196918412254));
#17329=CARTESIAN_POINT('Ctrl Pts',(-2.07061055216576,0.670547542022765,
3.19196918412254));
#17330=CARTESIAN_POINT('Ctrl Pts',(-2.23909845280547,-0.208000000000001,
3.12505646843295));
#17331=CARTESIAN_POINT('Ctrl Pts',(-2.23909845280547,0.670547542022765,
3.12505646843295));
#17332=CARTESIAN_POINT('Ctrl Pts',(-2.38189256086493,-0.208000000000001,
3.03403241435609));
#17333=CARTESIAN_POINT('Ctrl Pts',(-2.38189256086493,0.670547542022765,
3.03403241435609));
#17334=CARTESIAN_POINT('Ctrl Pts',(-2.49960870420481,-0.208000000000001,
2.91510580081997));
#17335=CARTESIAN_POINT('Ctrl Pts',(-2.49960870420481,0.670547542022765,
2.91510580081997));
#17336=CARTESIAN_POINT('Ctrl Pts',(-2.59397540849182,-0.208000000000001,
2.76722839711793));
#17337=CARTESIAN_POINT('Ctrl Pts',(-2.59397540849182,0.670547542022765,
2.76722839711793));
#17338=CARTESIAN_POINT('Ctrl Pts',(-2.66797634363209,-0.208000000000001,
2.59347738935767));
#17339=CARTESIAN_POINT('Ctrl Pts',(-2.66797634363209,0.670547542022765,
2.59347738935767));
#17340=CARTESIAN_POINT('Ctrl Pts',(-2.72531955636566,-0.208000000000001,
2.39962532458057));
#17341=CARTESIAN_POINT('Ctrl Pts',(-2.72531955636566,0.670547542022765,
2.39962532458057));
#17342=CARTESIAN_POINT('Ctrl Pts',(-2.76985908233936,-0.208000000000001,
2.19251877196088));
#17343=CARTESIAN_POINT('Ctrl Pts',(-2.76985908233936,0.670547542022765,
2.19251877196088));
#17344=CARTESIAN_POINT('Ctrl Pts',(-2.80505146480344,-0.208000000000001,
1.97856787413951));
#17345=CARTESIAN_POINT('Ctrl Pts',(-2.80505146480344,0.670547542022765,
1.97856787413951));
#17346=CARTESIAN_POINT('Ctrl Pts',(-2.8333568624899,-0.208000000000001,
1.76209503442131));
#17347=CARTESIAN_POINT('Ctrl Pts',(-2.8333568624899,0.670547542022765,1.76209503442131));
#17348=CARTESIAN_POINT('Ctrl Pts',(-2.85578261679294,-0.208000000000001,
1.54401727992238));
#17349=CARTESIAN_POINT('Ctrl Pts',(-2.85578261679294,0.670547542022765,
1.54401727992238));
#17350=CARTESIAN_POINT('Ctrl Pts',(-2.87284562964987,-0.208000000000001,
1.32371934078708));
#17351=CARTESIAN_POINT('Ctrl Pts',(-2.87284562964987,0.670547542022765,
1.32371934078708));
#17352=CARTESIAN_POINT('Ctrl Pts',(-2.88537704766869,-0.208000000000001,
1.10060381648384));
#17353=CARTESIAN_POINT('Ctrl Pts',(-2.88537704766869,0.670547542022765,
1.10060381648384));
#17354=CARTESIAN_POINT('Ctrl Pts',(-2.89547076625573,-0.208000000000001,
0.875890304828914));
#17355=CARTESIAN_POINT('Ctrl Pts',(-2.89547076625573,0.670547542022765,
0.875890304828914));
#17356=CARTESIAN_POINT('Ctrl Pts',(-2.90717911786707,-0.208000000000001,
0.654020230869684));
#17357=CARTESIAN_POINT('Ctrl Pts',(-2.90717911786707,0.670547542022765,
0.654020230869684));
#17358=CARTESIAN_POINT('Ctrl Pts',(-2.92780415844476,-0.208000000000001,
0.444963858672577));
#17359=CARTESIAN_POINT('Ctrl Pts',(-2.92780415844476,0.670547542022765,
0.444963858672577));
#17360=CARTESIAN_POINT('Ctrl Pts',(-2.96639254265869,-0.208000000000001,
0.262319630540737));
#17361=CARTESIAN_POINT('Ctrl Pts',(-2.96639254265869,0.670547542022765,
0.262319630540737));
#17362=CARTESIAN_POINT('Ctrl Pts',(-3.03063129752067,-0.208000000000001,
0.11901737132707));
#17363=CARTESIAN_POINT('Ctrl Pts',(-3.03063129752067,0.670547542022765,
0.11901737132707));
#17364=CARTESIAN_POINT('Ctrl Pts',(-3.12452733970658,-0.208000000000001,
0.0241851999813871));
#17365=CARTESIAN_POINT('Ctrl Pts',(-3.12452733970658,0.670547542022765,
0.0241851999813871));
#17366=CARTESIAN_POINT('Ctrl Pts',(-3.24511001026157,-0.208000000000001,
-0.0214179570895714));
#17367=CARTESIAN_POINT('Ctrl Pts',(-3.24511001026157,0.670547542022765,
-0.0214179570895714));
#17368=CARTESIAN_POINT('Ctrl Pts',(-3.38164698943802,-0.208000000000001,
-0.0263068037112043));
#17369=CARTESIAN_POINT('Ctrl Pts',(-3.38164698943802,0.670547542022765,
-0.0263068037112043));
#17370=CARTESIAN_POINT('Ctrl Pts',(-3.52045328348989,-0.208000000000001,
-0.00118366394785932));
#17371=CARTESIAN_POINT('Ctrl Pts',(-3.52045328348989,0.670547542022765,
-0.00118366394785932));
#17372=CARTESIAN_POINT('Ctrl Pts',(-3.64881642260079,-0.208000000000001,
0.0470540298718583));
#17373=CARTESIAN_POINT('Ctrl Pts',(-3.64881642260079,0.670547542022765,
0.0470540298718583));
#17374=CARTESIAN_POINT('Ctrl Pts',(-3.75872318140663,-0.208000000000001,
0.120497232333251));
#17375=CARTESIAN_POINT('Ctrl Pts',(-3.75872318140663,0.670547542022765,
0.120497232333251));
#17376=CARTESIAN_POINT('Ctrl Pts',(-3.84598208672296,-0.208000000000001,
0.224659532804408));
#17377=CARTESIAN_POINT('Ctrl Pts',(-3.84598208672296,0.670547542022765,
0.224659532804408));
#17378=CARTESIAN_POINT('Ctrl Pts',(-3.9098657241983,-0.208000000000001,
0.364350357241515));
#17379=CARTESIAN_POINT('Ctrl Pts',(-3.9098657241983,0.670547542022765,0.364350357241515));
#17380=CARTESIAN_POINT('Ctrl Pts',(-3.9525920016999,-0.208000000000001,
0.538436816836325));
#17381=CARTESIAN_POINT('Ctrl Pts',(-3.9525920016999,0.670547542022765,0.538436816836325));
#17382=CARTESIAN_POINT('Ctrl Pts',(-3.97841403016126,-0.208000000000001,
0.741129277895169));
#17383=CARTESIAN_POINT('Ctrl Pts',(-3.97841403016126,0.670547542022765,
0.741129277895169));
#17384=CARTESIAN_POINT('Ctrl Pts',(-3.99260375067011,-0.208000000000001,
0.964078729991154));
#17385=CARTESIAN_POINT('Ctrl Pts',(-3.99260375067011,0.670547542022765,
0.964078729991154));
#17386=CARTESIAN_POINT('Ctrl Pts',(-4.00047520099045,-0.208000000000001,
1.1981954227983));
#17387=CARTESIAN_POINT('Ctrl Pts',(-4.00047520099045,0.670547542022765,
1.1981954227983));
#17388=CARTESIAN_POINT('Ctrl Pts',(-4.00639322616607,-0.208000000000001,
1.43558101932923));
#17389=CARTESIAN_POINT('Ctrl Pts',(-4.00639322616607,0.670547542022765,
1.43558101932923));
#17390=CARTESIAN_POINT('Ctrl Pts',(-4.01278239926574,-0.208000000000001,
1.67142113207667));
#17391=CARTESIAN_POINT('Ctrl Pts',(-4.01278239926574,0.670547542022765,
1.67142113207667));
#17392=CARTESIAN_POINT('Ctrl Pts',(-4.02066709528487,-0.208000000000001,
1.90332556813333));
#17393=CARTESIAN_POINT('Ctrl Pts',(-4.02066709528487,0.670547542022765,
1.90332556813333));
#17394=CARTESIAN_POINT('Ctrl Pts',(-4.0302101444685,-0.208000000000001,
2.130657485557));
#17395=CARTESIAN_POINT('Ctrl Pts',(-4.0302101444685,0.670547542022765,2.130657485557));
#17396=CARTESIAN_POINT('Ctrl Pts',(-4.04126813644779,-0.208000000000001,
2.35385258470204));
#17397=CARTESIAN_POINT('Ctrl Pts',(-4.04126813644779,0.670547542022765,
2.35385258470204));
#17398=CARTESIAN_POINT('Ctrl Pts',(-4.05390260344525,-0.208000000000001,
2.57377631141659));
#17399=CARTESIAN_POINT('Ctrl Pts',(-4.05390260344525,0.670547542022765,
2.57377631141659));
#17400=CARTESIAN_POINT('Ctrl Pts',(-4.06899962712502,-0.208000000000001,
2.7909834104825));
#17401=CARTESIAN_POINT('Ctrl Pts',(-4.06899962712502,0.670547542022765,
2.7909834104825));
#17402=CARTESIAN_POINT('Ctrl Pts',(-4.08854433447739,-0.208000000000001,
3.00529120729338));
#17403=CARTESIAN_POINT('Ctrl Pts',(-4.08854433447739,0.670547542022765,
3.00529120729338));
#17404=CARTESIAN_POINT('Ctrl Pts',(-4.11518318246524,-0.208000000000001,
3.21600287470921));
#17405=CARTESIAN_POINT('Ctrl Pts',(-4.11518318246524,0.670547542022765,
3.21600287470921));
#17406=CARTESIAN_POINT('Ctrl Pts',(-4.15193466045748,-0.208000000000001,
3.42199345348447));
#17407=CARTESIAN_POINT('Ctrl Pts',(-4.15193466045748,0.670547542022765,
3.42199345348447));
#17408=CARTESIAN_POINT('Ctrl Pts',(-4.20184334854115,-0.208000000000001,
3.62185203209171));
#17409=CARTESIAN_POINT('Ctrl Pts',(-4.20184334854115,0.670547542022765,
3.62185203209171));
#17410=CARTESIAN_POINT('Ctrl Pts',(-4.26765207024395,-0.208000000000001,
3.81399668859083));
#17411=CARTESIAN_POINT('Ctrl Pts',(-4.26765207024395,0.670547542022765,
3.81399668859083));
#17412=CARTESIAN_POINT('Ctrl Pts',(-4.35148411330718,-0.208000000000001,
3.99681013615577));
#17413=CARTESIAN_POINT('Ctrl Pts',(-4.35148411330718,0.670547542022765,
3.99681013615577));
#17414=CARTESIAN_POINT('Ctrl Pts',(-4.45474519640294,-0.208000000000001,
4.16885849319142));
#17415=CARTESIAN_POINT('Ctrl Pts',(-4.45474519640294,0.670547542022765,
4.16885849319142));
#17416=CARTESIAN_POINT('Ctrl Pts',(-4.57800047823775,-0.208000000000001,
4.32911151507774));
#17417=CARTESIAN_POINT('Ctrl Pts',(-4.57800047823775,0.670547542022765,
4.32911151507774));
#17418=CARTESIAN_POINT('Ctrl Pts',(-4.7208720035032,-0.208000000000001,
4.47714872481861));
#17419=CARTESIAN_POINT('Ctrl Pts',(-4.7208720035032,0.670547542022765,4.47714872481861));
#17420=CARTESIAN_POINT('Ctrl Pts',(-4.88190185104852,-0.208000000000001,
4.61340315498244));
#17421=CARTESIAN_POINT('Ctrl Pts',(-4.88190185104852,0.670547542022765,
4.61340315498244));
#17422=CARTESIAN_POINT('Ctrl Pts',(-5.05850630701885,-0.208000000000001,
4.73929437247796));
#17423=CARTESIAN_POINT('Ctrl Pts',(-5.05850630701885,0.670547542022765,
4.73929437247796));
#17424=CARTESIAN_POINT('Ctrl Pts',(-5.24741086000019,-0.208000000000001,
4.8567611153285));
#17425=CARTESIAN_POINT('Ctrl Pts',(-5.24741086000019,0.670547542022765,
4.8567611153285));
#17426=CARTESIAN_POINT('Ctrl Pts',(-5.44501860313342,-0.208000000000001,
4.96787993373728));
#17427=CARTESIAN_POINT('Ctrl Pts',(-5.44501860313342,0.670547542022765,
4.96787993373728));
#17428=CARTESIAN_POINT('Ctrl Pts',(-5.64781737380319,-0.208000000000001,
5.07442896098937));
#17429=CARTESIAN_POINT('Ctrl Pts',(-5.64781737380319,0.670547542022765,
5.07442896098937));
#17430=CARTESIAN_POINT('Ctrl Pts',(-5.85274048349242,-0.208000000000001,
5.17752467829109));
#17431=CARTESIAN_POINT('Ctrl Pts',(-5.85274048349242,0.670547542022765,
5.17752467829109));
#17432=CARTESIAN_POINT('Ctrl Pts',(-6.05762450882858,-0.208000000000001,
5.27709955371564));
#17433=CARTESIAN_POINT('Ctrl Pts',(-6.05762450882858,0.670547542022765,
5.27709955371564));
#17434=CARTESIAN_POINT('Ctrl Pts',(-6.26112587698772,-0.208000000000001,
5.37226655127787));
#17435=CARTESIAN_POINT('Ctrl Pts',(-6.26112587698772,0.670547542022765,
5.37226655127787));
#17436=CARTESIAN_POINT('Ctrl Pts',(-6.46246210121964,-0.208000000000001,
5.46195513100446));
#17437=CARTESIAN_POINT('Ctrl Pts',(-6.46246210121964,0.670547542022765,
5.46195513100446));
#17438=CARTESIAN_POINT('Ctrl Pts',(-6.66121503090592,-0.208000000000001,
5.54547963906637));
#17439=CARTESIAN_POINT('Ctrl Pts',(-6.66121503090592,0.670547542022765,
5.54547963906637));
#17440=CARTESIAN_POINT('Ctrl Pts',(-6.8570997603751,-0.208000000000001,
5.62308582598972));
#17441=CARTESIAN_POINT('Ctrl Pts',(-6.8570997603751,0.670547542022765,5.62308582598972));
#17442=CARTESIAN_POINT('Ctrl Pts',(-7.04976847947249,-0.208000000000001,
5.69662713609756));
#17443=CARTESIAN_POINT('Ctrl Pts',(-7.04976847947249,0.670547542022765,
5.69662713609756));
#17444=CARTESIAN_POINT('Ctrl Pts',(-7.23853768475,-0.208000000000001,5.76979878895672));
#17445=CARTESIAN_POINT('Ctrl Pts',(-7.23853768475,0.670547542022765,5.76979878895672));
#17446=CARTESIAN_POINT('Ctrl Pts',(-7.42198551710617,-0.208000000000001,
5.84723737025949));
#17447=CARTESIAN_POINT('Ctrl Pts',(-7.42198551710617,0.670547542022765,
5.84723737025949));
#17448=CARTESIAN_POINT('Ctrl Pts',(-7.59751903688412,-0.208000000000001,
5.93381436957244));
#17449=CARTESIAN_POINT('Ctrl Pts',(-7.59751903688412,0.670547542022765,
5.93381436957244));
#17450=CARTESIAN_POINT('Ctrl Pts',(-7.76106756457753,-0.208000000000001,
6.03389995867283));
#17451=CARTESIAN_POINT('Ctrl Pts',(-7.76106756457753,0.670547542022765,
6.03389995867283));
#17452=CARTESIAN_POINT('Ctrl Pts',(-7.90644860448901,-0.208000000000001,
6.15052660592937));
#17453=CARTESIAN_POINT('Ctrl Pts',(-7.90644860448901,0.670547542022765,
6.15052660592937));
#17454=CARTESIAN_POINT('Ctrl Pts',(-8.02580908828117,-0.208000000000001,
6.28498018271686));
#17455=CARTESIAN_POINT('Ctrl Pts',(-8.02580908828117,0.670547542022765,
6.28498018271686));
#17456=CARTESIAN_POINT('Ctrl Pts',(-8.11207116917861,-0.208000000000001,
6.43720976255636));
#17457=CARTESIAN_POINT('Ctrl Pts',(-8.11207116917861,0.670547542022765,
6.43720976255636));
#17458=CARTESIAN_POINT('Ctrl Pts',(-8.16089752265956,-0.208000000000001,
6.60605451948903));
#17459=CARTESIAN_POINT('Ctrl Pts',(-8.16089752265956,0.670547542022765,
6.60605451948903));
#17460=CARTESIAN_POINT('Ctrl Pts',(-8.17293082304181,-0.208000000000001,
6.78954489191904));
#17461=CARTESIAN_POINT('Ctrl Pts',(-8.17293082304181,0.670547542022765,
6.78954489191904));
#17462=CARTESIAN_POINT('Ctrl Pts',(-8.15569042861244,-0.208000000000001,
6.9851692342788));
#17463=CARTESIAN_POINT('Ctrl Pts',(-8.15569042861244,0.670547542022765,
6.9851692342788));
#17464=CARTESIAN_POINT('Ctrl Pts',(-8.12057943633387,-0.208000000000001,
7.19009032473164));
#17465=CARTESIAN_POINT('Ctrl Pts',(-8.12057943633387,0.670547542022765,
7.19009032473164));
#17466=CARTESIAN_POINT('Ctrl Pts',(-8.08008348678073,-0.208000000000001,
7.40136016279791));
#17467=CARTESIAN_POINT('Ctrl Pts',(-8.08008348678073,0.670547542022765,
7.40136016279791));
#17468=CARTESIAN_POINT('Ctrl Pts',(-8.04494633492831,-0.208000000000001,
7.61613341658677));
#17469=CARTESIAN_POINT('Ctrl Pts',(-8.04494633492831,0.670547542022765,
7.61613341658677));
#17470=CARTESIAN_POINT('Ctrl Pts',(-8.02124364536279,-0.208000000000001,
7.83188673232793));
#17471=CARTESIAN_POINT('Ctrl Pts',(-8.02124364536279,0.670547542022765,
7.83188673232793));
#17472=CARTESIAN_POINT('Ctrl Pts',(-8.007818938056,-0.208000000000001,8.04662057355248));
#17473=CARTESIAN_POINT('Ctrl Pts',(-8.007818938056,0.670547542022765,8.04662057355248));
#17474=CARTESIAN_POINT('Ctrl Pts',(-7.99879843919661,-0.208000000000001,
8.25883677791483));
#17475=CARTESIAN_POINT('Ctrl Pts',(-7.99879843919661,0.670547542022765,
8.25883677791483));
#17476=CARTESIAN_POINT('Ctrl Pts',(-7.98575825096101,-0.208000000000001,
8.46752658699528));
#17477=CARTESIAN_POINT('Ctrl Pts',(-7.98575825096101,0.670547542022765,
8.46752658699528));
#17478=CARTESIAN_POINT('Ctrl Pts',(-7.96007609558389,-0.208000000000001,
8.67216210283896));
#17479=CARTESIAN_POINT('Ctrl Pts',(-7.96007609558389,0.670547542022765,
8.67216210283896));
#17480=CARTESIAN_POINT('Ctrl Pts',(-7.91508259073019,-0.208000000000001,
8.87266947141823));
#17481=CARTESIAN_POINT('Ctrl Pts',(-7.91508259073019,0.670547542022765,
8.87266947141823));
#17482=CARTESIAN_POINT('Ctrl Pts',(-7.84862074946261,-0.208000000000001,
9.06945407016992));
#17483=CARTESIAN_POINT('Ctrl Pts',(-7.84862074946261,0.670547542022765,
9.06945407016992));
#17484=CARTESIAN_POINT('Ctrl Pts',(-7.76209282457479,-0.208000000000001,
9.26297089919765));
#17485=CARTESIAN_POINT('Ctrl Pts',(-7.76209282457479,0.670547542022765,
9.26297089919765));
#17486=CARTESIAN_POINT('Ctrl Pts',(-7.65900038660722,-0.208000000000001,
9.4532499945042));
#17487=CARTESIAN_POINT('Ctrl Pts',(-7.65900038660722,0.670547542022765,
9.4532499945042));
#17488=CARTESIAN_POINT('Ctrl Pts',(-7.5436057352653,-0.208000000000001,
9.63939026966035));
#17489=CARTESIAN_POINT('Ctrl Pts',(-7.5436057352653,0.670547542022765,9.63939026966035));
#17490=CARTESIAN_POINT('Ctrl Pts',(-7.41967047355001,-0.208000000000001,
9.81917361987397));
#17491=CARTESIAN_POINT('Ctrl Pts',(-7.41967047355001,0.670547542022765,
9.81917361987397));
#17492=CARTESIAN_POINT('Ctrl Pts',(-7.28883796912703,-0.208000000000001,
9.98835756998572));
#17493=CARTESIAN_POINT('Ctrl Pts',(-7.28883796912703,0.670547542022765,
9.98835756998572));
#17494=CARTESIAN_POINT('Ctrl Pts',(-7.15081550722306,-0.208000000000001,
10.1414720974148));
#17495=CARTESIAN_POINT('Ctrl Pts',(-7.15081550722306,0.670547542022765,
10.1414720974148));
#17496=CARTESIAN_POINT('Ctrl Pts',(-7.0044544864105,-0.208000000000001,
10.2733319413008));
#17497=CARTESIAN_POINT('Ctrl Pts',(-7.0044544864105,0.670547542022765,10.2733319413008));
#17498=CARTESIAN_POINT('Ctrl Pts',(-6.84859008776113,-0.208000000000001,
10.3804015453596));
#17499=CARTESIAN_POINT('Ctrl Pts',(-6.84859008776113,0.670547542022765,
10.3804015453596));
#17500=CARTESIAN_POINT('Ctrl Pts',(-6.68288828293938,-0.208000000000001,
10.4620502678778));
#17501=CARTESIAN_POINT('Ctrl Pts',(-6.68288828293938,0.670547542022765,
10.4620502678778));
#17502=CARTESIAN_POINT('Ctrl Pts',(-6.50892555577766,-0.208000000000001,
10.522290883026));
#17503=CARTESIAN_POINT('Ctrl Pts',(-6.50892555577766,0.670547542022765,
10.522290883026));
#17504=CARTESIAN_POINT('Ctrl Pts',(-6.32976796473811,-0.208000000000001,
10.5687216653902));
#17505=CARTESIAN_POINT('Ctrl Pts',(-6.32976796473811,0.670547542022765,
10.5687216653902));
#17506=CARTESIAN_POINT('Ctrl Pts',(-6.14893768388701,-0.208000000000001,
10.6103475969885));
#17507=CARTESIAN_POINT('Ctrl Pts',(-6.14893768388701,0.670547542022765,
10.6103475969885));
#17508=CARTESIAN_POINT('Ctrl Pts',(-5.96961932707142,-0.208000000000001,
10.6558377434043));
#17509=CARTESIAN_POINT('Ctrl Pts',(-5.96961932707142,0.670547542022765,
10.6558377434043));
#17510=CARTESIAN_POINT('Ctrl Pts',(-5.79367695415031,-0.208000000000001,
10.7114411549114));
#17511=CARTESIAN_POINT('Ctrl Pts',(-5.79367695415031,0.670547542022765,
10.7114411549114));
#17512=CARTESIAN_POINT('Ctrl Pts',(-5.62101499943431,-0.208000000000001,
10.7795199127535));
#17513=CARTESIAN_POINT('Ctrl Pts',(-5.62101499943431,0.670547542022765,
10.7795199127535));
#17514=CARTESIAN_POINT('Ctrl Pts',(-5.45051506148982,-0.208000000000001,
10.8599381259737));
#17515=CARTESIAN_POINT('Ctrl Pts',(-5.45051506148982,0.670547542022765,
10.8599381259737));
#17516=CARTESIAN_POINT('Ctrl Pts',(-5.28082876351929,-0.208000000000001,
10.9511663773826));
#17517=CARTESIAN_POINT('Ctrl Pts',(-5.28082876351929,0.670547542022765,
10.9511663773826));
#17518=CARTESIAN_POINT('Ctrl Pts',(-5.11112998264616,-0.208000000000001,
11.0513704191329));
#17519=CARTESIAN_POINT('Ctrl Pts',(-5.11112998264616,0.670547542022765,
11.0513704191329));
#17520=CARTESIAN_POINT('Ctrl Pts',(-4.94211773226973,-0.208000000000001,
11.1598106424589));
#17521=CARTESIAN_POINT('Ctrl Pts',(-4.94211773226973,0.670547542022765,
11.1598106424589));
#17522=CARTESIAN_POINT('Ctrl Pts',(-4.77596612414951,-0.208000000000001,
11.2768795166235));
#17523=CARTESIAN_POINT('Ctrl Pts',(-4.77596612414951,0.670547542022765,
11.2768795166235));
#17524=CARTESIAN_POINT('Ctrl Pts',(-4.61532593596946,-0.208000000000001,
11.4029224160731));
#17525=CARTESIAN_POINT('Ctrl Pts',(-4.61532593596946,0.670547542022765,
11.4029224160731));
#17526=CARTESIAN_POINT('Ctrl Pts',(-4.46255574628757,-0.208000000000001,
11.5373242211527));
#17527=CARTESIAN_POINT('Ctrl Pts',(-4.46255574628757,0.670547542022765,
11.5373242211527));
#17528=CARTESIAN_POINT('Ctrl Pts',(-4.31893584999241,-0.208000000000001,
11.6776492463597));
#17529=CARTESIAN_POINT('Ctrl Pts',(-4.31893584999241,0.670547542022765,
11.6776492463597));
#17530=CARTESIAN_POINT('Ctrl Pts',(-4.18369962429796,-0.208000000000001,
11.8183570873721));
#17531=CARTESIAN_POINT('Ctrl Pts',(-4.18369962429796,0.670547542022765,
11.8183570873721));
#17532=CARTESIAN_POINT('Ctrl Pts',(-4.05395481372655,-0.208000000000001,
11.9514202619522));
#17533=CARTESIAN_POINT('Ctrl Pts',(-4.05395481372655,0.670547542022765,
11.9514202619522));
#17534=CARTESIAN_POINT('Ctrl Pts',(-3.92533033057354,-0.208000000000001,
12.0684942936867));
#17535=CARTESIAN_POINT('Ctrl Pts',(-3.92533033057354,0.670547542022765,
12.0684942936867));
#17536=CARTESIAN_POINT('Ctrl Pts',(-3.79241297762166,-0.208000000000001,
12.1626050652586));
#17537=CARTESIAN_POINT('Ctrl Pts',(-3.79241297762166,0.670547542022765,
12.1626050652586));
#17538=CARTESIAN_POINT('Ctrl Pts',(-3.64927048315908,-0.208000000000001,
12.2301117722809));
#17539=CARTESIAN_POINT('Ctrl Pts',(-3.64927048315908,0.670547542022765,
12.2301117722809));
#17540=CARTESIAN_POINT('Ctrl Pts',(-3.48993681214334,-0.208000000000001,
12.2723364229645));
#17541=CARTESIAN_POINT('Ctrl Pts',(-3.48993681214334,0.670547542022765,
12.2723364229645));
#17542=CARTESIAN_POINT('Ctrl Pts',(-3.30884480305534,-0.208000000000001,
12.2938762651139));
#17543=CARTESIAN_POINT('Ctrl Pts',(-3.30884480305534,0.670547542022765,
12.2938762651139));
#17544=CARTESIAN_POINT('Ctrl Pts',(-3.10127560868576,-0.208000000000001,
12.3010487961981));
#17545=CARTESIAN_POINT('Ctrl Pts',(-3.10127560868576,0.670547542022765,
12.3010487961981));
#17546=CARTESIAN_POINT('Ctrl Pts',(-2.86376302967345,-0.208000000000001,
12.300400839059));
#17547=CARTESIAN_POINT('Ctrl Pts',(-2.86376302967345,0.670547542022765,
12.300400839059));
#17548=CARTESIAN_POINT('Ctrl Pts',(-2.59461297443094,-0.208000000000001,
12.2969132923574));
#17549=CARTESIAN_POINT('Ctrl Pts',(-2.59461297443094,0.670547542022765,
12.2969132923574));
#17550=CARTESIAN_POINT('Ctrl Pts',(-2.29394197380209,-0.208000000000001,
12.2935845551224));
#17551=CARTESIAN_POINT('Ctrl Pts',(-2.29394197380209,0.670547542022765,
12.2935845551224));
#17552=CARTESIAN_POINT('Ctrl Pts',(-1.96338745719135,-0.208000000000001,
12.2919684497906));
#17553=CARTESIAN_POINT('Ctrl Pts',(-1.96338745719135,0.670547542022765,
12.2919684497906));
#17554=CARTESIAN_POINT('Ctrl Pts',(-1.60591558979456,-0.208000000000001,
12.2924280531798));
#17555=CARTESIAN_POINT('Ctrl Pts',(-1.60591558979456,0.670547542022765,
12.2924280531798));
#17556=CARTESIAN_POINT('Ctrl Pts',(-1.22558901314075,-0.208000000000001,
12.2945066442122));
#17557=CARTESIAN_POINT('Ctrl Pts',(-1.22558901314075,0.670547542022765,
12.2945066442122));
#17558=CARTESIAN_POINT('Ctrl Pts',(-0.827351903312651,-0.208000000000001,
12.2972483292773));
#17559=CARTESIAN_POINT('Ctrl Pts',(-0.827351903312651,0.670547542022765,
12.2972483292773));
#17560=CARTESIAN_POINT('Ctrl Pts',(-0.498916532526571,-0.208000000000001,
12.299081889758));
#17561=CARTESIAN_POINT('Ctrl Pts',(-0.498916532526571,0.670547542022765,
12.299081889758));
#17562=CARTESIAN_POINT('Ctrl Pts',(-0.249771440080693,-0.208000000000001,
12.2998330708668));
#17563=CARTESIAN_POINT('Ctrl Pts',(-0.249771440080693,0.670547542022765,
12.2998330708668));
#17564=CARTESIAN_POINT('Ctrl Pts',(-0.0832571466935557,-0.208000000000001,
12.2999999999989));
#17565=CARTESIAN_POINT('Ctrl Pts',(-0.0832571466935557,0.670547542022765,
12.2999999999989));
#17566=CARTESIAN_POINT('Ctrl Pts',(0.,-0.208000000000001,12.3));
#17567=CARTESIAN_POINT('Ctrl Pts',(0.,0.670547542022765,12.3));
#17568=CARTESIAN_POINT('Ctrl Pts',(0.0832571466935396,-0.208000000000001,
12.3000000000011));
#17569=CARTESIAN_POINT('Ctrl Pts',(0.0832571466935396,0.670547542022765,
12.3000000000011));
#17570=CARTESIAN_POINT('Ctrl Pts',(0.24977144008061,-0.208000000000001,
12.2998330708736));
#17571=CARTESIAN_POINT('Ctrl Pts',(0.24977144008061,0.670547542022765,12.2998330708736));
#17572=CARTESIAN_POINT('Ctrl Pts',(0.498916532526534,-0.208000000000001,
12.2990818897713));
#17573=CARTESIAN_POINT('Ctrl Pts',(0.498916532526534,0.670547542022765,
12.2990818897713));
#17574=CARTESIAN_POINT('Ctrl Pts',(0.827351903312438,-0.208000000000001,
12.2972483292974));
#17575=CARTESIAN_POINT('Ctrl Pts',(0.827351903312438,0.670547542022765,
12.2972483292974));
#17576=CARTESIAN_POINT('Ctrl Pts',(1.22558901314046,-0.208000000000001,
12.2945066442369));
#17577=CARTESIAN_POINT('Ctrl Pts',(1.22558901314046,0.670547542022765,12.2945066442369));
#17578=CARTESIAN_POINT('Ctrl Pts',(1.60591558979418,-0.208000000000001,
12.2924280532047));
#17579=CARTESIAN_POINT('Ctrl Pts',(1.60591558979418,0.670547542022765,12.2924280532047));
#17580=CARTESIAN_POINT('Ctrl Pts',(1.96338745719096,-0.208000000000001,
12.291968449812));
#17581=CARTESIAN_POINT('Ctrl Pts',(1.96338745719096,0.670547542022765,12.291968449812));
#17582=CARTESIAN_POINT('Ctrl Pts',(2.29394197380175,-0.208000000000001,
12.2935845551378));
#17583=CARTESIAN_POINT('Ctrl Pts',(2.29394197380175,0.670547542022765,12.2935845551378));
#17584=CARTESIAN_POINT('Ctrl Pts',(2.59461297443069,-0.208000000000001,
12.2969132923658));
#17585=CARTESIAN_POINT('Ctrl Pts',(2.59461297443069,0.670547542022765,12.2969132923658));
#17586=CARTESIAN_POINT('Ctrl Pts',(2.86376302967335,-0.208000000000001,
12.3004008390612));
#17587=CARTESIAN_POINT('Ctrl Pts',(2.86376302967335,0.670547542022765,12.3004008390612));
#17588=CARTESIAN_POINT('Ctrl Pts',(3.10127560868576,-0.208000000000001,
12.3010487961961));
#17589=CARTESIAN_POINT('Ctrl Pts',(3.10127560868576,0.670547542022765,12.3010487961961));
#17590=CARTESIAN_POINT('Ctrl Pts',(3.30884480305537,-0.208000000000001,
12.2938762651102));
#17591=CARTESIAN_POINT('Ctrl Pts',(3.30884480305537,0.670547542022765,12.2938762651102));
#17592=CARTESIAN_POINT('Ctrl Pts',(3.48993681214337,-0.208000000000001,
12.2723364229612));
#17593=CARTESIAN_POINT('Ctrl Pts',(3.48993681214337,0.670547542022765,12.2723364229612));
#17594=CARTESIAN_POINT('Ctrl Pts',(3.64927048315907,-0.208000000000001,
12.2301117722792));
#17595=CARTESIAN_POINT('Ctrl Pts',(3.64927048315907,0.670547542022765,12.2301117722792));
#17596=CARTESIAN_POINT('Ctrl Pts',(3.79241297762162,-0.208000000000001,
12.1626050652587));
#17597=CARTESIAN_POINT('Ctrl Pts',(3.79241297762162,0.670547542022765,12.1626050652587));
#17598=CARTESIAN_POINT('Ctrl Pts',(3.92533033057351,-0.208000000000001,
12.0684942936878));
#17599=CARTESIAN_POINT('Ctrl Pts',(3.92533033057351,0.670547542022765,12.0684942936878));
#17600=CARTESIAN_POINT('Ctrl Pts',(4.05395481372655,-0.208000000000001,
11.9514202619535));
#17601=CARTESIAN_POINT('Ctrl Pts',(4.05395481372655,0.670547542022765,11.9514202619535));
#17602=CARTESIAN_POINT('Ctrl Pts',(4.18369962429796,-0.208000000000001,
11.8183570873731));
#17603=CARTESIAN_POINT('Ctrl Pts',(4.18369962429796,0.670547542022765,11.8183570873731));
#17604=CARTESIAN_POINT('Ctrl Pts',(4.3189358499924,-0.208000000000001,11.67764924636));
#17605=CARTESIAN_POINT('Ctrl Pts',(4.3189358499924,0.670547542022765,11.67764924636));
#17606=CARTESIAN_POINT('Ctrl Pts',(4.46255574628753,-0.208000000000001,
11.5373242211525));
#17607=CARTESIAN_POINT('Ctrl Pts',(4.46255574628753,0.670547542022765,11.5373242211525));
#17608=CARTESIAN_POINT('Ctrl Pts',(4.61532593596939,-0.208000000000001,
11.4029224160728));
#17609=CARTESIAN_POINT('Ctrl Pts',(4.61532593596939,0.670547542022765,11.4029224160728));
#17610=CARTESIAN_POINT('Ctrl Pts',(4.77596612414944,-0.208000000000001,
11.2768795166233));
#17611=CARTESIAN_POINT('Ctrl Pts',(4.77596612414944,0.670547542022765,11.2768795166233));
#17612=CARTESIAN_POINT('Ctrl Pts',(4.94211773226968,-0.208000000000001,
11.1598106424589));
#17613=CARTESIAN_POINT('Ctrl Pts',(4.94211773226968,0.670547542022765,11.1598106424589));
#17614=CARTESIAN_POINT('Ctrl Pts',(5.11112998264613,-0.208000000000001,
11.051370419133));
#17615=CARTESIAN_POINT('Ctrl Pts',(5.11112998264613,0.670547542022765,11.051370419133));
#17616=CARTESIAN_POINT('Ctrl Pts',(5.28082876351925,-0.208000000000001,
10.9511663773825));
#17617=CARTESIAN_POINT('Ctrl Pts',(5.28082876351925,0.670547542022765,10.9511663773825));
#17618=CARTESIAN_POINT('Ctrl Pts',(5.45051506148977,-0.208000000000001,
10.8599381259735));
#17619=CARTESIAN_POINT('Ctrl Pts',(5.45051506148977,0.670547542022765,10.8599381259735));
#17620=CARTESIAN_POINT('Ctrl Pts',(5.62101499943423,-0.208000000000001,
10.7795199127532));
#17621=CARTESIAN_POINT('Ctrl Pts',(5.62101499943423,0.670547542022765,10.7795199127532));
#17622=CARTESIAN_POINT('Ctrl Pts',(5.7936769541502,-0.208000000000001,10.7114411549111));
#17623=CARTESIAN_POINT('Ctrl Pts',(5.7936769541502,0.670547542022765,10.7114411549111));
#17624=CARTESIAN_POINT('Ctrl Pts',(5.96961932707136,-0.208000000000001,
10.6558377434042));
#17625=CARTESIAN_POINT('Ctrl Pts',(5.96961932707136,0.670547542022765,10.6558377434042));
#17626=CARTESIAN_POINT('Ctrl Pts',(6.14893768388704,-0.208000000000001,
10.6103475969888));
#17627=CARTESIAN_POINT('Ctrl Pts',(6.14893768388704,0.670547542022765,10.6103475969888));
#17628=CARTESIAN_POINT('Ctrl Pts',(6.32976796473819,-0.208000000000001,
10.5687216653907));
#17629=CARTESIAN_POINT('Ctrl Pts',(6.32976796473819,0.670547542022765,10.5687216653907));
#17630=CARTESIAN_POINT('Ctrl Pts',(6.50892555577775,-0.208000000000001,
10.5222908830264));
#17631=CARTESIAN_POINT('Ctrl Pts',(6.50892555577775,0.670547542022765,10.5222908830264));
#17632=CARTESIAN_POINT('Ctrl Pts',(6.68288828293941,-0.208000000000001,
10.462050267878));
#17633=CARTESIAN_POINT('Ctrl Pts',(6.68288828293941,0.670547542022765,10.462050267878));
#17634=CARTESIAN_POINT('Ctrl Pts',(6.84859008776107,-0.208000000000001,
10.3804015453596));
#17635=CARTESIAN_POINT('Ctrl Pts',(6.84859008776107,0.670547542022765,10.3804015453596));
#17636=CARTESIAN_POINT('Ctrl Pts',(7.00445448641038,-0.208000000000001,
10.2733319413005));
#17637=CARTESIAN_POINT('Ctrl Pts',(7.00445448641038,0.670547542022765,10.2733319413005));
#17638=CARTESIAN_POINT('Ctrl Pts',(7.15081550722288,-0.208000000000001,
10.1414720974144));
#17639=CARTESIAN_POINT('Ctrl Pts',(7.15081550722288,0.670547542022765,10.1414720974144));
#17640=CARTESIAN_POINT('Ctrl Pts',(7.28883796912684,-0.208000000000001,
9.98835756998534));
#17641=CARTESIAN_POINT('Ctrl Pts',(7.28883796912684,0.670547542022765,9.98835756998534));
#17642=CARTESIAN_POINT('Ctrl Pts',(7.41967047354988,-0.208000000000001,
9.81917361987377));
#17643=CARTESIAN_POINT('Ctrl Pts',(7.41967047354988,0.670547542022765,9.81917361987377));
#17644=CARTESIAN_POINT('Ctrl Pts',(7.54360573526532,-0.208000000000001,
9.63939026966049));
#17645=CARTESIAN_POINT('Ctrl Pts',(7.54360573526532,0.670547542022765,9.63939026966049));
#17646=CARTESIAN_POINT('Ctrl Pts',(7.6590003866074,-0.208000000000001,9.45324999450471));
#17647=CARTESIAN_POINT('Ctrl Pts',(7.6590003866074,0.670547542022765,9.45324999450471));
#17648=CARTESIAN_POINT('Ctrl Pts',(7.76209282457502,-0.208000000000001,
9.26297089919836));
#17649=CARTESIAN_POINT('Ctrl Pts',(7.76209282457502,0.670547542022765,9.26297089919836));
#17650=CARTESIAN_POINT('Ctrl Pts',(7.84862074946283,-0.208000000000001,
9.06945407017055));
#17651=CARTESIAN_POINT('Ctrl Pts',(7.84862074946283,0.670547542022765,9.06945407017055));
#17652=CARTESIAN_POINT('Ctrl Pts',(7.91508259073031,-0.208000000000001,
8.87266947141857));
#17653=CARTESIAN_POINT('Ctrl Pts',(7.91508259073031,0.670547542022765,8.87266947141857));
#17654=CARTESIAN_POINT('Ctrl Pts',(7.96007609558387,-0.208000000000001,
8.67216210283894));
#17655=CARTESIAN_POINT('Ctrl Pts',(7.96007609558387,0.670547542022765,8.67216210283894));
#17656=CARTESIAN_POINT('Ctrl Pts',(7.98575825096082,-0.208000000000001,
8.46752658699496));
#17657=CARTESIAN_POINT('Ctrl Pts',(7.98575825096082,0.670547542022765,8.46752658699496));
#17658=CARTESIAN_POINT('Ctrl Pts',(7.9987984391963,-0.208000000000001,8.25883677791438));
#17659=CARTESIAN_POINT('Ctrl Pts',(7.9987984391963,0.670547542022765,8.25883677791438));
#17660=CARTESIAN_POINT('Ctrl Pts',(8.00781893805568,-0.208000000000001,
8.04662057355209));
#17661=CARTESIAN_POINT('Ctrl Pts',(8.00781893805568,0.670547542022765,8.04662057355209));
#17662=CARTESIAN_POINT('Ctrl Pts',(8.02124364536257,-0.208000000000001,
7.8318867323277));
#17663=CARTESIAN_POINT('Ctrl Pts',(8.02124364536257,0.670547542022765,7.8318867323277));
#17664=CARTESIAN_POINT('Ctrl Pts',(8.04494633492827,-0.208000000000001,
7.61613341658679));
#17665=CARTESIAN_POINT('Ctrl Pts',(8.04494633492827,0.670547542022765,7.61613341658679));
#17666=CARTESIAN_POINT('Ctrl Pts',(8.08008348678094,-0.208000000000001,
7.40136016279815));
#17667=CARTESIAN_POINT('Ctrl Pts',(8.08008348678094,0.670547542022765,7.40136016279815));
#17668=CARTESIAN_POINT('Ctrl Pts',(8.12057943633426,-0.208000000000001,
7.19009032473197));
#17669=CARTESIAN_POINT('Ctrl Pts',(8.12057943633426,0.670547542022765,7.19009032473197));
#17670=CARTESIAN_POINT('Ctrl Pts',(8.15569042861283,-0.208000000000001,
6.98516923427904));
#17671=CARTESIAN_POINT('Ctrl Pts',(8.15569042861283,0.670547542022765,6.98516923427904));
#17672=CARTESIAN_POINT('Ctrl Pts',(8.17293082304204,-0.208000000000001,
6.78954489191915));
#17673=CARTESIAN_POINT('Ctrl Pts',(8.17293082304204,0.670547542022765,6.78954489191915));
#17674=CARTESIAN_POINT('Ctrl Pts',(8.16089752265956,-0.208000000000001,
6.60605451948904));
#17675=CARTESIAN_POINT('Ctrl Pts',(8.16089752265956,0.670547542022765,6.60605451948904));
#17676=CARTESIAN_POINT('Ctrl Pts',(8.11207116917844,-0.208000000000001,
6.43720976255638));
#17677=CARTESIAN_POINT('Ctrl Pts',(8.11207116917844,0.670547542022765,6.43720976255638));
#17678=CARTESIAN_POINT('Ctrl Pts',(8.02580908828092,-0.208000000000001,
6.28498018271691));
#17679=CARTESIAN_POINT('Ctrl Pts',(8.02580908828092,0.670547542022765,6.28498018271691));
#17680=CARTESIAN_POINT('Ctrl Pts',(7.90644860448881,-0.208000000000001,
6.15052660592943));
#17681=CARTESIAN_POINT('Ctrl Pts',(7.90644860448881,0.670547542022765,6.15052660592943));
#17682=CARTESIAN_POINT('Ctrl Pts',(7.76106756457749,-0.208000000000001,
6.03389995867286));
#17683=CARTESIAN_POINT('Ctrl Pts',(7.76106756457749,0.670547542022765,6.03389995867286));
#17684=CARTESIAN_POINT('Ctrl Pts',(7.59751903688427,-0.208000000000001,
5.93381436957244));
#17685=CARTESIAN_POINT('Ctrl Pts',(7.59751903688427,0.670547542022765,5.93381436957244));
#17686=CARTESIAN_POINT('Ctrl Pts',(7.42198551710643,-0.208000000000001,
5.84723737025948));
#17687=CARTESIAN_POINT('Ctrl Pts',(7.42198551710643,0.670547542022765,5.84723737025948));
#17688=CARTESIAN_POINT('Ctrl Pts',(7.23853768475023,-0.208000000000001,
5.76979878895671));
#17689=CARTESIAN_POINT('Ctrl Pts',(7.23853768475023,0.670547542022765,5.76979878895671));
#17690=CARTESIAN_POINT('Ctrl Pts',(7.04976847947264,-0.208000000000001,
5.69662713609756));
#17691=CARTESIAN_POINT('Ctrl Pts',(7.04976847947264,0.670547542022765,5.69662713609756));
#17692=CARTESIAN_POINT('Ctrl Pts',(6.85709976037512,-0.208000000000001,
5.62308582598972));
#17693=CARTESIAN_POINT('Ctrl Pts',(6.85709976037512,0.670547542022765,5.62308582598972));
#17694=CARTESIAN_POINT('Ctrl Pts',(6.66121503090593,-0.208000000000001,
5.54547963906641));
#17695=CARTESIAN_POINT('Ctrl Pts',(6.66121503090593,0.670547542022765,5.54547963906641));
#17696=CARTESIAN_POINT('Ctrl Pts',(6.46246210121974,-0.208000000000001,
5.46195513100458));
#17697=CARTESIAN_POINT('Ctrl Pts',(6.46246210121974,0.670547542022765,5.46195513100458));
#17698=CARTESIAN_POINT('Ctrl Pts',(6.26112587698791,-0.208000000000001,
5.37226655127806));
#17699=CARTESIAN_POINT('Ctrl Pts',(6.26112587698791,0.670547542022765,5.37226655127806));
#17700=CARTESIAN_POINT('Ctrl Pts',(6.05762450882876,-0.208000000000001,
5.27709955371581));
#17701=CARTESIAN_POINT('Ctrl Pts',(6.05762450882876,0.670547542022765,5.27709955371581));
#17702=CARTESIAN_POINT('Ctrl Pts',(5.85274048349253,-0.208000000000001,
5.17752467829117));
#17703=CARTESIAN_POINT('Ctrl Pts',(5.85274048349253,0.670547542022765,5.17752467829117));
#17704=CARTESIAN_POINT('Ctrl Pts',(5.6478173738032,-0.208000000000001,5.07442896098936));
#17705=CARTESIAN_POINT('Ctrl Pts',(5.6478173738032,0.670547542022765,5.07442896098936));
#17706=CARTESIAN_POINT('Ctrl Pts',(5.44501860313336,-0.208000000000001,
4.96787993373722));
#17707=CARTESIAN_POINT('Ctrl Pts',(5.44501860313336,0.670547542022765,4.96787993373722));
#17708=CARTESIAN_POINT('Ctrl Pts',(5.24741086000008,-0.208000000000001,
4.85676111532844));
#17709=CARTESIAN_POINT('Ctrl Pts',(5.24741086000008,0.670547542022765,4.85676111532844));
#17710=CARTESIAN_POINT('Ctrl Pts',(5.05850630701875,-0.208000000000001,
4.73929437247794));
#17711=CARTESIAN_POINT('Ctrl Pts',(5.05850630701875,0.670547542022765,4.73929437247794));
#17712=CARTESIAN_POINT('Ctrl Pts',(4.88190185104846,-0.208000000000001,
4.61340315498245));
#17713=CARTESIAN_POINT('Ctrl Pts',(4.88190185104846,0.670547542022765,4.61340315498245));
#17714=CARTESIAN_POINT('Ctrl Pts',(4.7208720035032,-0.208000000000001,4.47714872481864));
#17715=CARTESIAN_POINT('Ctrl Pts',(4.7208720035032,0.670547542022765,4.47714872481864));
#17716=CARTESIAN_POINT('Ctrl Pts',(4.57800047823784,-0.208000000000001,
4.32911151507775));
#17717=CARTESIAN_POINT('Ctrl Pts',(4.57800047823784,0.670547542022765,4.32911151507775));
#17718=CARTESIAN_POINT('Ctrl Pts',(4.4547451964031,-0.208000000000001,4.16885849319143));
#17719=CARTESIAN_POINT('Ctrl Pts',(4.4547451964031,0.670547542022765,4.16885849319143));
#17720=CARTESIAN_POINT('Ctrl Pts',(4.35148411330737,-0.208000000000001,
3.99681013615577));
#17721=CARTESIAN_POINT('Ctrl Pts',(4.35148411330737,0.670547542022765,3.99681013615577));
#17722=CARTESIAN_POINT('Ctrl Pts',(4.26765207024408,-0.208000000000001,
3.81399668859083));
#17723=CARTESIAN_POINT('Ctrl Pts',(4.26765207024408,0.670547542022765,3.81399668859083));
#17724=CARTESIAN_POINT('Ctrl Pts',(4.20184334854117,-0.208000000000001,
3.62185203209172));
#17725=CARTESIAN_POINT('Ctrl Pts',(4.20184334854117,0.670547542022765,3.62185203209172));
#17726=CARTESIAN_POINT('Ctrl Pts',(4.15193466045737,-0.208000000000001,
3.42199345348454));
#17727=CARTESIAN_POINT('Ctrl Pts',(4.15193466045737,0.670547542022765,3.42199345348454));
#17728=CARTESIAN_POINT('Ctrl Pts',(4.11518318246501,-0.208000000000001,
3.21600287470933));
#17729=CARTESIAN_POINT('Ctrl Pts',(4.11518318246501,0.670547542022765,3.21600287470933));
#17730=CARTESIAN_POINT('Ctrl Pts',(4.08854433447712,-0.208000000000001,
3.00529120729351));
#17731=CARTESIAN_POINT('Ctrl Pts',(4.08854433447712,0.670547542022765,3.00529120729351));
#17732=CARTESIAN_POINT('Ctrl Pts',(4.06899962712481,-0.208000000000001,
2.7909834104826));
#17733=CARTESIAN_POINT('Ctrl Pts',(4.06899962712481,0.670547542022765,2.7909834104826));
#17734=CARTESIAN_POINT('Ctrl Pts',(4.05390260344518,-0.208000000000001,
2.57377631141663));
#17735=CARTESIAN_POINT('Ctrl Pts',(4.05390260344518,0.670547542022765,2.57377631141663));
#17736=CARTESIAN_POINT('Ctrl Pts',(4.04126813644791,-0.208000000000001,
2.35385258470204));
#17737=CARTESIAN_POINT('Ctrl Pts',(4.04126813644791,0.670547542022765,2.35385258470204));
#17738=CARTESIAN_POINT('Ctrl Pts',(4.03021014446877,-0.208000000000001,
2.13065748555701));
#17739=CARTESIAN_POINT('Ctrl Pts',(4.03021014446877,0.670547542022765,2.13065748555701));
#17740=CARTESIAN_POINT('Ctrl Pts',(4.02066709528519,-0.208000000000001,
1.9033255681334));
#17741=CARTESIAN_POINT('Ctrl Pts',(4.02066709528519,0.670547542022765,1.9033255681334));
#17742=CARTESIAN_POINT('Ctrl Pts',(4.01278884602726,-0.208000000000001,
1.67161074402007));
#17743=CARTESIAN_POINT('Ctrl Pts',(4.01278884602726,0.670547542022765,1.67161074402007));
#17744=CARTESIAN_POINT('Ctrl Pts',(4.00768150999064,-0.208000000000001,
1.4831346983285));
#17745=CARTESIAN_POINT('Ctrl Pts',(4.00768150999064,0.670547542022765,1.4831346983285));
#17746=CARTESIAN_POINT('Ctrl Pts',(4.00406437985138,-0.208000000000001,
1.34113083543346));
#17747=CARTESIAN_POINT('Ctrl Pts',(4.00406437985138,0.670547542022765,1.34113083543346));
#17748=CARTESIAN_POINT('Ctrl Pts',(4.00142780906472,-0.208000000000001,
1.24685503532231));
#17749=CARTESIAN_POINT('Ctrl Pts',(4.00142780906472,0.670547542022765,1.24685503532231));
#17750=CARTESIAN_POINT('Ctrl Pts',(4.,-0.208000000000001,1.2));
#17751=CARTESIAN_POINT('Ctrl Pts',(4.,0.670547542022765,1.2));
#17752=CARTESIAN_POINT('',(2.88353005387235,0.507243591474958,1.12422135153943));
#17753=CARTESIAN_POINT('',(2.88353005387235,0.507243591474958,1.12422135153943));
#17754=CARTESIAN_POINT('Origin',(2.87260862269811,0.9008070635013,1.19957807558011));
#17755=CARTESIAN_POINT('Origin',(3.2,0.9,1.2));
#17756=CARTESIAN_POINT('',(-4.5,0.,1.2));
#17757=CARTESIAN_POINT('Ctrl Pts',(2.80364150531137,0.507243591474958,1.2));
#17758=CARTESIAN_POINT('Ctrl Pts',(2.80364150531137,-0.00544871829499161,
1.2));
#17759=CARTESIAN_POINT('Ctrl Pts',(2.82677300877721,0.507243591474958,1.2));
#17760=CARTESIAN_POINT('Ctrl Pts',(2.82677300877721,-0.00544871829499161,
1.2));
#17761=CARTESIAN_POINT('Ctrl Pts',(2.86687234890104,0.507243591474958,1.18130982994417));
#17762=CARTESIAN_POINT('Ctrl Pts',(2.86687234890104,-0.00544871829499161,
1.18130982994417));
#17763=CARTESIAN_POINT('Ctrl Pts',(2.88261462067456,0.507243591474958,1.14154581001993));
#17764=CARTESIAN_POINT('Ctrl Pts',(2.88261462067456,-0.00544871829499161,
1.14154581001993));
#17765=CARTESIAN_POINT('Ctrl Pts',(2.88353005387235,0.507243591474958,1.12422135153943));
#17766=CARTESIAN_POINT('Ctrl Pts',(2.88353005387235,-0.00544871829499161,
1.12422135153943));
#17767=CARTESIAN_POINT('',(2.80364150531137,0.5,1.2));
#17768=CARTESIAN_POINT('',(2.80364150531137,0.08,1.2));
#17769=CARTESIAN_POINT('Ctrl Pts',(2.80364150531137,0.5,1.2));
#17770=CARTESIAN_POINT('Ctrl Pts',(2.81379585169868,0.5,1.2));
#17771=CARTESIAN_POINT('Ctrl Pts',(2.82391024805161,0.499987289115092,1.19794137540632));
#17772=CARTESIAN_POINT('Ctrl Pts',(2.84273358019748,0.500098331041066,1.19035456836199));
#17773=CARTESIAN_POINT('Ctrl Pts',(2.85145390051855,0.500227305282778,1.18482590803764));
#17774=CARTESIAN_POINT('Ctrl Pts',(2.86742097463828,0.501061125385064,1.16977413119873));
#17775=CARTESIAN_POINT('Ctrl Pts',(2.87283116118724,0.501825922612233,1.16103188260708));
#17776=CARTESIAN_POINT('Ctrl Pts',(2.88055159121655,0.503819244531482,1.14408694758658));
#17777=CARTESIAN_POINT('Ctrl Pts',(2.8830040002538,0.505322771788675,1.13417685030768));
#17778=CARTESIAN_POINT('Ctrl Pts',(2.88353005387235,0.507243591474958,1.12422135153943));
#17779=CARTESIAN_POINT('Origin',(-4.18004567262178,-4.54425157915634E-9,
3.08202038908016));
#17780=CARTESIAN_POINT('',(-4.10062628985476,0.500000490290817,3.09201395473891));
#17781=CARTESIAN_POINT('',(-4.1,0.5,3.08202325217327));
#17782=CARTESIAN_POINT('Origin',(-4.1800260995291,0.500109554898197,3.08202161069944));
#17783=CARTESIAN_POINT('',(-4.1,0.5,3.08202325217208));
#17784=CARTESIAN_POINT('',(-4.1006262898548,2.17910572199157E-7,3.09201395473924));
#17785=CARTESIAN_POINT('Ctrl Pts',(-4.07743349288644,-3.,2.87542908850901));
#17786=CARTESIAN_POINT('Ctrl Pts',(-4.07743349288644,4.2,2.87542908850901));
#17787=CARTESIAN_POINT('Ctrl Pts',(-4.07979010068817,-3.,2.90134289838335));
#17788=CARTESIAN_POINT('Ctrl Pts',(-4.07979010068817,4.2,2.90134289838335));
#17789=CARTESIAN_POINT('Ctrl Pts',(-4.08631563412149,-3.,2.97000159076542));
#17790=CARTESIAN_POINT('Ctrl Pts',(-4.08631563412149,4.2,2.97000159076542));
#17791=CARTESIAN_POINT('Ctrl Pts',(-4.09817039437236,-3.,3.08076873096245));
#17792=CARTESIAN_POINT('Ctrl Pts',(-4.09817039437236,4.2,3.08076873096245));
#17793=CARTESIAN_POINT('Ctrl Pts',(-4.11809350439417,-3.,3.23231511387111));
#17794=CARTESIAN_POINT('Ctrl Pts',(-4.11809350439417,4.2,3.23231511387111));
#17795=CARTESIAN_POINT('Ctrl Pts',(-4.15193466045748,-3.,3.42199345348447));
#17796=CARTESIAN_POINT('Ctrl Pts',(-4.15193466045748,4.2,3.42199345348447));
#17797=CARTESIAN_POINT('Ctrl Pts',(-4.20184334854115,-3.,3.62185203209171));
#17798=CARTESIAN_POINT('Ctrl Pts',(-4.20184334854115,4.2,3.62185203209171));
#17799=CARTESIAN_POINT('Ctrl Pts',(-4.26765207024395,-3.,3.81399668859083));
#17800=CARTESIAN_POINT('Ctrl Pts',(-4.26765207024395,4.2,3.81399668859083));
#17801=CARTESIAN_POINT('Ctrl Pts',(-4.35148411330718,-3.,3.99681013615577));
#17802=CARTESIAN_POINT('Ctrl Pts',(-4.35148411330718,4.2,3.99681013615577));
#17803=CARTESIAN_POINT('Ctrl Pts',(-4.45474519640294,-3.,4.16885849319142));
#17804=CARTESIAN_POINT('Ctrl Pts',(-4.45474519640294,4.2,4.16885849319142));
#17805=CARTESIAN_POINT('Ctrl Pts',(-4.57800047823775,-3.,4.32911151507774));
#17806=CARTESIAN_POINT('Ctrl Pts',(-4.57800047823775,4.2,4.32911151507774));
#17807=CARTESIAN_POINT('Ctrl Pts',(-4.7208720035032,-3.,4.47714872481861));
#17808=CARTESIAN_POINT('Ctrl Pts',(-4.7208720035032,4.2,4.47714872481861));
#17809=CARTESIAN_POINT('Ctrl Pts',(-4.88190185104852,-3.,4.61340315498244));
#17810=CARTESIAN_POINT('Ctrl Pts',(-4.88190185104852,4.2,4.61340315498244));
#17811=CARTESIAN_POINT('Ctrl Pts',(-5.05850630701885,-3.,4.73929437247796));
#17812=CARTESIAN_POINT('Ctrl Pts',(-5.05850630701885,4.2,4.73929437247796));
#17813=CARTESIAN_POINT('Ctrl Pts',(-5.24741086000019,-3.,4.8567611153285));
#17814=CARTESIAN_POINT('Ctrl Pts',(-5.24741086000019,4.2,4.8567611153285));
#17815=CARTESIAN_POINT('Ctrl Pts',(-5.44501860313342,-3.,4.96787993373728));
#17816=CARTESIAN_POINT('Ctrl Pts',(-5.44501860313342,4.2,4.96787993373728));
#17817=CARTESIAN_POINT('Ctrl Pts',(-5.64781737380319,-3.,5.07442896098937));
#17818=CARTESIAN_POINT('Ctrl Pts',(-5.64781737380319,4.2,5.07442896098937));
#17819=CARTESIAN_POINT('Ctrl Pts',(-5.85274048349242,-3.,5.17752467829109));
#17820=CARTESIAN_POINT('Ctrl Pts',(-5.85274048349242,4.2,5.17752467829109));
#17821=CARTESIAN_POINT('Ctrl Pts',(-6.05762450882858,-3.,5.27709955371564));
#17822=CARTESIAN_POINT('Ctrl Pts',(-6.05762450882858,4.2,5.27709955371564));
#17823=CARTESIAN_POINT('Ctrl Pts',(-6.26112587698772,-3.,5.37226655127787));
#17824=CARTESIAN_POINT('Ctrl Pts',(-6.26112587698772,4.2,5.37226655127787));
#17825=CARTESIAN_POINT('Ctrl Pts',(-6.46246210121964,-3.,5.46195513100446));
#17826=CARTESIAN_POINT('Ctrl Pts',(-6.46246210121964,4.2,5.46195513100446));
#17827=CARTESIAN_POINT('Ctrl Pts',(-6.66121503090592,-3.,5.54547963906637));
#17828=CARTESIAN_POINT('Ctrl Pts',(-6.66121503090592,4.2,5.54547963906637));
#17829=CARTESIAN_POINT('Ctrl Pts',(-6.8570997603751,-3.,5.62308582598972));
#17830=CARTESIAN_POINT('Ctrl Pts',(-6.8570997603751,4.2,5.62308582598972));
#17831=CARTESIAN_POINT('Ctrl Pts',(-7.04976847947249,-3.,5.69662713609756));
#17832=CARTESIAN_POINT('Ctrl Pts',(-7.04976847947249,4.2,5.69662713609756));
#17833=CARTESIAN_POINT('Ctrl Pts',(-7.23853768475,-3.,5.76979878895672));
#17834=CARTESIAN_POINT('Ctrl Pts',(-7.23853768475,4.2,5.76979878895672));
#17835=CARTESIAN_POINT('Ctrl Pts',(-7.42198551710617,-3.,5.84723737025949));
#17836=CARTESIAN_POINT('Ctrl Pts',(-7.42198551710617,4.2,5.84723737025949));
#17837=CARTESIAN_POINT('Ctrl Pts',(-7.59751903688412,-3.,5.93381436957244));
#17838=CARTESIAN_POINT('Ctrl Pts',(-7.59751903688412,4.2,5.93381436957244));
#17839=CARTESIAN_POINT('Ctrl Pts',(-7.76106756457753,-3.,6.03389995867283));
#17840=CARTESIAN_POINT('Ctrl Pts',(-7.76106756457753,4.2,6.03389995867283));
#17841=CARTESIAN_POINT('Ctrl Pts',(-7.90644860448901,-3.,6.15052660592937));
#17842=CARTESIAN_POINT('Ctrl Pts',(-7.90644860448901,4.2,6.15052660592937));
#17843=CARTESIAN_POINT('Ctrl Pts',(-8.02580908828117,-3.,6.28498018271686));
#17844=CARTESIAN_POINT('Ctrl Pts',(-8.02580908828117,4.2,6.28498018271686));
#17845=CARTESIAN_POINT('Ctrl Pts',(-8.11207116917861,-3.,6.43720976255636));
#17846=CARTESIAN_POINT('Ctrl Pts',(-8.11207116917861,4.2,6.43720976255636));
#17847=CARTESIAN_POINT('Ctrl Pts',(-8.16089752265956,-3.,6.60605451948903));
#17848=CARTESIAN_POINT('Ctrl Pts',(-8.16089752265956,4.2,6.60605451948903));
#17849=CARTESIAN_POINT('Ctrl Pts',(-8.17293082304181,-3.,6.78954489191904));
#17850=CARTESIAN_POINT('Ctrl Pts',(-8.17293082304181,4.2,6.78954489191904));
#17851=CARTESIAN_POINT('Ctrl Pts',(-8.15569042861244,-3.,6.9851692342788));
#17852=CARTESIAN_POINT('Ctrl Pts',(-8.15569042861244,4.2,6.9851692342788));
#17853=CARTESIAN_POINT('Ctrl Pts',(-8.12057943633387,-3.,7.19009032473164));
#17854=CARTESIAN_POINT('Ctrl Pts',(-8.12057943633387,4.2,7.19009032473164));
#17855=CARTESIAN_POINT('Ctrl Pts',(-8.08008348678073,-3.,7.40136016279791));
#17856=CARTESIAN_POINT('Ctrl Pts',(-8.08008348678073,4.2,7.40136016279791));
#17857=CARTESIAN_POINT('Ctrl Pts',(-8.04494633492831,-3.,7.61613341658677));
#17858=CARTESIAN_POINT('Ctrl Pts',(-8.04494633492831,4.2,7.61613341658677));
#17859=CARTESIAN_POINT('Ctrl Pts',(-8.02124364536279,-3.,7.83188673232793));
#17860=CARTESIAN_POINT('Ctrl Pts',(-8.02124364536279,4.2,7.83188673232793));
#17861=CARTESIAN_POINT('Ctrl Pts',(-8.007818938056,-3.,8.04662057355248));
#17862=CARTESIAN_POINT('Ctrl Pts',(-8.007818938056,4.2,8.04662057355248));
#17863=CARTESIAN_POINT('Ctrl Pts',(-7.99879843919661,-3.,8.25883677791483));
#17864=CARTESIAN_POINT('Ctrl Pts',(-7.99879843919661,4.2,8.25883677791483));
#17865=CARTESIAN_POINT('Ctrl Pts',(-7.98575825096101,-3.,8.46752658699528));
#17866=CARTESIAN_POINT('Ctrl Pts',(-7.98575825096101,4.2,8.46752658699528));
#17867=CARTESIAN_POINT('Ctrl Pts',(-7.96007609558389,-3.,8.67216210283896));
#17868=CARTESIAN_POINT('Ctrl Pts',(-7.96007609558389,4.2,8.67216210283896));
#17869=CARTESIAN_POINT('Ctrl Pts',(-7.91508259073019,-3.,8.87266947141823));
#17870=CARTESIAN_POINT('Ctrl Pts',(-7.91508259073019,4.2,8.87266947141823));
#17871=CARTESIAN_POINT('Ctrl Pts',(-7.84862074946261,-3.,9.06945407016992));
#17872=CARTESIAN_POINT('Ctrl Pts',(-7.84862074946261,4.2,9.06945407016992));
#17873=CARTESIAN_POINT('Ctrl Pts',(-7.76209282457479,-3.,9.26297089919765));
#17874=CARTESIAN_POINT('Ctrl Pts',(-7.76209282457479,4.2,9.26297089919765));
#17875=CARTESIAN_POINT('Ctrl Pts',(-7.65900038660722,-3.,9.4532499945042));
#17876=CARTESIAN_POINT('Ctrl Pts',(-7.65900038660722,4.2,9.4532499945042));
#17877=CARTESIAN_POINT('Ctrl Pts',(-7.5436057352653,-3.,9.63939026966035));
#17878=CARTESIAN_POINT('Ctrl Pts',(-7.5436057352653,4.2,9.63939026966035));
#17879=CARTESIAN_POINT('Ctrl Pts',(-7.41967047355001,-3.,9.81917361987397));
#17880=CARTESIAN_POINT('Ctrl Pts',(-7.41967047355001,4.2,9.81917361987397));
#17881=CARTESIAN_POINT('Ctrl Pts',(-7.28883796912703,-3.,9.98835756998572));
#17882=CARTESIAN_POINT('Ctrl Pts',(-7.28883796912703,4.2,9.98835756998572));
#17883=CARTESIAN_POINT('Ctrl Pts',(-7.15081550722306,-3.,10.1414720974148));
#17884=CARTESIAN_POINT('Ctrl Pts',(-7.15081550722306,4.2,10.1414720974148));
#17885=CARTESIAN_POINT('Ctrl Pts',(-7.0044544864105,-3.,10.2733319413008));
#17886=CARTESIAN_POINT('Ctrl Pts',(-7.0044544864105,4.2,10.2733319413008));
#17887=CARTESIAN_POINT('Ctrl Pts',(-6.84859008776113,-3.,10.3804015453596));
#17888=CARTESIAN_POINT('Ctrl Pts',(-6.84859008776113,4.2,10.3804015453596));
#17889=CARTESIAN_POINT('Ctrl Pts',(-6.68288828293938,-3.,10.4620502678778));
#17890=CARTESIAN_POINT('Ctrl Pts',(-6.68288828293938,4.2,10.4620502678778));
#17891=CARTESIAN_POINT('Ctrl Pts',(-6.50892555577766,-3.,10.522290883026));
#17892=CARTESIAN_POINT('Ctrl Pts',(-6.50892555577766,4.2,10.522290883026));
#17893=CARTESIAN_POINT('Ctrl Pts',(-6.32976796473811,-3.,10.5687216653902));
#17894=CARTESIAN_POINT('Ctrl Pts',(-6.32976796473811,4.2,10.5687216653902));
#17895=CARTESIAN_POINT('Ctrl Pts',(-6.14893768388701,-3.,10.6103475969885));
#17896=CARTESIAN_POINT('Ctrl Pts',(-6.14893768388701,4.2,10.6103475969885));
#17897=CARTESIAN_POINT('Ctrl Pts',(-5.96961932707142,-3.,10.6558377434043));
#17898=CARTESIAN_POINT('Ctrl Pts',(-5.96961932707142,4.2,10.6558377434043));
#17899=CARTESIAN_POINT('Ctrl Pts',(-5.79367695415031,-3.,10.7114411549114));
#17900=CARTESIAN_POINT('Ctrl Pts',(-5.79367695415031,4.2,10.7114411549114));
#17901=CARTESIAN_POINT('Ctrl Pts',(-5.62101499943431,-3.,10.7795199127535));
#17902=CARTESIAN_POINT('Ctrl Pts',(-5.62101499943431,4.2,10.7795199127535));
#17903=CARTESIAN_POINT('Ctrl Pts',(-5.45051506148982,-3.,10.8599381259737));
#17904=CARTESIAN_POINT('Ctrl Pts',(-5.45051506148982,4.2,10.8599381259737));
#17905=CARTESIAN_POINT('Ctrl Pts',(-5.28082876351929,-3.,10.9511663773826));
#17906=CARTESIAN_POINT('Ctrl Pts',(-5.28082876351929,4.2,10.9511663773826));
#17907=CARTESIAN_POINT('Ctrl Pts',(-5.11112998264616,-3.,11.0513704191329));
#17908=CARTESIAN_POINT('Ctrl Pts',(-5.11112998264616,4.2,11.0513704191329));
#17909=CARTESIAN_POINT('Ctrl Pts',(-4.94211773226973,-3.,11.1598106424589));
#17910=CARTESIAN_POINT('Ctrl Pts',(-4.94211773226973,4.2,11.1598106424589));
#17911=CARTESIAN_POINT('Ctrl Pts',(-4.77596612414951,-3.,11.2768795166235));
#17912=CARTESIAN_POINT('Ctrl Pts',(-4.77596612414951,4.2,11.2768795166235));
#17913=CARTESIAN_POINT('Ctrl Pts',(-4.61532593596946,-3.,11.4029224160731));
#17914=CARTESIAN_POINT('Ctrl Pts',(-4.61532593596946,4.2,11.4029224160731));
#17915=CARTESIAN_POINT('Ctrl Pts',(-4.46255574628757,-3.,11.5373242211527));
#17916=CARTESIAN_POINT('Ctrl Pts',(-4.46255574628757,4.2,11.5373242211527));
#17917=CARTESIAN_POINT('Ctrl Pts',(-4.31893584999241,-3.,11.6776492463597));
#17918=CARTESIAN_POINT('Ctrl Pts',(-4.31893584999241,4.2,11.6776492463597));
#17919=CARTESIAN_POINT('Ctrl Pts',(-4.18369962429796,-3.,11.8183570873721));
#17920=CARTESIAN_POINT('Ctrl Pts',(-4.18369962429796,4.2,11.8183570873721));
#17921=CARTESIAN_POINT('Ctrl Pts',(-4.05395481372655,-3.,11.9514202619522));
#17922=CARTESIAN_POINT('Ctrl Pts',(-4.05395481372655,4.2,11.9514202619522));
#17923=CARTESIAN_POINT('Ctrl Pts',(-3.92533033057354,-3.,12.0684942936867));
#17924=CARTESIAN_POINT('Ctrl Pts',(-3.92533033057354,4.2,12.0684942936867));
#17925=CARTESIAN_POINT('Ctrl Pts',(-3.79241297762166,-3.,12.1626050652586));
#17926=CARTESIAN_POINT('Ctrl Pts',(-3.79241297762166,4.2,12.1626050652586));
#17927=CARTESIAN_POINT('Ctrl Pts',(-3.64927048315908,-3.,12.2301117722809));
#17928=CARTESIAN_POINT('Ctrl Pts',(-3.64927048315908,4.2,12.2301117722809));
#17929=CARTESIAN_POINT('Ctrl Pts',(-3.48993681214334,-3.,12.2723364229645));
#17930=CARTESIAN_POINT('Ctrl Pts',(-3.48993681214334,4.2,12.2723364229645));
#17931=CARTESIAN_POINT('Ctrl Pts',(-3.30884480305534,-3.,12.2938762651139));
#17932=CARTESIAN_POINT('Ctrl Pts',(-3.30884480305534,4.2,12.2938762651139));
#17933=CARTESIAN_POINT('Ctrl Pts',(-3.10127560868576,-3.,12.3010487961981));
#17934=CARTESIAN_POINT('Ctrl Pts',(-3.10127560868576,4.2,12.3010487961981));
#17935=CARTESIAN_POINT('Ctrl Pts',(-2.86376302967345,-3.,12.300400839059));
#17936=CARTESIAN_POINT('Ctrl Pts',(-2.86376302967345,4.2,12.300400839059));
#17937=CARTESIAN_POINT('Ctrl Pts',(-2.59461297443094,-3.,12.2969132923574));
#17938=CARTESIAN_POINT('Ctrl Pts',(-2.59461297443094,4.2,12.2969132923574));
#17939=CARTESIAN_POINT('Ctrl Pts',(-2.29394197380209,-3.,12.2935845551224));
#17940=CARTESIAN_POINT('Ctrl Pts',(-2.29394197380209,4.2,12.2935845551224));
#17941=CARTESIAN_POINT('Ctrl Pts',(-1.96338745719135,-3.,12.2919684497906));
#17942=CARTESIAN_POINT('Ctrl Pts',(-1.96338745719135,4.2,12.2919684497906));
#17943=CARTESIAN_POINT('Ctrl Pts',(-1.60591558979456,-3.,12.2924280531798));
#17944=CARTESIAN_POINT('Ctrl Pts',(-1.60591558979456,4.2,12.2924280531798));
#17945=CARTESIAN_POINT('Ctrl Pts',(-1.22558901314075,-3.,12.2945066442122));
#17946=CARTESIAN_POINT('Ctrl Pts',(-1.22558901314075,4.2,12.2945066442122));
#17947=CARTESIAN_POINT('Ctrl Pts',(-0.827351903312651,-3.,12.2972483292773));
#17948=CARTESIAN_POINT('Ctrl Pts',(-0.827351903312651,4.2,12.2972483292773));
#17949=CARTESIAN_POINT('Ctrl Pts',(-0.498916532526571,-3.,12.299081889758));
#17950=CARTESIAN_POINT('Ctrl Pts',(-0.498916532526571,4.2,12.299081889758));
#17951=CARTESIAN_POINT('Ctrl Pts',(-0.249771440080693,-3.,12.2998330708668));
#17952=CARTESIAN_POINT('Ctrl Pts',(-0.249771440080693,4.2,12.2998330708668));
#17953=CARTESIAN_POINT('Ctrl Pts',(-0.0832571466935557,-3.,12.2999999999989));
#17954=CARTESIAN_POINT('Ctrl Pts',(-0.0832571466935557,4.2,12.2999999999989));
#17955=CARTESIAN_POINT('Ctrl Pts',(0.,-3.,12.3));
#17956=CARTESIAN_POINT('Ctrl Pts',(0.,4.2,12.3));
#17957=CARTESIAN_POINT('Ctrl Pts',(0.0832571466935396,-3.,12.3000000000011));
#17958=CARTESIAN_POINT('Ctrl Pts',(0.0832571466935396,4.2,12.3000000000011));
#17959=CARTESIAN_POINT('Ctrl Pts',(0.24977144008061,-3.,12.2998330708736));
#17960=CARTESIAN_POINT('Ctrl Pts',(0.24977144008061,4.2,12.2998330708736));
#17961=CARTESIAN_POINT('Ctrl Pts',(0.498916532526534,-3.,12.2990818897713));
#17962=CARTESIAN_POINT('Ctrl Pts',(0.498916532526534,4.2,12.2990818897713));
#17963=CARTESIAN_POINT('Ctrl Pts',(0.827351903312438,-3.,12.2972483292974));
#17964=CARTESIAN_POINT('Ctrl Pts',(0.827351903312438,4.2,12.2972483292974));
#17965=CARTESIAN_POINT('Ctrl Pts',(1.22558901314046,-3.,12.2945066442369));
#17966=CARTESIAN_POINT('Ctrl Pts',(1.22558901314046,4.2,12.2945066442369));
#17967=CARTESIAN_POINT('Ctrl Pts',(1.60591558979418,-3.,12.2924280532047));
#17968=CARTESIAN_POINT('Ctrl Pts',(1.60591558979418,4.2,12.2924280532047));
#17969=CARTESIAN_POINT('Ctrl Pts',(1.96338745719096,-3.,12.291968449812));
#17970=CARTESIAN_POINT('Ctrl Pts',(1.96338745719096,4.2,12.291968449812));
#17971=CARTESIAN_POINT('Ctrl Pts',(2.29394197380175,-3.,12.2935845551378));
#17972=CARTESIAN_POINT('Ctrl Pts',(2.29394197380175,4.2,12.2935845551378));
#17973=CARTESIAN_POINT('Ctrl Pts',(2.59461297443069,-3.,12.2969132923658));
#17974=CARTESIAN_POINT('Ctrl Pts',(2.59461297443069,4.2,12.2969132923658));
#17975=CARTESIAN_POINT('Ctrl Pts',(2.86376302967335,-3.,12.3004008390612));
#17976=CARTESIAN_POINT('Ctrl Pts',(2.86376302967335,4.2,12.3004008390612));
#17977=CARTESIAN_POINT('Ctrl Pts',(3.10127560868576,-3.,12.3010487961961));
#17978=CARTESIAN_POINT('Ctrl Pts',(3.10127560868576,4.2,12.3010487961961));
#17979=CARTESIAN_POINT('Ctrl Pts',(3.30884480305537,-3.,12.2938762651102));
#17980=CARTESIAN_POINT('Ctrl Pts',(3.30884480305537,4.2,12.2938762651102));
#17981=CARTESIAN_POINT('Ctrl Pts',(3.48993681214337,-3.,12.2723364229612));
#17982=CARTESIAN_POINT('Ctrl Pts',(3.48993681214337,4.2,12.2723364229612));
#17983=CARTESIAN_POINT('Ctrl Pts',(3.64927048315907,-3.,12.2301117722792));
#17984=CARTESIAN_POINT('Ctrl Pts',(3.64927048315907,4.2,12.2301117722792));
#17985=CARTESIAN_POINT('Ctrl Pts',(3.79241297762162,-3.,12.1626050652587));
#17986=CARTESIAN_POINT('Ctrl Pts',(3.79241297762162,4.2,12.1626050652587));
#17987=CARTESIAN_POINT('Ctrl Pts',(3.92533033057351,-3.,12.0684942936878));
#17988=CARTESIAN_POINT('Ctrl Pts',(3.92533033057351,4.2,12.0684942936878));
#17989=CARTESIAN_POINT('Ctrl Pts',(4.05395481372655,-3.,11.9514202619535));
#17990=CARTESIAN_POINT('Ctrl Pts',(4.05395481372655,4.2,11.9514202619535));
#17991=CARTESIAN_POINT('Ctrl Pts',(4.18369962429796,-3.,11.8183570873731));
#17992=CARTESIAN_POINT('Ctrl Pts',(4.18369962429796,4.2,11.8183570873731));
#17993=CARTESIAN_POINT('Ctrl Pts',(4.3189358499924,-3.,11.67764924636));
#17994=CARTESIAN_POINT('Ctrl Pts',(4.3189358499924,4.2,11.67764924636));
#17995=CARTESIAN_POINT('Ctrl Pts',(4.46255574628753,-3.,11.5373242211525));
#17996=CARTESIAN_POINT('Ctrl Pts',(4.46255574628753,4.2,11.5373242211525));
#17997=CARTESIAN_POINT('Ctrl Pts',(4.61532593596939,-3.,11.4029224160728));
#17998=CARTESIAN_POINT('Ctrl Pts',(4.61532593596939,4.2,11.4029224160728));
#17999=CARTESIAN_POINT('Ctrl Pts',(4.77596612414944,-3.,11.2768795166233));
#18000=CARTESIAN_POINT('Ctrl Pts',(4.77596612414944,4.2,11.2768795166233));
#18001=CARTESIAN_POINT('Ctrl Pts',(4.94211773226968,-3.,11.1598106424589));
#18002=CARTESIAN_POINT('Ctrl Pts',(4.94211773226968,4.2,11.1598106424589));
#18003=CARTESIAN_POINT('Ctrl Pts',(5.11112998264613,-3.,11.051370419133));
#18004=CARTESIAN_POINT('Ctrl Pts',(5.11112998264613,4.2,11.051370419133));
#18005=CARTESIAN_POINT('Ctrl Pts',(5.28082876351925,-3.,10.9511663773825));
#18006=CARTESIAN_POINT('Ctrl Pts',(5.28082876351925,4.2,10.9511663773825));
#18007=CARTESIAN_POINT('Ctrl Pts',(5.45051506148977,-3.,10.8599381259735));
#18008=CARTESIAN_POINT('Ctrl Pts',(5.45051506148977,4.2,10.8599381259735));
#18009=CARTESIAN_POINT('Ctrl Pts',(5.62101499943423,-3.,10.7795199127532));
#18010=CARTESIAN_POINT('Ctrl Pts',(5.62101499943423,4.2,10.7795199127532));
#18011=CARTESIAN_POINT('Ctrl Pts',(5.7936769541502,-3.,10.7114411549111));
#18012=CARTESIAN_POINT('Ctrl Pts',(5.7936769541502,4.2,10.7114411549111));
#18013=CARTESIAN_POINT('Ctrl Pts',(5.96961932707136,-3.,10.6558377434042));
#18014=CARTESIAN_POINT('Ctrl Pts',(5.96961932707136,4.2,10.6558377434042));
#18015=CARTESIAN_POINT('Ctrl Pts',(6.14893768388704,-3.,10.6103475969888));
#18016=CARTESIAN_POINT('Ctrl Pts',(6.14893768388704,4.2,10.6103475969888));
#18017=CARTESIAN_POINT('Ctrl Pts',(6.32976796473819,-3.,10.5687216653907));
#18018=CARTESIAN_POINT('Ctrl Pts',(6.32976796473819,4.2,10.5687216653907));
#18019=CARTESIAN_POINT('Ctrl Pts',(6.50892555577775,-3.,10.5222908830264));
#18020=CARTESIAN_POINT('Ctrl Pts',(6.50892555577775,4.2,10.5222908830264));
#18021=CARTESIAN_POINT('Ctrl Pts',(6.68288828293941,-3.,10.462050267878));
#18022=CARTESIAN_POINT('Ctrl Pts',(6.68288828293941,4.2,10.462050267878));
#18023=CARTESIAN_POINT('Ctrl Pts',(6.84859008776107,-3.,10.3804015453596));
#18024=CARTESIAN_POINT('Ctrl Pts',(6.84859008776107,4.2,10.3804015453596));
#18025=CARTESIAN_POINT('Ctrl Pts',(7.00445448641038,-3.,10.2733319413005));
#18026=CARTESIAN_POINT('Ctrl Pts',(7.00445448641038,4.2,10.2733319413005));
#18027=CARTESIAN_POINT('Ctrl Pts',(7.15081550722288,-3.,10.1414720974144));
#18028=CARTESIAN_POINT('Ctrl Pts',(7.15081550722288,4.2,10.1414720974144));
#18029=CARTESIAN_POINT('Ctrl Pts',(7.28883796912684,-3.,9.98835756998534));
#18030=CARTESIAN_POINT('Ctrl Pts',(7.28883796912684,4.2,9.98835756998534));
#18031=CARTESIAN_POINT('Ctrl Pts',(7.41967047354988,-3.,9.81917361987377));
#18032=CARTESIAN_POINT('Ctrl Pts',(7.41967047354988,4.2,9.81917361987377));
#18033=CARTESIAN_POINT('Ctrl Pts',(7.54360573526532,-3.,9.63939026966049));
#18034=CARTESIAN_POINT('Ctrl Pts',(7.54360573526532,4.2,9.63939026966049));
#18035=CARTESIAN_POINT('Ctrl Pts',(7.6590003866074,-3.,9.45324999450471));
#18036=CARTESIAN_POINT('Ctrl Pts',(7.6590003866074,4.2,9.45324999450471));
#18037=CARTESIAN_POINT('Ctrl Pts',(7.76209282457502,-3.,9.26297089919836));
#18038=CARTESIAN_POINT('Ctrl Pts',(7.76209282457502,4.2,9.26297089919836));
#18039=CARTESIAN_POINT('Ctrl Pts',(7.84862074946283,-3.,9.06945407017055));
#18040=CARTESIAN_POINT('Ctrl Pts',(7.84862074946283,4.2,9.06945407017055));
#18041=CARTESIAN_POINT('Ctrl Pts',(7.91508259073031,-3.,8.87266947141857));
#18042=CARTESIAN_POINT('Ctrl Pts',(7.91508259073031,4.2,8.87266947141857));
#18043=CARTESIAN_POINT('Ctrl Pts',(7.96007609558387,-3.,8.67216210283894));
#18044=CARTESIAN_POINT('Ctrl Pts',(7.96007609558387,4.2,8.67216210283894));
#18045=CARTESIAN_POINT('Ctrl Pts',(7.98575825096082,-3.,8.46752658699496));
#18046=CARTESIAN_POINT('Ctrl Pts',(7.98575825096082,4.2,8.46752658699496));
#18047=CARTESIAN_POINT('Ctrl Pts',(7.9987984391963,-3.,8.25883677791438));
#18048=CARTESIAN_POINT('Ctrl Pts',(7.9987984391963,4.2,8.25883677791438));
#18049=CARTESIAN_POINT('Ctrl Pts',(8.00781893805568,-3.,8.04662057355209));
#18050=CARTESIAN_POINT('Ctrl Pts',(8.00781893805568,4.2,8.04662057355209));
#18051=CARTESIAN_POINT('Ctrl Pts',(8.02124364536257,-3.,7.8318867323277));
#18052=CARTESIAN_POINT('Ctrl Pts',(8.02124364536257,4.2,7.8318867323277));
#18053=CARTESIAN_POINT('Ctrl Pts',(8.04494633492827,-3.,7.61613341658679));
#18054=CARTESIAN_POINT('Ctrl Pts',(8.04494633492827,4.2,7.61613341658679));
#18055=CARTESIAN_POINT('Ctrl Pts',(8.08008348678094,-3.,7.40136016279815));
#18056=CARTESIAN_POINT('Ctrl Pts',(8.08008348678094,4.2,7.40136016279815));
#18057=CARTESIAN_POINT('Ctrl Pts',(8.12057943633426,-3.,7.19009032473197));
#18058=CARTESIAN_POINT('Ctrl Pts',(8.12057943633426,4.2,7.19009032473197));
#18059=CARTESIAN_POINT('Ctrl Pts',(8.15569042861283,-3.,6.98516923427904));
#18060=CARTESIAN_POINT('Ctrl Pts',(8.15569042861283,4.2,6.98516923427904));
#18061=CARTESIAN_POINT('Ctrl Pts',(8.17293082304204,-3.,6.78954489191915));
#18062=CARTESIAN_POINT('Ctrl Pts',(8.17293082304204,4.2,6.78954489191915));
#18063=CARTESIAN_POINT('Ctrl Pts',(8.16089752265956,-3.,6.60605451948904));
#18064=CARTESIAN_POINT('Ctrl Pts',(8.16089752265956,4.2,6.60605451948904));
#18065=CARTESIAN_POINT('Ctrl Pts',(8.11207116917844,-3.,6.43720976255638));
#18066=CARTESIAN_POINT('Ctrl Pts',(8.11207116917844,4.2,6.43720976255638));
#18067=CARTESIAN_POINT('Ctrl Pts',(8.02580908828092,-3.,6.28498018271691));
#18068=CARTESIAN_POINT('Ctrl Pts',(8.02580908828092,4.2,6.28498018271691));
#18069=CARTESIAN_POINT('Ctrl Pts',(7.90644860448881,-3.,6.15052660592943));
#18070=CARTESIAN_POINT('Ctrl Pts',(7.90644860448881,4.2,6.15052660592943));
#18071=CARTESIAN_POINT('Ctrl Pts',(7.76106756457749,-3.,6.03389995867286));
#18072=CARTESIAN_POINT('Ctrl Pts',(7.76106756457749,4.2,6.03389995867286));
#18073=CARTESIAN_POINT('Ctrl Pts',(7.59751903688427,-3.,5.93381436957244));
#18074=CARTESIAN_POINT('Ctrl Pts',(7.59751903688427,4.2,5.93381436957244));
#18075=CARTESIAN_POINT('Ctrl Pts',(7.42198551710643,-3.,5.84723737025948));
#18076=CARTESIAN_POINT('Ctrl Pts',(7.42198551710643,4.2,5.84723737025948));
#18077=CARTESIAN_POINT('Ctrl Pts',(7.23853768475023,-3.,5.76979878895671));
#18078=CARTESIAN_POINT('Ctrl Pts',(7.23853768475023,4.2,5.76979878895671));
#18079=CARTESIAN_POINT('Ctrl Pts',(7.04976847947264,-3.,5.69662713609756));
#18080=CARTESIAN_POINT('Ctrl Pts',(7.04976847947264,4.2,5.69662713609756));
#18081=CARTESIAN_POINT('Ctrl Pts',(6.85709976037512,-3.,5.62308582598972));
#18082=CARTESIAN_POINT('Ctrl Pts',(6.85709976037512,4.2,5.62308582598972));
#18083=CARTESIAN_POINT('Ctrl Pts',(6.66121503090593,-3.,5.54547963906641));
#18084=CARTESIAN_POINT('Ctrl Pts',(6.66121503090593,4.2,5.54547963906641));
#18085=CARTESIAN_POINT('Ctrl Pts',(6.46246210121974,-3.,5.46195513100458));
#18086=CARTESIAN_POINT('Ctrl Pts',(6.46246210121974,4.2,5.46195513100458));
#18087=CARTESIAN_POINT('Ctrl Pts',(6.26112587698791,-3.,5.37226655127806));
#18088=CARTESIAN_POINT('Ctrl Pts',(6.26112587698791,4.2,5.37226655127806));
#18089=CARTESIAN_POINT('Ctrl Pts',(6.05762450882876,-3.,5.27709955371581));
#18090=CARTESIAN_POINT('Ctrl Pts',(6.05762450882876,4.2,5.27709955371581));
#18091=CARTESIAN_POINT('Ctrl Pts',(5.85274048349253,-3.,5.17752467829117));
#18092=CARTESIAN_POINT('Ctrl Pts',(5.85274048349253,4.2,5.17752467829117));
#18093=CARTESIAN_POINT('Ctrl Pts',(5.6478173738032,-3.,5.07442896098936));
#18094=CARTESIAN_POINT('Ctrl Pts',(5.6478173738032,4.2,5.07442896098936));
#18095=CARTESIAN_POINT('Ctrl Pts',(5.44501860313336,-3.,4.96787993373722));
#18096=CARTESIAN_POINT('Ctrl Pts',(5.44501860313336,4.2,4.96787993373722));
#18097=CARTESIAN_POINT('Ctrl Pts',(5.24741086000008,-3.,4.85676111532844));
#18098=CARTESIAN_POINT('Ctrl Pts',(5.24741086000008,4.2,4.85676111532844));
#18099=CARTESIAN_POINT('Ctrl Pts',(5.05850630701875,-3.,4.73929437247794));
#18100=CARTESIAN_POINT('Ctrl Pts',(5.05850630701875,4.2,4.73929437247794));
#18101=CARTESIAN_POINT('Ctrl Pts',(4.88190185104846,-3.,4.61340315498245));
#18102=CARTESIAN_POINT('Ctrl Pts',(4.88190185104846,4.2,4.61340315498245));
#18103=CARTESIAN_POINT('Ctrl Pts',(4.7208720035032,-3.,4.47714872481864));
#18104=CARTESIAN_POINT('Ctrl Pts',(4.7208720035032,4.2,4.47714872481864));
#18105=CARTESIAN_POINT('Ctrl Pts',(4.57800047823784,-3.,4.32911151507775));
#18106=CARTESIAN_POINT('Ctrl Pts',(4.57800047823784,4.2,4.32911151507775));
#18107=CARTESIAN_POINT('Ctrl Pts',(4.4547451964031,-3.,4.16885849319143));
#18108=CARTESIAN_POINT('Ctrl Pts',(4.4547451964031,4.2,4.16885849319143));
#18109=CARTESIAN_POINT('Ctrl Pts',(4.35148411330737,-3.,3.99681013615577));
#18110=CARTESIAN_POINT('Ctrl Pts',(4.35148411330737,4.2,3.99681013615577));
#18111=CARTESIAN_POINT('Ctrl Pts',(4.26765207024408,-3.,3.81399668859083));
#18112=CARTESIAN_POINT('Ctrl Pts',(4.26765207024408,4.2,3.81399668859083));
#18113=CARTESIAN_POINT('Ctrl Pts',(4.20184334854117,-3.,3.62185203209172));
#18114=CARTESIAN_POINT('Ctrl Pts',(4.20184334854117,4.2,3.62185203209172));
#18115=CARTESIAN_POINT('Ctrl Pts',(4.15193466045737,-3.,3.42199345348454));
#18116=CARTESIAN_POINT('Ctrl Pts',(4.15193466045737,4.2,3.42199345348454));
#18117=CARTESIAN_POINT('Ctrl Pts',(4.11518318246501,-3.,3.21600287470933));
#18118=CARTESIAN_POINT('Ctrl Pts',(4.11518318246501,4.2,3.21600287470933));
#18119=CARTESIAN_POINT('Ctrl Pts',(4.08854433447712,-3.,3.00529120729351));
#18120=CARTESIAN_POINT('Ctrl Pts',(4.08854433447712,4.2,3.00529120729351));
#18121=CARTESIAN_POINT('Ctrl Pts',(4.06899962712481,-3.,2.7909834104826));
#18122=CARTESIAN_POINT('Ctrl Pts',(4.06899962712481,4.2,2.7909834104826));
#18123=CARTESIAN_POINT('Ctrl Pts',(4.05390260344518,-3.,2.57377631141663));
#18124=CARTESIAN_POINT('Ctrl Pts',(4.05390260344518,4.2,2.57377631141663));
#18125=CARTESIAN_POINT('Ctrl Pts',(4.04126813644791,-3.,2.35385258470204));
#18126=CARTESIAN_POINT('Ctrl Pts',(4.04126813644791,4.2,2.35385258470204));
#18127=CARTESIAN_POINT('Ctrl Pts',(4.03021014446877,-3.,2.13065748555701));
#18128=CARTESIAN_POINT('Ctrl Pts',(4.03021014446877,4.2,2.13065748555701));
#18129=CARTESIAN_POINT('Ctrl Pts',(4.02066709528519,-3.,1.9033255681334));
#18130=CARTESIAN_POINT('Ctrl Pts',(4.02066709528519,4.2,1.9033255681334));
#18131=CARTESIAN_POINT('Ctrl Pts',(4.012782399266,-3.,1.67142113207676));
#18132=CARTESIAN_POINT('Ctrl Pts',(4.012782399266,4.2,1.67142113207676));
#18133=CARTESIAN_POINT('Ctrl Pts',(4.00639322616619,-3.,1.4355810193293));
#18134=CARTESIAN_POINT('Ctrl Pts',(4.00639322616619,4.2,1.4355810193293));
#18135=CARTESIAN_POINT('Ctrl Pts',(4.00047520099043,-3.,1.19819542279832));
#18136=CARTESIAN_POINT('Ctrl Pts',(4.00047520099043,4.2,1.19819542279832));
#18137=CARTESIAN_POINT('Ctrl Pts',(3.99260375067002,-3.,0.964078729991153));
#18138=CARTESIAN_POINT('Ctrl Pts',(3.99260375067002,4.2,0.964078729991153));
#18139=CARTESIAN_POINT('Ctrl Pts',(3.97841403016118,-3.,0.741129277895168));
#18140=CARTESIAN_POINT('Ctrl Pts',(3.97841403016118,4.2,0.741129277895168));
#18141=CARTESIAN_POINT('Ctrl Pts',(3.95259200169988,-3.,0.538436816836329));
#18142=CARTESIAN_POINT('Ctrl Pts',(3.95259200169988,4.2,0.538436816836329));
#18143=CARTESIAN_POINT('Ctrl Pts',(3.90986572419832,-3.,0.364350357241537));
#18144=CARTESIAN_POINT('Ctrl Pts',(3.90986572419832,4.2,0.364350357241537));
#18145=CARTESIAN_POINT('Ctrl Pts',(3.84598208672298,-3.,0.224659532804428));
#18146=CARTESIAN_POINT('Ctrl Pts',(3.84598208672298,4.2,0.224659532804428));
#18147=CARTESIAN_POINT('Ctrl Pts',(3.75872318140661,-3.,0.120497232333236));
#18148=CARTESIAN_POINT('Ctrl Pts',(3.75872318140661,4.2,0.120497232333236));
#18149=CARTESIAN_POINT('Ctrl Pts',(3.64881642260075,-3.,0.0470540298718229));
#18150=CARTESIAN_POINT('Ctrl Pts',(3.64881642260075,4.2,0.0470540298718229));
#18151=CARTESIAN_POINT('Ctrl Pts',(3.52045328348988,-3.,-0.00118366394786523));
#18152=CARTESIAN_POINT('Ctrl Pts',(3.52045328348988,4.2,-0.00118366394786523));
#18153=CARTESIAN_POINT('Ctrl Pts',(3.3816469894381,-3.,-0.0263068037111615));
#18154=CARTESIAN_POINT('Ctrl Pts',(3.3816469894381,4.2,-0.0263068037111615));
#18155=CARTESIAN_POINT('Ctrl Pts',(3.2451100102617,-3.,-0.0214179570895094));
#18156=CARTESIAN_POINT('Ctrl Pts',(3.2451100102617,4.2,-0.0214179570895094));
#18157=CARTESIAN_POINT('Ctrl Pts',(3.12452733970665,-3.,0.0241851999814078));
#18158=CARTESIAN_POINT('Ctrl Pts',(3.12452733970665,4.2,0.0241851999814078));
#18159=CARTESIAN_POINT('Ctrl Pts',(3.03063129752059,-3.,0.119017371327004));
#18160=CARTESIAN_POINT('Ctrl Pts',(3.03063129752059,4.2,0.119017371327004));
#18161=CARTESIAN_POINT('Ctrl Pts',(2.96639254265844,-3.,0.262319630540593));
#18162=CARTESIAN_POINT('Ctrl Pts',(2.96639254265844,4.2,0.262319630540593));
#18163=CARTESIAN_POINT('Ctrl Pts',(2.92780415844446,-3.,0.444963858672424));
#18164=CARTESIAN_POINT('Ctrl Pts',(2.92780415844446,4.2,0.444963858672424));
#18165=CARTESIAN_POINT('Ctrl Pts',(2.90717911786689,-3.,0.65402023086958));
#18166=CARTESIAN_POINT('Ctrl Pts',(2.90717911786689,4.2,0.65402023086958));
#18167=CARTESIAN_POINT('Ctrl Pts',(2.89547076625581,-3.,0.875890304828918));
#18168=CARTESIAN_POINT('Ctrl Pts',(2.89547076625581,4.2,0.875890304828918));
#18169=CARTESIAN_POINT('Ctrl Pts',(2.88537704766906,-3.,1.10060381648398));
#18170=CARTESIAN_POINT('Ctrl Pts',(2.88537704766906,4.2,1.10060381648398));
#18171=CARTESIAN_POINT('Ctrl Pts',(2.8728456296504,-3.,1.32371934078733));
#18172=CARTESIAN_POINT('Ctrl Pts',(2.8728456296504,4.2,1.32371934078733));
#18173=CARTESIAN_POINT('Ctrl Pts',(2.85578261679345,-3.,1.54401727992264));
#18174=CARTESIAN_POINT('Ctrl Pts',(2.85578261679345,4.2,1.54401727992264));
#18175=CARTESIAN_POINT('Ctrl Pts',(2.83335686249019,-3.,1.76209503442146));
#18176=CARTESIAN_POINT('Ctrl Pts',(2.83335686249019,4.2,1.76209503442146));
#18177=CARTESIAN_POINT('Ctrl Pts',(2.80505146480345,-3.,1.97856787413951));
#18178=CARTESIAN_POINT('Ctrl Pts',(2.80505146480345,4.2,1.97856787413951));
#18179=CARTESIAN_POINT('Ctrl Pts',(2.76985908233915,-3.,2.19251877196071));
#18180=CARTESIAN_POINT('Ctrl Pts',(2.76985908233915,4.2,2.19251877196071));
#18181=CARTESIAN_POINT('Ctrl Pts',(2.72531955636536,-3.,2.39962532458029));
#18182=CARTESIAN_POINT('Ctrl Pts',(2.72531955636536,4.2,2.39962532458029));
#18183=CARTESIAN_POINT('Ctrl Pts',(2.66797634363184,-3.,2.59347738935741));
#18184=CARTESIAN_POINT('Ctrl Pts',(2.66797634363184,4.2,2.59347738935741));
#18185=CARTESIAN_POINT('Ctrl Pts',(2.59397540849171,-3.,2.7672283971178));
#18186=CARTESIAN_POINT('Ctrl Pts',(2.59397540849171,4.2,2.7672283971178));
#18187=CARTESIAN_POINT('Ctrl Pts',(2.49960870420485,-3.,2.91510580081997));
#18188=CARTESIAN_POINT('Ctrl Pts',(2.49960870420485,4.2,2.91510580081997));
#18189=CARTESIAN_POINT('Ctrl Pts',(2.38189256086504,-3.,3.03403241435618));
#18190=CARTESIAN_POINT('Ctrl Pts',(2.38189256086504,4.2,3.03403241435618));
#18191=CARTESIAN_POINT('Ctrl Pts',(2.23909845280558,-3.,3.12505646843308));
#18192=CARTESIAN_POINT('Ctrl Pts',(2.23909845280558,4.2,3.12505646843308));
#18193=CARTESIAN_POINT('Ctrl Pts',(2.07061055216582,-3.,3.19196918412265));
#18194=CARTESIAN_POINT('Ctrl Pts',(2.07061055216582,4.2,3.19196918412265));
#18195=CARTESIAN_POINT('Ctrl Pts',(1.87681490437036,-3.,3.24001322621211));
#18196=CARTESIAN_POINT('Ctrl Pts',(1.87681490437036,4.2,3.24001322621211));
#18197=CARTESIAN_POINT('Ctrl Pts',(1.65897747541321,-3.,3.27464765209773));
#18198=CARTESIAN_POINT('Ctrl Pts',(1.65897747541321,4.2,3.27464765209773));
#18199=CARTESIAN_POINT('Ctrl Pts',(1.4191255439272,-3.,3.30006519349576));
#18200=CARTESIAN_POINT('Ctrl Pts',(1.4191255439272,4.2,3.30006519349576));
#18201=CARTESIAN_POINT('Ctrl Pts',(1.15993538533448,-3.,3.31897283641381));
#18202=CARTESIAN_POINT('Ctrl Pts',(1.15993538533448,4.2,3.31897283641381));
#18203=CARTESIAN_POINT('Ctrl Pts',(0.884625090385968,-3.,3.33300441174764));
#18204=CARTESIAN_POINT('Ctrl Pts',(0.884625090385968,4.2,3.33300441174764));
#18205=CARTESIAN_POINT('Ctrl Pts',(0.596845720618978,-3.,3.34293392264922));
#18206=CARTESIAN_POINT('Ctrl Pts',(0.596845720618978,4.2,3.34293392264922));
#18207=CARTESIAN_POINT('Ctrl Pts',(0.30057321210183,-3.,3.34897162637417));
#18208=CARTESIAN_POINT('Ctrl Pts',(0.30057321210183,4.2,3.34897162637417));
#18209=CARTESIAN_POINT('Ctrl Pts',(1.66741620510891E-14,-3.,3.35102435732185));
#18210=CARTESIAN_POINT('Ctrl Pts',(1.66741620510891E-14,4.2,3.35102435732185));
#18211=CARTESIAN_POINT('Ctrl Pts',(-0.300573212101791,-3.,3.34897162637426));
#18212=CARTESIAN_POINT('Ctrl Pts',(-0.300573212101791,4.2,3.34897162637426));
#18213=CARTESIAN_POINT('Ctrl Pts',(-0.596845720618908,-3.,3.34293392264938));
#18214=CARTESIAN_POINT('Ctrl Pts',(-0.596845720618908,4.2,3.34293392264938));
#18215=CARTESIAN_POINT('Ctrl Pts',(-0.884625090385886,-3.,3.33300441174785));
#18216=CARTESIAN_POINT('Ctrl Pts',(-0.884625090385886,4.2,3.33300441174785));
#18217=CARTESIAN_POINT('Ctrl Pts',(-1.15993538533442,-3.,3.31897283641402));
#18218=CARTESIAN_POINT('Ctrl Pts',(-1.15993538533442,4.2,3.31897283641402));
#18219=CARTESIAN_POINT('Ctrl Pts',(-1.41912554392716,-3.,3.30006519349591));
#18220=CARTESIAN_POINT('Ctrl Pts',(-1.41912554392716,4.2,3.30006519349591));
#18221=CARTESIAN_POINT('Ctrl Pts',(-1.65897747541319,-3.,3.27464765209779));
#18222=CARTESIAN_POINT('Ctrl Pts',(-1.65897747541319,4.2,3.27464765209779));
#18223=CARTESIAN_POINT('Ctrl Pts',(-1.87681490437034,-3.,3.24001322621208));
#18224=CARTESIAN_POINT('Ctrl Pts',(-1.87681490437034,4.2,3.24001322621208));
#18225=CARTESIAN_POINT('Ctrl Pts',(-2.07061055216576,-3.,3.19196918412254));
#18226=CARTESIAN_POINT('Ctrl Pts',(-2.07061055216576,4.2,3.19196918412254));
#18227=CARTESIAN_POINT('Ctrl Pts',(-2.23909845280547,-3.,3.12505646843295));
#18228=CARTESIAN_POINT('Ctrl Pts',(-2.23909845280547,4.2,3.12505646843295));
#18229=CARTESIAN_POINT('Ctrl Pts',(-2.38189256086493,-3.,3.03403241435609));
#18230=CARTESIAN_POINT('Ctrl Pts',(-2.38189256086493,4.2,3.03403241435609));
#18231=CARTESIAN_POINT('Ctrl Pts',(-2.49960870420481,-3.,2.91510580081997));
#18232=CARTESIAN_POINT('Ctrl Pts',(-2.49960870420481,4.2,2.91510580081997));
#18233=CARTESIAN_POINT('Ctrl Pts',(-2.59397540849182,-3.,2.76722839711793));
#18234=CARTESIAN_POINT('Ctrl Pts',(-2.59397540849182,4.2,2.76722839711793));
#18235=CARTESIAN_POINT('Ctrl Pts',(-2.66797634363209,-3.,2.59347738935767));
#18236=CARTESIAN_POINT('Ctrl Pts',(-2.66797634363209,4.2,2.59347738935767));
#18237=CARTESIAN_POINT('Ctrl Pts',(-2.72531955636566,-3.,2.39962532458057));
#18238=CARTESIAN_POINT('Ctrl Pts',(-2.72531955636566,4.2,2.39962532458057));
#18239=CARTESIAN_POINT('Ctrl Pts',(-2.76985908233936,-3.,2.19251877196088));
#18240=CARTESIAN_POINT('Ctrl Pts',(-2.76985908233936,4.2,2.19251877196088));
#18241=CARTESIAN_POINT('Ctrl Pts',(-2.80505146480344,-3.,1.97856787413951));
#18242=CARTESIAN_POINT('Ctrl Pts',(-2.80505146480344,4.2,1.97856787413951));
#18243=CARTESIAN_POINT('Ctrl Pts',(-2.8333568624899,-3.,1.76209503442131));
#18244=CARTESIAN_POINT('Ctrl Pts',(-2.8333568624899,4.2,1.76209503442131));
#18245=CARTESIAN_POINT('Ctrl Pts',(-2.85578261679294,-3.,1.54401727992238));
#18246=CARTESIAN_POINT('Ctrl Pts',(-2.85578261679294,4.2,1.54401727992238));
#18247=CARTESIAN_POINT('Ctrl Pts',(-2.87284562964987,-3.,1.32371934078708));
#18248=CARTESIAN_POINT('Ctrl Pts',(-2.87284562964987,4.2,1.32371934078708));
#18249=CARTESIAN_POINT('Ctrl Pts',(-2.88537704766869,-3.,1.10060381648384));
#18250=CARTESIAN_POINT('Ctrl Pts',(-2.88537704766869,4.2,1.10060381648384));
#18251=CARTESIAN_POINT('Ctrl Pts',(-2.89547076625573,-3.,0.875890304828914));
#18252=CARTESIAN_POINT('Ctrl Pts',(-2.89547076625573,4.2,0.875890304828914));
#18253=CARTESIAN_POINT('Ctrl Pts',(-2.90717911786707,-3.,0.654020230869684));
#18254=CARTESIAN_POINT('Ctrl Pts',(-2.90717911786707,4.2,0.654020230869684));
#18255=CARTESIAN_POINT('Ctrl Pts',(-2.92780415844476,-3.,0.444963858672577));
#18256=CARTESIAN_POINT('Ctrl Pts',(-2.92780415844476,4.2,0.444963858672577));
#18257=CARTESIAN_POINT('Ctrl Pts',(-2.96639254265869,-3.,0.262319630540737));
#18258=CARTESIAN_POINT('Ctrl Pts',(-2.96639254265869,4.2,0.262319630540737));
#18259=CARTESIAN_POINT('Ctrl Pts',(-3.03063129752067,-3.,0.11901737132707));
#18260=CARTESIAN_POINT('Ctrl Pts',(-3.03063129752067,4.2,0.11901737132707));
#18261=CARTESIAN_POINT('Ctrl Pts',(-3.12452733970658,-3.,0.0241851999813871));
#18262=CARTESIAN_POINT('Ctrl Pts',(-3.12452733970658,4.2,0.0241851999813871));
#18263=CARTESIAN_POINT('Ctrl Pts',(-3.24511001026157,-3.,-0.0214179570895714));
#18264=CARTESIAN_POINT('Ctrl Pts',(-3.24511001026157,4.2,-0.0214179570895714));
#18265=CARTESIAN_POINT('Ctrl Pts',(-3.38164698943802,-3.,-0.0263068037112043));
#18266=CARTESIAN_POINT('Ctrl Pts',(-3.38164698943802,4.2,-0.0263068037112043));
#18267=CARTESIAN_POINT('Ctrl Pts',(-3.52045328348989,-3.,-0.00118366394785932));
#18268=CARTESIAN_POINT('Ctrl Pts',(-3.52045328348989,4.2,-0.00118366394785932));
#18269=CARTESIAN_POINT('Ctrl Pts',(-3.64881642260079,-3.,0.0470540298718583));
#18270=CARTESIAN_POINT('Ctrl Pts',(-3.64881642260079,4.2,0.0470540298718583));
#18271=CARTESIAN_POINT('Ctrl Pts',(-3.75872318140663,-3.,0.120497232333251));
#18272=CARTESIAN_POINT('Ctrl Pts',(-3.75872318140663,4.2,0.120497232333251));
#18273=CARTESIAN_POINT('Ctrl Pts',(-3.84598208672296,-3.,0.224659532804408));
#18274=CARTESIAN_POINT('Ctrl Pts',(-3.84598208672296,4.2,0.224659532804408));
#18275=CARTESIAN_POINT('Ctrl Pts',(-3.9098657241983,-3.,0.364350357241515));
#18276=CARTESIAN_POINT('Ctrl Pts',(-3.9098657241983,4.2,0.364350357241515));
#18277=CARTESIAN_POINT('Ctrl Pts',(-3.9525920016999,-3.,0.538436816836325));
#18278=CARTESIAN_POINT('Ctrl Pts',(-3.9525920016999,4.2,0.538436816836325));
#18279=CARTESIAN_POINT('Ctrl Pts',(-3.97841403016126,-3.,0.741129277895169));
#18280=CARTESIAN_POINT('Ctrl Pts',(-3.97841403016126,4.2,0.741129277895169));
#18281=CARTESIAN_POINT('Ctrl Pts',(-3.99260375067011,-3.,0.964078729991154));
#18282=CARTESIAN_POINT('Ctrl Pts',(-3.99260375067011,4.2,0.964078729991154));
#18283=CARTESIAN_POINT('Ctrl Pts',(-4.00047520099045,-3.,1.1981954227983));
#18284=CARTESIAN_POINT('Ctrl Pts',(-4.00047520099045,4.2,1.1981954227983));
#18285=CARTESIAN_POINT('Ctrl Pts',(-4.00639322616607,-3.,1.43558101932923));
#18286=CARTESIAN_POINT('Ctrl Pts',(-4.00639322616607,4.2,1.43558101932923));
#18287=CARTESIAN_POINT('Ctrl Pts',(-4.01278239926574,-3.,1.67142113207667));
#18288=CARTESIAN_POINT('Ctrl Pts',(-4.01278239926574,4.2,1.67142113207667));
#18289=CARTESIAN_POINT('Ctrl Pts',(-4.02066709528487,-3.,1.90332556813333));
#18290=CARTESIAN_POINT('Ctrl Pts',(-4.02066709528487,4.2,1.90332556813333));
#18291=CARTESIAN_POINT('Ctrl Pts',(-4.0302101444685,-3.,2.130657485557));
#18292=CARTESIAN_POINT('Ctrl Pts',(-4.0302101444685,4.2,2.130657485557));
#18293=CARTESIAN_POINT('Ctrl Pts',(-4.04126813644779,-3.,2.35385258470204));
#18294=CARTESIAN_POINT('Ctrl Pts',(-4.04126813644779,4.2,2.35385258470204));
#18295=CARTESIAN_POINT('Ctrl Pts',(-4.05237622399436,-3.,2.5472071607522));
#18296=CARTESIAN_POINT('Ctrl Pts',(-4.05237622399436,4.2,2.5472071607522));
#18297=CARTESIAN_POINT('Ctrl Pts',(-4.0623773838412,-3.,2.69501052271264));
#18298=CARTESIAN_POINT('Ctrl Pts',(-4.0623773838412,4.2,2.69501052271264));
#18299=CARTESIAN_POINT('Ctrl Pts',(-4.07059539687633,-3.,2.79846879209956));
#18300=CARTESIAN_POINT('Ctrl Pts',(-4.07059539687633,4.2,2.79846879209956));
#18301=CARTESIAN_POINT('Ctrl Pts',(-4.07588877936474,-3.,2.85844305779059));
#18302=CARTESIAN_POINT('Ctrl Pts',(-4.07588877936474,4.2,2.85844305779059));
#18303=CARTESIAN_POINT('Ctrl Pts',(-4.07743349288644,-3.,2.87542908850901));
#18304=CARTESIAN_POINT('Ctrl Pts',(-4.07743349288644,4.2,2.87542908850901));
#18305=CARTESIAN_POINT('Ctrl Pts',(-4.26562934894771,0.281862854502613,
3.79515655425571));
#18306=CARTESIAN_POINT('Ctrl Pts',(-4.28076756904347,0.225365966174025,
3.83396390718086));
#18307=CARTESIAN_POINT('Ctrl Pts',(-4.29636831527147,0.167143869993732,
3.87046814413346));
#18308=CARTESIAN_POINT('Ctrl Pts',(-4.31223161698407,0.107940822442962,
3.90484829258838));
#18309=CARTESIAN_POINT('Ctrl Pts',(-4.20352761804101,0.513629669484374,
3.61216526483895));
#18310=CARTESIAN_POINT('Ctrl Pts',(-4.17637358974273,0.506353769530596,
3.51942422402296));
#18311=CARTESIAN_POINT('Ctrl Pts',(-4.1544631012454,0.503326431198334,3.42375049497737));
#18312=CARTESIAN_POINT('Ctrl Pts',(-4.12235794997748,0.500363612845377,
3.2498423204338));
#18313=CARTESIAN_POINT('Ctrl Pts',(-4.11054280568554,0.500016016851208,
3.17079826924657));
#18314=CARTESIAN_POINT('Ctrl Pts',(-4.10062628985476,0.500000490299028,
3.09201395473891));
#18315=CARTESIAN_POINT('Ctrl Pts',(4.03928538163603,0.5,2.62055334362004));
#18316=CARTESIAN_POINT('Ctrl Pts',(4.04632311223308,0.5,2.71168199850908));
#18317=CARTESIAN_POINT('Ctrl Pts',(4.05429381417606,0.5,2.80274587021811));
#18318=CARTESIAN_POINT('Ctrl Pts',(4.06419081564702,0.5,2.89360843325953));
#18319=CARTESIAN_POINT('Ctrl Pts',(4.04946587537915,0.5,2.61976711921679));
#18320=CARTESIAN_POINT('Ctrl Pts',(4.05599586658109,0.499999012141377,2.71086143217845));
#18321=CARTESIAN_POINT('Ctrl Pts',(4.06337743637285,0.500000842758452,2.8018781295488));
#18322=CARTESIAN_POINT('Ctrl Pts',(4.07248440131376,0.5,2.89270507298886));
#18323=CARTESIAN_POINT('Ctrl Pts',(4.05964274711213,0.498021577508466,2.618981174536));
#18324=CARTESIAN_POINT('Ctrl Pts',(4.06566601882076,0.498217963156433,2.71004109669973));
#18325=CARTESIAN_POINT('Ctrl Pts',(4.07245903442752,0.49843691230792,2.80101058727309));
#18326=CARTESIAN_POINT('Ctrl Pts',(4.0807766690114,0.49868446715054,2.89180185627502));
#18327=CARTESIAN_POINT('Ctrl Pts',(4.06908600086855,0.494206646511993,2.61825188608136));
#18328=CARTESIAN_POINT('Ctrl Pts',(4.07471056556753,0.494770866965848,2.70927438603916));
#18329=CARTESIAN_POINT('Ctrl Pts',(4.08102662411876,0.495395378179633,2.80019313822991));
#18330=CARTESIAN_POINT('Ctrl Pts',(4.08866768906678,0.496116848585951,2.89094234456325));
#18331=CARTESIAN_POINT('',(4.06895185517798,0.494291809244787,2.61828946467431));
#18332=CARTESIAN_POINT('',(4.03928538163603,0.5,2.62055334362004));
#18333=CARTESIAN_POINT('Origin',(4.03928538163603,0.42,2.62055334362004));
#18334=CARTESIAN_POINT('',(4.06419081564702,0.5,2.89360843325953));
#18335=CARTESIAN_POINT('Ctrl Pts',(4.03928538163603,0.5,2.62055334362004));
#18336=CARTESIAN_POINT('Ctrl Pts',(4.04632311223308,0.5,2.71168199850908));
#18337=CARTESIAN_POINT('Ctrl Pts',(4.05429381417606,0.5,2.80274587021811));
#18338=CARTESIAN_POINT('Ctrl Pts',(4.06419081564702,0.5,2.89360843325953));
#18339=CARTESIAN_POINT('',(4.08866768906134,0.496116848587722,2.89094234456384));
#18340=CARTESIAN_POINT('Origin',(4.06419081564702,0.42,2.89360843325953));
#18341=CARTESIAN_POINT('',(4.06920856586713,0.494219105064871,2.62023245236732));
#18342=CARTESIAN_POINT('Ctrl Pts',(4.08866768906678,0.496116848585951,2.89094234456325));
#18343=CARTESIAN_POINT('Ctrl Pts',(4.08108204558666,0.495400611082276,2.80085135200771));
#18344=CARTESIAN_POINT('Ctrl Pts',(4.07480225738019,0.494779931360968,2.71059326414412));
#18345=CARTESIAN_POINT('Ctrl Pts',(4.06920849696627,0.494218933096588,2.62023245770026));
#18346=CARTESIAN_POINT('Ctrl Pts',(4.06894150822957,0.49426616699978,2.61829026217753));
#18347=CARTESIAN_POINT('Ctrl Pts',(4.06903049704884,0.494250393508785,2.61893766197901));
#18348=CARTESIAN_POINT('Ctrl Pts',(4.06911951629768,0.494234706228949,2.61958505872445));
#18349=CARTESIAN_POINT('Ctrl Pts',(4.06920856586577,0.494219105065422,2.62023245236742));
#18350=CARTESIAN_POINT('Ctrl Pts',(4.06419081564702,0.5,2.89360843325953));
#18351=CARTESIAN_POINT('Ctrl Pts',(4.07131106760875,0.5,2.95897816616719));
#18352=CARTESIAN_POINT('Ctrl Pts',(4.07943237959568,0.5,3.02424484221767));
#18353=CARTESIAN_POINT('Ctrl Pts',(4.08915845468123,0.5,3.0892779371144));
#18354=CARTESIAN_POINT('Ctrl Pts',(4.07248440131376,0.5,2.89270507298886));
#18355=CARTESIAN_POINT('Ctrl Pts',(4.07903627312829,0.499999393689843,2.95804917989885));
#18356=CARTESIAN_POINT('Ctrl Pts',(4.08648871622279,0.500000399314335,3.02329507294375));
#18357=CARTESIAN_POINT('Ctrl Pts',(4.09533030979853,0.5,3.08835490052229));
#18358=CARTESIAN_POINT('Ctrl Pts',(4.0807766690114,0.49868446715054,2.89180185627502));
#18359=CARTESIAN_POINT('Ctrl Pts',(4.08676066872451,0.498862566836487,2.95712029773586));
#18360=CARTESIAN_POINT('Ctrl Pts',(4.09354449716726,0.499059402802659,3.02234538076767));
#18361=CARTESIAN_POINT('Ctrl Pts',(4.10150185721175,0.499266489702861,3.0874319099491));
#18362=CARTESIAN_POINT('Ctrl Pts',(4.08866768906678,0.496116848585951,2.89094234456325));
#18363=CARTESIAN_POINT('Ctrl Pts',(4.09416494071875,0.496635899845162,2.9562305246566));
#18364=CARTESIAN_POINT('Ctrl Pts',(4.1003612228726,0.49720813915017,3.02142856695316));
#18365=CARTESIAN_POINT('Ctrl Pts',(4.10750548227104,0.497819390704154,3.08653403313415));
#18366=CARTESIAN_POINT('',(4.08915845468123,0.5,3.0892779371144));
#18367=CARTESIAN_POINT('',(4.10750548294116,0.497819393547925,3.08653403303397));
#18368=CARTESIAN_POINT('Origin',(4.08915845468123,0.42,3.0892779371144));
#18369=CARTESIAN_POINT('Ctrl Pts',(4.10750548227104,0.497819390704154,3.08653403313415));
#18370=CARTESIAN_POINT('Ctrl Pts',(4.1003612228726,0.49720813915017,3.02142856695316));
#18371=CARTESIAN_POINT('Ctrl Pts',(4.09416494071875,0.496635899845162,2.9562305246566));
#18372=CARTESIAN_POINT('Ctrl Pts',(4.08866768906678,0.496116848585951,2.89094234456325));
#18373=CARTESIAN_POINT('Ctrl Pts',(4.06419081564702,0.5,2.89360843325953));
#18374=CARTESIAN_POINT('Ctrl Pts',(4.07131106760875,0.5,2.95897816616719));
#18375=CARTESIAN_POINT('Ctrl Pts',(4.07943237959568,0.5,3.02424484221767));
#18376=CARTESIAN_POINT('Ctrl Pts',(4.08915845468123,0.5,3.0892779371144));
#18377=CARTESIAN_POINT('Ctrl Pts',(4.07450283659624,0.492655764110889,2.63858224625082));
#18378=CARTESIAN_POINT('Ctrl Pts',(4.05896272385424,0.496331141448606,2.56408596426312));
#18379=CARTESIAN_POINT('Ctrl Pts',(4.04957454955023,0.500000000000001,2.48480145080403));
#18380=CARTESIAN_POINT('Ctrl Pts',(4.04448131648779,0.500000000000001,2.40449423379407));
#18381=CARTESIAN_POINT('Ctrl Pts',(4.06410669092888,0.497480565443957,2.63967404822527));
#18382=CARTESIAN_POINT('Ctrl Pts',(4.05053789212333,0.498773941797688,2.56386105153688));
#18383=CARTESIAN_POINT('Ctrl Pts',(4.04494307880602,0.500000000000001,2.48428386223388));
#18384=CARTESIAN_POINT('Ctrl Pts',(4.04448131648779,0.500000000000001,2.40449423379407));
#18385=CARTESIAN_POINT('Ctrl Pts',(4.05265695048639,0.500002014863448,2.64087431669902));
#18386=CARTESIAN_POINT('Ctrl Pts',(4.04188900161745,0.499993283788508,2.56356311273528));
#18387=CARTESIAN_POINT('Ctrl Pts',(4.04031160806179,0.500000000000001,2.48376627366372));
#18388=CARTESIAN_POINT('Ctrl Pts',(4.04448131648779,0.500000000000001,2.40449423379407));
#18389=CARTESIAN_POINT('Ctrl Pts',(4.0412012036484,0.5,2.64207519476898));
#18390=CARTESIAN_POINT('Ctrl Pts',(4.03324251291048,0.5,2.56326450267563));
#18391=CARTESIAN_POINT('Ctrl Pts',(4.03568013731757,0.500000000000001,2.48324868509357));
#18392=CARTESIAN_POINT('Ctrl Pts',(4.04448131648779,0.500000000000001,2.40449423379407));
#18393=CARTESIAN_POINT('',(4.04442943268642,0.499941163643867,2.40450168102723));
#18394=CARTESIAN_POINT('Ctrl Pts',(4.06886801794898,0.49433551594449,2.61829782579792));
#18395=CARTESIAN_POINT('Ctrl Pts',(4.06465789083201,0.495298098708667,2.59562064419044));
#18396=CARTESIAN_POINT('Ctrl Pts',(4.0608935194358,0.496315176554883,2.57122223594089));
#18397=CARTESIAN_POINT('Ctrl Pts',(4.05758292507581,0.497209522471247,2.54587396190639));
#18398=CARTESIAN_POINT('Ctrl Pts',(4.05456867152398,0.498023812916352,2.52279468467315));
#18399=CARTESIAN_POINT('Ctrl Pts',(4.05193046449298,0.498735979011545,2.49892750607437));
#18400=CARTESIAN_POINT('Ctrl Pts',(4.0497085040971,0.499233961791349,2.47484691613384));
#18401=CARTESIAN_POINT('Ctrl Pts',(4.04754737437031,0.499718311283297,2.45142558114697));
#18402=CARTESIAN_POINT('Ctrl Pts',(4.04577933129341,0.499999944019269,2.42780226396996));
#18403=CARTESIAN_POINT('Ctrl Pts',(4.044481720465,0.499999999991593,2.40450148814583));
#18404=CARTESIAN_POINT('Ctrl Pts',(4.04447960468408,0.500000000000001,2.40450955203947));
#18405=CARTESIAN_POINT('Ctrl Pts',(4.0364798534531,0.500000000000001,2.47609955036283));
#18406=CARTESIAN_POINT('Ctrl Pts',(4.03373870432118,0.5,2.5487317193285));
#18407=CARTESIAN_POINT('Ctrl Pts',(4.03928538163603,0.5,2.62055334362004));
#18408=CARTESIAN_POINT('Ctrl Pts',(4.1,0.5,3.15505167992283));
#18409=CARTESIAN_POINT('Ctrl Pts',(4.12354928830202,0.5,3.3096462519264));
#18410=CARTESIAN_POINT('Ctrl Pts',(4.15597088871579,0.501106120178651,3.46379338521867));
#18411=CARTESIAN_POINT('Ctrl Pts',(4.20302510049204,0.513494829718804,3.61060092780471));
#18412=CARTESIAN_POINT('Ctrl Pts',(4.20327611767679,0.513562280164884,3.61138321913356));
#18413=CARTESIAN_POINT('Ctrl Pts',(4.20352761804101,0.513629669484372,3.61216526483892));
#18414=CARTESIAN_POINT('Ctrl Pts',(4.10514574956508,0.5,3.15411106159347));
#18415=CARTESIAN_POINT('Ctrl Pts',(4.12748779335588,0.500302630511343,3.3086923919502));
#18416=CARTESIAN_POINT('Ctrl Pts',(4.15822497958996,0.501690302643301,3.46288253392766));
#18417=CARTESIAN_POINT('Ctrl Pts',(4.20304883308115,0.513501203389107,3.61059108834772));
#18418=CARTESIAN_POINT('Ctrl Pts',(4.20328800103192,0.513565464300295,3.61137830395557));
#18419=CARTESIAN_POINT('Ctrl Pts',(4.20352761804101,0.513629669484372,3.61216526483892));
#18420=CARTESIAN_POINT('Ctrl Pts',(4.11029137237376,0.499485295444531,3.15317046643458));
#18421=CARTESIAN_POINT('Ctrl Pts',(4.13145665971031,0.500324828934127,3.30773853156512));
#18422=CARTESIAN_POINT('Ctrl Pts',(4.1604840495311,0.502266600047225,3.46197168157039));
#18423=CARTESIAN_POINT('Ctrl Pts',(4.20307255308428,0.513507583754598,3.61058124889467));
#18424=CARTESIAN_POINT('Ctrl Pts',(4.20329988438705,0.513568648435705,3.61137338877759));
#18425=CARTESIAN_POINT('Ctrl Pts',(4.20352761804101,0.513629669484372,3.61216526483892));
#18426=CARTESIAN_POINT('Ctrl Pts',(4.11533843497839,0.498465732400005,3.15224788760805));
#18427=CARTESIAN_POINT('Ctrl Pts',(4.13542434682827,0.500061728589708,3.30679480627255));
#18428=CARTESIAN_POINT('Ctrl Pts',(4.16275021805235,0.502834940834963,3.46106041128606));
#18429=CARTESIAN_POINT('Ctrl Pts',(4.20309625252131,0.513513971085243,3.61057141101541));
#18430=CARTESIAN_POINT('Ctrl Pts',(4.20331176774218,0.513571832571116,3.6113684735996));
#18431=CARTESIAN_POINT('Ctrl Pts',(4.20352761804101,0.513629669484372,3.61216526483892));
#18432=CARTESIAN_POINT('',(4.1,0.5,3.15505167992283));
#18433=CARTESIAN_POINT('Ctrl Pts',(4.1,0.5,3.15505167992283));
#18434=CARTESIAN_POINT('Ctrl Pts',(4.12354928830202,0.5,3.3096462519264));
#18435=CARTESIAN_POINT('Ctrl Pts',(4.15597088871579,0.501106120178651,3.46379338521867));
#18436=CARTESIAN_POINT('Ctrl Pts',(4.20302510049204,0.513494829718804,3.61060092780471));
#18437=CARTESIAN_POINT('Ctrl Pts',(4.20327611767679,0.513562280164884,3.61138321913356));
#18438=CARTESIAN_POINT('Ctrl Pts',(4.20352761804101,0.513629669484372,3.61216526483892));
#18439=CARTESIAN_POINT('',(4.20223747325117,0.513287047238827,3.60738446017534));
#18440=CARTESIAN_POINT('Ctrl Pts',(4.20352761804101,0.513629669484372,3.61216526483892));
#18441=CARTESIAN_POINT('Ctrl Pts',(4.20331176774218,0.513571832571116,3.6113684735996));
#18442=CARTESIAN_POINT('Ctrl Pts',(4.20309625252131,0.513513971085243,3.61057141101541));
#18443=CARTESIAN_POINT('Ctrl Pts',(4.20266625878817,0.513400157766436,3.60897797578032));
#18444=CARTESIAN_POINT('Ctrl Pts',(4.20245168277568,0.513343490433672,3.60818129720179));
#18445=CARTESIAN_POINT('Ctrl Pts',(4.20223747325117,0.513287047238827,3.60738446017534));
#18446=CARTESIAN_POINT('',(4.11533843497839,0.498465732400005,3.15224788760805));
#18447=CARTESIAN_POINT('Ctrl Pts',(4.20223747325117,0.513287047238827,3.60738446017534));
#18448=CARTESIAN_POINT('Ctrl Pts',(4.16245770855631,0.502805267707013,3.45940789617989));
#18449=CARTESIAN_POINT('Ctrl Pts',(4.13531676578111,0.500053180362341,3.30596704602595));
#18450=CARTESIAN_POINT('Ctrl Pts',(4.11533843497839,0.498465732400005,3.15224788760805));
#18451=CARTESIAN_POINT('Origin',(4.1,0.42,3.15505167992283));
#18452=CARTESIAN_POINT('Ctrl Pts',(4.08915845468123,0.5,3.0892779371144));
#18453=CARTESIAN_POINT('Ctrl Pts',(4.09244523897257,0.5,3.11125491681526));
#18454=CARTESIAN_POINT('Ctrl Pts',(4.09600424357276,0.5,3.13319248235467));
#18455=CARTESIAN_POINT('Ctrl Pts',(4.1,0.5,3.15505167992283));
#18456=CARTESIAN_POINT('Ctrl Pts',(4.09533030979853,0.5,3.08835490052229));
#18457=CARTESIAN_POINT('Ctrl Pts',(4.09831694095011,0.499999865724806,3.11032259202407));
#18458=CARTESIAN_POINT('Ctrl Pts',(4.10154259105465,0.500000103565783,3.13225323052938));
#18459=CARTESIAN_POINT('Ctrl Pts',(4.10514574956508,0.5,3.15411106159347));
#18460=CARTESIAN_POINT('Ctrl Pts',(4.10150185721175,0.499266489702861,3.0874319099491));
#18461=CARTESIAN_POINT('Ctrl Pts',(4.10418841876551,0.499336125654538,3.10939030384142));
#18462=CARTESIAN_POINT('Ctrl Pts',(4.10708075806979,0.4994092082085,3.13131400963607));
#18463=CARTESIAN_POINT('Ctrl Pts',(4.11029137237376,0.499485295444531,3.15317046643458));
#18464=CARTESIAN_POINT('Ctrl Pts',(4.10750548227104,0.497819390704154,3.08653403313415));
#18465=CARTESIAN_POINT('Ctrl Pts',(4.10991596810902,0.49802493283953,3.10848101609958));
#18466=CARTESIAN_POINT('Ctrl Pts',(4.11249834874657,0.498240063441667,3.13039542807567));
#18467=CARTESIAN_POINT('Ctrl Pts',(4.1153384349784,0.498465732400005,3.15224788760805));
#18468=CARTESIAN_POINT('Ctrl Pts',(4.11533084388102,0.498427288961305,3.15224922644314));
#18469=CARTESIAN_POINT('Ctrl Pts',(4.11249458022437,0.498223938268274,3.13039599596135));
#18470=CARTESIAN_POINT('Ctrl Pts',(4.10991588274464,0.498024571772185,3.10848102746594));
#18471=CARTESIAN_POINT('Ctrl Pts',(4.10750548495196,0.497819402079132,3.08653403273337));
#18472=CARTESIAN_POINT('Ctrl Pts',(4.08915845468123,0.5,3.0892779371144));
#18473=CARTESIAN_POINT('Ctrl Pts',(4.09244523897257,0.5,3.11125491681526));
#18474=CARTESIAN_POINT('Ctrl Pts',(4.09600424357276,0.5,3.13319248235467));
#18475=CARTESIAN_POINT('Ctrl Pts',(4.1,0.5,3.15505167992283));
#18476=CARTESIAN_POINT('Ctrl Pts',(4.08866768906678,0.496116848585951,2.89094234456324));
#18477=CARTESIAN_POINT('Ctrl Pts',(4.08065486646877,0.49551208126272,2.80011197287451));
#18478=CARTESIAN_POINT('Ctrl Pts',(4.07407036444164,0.495008985691453,2.70919313424665));
#18479=CARTESIAN_POINT('Ctrl Pts',(4.06822070400199,0.494561147702366,2.61828756807606));
#18480=CARTESIAN_POINT('Ctrl Pts',(4.10320659093045,0.491413943800592,2.89015338698478));
#18481=CARTESIAN_POINT('Ctrl Pts',(4.09590560906221,0.490023602254911,2.79936307019029));
#18482=CARTESIAN_POINT('Ctrl Pts',(4.08980775472146,0.488878406811895,2.7084928654444));
#18483=CARTESIAN_POINT('Ctrl Pts',(4.08435563880312,0.487840362968629,2.61762358805541));
#18484=CARTESIAN_POINT('Ctrl Pts',(4.11909837273532,0.491006921387143,2.88921565674865));
#18485=CARTESIAN_POINT('Ctrl Pts',(4.11282012019298,0.489318592483934,2.79845239738339));
#18486=CARTESIAN_POINT('Ctrl Pts',(4.10749604313151,0.487903857194521,2.7076259216545));
#18487=CARTESIAN_POINT('Ctrl Pts',(4.10271622937717,0.486617339304039,2.61678827445837));
#18488=CARTESIAN_POINT('Ctrl Pts',(4.13385008609474,0.494959631068776,2.88827625586696));
#18489=CARTESIAN_POINT('Ctrl Pts',(4.12845897149287,0.493515086264903,2.79753965428624));
#18490=CARTESIAN_POINT('Ctrl Pts',(4.12379844489011,0.492266301925388,2.70675672533888));
#18491=CARTESIAN_POINT('Ctrl Pts',(4.11959214370927,0.491139226920861,2.61595042854269));
#18492=CARTESIAN_POINT('',(4.1102894955425,0.490554628217515,2.74850282871571));
#18493=CARTESIAN_POINT('Ctrl Pts',(4.10983817729973,0.490298889823543,2.74868144584745));
#18494=CARTESIAN_POINT('Ctrl Pts',(4.09912059002179,0.489547803684328,2.73380263969482));
#18495=CARTESIAN_POINT('Ctrl Pts',(4.09060288993725,0.490523597563226,2.70804325577999));
#18496=CARTESIAN_POINT('Ctrl Pts',(4.07916964200075,0.492005281603662,2.66917053317873));
#18497=CARTESIAN_POINT('Ctrl Pts',(4.07363486591143,0.493180967854886,2.64394223670214));
#18498=CARTESIAN_POINT('Ctrl Pts',(4.06920856586713,0.494219105064871,2.62023245236732));
#18499=CARTESIAN_POINT('Origin',(4.11314456248654,0.572233697171902,2.88827625586697));
#18500=CARTESIAN_POINT('Ctrl Pts',(4.12725971987735,0.493193747719603,2.77093882623153));
#18501=CARTESIAN_POINT('Ctrl Pts',(4.12455800459528,0.492469895869088,2.76708747448196));
#18502=CARTESIAN_POINT('Ctrl Pts',(4.1218042657884,0.491865483418447,2.76326519725518));
#18503=CARTESIAN_POINT('Ctrl Pts',(4.11625238064331,0.490914087391762,2.75567430292574));
#18504=CARTESIAN_POINT('Ctrl Pts',(4.11346892427127,0.490565796408723,2.75192428752783));
#18505=CARTESIAN_POINT('Ctrl Pts',(4.11066809033619,0.490343257580657,2.74816669957651));
#18506=CARTESIAN_POINT('Ctrl Pts',(4.10750548227104,0.497819390704154,3.08653403313415));
#18507=CARTESIAN_POINT('Ctrl Pts',(4.09988751844767,0.497321971238036,3.02148952956988));
#18508=CARTESIAN_POINT('Ctrl Pts',(4.09333086416513,0.496883068938475,2.95626908269239));
#18509=CARTESIAN_POINT('Ctrl Pts',(4.08753393606525,0.496492976538145,2.89100371845852));
#18510=CARTESIAN_POINT('Ctrl Pts',(4.12030577414111,0.494771961793561,3.08569517253432));
#18511=CARTESIAN_POINT('Ctrl Pts',(4.11358761799295,0.493524694122167,3.02063134445983));
#18512=CARTESIAN_POINT('Ctrl Pts',(4.1076623367844,0.492431642898789,2.9554374626284));
#18513=CARTESIAN_POINT('Ctrl Pts',(4.10237819873081,0.491444738231125,2.89020211564854));
#18514=CARTESIAN_POINT('Ctrl Pts',(4.13385584109311,0.494961173115941,3.08474311994105));
#18515=CARTESIAN_POINT('Ctrl Pts',(4.12828398728823,0.493463687530671,3.01963734956761));
#18516=CARTESIAN_POINT('Ctrl Pts',(4.12324167296667,0.492121940958461,2.95445550879435));
#18517=CARTESIAN_POINT('Ctrl Pts',(4.11871398375975,0.490903924671562,2.88924013494544));
#18518=CARTESIAN_POINT('Ctrl Pts',(4.14655803346906,0.498364715305182,3.0837901291539));
#18519=CARTESIAN_POINT('Ctrl Pts',(4.14199767141828,0.497142769976483,3.01864202972875));
#18520=CARTESIAN_POINT('Ctrl Pts',(4.13772368979234,0.495997560051348,2.95347198278946));
#18521=CARTESIAN_POINT('Ctrl Pts',(4.13385008609474,0.494959631068777,2.88827625586697));
#18522=CARTESIAN_POINT('Origin',(4.12585250986086,0.575638781408308,3.0837901291539));
#18523=CARTESIAN_POINT('Ctrl Pts',(4.20352761804101,0.513629669484372,3.61216526483892));
#18524=CARTESIAN_POINT('Ctrl Pts',(4.2034515520887,0.51360928767388,3.61188709994706));
#18525=CARTESIAN_POINT('Ctrl Pts',(4.20337579441033,0.513588620909437,3.61160915407523));
#18526=CARTESIAN_POINT('Ctrl Pts',(4.15654326855526,0.501204320694855,3.43986804670352));
#18527=CARTESIAN_POINT('Ctrl Pts',(4.12742700794855,0.499257234215814,3.26327059408423));
#18528=CARTESIAN_POINT('Ctrl Pts',(4.10655417222842,0.498052118158934,3.0865962596308));
#18529=CARTESIAN_POINT('Ctrl Pts',(4.20352761804101,0.513629669484372,3.61216526483892));
#18530=CARTESIAN_POINT('Ctrl Pts',(4.20346328242755,0.5136124308087,3.61188634858972));
#18531=CARTESIAN_POINT('Ctrl Pts',(4.20339351891518,0.513598371022242,3.61160471600277));
#18532=CARTESIAN_POINT('Ctrl Pts',(4.16301739273852,0.502680404850424,3.4388303755424));
#18533=CARTESIAN_POINT('Ctrl Pts',(4.13810208850384,0.497947580543976,3.26236737839722));
#18534=CARTESIAN_POINT('Ctrl Pts',(4.11963294253909,0.494765631312812,3.08574238943294));
#18535=CARTESIAN_POINT('Ctrl Pts',(4.20352761804101,0.513629669484372,3.61216526483892));
#18536=CARTESIAN_POINT('Ctrl Pts',(4.20347237327524,0.513614866693999,3.61188267429505));
#18537=CARTESIAN_POINT('Ctrl Pts',(4.20341613842376,0.513599798610958,3.61160296503507));
#18538=CARTESIAN_POINT('Ctrl Pts',(4.16924973697742,0.504444938935139,3.43771198364712));
#18539=CARTESIAN_POINT('Ctrl Pts',(4.14873646433035,0.498948424095233,3.26128633907584));
#18540=CARTESIAN_POINT('Ctrl Pts',(4.13354070272714,0.494876732045277,3.08476676341538));
#18541=CARTESIAN_POINT('Ctrl Pts',(4.20352761804101,0.513629669484372,3.61216526483892));
#18542=CARTESIAN_POINT('Ctrl Pts',(4.20348225943688,0.513617515683026,3.61188189200445));
#18543=CARTESIAN_POINT('Ctrl Pts',(4.20343686017451,0.513605350987338,3.61159855052174));
#18544=CARTESIAN_POINT('Ctrl Pts',(4.17554861335302,0.506132717773207,3.43668170480236));
#18545=CARTESIAN_POINT('Ctrl Pts',(4.15891388414094,0.501675455514513,3.26030247161513));
#18546=CARTESIAN_POINT('Ctrl Pts',(4.14655803346906,0.498364715305183,3.0837901291539));
#18547=CARTESIAN_POINT('Ctrl Pts',(4.06730463307991,0.5,2.7548988716696));
#18548=CARTESIAN_POINT('Ctrl Pts',(4.04477623135907,0.5,2.46323477342689));
#18549=CARTESIAN_POINT('Ctrl Pts',(4.03124587888692,0.500000000000004,2.17098509479316));
#18550=CARTESIAN_POINT('Ctrl Pts',(4.02013482858588,0.5,1.87705481005079));
#18551=CARTESIAN_POINT('Ctrl Pts',(4.02006773773253,0.5,1.87522368040185));
#18552=CARTESIAN_POINT('Ctrl Pts',(4.02,0.5,1.87339241925346));
#18553=CARTESIAN_POINT('Ctrl Pts',(4.0701214409961,0.488945949397786,2.75298513275217));
#18554=CARTESIAN_POINT('Ctrl Pts',(4.0521727324952,0.495960044053856,2.46215351379707));
#18555=CARTESIAN_POINT('Ctrl Pts',(4.03379752250834,0.500113514316493,2.17064344747657));
#18556=CARTESIAN_POINT('Ctrl Pts',(4.02016777946955,0.49999925948703,1.8770506998427));
#18557=CARTESIAN_POINT('Ctrl Pts',(4.02008397514388,0.5,1.87522162637816));
#18558=CARTESIAN_POINT('Ctrl Pts',(4.02,0.5,1.87339241925346));
#18559=CARTESIAN_POINT('Ctrl Pts',(4.07538773587724,0.478557974340581,2.7508822733927));
#18560=CARTESIAN_POINT('Ctrl Pts',(4.05924753225934,0.493164525555191,2.46115599049795));
#18561=CARTESIAN_POINT('Ctrl Pts',(4.03637623393824,0.500137583027881,2.17029238050623));
#18562=CARTESIAN_POINT('Ctrl Pts',(4.02020061161559,0.499998948815406,1.87704663109656));
#18563=CARTESIAN_POINT('Ctrl Pts',(4.02010021255523,0.5,1.87521957235447));
#18564=CARTESIAN_POINT('Ctrl Pts',(4.02,0.5,1.87339241925346));
#18565=CARTESIAN_POINT('Ctrl Pts',(4.08262506058196,0.469786517311005,2.74878220268511));
#18566=CARTESIAN_POINT('Ctrl Pts',(4.0658320892877,0.491020613169402,2.46015855202445));
#18567=CARTESIAN_POINT('Ctrl Pts',(4.03900592459406,0.500139057369812,2.16994131329339));
#18568=CARTESIAN_POINT('Ctrl Pts',(4.02023321948065,0.49999877382774,1.8770425623582));
#18569=CARTESIAN_POINT('Ctrl Pts',(4.02011644996657,0.5,1.87521751833078));
#18570=CARTESIAN_POINT('Ctrl Pts',(4.02,0.5,1.87339241925346));
#18571=CARTESIAN_POINT('',(4.07425885705739,0.479232380498994,2.68379303474969));
#18572=CARTESIAN_POINT('Ctrl Pts',(4.04448172046659,0.499999999988976,2.40450148817435));
#18573=CARTESIAN_POINT('Ctrl Pts',(4.04463591392868,0.499999991267764,2.40727029004885));
#18574=CARTESIAN_POINT('Ctrl Pts',(4.04479651104661,0.499994808468355,2.4100383627539));
#18575=CARTESIAN_POINT('Ctrl Pts',(4.04496328520179,0.499984248258457,2.41280641893295));
#18576=CARTESIAN_POINT('Ctrl Pts',(4.04516949057082,0.499971191247455,2.41622893991844));
#18577=CARTESIAN_POINT('Ctrl Pts',(4.04538506477277,0.499949917237401,2.41965021876981));
#18578=CARTESIAN_POINT('Ctrl Pts',(4.04560958710345,0.499920089612813,2.42307148910707));
#18579=CARTESIAN_POINT('Ctrl Pts',(4.046168184163,0.49984588040904,2.43158338876807));
#18580=CARTESIAN_POINT('Ctrl Pts',(4.04678126083676,0.499718763421518,2.44008296252431));
#18581=CARTESIAN_POINT('Ctrl Pts',(4.04744268468172,0.499534811332572,2.44858609368312));
#18582=CARTESIAN_POINT('Ctrl Pts',(4.04916608154842,0.4990555083015,2.47074173519485));
#18583=CARTESIAN_POINT('Ctrl Pts',(4.0512029869943,0.49818690046067,2.49278507911436));
#18584=CARTESIAN_POINT('Ctrl Pts',(4.05345548579231,0.496916182347658,2.51477945136454));
#18585=CARTESIAN_POINT('Ctrl Pts',(4.05591683934511,0.495527641521432,2.53881317174981));
#18586=CARTESIAN_POINT('Ctrl Pts',(4.05863587671313,0.493660110871332,2.56278860465434));
#18587=CARTESIAN_POINT('Ctrl Pts',(4.06154550645518,0.49131004765369,2.58679034176726));
#18588=CARTESIAN_POINT('Ctrl Pts',(4.06260468059428,0.490454568982503,2.59552754254441));
#18589=CARTESIAN_POINT('Ctrl Pts',(4.06368963170895,0.489535178864469,2.60426823220296));
#18590=CARTESIAN_POINT('Ctrl Pts',(4.06479877481585,0.488551656167653,2.61301647477758));
#18591=CARTESIAN_POINT('Ctrl Pts',(4.06741316103876,0.486233372645465,2.63363715457938));
#18592=CARTESIAN_POINT('Ctrl Pts',(4.07015511481845,0.483565049488091,2.65424997138026));
#18593=CARTESIAN_POINT('Ctrl Pts',(4.07300374745784,0.480567084366157,2.67479487671516));
#18594=CARTESIAN_POINT('Ctrl Pts',(4.0734198337187,0.480129185817727,2.67779577360951));
#18595=CARTESIAN_POINT('Ctrl Pts',(4.07383822268607,0.479684259277039,2.68079522108865));
#18596=CARTESIAN_POINT('Ctrl Pts',(4.07425885705739,0.479232380498994,2.68379303474969));
#18597=CARTESIAN_POINT('',(4.0809602708998,0.471805843027818,2.72818635208988));
#18598=CARTESIAN_POINT('Ctrl Pts',(4.07431256837795,0.479317097635081,2.68379826229727));
#18599=CARTESIAN_POINT('Ctrl Pts',(4.07535643858548,0.478197393643414,2.69122711204079));
#18600=CARTESIAN_POINT('Ctrl Pts',(4.0764134383116,0.477033123389242,2.69864815707777));
#18601=CARTESIAN_POINT('Ctrl Pts',(4.07855234656971,0.474619335589603,2.71346580990626));
#18602=CARTESIAN_POINT('Ctrl Pts',(4.07963448015113,0.473369601956344,2.7208641126329));
#18603=CARTESIAN_POINT('Ctrl Pts',(4.08072980562297,0.472078321008102,2.72825206195681));
#18604=CARTESIAN_POINT('',(4.02,0.5,1.87339241925342));
#18605=CARTESIAN_POINT('Ctrl Pts',(4.0809602708998,0.471805843027818,2.72818635208988));
#18606=CARTESIAN_POINT('Ctrl Pts',(4.07764839286774,0.475702951350386,2.67263460081295));
#18607=CARTESIAN_POINT('Ctrl Pts',(4.07398527921688,0.479249586578106,2.61702556232049));
#18608=CARTESIAN_POINT('Ctrl Pts',(4.07009274281801,0.482375613159057,2.56136441565828));
#18609=CARTESIAN_POINT('Ctrl Pts',(4.06612731105444,0.485560180707732,2.50466090505392));
#18610=CARTESIAN_POINT('Ctrl Pts',(4.06192505627188,0.488307767931295,2.44790331635054));
#18611=CARTESIAN_POINT('Ctrl Pts',(4.05763254837964,0.490595972282094,2.39109712504011));
#18612=CARTESIAN_POINT('Ctrl Pts',(4.05327949071071,0.492916453862411,2.33348963008985));
#18613=CARTESIAN_POINT('Ctrl Pts',(4.04883495697235,0.49476468329804,2.27583215169267));
#18614=CARTESIAN_POINT('Ctrl Pts',(4.0444496090073,0.496172282487727,2.21813040033497));
#18615=CARTESIAN_POINT('Ctrl Pts',(4.03986024699307,0.497645365651001,2.15774426269066));
#18616=CARTESIAN_POINT('Ctrl Pts',(4.03533701131399,0.498636468850484,2.0973096369561));
#18617=CARTESIAN_POINT('Ctrl Pts',(4.03102904348286,0.499236104143585,2.03683306825523));
#18618=CARTESIAN_POINT('Ctrl Pts',(4.02728039024729,0.49975788723709,1.98420832874381));
#18619=CARTESIAN_POINT('Ctrl Pts',(4.02369449212959,0.499984720705903,1.93155183038186));
#18620=CARTESIAN_POINT('Ctrl Pts',(4.02034716371852,0.499999246729907,1.87886788564175));
#18621=CARTESIAN_POINT('Ctrl Pts',(4.02023120593227,0.499999749938848,1.87704281416613));
#18622=CARTESIAN_POINT('Ctrl Pts',(4.02011544505978,0.5,1.87521764545094));
#18623=CARTESIAN_POINT('Ctrl Pts',(4.02,0.5,1.87339241925346));
#18624=CARTESIAN_POINT('Ctrl Pts',(4.02,0.5,1.87339241925346));
#18625=CARTESIAN_POINT('Ctrl Pts',(4.02002404870585,0.5,1.87404256591536));
#18626=CARTESIAN_POINT('Ctrl Pts',(4.020048124588,0.499999999225747,1.87469286273721));
#18627=CARTESIAN_POINT('Ctrl Pts',(4.02007222763371,0.49999999809316,1.87534330899108));
#18628=CARTESIAN_POINT('Ctrl Pts',(4.02009633067943,0.499999996960572,1.87599375524495));
#18629=CARTESIAN_POINT('Ctrl Pts',(4.0201204602048,0.499999996385127,1.87664435102068));
#18630=CARTESIAN_POINT('Ctrl Pts',(4.02014462258731,0.4999999976786,1.87729509477937));
#18631=CARTESIAN_POINT('Ctrl Pts',(4.0201643119008,0.499999998732619,1.8778253693857));
#18632=CARTESIAN_POINT('Ctrl Pts',(4.02018411754459,0.499999999632519,1.87835571847931));
#18633=CARTESIAN_POINT('Ctrl Pts',(4.02020412741357,0.499999999958576,1.87888616583914));
#18634=CARTESIAN_POINT('Ctrl Pts',(4.0202332290698,0.50000000043278,1.87965762999687));
#18635=CARTESIAN_POINT('Ctrl Pts',(4.02026240571076,0.5,1.88042926065977));
#18636=CARTESIAN_POINT('Ctrl Pts',(4.02029161790995,0.5,1.88120111622291));
#18637=CARTESIAN_POINT('Ctrl Pts',(4.02039021406171,0.5,1.88380626031799));
#18638=CARTESIAN_POINT('Ctrl Pts',(4.02048909882791,0.5,1.88641377586908));
#18639=CARTESIAN_POINT('Ctrl Pts',(4.02058827628576,0.5,1.88902361917288));
#18640=CARTESIAN_POINT('Ctrl Pts',(4.02078663120146,0.5,1.89424330578047));
#18641=CARTESIAN_POINT('Ctrl Pts',(4.02098611903685,0.500000001963655,1.89947230693178));
#18642=CARTESIAN_POINT('Ctrl Pts',(4.02118710576848,0.499999999141363,1.90471020328437));
#18643=CARTESIAN_POINT('Ctrl Pts',(4.02348494037357,0.499999966874759,1.96459385530179));
#18644=CARTESIAN_POINT('Ctrl Pts',(4.02595913585852,0.499998572838881,2.02564279695681));
#18645=CARTESIAN_POINT('Ctrl Pts',(4.02865623488046,0.499980627301766,2.08729249963769));
#18646=CARTESIAN_POINT('Ctrl Pts',(4.03110154710007,0.499964357064434,2.143186914368));
#18647=CARTESIAN_POINT('Ctrl Pts',(4.03372928221755,0.499932544589326,2.19957498349665));
#18648=CARTESIAN_POINT('Ctrl Pts',(4.03653956308091,0.499898182578179,2.25604062027684));
#18649=CARTESIAN_POINT('Ctrl Pts',(4.03900413643723,0.499868047619696,2.30556012054119));
#18650=CARTESIAN_POINT('Ctrl Pts',(4.04160722520186,0.499835636299494,2.35513929660828));
#18651=CARTESIAN_POINT('Ctrl Pts',(4.04434137221638,0.499842074417939,2.40450200575315));
#18652=CARTESIAN_POINT('Ctrl Pts',(4.22955939312853,0.10102905344224,11.7707450664009));
#18653=CARTESIAN_POINT('Ctrl Pts',(4.21654931683645,0.207401903813072,11.7841012806179));
#18654=CARTESIAN_POINT('Ctrl Pts',(4.20605403928643,0.31441823415144,11.7948904430433));
#18655=CARTESIAN_POINT('Ctrl Pts',(4.19893756066089,0.421920994121332,11.8021991336745));
#18656=CARTESIAN_POINT('Ctrl Pts',(4.24536267111276,0.104989885152963,11.7545212387652));
#18657=CARTESIAN_POINT('Ctrl Pts',(4.23114949583097,0.210504261951862,11.7691939848541));
#18658=CARTESIAN_POINT('Ctrl Pts',(4.21935602279,0.316778326210449,11.7811764288609));
#18659=CARTESIAN_POINT('Ctrl Pts',(4.21085539742978,0.423544704078567,11.7899594459956));
#18660=CARTESIAN_POINT('Ctrl Pts',(4.28598710678366,0.111856705035166,11.7392780563968));
#18661=CARTESIAN_POINT('Ctrl Pts',(4.2674307302526,0.215927568411162,11.7537105073236));
#18662=CARTESIAN_POINT('Ctrl Pts',(4.25155716799185,0.320887527746463,11.7661024302623));
#18663=CARTESIAN_POINT('Ctrl Pts',(4.23883095697931,0.42637816873375,11.77559001791));
#18664=CARTESIAN_POINT('Ctrl Pts',(4.32514653100426,0.114600833742749,11.7555174901866));
#18665=CARTESIAN_POINT('Ctrl Pts',(4.30459583266175,0.218704714738053,11.7646869062335));
#18666=CARTESIAN_POINT('Ctrl Pts',(4.28594490659705,0.323351812836807,11.7725098097745));
#18667=CARTESIAN_POINT('Ctrl Pts',(4.26959555894274,0.428231125093901,11.7783349626985));
#18668=CARTESIAN_POINT('Ctrl Pts',(4.33821035750186,0.1147842101985,11.7667789364918));
#18669=CARTESIAN_POINT('Ctrl Pts',(4.31798914414459,0.219217033838757,11.7734397365619));
#18670=CARTESIAN_POINT('Ctrl Pts',(4.29900887782759,0.323961874179476,11.7788360517208));
#18671=CARTESIAN_POINT('Ctrl Pts',(4.28176747596058,0.428754931584936,11.7824947042679));
#18672=CARTESIAN_POINT('',(4.28177589321514,0.428644841197042,11.7824875832413));
#18673=CARTESIAN_POINT('',(4.19894501008283,0.421808480676737,11.8021914830441));
#18674=CARTESIAN_POINT('Origin',(4.25626225479035,0.421808480673776,11.858001280205));
#18675=CARTESIAN_POINT('',(4.2295457775513,0.101140384725978,11.770759044231));
#18676=CARTESIAN_POINT('Ctrl Pts',(4.19894501008295,0.421808480673776,11.802191483044));
#18677=CARTESIAN_POINT('Ctrl Pts',(4.20605887902608,0.314381068971518,11.7948854653236));
#18678=CARTESIAN_POINT('Ctrl Pts',(4.21654653248185,0.2074394630476,11.7841041492711));
#18679=CARTESIAN_POINT('Ctrl Pts',(4.2295457775513,0.101140384725978,11.770759044231));
#18680=CARTESIAN_POINT('',(4.33817886049863,0.114893365388572,11.7667770031876));
#18681=CARTESIAN_POINT('Origin',(4.28685203791006,0.101140384725978,11.8265801202122));
#18682=CARTESIAN_POINT('Ctrl Pts',(4.33817886049861,0.114893365388635,11.7667770031876));
#18683=CARTESIAN_POINT('Ctrl Pts',(4.3293833989095,0.16031902928837,11.7696747648638));
#18684=CARTESIAN_POINT('Ctrl Pts',(4.32083110204483,0.205805953395781,11.7723064625421));
#18685=CARTESIAN_POINT('Ctrl Pts',(4.31254982212002,0.251328908890292,11.7746750829505));
#18686=CARTESIAN_POINT('Ctrl Pts',(4.30465032591334,0.294753164260322,11.7769345051777));
#18687=CARTESIAN_POINT('Ctrl Pts',(4.29699862304371,0.338210524013558,11.7789549955099));
#18688=CARTESIAN_POINT('Ctrl Pts',(4.2896312933914,0.381682414128188,11.7806948857785));
#18689=CARTESIAN_POINT('Ctrl Pts',(4.28697846310439,0.397335785454289,11.781321385992));
#18690=CARTESIAN_POINT('Ctrl Pts',(4.28436254073142,0.412991050589563,11.7819110385617));
#18691=CARTESIAN_POINT('Ctrl Pts',(4.28178519416781,0.428647331668438,11.7824601840726));
#18692=CARTESIAN_POINT('Ctrl Pts',(4.2486735668154,0.525726490000048,11.7797315270537));
#18693=CARTESIAN_POINT('Ctrl Pts',(4.26374619995914,0.497289984563685,11.7830226438474));
#18694=CARTESIAN_POINT('Ctrl Pts',(4.27616566022512,0.462742784615148,11.783679000487));
#18695=CARTESIAN_POINT('Ctrl Pts',(4.28177589348483,0.428644839557943,11.782487583184));
#18696=CARTESIAN_POINT('Ctrl Pts',(4.2368038791629,0.514253184188583,11.773132618748));
#18697=CARTESIAN_POINT('Ctrl Pts',(4.25038555537826,0.48960012188578,11.777985280354));
#18698=CARTESIAN_POINT('Ctrl Pts',(4.26245207313798,0.458525980311001,11.7793725972104));
#18699=CARTESIAN_POINT('Ctrl Pts',(4.26757735435752,0.428033621458704,11.7776350210923));
#18700=CARTESIAN_POINT('Ctrl Pts',(4.20817000679401,0.490033235054154,11.7711728984776));
#18701=CARTESIAN_POINT('Ctrl Pts',(4.22105394566052,0.473487226884366,11.7768547886379));
#18702=CARTESIAN_POINT('Ctrl Pts',(4.23282911654911,0.449515232679256,11.7785372227129));
#18703=CARTESIAN_POINT('Ctrl Pts',(4.2364394051555,0.426069510514664,11.7761487419229));
#18704=CARTESIAN_POINT('Ctrl Pts',(4.18191946942526,0.473520527526364,11.7923527205827));
#18705=CARTESIAN_POINT('Ctrl Pts',(4.19617224734773,0.460605230875895,11.7941633853966));
#18706=CARTESIAN_POINT('Ctrl Pts',(4.20728837804396,0.442036565491117,11.7934702039683));
#18707=CARTESIAN_POINT('Ctrl Pts',(4.20937438480907,0.423229901258667,11.7914804062487));
#18708=CARTESIAN_POINT('Ctrl Pts',(4.17218826315047,0.468962654353794,11.80651609725));
#18709=CARTESIAN_POINT('Ctrl Pts',(4.18688126868098,0.455889756420883,11.806032917619));
#18710=CARTESIAN_POINT('Ctrl Pts',(4.19736873106825,0.439262007746224,11.8038103380598));
#18711=CARTESIAN_POINT('Ctrl Pts',(4.19894501008283,0.421808480676737,11.8021914830441));
#18712=CARTESIAN_POINT('Ctrl Pts',(4.28177589321514,0.428644841197042,11.7824875832413));
#18713=CARTESIAN_POINT('Ctrl Pts',(4.27616577833755,0.462742065438141,11.7836789752985));
#18714=CARTESIAN_POINT('Ctrl Pts',(4.26374672441132,0.497288525471169,11.7830226715236));
#18715=CARTESIAN_POINT('Ctrl Pts',(4.24867452199362,0.525724687915784,11.7797317356146));
#18716=CARTESIAN_POINT('',(4.17218826315256,0.468962654354822,11.8065160972469));
#18717=CARTESIAN_POINT('Origin',(4.21654544948669,0.517117786907486,11.8524891679444));
#18718=CARTESIAN_POINT('Ctrl Pts',(4.17218826315047,0.468962654353794,11.80651609725));
#18719=CARTESIAN_POINT('Ctrl Pts',(4.18688126868098,0.455889756420883,11.806032917619));
#18720=CARTESIAN_POINT('Ctrl Pts',(4.19736873106825,0.439262007746224,11.8038103380598));
#18721=CARTESIAN_POINT('Ctrl Pts',(4.19894501008283,0.421808480676737,11.8021914830441));
#18722=CARTESIAN_POINT('Ctrl Pts',(4.23244357912718,0.0834503638580652,
11.7677845155721));
#18723=CARTESIAN_POINT('Ctrl Pts',(4.23124359603722,0.0892621551574759,
11.7690161098144));
#18724=CARTESIAN_POINT('Ctrl Pts',(4.23027567575553,0.0951717685553224,
11.7700097262397));
#18725=CARTESIAN_POINT('Ctrl Pts',(4.22954577757009,0.101140384729842,11.7707590442118));
#18726=CARTESIAN_POINT('Ctrl Pts',(4.24783021369305,0.0899565784776398,
11.7519925509196));
#18727=CARTESIAN_POINT('Ctrl Pts',(4.24680279265781,0.0949288632967188,
11.7530451914931));
#18728=CARTESIAN_POINT('Ctrl Pts',(4.24597265680021,0.0999940784592962,
11.7538961092212));
#18729=CARTESIAN_POINT('Ctrl Pts',(4.24534779634232,0.105100317994799,11.7545365944285));
#18730=CARTESIAN_POINT('Ctrl Pts',(4.28772157465326,0.101235139924101,11.7374963477574));
#18731=CARTESIAN_POINT('Ctrl Pts',(4.28699316039155,0.104761359558322,11.7382410744884));
#18732=CARTESIAN_POINT('Ctrl Pts',(4.28640608685963,0.108344058397789,11.7388415688776));
#18733=CARTESIAN_POINT('Ctrl Pts',(4.28596309958905,0.111964864227218,11.7392947835658));
#18734=CARTESIAN_POINT('Ctrl Pts',(4.32658203586776,0.105745113375536,11.7540207776828));
#18735=CARTESIAN_POINT('Ctrl Pts',(4.32597549644476,0.108688259084721,11.7546424103689));
#18736=CARTESIAN_POINT('Ctrl Pts',(4.32548517203557,0.111686864219622,11.7551450805111));
#18737=CARTESIAN_POINT('Ctrl Pts',(4.32511617292258,0.114709169987786,11.7555234177697));
#18738=CARTESIAN_POINT('Ctrl Pts',(4.33962418453247,0.106048354957064,11.7652934103049));
#18739=CARTESIAN_POINT('Ctrl Pts',(4.3390257792157,0.108954250606769,11.7659075794119));
#18740=CARTESIAN_POINT('Ctrl Pts',(4.33854297284435,0.111909057305692,11.7664032032109));
#18741=CARTESIAN_POINT('Ctrl Pts',(4.33817886051713,0.114893365392952,11.7667770031683));
#18742=CARTESIAN_POINT('',(4.23244376179554,0.0834501820051857,11.7677846774689));
#18743=CARTESIAN_POINT('',(4.33962418453247,0.106048354957064,11.7652934103049));
#18744=CARTESIAN_POINT('Origin',(4.28974268595947,0.0834503638580657,11.8236129344662));
#18745=CARTESIAN_POINT('Origin',(4.39309251486109,0.128651272185532,11.7104388275966));
#18746=CARTESIAN_POINT('Origin',(4.33906241113996,0.128640496010329,11.6584014009706));
#18747=CARTESIAN_POINT('Ctrl Pts',(4.1864400889711,0.599559286979599,11.7367177974007));
#18748=CARTESIAN_POINT('Ctrl Pts',(4.1886804737254,0.599217388237333,11.7419000771489));
#18749=CARTESIAN_POINT('Ctrl Pts',(4.19485662924956,0.59640540998248,11.7517403335914));
#18750=CARTESIAN_POINT('Ctrl Pts',(4.20959478601258,0.583418316193309,11.7648503721434));
#18751=CARTESIAN_POINT('Ctrl Pts',(4.22860122563327,0.56002441203863,11.7744735096015));
#18752=CARTESIAN_POINT('Ctrl Pts',(4.24226657406414,0.537814124752668,11.7783325570636));
#18753=CARTESIAN_POINT('Ctrl Pts',(4.24867356681529,0.525726490000265,11.7797315270537));
#18754=CARTESIAN_POINT('Ctrl Pts',(4.18952705913928,0.586463809002539,11.735700158011));
#18755=CARTESIAN_POINT('Ctrl Pts',(4.19137342751675,0.585902923557031,11.7399942324166));
#18756=CARTESIAN_POINT('Ctrl Pts',(4.19607564927109,0.582996738128302,11.7478909268382));
#18757=CARTESIAN_POINT('Ctrl Pts',(4.20718567353011,0.571444962213375,11.759339123899));
#18758=CARTESIAN_POINT('Ctrl Pts',(4.22315764354396,0.550663720789415,11.7694614446329));
#18759=CARTESIAN_POINT('Ctrl Pts',(4.23584186027139,0.530339176921929,11.7741901849771));
#18760=CARTESIAN_POINT('Ctrl Pts',(4.24189088815672,0.51917031525084,11.7759607223076));
#18761=CARTESIAN_POINT('Ctrl Pts',(4.18941786442921,0.5586701286686,11.7362685864366));
#18762=CARTESIAN_POINT('Ctrl Pts',(4.19047278915203,0.557673290482625,11.7393205950847));
#18763=CARTESIAN_POINT('Ctrl Pts',(4.19257132672879,0.554666512895981,11.7443495285969));
#18764=CARTESIAN_POINT('Ctrl Pts',(4.19793491703686,0.546370059453453,11.7532207324389));
#18765=CARTESIAN_POINT('Ctrl Pts',(4.20960649937055,0.531257609322764,11.763935815195));
#18766=CARTESIAN_POINT('Ctrl Pts',(4.22112932284417,0.514903265836773,11.7697717579804));
#18767=CARTESIAN_POINT('Ctrl Pts',(4.22676242995304,0.505649359848945,11.7720002083824));
#18768=CARTESIAN_POINT('Ctrl Pts',(4.16745842900663,0.516177609788138,11.7460636132259));
#18769=CARTESIAN_POINT('Ctrl Pts',(4.16745960968501,0.514934209415718,11.7493116799598));
#18770=CARTESIAN_POINT('Ctrl Pts',(4.16742526266361,0.512400102456327,11.754170815901));
#18771=CARTESIAN_POINT('Ctrl Pts',(4.1702424679982,0.508565778427457,11.7620313775964));
#18772=CARTESIAN_POINT('Ctrl Pts',(4.18112328052461,0.500936758529474,11.7716132782273));
#18773=CARTESIAN_POINT('Ctrl Pts',(4.19285904104883,0.490293107380878,11.776638091041));
#18774=CARTESIAN_POINT('Ctrl Pts',(4.19855158379117,0.483870890196332,11.7784814265239));
#18775=CARTESIAN_POINT('Ctrl Pts',(4.13708840011498,0.501283154238658,11.7587835155587));
#18776=CARTESIAN_POINT('Ctrl Pts',(4.13701026579034,0.500653265378882,11.7642021491914));
#18777=CARTESIAN_POINT('Ctrl Pts',(4.13829951247469,0.49908582037805,11.7733140929352));
#18778=CARTESIAN_POINT('Ctrl Pts',(4.14609086019466,0.495348174409366,11.7840463234316));
#18779=CARTESIAN_POINT('Ctrl Pts',(4.16138741638408,0.487734747778109,11.791448977135));
#18780=CARTESIAN_POINT('Ctrl Pts',(4.17444554632098,0.478374076350456,11.7937488231701));
#18781=CARTESIAN_POINT('Ctrl Pts',(4.18052929710018,0.472869402787525,11.7943760601066));
#18782=CARTESIAN_POINT('Ctrl Pts',(4.11838193196953,0.500422592509204,11.7664617086384));
#18783=CARTESIAN_POINT('Ctrl Pts',(4.11865168183635,0.500435001928776,11.7735428707743));
#18784=CARTESIAN_POINT('Ctrl Pts',(4.12165523740038,0.499626427226189,11.7860588810822));
#18785=CARTESIAN_POINT('Ctrl Pts',(4.13375709461643,0.494528711775158,11.7996999793846));
#18786=CARTESIAN_POINT('Ctrl Pts',(4.15222669835934,0.484505223058561,11.8062291222987));
#18787=CARTESIAN_POINT('Ctrl Pts',(4.16594264043612,0.474519610560075,11.8067214846143));
#18788=CARTESIAN_POINT('Ctrl Pts',(4.17218826315036,0.468962654353894,11.80651609725));
#18789=CARTESIAN_POINT('',(4.11838200569138,0.500422526122696,11.7664617661004));
#18790=CARTESIAN_POINT('Ctrl Pts',(4.20352712124656,0.513629536369044,11.7694536414083));
#18791=CARTESIAN_POINT('Ctrl Pts',(4.18960278591621,0.509898541151459,11.769080316127));
#18792=CARTESIAN_POINT('Ctrl Pts',(4.17615741309794,0.507139097066293,11.7705957934386));
#18793=CARTESIAN_POINT('Ctrl Pts',(4.15632514529375,0.503898993650465,11.7723830647377));
#18794=CARTESIAN_POINT('Ctrl Pts',(4.14962589610481,0.503026780112622,11.7727554305325));
#18795=CARTESIAN_POINT('Ctrl Pts',(4.1351819577934,0.501481089633748,11.7717516560017));
#18796=CARTESIAN_POINT('Ctrl Pts',(4.12736858237728,0.500845146597188,11.7702972624861));
#18797=CARTESIAN_POINT('Ctrl Pts',(4.11865840483925,0.500435383006644,11.7665811325368));
#18798=CARTESIAN_POINT('Ctrl Pts',(4.11852016115429,0.500428951553896,11.7665216619244));
#18799=CARTESIAN_POINT('Ctrl Pts',(4.11838201228193,0.500422596203858,11.7664617434719));
#18800=CARTESIAN_POINT('Ctrl Pts',(4.11838193425775,0.500422592614458,11.7664617687052));
#18801=CARTESIAN_POINT('Ctrl Pts',(4.11865169032903,0.500434999642494,11.7735429061638));
#18802=CARTESIAN_POINT('Ctrl Pts',(4.12165524766592,0.499626422901991,11.7860588926534));
#18803=CARTESIAN_POINT('Ctrl Pts',(4.13375709461643,0.494528711775158,11.7996999793846));
#18804=CARTESIAN_POINT('Ctrl Pts',(4.15222669835934,0.484505223058561,11.8062291222987));
#18805=CARTESIAN_POINT('Ctrl Pts',(4.16594264043612,0.474519610560075,11.8067214846143));
#18806=CARTESIAN_POINT('Ctrl Pts',(4.17218826315036,0.468962654353894,11.80651609725));
#18807=CARTESIAN_POINT('Ctrl Pts',(4.33962418453247,0.106048354957063,11.7652934103049));
#18808=CARTESIAN_POINT('Ctrl Pts',(4.34246949077866,0.0922313603362983,
11.7623731501614));
#18809=CARTESIAN_POINT('Ctrl Pts',(4.34745706311513,0.0672688955414189,
11.7459971874554));
#18810=CARTESIAN_POINT('Ctrl Pts',(4.3556551375003,0.0558301882629109,11.7196032056567));
#18811=CARTESIAN_POINT('Ctrl Pts',(4.36216987636126,0.0534615492574821,
11.7069738861294));
#18812=CARTESIAN_POINT('Ctrl Pts',(4.32223465297952,0.10564403284836,11.7502632334754));
#18813=CARTESIAN_POINT('Ctrl Pts',(4.32478575489734,0.095417896876601,11.748512775078));
#18814=CARTESIAN_POINT('Ctrl Pts',(4.3306965583525,0.0742071101490252,11.737276832848));
#18815=CARTESIAN_POINT('Ctrl Pts',(4.34109202085652,0.0611390274796559,
11.7121170913212));
#18816=CARTESIAN_POINT('Ctrl Pts',(4.34880635645981,0.0583202788559448,
11.6991691569315));
#18817=CARTESIAN_POINT('Ctrl Pts',(4.28058245277421,0.0997299260061634,
11.7376622728835));
#18818=CARTESIAN_POINT('Ctrl Pts',(4.28392629294866,0.092691693017298,11.7364042543565));
#18819=CARTESIAN_POINT('Ctrl Pts',(4.29468264038552,0.0750207280329448,
11.7276251801877));
#18820=CARTESIAN_POINT('Ctrl Pts',(4.31151716837604,0.0612211827675296,
11.7004931914203));
#18821=CARTESIAN_POINT('Ctrl Pts',(4.3224279424754,0.0584221672677555,11.6855429425366));
#18822=CARTESIAN_POINT('Ctrl Pts',(4.24398355505158,0.0883300248227467,
11.7559405420827));
#18823=CARTESIAN_POINT('Ctrl Pts',(4.24866969340974,0.0774044433934375,
11.7521028590549));
#18824=CARTESIAN_POINT('Ctrl Pts',(4.26266537403032,0.0561815068305335,
11.7323050480364));
#18825=CARTESIAN_POINT('Ctrl Pts',(4.28486228403869,0.0454021943366394,
11.6953979077451));
#18826=CARTESIAN_POINT('Ctrl Pts',(4.2989472341934,0.0439270963371727,11.6761491591203));
#18827=CARTESIAN_POINT('Ctrl Pts',(4.23244357912718,0.0834503638580655,
11.7677845155721));
#18828=CARTESIAN_POINT('Ctrl Pts',(4.23751751309539,0.0698384627757711,
11.7625769189705));
#18829=CARTESIAN_POINT('Ctrl Pts',(4.25171234512073,0.0457415007973147,
11.7367473849806));
#18830=CARTESIAN_POINT('Ctrl Pts',(4.27527634265085,0.0364965974668743,
11.6946834568217));
#18831=CARTESIAN_POINT('Ctrl Pts',(4.29045125549198,0.035695688094989,11.6733103800476));
#18832=CARTESIAN_POINT('',(4.29045125544124,0.0356956880470215,11.6733103800327));
#18833=CARTESIAN_POINT('',(4.36216987635991,0.0534615492579749,11.7069738861286));
#18834=CARTESIAN_POINT('Origin',(4.33483406961706,-0.0217232475410972,11.7069738861151));
#18835=CARTESIAN_POINT('Ctrl Pts',(4.36216987636126,0.0534615492574821,
11.7069738861294));
#18836=CARTESIAN_POINT('Ctrl Pts',(4.3556551375003,0.0558301882629109,11.7196032056567));
#18837=CARTESIAN_POINT('Ctrl Pts',(4.34745706311513,0.0672688955414189,
11.7459971874554));
#18838=CARTESIAN_POINT('Ctrl Pts',(4.34246949077866,0.0922313603362983,
11.7623731501614));
#18839=CARTESIAN_POINT('Ctrl Pts',(4.33962418453247,0.106048354957063,11.7652934103049));
#18840=CARTESIAN_POINT('Ctrl Pts',(4.23245081468777,0.0834309576742871,
11.7677770855905));
#18841=CARTESIAN_POINT('Ctrl Pts',(4.23752425974456,0.0698270114887331,
11.7625646425201));
#18842=CARTESIAN_POINT('Ctrl Pts',(4.2517179445374,0.0457393039686254,11.7367373895008));
#18843=CARTESIAN_POINT('Ctrl Pts',(4.27527634265085,0.0364965974668743,
11.6946834568217));
#18844=CARTESIAN_POINT('Ctrl Pts',(4.29045125549198,0.035695688094989,11.6733103800476));
#18845=CARTESIAN_POINT('Ctrl Pts',(4.34421258421314,0.0378725448121803,
11.5962093343554));
#18846=CARTESIAN_POINT('Ctrl Pts',(4.32681581897869,0.0356051827682455,
11.6219251290513));
#18847=CARTESIAN_POINT('Ctrl Pts',(4.30862493048636,0.0347365085016417,
11.64771370248));
#18848=CARTESIAN_POINT('Ctrl Pts',(4.29045125548377,0.0356956880906077,
11.673310380051));
#18849=CARTESIAN_POINT('Ctrl Pts',(4.35122162761644,0.0423700546448687,
11.5993028404662));
#18850=CARTESIAN_POINT('Ctrl Pts',(4.33537392032581,0.0418771635834138,
11.6257460902884));
#18851=CARTESIAN_POINT('Ctrl Pts',(4.31864236216508,0.0431620305839684,
11.6518872279534));
#18852=CARTESIAN_POINT('Ctrl Pts',(4.30177922708538,0.0466708990771757,
11.6770954188119));
#18853=CARTESIAN_POINT('Ctrl Pts',(4.36466668386284,0.0479840668591653,
11.605316017609));
#18854=CARTESIAN_POINT('Ctrl Pts',(4.35226885751852,0.0494632699189516,
11.6335433648312));
#18855=CARTESIAN_POINT('Ctrl Pts',(4.33918335764944,0.0531330803712445,
11.6611567729366));
#18856=CARTESIAN_POINT('Ctrl Pts',(4.32650404086796,0.0594318912603617,
11.6874561924858));
#18857=CARTESIAN_POINT('Ctrl Pts',(4.37888556984392,0.0491234947965908,
11.6118011873195));
#18858=CARTESIAN_POINT('Ctrl Pts',(4.37020796655163,0.0501668611945751,
11.6422225306338));
#18859=CARTESIAN_POINT('Ctrl Pts',(4.36099713174971,0.0527032630974422,
11.6720529183227));
#18860=CARTESIAN_POINT('Ctrl Pts',(4.35214723642143,0.0571055964480933,
11.7011203392195));
#18861=CARTESIAN_POINT('Ctrl Pts',(4.38493129402142,0.048777234595766,11.6145804154759));
#18862=CARTESIAN_POINT('Ctrl Pts',(4.37774644585057,0.0491887364932216,
11.6459417104654));
#18863=CARTESIAN_POINT('Ctrl Pts',(4.36997201320337,0.0506248360545129,
11.6767238081028));
#18864=CARTESIAN_POINT('Ctrl Pts',(4.36216987634685,0.0534615492511837,
11.7069738861159));
#18865=CARTESIAN_POINT('',(4.38493129402142,0.0487772345957665,11.6145804154759));
#18866=CARTESIAN_POINT('',(4.32736007730607,0.0514806398808873,11.6713697523917));
#18867=CARTESIAN_POINT('Ctrl Pts',(4.38493129402142,0.048777234595766,11.6145804154759));
#18868=CARTESIAN_POINT('Ctrl Pts',(4.37601770603885,0.0492877475921092,
11.6232421393828));
#18869=CARTESIAN_POINT('Ctrl Pts',(4.3668693999289,0.049677922134395,11.632197583949));
#18870=CARTESIAN_POINT('Ctrl Pts',(4.35762739235915,0.0500769766269212,
11.6413098490428));
#18871=CARTESIAN_POINT('Ctrl Pts',(4.35431874628973,0.0502198384530139,
11.6445720472024));
#18872=CARTESIAN_POINT('Ctrl Pts',(4.35101123017846,0.0503624490374187,
11.6478412754132));
#18873=CARTESIAN_POINT('Ctrl Pts',(4.34770259990182,0.0505083669896217,
11.6511194166589));
#18874=CARTESIAN_POINT('Ctrl Pts',(4.3409327813208,0.0508069310422763,11.6578268513558));
#18875=CARTESIAN_POINT('Ctrl Pts',(4.33415830379631,0.051119715599887,11.6645715917699));
#18876=CARTESIAN_POINT('Ctrl Pts',(4.32736007730607,0.0514806398808858,
11.6713697523917));
#18877=CARTESIAN_POINT('Ctrl Pts',(4.38493129402142,0.048777234595766,11.6145804154759));
#18878=CARTESIAN_POINT('Ctrl Pts',(4.37774644585057,0.0491887364932216,
11.6459417104654));
#18879=CARTESIAN_POINT('Ctrl Pts',(4.36997201320337,0.0506248360545129,
11.6767238081028));
#18880=CARTESIAN_POINT('Ctrl Pts',(4.36216987634685,0.0534615492511837,
11.7069738861159));
#18881=CARTESIAN_POINT('',(4.33139507209999,0.0364734805255282,11.6149738861246));
#18882=CARTESIAN_POINT('Ctrl Pts',(4.29045125548377,0.0356956880906077,
11.673310380051));
#18883=CARTESIAN_POINT('Ctrl Pts',(4.30420562082409,0.0349697531054306,
11.6539380706662));
#18884=CARTESIAN_POINT('Ctrl Pts',(4.31796984588305,0.0352907949390317,
11.63445584521));
#18885=CARTESIAN_POINT('Ctrl Pts',(4.33139221270344,0.0364727682572349,
11.614978441252));
#18886=CARTESIAN_POINT('Ctrl Pts',(4.32736007730609,0.051480639880892,11.6713697523917));
#18887=CARTESIAN_POINT('Ctrl Pts',(4.32798253826001,0.0491575839751223,
11.6619619576146));
#18888=CARTESIAN_POINT('Ctrl Pts',(4.32862960298899,0.0467427055308035,
11.6524786614797));
#18889=CARTESIAN_POINT('Ctrl Pts',(4.3299579720458,0.0417851647195623,11.6337717205853));
#18890=CARTESIAN_POINT('Ctrl Pts',(4.33065634771171,0.0391787912516445,
11.6243066674654));
#18891=CARTESIAN_POINT('Ctrl Pts',(4.33138167302864,0.0364718403168447,
11.614993735436));
#18892=CARTESIAN_POINT('Ctrl Pts',(4.44483865181741,0.143472770337244,11.7628168777948));
#18893=CARTESIAN_POINT('Ctrl Pts',(4.31439385308573,0.630299386786979,11.7628168777948));
#18894=CARTESIAN_POINT('Ctrl Pts',(4.42917451869962,0.1392755785182,11.7794523105961));
#18895=CARTESIAN_POINT('Ctrl Pts',(4.29872971996794,0.626102194967936,11.7794523105961));
#18896=CARTESIAN_POINT('Ctrl Pts',(4.38897935642072,0.128505317245929,11.7951014042888));
#18897=CARTESIAN_POINT('Ctrl Pts',(4.25853455768904,0.615331933695665,11.7951014042888));
#18898=CARTESIAN_POINT('Ctrl Pts',(4.35076008096908,0.118264493253361,11.7783502649473));
#18899=CARTESIAN_POINT('Ctrl Pts',(4.2203152822374,0.605091109703097,11.7783502649473));
#18900=CARTESIAN_POINT('Ctrl Pts',(4.33817886049864,0.114893365388508,11.7667770031876));
#18901=CARTESIAN_POINT('Ctrl Pts',(4.20773406176696,0.601719981838243,11.7667770031876));
#18902=CARTESIAN_POINT('',(4.44483865181741,0.143472770337245,11.7628168777948));
#18903=CARTESIAN_POINT('Origin',(4.38950568308719,0.128646346051165,11.706973886163));
#18904=CARTESIAN_POINT('',(4.44483865181741,0.143472770337244,11.7628168777948));
#18905=CARTESIAN_POINT('Origin',(4.38950568310546,0.128646346056062,11.7069738861436));
#18906=CARTESIAN_POINT('Origin',(4.38950568308719,0.128646346051166,11.7069738861252));
#18907=CARTESIAN_POINT('Origin',(4.38950568310546,0.128646346056062,11.7069738861436));
#18908=CARTESIAN_POINT('Origin',(4.38950568308719,0.128646346051166,5.29092677993983));
#18909=CARTESIAN_POINT('Origin',(4.38948772286522,0.129021219720988,11.6136857339278));
#18910=CARTESIAN_POINT('Ctrl Pts',(4.08617023400024,-0.552060840994624,
11.9163435012344));
#18911=CARTESIAN_POINT('Ctrl Pts',(4.08617023400024,1.61522066995007,11.9163435012344));
#18912=CARTESIAN_POINT('Ctrl Pts',(4.10576511646638,-0.552060840994624,
11.8970344456328));
#18913=CARTESIAN_POINT('Ctrl Pts',(4.10576511646638,1.61522066995007,11.8970344456328));
#18914=CARTESIAN_POINT('Ctrl Pts',(4.15149421914094,-0.552060840994624,
11.8511956487512));
#18915=CARTESIAN_POINT('Ctrl Pts',(4.15149421914094,1.61522066995007,11.8511956487512));
#18916=CARTESIAN_POINT('Ctrl Pts',(4.22408937937455,-0.552060840994624,
11.7763607682953));
#18917=CARTESIAN_POINT('Ctrl Pts',(4.22408937937455,1.61522066995007,11.7763607682953));
#18918=CARTESIAN_POINT('Ctrl Pts',(4.3260071847331,-0.552060840994624,11.6707401393954));
#18919=CARTESIAN_POINT('Ctrl Pts',(4.3260071847331,1.61522066995007,11.6707401393954));
#18920=CARTESIAN_POINT('Ctrl Pts',(4.46255574628753,-0.552060840994624,
11.5373242211525));
#18921=CARTESIAN_POINT('Ctrl Pts',(4.46255574628753,1.61522066995007,11.5373242211525));
#18922=CARTESIAN_POINT('Ctrl Pts',(4.61532593596939,-0.552060840994624,
11.4029224160728));
#18923=CARTESIAN_POINT('Ctrl Pts',(4.61532593596939,1.61522066995007,11.4029224160728));
#18924=CARTESIAN_POINT('Ctrl Pts',(4.77596612414944,-0.552060840994624,
11.2768795166233));
#18925=CARTESIAN_POINT('Ctrl Pts',(4.77596612414944,1.61522066995007,11.2768795166233));
#18926=CARTESIAN_POINT('Ctrl Pts',(4.94211773226968,-0.552060840994624,
11.1598106424589));
#18927=CARTESIAN_POINT('Ctrl Pts',(4.94211773226968,1.61522066995007,11.1598106424589));
#18928=CARTESIAN_POINT('Ctrl Pts',(5.11112998264613,-0.552060840994624,
11.051370419133));
#18929=CARTESIAN_POINT('Ctrl Pts',(5.11112998264613,1.61522066995007,11.051370419133));
#18930=CARTESIAN_POINT('Ctrl Pts',(5.28082876351925,-0.552060840994624,
10.9511663773825));
#18931=CARTESIAN_POINT('Ctrl Pts',(5.28082876351925,1.61522066995007,10.9511663773825));
#18932=CARTESIAN_POINT('Ctrl Pts',(5.45051506148977,-0.552060840994624,
10.8599381259735));
#18933=CARTESIAN_POINT('Ctrl Pts',(5.45051506148977,1.61522066995007,10.8599381259735));
#18934=CARTESIAN_POINT('Ctrl Pts',(5.62101499943423,-0.552060840994624,
10.7795199127532));
#18935=CARTESIAN_POINT('Ctrl Pts',(5.62101499943423,1.61522066995007,10.7795199127532));
#18936=CARTESIAN_POINT('Ctrl Pts',(5.7936769541502,-0.552060840994624,10.7114411549111));
#18937=CARTESIAN_POINT('Ctrl Pts',(5.7936769541502,1.61522066995007,10.7114411549111));
#18938=CARTESIAN_POINT('Ctrl Pts',(5.96961932707136,-0.552060840994624,
10.6558377434042));
#18939=CARTESIAN_POINT('Ctrl Pts',(5.96961932707136,1.61522066995007,10.6558377434042));
#18940=CARTESIAN_POINT('Ctrl Pts',(6.14893768388704,-0.552060840994624,
10.6103475969888));
#18941=CARTESIAN_POINT('Ctrl Pts',(6.14893768388704,1.61522066995007,10.6103475969888));
#18942=CARTESIAN_POINT('Ctrl Pts',(6.32976796473819,-0.552060840994624,
10.5687216653907));
#18943=CARTESIAN_POINT('Ctrl Pts',(6.32976796473819,1.61522066995007,10.5687216653907));
#18944=CARTESIAN_POINT('Ctrl Pts',(6.50892555577775,-0.552060840994624,
10.5222908830264));
#18945=CARTESIAN_POINT('Ctrl Pts',(6.50892555577775,1.61522066995007,10.5222908830264));
#18946=CARTESIAN_POINT('Ctrl Pts',(6.68288828293941,-0.552060840994624,
10.462050267878));
#18947=CARTESIAN_POINT('Ctrl Pts',(6.68288828293941,1.61522066995007,10.462050267878));
#18948=CARTESIAN_POINT('Ctrl Pts',(6.84859008776107,-0.552060840994624,
10.3804015453596));
#18949=CARTESIAN_POINT('Ctrl Pts',(6.84859008776107,1.61522066995007,10.3804015453596));
#18950=CARTESIAN_POINT('Ctrl Pts',(7.00445448641038,-0.552060840994624,
10.2733319413005));
#18951=CARTESIAN_POINT('Ctrl Pts',(7.00445448641038,1.61522066995007,10.2733319413005));
#18952=CARTESIAN_POINT('Ctrl Pts',(7.15081550722288,-0.552060840994624,
10.1414720974144));
#18953=CARTESIAN_POINT('Ctrl Pts',(7.15081550722288,1.61522066995007,10.1414720974144));
#18954=CARTESIAN_POINT('Ctrl Pts',(7.28883796912684,-0.552060840994624,
9.98835756998534));
#18955=CARTESIAN_POINT('Ctrl Pts',(7.28883796912684,1.61522066995007,9.98835756998534));
#18956=CARTESIAN_POINT('Ctrl Pts',(7.41967047354988,-0.552060840994624,
9.81917361987377));
#18957=CARTESIAN_POINT('Ctrl Pts',(7.41967047354988,1.61522066995007,9.81917361987377));
#18958=CARTESIAN_POINT('Ctrl Pts',(7.54360573526532,-0.552060840994624,
9.63939026966049));
#18959=CARTESIAN_POINT('Ctrl Pts',(7.54360573526532,1.61522066995007,9.63939026966049));
#18960=CARTESIAN_POINT('Ctrl Pts',(7.6590003866074,-0.552060840994624,9.45324999450471));
#18961=CARTESIAN_POINT('Ctrl Pts',(7.6590003866074,1.61522066995007,9.45324999450471));
#18962=CARTESIAN_POINT('Ctrl Pts',(7.76209282457502,-0.552060840994624,
9.26297089919836));
#18963=CARTESIAN_POINT('Ctrl Pts',(7.76209282457502,1.61522066995007,9.26297089919836));
#18964=CARTESIAN_POINT('Ctrl Pts',(7.84862074946283,-0.552060840994624,
9.06945407017055));
#18965=CARTESIAN_POINT('Ctrl Pts',(7.84862074946283,1.61522066995007,9.06945407017055));
#18966=CARTESIAN_POINT('Ctrl Pts',(7.91508259073031,-0.552060840994624,
8.87266947141857));
#18967=CARTESIAN_POINT('Ctrl Pts',(7.91508259073031,1.61522066995007,8.87266947141857));
#18968=CARTESIAN_POINT('Ctrl Pts',(7.96007609558387,-0.552060840994624,
8.67216210283894));
#18969=CARTESIAN_POINT('Ctrl Pts',(7.96007609558387,1.61522066995007,8.67216210283894));
#18970=CARTESIAN_POINT('Ctrl Pts',(7.98575825096082,-0.552060840994624,
8.46752658699496));
#18971=CARTESIAN_POINT('Ctrl Pts',(7.98575825096082,1.61522066995007,8.46752658699496));
#18972=CARTESIAN_POINT('Ctrl Pts',(7.9987984391963,-0.552060840994624,8.25883677791438));
#18973=CARTESIAN_POINT('Ctrl Pts',(7.9987984391963,1.61522066995007,8.25883677791438));
#18974=CARTESIAN_POINT('Ctrl Pts',(8.00781893805568,-0.552060840994624,
8.04662057355209));
#18975=CARTESIAN_POINT('Ctrl Pts',(8.00781893805568,1.61522066995007,8.04662057355209));
#18976=CARTESIAN_POINT('Ctrl Pts',(8.02124364536257,-0.552060840994624,
7.8318867323277));
#18977=CARTESIAN_POINT('Ctrl Pts',(8.02124364536257,1.61522066995007,7.8318867323277));
#18978=CARTESIAN_POINT('Ctrl Pts',(8.04494633492827,-0.552060840994624,
7.61613341658679));
#18979=CARTESIAN_POINT('Ctrl Pts',(8.04494633492827,1.61522066995007,7.61613341658679));
#18980=CARTESIAN_POINT('Ctrl Pts',(8.08008348678094,-0.552060840994624,
7.40136016279815));
#18981=CARTESIAN_POINT('Ctrl Pts',(8.08008348678094,1.61522066995007,7.40136016279815));
#18982=CARTESIAN_POINT('Ctrl Pts',(8.12057943633426,-0.552060840994624,
7.19009032473197));
#18983=CARTESIAN_POINT('Ctrl Pts',(8.12057943633426,1.61522066995007,7.19009032473197));
#18984=CARTESIAN_POINT('Ctrl Pts',(8.15569042861283,-0.552060840994624,
6.98516923427904));
#18985=CARTESIAN_POINT('Ctrl Pts',(8.15569042861283,1.61522066995007,6.98516923427904));
#18986=CARTESIAN_POINT('Ctrl Pts',(8.17293082304204,-0.552060840994624,
6.78954489191915));
#18987=CARTESIAN_POINT('Ctrl Pts',(8.17293082304204,1.61522066995007,6.78954489191915));
#18988=CARTESIAN_POINT('Ctrl Pts',(8.16089752265956,-0.552060840994624,
6.60605451948904));
#18989=CARTESIAN_POINT('Ctrl Pts',(8.16089752265956,1.61522066995007,6.60605451948904));
#18990=CARTESIAN_POINT('Ctrl Pts',(8.11207116917844,-0.552060840994624,
6.43720976255638));
#18991=CARTESIAN_POINT('Ctrl Pts',(8.11207116917844,1.61522066995007,6.43720976255638));
#18992=CARTESIAN_POINT('Ctrl Pts',(8.02580908828092,-0.552060840994624,
6.28498018271691));
#18993=CARTESIAN_POINT('Ctrl Pts',(8.02580908828092,1.61522066995007,6.28498018271691));
#18994=CARTESIAN_POINT('Ctrl Pts',(7.90644860448881,-0.552060840994624,
6.15052660592943));
#18995=CARTESIAN_POINT('Ctrl Pts',(7.90644860448881,1.61522066995007,6.15052660592943));
#18996=CARTESIAN_POINT('Ctrl Pts',(7.76106756457749,-0.552060840994624,
6.03389995867286));
#18997=CARTESIAN_POINT('Ctrl Pts',(7.76106756457749,1.61522066995007,6.03389995867286));
#18998=CARTESIAN_POINT('Ctrl Pts',(7.59751903688427,-0.552060840994624,
5.93381436957244));
#18999=CARTESIAN_POINT('Ctrl Pts',(7.59751903688427,1.61522066995007,5.93381436957244));
#19000=CARTESIAN_POINT('Ctrl Pts',(7.42198551710643,-0.552060840994624,
5.84723737025948));
#19001=CARTESIAN_POINT('Ctrl Pts',(7.42198551710643,1.61522066995007,5.84723737025948));
#19002=CARTESIAN_POINT('Ctrl Pts',(7.23853768475023,-0.552060840994624,
5.76979878895671));
#19003=CARTESIAN_POINT('Ctrl Pts',(7.23853768475023,1.61522066995007,5.76979878895671));
#19004=CARTESIAN_POINT('Ctrl Pts',(7.04976847947264,-0.552060840994624,
5.69662713609756));
#19005=CARTESIAN_POINT('Ctrl Pts',(7.04976847947264,1.61522066995007,5.69662713609756));
#19006=CARTESIAN_POINT('Ctrl Pts',(6.85709976037512,-0.552060840994624,
5.62308582598972));
#19007=CARTESIAN_POINT('Ctrl Pts',(6.85709976037512,1.61522066995007,5.62308582598972));
#19008=CARTESIAN_POINT('Ctrl Pts',(6.66121503090593,-0.552060840994624,
5.54547963906641));
#19009=CARTESIAN_POINT('Ctrl Pts',(6.66121503090593,1.61522066995007,5.54547963906641));
#19010=CARTESIAN_POINT('Ctrl Pts',(6.46246210121974,-0.552060840994624,
5.46195513100458));
#19011=CARTESIAN_POINT('Ctrl Pts',(6.46246210121974,1.61522066995007,5.46195513100458));
#19012=CARTESIAN_POINT('Ctrl Pts',(6.26112587698791,-0.552060840994624,
5.37226655127806));
#19013=CARTESIAN_POINT('Ctrl Pts',(6.26112587698791,1.61522066995007,5.37226655127806));
#19014=CARTESIAN_POINT('Ctrl Pts',(6.05762450882876,-0.552060840994624,
5.27709955371581));
#19015=CARTESIAN_POINT('Ctrl Pts',(6.05762450882876,1.61522066995007,5.27709955371581));
#19016=CARTESIAN_POINT('Ctrl Pts',(5.85274048349253,-0.552060840994624,
5.17752467829117));
#19017=CARTESIAN_POINT('Ctrl Pts',(5.85274048349253,1.61522066995007,5.17752467829117));
#19018=CARTESIAN_POINT('Ctrl Pts',(5.6478173738032,-0.552060840994624,5.07442896098936));
#19019=CARTESIAN_POINT('Ctrl Pts',(5.6478173738032,1.61522066995007,5.07442896098936));
#19020=CARTESIAN_POINT('Ctrl Pts',(5.44501860313336,-0.552060840994624,
4.96787993373722));
#19021=CARTESIAN_POINT('Ctrl Pts',(5.44501860313336,1.61522066995007,4.96787993373722));
#19022=CARTESIAN_POINT('Ctrl Pts',(5.24741086000008,-0.552060840994624,
4.85676111532844));
#19023=CARTESIAN_POINT('Ctrl Pts',(5.24741086000008,1.61522066995007,4.85676111532844));
#19024=CARTESIAN_POINT('Ctrl Pts',(5.05850630701875,-0.552060840994624,
4.73929437247794));
#19025=CARTESIAN_POINT('Ctrl Pts',(5.05850630701875,1.61522066995007,4.73929437247794));
#19026=CARTESIAN_POINT('Ctrl Pts',(4.88190185104846,-0.552060840994624,
4.61340315498245));
#19027=CARTESIAN_POINT('Ctrl Pts',(4.88190185104846,1.61522066995007,4.61340315498245));
#19028=CARTESIAN_POINT('Ctrl Pts',(4.7208720035032,-0.552060840994624,4.47714872481864));
#19029=CARTESIAN_POINT('Ctrl Pts',(4.7208720035032,1.61522066995007,4.47714872481864));
#19030=CARTESIAN_POINT('Ctrl Pts',(4.57800047823784,-0.552060840994624,
4.32911151507775));
#19031=CARTESIAN_POINT('Ctrl Pts',(4.57800047823784,1.61522066995007,4.32911151507775));
#19032=CARTESIAN_POINT('Ctrl Pts',(4.4547451964031,-0.552060840994624,4.16885849319143));
#19033=CARTESIAN_POINT('Ctrl Pts',(4.4547451964031,1.61522066995007,4.16885849319143));
#19034=CARTESIAN_POINT('Ctrl Pts',(4.35148411330737,-0.552060840994624,
3.99681013615577));
#19035=CARTESIAN_POINT('Ctrl Pts',(4.35148411330737,1.61522066995007,3.99681013615577));
#19036=CARTESIAN_POINT('Ctrl Pts',(4.26765207024408,-0.552060840994624,
3.81399668859083));
#19037=CARTESIAN_POINT('Ctrl Pts',(4.26765207024408,1.61522066995007,3.81399668859083));
#19038=CARTESIAN_POINT('Ctrl Pts',(4.20184334854117,-0.552060840994624,
3.62185203209172));
#19039=CARTESIAN_POINT('Ctrl Pts',(4.20184334854117,1.61522066995007,3.62185203209172));
#19040=CARTESIAN_POINT('Ctrl Pts',(4.15193466045737,-0.552060840994624,
3.42199345348454));
#19041=CARTESIAN_POINT('Ctrl Pts',(4.15193466045737,1.61522066995007,3.42199345348454));
#19042=CARTESIAN_POINT('Ctrl Pts',(4.11518318246501,-0.552060840994624,
3.21600287470933));
#19043=CARTESIAN_POINT('Ctrl Pts',(4.11518318246501,1.61522066995007,3.21600287470933));
#19044=CARTESIAN_POINT('Ctrl Pts',(4.08854433447712,-0.552060840994624,
3.00529120729351));
#19045=CARTESIAN_POINT('Ctrl Pts',(4.08854433447712,1.61522066995007,3.00529120729351));
#19046=CARTESIAN_POINT('Ctrl Pts',(4.06899962712481,-0.552060840994624,
2.7909834104826));
#19047=CARTESIAN_POINT('Ctrl Pts',(4.06899962712481,1.61522066995007,2.7909834104826));
#19048=CARTESIAN_POINT('Ctrl Pts',(4.05390260344518,-0.552060840994624,
2.57377631141663));
#19049=CARTESIAN_POINT('Ctrl Pts',(4.05390260344518,1.61522066995007,2.57377631141663));
#19050=CARTESIAN_POINT('Ctrl Pts',(4.04126813644791,-0.552060840994624,
2.35385258470204));
#19051=CARTESIAN_POINT('Ctrl Pts',(4.04126813644791,1.61522066995007,2.35385258470204));
#19052=CARTESIAN_POINT('Ctrl Pts',(4.03021014446877,-0.552060840994624,
2.13065748555701));
#19053=CARTESIAN_POINT('Ctrl Pts',(4.03021014446877,1.61522066995007,2.13065748555701));
#19054=CARTESIAN_POINT('Ctrl Pts',(4.02066709528519,-0.552060840994624,
1.9033255681334));
#19055=CARTESIAN_POINT('Ctrl Pts',(4.02066709528519,1.61522066995007,1.9033255681334));
#19056=CARTESIAN_POINT('Ctrl Pts',(4.012782399266,-0.552060840994624,1.67142113207676));
#19057=CARTESIAN_POINT('Ctrl Pts',(4.012782399266,1.61522066995007,1.67142113207676));
#19058=CARTESIAN_POINT('Ctrl Pts',(4.00639322616619,-0.552060840994624,
1.4355810193293));
#19059=CARTESIAN_POINT('Ctrl Pts',(4.00639322616619,1.61522066995007,1.4355810193293));
#19060=CARTESIAN_POINT('Ctrl Pts',(4.00047520099043,-0.552060840994624,
1.19819542279832));
#19061=CARTESIAN_POINT('Ctrl Pts',(4.00047520099043,1.61522066995007,1.19819542279832));
#19062=CARTESIAN_POINT('Ctrl Pts',(3.99260375067002,-0.552060840994624,
0.964078729991153));
#19063=CARTESIAN_POINT('Ctrl Pts',(3.99260375067002,1.61522066995007,0.964078729991153));
#19064=CARTESIAN_POINT('Ctrl Pts',(3.97841403016118,-0.552060840994624,
0.741129277895168));
#19065=CARTESIAN_POINT('Ctrl Pts',(3.97841403016118,1.61522066995007,0.741129277895168));
#19066=CARTESIAN_POINT('Ctrl Pts',(3.95259200169988,-0.552060840994624,
0.538436816836329));
#19067=CARTESIAN_POINT('Ctrl Pts',(3.95259200169988,1.61522066995007,0.538436816836329));
#19068=CARTESIAN_POINT('Ctrl Pts',(3.90986572419832,-0.552060840994624,
0.364350357241537));
#19069=CARTESIAN_POINT('Ctrl Pts',(3.90986572419832,1.61522066995007,0.364350357241537));
#19070=CARTESIAN_POINT('Ctrl Pts',(3.84598208672298,-0.552060840994624,
0.224659532804428));
#19071=CARTESIAN_POINT('Ctrl Pts',(3.84598208672298,1.61522066995007,0.224659532804428));
#19072=CARTESIAN_POINT('Ctrl Pts',(3.75872318140661,-0.552060840994624,
0.120497232333236));
#19073=CARTESIAN_POINT('Ctrl Pts',(3.75872318140661,1.61522066995007,0.120497232333236));
#19074=CARTESIAN_POINT('Ctrl Pts',(3.64881642260075,-0.552060840994624,
0.0470540298718229));
#19075=CARTESIAN_POINT('Ctrl Pts',(3.64881642260075,1.61522066995007,0.0470540298718229));
#19076=CARTESIAN_POINT('Ctrl Pts',(3.52045328348988,-0.552060840994624,
-0.00118366394786523));
#19077=CARTESIAN_POINT('Ctrl Pts',(3.52045328348988,1.61522066995007,-0.00118366394786523));
#19078=CARTESIAN_POINT('Ctrl Pts',(3.3816469894381,-0.552060840994624,-0.0263068037111615));
#19079=CARTESIAN_POINT('Ctrl Pts',(3.3816469894381,1.61522066995007,-0.0263068037111615));
#19080=CARTESIAN_POINT('Ctrl Pts',(3.2451100102617,-0.552060840994624,-0.0214179570895094));
#19081=CARTESIAN_POINT('Ctrl Pts',(3.2451100102617,1.61522066995007,-0.0214179570895094));
#19082=CARTESIAN_POINT('Ctrl Pts',(3.12452733970665,-0.552060840994624,
0.0241851999814078));
#19083=CARTESIAN_POINT('Ctrl Pts',(3.12452733970665,1.61522066995007,0.0241851999814078));
#19084=CARTESIAN_POINT('Ctrl Pts',(3.03063129752059,-0.552060840994624,
0.119017371327004));
#19085=CARTESIAN_POINT('Ctrl Pts',(3.03063129752059,1.61522066995007,0.119017371327004));
#19086=CARTESIAN_POINT('Ctrl Pts',(2.96639254265844,-0.552060840994624,
0.262319630540593));
#19087=CARTESIAN_POINT('Ctrl Pts',(2.96639254265844,1.61522066995007,0.262319630540593));
#19088=CARTESIAN_POINT('Ctrl Pts',(2.92780415844446,-0.552060840994624,
0.444963858672424));
#19089=CARTESIAN_POINT('Ctrl Pts',(2.92780415844446,1.61522066995007,0.444963858672424));
#19090=CARTESIAN_POINT('Ctrl Pts',(2.90717911786689,-0.552060840994624,
0.65402023086958));
#19091=CARTESIAN_POINT('Ctrl Pts',(2.90717911786689,1.61522066995007,0.65402023086958));
#19092=CARTESIAN_POINT('Ctrl Pts',(2.89547076625581,-0.552060840994624,
0.875890304828918));
#19093=CARTESIAN_POINT('Ctrl Pts',(2.89547076625581,1.61522066995007,0.875890304828918));
#19094=CARTESIAN_POINT('Ctrl Pts',(2.88537704766906,-0.552060840994624,
1.10060381648398));
#19095=CARTESIAN_POINT('Ctrl Pts',(2.88537704766906,1.61522066995007,1.10060381648398));
#19096=CARTESIAN_POINT('Ctrl Pts',(2.8728456296504,-0.552060840994624,1.32371934078733));
#19097=CARTESIAN_POINT('Ctrl Pts',(2.8728456296504,1.61522066995007,1.32371934078733));
#19098=CARTESIAN_POINT('Ctrl Pts',(2.85578261679345,-0.552060840994624,
1.54401727992264));
#19099=CARTESIAN_POINT('Ctrl Pts',(2.85578261679345,1.61522066995007,1.54401727992264));
#19100=CARTESIAN_POINT('Ctrl Pts',(2.83335686249019,-0.552060840994624,
1.76209503442146));
#19101=CARTESIAN_POINT('Ctrl Pts',(2.83335686249019,1.61522066995007,1.76209503442146));
#19102=CARTESIAN_POINT('Ctrl Pts',(2.80505146480345,-0.552060840994624,
1.97856787413951));
#19103=CARTESIAN_POINT('Ctrl Pts',(2.80505146480345,1.61522066995007,1.97856787413951));
#19104=CARTESIAN_POINT('Ctrl Pts',(2.76985908233915,-0.552060840994624,
2.19251877196071));
#19105=CARTESIAN_POINT('Ctrl Pts',(2.76985908233915,1.61522066995007,2.19251877196071));
#19106=CARTESIAN_POINT('Ctrl Pts',(2.72531955636536,-0.552060840994624,
2.39962532458029));
#19107=CARTESIAN_POINT('Ctrl Pts',(2.72531955636536,1.61522066995007,2.39962532458029));
#19108=CARTESIAN_POINT('Ctrl Pts',(2.66797634363184,-0.552060840994624,
2.59347738935741));
#19109=CARTESIAN_POINT('Ctrl Pts',(2.66797634363184,1.61522066995007,2.59347738935741));
#19110=CARTESIAN_POINT('Ctrl Pts',(2.59397540849171,-0.552060840994624,
2.7672283971178));
#19111=CARTESIAN_POINT('Ctrl Pts',(2.59397540849171,1.61522066995007,2.7672283971178));
#19112=CARTESIAN_POINT('Ctrl Pts',(2.49960870420485,-0.552060840994624,
2.91510580081997));
#19113=CARTESIAN_POINT('Ctrl Pts',(2.49960870420485,1.61522066995007,2.91510580081997));
#19114=CARTESIAN_POINT('Ctrl Pts',(2.38189256086504,-0.552060840994624,
3.03403241435618));
#19115=CARTESIAN_POINT('Ctrl Pts',(2.38189256086504,1.61522066995007,3.03403241435618));
#19116=CARTESIAN_POINT('Ctrl Pts',(2.23909845280558,-0.552060840994624,
3.12505646843308));
#19117=CARTESIAN_POINT('Ctrl Pts',(2.23909845280558,1.61522066995007,3.12505646843308));
#19118=CARTESIAN_POINT('Ctrl Pts',(2.07061055216582,-0.552060840994624,
3.19196918412265));
#19119=CARTESIAN_POINT('Ctrl Pts',(2.07061055216582,1.61522066995007,3.19196918412265));
#19120=CARTESIAN_POINT('Ctrl Pts',(1.87681490437036,-0.552060840994624,
3.24001322621211));
#19121=CARTESIAN_POINT('Ctrl Pts',(1.87681490437036,1.61522066995007,3.24001322621211));
#19122=CARTESIAN_POINT('Ctrl Pts',(1.65897747541321,-0.552060840994624,
3.27464765209773));
#19123=CARTESIAN_POINT('Ctrl Pts',(1.65897747541321,1.61522066995007,3.27464765209773));
#19124=CARTESIAN_POINT('Ctrl Pts',(1.4191255439272,-0.552060840994624,3.30006519349576));
#19125=CARTESIAN_POINT('Ctrl Pts',(1.4191255439272,1.61522066995007,3.30006519349576));
#19126=CARTESIAN_POINT('Ctrl Pts',(1.15993538533448,-0.552060840994624,
3.31897283641381));
#19127=CARTESIAN_POINT('Ctrl Pts',(1.15993538533448,1.61522066995007,3.31897283641381));
#19128=CARTESIAN_POINT('Ctrl Pts',(0.884625090385968,-0.552060840994624,
3.33300441174764));
#19129=CARTESIAN_POINT('Ctrl Pts',(0.884625090385968,1.61522066995007,3.33300441174764));
#19130=CARTESIAN_POINT('Ctrl Pts',(0.596845720618978,-0.552060840994624,
3.34293392264922));
#19131=CARTESIAN_POINT('Ctrl Pts',(0.596845720618978,1.61522066995007,3.34293392264922));
#19132=CARTESIAN_POINT('Ctrl Pts',(0.30057321210183,-0.552060840994624,
3.34897162637417));
#19133=CARTESIAN_POINT('Ctrl Pts',(0.30057321210183,1.61522066995007,3.34897162637417));
#19134=CARTESIAN_POINT('Ctrl Pts',(1.66741620510891E-14,-0.552060840994624,
3.35102435732185));
#19135=CARTESIAN_POINT('Ctrl Pts',(1.66741620510891E-14,1.61522066995007,
3.35102435732185));
#19136=CARTESIAN_POINT('Ctrl Pts',(-0.300573212101791,-0.552060840994624,
3.34897162637426));
#19137=CARTESIAN_POINT('Ctrl Pts',(-0.300573212101791,1.61522066995007,
3.34897162637426));
#19138=CARTESIAN_POINT('Ctrl Pts',(-0.596845720618908,-0.552060840994624,
3.34293392264938));
#19139=CARTESIAN_POINT('Ctrl Pts',(-0.596845720618908,1.61522066995007,
3.34293392264938));
#19140=CARTESIAN_POINT('Ctrl Pts',(-0.884625090385886,-0.552060840994624,
3.33300441174785));
#19141=CARTESIAN_POINT('Ctrl Pts',(-0.884625090385886,1.61522066995007,
3.33300441174785));
#19142=CARTESIAN_POINT('Ctrl Pts',(-1.15993538533442,-0.552060840994624,
3.31897283641402));
#19143=CARTESIAN_POINT('Ctrl Pts',(-1.15993538533442,1.61522066995007,3.31897283641402));
#19144=CARTESIAN_POINT('Ctrl Pts',(-1.41912554392716,-0.552060840994624,
3.30006519349591));
#19145=CARTESIAN_POINT('Ctrl Pts',(-1.41912554392716,1.61522066995007,3.30006519349591));
#19146=CARTESIAN_POINT('Ctrl Pts',(-1.65897747541319,-0.552060840994624,
3.27464765209779));
#19147=CARTESIAN_POINT('Ctrl Pts',(-1.65897747541319,1.61522066995007,3.27464765209779));
#19148=CARTESIAN_POINT('Ctrl Pts',(-1.87681490437034,-0.552060840994624,
3.24001322621208));
#19149=CARTESIAN_POINT('Ctrl Pts',(-1.87681490437034,1.61522066995007,3.24001322621208));
#19150=CARTESIAN_POINT('Ctrl Pts',(-2.07061055216576,-0.552060840994624,
3.19196918412254));
#19151=CARTESIAN_POINT('Ctrl Pts',(-2.07061055216576,1.61522066995007,3.19196918412254));
#19152=CARTESIAN_POINT('Ctrl Pts',(-2.23909845280547,-0.552060840994624,
3.12505646843295));
#19153=CARTESIAN_POINT('Ctrl Pts',(-2.23909845280547,1.61522066995007,3.12505646843295));
#19154=CARTESIAN_POINT('Ctrl Pts',(-2.38189256086493,-0.552060840994624,
3.03403241435609));
#19155=CARTESIAN_POINT('Ctrl Pts',(-2.38189256086493,1.61522066995007,3.03403241435609));
#19156=CARTESIAN_POINT('Ctrl Pts',(-2.49960870420481,-0.552060840994624,
2.91510580081997));
#19157=CARTESIAN_POINT('Ctrl Pts',(-2.49960870420481,1.61522066995007,2.91510580081997));
#19158=CARTESIAN_POINT('Ctrl Pts',(-2.59397540849182,-0.552060840994624,
2.76722839711793));
#19159=CARTESIAN_POINT('Ctrl Pts',(-2.59397540849182,1.61522066995007,2.76722839711793));
#19160=CARTESIAN_POINT('Ctrl Pts',(-2.66797634363209,-0.552060840994624,
2.59347738935767));
#19161=CARTESIAN_POINT('Ctrl Pts',(-2.66797634363209,1.61522066995007,2.59347738935767));
#19162=CARTESIAN_POINT('Ctrl Pts',(-2.72531955636566,-0.552060840994624,
2.39962532458057));
#19163=CARTESIAN_POINT('Ctrl Pts',(-2.72531955636566,1.61522066995007,2.39962532458057));
#19164=CARTESIAN_POINT('Ctrl Pts',(-2.76985908233936,-0.552060840994624,
2.19251877196088));
#19165=CARTESIAN_POINT('Ctrl Pts',(-2.76985908233936,1.61522066995007,2.19251877196088));
#19166=CARTESIAN_POINT('Ctrl Pts',(-2.80505146480344,-0.552060840994624,
1.97856787413951));
#19167=CARTESIAN_POINT('Ctrl Pts',(-2.80505146480344,1.61522066995007,1.97856787413951));
#19168=CARTESIAN_POINT('Ctrl Pts',(-2.8333568624899,-0.552060840994624,
1.76209503442131));
#19169=CARTESIAN_POINT('Ctrl Pts',(-2.8333568624899,1.61522066995007,1.76209503442131));
#19170=CARTESIAN_POINT('Ctrl Pts',(-2.85578261679294,-0.552060840994624,
1.54401727992238));
#19171=CARTESIAN_POINT('Ctrl Pts',(-2.85578261679294,1.61522066995007,1.54401727992238));
#19172=CARTESIAN_POINT('Ctrl Pts',(-2.87284562964987,-0.552060840994624,
1.32371934078708));
#19173=CARTESIAN_POINT('Ctrl Pts',(-2.87284562964987,1.61522066995007,1.32371934078708));
#19174=CARTESIAN_POINT('Ctrl Pts',(-2.88537704766869,-0.552060840994624,
1.10060381648384));
#19175=CARTESIAN_POINT('Ctrl Pts',(-2.88537704766869,1.61522066995007,1.10060381648384));
#19176=CARTESIAN_POINT('Ctrl Pts',(-2.89547076625573,-0.552060840994624,
0.875890304828914));
#19177=CARTESIAN_POINT('Ctrl Pts',(-2.89547076625573,1.61522066995007,0.875890304828914));
#19178=CARTESIAN_POINT('Ctrl Pts',(-2.90717911786707,-0.552060840994624,
0.654020230869684));
#19179=CARTESIAN_POINT('Ctrl Pts',(-2.90717911786707,1.61522066995007,0.654020230869684));
#19180=CARTESIAN_POINT('Ctrl Pts',(-2.92780415844476,-0.552060840994624,
0.444963858672577));
#19181=CARTESIAN_POINT('Ctrl Pts',(-2.92780415844476,1.61522066995007,0.444963858672577));
#19182=CARTESIAN_POINT('Ctrl Pts',(-2.96639254265869,-0.552060840994624,
0.262319630540737));
#19183=CARTESIAN_POINT('Ctrl Pts',(-2.96639254265869,1.61522066995007,0.262319630540737));
#19184=CARTESIAN_POINT('Ctrl Pts',(-3.03063129752067,-0.552060840994624,
0.11901737132707));
#19185=CARTESIAN_POINT('Ctrl Pts',(-3.03063129752067,1.61522066995007,0.11901737132707));
#19186=CARTESIAN_POINT('Ctrl Pts',(-3.12452733970658,-0.552060840994624,
0.0241851999813871));
#19187=CARTESIAN_POINT('Ctrl Pts',(-3.12452733970658,1.61522066995007,0.0241851999813871));
#19188=CARTESIAN_POINT('Ctrl Pts',(-3.24511001026157,-0.552060840994624,
-0.0214179570895714));
#19189=CARTESIAN_POINT('Ctrl Pts',(-3.24511001026157,1.61522066995007,-0.0214179570895714));
#19190=CARTESIAN_POINT('Ctrl Pts',(-3.38164698943802,-0.552060840994624,
-0.0263068037112043));
#19191=CARTESIAN_POINT('Ctrl Pts',(-3.38164698943802,1.61522066995007,-0.0263068037112043));
#19192=CARTESIAN_POINT('Ctrl Pts',(-3.52045328348989,-0.552060840994624,
-0.00118366394785932));
#19193=CARTESIAN_POINT('Ctrl Pts',(-3.52045328348989,1.61522066995007,-0.00118366394785932));
#19194=CARTESIAN_POINT('Ctrl Pts',(-3.64881642260079,-0.552060840994624,
0.0470540298718583));
#19195=CARTESIAN_POINT('Ctrl Pts',(-3.64881642260079,1.61522066995007,0.0470540298718583));
#19196=CARTESIAN_POINT('Ctrl Pts',(-3.75872318140663,-0.552060840994624,
0.120497232333251));
#19197=CARTESIAN_POINT('Ctrl Pts',(-3.75872318140663,1.61522066995007,0.120497232333251));
#19198=CARTESIAN_POINT('Ctrl Pts',(-3.84598208672296,-0.552060840994624,
0.224659532804408));
#19199=CARTESIAN_POINT('Ctrl Pts',(-3.84598208672296,1.61522066995007,0.224659532804408));
#19200=CARTESIAN_POINT('Ctrl Pts',(-3.9098657241983,-0.552060840994624,
0.364350357241515));
#19201=CARTESIAN_POINT('Ctrl Pts',(-3.9098657241983,1.61522066995007,0.364350357241515));
#19202=CARTESIAN_POINT('Ctrl Pts',(-3.9525920016999,-0.552060840994624,
0.538436816836325));
#19203=CARTESIAN_POINT('Ctrl Pts',(-3.9525920016999,1.61522066995007,0.538436816836325));
#19204=CARTESIAN_POINT('Ctrl Pts',(-3.97841403016126,-0.552060840994624,
0.741129277895169));
#19205=CARTESIAN_POINT('Ctrl Pts',(-3.97841403016126,1.61522066995007,0.741129277895169));
#19206=CARTESIAN_POINT('Ctrl Pts',(-3.99260375067011,-0.552060840994624,
0.964078729991154));
#19207=CARTESIAN_POINT('Ctrl Pts',(-3.99260375067011,1.61522066995007,0.964078729991154));
#19208=CARTESIAN_POINT('Ctrl Pts',(-4.00047520099045,-0.552060840994624,
1.1981954227983));
#19209=CARTESIAN_POINT('Ctrl Pts',(-4.00047520099045,1.61522066995007,1.1981954227983));
#19210=CARTESIAN_POINT('Ctrl Pts',(-4.00639322616607,-0.552060840994624,
1.43558101932923));
#19211=CARTESIAN_POINT('Ctrl Pts',(-4.00639322616607,1.61522066995007,1.43558101932923));
#19212=CARTESIAN_POINT('Ctrl Pts',(-4.01278239926574,-0.552060840994624,
1.67142113207667));
#19213=CARTESIAN_POINT('Ctrl Pts',(-4.01278239926574,1.61522066995007,1.67142113207667));
#19214=CARTESIAN_POINT('Ctrl Pts',(-4.02066709528487,-0.552060840994624,
1.90332556813333));
#19215=CARTESIAN_POINT('Ctrl Pts',(-4.02066709528487,1.61522066995007,1.90332556813333));
#19216=CARTESIAN_POINT('Ctrl Pts',(-4.0302101444685,-0.552060840994624,
2.130657485557));
#19217=CARTESIAN_POINT('Ctrl Pts',(-4.0302101444685,1.61522066995007,2.130657485557));
#19218=CARTESIAN_POINT('Ctrl Pts',(-4.04126813644779,-0.552060840994624,
2.35385258470204));
#19219=CARTESIAN_POINT('Ctrl Pts',(-4.04126813644779,1.61522066995007,2.35385258470204));
#19220=CARTESIAN_POINT('Ctrl Pts',(-4.05390260344525,-0.552060840994624,
2.57377631141659));
#19221=CARTESIAN_POINT('Ctrl Pts',(-4.05390260344525,1.61522066995007,2.57377631141659));
#19222=CARTESIAN_POINT('Ctrl Pts',(-4.06899962712502,-0.552060840994624,
2.7909834104825));
#19223=CARTESIAN_POINT('Ctrl Pts',(-4.06899962712502,1.61522066995007,2.7909834104825));
#19224=CARTESIAN_POINT('Ctrl Pts',(-4.08854433447739,-0.552060840994624,
3.00529120729338));
#19225=CARTESIAN_POINT('Ctrl Pts',(-4.08854433447739,1.61522066995007,3.00529120729338));
#19226=CARTESIAN_POINT('Ctrl Pts',(-4.11518318246524,-0.552060840994624,
3.21600287470921));
#19227=CARTESIAN_POINT('Ctrl Pts',(-4.11518318246524,1.61522066995007,3.21600287470921));
#19228=CARTESIAN_POINT('Ctrl Pts',(-4.15193466045748,-0.552060840994624,
3.42199345348447));
#19229=CARTESIAN_POINT('Ctrl Pts',(-4.15193466045748,1.61522066995007,3.42199345348447));
#19230=CARTESIAN_POINT('Ctrl Pts',(-4.20184334854115,-0.552060840994624,
3.62185203209171));
#19231=CARTESIAN_POINT('Ctrl Pts',(-4.20184334854115,1.61522066995007,3.62185203209171));
#19232=CARTESIAN_POINT('Ctrl Pts',(-4.26765207024395,-0.552060840994624,
3.81399668859083));
#19233=CARTESIAN_POINT('Ctrl Pts',(-4.26765207024395,1.61522066995007,3.81399668859083));
#19234=CARTESIAN_POINT('Ctrl Pts',(-4.35148411330718,-0.552060840994624,
3.99681013615577));
#19235=CARTESIAN_POINT('Ctrl Pts',(-4.35148411330718,1.61522066995007,3.99681013615577));
#19236=CARTESIAN_POINT('Ctrl Pts',(-4.45474519640294,-0.552060840994624,
4.16885849319142));
#19237=CARTESIAN_POINT('Ctrl Pts',(-4.45474519640294,1.61522066995007,4.16885849319142));
#19238=CARTESIAN_POINT('Ctrl Pts',(-4.57800047823775,-0.552060840994624,
4.32911151507774));
#19239=CARTESIAN_POINT('Ctrl Pts',(-4.57800047823775,1.61522066995007,4.32911151507774));
#19240=CARTESIAN_POINT('Ctrl Pts',(-4.7208720035032,-0.552060840994624,
4.47714872481861));
#19241=CARTESIAN_POINT('Ctrl Pts',(-4.7208720035032,1.61522066995007,4.47714872481861));
#19242=CARTESIAN_POINT('Ctrl Pts',(-4.88190185104852,-0.552060840994624,
4.61340315498244));
#19243=CARTESIAN_POINT('Ctrl Pts',(-4.88190185104852,1.61522066995007,4.61340315498244));
#19244=CARTESIAN_POINT('Ctrl Pts',(-5.05850630701885,-0.552060840994624,
4.73929437247796));
#19245=CARTESIAN_POINT('Ctrl Pts',(-5.05850630701885,1.61522066995007,4.73929437247796));
#19246=CARTESIAN_POINT('Ctrl Pts',(-5.24741086000019,-0.552060840994624,
4.8567611153285));
#19247=CARTESIAN_POINT('Ctrl Pts',(-5.24741086000019,1.61522066995007,4.8567611153285));
#19248=CARTESIAN_POINT('Ctrl Pts',(-5.44501860313342,-0.552060840994624,
4.96787993373728));
#19249=CARTESIAN_POINT('Ctrl Pts',(-5.44501860313342,1.61522066995007,4.96787993373728));
#19250=CARTESIAN_POINT('Ctrl Pts',(-5.64781737380319,-0.552060840994624,
5.07442896098937));
#19251=CARTESIAN_POINT('Ctrl Pts',(-5.64781737380319,1.61522066995007,5.07442896098937));
#19252=CARTESIAN_POINT('Ctrl Pts',(-5.85274048349242,-0.552060840994624,
5.17752467829109));
#19253=CARTESIAN_POINT('Ctrl Pts',(-5.85274048349242,1.61522066995007,5.17752467829109));
#19254=CARTESIAN_POINT('Ctrl Pts',(-6.05762450882858,-0.552060840994624,
5.27709955371564));
#19255=CARTESIAN_POINT('Ctrl Pts',(-6.05762450882858,1.61522066995007,5.27709955371564));
#19256=CARTESIAN_POINT('Ctrl Pts',(-6.26112587698772,-0.552060840994624,
5.37226655127787));
#19257=CARTESIAN_POINT('Ctrl Pts',(-6.26112587698772,1.61522066995007,5.37226655127787));
#19258=CARTESIAN_POINT('Ctrl Pts',(-6.46246210121964,-0.552060840994624,
5.46195513100446));
#19259=CARTESIAN_POINT('Ctrl Pts',(-6.46246210121964,1.61522066995007,5.46195513100446));
#19260=CARTESIAN_POINT('Ctrl Pts',(-6.66121503090592,-0.552060840994624,
5.54547963906637));
#19261=CARTESIAN_POINT('Ctrl Pts',(-6.66121503090592,1.61522066995007,5.54547963906637));
#19262=CARTESIAN_POINT('Ctrl Pts',(-6.8570997603751,-0.552060840994624,
5.62308582598972));
#19263=CARTESIAN_POINT('Ctrl Pts',(-6.8570997603751,1.61522066995007,5.62308582598972));
#19264=CARTESIAN_POINT('Ctrl Pts',(-7.04976847947249,-0.552060840994624,
5.69662713609756));
#19265=CARTESIAN_POINT('Ctrl Pts',(-7.04976847947249,1.61522066995007,5.69662713609756));
#19266=CARTESIAN_POINT('Ctrl Pts',(-7.23853768475,-0.552060840994624,5.76979878895672));
#19267=CARTESIAN_POINT('Ctrl Pts',(-7.23853768475,1.61522066995007,5.76979878895672));
#19268=CARTESIAN_POINT('Ctrl Pts',(-7.42198551710617,-0.552060840994624,
5.84723737025949));
#19269=CARTESIAN_POINT('Ctrl Pts',(-7.42198551710617,1.61522066995007,5.84723737025949));
#19270=CARTESIAN_POINT('Ctrl Pts',(-7.59751903688412,-0.552060840994624,
5.93381436957244));
#19271=CARTESIAN_POINT('Ctrl Pts',(-7.59751903688412,1.61522066995007,5.93381436957244));
#19272=CARTESIAN_POINT('Ctrl Pts',(-7.76106756457753,-0.552060840994624,
6.03389995867283));
#19273=CARTESIAN_POINT('Ctrl Pts',(-7.76106756457753,1.61522066995007,6.03389995867283));
#19274=CARTESIAN_POINT('Ctrl Pts',(-7.90644860448901,-0.552060840994624,
6.15052660592937));
#19275=CARTESIAN_POINT('Ctrl Pts',(-7.90644860448901,1.61522066995007,6.15052660592937));
#19276=CARTESIAN_POINT('Ctrl Pts',(-8.02580908828117,-0.552060840994624,
6.28498018271686));
#19277=CARTESIAN_POINT('Ctrl Pts',(-8.02580908828117,1.61522066995007,6.28498018271686));
#19278=CARTESIAN_POINT('Ctrl Pts',(-8.11207116917861,-0.552060840994624,
6.43720976255636));
#19279=CARTESIAN_POINT('Ctrl Pts',(-8.11207116917861,1.61522066995007,6.43720976255636));
#19280=CARTESIAN_POINT('Ctrl Pts',(-8.16089752265956,-0.552060840994624,
6.60605451948903));
#19281=CARTESIAN_POINT('Ctrl Pts',(-8.16089752265956,1.61522066995007,6.60605451948903));
#19282=CARTESIAN_POINT('Ctrl Pts',(-8.17293082304181,-0.552060840994624,
6.78954489191904));
#19283=CARTESIAN_POINT('Ctrl Pts',(-8.17293082304181,1.61522066995007,6.78954489191904));
#19284=CARTESIAN_POINT('Ctrl Pts',(-8.15569042861244,-0.552060840994624,
6.9851692342788));
#19285=CARTESIAN_POINT('Ctrl Pts',(-8.15569042861244,1.61522066995007,6.9851692342788));
#19286=CARTESIAN_POINT('Ctrl Pts',(-8.12057943633387,-0.552060840994624,
7.19009032473164));
#19287=CARTESIAN_POINT('Ctrl Pts',(-8.12057943633387,1.61522066995007,7.19009032473164));
#19288=CARTESIAN_POINT('Ctrl Pts',(-8.08008348678073,-0.552060840994624,
7.40136016279791));
#19289=CARTESIAN_POINT('Ctrl Pts',(-8.08008348678073,1.61522066995007,7.40136016279791));
#19290=CARTESIAN_POINT('Ctrl Pts',(-8.04494633492831,-0.552060840994624,
7.61613341658677));
#19291=CARTESIAN_POINT('Ctrl Pts',(-8.04494633492831,1.61522066995007,7.61613341658677));
#19292=CARTESIAN_POINT('Ctrl Pts',(-8.02124364536279,-0.552060840994624,
7.83188673232793));
#19293=CARTESIAN_POINT('Ctrl Pts',(-8.02124364536279,1.61522066995007,7.83188673232793));
#19294=CARTESIAN_POINT('Ctrl Pts',(-8.007818938056,-0.552060840994624,8.04662057355248));
#19295=CARTESIAN_POINT('Ctrl Pts',(-8.007818938056,1.61522066995007,8.04662057355248));
#19296=CARTESIAN_POINT('Ctrl Pts',(-7.99879843919661,-0.552060840994624,
8.25883677791483));
#19297=CARTESIAN_POINT('Ctrl Pts',(-7.99879843919661,1.61522066995007,8.25883677791483));
#19298=CARTESIAN_POINT('Ctrl Pts',(-7.98575825096101,-0.552060840994624,
8.46752658699528));
#19299=CARTESIAN_POINT('Ctrl Pts',(-7.98575825096101,1.61522066995007,8.46752658699528));
#19300=CARTESIAN_POINT('Ctrl Pts',(-7.96007609558389,-0.552060840994624,
8.67216210283896));
#19301=CARTESIAN_POINT('Ctrl Pts',(-7.96007609558389,1.61522066995007,8.67216210283896));
#19302=CARTESIAN_POINT('Ctrl Pts',(-7.91508259073019,-0.552060840994624,
8.87266947141823));
#19303=CARTESIAN_POINT('Ctrl Pts',(-7.91508259073019,1.61522066995007,8.87266947141823));
#19304=CARTESIAN_POINT('Ctrl Pts',(-7.84862074946261,-0.552060840994624,
9.06945407016992));
#19305=CARTESIAN_POINT('Ctrl Pts',(-7.84862074946261,1.61522066995007,9.06945407016992));
#19306=CARTESIAN_POINT('Ctrl Pts',(-7.76209282457479,-0.552060840994624,
9.26297089919765));
#19307=CARTESIAN_POINT('Ctrl Pts',(-7.76209282457479,1.61522066995007,9.26297089919765));
#19308=CARTESIAN_POINT('Ctrl Pts',(-7.65900038660722,-0.552060840994624,
9.4532499945042));
#19309=CARTESIAN_POINT('Ctrl Pts',(-7.65900038660722,1.61522066995007,9.4532499945042));
#19310=CARTESIAN_POINT('Ctrl Pts',(-7.5436057352653,-0.552060840994624,
9.63939026966035));
#19311=CARTESIAN_POINT('Ctrl Pts',(-7.5436057352653,1.61522066995007,9.63939026966035));
#19312=CARTESIAN_POINT('Ctrl Pts',(-7.41967047355001,-0.552060840994624,
9.81917361987397));
#19313=CARTESIAN_POINT('Ctrl Pts',(-7.41967047355001,1.61522066995007,9.81917361987397));
#19314=CARTESIAN_POINT('Ctrl Pts',(-7.28883796912703,-0.552060840994624,
9.98835756998572));
#19315=CARTESIAN_POINT('Ctrl Pts',(-7.28883796912703,1.61522066995007,9.98835756998572));
#19316=CARTESIAN_POINT('Ctrl Pts',(-7.15081550722306,-0.552060840994624,
10.1414720974148));
#19317=CARTESIAN_POINT('Ctrl Pts',(-7.15081550722306,1.61522066995007,10.1414720974148));
#19318=CARTESIAN_POINT('Ctrl Pts',(-7.0044544864105,-0.552060840994624,
10.2733319413008));
#19319=CARTESIAN_POINT('Ctrl Pts',(-7.0044544864105,1.61522066995007,10.2733319413008));
#19320=CARTESIAN_POINT('Ctrl Pts',(-6.84859008776113,-0.552060840994624,
10.3804015453596));
#19321=CARTESIAN_POINT('Ctrl Pts',(-6.84859008776113,1.61522066995007,10.3804015453596));
#19322=CARTESIAN_POINT('Ctrl Pts',(-6.68288828293938,-0.552060840994624,
10.4620502678778));
#19323=CARTESIAN_POINT('Ctrl Pts',(-6.68288828293938,1.61522066995007,10.4620502678778));
#19324=CARTESIAN_POINT('Ctrl Pts',(-6.50892555577766,-0.552060840994624,
10.522290883026));
#19325=CARTESIAN_POINT('Ctrl Pts',(-6.50892555577766,1.61522066995007,10.522290883026));
#19326=CARTESIAN_POINT('Ctrl Pts',(-6.32976796473811,-0.552060840994624,
10.5687216653902));
#19327=CARTESIAN_POINT('Ctrl Pts',(-6.32976796473811,1.61522066995007,10.5687216653902));
#19328=CARTESIAN_POINT('Ctrl Pts',(-6.14893768388701,-0.552060840994624,
10.6103475969885));
#19329=CARTESIAN_POINT('Ctrl Pts',(-6.14893768388701,1.61522066995007,10.6103475969885));
#19330=CARTESIAN_POINT('Ctrl Pts',(-5.96961932707142,-0.552060840994624,
10.6558377434043));
#19331=CARTESIAN_POINT('Ctrl Pts',(-5.96961932707142,1.61522066995007,10.6558377434043));
#19332=CARTESIAN_POINT('Ctrl Pts',(-5.79367695415031,-0.552060840994624,
10.7114411549114));
#19333=CARTESIAN_POINT('Ctrl Pts',(-5.79367695415031,1.61522066995007,10.7114411549114));
#19334=CARTESIAN_POINT('Ctrl Pts',(-5.62101499943431,-0.552060840994624,
10.7795199127535));
#19335=CARTESIAN_POINT('Ctrl Pts',(-5.62101499943431,1.61522066995007,10.7795199127535));
#19336=CARTESIAN_POINT('Ctrl Pts',(-5.45051506148982,-0.552060840994624,
10.8599381259737));
#19337=CARTESIAN_POINT('Ctrl Pts',(-5.45051506148982,1.61522066995007,10.8599381259737));
#19338=CARTESIAN_POINT('Ctrl Pts',(-5.28082876351929,-0.552060840994624,
10.9511663773826));
#19339=CARTESIAN_POINT('Ctrl Pts',(-5.28082876351929,1.61522066995007,10.9511663773826));
#19340=CARTESIAN_POINT('Ctrl Pts',(-5.11112998264616,-0.552060840994624,
11.0513704191329));
#19341=CARTESIAN_POINT('Ctrl Pts',(-5.11112998264616,1.61522066995007,11.0513704191329));
#19342=CARTESIAN_POINT('Ctrl Pts',(-4.94211773226973,-0.552060840994624,
11.1598106424589));
#19343=CARTESIAN_POINT('Ctrl Pts',(-4.94211773226973,1.61522066995007,11.1598106424589));
#19344=CARTESIAN_POINT('Ctrl Pts',(-4.77596612414951,-0.552060840994624,
11.2768795166235));
#19345=CARTESIAN_POINT('Ctrl Pts',(-4.77596612414951,1.61522066995007,11.2768795166235));
#19346=CARTESIAN_POINT('Ctrl Pts',(-4.61532593596946,-0.552060840994624,
11.4029224160731));
#19347=CARTESIAN_POINT('Ctrl Pts',(-4.61532593596946,1.61522066995007,11.4029224160731));
#19348=CARTESIAN_POINT('Ctrl Pts',(-4.46255574628757,-0.552060840994624,
11.5373242211527));
#19349=CARTESIAN_POINT('Ctrl Pts',(-4.46255574628757,1.61522066995007,11.5373242211527));
#19350=CARTESIAN_POINT('Ctrl Pts',(-4.31893584999241,-0.552060840994624,
11.6776492463597));
#19351=CARTESIAN_POINT('Ctrl Pts',(-4.31893584999241,1.61522066995007,11.6776492463597));
#19352=CARTESIAN_POINT('Ctrl Pts',(-4.18369962429796,-0.552060840994624,
11.8183570873721));
#19353=CARTESIAN_POINT('Ctrl Pts',(-4.18369962429796,1.61522066995007,11.8183570873721));
#19354=CARTESIAN_POINT('Ctrl Pts',(-4.05395481372655,-0.552060840994624,
11.9514202619522));
#19355=CARTESIAN_POINT('Ctrl Pts',(-4.05395481372655,1.61522066995007,11.9514202619522));
#19356=CARTESIAN_POINT('Ctrl Pts',(-3.92533033057354,-0.552060840994624,
12.0684942936867));
#19357=CARTESIAN_POINT('Ctrl Pts',(-3.92533033057354,1.61522066995007,12.0684942936867));
#19358=CARTESIAN_POINT('Ctrl Pts',(-3.79241297762166,-0.552060840994624,
12.1626050652586));
#19359=CARTESIAN_POINT('Ctrl Pts',(-3.79241297762166,1.61522066995007,12.1626050652586));
#19360=CARTESIAN_POINT('Ctrl Pts',(-3.64927048315908,-0.552060840994624,
12.2301117722809));
#19361=CARTESIAN_POINT('Ctrl Pts',(-3.64927048315908,1.61522066995007,12.2301117722809));
#19362=CARTESIAN_POINT('Ctrl Pts',(-3.48993681214334,-0.552060840994624,
12.2723364229645));
#19363=CARTESIAN_POINT('Ctrl Pts',(-3.48993681214334,1.61522066995007,12.2723364229645));
#19364=CARTESIAN_POINT('Ctrl Pts',(-3.30884480305534,-0.552060840994624,
12.2938762651139));
#19365=CARTESIAN_POINT('Ctrl Pts',(-3.30884480305534,1.61522066995007,12.2938762651139));
#19366=CARTESIAN_POINT('Ctrl Pts',(-3.10127560868576,-0.552060840994624,
12.3010487961981));
#19367=CARTESIAN_POINT('Ctrl Pts',(-3.10127560868576,1.61522066995007,12.3010487961981));
#19368=CARTESIAN_POINT('Ctrl Pts',(-2.86376302967345,-0.552060840994624,
12.300400839059));
#19369=CARTESIAN_POINT('Ctrl Pts',(-2.86376302967345,1.61522066995007,12.300400839059));
#19370=CARTESIAN_POINT('Ctrl Pts',(-2.59461297443094,-0.552060840994624,
12.2969132923574));
#19371=CARTESIAN_POINT('Ctrl Pts',(-2.59461297443094,1.61522066995007,12.2969132923574));
#19372=CARTESIAN_POINT('Ctrl Pts',(-2.29394197380209,-0.552060840994624,
12.2935845551224));
#19373=CARTESIAN_POINT('Ctrl Pts',(-2.29394197380209,1.61522066995007,12.2935845551224));
#19374=CARTESIAN_POINT('Ctrl Pts',(-1.96338745719135,-0.552060840994624,
12.2919684497906));
#19375=CARTESIAN_POINT('Ctrl Pts',(-1.96338745719135,1.61522066995007,12.2919684497906));
#19376=CARTESIAN_POINT('Ctrl Pts',(-1.60591558979456,-0.552060840994624,
12.2924280531798));
#19377=CARTESIAN_POINT('Ctrl Pts',(-1.60591558979456,1.61522066995007,12.2924280531798));
#19378=CARTESIAN_POINT('Ctrl Pts',(-1.22558901314075,-0.552060840994624,
12.2945066442122));
#19379=CARTESIAN_POINT('Ctrl Pts',(-1.22558901314075,1.61522066995007,12.2945066442122));
#19380=CARTESIAN_POINT('Ctrl Pts',(-0.827351903312651,-0.552060840994624,
12.2972483292773));
#19381=CARTESIAN_POINT('Ctrl Pts',(-0.827351903312651,1.61522066995007,
12.2972483292773));
#19382=CARTESIAN_POINT('Ctrl Pts',(-0.498916532526571,-0.552060840994624,
12.299081889758));
#19383=CARTESIAN_POINT('Ctrl Pts',(-0.498916532526571,1.61522066995007,
12.299081889758));
#19384=CARTESIAN_POINT('Ctrl Pts',(-0.249771440080693,-0.552060840994624,
12.2998330708668));
#19385=CARTESIAN_POINT('Ctrl Pts',(-0.249771440080693,1.61522066995007,
12.2998330708668));
#19386=CARTESIAN_POINT('Ctrl Pts',(-0.0832571466935557,-0.552060840994624,
12.2999999999989));
#19387=CARTESIAN_POINT('Ctrl Pts',(-0.0832571466935557,1.61522066995007,
12.2999999999989));
#19388=CARTESIAN_POINT('Ctrl Pts',(0.,-0.552060840994624,12.3));
#19389=CARTESIAN_POINT('Ctrl Pts',(0.,1.61522066995007,12.3));
#19390=CARTESIAN_POINT('Ctrl Pts',(0.0832571466935396,-0.552060840994624,
12.3000000000011));
#19391=CARTESIAN_POINT('Ctrl Pts',(0.0832571466935396,1.61522066995007,
12.3000000000011));
#19392=CARTESIAN_POINT('Ctrl Pts',(0.24977144008061,-0.552060840994624,
12.2998330708736));
#19393=CARTESIAN_POINT('Ctrl Pts',(0.24977144008061,1.61522066995007,12.2998330708736));
#19394=CARTESIAN_POINT('Ctrl Pts',(0.498916532526534,-0.552060840994624,
12.2990818897713));
#19395=CARTESIAN_POINT('Ctrl Pts',(0.498916532526534,1.61522066995007,12.2990818897713));
#19396=CARTESIAN_POINT('Ctrl Pts',(0.827351903312438,-0.552060840994624,
12.2972483292974));
#19397=CARTESIAN_POINT('Ctrl Pts',(0.827351903312438,1.61522066995007,12.2972483292974));
#19398=CARTESIAN_POINT('Ctrl Pts',(1.22558901314046,-0.552060840994624,
12.2945066442369));
#19399=CARTESIAN_POINT('Ctrl Pts',(1.22558901314046,1.61522066995007,12.2945066442369));
#19400=CARTESIAN_POINT('Ctrl Pts',(1.60591558979418,-0.552060840994624,
12.2924280532047));
#19401=CARTESIAN_POINT('Ctrl Pts',(1.60591558979418,1.61522066995007,12.2924280532047));
#19402=CARTESIAN_POINT('Ctrl Pts',(1.96338745719096,-0.552060840994624,
12.291968449812));
#19403=CARTESIAN_POINT('Ctrl Pts',(1.96338745719096,1.61522066995007,12.291968449812));
#19404=CARTESIAN_POINT('Ctrl Pts',(2.29394197380175,-0.552060840994624,
12.2935845551378));
#19405=CARTESIAN_POINT('Ctrl Pts',(2.29394197380175,1.61522066995007,12.2935845551378));
#19406=CARTESIAN_POINT('Ctrl Pts',(2.59461297443069,-0.552060840994624,
12.2969132923658));
#19407=CARTESIAN_POINT('Ctrl Pts',(2.59461297443069,1.61522066995007,12.2969132923658));
#19408=CARTESIAN_POINT('Ctrl Pts',(2.86376302967335,-0.552060840994624,
12.3004008390612));
#19409=CARTESIAN_POINT('Ctrl Pts',(2.86376302967335,1.61522066995007,12.3004008390612));
#19410=CARTESIAN_POINT('Ctrl Pts',(3.10127560868576,-0.552060840994624,
12.3010487961961));
#19411=CARTESIAN_POINT('Ctrl Pts',(3.10127560868576,1.61522066995007,12.3010487961961));
#19412=CARTESIAN_POINT('Ctrl Pts',(3.30884480305537,-0.552060840994624,
12.2938762651102));
#19413=CARTESIAN_POINT('Ctrl Pts',(3.30884480305537,1.61522066995007,12.2938762651102));
#19414=CARTESIAN_POINT('Ctrl Pts',(3.48993681214337,-0.552060840994624,
12.2723364229612));
#19415=CARTESIAN_POINT('Ctrl Pts',(3.48993681214337,1.61522066995007,12.2723364229612));
#19416=CARTESIAN_POINT('Ctrl Pts',(3.64927048315907,-0.552060840994624,
12.2301117722792));
#19417=CARTESIAN_POINT('Ctrl Pts',(3.64927048315907,1.61522066995007,12.2301117722792));
#19418=CARTESIAN_POINT('Ctrl Pts',(3.79241297762162,-0.552060840994624,
12.1626050652587));
#19419=CARTESIAN_POINT('Ctrl Pts',(3.79241297762162,1.61522066995007,12.1626050652587));
#19420=CARTESIAN_POINT('Ctrl Pts',(3.90529123941674,-0.552060840994624,
12.0826827671148));
#19421=CARTESIAN_POINT('Ctrl Pts',(3.90529123941674,1.61522066995007,12.0826827671148));
#19422=CARTESIAN_POINT('Ctrl Pts',(3.98932418204563,-0.552060840994624,
12.0094836266392));
#19423=CARTESIAN_POINT('Ctrl Pts',(3.98932418204563,1.61522066995007,12.0094836266392));
#19424=CARTESIAN_POINT('Ctrl Pts',(4.04740991713241,-0.552060840994624,
11.9543581845679));
#19425=CARTESIAN_POINT('Ctrl Pts',(4.04740991713241,1.61522066995007,11.9543581845679));
#19426=CARTESIAN_POINT('Ctrl Pts',(4.07977092452996,-0.552060840994624,
11.9226494651812));
#19427=CARTESIAN_POINT('Ctrl Pts',(4.07977092452996,1.61522066995007,11.9226494651812));
#19428=CARTESIAN_POINT('Ctrl Pts',(4.08617023400024,-0.552060840994624,
11.9163435012344));
#19429=CARTESIAN_POINT('Ctrl Pts',(4.08617023400024,1.61522066995007,11.9163435012344));
#19430=CARTESIAN_POINT('Ctrl Pts',(4.32736007730607,0.051480639880881,11.6713697523917));
#19431=CARTESIAN_POINT('Ctrl Pts',(4.32922017460619,0.0445386622515201,
11.6695096731142));
#19432=CARTESIAN_POINT('Ctrl Pts',(4.33107905956623,0.0376012091336625,
11.6676530278345));
#19433=CARTESIAN_POINT('Ctrl Pts',(4.33293714059226,0.0306667563398385,
11.6657994729934));
#19434=CARTESIAN_POINT('Ctrl Pts',(4.3617605754817,-0.0769037671161592,
11.9026515720695));
#19435=CARTESIAN_POINT('Ctrl Pts',(4.11947753888128,0.827308835288644,11.9026515720695));
#19436=CARTESIAN_POINT('Ctrl Pts',(4.37804997056012,-0.0725390368597044,
11.8858809149492));
#19437=CARTESIAN_POINT('Ctrl Pts',(4.1357669339597,0.831673565545099,11.8858809149492));
#19438=CARTESIAN_POINT('Ctrl Pts',(4.41963045011986,-0.0613975809407722,
11.842517268502));
#19439=CARTESIAN_POINT('Ctrl Pts',(4.17734741351944,0.842815021464031,11.842517268502));
#19440=CARTESIAN_POINT('Ctrl Pts',(4.48720217786378,-0.0432917910606122,
11.7703786717735));
#19441=CARTESIAN_POINT('Ctrl Pts',(4.24491914126336,0.860920811344191,11.7703786717735));
#19442=CARTESIAN_POINT('Ctrl Pts',(4.58301627616637,-0.0176184807969185,
11.667756621275));
#19443=CARTESIAN_POINT('Ctrl Pts',(4.34073323956595,0.886594121607884,11.667756621275));
#19444=CARTESIAN_POINT('Ctrl Pts',(4.71196253429032,0.0169325649344106,
11.5373242211525));
#19445=CARTESIAN_POINT('Ctrl Pts',(4.4696794976899,0.921145167339214,11.5373242211525));
#19446=CARTESIAN_POINT('Ctrl Pts',(4.85952720599112,0.056472399548002,11.4029224160728));
#19447=CARTESIAN_POINT('Ctrl Pts',(4.6172441693907,0.960685001952805,11.4029224160728));
#19448=CARTESIAN_POINT('Ctrl Pts',(5.01469371249416,0.0980491396578512,
11.2768795166233));
#19449=CARTESIAN_POINT('Ctrl Pts',(4.77241067589374,1.00226174206265,11.2768795166233));
#19450=CARTESIAN_POINT('Ctrl Pts',(5.17518384185696,0.141052340213779,11.1598106424589));
#19451=CARTESIAN_POINT('Ctrl Pts',(4.93290080525654,1.04526494261858,11.1598106424589));
#19452=CARTESIAN_POINT('Ctrl Pts',(5.33843713945481,0.18479592946684,11.051370419133));
#19453=CARTESIAN_POINT('Ctrl Pts',(5.09615410285439,1.08900853187164,11.051370419133));
#19454=CARTESIAN_POINT('Ctrl Pts',(5.50235357458993,0.228717205887484,10.9511663773825));
#19455=CARTESIAN_POINT('Ctrl Pts',(5.26007053798951,1.13292980829229,10.9511663773825));
#19456=CARTESIAN_POINT('Ctrl Pts',(5.66625795216703,0.272635251495195,10.8599381259735));
#19457=CARTESIAN_POINT('Ctrl Pts',(5.42397491556661,1.1768478539,10.8599381259735));
#19458=CARTESIAN_POINT('Ctrl Pts',(5.83094824560827,0.31676388262402,10.7795199127532));
#19459=CARTESIAN_POINT('Ctrl Pts',(5.58866520900785,1.22097648502882,10.7795199127532));
#19460=CARTESIAN_POINT('Ctrl Pts',(5.99772688688598,0.361452084869143,10.7114411549111));
#19461=CARTESIAN_POINT('Ctrl Pts',(5.75544385028556,1.26566468727395,10.7114411549111));
#19462=CARTESIAN_POINT('Ctrl Pts',(6.16767416882911,0.406989321821667,10.6558377434042));
#19463=CARTESIAN_POINT('Ctrl Pts',(5.92539113222869,1.31120192422647,10.6558377434042));
#19464=CARTESIAN_POINT('Ctrl Pts',(6.3408824008051,0.453400327702056,10.6103475969888));
#19465=CARTESIAN_POINT('Ctrl Pts',(6.09859936420468,1.35761293010686,10.6103475969888));
#19466=CARTESIAN_POINT('Ctrl Pts',(6.51555103925432,0.50020264831757,10.5687216653907));
#19467=CARTESIAN_POINT('Ctrl Pts',(6.2732680026539,1.40441525072237,10.5687216653907));
#19468=CARTESIAN_POINT('Ctrl Pts',(6.68860398341517,0.546572044953298,10.5222908830264));
#19469=CARTESIAN_POINT('Ctrl Pts',(6.44632094681475,1.4507846473581,10.5222908830264));
#19470=CARTESIAN_POINT('Ctrl Pts',(6.8566390743923,0.591596911880709,10.462050267878));
#19471=CARTESIAN_POINT('Ctrl Pts',(6.61435603779188,1.49580951428551,10.462050267878));
#19472=CARTESIAN_POINT('Ctrl Pts',(7.01669472713225,0.634483694776415,10.3804015453596));
#19473=CARTESIAN_POINT('Ctrl Pts',(6.77441169053183,1.53869629718122,10.3804015453596));
#19474=CARTESIAN_POINT('Ctrl Pts',(7.16724817518663,0.674824369600307,10.2733319413005));
#19475=CARTESIAN_POINT('Ctrl Pts',(6.92496513858621,1.57903697200511,10.2733319413005));
#19476=CARTESIAN_POINT('Ctrl Pts',(7.30862206515146,0.71270538924723,10.1414720974144));
#19477=CARTESIAN_POINT('Ctrl Pts',(7.06633902855104,1.61691799165203,10.1414720974144));
#19478=CARTESIAN_POINT('Ctrl Pts',(7.44194152571249,0.748428231039911,9.98835756998534));
#19479=CARTESIAN_POINT('Ctrl Pts',(7.19965848911207,1.65264083344471,9.98835756998534));
#19480=CARTESIAN_POINT('Ctrl Pts',(7.56831602065279,0.782290174903054,9.81917361987377));
#19481=CARTESIAN_POINT('Ctrl Pts',(7.32603298405237,1.68650277730786,9.81917361987377));
#19482=CARTESIAN_POINT('Ctrl Pts',(7.68802829073163,0.814366980994775,9.63939026966049));
#19483=CARTESIAN_POINT('Ctrl Pts',(7.44574525413121,1.71857958339958,9.63939026966049));
#19484=CARTESIAN_POINT('Ctrl Pts',(7.79949096467857,0.844233314465072,9.45324999450471));
#19485=CARTESIAN_POINT('Ctrl Pts',(7.55720792807815,1.74844591686987,9.45324999450471));
#19486=CARTESIAN_POINT('Ctrl Pts',(7.89907061300659,0.87091560081714,9.26297089919836));
#19487=CARTESIAN_POINT('Ctrl Pts',(7.65678757640617,1.77512820322194,9.26297089919836));
#19488=CARTESIAN_POINT('Ctrl Pts',(7.98265017035093,0.893310675711308,9.06945407017055));
#19489=CARTESIAN_POINT('Ctrl Pts',(7.74036713375051,1.79752327811611,9.06945407017055));
#19490=CARTESIAN_POINT('Ctrl Pts',(8.04684737929391,0.910512266003911,8.87266947141857));
#19491=CARTESIAN_POINT('Ctrl Pts',(7.80456434269349,1.81472486840871,8.87266947141857));
#19492=CARTESIAN_POINT('Ctrl Pts',(8.09030776764722,0.922157441965925,8.67216210283894));
#19493=CARTESIAN_POINT('Ctrl Pts',(7.8480247310468,1.82637004437073,8.67216210283894));
#19494=CARTESIAN_POINT('Ctrl Pts',(8.11511482480059,0.928804472896761,8.46752658699496));
#19495=CARTESIAN_POINT('Ctrl Pts',(7.87283178820017,1.83301707530156,8.46752658699496));
#19496=CARTESIAN_POINT('Ctrl Pts',(8.12771067939691,0.932179521963826,8.25883677791438));
#19497=CARTESIAN_POINT('Ctrl Pts',(7.88542764279649,1.83639212436863,8.25883677791438));
#19498=CARTESIAN_POINT('Ctrl Pts',(8.1364238122112,0.93451419886496,8.04662057355209));
#19499=CARTESIAN_POINT('Ctrl Pts',(7.89414077561078,1.83872680126976,8.04662057355209));
#19500=CARTESIAN_POINT('Ctrl Pts',(8.1493910837093,0.937988768790909,7.8318867323277));
#19501=CARTESIAN_POINT('Ctrl Pts',(7.90710804710888,1.84220137119571,7.8318867323277));
#19502=CARTESIAN_POINT('Ctrl Pts',(8.17228612371332,0.944123476270666,7.61613341658679));
#19503=CARTESIAN_POINT('Ctrl Pts',(7.9300030871129,1.84833607867547,7.61613341658679));
#19504=CARTESIAN_POINT('Ctrl Pts',(8.20622600615005,0.953217640360794,7.40136016279815));
#19505=CARTESIAN_POINT('Ctrl Pts',(7.96394296954963,1.8574302427656,7.40136016279815));
#19506=CARTESIAN_POINT('Ctrl Pts',(8.2453420896837,0.963698763354704,7.19009032473197));
#19507=CARTESIAN_POINT('Ctrl Pts',(8.00305905308328,1.86791136575951,7.19009032473197));
#19508=CARTESIAN_POINT('Ctrl Pts',(8.27925670391221,0.972786156848846,6.98516923427904));
#19509=CARTESIAN_POINT('Ctrl Pts',(8.03697366731179,1.87699875925365,6.98516923427904));
#19510=CARTESIAN_POINT('Ctrl Pts',(8.2959096461468,0.977248299272207,6.78954489191915));
#19511=CARTESIAN_POINT('Ctrl Pts',(8.05362660954638,1.88146090167701,6.78954489191915));
#19512=CARTESIAN_POINT('Ctrl Pts',(8.28428637053186,0.974133851957781,6.60605451948904));
#19513=CARTESIAN_POINT('Ctrl Pts',(8.04200333393144,1.87834645436258,6.60605451948904));
#19514=CARTESIAN_POINT('Ctrl Pts',(8.23712373470092,0.961496661773958,6.43720976255638));
#19515=CARTESIAN_POINT('Ctrl Pts',(7.9948406981005,1.86570926417876,6.43720976255638));
#19516=CARTESIAN_POINT('Ctrl Pts',(8.15380096293257,0.939170392367506,6.28498018271691));
#19517=CARTESIAN_POINT('Ctrl Pts',(7.91151792633215,1.84338299477231,6.28498018271691));
#19518=CARTESIAN_POINT('Ctrl Pts',(8.03850758899942,0.908277625929457,6.15052660592943));
#19519=CARTESIAN_POINT('Ctrl Pts',(7.796224552399,1.81249022833426,6.15052660592943));
#19520=CARTESIAN_POINT('Ctrl Pts',(7.89808028789632,0.870650244003599,6.03389995867286));
#19521=CARTESIAN_POINT('Ctrl Pts',(7.6557972512959,1.7748628464084,6.03389995867286));
#19522=CARTESIAN_POINT('Ctrl Pts',(7.74010454114588,0.828320770238116,5.93381436957244));
#19523=CARTESIAN_POINT('Ctrl Pts',(7.49782150454546,1.73253337264292,5.93381436957244));
#19524=CARTESIAN_POINT('Ctrl Pts',(7.57055218101304,0.78288935226573,5.84723737025948));
#19525=CARTESIAN_POINT('Ctrl Pts',(7.32826914441262,1.68710195467053,5.84723737025948));
#19526=CARTESIAN_POINT('Ctrl Pts',(7.39335518196344,0.735409559469172,5.76979878895671));
#19527=CARTESIAN_POINT('Ctrl Pts',(7.15107214536302,1.63962216187397,5.76979878895671));
#19528=CARTESIAN_POINT('Ctrl Pts',(7.21101813137776,0.686552494014464,5.69662713609756));
#19529=CARTESIAN_POINT('Ctrl Pts',(6.96873509477734,1.59076509641927,5.69662713609756));
#19530=CARTESIAN_POINT('Ctrl Pts',(7.02491443968342,0.636686160116518,5.62308582598972));
#19531=CARTESIAN_POINT('Ctrl Pts',(6.782631403083,1.54089876252132,5.62308582598972));
#19532=CARTESIAN_POINT('Ctrl Pts',(6.83570432051349,0.585987461485138,5.54547963906641));
#19533=CARTESIAN_POINT('Ctrl Pts',(6.59342128391307,1.49020006388994,5.54547963906641));
#19534=CARTESIAN_POINT('Ctrl Pts',(6.64372373267898,0.53454641801243,5.46195513100458));
#19535=CARTESIAN_POINT('Ctrl Pts',(6.40144069607856,1.43875902041723,5.46195513100458));
#19536=CARTESIAN_POINT('Ctrl Pts',(6.44924787392593,0.482436768712199,5.37226655127806));
#19537=CARTESIAN_POINT('Ctrl Pts',(6.20696483732551,1.386649371117,5.37226655127806));
#19538=CARTESIAN_POINT('Ctrl Pts',(6.25268064673585,0.429766738928191,5.27709955371581));
#19539=CARTESIAN_POINT('Ctrl Pts',(6.01039761013543,1.33397934133299,5.27709955371581));
#19540=CARTESIAN_POINT('Ctrl Pts',(6.05477787526952,0.376738851133908,5.17752467829117));
#19541=CARTESIAN_POINT('Ctrl Pts',(5.8124948386691,1.28095145353871,5.17752467829117));
#19542=CARTESIAN_POINT('Ctrl Pts',(5.85683735121713,0.323700847564676,5.07442896098936));
#19543=CARTESIAN_POINT('Ctrl Pts',(5.61455431461671,1.22791344996948,5.07442896098936));
#19544=CARTESIAN_POINT('Ctrl Pts',(5.66094878108745,0.271212663391943,4.96787993373722));
#19545=CARTESIAN_POINT('Ctrl Pts',(5.41866574448703,1.17542526579675,4.96787993373722));
#19546=CARTESIAN_POINT('Ctrl Pts',(5.47007435852032,0.220068016009324,4.85676111532844));
#19547=CARTESIAN_POINT('Ctrl Pts',(5.2277913219199,1.12428061841413,4.85676111532844));
#19548=CARTESIAN_POINT('Ctrl Pts',(5.28760657209206,0.171175919991177,4.73929437247794));
#19549=CARTESIAN_POINT('Ctrl Pts',(5.04532353549164,1.07538852239598,4.73929437247794));
#19550=CARTESIAN_POINT('Ctrl Pts',(5.11701976703263,0.125467323336097,4.61340315498245));
#19551=CARTESIAN_POINT('Ctrl Pts',(4.87473673043221,1.0296799257409,4.61340315498245));
#19552=CARTESIAN_POINT('Ctrl Pts',(4.96147687848527,0.0837897319614274,
4.47714872481864));
#19553=CARTESIAN_POINT('Ctrl Pts',(4.71919384188485,0.98800233436623,4.47714872481864));
#19554=CARTESIAN_POINT('Ctrl Pts',(4.82347358239015,0.0468118602199075,
4.32911151507775));
#19555=CARTESIAN_POINT('Ctrl Pts',(4.58119054578973,0.95102446262471,4.32911151507775));
#19556=CARTESIAN_POINT('Ctrl Pts',(4.70441812243944,0.0149110458715985,
4.16885849319143));
#19557=CARTESIAN_POINT('Ctrl Pts',(4.46213508583902,0.919123648276401,4.16885849319143));
#19558=CARTESIAN_POINT('Ctrl Pts',(4.60467557542669,-0.0118148890514923,
3.99681013615577));
#19559=CARTESIAN_POINT('Ctrl Pts',(4.36239253882627,0.892397713353311,3.99681013615577));
#19560=CARTESIAN_POINT('Ctrl Pts',(4.52370003996128,-0.0335122183861244,
3.81399668859083));
#19561=CARTESIAN_POINT('Ctrl Pts',(4.28141700336086,0.870700384018679,3.81399668859083));
#19562=CARTESIAN_POINT('Ctrl Pts',(4.46013369607337,-0.050544768896689,
3.62185203209172));
#19563=CARTESIAN_POINT('Ctrl Pts',(4.21785065947295,0.853667833508114,3.62185203209172));
#19564=CARTESIAN_POINT('Ctrl Pts',(4.41192560529702,-0.0634620878888593,
3.42199345348454));
#19565=CARTESIAN_POINT('Ctrl Pts',(4.1696425686966,0.840750514515944,3.42199345348454));
#19566=CARTESIAN_POINT('Ctrl Pts',(4.37642640354991,-0.0729740703289478,
3.21600287470933));
#19567=CARTESIAN_POINT('Ctrl Pts',(4.13414336694949,0.831238532075855,3.21600287470933));
#19568=CARTESIAN_POINT('Ctrl Pts',(4.35069525229582,-0.079868711527804,
3.00529120729351));
#19569=CARTESIAN_POINT('Ctrl Pts',(4.1084122156954,0.824343890876999,3.00529120729351));
#19570=CARTESIAN_POINT('Ctrl Pts',(4.33181651469696,-0.0849272540215386,
2.7909834104826));
#19571=CARTESIAN_POINT('Ctrl Pts',(4.08953347809654,0.819285348383264,2.7909834104826));
#19572=CARTESIAN_POINT('Ctrl Pts',(4.31723390962471,-0.0888346512741886,
2.57377631141663));
#19573=CARTESIAN_POINT('Ctrl Pts',(4.07495087302429,0.815377951130614,2.57377631141663));
#19574=CARTESIAN_POINT('Ctrl Pts',(4.30502995165065,-0.0921046919578018,
2.35385258470204));
#19575=CARTESIAN_POINT('Ctrl Pts',(4.06274691505023,0.812107910447001,2.35385258470204));
#19576=CARTESIAN_POINT('Ctrl Pts',(4.2943487516111,-0.0949667108825953,
2.13065748555701));
#19577=CARTESIAN_POINT('Ctrl Pts',(4.05206571501068,0.809245891522208,2.13065748555701));
#19578=CARTESIAN_POINT('Ctrl Pts',(4.28513087394313,-0.0974366337596561,
1.9033255681334));
#19579=CARTESIAN_POINT('Ctrl Pts',(4.04284783734271,0.806775968645147,1.9033255681334));
#19580=CARTESIAN_POINT('Ctrl Pts',(4.27751484242575,-0.0994773432542665,
1.67142113207676));
#19581=CARTESIAN_POINT('Ctrl Pts',(4.03523180582533,0.804735259150536,1.67142113207676));
#19582=CARTESIAN_POINT('Ctrl Pts',(4.27134337512002,-0.101130982934953,
1.4355810193293));
#19583=CARTESIAN_POINT('Ctrl Pts',(4.0290603385196,0.80308161946985,1.4355810193293));
#19584=CARTESIAN_POINT('Ctrl Pts',(4.26562700176213,-0.102662680559835,
1.19819542279832));
#19585=CARTESIAN_POINT('Ctrl Pts',(4.02334396516171,0.801549921844968,1.19819542279832));
#19586=CARTESIAN_POINT('Ctrl Pts',(4.25802376460729,-0.104699961815337,
0.964078729991153));
#19587=CARTESIAN_POINT('Ctrl Pts',(4.01574072800687,0.799512640589466,0.964078729991153));
#19588=CARTESIAN_POINT('Ctrl Pts',(4.24431754709998,-0.108372531727705,
0.741129277895168));
#19589=CARTESIAN_POINT('Ctrl Pts',(4.00203451049956,0.795840070677098,0.741129277895168));
#19590=CARTESIAN_POINT('Ctrl Pts',(4.21937538292203,-0.115055764476671,
0.538436816836329));
#19591=CARTESIAN_POINT('Ctrl Pts',(3.97709234632161,0.789156837928132,0.538436816836329));
#19592=CARTESIAN_POINT('Ctrl Pts',(4.17810496802208,-0.12611413882041,0.364350357241537));
#19593=CARTESIAN_POINT('Ctrl Pts',(3.93582193142166,0.778098463584393,0.364350357241537));
#19594=CARTESIAN_POINT('Ctrl Pts',(4.11639811270736,-0.142648440869452,
0.224659532804428));
#19595=CARTESIAN_POINT('Ctrl Pts',(3.87411507610694,0.761564161535351,0.224659532804428));
#19596=CARTESIAN_POINT('Ctrl Pts',(4.03211248248857,-0.165232707420125,
0.120497232333236));
#19597=CARTESIAN_POINT('Ctrl Pts',(3.78982944588815,0.738979894984678,0.120497232333236));
#19598=CARTESIAN_POINT('Ctrl Pts',(3.92595070567427,-0.193678669784572,
0.0470540298718229));
#19599=CARTESIAN_POINT('Ctrl Pts',(3.68366766907385,0.710533932620231,0.0470540298718229));
#19600=CARTESIAN_POINT('Ctrl Pts',(3.80196143446354,-0.22690149487561,-0.00118366394786523));
#19601=CARTESIAN_POINT('Ctrl Pts',(3.55967839786312,0.677311107529193,-0.00118366394786523));
#19602=CARTESIAN_POINT('Ctrl Pts',(3.66788485018745,-0.26282720735631,-0.0263068037111615));
#19603=CARTESIAN_POINT('Ctrl Pts',(3.42560181358703,0.641385395048493,-0.0263068037111615));
#19604=CARTESIAN_POINT('Ctrl Pts',(3.53600025575747,-0.29816557792793,-0.0214179570895094));
#19605=CARTESIAN_POINT('Ctrl Pts',(3.29371721915705,0.606047024476873,-0.0214179570895094));
#19606=CARTESIAN_POINT('Ctrl Pts',(3.41952634006544,-0.329374669576901,
0.0241851999814078));
#19607=CARTESIAN_POINT('Ctrl Pts',(3.17724330346502,0.574837932827902,0.0241851999814078));
#19608=CARTESIAN_POINT('Ctrl Pts',(3.32882972793161,-0.3536767535544,0.119017371327004));
#19609=CARTESIAN_POINT('Ctrl Pts',(3.08654669133119,0.550535848850403,0.119017371327004));
#19610=CARTESIAN_POINT('Ctrl Pts',(3.2667798555616,-0.370302966746397,0.262319630540593));
#19611=CARTESIAN_POINT('Ctrl Pts',(3.02449681896118,0.533909635658406,0.262319630540593));
#19612=CARTESIAN_POINT('Ctrl Pts',(3.22950633865455,-0.38029037550071,0.444963858672424));
#19613=CARTESIAN_POINT('Ctrl Pts',(2.98722330205413,0.523922226904093,0.444963858672424));
#19614=CARTESIAN_POINT('Ctrl Pts',(3.20958407929241,-0.385628528808198,
0.65402023086958));
#19615=CARTESIAN_POINT('Ctrl Pts',(2.96730104269199,0.518584073596605,0.65402023086958));
#19616=CARTESIAN_POINT('Ctrl Pts',(3.198274680088,-0.3886588731919,0.875890304828918));
#19617=CARTESIAN_POINT('Ctrl Pts',(2.95599164348758,0.515553729212903,0.875890304828918));
#19618=CARTESIAN_POINT('Ctrl Pts',(3.18852489662177,-0.391271319798056,
1.10060381648398));
#19619=CARTESIAN_POINT('Ctrl Pts',(2.94624186002135,0.512941282606747,1.10060381648398));
#19620=CARTESIAN_POINT('Ctrl Pts',(3.17642047631752,-0.394514689443426,
1.32371934078733));
#19621=CARTESIAN_POINT('Ctrl Pts',(2.9341374397171,0.509697912961377,1.32371934078733));
#19622=CARTESIAN_POINT('Ctrl Pts',(3.15993887152468,-0.398930922137636,
1.54401727992264));
#19623=CARTESIAN_POINT('Ctrl Pts',(2.91765583492426,0.505281680267167,1.54401727992264));
#19624=CARTESIAN_POINT('Ctrl Pts',(3.13827725626916,-0.404735134452108,
1.76209503442146));
#19625=CARTESIAN_POINT('Ctrl Pts',(2.89599421966874,0.499477467952695,1.76209503442146));
#19626=CARTESIAN_POINT('Ctrl Pts',(3.11093634162015,-0.412061110452637,
1.97856787413951));
#19627=CARTESIAN_POINT('Ctrl Pts',(2.86865330501973,0.492151491952166,1.97856787413951));
#19628=CARTESIAN_POINT('Ctrl Pts',(3.07694311050924,-0.421169569276931,
2.19251877196071));
#19629=CARTESIAN_POINT('Ctrl Pts',(2.83466007390882,0.483043033127872,2.19251877196071));
#19630=CARTESIAN_POINT('Ctrl Pts',(3.03392123208049,-0.432697246858785,
2.39962532458029));
#19631=CARTESIAN_POINT('Ctrl Pts',(2.79163819548007,0.471515355546018,2.39962532458029));
#19632=CARTESIAN_POINT('Ctrl Pts',(2.97853194193879,-0.447538762421585,
2.59347738935741));
#19633=CARTESIAN_POINT('Ctrl Pts',(2.73624890533837,0.456673839983218,2.59347738935741));
#19634=CARTESIAN_POINT('Ctrl Pts',(2.90705252751739,-0.466691613791248,
2.7672283971178));
#19635=CARTESIAN_POINT('Ctrl Pts',(2.66476949091697,0.437520988613555,2.7672283971178));
#19636=CARTESIAN_POINT('Ctrl Pts',(2.81590129070493,-0.491115514084246,
2.91510580081997));
#19637=CARTESIAN_POINT('Ctrl Pts',(2.57361825410451,0.413097088320557,2.91510580081997));
#19638=CARTESIAN_POINT('Ctrl Pts',(2.70219622768186,-0.521582693896607,
3.03403241435618));
#19639=CARTESIAN_POINT('Ctrl Pts',(2.45991319108144,0.382629908508196,3.03403241435618));
#19640=CARTESIAN_POINT('Ctrl Pts',(2.56426771086532,-0.558540528590822,
3.12505646843308));
#19641=CARTESIAN_POINT('Ctrl Pts',(2.3219846742649,0.345672073813981,3.12505646843308));
#19642=CARTESIAN_POINT('Ctrl Pts',(2.40152089622015,-0.602148406145732,
3.19196918412265));
#19643=CARTESIAN_POINT('Ctrl Pts',(2.15923785961973,0.302064196259071,3.19196918412265));
#19644=CARTESIAN_POINT('Ctrl Pts',(2.21432867499209,-0.652306410653179,
3.24001322621211));
#19645=CARTESIAN_POINT('Ctrl Pts',(1.97204563839167,0.251906191751624,3.24001322621211));
#19646=CARTESIAN_POINT('Ctrl Pts',(2.00391387642997,-0.708686886003457,
3.27464765209773));
#19647=CARTESIAN_POINT('Ctrl Pts',(1.76163083982955,0.195525716401346,3.27464765209773));
#19648=CARTESIAN_POINT('Ctrl Pts',(1.77223470132232,-0.770765133876661,
3.30006519349576));
#19649=CARTESIAN_POINT('Ctrl Pts',(1.5299516647219,0.133447468528142,3.30006519349576));
#19650=CARTESIAN_POINT('Ctrl Pts',(1.52187623321765,-0.837848483223599,
3.31897283641381));
#19651=CARTESIAN_POINT('Ctrl Pts',(1.27959319661723,0.066364119181204,3.31897283641381));
#19652=CARTESIAN_POINT('Ctrl Pts',(1.25594690908362,-0.909104030869067,
3.33300441174764));
#19653=CARTESIAN_POINT('Ctrl Pts',(1.0136638724832,-0.00489142846426405,
3.33300441174764));
#19654=CARTESIAN_POINT('Ctrl Pts',(0.977973383552497,-0.983586812552364,
3.34293392264922));
#19655=CARTESIAN_POINT('Ctrl Pts',(0.735690346952077,-0.0793742101475611,
3.34293392264922));
#19656=CARTESIAN_POINT('Ctrl Pts',(0.691796115956336,-1.0602677802969,3.34897162637417));
#19657=CARTESIAN_POINT('Ctrl Pts',(0.449513079355916,-0.156055177892097,
3.34897162637417));
#19658=CARTESIAN_POINT('Ctrl Pts',(0.401464687696532,-1.13806185203649,
3.35102435732185));
#19659=CARTESIAN_POINT('Ctrl Pts',(0.159181651096112,-0.233849249631687,
3.35102435732185));
#19660=CARTESIAN_POINT('Ctrl Pts',(0.111133259436734,-1.21585592377608,
3.34897162637426));
#19661=CARTESIAN_POINT('Ctrl Pts',(-0.131149777163686,-0.311643321371277,
3.34897162637426));
#19662=CARTESIAN_POINT('Ctrl Pts',(-0.175044008159397,-1.29253689152061,
3.34293392264938));
#19663=CARTESIAN_POINT('Ctrl Pts',(-0.417327044759817,-0.388324289115807,
3.34293392264938));
#19664=CARTESIAN_POINT('Ctrl Pts',(-0.453017533690513,-1.3670196732039,
3.33300441174785));
#19665=CARTESIAN_POINT('Ctrl Pts',(-0.695300570290933,-0.462807070799097,
3.33300441174785));
#19666=CARTESIAN_POINT('Ctrl Pts',(-0.718946857824558,-1.43827522084937,
3.31897283641402));
#19667=CARTESIAN_POINT('Ctrl Pts',(-0.961229894424978,-0.534062618444567,
3.31897283641402));
#19668=CARTESIAN_POINT('Ctrl Pts',(-0.969305325929253,-1.50535857019632,
3.30006519349591));
#19669=CARTESIAN_POINT('Ctrl Pts',(-1.21158836252967,-0.601145967791517,
3.30006519349591));
#19670=CARTESIAN_POINT('Ctrl Pts',(-1.20098450103692,-1.56743681806953,
3.27464765209779));
#19671=CARTESIAN_POINT('Ctrl Pts',(-1.44326753763734,-0.663224215664727,
3.27464765209779));
#19672=CARTESIAN_POINT('Ctrl Pts',(-1.41139929959904,-1.6238172934198,3.24001322621208));
#19673=CARTESIAN_POINT('Ctrl Pts',(-1.65368233619946,-0.719604691014997,
3.24001322621208));
#19674=CARTESIAN_POINT('Ctrl Pts',(-1.59859152082706,-1.67397529792724,
3.19196918412254));
#19675=CARTESIAN_POINT('Ctrl Pts',(-1.84087455742748,-0.769762695522437,
3.19196918412254));
#19676=CARTESIAN_POINT('Ctrl Pts',(-1.76133833547218,-1.71758317548214,
3.12505646843295));
#19677=CARTESIAN_POINT('Ctrl Pts',(-2.0036213720726,-0.813370573077337,
3.12505646843295));
#19678=CARTESIAN_POINT('Ctrl Pts',(-1.89926685228873,-1.75454101017635,
3.03403241435609));
#19679=CARTESIAN_POINT('Ctrl Pts',(-2.14154988888915,-0.850328407771547,
3.03403241435609));
#19680=CARTESIAN_POINT('Ctrl Pts',(-2.01297191531186,-1.78500818998873,
2.91510580081997));
#19681=CARTESIAN_POINT('Ctrl Pts',(-2.25525495191228,-0.880795587583927,
2.91510580081997));
#19682=CARTESIAN_POINT('Ctrl Pts',(-2.10412315212447,-1.80943209028177,
2.76722839711793));
#19683=CARTESIAN_POINT('Ctrl Pts',(-2.34640618872489,-0.905219487876967,
2.76722839711793));
#19684=CARTESIAN_POINT('Ctrl Pts',(-2.175602566546,-1.82858494165147,2.59347738935767));
#19685=CARTESIAN_POINT('Ctrl Pts',(-2.41788560314642,-0.924372339246667,
2.59347738935767));
#19686=CARTESIAN_POINT('Ctrl Pts',(-2.23099185668774,-1.84342645721428,
2.39962532458057));
#19687=CARTESIAN_POINT('Ctrl Pts',(-2.47327489328816,-0.939213854809477,
2.39962532458057));
#19688=CARTESIAN_POINT('Ctrl Pts',(-2.27401373511641,-1.85495413479611,
2.19251877196088));
#19689=CARTESIAN_POINT('Ctrl Pts',(-2.51629677171683,-0.950741532391307,
2.19251877196088));
#19690=CARTESIAN_POINT('Ctrl Pts',(-2.30800696622711,-1.86406259362035,
1.97856787413951));
#19691=CARTESIAN_POINT('Ctrl Pts',(-2.55029000282753,-0.959849991215547,
1.97856787413951));
#19692=CARTESIAN_POINT('Ctrl Pts',(-2.33534788087584,-1.8713885696208,1.76209503442131));
#19693=CARTESIAN_POINT('Ctrl Pts',(-2.57763091747626,-0.967175967215997,
1.76209503442131));
#19694=CARTESIAN_POINT('Ctrl Pts',(-2.35700949613116,-1.87719278193522,
1.54401727992238));
#19695=CARTESIAN_POINT('Ctrl Pts',(-2.59929253273158,-0.972980179530417,
1.54401727992238));
#19696=CARTESIAN_POINT('Ctrl Pts',(-2.37349110092397,-1.88160901462942,
1.32371934078708));
#19697=CARTESIAN_POINT('Ctrl Pts',(-2.61577413752439,-0.977396412224617,
1.32371934078708));
#19698=CARTESIAN_POINT('Ctrl Pts',(-2.38559552122837,-1.88485238427483,
1.10060381648384));
#19699=CARTESIAN_POINT('Ctrl Pts',(-2.62787855782879,-0.980639781870027,
1.10060381648384));
#19700=CARTESIAN_POINT('Ctrl Pts',(-2.39534530469489,-1.88746483088107,
0.875890304828914));
#19701=CARTESIAN_POINT('Ctrl Pts',(-2.63762834129531,-0.983252228476267,
0.875890304828914));
#19702=CARTESIAN_POINT('Ctrl Pts',(-2.40665470389955,-1.89049517526484,
0.654020230869684));
#19703=CARTESIAN_POINT('Ctrl Pts',(-2.64893774049997,-0.986282572860037,
0.654020230869684));
#19704=CARTESIAN_POINT('Ctrl Pts',(-2.42657696326181,-1.89583332857236,
0.444963858672577));
#19705=CARTESIAN_POINT('Ctrl Pts',(-2.66885999986223,-0.991620726167557,
0.444963858672577));
#19706=CARTESIAN_POINT('Ctrl Pts',(-2.46385048016881,-1.90582073732665,
0.262319630540737));
#19707=CARTESIAN_POINT('Ctrl Pts',(-2.70613351676923,-1.00160813492185,
0.262319630540737));
#19708=CARTESIAN_POINT('Ctrl Pts',(-2.52590035253865,-1.92244695051861,
0.11901737132707));
#19709=CARTESIAN_POINT('Ctrl Pts',(-2.76818338913907,-1.01823434811381,
0.11901737132707));
#19710=CARTESIAN_POINT('Ctrl Pts',(-2.61659696467234,-1.94674903449607,
0.0241851999813871));
#19711=CARTESIAN_POINT('Ctrl Pts',(-2.85888000127276,-1.04253643209127,
0.0241851999813871));
#19712=CARTESIAN_POINT('Ctrl Pts',(-2.73307088036432,-1.97795812614502,
-0.0214179570895714));
#19713=CARTESIAN_POINT('Ctrl Pts',(-2.97535391696474,-1.07374552374022,
-0.0214179570895714));
#19714=CARTESIAN_POINT('Ctrl Pts',(-2.86495547479434,-2.01329649671666,
-0.0263068037112043));
#19715=CARTESIAN_POINT('Ctrl Pts',(-3.10723851139476,-1.10908389431186,
-0.0263068037112043));
#19716=CARTESIAN_POINT('Ctrl Pts',(-2.99903205907052,-2.04922220919738,
-0.00118366394785932));
#19717=CARTESIAN_POINT('Ctrl Pts',(-3.24131509567094,-1.14500960679258,
-0.00118366394785932));
#19718=CARTESIAN_POINT('Ctrl Pts',(-3.12302133028127,-2.08244503428843,
0.0470540298718583));
#19719=CARTESIAN_POINT('Ctrl Pts',(-3.36530436688169,-1.17823243188363,
0.0470540298718583));
#19720=CARTESIAN_POINT('Ctrl Pts',(-3.22918310709556,-2.11089099665287,
0.120497232333251));
#19721=CARTESIAN_POINT('Ctrl Pts',(-3.47146614369598,-1.20667839424807,
0.120497232333251));
#19722=CARTESIAN_POINT('Ctrl Pts',(-3.31346873731432,-2.13347526320353,
0.224659532804408));
#19723=CARTESIAN_POINT('Ctrl Pts',(-3.55575177391474,-1.22926266079873,
0.224659532804408));
#19724=CARTESIAN_POINT('Ctrl Pts',(-3.37517559262903,-2.15000956525257,
0.364350357241515));
#19725=CARTESIAN_POINT('Ctrl Pts',(-3.61745862922945,-1.24579696284777,
0.364350357241515));
#19726=CARTESIAN_POINT('Ctrl Pts',(-3.41644600752903,-2.16106793959632,
0.538436816836325));
#19727=CARTESIAN_POINT('Ctrl Pts',(-3.65872904412945,-1.25685533719152,
0.538436816836325));
#19728=CARTESIAN_POINT('Ctrl Pts',(-3.44138817170702,-2.1677511723453,0.741129277895169));
#19729=CARTESIAN_POINT('Ctrl Pts',(-3.68367120830744,-1.2635385699405,0.741129277895169));
#19730=CARTESIAN_POINT('Ctrl Pts',(-3.45509438921434,-2.17142374225767,
0.964078729991154));
#19731=CARTESIAN_POINT('Ctrl Pts',(-3.69737742581476,-1.26721113985287,
0.964078729991154));
#19732=CARTESIAN_POINT('Ctrl Pts',(-3.46269762636911,-2.17346102351316,
1.1981954227983));
#19733=CARTESIAN_POINT('Ctrl Pts',(-3.70498066296953,-1.26924842110836,
1.1981954227983));
#19734=CARTESIAN_POINT('Ctrl Pts',(-3.46841399972688,-2.174992721138,1.43558101932923));
#19735=CARTESIAN_POINT('Ctrl Pts',(-3.7106970363273,-1.2707801187332,1.43558101932923));
#19736=CARTESIAN_POINT('Ctrl Pts',(-3.47458546703248,-2.17664636081866,
1.67142113207667));
#19737=CARTESIAN_POINT('Ctrl Pts',(-3.7168685036329,-1.27243375841386,1.67142113207667));
#19738=CARTESIAN_POINT('Ctrl Pts',(-3.48220149854979,-2.17868707031325,
1.90332556813333));
#19739=CARTESIAN_POINT('Ctrl Pts',(-3.72448453515021,-1.27447446790845,
1.90332556813333));
#19740=CARTESIAN_POINT('Ctrl Pts',(-3.4914193762178,-2.18115699319032,2.130657485557));
#19741=CARTESIAN_POINT('Ctrl Pts',(-3.73370241281822,-1.27694439078552,
2.130657485557));
#19742=CARTESIAN_POINT('Ctrl Pts',(-3.5021005762575,-2.18401901211515,2.35385258470204));
#19743=CARTESIAN_POINT('Ctrl Pts',(-3.74438361285792,-1.27980640971035,
2.35385258470204));
#19744=CARTESIAN_POINT('Ctrl Pts',(-3.51430453423174,-2.18728905279882,
2.57377631141659));
#19745=CARTESIAN_POINT('Ctrl Pts',(-3.75658757083216,-1.28307645039402,
2.57377631141659));
#19746=CARTESIAN_POINT('Ctrl Pts',(-3.52888713930413,-2.1911964500515,2.7909834104825));
#19747=CARTESIAN_POINT('Ctrl Pts',(-3.77117017590455,-1.2869838476467,2.7909834104825));
#19748=CARTESIAN_POINT('Ctrl Pts',(-3.54776587690305,-2.19625499254525,
3.00529120729338));
#19749=CARTESIAN_POINT('Ctrl Pts',(-3.79004891350347,-1.29204239014045,
3.00529120729338));
#19750=CARTESIAN_POINT('Ctrl Pts',(-3.5734970281571,-2.2031496337441,3.21600287470921));
#19751=CARTESIAN_POINT('Ctrl Pts',(-3.81578006475752,-1.2989370313393,3.21600287470921));
#19752=CARTESIAN_POINT('Ctrl Pts',(-3.6089962299041,-2.21266161618416,3.42199345348447));
#19753=CARTESIAN_POINT('Ctrl Pts',(-3.85127926650452,-1.30844901377936,
3.42199345348447));
#19754=CARTESIAN_POINT('Ctrl Pts',(-3.65720432068032,-2.22557893517629,
3.62185203209171));
#19755=CARTESIAN_POINT('Ctrl Pts',(-3.89948735728074,-1.32136633277149,
3.62185203209171));
#19756=CARTESIAN_POINT('Ctrl Pts',(-3.72077066456812,-2.24261148568683,
3.81399668859083));
#19757=CARTESIAN_POINT('Ctrl Pts',(-3.96305370116854,-1.33839888328203,
3.81399668859083));
#19758=CARTESIAN_POINT('Ctrl Pts',(-3.80174620003347,-2.26430881502145,
3.99681013615577));
#19759=CARTESIAN_POINT('Ctrl Pts',(-4.04402923663389,-1.36009621261665,
3.99681013615577));
#19760=CARTESIAN_POINT('Ctrl Pts',(-3.90148874704625,-2.29103474994454,
4.16885849319142));
#19761=CARTESIAN_POINT('Ctrl Pts',(-4.14377178364667,-1.38682214753974,
4.16885849319142));
#19762=CARTESIAN_POINT('Ctrl Pts',(-4.02054420699703,-2.32293556429287,
4.32911151507774));
#19763=CARTESIAN_POINT('Ctrl Pts',(-4.26282724359745,-1.41872296188807,
4.32911151507774));
#19764=CARTESIAN_POINT('Ctrl Pts',(-4.15854750309224,-2.35991343603441,
4.47714872481861));
#19765=CARTESIAN_POINT('Ctrl Pts',(-4.40083053969266,-1.45570083362961,
4.47714872481861));
#19766=CARTESIAN_POINT('Ctrl Pts',(-4.31409039163966,-2.4015910274091,4.61340315498244));
#19767=CARTESIAN_POINT('Ctrl Pts',(-4.55637342824008,-1.4973784250043,4.61340315498244));
#19768=CARTESIAN_POINT('Ctrl Pts',(-4.48467719669913,-2.44729962406419,
4.73929437247796));
#19769=CARTESIAN_POINT('Ctrl Pts',(-4.72696023329955,-1.54308702165939,
4.73929437247796));
#19770=CARTESIAN_POINT('Ctrl Pts',(-4.66714498312739,-2.49619172008234,
4.8567611153285));
#19771=CARTESIAN_POINT('Ctrl Pts',(-4.90942801972781,-1.59197911767754,
4.8567611153285));
#19772=CARTESIAN_POINT('Ctrl Pts',(-4.85801940569448,-2.54733636746495,
4.96787993373728));
#19773=CARTESIAN_POINT('Ctrl Pts',(-5.1003024422949,-1.64312376506015,4.96787993373728));
#19774=CARTESIAN_POINT('Ctrl Pts',(-5.05390797582409,-2.59982455163766,
5.07442896098937));
#19775=CARTESIAN_POINT('Ctrl Pts',(-5.29619101242451,-1.69561194923286,
5.07442896098937));
#19776=CARTESIAN_POINT('Ctrl Pts',(-5.25184849987638,-2.65286255520687,
5.17752467829109));
#19777=CARTESIAN_POINT('Ctrl Pts',(-5.4941315364768,-1.74864995280207,5.17752467829109));
#19778=CARTESIAN_POINT('Ctrl Pts',(-5.44975127134264,-2.70589044300113,
5.27709955371564));
#19779=CARTESIAN_POINT('Ctrl Pts',(-5.69203430794306,-1.80167784059633,
5.27709955371564));
#19780=CARTESIAN_POINT('Ctrl Pts',(-5.64631849853272,-2.75856047278514,
5.37226655127787));
#19781=CARTESIAN_POINT('Ctrl Pts',(-5.88860153513314,-1.85434787038034,
5.37226655127787));
#19782=CARTESIAN_POINT('Ctrl Pts',(-5.84079435728585,-2.81067012208539,
5.46195513100446));
#19783=CARTESIAN_POINT('Ctrl Pts',(-6.08307739388627,-1.90645751968059,
5.46195513100446));
#19784=CARTESIAN_POINT('Ctrl Pts',(-6.03277494512045,-2.86211116555812,
5.54547963906637));
#19785=CARTESIAN_POINT('Ctrl Pts',(-6.27505798172087,-1.95789856315332,
5.54547963906637));
#19786=CARTESIAN_POINT('Ctrl Pts',(-6.22198506429037,-2.9128098641895,5.62308582598972));
#19787=CARTESIAN_POINT('Ctrl Pts',(-6.46426810089079,-2.0085972617847,5.62308582598972));
#19788=CARTESIAN_POINT('Ctrl Pts',(-6.40808875598458,-2.96267619808741,
5.69662713609756));
#19789=CARTESIAN_POINT('Ctrl Pts',(-6.650371792585,-2.05846359568261,5.69662713609756));
#19790=CARTESIAN_POINT('Ctrl Pts',(-6.59042580657019,-3.0115332635421,5.76979878895672));
#19791=CARTESIAN_POINT('Ctrl Pts',(-6.83270884317061,-2.1073206611373,5.76979878895672));
#19792=CARTESIAN_POINT('Ctrl Pts',(-6.76762280561976,-3.05901305633865,
5.84723737025949));
#19793=CARTESIAN_POINT('Ctrl Pts',(-7.00990584222018,-2.15480045393385,
5.84723737025949));
#19794=CARTESIAN_POINT('Ctrl Pts',(-6.9371751657527,-3.10444447431107,5.93381436957244));
#19795=CARTESIAN_POINT('Ctrl Pts',(-7.17945820235312,-2.20023187190627,
5.93381436957244));
#19796=CARTESIAN_POINT('Ctrl Pts',(-7.09515091250332,-3.1467739480766,6.03389995867283));
#19797=CARTESIAN_POINT('Ctrl Pts',(-7.33743394910374,-2.2425613456718,6.03389995867283));
#19798=CARTESIAN_POINT('Ctrl Pts',(-7.23557821360659,-3.1844013300025,6.15052660592937));
#19799=CARTESIAN_POINT('Ctrl Pts',(-7.47786125020701,-2.2801887275977,6.15052660592937));
#19800=CARTESIAN_POINT('Ctrl Pts',(-7.35087158753979,-3.21529409644056,
6.28498018271686));
#19801=CARTESIAN_POINT('Ctrl Pts',(-7.59315462414021,-2.31108149403576,
6.28498018271686));
#19802=CARTESIAN_POINT('Ctrl Pts',(-7.43419435930806,-3.23762036584699,
6.43720976255636));
#19803=CARTESIAN_POINT('Ctrl Pts',(-7.67647739590848,-2.33340776344219,
6.43720976255636));
#19804=CARTESIAN_POINT('Ctrl Pts',(-7.48135699513883,-3.25025755603077,
6.60605451948903));
#19805=CARTESIAN_POINT('Ctrl Pts',(-7.72364003173925,-2.34604495362597,
6.60605451948903));
#19806=CARTESIAN_POINT('Ctrl Pts',(-7.49298027075354,-3.25337200334513,
6.78954489191904));
#19807=CARTESIAN_POINT('Ctrl Pts',(-7.73526330735396,-2.34915940094033,
6.78954489191904));
#19808=CARTESIAN_POINT('Ctrl Pts',(-7.4763273285188,-3.24890986092173,6.9851692342788));
#19809=CARTESIAN_POINT('Ctrl Pts',(-7.71861036511922,-2.34469725851693,
6.9851692342788));
#19810=CARTESIAN_POINT('Ctrl Pts',(-7.44241271429029,-3.23982246742759,
7.19009032473164));
#19811=CARTESIAN_POINT('Ctrl Pts',(-7.68469575089071,-2.33560986502279,
7.19009032473164));
#19812=CARTESIAN_POINT('Ctrl Pts',(-7.40329663075682,-3.22934134443373,
7.40136016279791));
#19813=CARTESIAN_POINT('Ctrl Pts',(-7.64557966735724,-2.32512874202893,
7.40136016279791));
#19814=CARTESIAN_POINT('Ctrl Pts',(-7.36935674832032,-3.22024718034366,
7.61613341658677));
#19815=CARTESIAN_POINT('Ctrl Pts',(-7.61163978492074,-2.31603457793886,
7.61613341658677));
#19816=CARTESIAN_POINT('Ctrl Pts',(-7.34646170831648,-3.21411247286395,
7.83188673232793));
#19817=CARTESIAN_POINT('Ctrl Pts',(-7.5887447449169,-2.30989987045915,7.83188673232793));
#19818=CARTESIAN_POINT('Ctrl Pts',(-7.33349443681848,-3.21063790293803,
8.04662057355248));
#19819=CARTESIAN_POINT('Ctrl Pts',(-7.5757774734189,-2.30642530053323,8.04662057355248));
#19820=CARTESIAN_POINT('Ctrl Pts',(-7.32478130400418,-3.20830322603689,
8.25883677791483));
#19821=CARTESIAN_POINT('Ctrl Pts',(-7.5670643406046,-2.30409062363209,8.25883677791483));
#19822=CARTESIAN_POINT('Ctrl Pts',(-7.31218544940774,-3.2049281769698,8.46752658699528));
#19823=CARTESIAN_POINT('Ctrl Pts',(-7.55446848600816,-2.300715574565,8.46752658699528));
#19824=CARTESIAN_POINT('Ctrl Pts',(-7.28737839225422,-3.19828114603892,
8.67216210283896));
#19825=CARTESIAN_POINT('Ctrl Pts',(-7.52966142885464,-2.29406854363412,
8.67216210283896));
#19826=CARTESIAN_POINT('Ctrl Pts',(-7.24391800390076,-3.18663597007687,
8.87266947141823));
#19827=CARTESIAN_POINT('Ctrl Pts',(-7.48620104050118,-2.28242336767207,
8.87266947141823));
#19828=CARTESIAN_POINT('Ctrl Pts',(-7.17972079495768,-3.16943437978424,
9.06945407016992));
#19829=CARTESIAN_POINT('Ctrl Pts',(-7.4220038315581,-2.26522177737944,9.06945407016992));
#19830=CARTESIAN_POINT('Ctrl Pts',(-7.09614123761334,-3.14703930489007,
9.26297089919765));
#19831=CARTESIAN_POINT('Ctrl Pts',(-7.33842427421376,-2.24282670248527,
9.26297089919765));
#19832=CARTESIAN_POINT('Ctrl Pts',(-6.99656158928535,-3.12035701853801,
9.4532499945042));
#19833=CARTESIAN_POINT('Ctrl Pts',(-7.23884462588577,-2.21614441613321,
9.4532499945042));
#19834=CARTESIAN_POINT('Ctrl Pts',(-6.88509891533857,-3.09049068506776,
9.63939026966035));
#19835=CARTESIAN_POINT('Ctrl Pts',(-7.12738195193899,-2.18627808266296,
9.63939026966035));
#19836=CARTESIAN_POINT('Ctrl Pts',(-6.76538664525988,-3.05841387897608,
9.81917361987397));
#19837=CARTESIAN_POINT('Ctrl Pts',(-7.0076696818603,-2.15420127657128,9.81917361987397));
#19838=CARTESIAN_POINT('Ctrl Pts',(-6.63901215031964,-3.02455193511295,
9.98835756998572));
#19839=CARTESIAN_POINT('Ctrl Pts',(-6.88129518692006,-2.12033933270815,
9.98835756998572));
#19840=CARTESIAN_POINT('Ctrl Pts',(-6.5056926897586,-2.98882909332026,10.1414720974148));
#19841=CARTESIAN_POINT('Ctrl Pts',(-6.74797572635902,-2.08461649091546,
10.1414720974148));
#19842=CARTESIAN_POINT('Ctrl Pts',(-6.36431879979372,-2.95094807367333,
10.2733319413008));
#19843=CARTESIAN_POINT('Ctrl Pts',(-6.60660183639414,-2.04673547126853,
10.2733319413008));
#19844=CARTESIAN_POINT('Ctrl Pts',(-6.21376535173928,-2.91060739884942,
10.3804015453596));
#19845=CARTESIAN_POINT('Ctrl Pts',(-6.4560483883397,-2.00639479644462,10.3804015453596));
#19846=CARTESIAN_POINT('Ctrl Pts',(-6.05370969899924,-2.86772061595369,
10.4620502678778));
#19847=CARTESIAN_POINT('Ctrl Pts',(-6.29599273559966,-1.96350801354889,
10.4620502678778));
#19848=CARTESIAN_POINT('Ctrl Pts',(-5.88567460802205,-2.82269574902626,
10.522290883026));
#19849=CARTESIAN_POINT('Ctrl Pts',(-6.12795764462247,-1.91848314662146,
10.522290883026));
#19850=CARTESIAN_POINT('Ctrl Pts',(-5.71262166386122,-2.77632635239054,
10.5687216653902));
#19851=CARTESIAN_POINT('Ctrl Pts',(-5.95490470046164,-1.87211374998574,
10.5687216653902));
#19852=CARTESIAN_POINT('Ctrl Pts',(-5.53795302541203,-2.72952403177503,
10.6103475969885));
#19853=CARTESIAN_POINT('Ctrl Pts',(-5.78023606201245,-1.82531142937023,
10.6103475969885));
#19854=CARTESIAN_POINT('Ctrl Pts',(-5.36474479343613,-2.68311302589467,
10.6558377434043));
#19855=CARTESIAN_POINT('Ctrl Pts',(-5.60702783003655,-1.77890042348987,
10.6558377434043));
#19856=CARTESIAN_POINT('Ctrl Pts',(-5.19479751149305,-2.63757578894216,
10.7114411549114));
#19857=CARTESIAN_POINT('Ctrl Pts',(-5.43708054809347,-1.73336318653736,
10.7114411549114));
#19858=CARTESIAN_POINT('Ctrl Pts',(-5.02801887021532,-2.59288758669703,
10.7795199127535));
#19859=CARTESIAN_POINT('Ctrl Pts',(-5.27030190681574,-1.68867498429223,
10.7795199127535));
#19860=CARTESIAN_POINT('Ctrl Pts',(-4.86332857677405,-2.5487589555682,10.8599381259737));
#19861=CARTESIAN_POINT('Ctrl Pts',(-5.10561161337447,-1.6445463531634,10.8599381259737));
#19862=CARTESIAN_POINT('Ctrl Pts',(-4.69942419919693,-2.50484090996048,
10.9511663773826));
#19863=CARTESIAN_POINT('Ctrl Pts',(-4.94170723579735,-1.60062830755568,
10.9511663773826));
#19864=CARTESIAN_POINT('Ctrl Pts',(-4.53550776406181,-2.46091963353984,
11.0513704191329));
#19865=CARTESIAN_POINT('Ctrl Pts',(-4.77779080066223,-1.55670703113504,
11.0513704191329));
#19866=CARTESIAN_POINT('Ctrl Pts',(-4.37225446646398,-2.41717604428678,
11.1598106424589));
#19867=CARTESIAN_POINT('Ctrl Pts',(-4.6145375030644,-1.51296344188198,11.1598106424589));
#19868=CARTESIAN_POINT('Ctrl Pts',(-4.2117643371012,-2.37417284373086,11.2768795166235));
#19869=CARTESIAN_POINT('Ctrl Pts',(-4.45404737370162,-1.46996024132606,
11.2768795166235));
#19870=CARTESIAN_POINT('Ctrl Pts',(-4.05659783059815,-2.33259610362101,
11.4029224160731));
#19871=CARTESIAN_POINT('Ctrl Pts',(-4.29888086719857,-1.42838350121621,
11.4029224160731));
#19872=CARTESIAN_POINT('Ctrl Pts',(-3.90903315889734,-2.29305626900741,
11.5373242211527));
#19873=CARTESIAN_POINT('Ctrl Pts',(-4.15131619549776,-1.38884366660261,
11.5373242211527));
#19874=CARTESIAN_POINT('Ctrl Pts',(-3.77030699189688,-2.25588470459057,
11.6776492463597));
#19875=CARTESIAN_POINT('Ctrl Pts',(-4.0125900284973,-1.35167210218577,11.6776492463597));
#19876=CARTESIAN_POINT('Ctrl Pts',(-3.63967882884875,-2.22088299379307,
11.8183570873721));
#19877=CARTESIAN_POINT('Ctrl Pts',(-3.88196186544917,-1.31667039138827,
11.8183570873721));
#19878=CARTESIAN_POINT('Ctrl Pts',(-3.51435496549085,-2.18730256581397,
11.9514202619522));
#19879=CARTESIAN_POINT('Ctrl Pts',(-3.75663800209127,-1.28308996340917,
11.9514202619522));
#19880=CARTESIAN_POINT('Ctrl Pts',(-3.39011325532028,-2.1540120999075,12.0684942936867));
#19881=CARTESIAN_POINT('Ctrl Pts',(-3.6323962919207,-1.2497994975027,12.0684942936867));
#19882=CARTESIAN_POINT('Ctrl Pts',(-3.26172495134207,-2.11961055753894,
12.1626050652586));
#19883=CARTESIAN_POINT('Ctrl Pts',(-3.50400798794249,-1.21539795513414,
12.1626050652586));
#19884=CARTESIAN_POINT('Ctrl Pts',(-3.12345991910123,-2.08256255380854,
12.2301117722809));
#19885=CARTESIAN_POINT('Ctrl Pts',(-3.36574295570165,-1.17834995140374,
12.2301117722809));
#19886=CARTESIAN_POINT('Ctrl Pts',(-2.96955541126968,-2.04132396522357,
12.2723364229645));
#19887=CARTESIAN_POINT('Ctrl Pts',(-3.2118384478701,-1.13711136281877,12.2723364229645));
#19888=CARTESIAN_POINT('Ctrl Pts',(-2.79463396275701,-1.99445390435572,
12.2938762651139));
#19889=CARTESIAN_POINT('Ctrl Pts',(-3.03691699935743,-1.09024130195092,
12.2938762651139));
#19890=CARTESIAN_POINT('Ctrl Pts',(-2.59413751717341,-1.94073104367628,
12.3010487961981));
#19891=CARTESIAN_POINT('Ctrl Pts',(-2.83642055377383,-1.03651844127148,
12.3010487961981));
#19892=CARTESIAN_POINT('Ctrl Pts',(-2.3647179830369,-1.87925826477648,12.300400839059));
#19893=CARTESIAN_POINT('Ctrl Pts',(-2.60700101963732,-0.975045662371677,
12.300400839059));
#19894=CARTESIAN_POINT('Ctrl Pts',(-2.10473899353102,-1.80959710448932,
12.2969132923574));
#19895=CARTESIAN_POINT('Ctrl Pts',(-2.34702203013144,-0.905384502084517,
12.2969132923574));
#19896=CARTESIAN_POINT('Ctrl Pts',(-1.81431310880745,-1.73177772321654,
12.2935845551224));
#19897=CARTESIAN_POINT('Ctrl Pts',(-2.05659614540787,-0.827565120811737,
12.2935845551224));
#19898=CARTESIAN_POINT('Ctrl Pts',(-1.49502196421663,-1.64622391887302,
12.2919684497906));
#19899=CARTESIAN_POINT('Ctrl Pts',(-1.73730500081705,-0.742011316468217,
12.2919684497906));
#19900=CARTESIAN_POINT('Ctrl Pts',(-1.14973065532629,-1.55370339150237,
12.2924280531798));
#19901=CARTESIAN_POINT('Ctrl Pts',(-1.39201369192671,-0.649490789097567,
12.2924280531798));
#19902=CARTESIAN_POINT('Ctrl Pts',(-0.782363392512268,-1.45526763010572,
12.2945066442122));
#19903=CARTESIAN_POINT('Ctrl Pts',(-1.02464642911269,-0.551055027700917,
12.2945066442122));
#19904=CARTESIAN_POINT('Ctrl Pts',(-0.39769588314259,-1.35219628161563,
12.2972483292773));
#19905=CARTESIAN_POINT('Ctrl Pts',(-0.63997891974301,-0.447983679210827,
12.2972483292773));
#19906=CARTESIAN_POINT('Ctrl Pts',(-0.0804516762334893,-1.26719095257088,
12.299081889758));
#19907=CARTESIAN_POINT('Ctrl Pts',(-0.322734712833909,-0.362978350166077,
12.299081889758));
#19908=CARTESIAN_POINT('Ctrl Pts',(0.160204003053163,-1.20270745765206,
12.2998330708668));
#19909=CARTESIAN_POINT('Ctrl Pts',(-0.0820790335472567,-0.298494855247257,
12.2998330708668));
#19910=CARTESIAN_POINT('Ctrl Pts',(0.321044459482073,-1.15961038724168,
12.2999999999989));
#19911=CARTESIAN_POINT('Ctrl Pts',(0.0787614228816533,-0.255397784836877,
12.2999999999989));
#19912=CARTESIAN_POINT('Ctrl Pts',(0.401464687696516,-1.13806185203649,
12.3));
#19913=CARTESIAN_POINT('Ctrl Pts',(0.159181651096096,-0.233849249631687,
12.3));
#19914=CARTESIAN_POINT('Ctrl Pts',(0.481884915910943,-1.11651331683131,
12.3000000000011));
#19915=CARTESIAN_POINT('Ctrl Pts',(0.239601879310523,-0.212300714426507,
12.3000000000011));
#19916=CARTESIAN_POINT('Ctrl Pts',(0.642725372339789,-1.07341624642095,
12.2998330708736));
#19917=CARTESIAN_POINT('Ctrl Pts',(0.400442335739369,-0.169203644016147,
12.2998330708736));
#19918=CARTESIAN_POINT('Ctrl Pts',(0.883381051626486,-1.00893275150212,
12.2990818897713));
#19919=CARTESIAN_POINT('Ctrl Pts',(0.641098015026066,-0.104720149097317,
12.2990818897713));
#19920=CARTESIAN_POINT('Ctrl Pts',(1.20062525853542,-0.923927422457416,
12.2972483292974));
#19921=CARTESIAN_POINT('Ctrl Pts',(0.958342221935,-0.019714820052613,12.2972483292974));
#19922=CARTESIAN_POINT('Ctrl Pts',(1.58529276790501,-0.82085607396734,12.2945066442369));
#19923=CARTESIAN_POINT('Ctrl Pts',(1.34300973130459,0.083356528437463,12.2945066442369));
#19924=CARTESIAN_POINT('Ctrl Pts',(1.95266003071895,-0.722420312570714,
12.2924280532047));
#19925=CARTESIAN_POINT('Ctrl Pts',(1.71037699411853,0.181792289834089,12.2924280532047));
#19926=CARTESIAN_POINT('Ctrl Pts',(2.29795133960928,-0.629899785200065,
12.291968449812));
#19927=CARTESIAN_POINT('Ctrl Pts',(2.05566830300886,0.274312817204738,12.291968449812));
#19928=CARTESIAN_POINT('Ctrl Pts',(2.61724248420015,-0.544345980856534,
12.2935845551378));
#19929=CARTESIAN_POINT('Ctrl Pts',(2.37495944759973,0.359866621548269,12.2935845551378));
#19930=CARTESIAN_POINT('Ctrl Pts',(2.90766836892382,-0.46652659958373,12.2969132923658));
#19931=CARTESIAN_POINT('Ctrl Pts',(2.6653853323234,0.437686002821073,12.2969132923658));
#19932=CARTESIAN_POINT('Ctrl Pts',(3.16764735842983,-0.396865439296537,
12.3004008390612));
#19933=CARTESIAN_POINT('Ctrl Pts',(2.92536432182941,0.507347163108266,12.3004008390612));
#19934=CARTESIAN_POINT('Ctrl Pts',(3.39706689256644,-0.335392660396708,
12.3010487961961));
#19935=CARTESIAN_POINT('Ctrl Pts',(3.15478385596602,0.568819942008095,12.3010487961961));
#19936=CARTESIAN_POINT('Ctrl Pts',(3.59756333815007,-0.281669799717264,
12.2938762651102));
#19937=CARTESIAN_POINT('Ctrl Pts',(3.35528030154965,0.622542802687539,12.2938762651102));
#19938=CARTESIAN_POINT('Ctrl Pts',(3.77248478666274,-0.234799738849412,
12.2723364229612));
#19939=CARTESIAN_POINT('Ctrl Pts',(3.53020175006232,0.669412863555391,12.2723364229612));
#19940=CARTESIAN_POINT('Ctrl Pts',(3.92638929449424,-0.19356115026445,12.2301117722792));
#19941=CARTESIAN_POINT('Ctrl Pts',(3.68410625789382,0.710651452140353,12.2301117722792));
#19942=CARTESIAN_POINT('Ctrl Pts',(4.06465432673507,-0.156513146534059,
12.1626050652587));
#19943=CARTESIAN_POINT('Ctrl Pts',(3.82237129013465,0.747699455870744,12.1626050652587));
#19944=CARTESIAN_POINT('Ctrl Pts',(4.17641608075606,-0.126566674799447,
12.0806818325566));
#19945=CARTESIAN_POINT('Ctrl Pts',(3.93413304415564,0.777645927605356,12.0806818325566));
#19946=CARTESIAN_POINT('Ctrl Pts',(4.26016995678755,-0.104124891353834,
12.0046763352305));
#19947=CARTESIAN_POINT('Ctrl Pts',(4.01788692018713,0.800087711050969,12.0046763352305));
#19948=CARTESIAN_POINT('Ctrl Pts',(4.31892840257442,-0.0883806132567331,
11.9465013108381));
#19949=CARTESIAN_POINT('Ctrl Pts',(4.076645365974,0.81583198914807,11.9465013108381));
#19950=CARTESIAN_POINT('Ctrl Pts',(4.35289300399361,-0.0792798257352161,
11.9117811315282));
#19951=CARTESIAN_POINT('Ctrl Pts',(4.11060996739319,0.824932776669587,11.9117811315282));
#19952=CARTESIAN_POINT('Ctrl Pts',(4.3617605754817,-0.0769037671161592,
11.9026515720695));
#19953=CARTESIAN_POINT('Ctrl Pts',(4.11947753888128,0.827308835288644,11.9026515720695));
#19954=CARTESIAN_POINT('',(4.40285823325642,0.132224151085944,3.57811407583582));
#19955=CARTESIAN_POINT('Ctrl Pts',(4.40285823325641,0.132224151085904,3.57811407583577));
#19956=CARTESIAN_POINT('Ctrl Pts',(4.43940677028145,0.142017302066303,3.71456495367834));
#19957=CARTESIAN_POINT('Ctrl Pts',(4.53463296379915,0.167533083717659,3.9794750710438));
#19958=CARTESIAN_POINT('Ctrl Pts',(4.76097163197783,0.228180347072074,4.33028299830215));
#19959=CARTESIAN_POINT('Ctrl Pts',(5.06150763834345,0.308708727274215,4.61783411696581));
#19960=CARTESIAN_POINT('Ctrl Pts',(5.40852054959526,0.401690556607312,4.85362603977077));
#19961=CARTESIAN_POINT('Ctrl Pts',(5.77679893037258,0.500370451326437,5.05954568690866));
#19962=CARTESIAN_POINT('Ctrl Pts',(6.28064189604197,0.635374767089651,5.31961833864166));
#19963=CARTESIAN_POINT('Ctrl Pts',(6.81213487368419,0.777787881231695,5.56423083230834));
#19964=CARTESIAN_POINT('Ctrl Pts',(7.25326088523284,0.895987239786518,5.73088688746923));
#19965=CARTESIAN_POINT('Ctrl Pts',(7.60545358372097,0.990356988926552,5.88645382774441));
#19966=CARTESIAN_POINT('Ctrl Pts',(7.89304985394669,1.06741817727973,6.03509348122348));
#19967=CARTESIAN_POINT('Ctrl Pts',(8.13408614953057,1.13200365802803,6.32217794399327));
#19968=CARTESIAN_POINT('Ctrl Pts',(8.21367576229283,1.15332963049358,6.52713122561373));
#19969=CARTESIAN_POINT('Ctrl Pts',(8.24820562306135,1.16258187880126,6.74090493270784));
#19970=CARTESIAN_POINT('Ctrl Pts',(8.22962792994722,1.1576040009341,6.99851570691194));
#19971=CARTESIAN_POINT('Ctrl Pts',(8.15840156120257,1.13851895294917,7.38504607625248));
#19972=CARTESIAN_POINT('Ctrl Pts',(8.08669712828127,1.11930580805417,7.85408399146071));
#19973=CARTESIAN_POINT('Ctrl Pts',(8.08101604477191,1.11778356631571,8.34143039554977));
#19974=CARTESIAN_POINT('Ctrl Pts',(8.03131448784197,1.10446607427376,8.73832152751838));
#19975=CARTESIAN_POINT('Ctrl Pts',(7.92226315679741,1.07524585818683,9.12864980257357));
#19976=CARTESIAN_POINT('Ctrl Pts',(7.69129240392847,1.01335743148039,9.57126835989378));
#19977=CARTESIAN_POINT('Ctrl Pts',(7.4152185798584,0.939383673269444,9.97380310172652));
#19978=CARTESIAN_POINT('Ctrl Pts',(7.1368016643945,0.864782085611728,10.2639387973189));
#19979=CARTESIAN_POINT('Ctrl Pts',(6.88183638015527,0.796464343601853,10.4339697781547));
#19980=CARTESIAN_POINT('Ctrl Pts',(6.60023402171546,0.721009219071207,10.5367578512231));
#19981=CARTESIAN_POINT('Ctrl Pts',(6.22971711106489,0.621729512080313,10.623044675585));
#19982=CARTESIAN_POINT('Ctrl Pts',(5.93468051661777,0.542674694860579,10.7102223023981));
#19983=CARTESIAN_POINT('Ctrl Pts',(5.64132565171833,0.464070495715032,10.8473463161695));
#19984=CARTESIAN_POINT('Ctrl Pts',(5.39460105858856,0.397960840233013,10.9821160664838));
#19985=CARTESIAN_POINT('Ctrl Pts',(5.06953125376008,0.310858648545478,11.1942553330246));
#19986=CARTESIAN_POINT('Ctrl Pts',(4.74015401319374,0.222602282930538,11.4563092607288));
#19987=CARTESIAN_POINT('Ctrl Pts',(4.54249036453264,0.169638467898806,11.6591099894158));
#19988=CARTESIAN_POINT('Ctrl Pts',(4.44483865181741,0.143472770337245,11.7628168777948));
#19989=CARTESIAN_POINT('Ctrl Pts',(4.19359661830351,0.510762161999066,2.99727332026023));
#19990=CARTESIAN_POINT('Ctrl Pts',(4.21373513499808,0.476613798189458,3.09465434585502));
#19991=CARTESIAN_POINT('Ctrl Pts',(4.26953516459727,0.380870576396472,3.3133840657309));
#19992=CARTESIAN_POINT('Ctrl Pts',(4.35198159611048,0.232981640725298,3.49493665183918));
#19993=CARTESIAN_POINT('Ctrl Pts',(4.40285823325642,0.132224151085984,3.57811407583586));
#19994=CARTESIAN_POINT('Ctrl Pts',(4.40285823325641,0.132224151085904,3.57811407583577));
#19995=CARTESIAN_POINT('Ctrl Pts',(4.43940677028145,0.142017302066303,3.71456495367834));
#19996=CARTESIAN_POINT('Ctrl Pts',(4.53463296379915,0.167533083717659,3.9794750710438));
#19997=CARTESIAN_POINT('Ctrl Pts',(4.76097163197783,0.228180347072074,4.33028299830215));
#19998=CARTESIAN_POINT('Ctrl Pts',(5.06150763834345,0.308708727274215,4.61783411696581));
#19999=CARTESIAN_POINT('Ctrl Pts',(5.40852054959526,0.401690556607312,4.85362603977077));
#20000=CARTESIAN_POINT('Ctrl Pts',(5.77679893037258,0.500370451326437,5.05954568690866));
#20001=CARTESIAN_POINT('Ctrl Pts',(6.28064189604197,0.635374767089651,5.31961833864166));
#20002=CARTESIAN_POINT('Ctrl Pts',(6.81213487368419,0.777787881231695,5.56423083230834));
#20003=CARTESIAN_POINT('Ctrl Pts',(7.25326088523284,0.895987239786518,5.73088688746923));
#20004=CARTESIAN_POINT('Ctrl Pts',(7.60545358372097,0.990356988926552,5.88645382774441));
#20005=CARTESIAN_POINT('Ctrl Pts',(7.89304985394669,1.06741817727973,6.03509348122348));
#20006=CARTESIAN_POINT('Ctrl Pts',(8.13408614953057,1.13200365802803,6.32217794399327));
#20007=CARTESIAN_POINT('Ctrl Pts',(8.21367576229283,1.15332963049358,6.52713122561373));
#20008=CARTESIAN_POINT('Ctrl Pts',(8.24820562306135,1.16258187880126,6.74090493270784));
#20009=CARTESIAN_POINT('Ctrl Pts',(8.22962792994722,1.1576040009341,6.99851570691194));
#20010=CARTESIAN_POINT('Ctrl Pts',(8.15840156120257,1.13851895294917,7.38504607625248));
#20011=CARTESIAN_POINT('Ctrl Pts',(8.08669712828127,1.11930580805417,7.85408399146071));
#20012=CARTESIAN_POINT('Ctrl Pts',(8.08101604477191,1.11778356631571,8.34143039554977));
#20013=CARTESIAN_POINT('Ctrl Pts',(8.03131448784197,1.10446607427376,8.73832152751838));
#20014=CARTESIAN_POINT('Ctrl Pts',(7.92226315679741,1.07524585818683,9.12864980257357));
#20015=CARTESIAN_POINT('Ctrl Pts',(7.69129240392847,1.01335743148039,9.57126835989378));
#20016=CARTESIAN_POINT('Ctrl Pts',(7.4152185798584,0.939383673269444,9.97380310172652));
#20017=CARTESIAN_POINT('Ctrl Pts',(7.1368016643945,0.864782085611728,10.2639387973189));
#20018=CARTESIAN_POINT('Ctrl Pts',(6.88183638015527,0.796464343601853,10.4339697781547));
#20019=CARTESIAN_POINT('Ctrl Pts',(6.60023402171546,0.721009219071207,10.5367578512231));
#20020=CARTESIAN_POINT('Ctrl Pts',(6.22971711106489,0.621729512080313,10.623044675585));
#20021=CARTESIAN_POINT('Ctrl Pts',(5.93468051661777,0.542674694860579,10.7102223023981));
#20022=CARTESIAN_POINT('Ctrl Pts',(5.64132565171833,0.464070495715032,10.8473463161695));
#20023=CARTESIAN_POINT('Ctrl Pts',(5.39460105858856,0.397960840233013,10.9821160664838));
#20024=CARTESIAN_POINT('Ctrl Pts',(5.06953125376008,0.310858648545478,11.1942553330246));
#20025=CARTESIAN_POINT('Ctrl Pts',(4.74015401319374,0.222602282930538,11.4563092607288));
#20026=CARTESIAN_POINT('Ctrl Pts',(4.54249036453264,0.169638467898806,11.6591099894158));
#20027=CARTESIAN_POINT('Ctrl Pts',(4.44483865181741,0.143472770337245,11.7628168777948));
#20028=CARTESIAN_POINT('Ctrl Pts',(4.4090533114332,0.109103804573277,3.57811407583577));
#20029=CARTESIAN_POINT('Ctrl Pts',(4.44559813622809,0.118895960864605,3.71455109438044));
#20030=CARTESIAN_POINT('Ctrl Pts',(4.54083607335543,0.14441488920668,3.97948069543409));
#20031=CARTESIAN_POINT('Ctrl Pts',(4.7671666003941,0.205059971149203,4.33027237668467));
#20032=CARTESIAN_POINT('Ctrl Pts',(5.06769840870851,0.285587226486915,4.61782723492783));
#20033=CARTESIAN_POINT('Ctrl Pts',(5.41470997442562,0.378568695285074,4.85362027669949));
#20034=CARTESIAN_POINT('Ctrl Pts',(5.78299034154921,0.477249122244079,5.05954319866726));
#20035=CARTESIAN_POINT('Ctrl Pts',(6.28684021661948,0.612255289375677,5.31961985792902));
#20036=CARTESIAN_POINT('Ctrl Pts',(6.81832385480766,0.754665901018556,5.564227040406));
#20037=CARTESIAN_POINT('Ctrl Pts',(7.25944357588469,0.872863574046589,5.73087878972347));
#20038=CARTESIAN_POINT('Ctrl Pts',(7.61163865214237,0.967233960308051,5.88644101461346));
#20039=CARTESIAN_POINT('Ctrl Pts',(7.89922275747532,1.04429188908804,6.03505547921762));
#20040=CARTESIAN_POINT('Ctrl Pts',(8.14029443856229,1.10888685135331,6.32215841122141));
#20041=CARTESIAN_POINT('Ctrl Pts',(8.21989163690174,1.13021485636814,6.5271379469616));
#20042=CARTESIAN_POINT('Ctrl Pts',(8.25441840505932,1.13946627601322,6.74093595724302));
#20043=CARTESIAN_POINT('Ctrl Pts',(8.23582818046237,1.13448504034536,6.99854971389734));
#20044=CARTESIAN_POINT('Ctrl Pts',(8.16459707704539,1.1153987237088,7.3850681120554));
#20045=CARTESIAN_POINT('Ctrl Pts',(8.09289299023897,1.09618567155501,7.85407732011957));
#20046=CARTESIAN_POINT('Ctrl Pts',(8.0872159078158,1.09466450190436,8.34140461217029));
#20047=CARTESIAN_POINT('Ctrl Pts',(8.03751561754474,1.08134734926263,8.73830742082599));
#20048=CARTESIAN_POINT('Ctrl Pts',(7.92846039739064,1.05212609109194,9.12865849166385));
#20049=CARTESIAN_POINT('Ctrl Pts',(7.69748287548657,0.990235850628008,9.5712757246142));
#20050=CARTESIAN_POINT('Ctrl Pts',(7.42143118324782,0.916268022623389,9.97378978761487));
#20051=CARTESIAN_POINT('Ctrl Pts',(7.14300814718688,0.841664794956637,10.2639374823751));
#20052=CARTESIAN_POINT('Ctrl Pts',(6.88801376154103,0.773339255248362,10.4339879035537));
#20053=CARTESIAN_POINT('Ctrl Pts',(6.60641208432421,0.697884313250866,10.536766070865));
#20054=CARTESIAN_POINT('Ctrl Pts',(6.23589390298475,0.598604265779908,10.6230512239787));
#20055=CARTESIAN_POINT('Ctrl Pts',(5.94087044850798,0.519552969404618,10.7102267075257));
#20056=CARTESIAN_POINT('Ctrl Pts',(5.64752558195459,0.440951449307822,10.8473451314547));
#20057=CARTESIAN_POINT('Ctrl Pts',(5.40080787303593,0.37484363844461,10.9821110393344));
#20058=CARTESIAN_POINT('Ctrl Pts',(5.07572294615792,0.287737394816118,11.1942590991363));
#20059=CARTESIAN_POINT('Ctrl Pts',(4.74634791397138,0.19948162093476,11.4563122548706));
#20060=CARTESIAN_POINT('Ctrl Pts',(4.54868443730922,0.146517851990004,11.6591110571587));
#20061=CARTESIAN_POINT('Ctrl Pts',(4.4510337299942,0.120352423824617,11.7628168777948));
#20062=CARTESIAN_POINT('Ctrl Pts',(4.40106171131969,0.0640775387299355,
3.5834861945331));
#20063=CARTESIAN_POINT('Ctrl Pts',(4.43790303359015,0.0739491412803999,
3.72103016137481));
#20064=CARTESIAN_POINT('Ctrl Pts',(4.53402257603767,0.0997042950560617,
3.98857423439157));
#20065=CARTESIAN_POINT('Ctrl Pts',(4.76306341192281,0.161075602065234,4.34358222601213));
#20066=CARTESIAN_POINT('Ctrl Pts',(5.06667005322962,0.24242675642012,4.63394435000544));
#20067=CARTESIAN_POINT('Ctrl Pts',(5.41565268579315,0.335936370988005,4.87101890352248));
#20068=CARTESIAN_POINT('Ctrl Pts',(5.7849003361388,0.434875980705211,5.07744965319006));
#20069=CARTESIAN_POINT('Ctrl Pts',(6.28913493446496,0.569985234122539,5.33776665098138));
#20070=CARTESIAN_POINT('Ctrl Pts',(6.82196111316944,0.712755578412563,5.58292297422199));
#20071=CARTESIAN_POINT('Ctrl Pts',(7.26330723858452,0.83101391630014,5.74971217255928));
#20072=CARTESIAN_POINT('Ctrl Pts',(7.61396716546967,0.924972960526974,5.90453629054123));
#20073=CARTESIAN_POINT('Ctrl Pts',(7.89891366870189,1.00132414595412,6.05235368516109));
#20074=CARTESIAN_POINT('Ctrl Pts',(8.13437391799379,1.06441552960151,6.33330907644365));
#20075=CARTESIAN_POINT('Ctrl Pts',(8.21170963215847,1.08513757175802,6.53255536921129));
#20076=CARTESIAN_POINT('Ctrl Pts',(8.24550570678105,1.09419320266049,6.74112857932929));
#20077=CARTESIAN_POINT('Ctrl Pts',(8.22735380727456,1.08932941584663,6.99539650801542));
#20078=CARTESIAN_POINT('Ctrl Pts',(8.15627988619041,1.07028521608922,7.38089406911332));
#20079=CARTESIAN_POINT('Ctrl Pts',(8.08417079901181,1.05096364441277,7.8529025756585));
#20080=CARTESIAN_POINT('Ctrl Pts',(8.07851394340125,1.04944789452022,8.34085105008331));
#20081=CARTESIAN_POINT('Ctrl Pts',(8.02910143470183,1.03620785271821,8.73430700697211));
#20082=CARTESIAN_POINT('Ctrl Pts',(7.92127213001242,1.00731507760628,9.12048137472438));
#20083=CARTESIAN_POINT('Ctrl Pts',(7.69186349651382,0.9458452195236,9.56036990607636));
#20084=CARTESIAN_POINT('Ctrl Pts',(7.41674295651521,0.872126893009758,9.96140578441748));
#20085=CARTESIAN_POINT('Ctrl Pts',(7.14117040174745,0.798287449503556,10.2483733431293));
#20086=CARTESIAN_POINT('Ctrl Pts',(6.8902954129788,0.731065698861828,10.4156376689661));
#20087=CARTESIAN_POINT('Ctrl Pts',(6.61225089452466,0.65656389468214,10.5172850890292));
#20088=CARTESIAN_POINT('Ctrl Pts',(6.24261997408572,0.557521588052954,10.603363191263));
#20089=CARTESIAN_POINT('Ctrl Pts',(5.94489265314603,0.477745792842484,10.6912647738558));
#20090=CARTESIAN_POINT('Ctrl Pts',(5.6495876077844,0.398619044416999,10.8293357996365));
#20091=CARTESIAN_POINT('Ctrl Pts',(5.40165483192268,0.332185657347644,10.9647672453765));
#20092=CARTESIAN_POINT('Ctrl Pts',(5.07547427893545,0.244785841587978,11.1776402225937));
#20093=CARTESIAN_POINT('Ctrl Pts',(4.74424250329149,0.156032554796651,11.4411353182047));
#20094=CARTESIAN_POINT('Ctrl Pts',(4.5455807954736,0.102801310619861,11.6449924329457));
#20095=CARTESIAN_POINT('Ctrl Pts',(4.44784978639617,0.076614365662085,11.7487835346862));
#20096=CARTESIAN_POINT('Ctrl Pts',(4.36580935114124,0.0394748386098602,
3.59469433164577));
#20097=CARTESIAN_POINT('Ctrl Pts',(4.40325934412277,0.0495095339858135,
3.73451071920807));
#20098=CARTESIAN_POINT('Ctrl Pts',(4.50124963302018,0.0757659527619658,
4.00756161013495));
#20099=CARTESIAN_POINT('Ctrl Pts',(4.73592335833677,0.13864658794535,4.37132286716819));
#20100=CARTESIAN_POINT('Ctrl Pts',(5.0459339603424,0.221713678397845,4.66755193997466));
#20101=CARTESIAN_POINT('Ctrl Pts',(5.39902533614519,0.316324227398598,4.90730317213381));
#20102=CARTESIAN_POINT('Ctrl Pts',(5.77029639310752,0.415806007284703,5.11480218775024));
#20103=CARTESIAN_POINT('Ctrl Pts',(6.27535213809375,0.551135286286462,5.37563133408309));
#20104=CARTESIAN_POINT('Ctrl Pts',(6.81095435368323,0.694649467417985,5.6219191550161));
#20105=CARTESIAN_POINT('Ctrl Pts',(7.25275601568305,0.81302986596556,5.78898360528629));
#20106=CARTESIAN_POINT('Ctrl Pts',(7.60021943769446,0.906132409292876,5.94225516102438));
#20107=CARTESIAN_POINT('Ctrl Pts',(7.87963043829654,0.981000361260572,6.08834222260924));
#20108=CARTESIAN_POINT('Ctrl Pts',(8.10347789154437,1.04098010558609,6.35652106548154));
#20109=CARTESIAN_POINT('Ctrl Pts',(8.17611563731258,1.0604433309047,6.54387600067759));
#20110=CARTESIAN_POINT('Ctrl Pts',(8.20837895644931,1.06908826121254,6.74161342706472));
#20111=CARTESIAN_POINT('Ctrl Pts',(8.19110804451059,1.06446053430601,6.98890875288788));
#20112=CARTESIAN_POINT('Ctrl Pts',(8.12034939918785,1.04550081243426,7.37224447234147));
#20113=CARTESIAN_POINT('Ctrl Pts',(8.04739626380834,1.025953078724,7.85043380236922));
#20114=CARTESIAN_POINT('Ctrl Pts',(8.0417923087215,1.02445150348406,8.33962717062775));
#20115=CARTESIAN_POINT('Ctrl Pts',(7.99298360150036,1.01137324980055,8.72592300463577));
#20116=CARTESIAN_POINT('Ctrl Pts',(7.88770158869635,0.983163019492191,9.10344425805828));
#20117=CARTESIAN_POINT('Ctrl Pts',(7.66154810789234,0.922565376945272,9.53763621224937));
#20118=CARTESIAN_POINT('Ctrl Pts',(7.38842946831295,0.849383458032085,9.93553277313259));
#20119=CARTESIAN_POINT('Ctrl Pts',(7.11878765582192,0.777133152129452,10.2158975345821));
#20120=CARTESIAN_POINT('Ctrl Pts',(6.87642935703478,0.712193441690456,10.3774010714523));
#20121=CARTESIAN_POINT('Ctrl Pts',(6.60580815001857,0.639680707815727,10.476662862038));
#20122=CARTESIAN_POINT('Ctrl Pts',(6.23802497096264,0.541133501997939,10.5623045135241));
#20123=CARTESIAN_POINT('Ctrl Pts',(5.9346915702303,0.459855562234322,10.6517152633816));
#20124=CARTESIAN_POINT('Ctrl Pts',(5.63532363844642,0.379640166673058,10.7917588039818));
#20125=CARTESIAN_POINT('Ctrl Pts',(5.3848742144548,0.312532445769662,10.9285685208154));
#20126=CARTESIAN_POINT('Ctrl Pts',(5.05636735697362,0.224509298599493,11.1429774479459));
#20127=CARTESIAN_POINT('Ctrl Pts',(4.72126766459807,0.134719606643546,11.4094788749468));
#20128=CARTESIAN_POINT('Ctrl Pts',(4.52052375398258,0.0809304379086621,
11.6155388514382));
#20129=CARTESIAN_POINT('Ctrl Pts',(4.42262789584284,0.0546993217777655,
11.719505024182));
#20130=CARTESIAN_POINT('Ctrl Pts',(4.34909964308327,0.0349974858299679,
3.59949138964752));
#20131=CARTESIAN_POINT('Ctrl Pts',(4.38680976101687,0.0451018814767583,
3.74027893176065));
#20132=CARTESIAN_POINT('Ctrl Pts',(4.48560194249773,0.071573166723062,4.01568874810612));
#20133=CARTESIAN_POINT('Ctrl Pts',(4.72268568825884,0.135099564938299,4.38319469956436));
#20134=CARTESIAN_POINT('Ctrl Pts',(5.0354367362137,0.21890095566979,4.68193520114933));
#20135=CARTESIAN_POINT('Ctrl Pts',(5.39028650561027,0.313982664813972,4.92283216185341));
#20136=CARTESIAN_POINT('Ctrl Pts',(5.76242378203297,0.413696547504953,5.13078873237884));
#20137=CARTESIAN_POINT('Ctrl Pts',(6.26783169213932,0.54912018886625,5.39183749253912));
#20138=CARTESIAN_POINT('Ctrl Pts',(6.8046210773698,0.692952471144354,5.63860904148901));
#20139=CARTESIAN_POINT('Ctrl Pts',(7.24661705601864,0.811384936681117,5.80579085268058));
#20140=CARTESIAN_POINT('Ctrl Pts',(7.59271262743873,0.904120965547118,5.95839742644866));
#20141=CARTESIAN_POINT('Ctrl Pts',(7.8697531842168,0.978353759006469,6.10374129848354));
#20142=CARTESIAN_POINT('Ctrl Pts',(8.08863405403125,1.03700271131187,6.36645372110484));
#20143=CARTESIAN_POINT('Ctrl Pts',(8.15926186591506,1.05592737646932,6.54872190268123));
#20144=CARTESIAN_POINT('Ctrl Pts',(8.19086884853079,1.06439644193639,6.74182415651423));
#20145=CARTESIAN_POINT('Ctrl Pts',(8.17397369844545,1.05986940011502,6.98613553279737));
#20146=CARTESIAN_POINT('Ctrl Pts',(8.10334949970651,1.04094570309683,7.36854474797747));
#20147=CARTESIAN_POINT('Ctrl Pts',(8.03003514943051,1.02130118214676,7.84937648135502));
#20148=CARTESIAN_POINT('Ctrl Pts',(8.02445425036305,1.01980578474859,8.33910068047419));
#20149=CARTESIAN_POINT('Ctrl Pts',(7.97590410013386,1.00679681120227,8.72233320794333));
#20150=CARTESIAN_POINT('Ctrl Pts',(7.87171191954179,0.978878600554987,9.09615331026656));
#20151=CARTESIAN_POINT('Ctrl Pts',(7.64695093531355,0.918654076341007,9.5279070047071));
#20152=CARTESIAN_POINT('Ctrl Pts',(7.37469139866462,0.845702353364252,9.92445780127518));
#20153=CARTESIAN_POINT('Ctrl Pts',(7.10758729640882,0.774132024869772,10.2019978237482));
#20154=CARTESIAN_POINT('Ctrl Pts',(6.86887110582377,0.710168214382273,10.3610377706145));
#20155=CARTESIAN_POINT('Ctrl Pts',(6.60142713036405,0.638506817137273,10.4592774903079));
#20156=CARTESIAN_POINT('Ctrl Pts',(6.23443464884433,0.540171478085771,10.5447321686106));
#20157=CARTESIAN_POINT('Ctrl Pts',(5.92870322026153,0.458250988696196,10.6347886165848));
#20158=CARTESIAN_POINT('Ctrl Pts',(5.62759741836264,0.377569932241062,10.7756758097979));
#20159=CARTESIAN_POINT('Ctrl Pts',(5.37607158806058,0.310173789136056,10.9130750253569));
#20160=CARTESIAN_POINT('Ctrl Pts',(5.04656750998174,0.22188343751207,11.1281422470874));
#20161=CARTESIAN_POINT('Ctrl Pts',(4.70981258666106,0.131650227761089,11.3959302972882));
#20162=CARTESIAN_POINT('Ctrl Pts',(4.50817751566127,0.0776222733209033,
11.6029328940868));
#20163=CARTESIAN_POINT('Ctrl Pts',(4.4102112066954,0.0513722799480404,11.706973886163));
#20164=CARTESIAN_POINT('Origin',(4.32839411947507,0.112271551933094,3.59949138964752));
#20165=CARTESIAN_POINT('Origin',(4.33293714059227,0.0306667563398384,3.08701851589662));
#20166=CARTESIAN_POINT('Ctrl Pts',(4.33135810013194,0.0365598155649942,
11.6149485836148));
#20167=CARTESIAN_POINT('Ctrl Pts',(4.33187792676856,0.0346197961459941,
11.6082911303789));
#20168=CARTESIAN_POINT('Ctrl Pts',(4.33227188276068,0.0331495322847722,
11.6014592124169));
#20169=CARTESIAN_POINT('Ctrl Pts',(4.33280071341379,0.0311759094187438,
11.5876929996279));
#20170=CARTESIAN_POINT('Ctrl Pts',(4.33293714059227,0.0306667563398198,
11.5807132391622));
#20171=CARTESIAN_POINT('Ctrl Pts',(4.33293714059227,0.0306667563398385,
11.5737513317737));
#20172=CARTESIAN_POINT('Origin',(2.05,0.08,1.28));
#20173=CARTESIAN_POINT('',(-2.803641505311,0.,1.28));
#20174=CARTESIAN_POINT('',(2.05,0.,1.28));
#20175=CARTESIAN_POINT('',(-2.803641505311,0.08,1.2));
#20176=CARTESIAN_POINT('Origin',(-2.803641505311,0.08,1.28));
#20177=CARTESIAN_POINT('',(2.05,0.08,1.2));
#20178=CARTESIAN_POINT('Ctrl Pts',(-2.96341860243295,0.00343337974884617,
1.1214615033794));
#20179=CARTESIAN_POINT('Ctrl Pts',(-2.96630515786593,0.00868558376862438,
1.06150427209154));
#20180=CARTESIAN_POINT('Ctrl Pts',(-2.96893720254462,0.0199743192711058,
1.00206230831012));
#20181=CARTESIAN_POINT('Ctrl Pts',(-2.97150840940722,0.0370763911099046,
0.944338416612715));
#20182=CARTESIAN_POINT('Ctrl Pts',(-2.93958582132551,0.00354285648575689,
1.12021175717555));
#20183=CARTESIAN_POINT('Ctrl Pts',(-2.94251954168973,0.00887597719617225,
1.06031972093586));
#20184=CARTESIAN_POINT('Ctrl Pts',(-2.94518955488367,0.0202169542943542,
1.00097374956333));
#20185=CARTESIAN_POINT('Ctrl Pts',(-2.94780986467339,0.0373919530059805,
0.943273314040079));
#20186=CARTESIAN_POINT('Ctrl Pts',(-2.89832135056165,0.0236236998221979,
1.11979038686963));
#20187=CARTESIAN_POINT('Ctrl Pts',(-2.90132976176868,0.0288805527885566,
1.06138252620797));
#20188=CARTESIAN_POINT('Ctrl Pts',(-2.90406886065643,0.0400205415337996,
1.00340420949257));
#20189=CARTESIAN_POINT('Ctrl Pts',(-2.90676750629242,0.0568440093652064,
0.94702993218099));
#20190=CARTESIAN_POINT('Ctrl Pts',(-2.8836123610279,0.0652969522995559,
1.12266369893431));
#20191=CARTESIAN_POINT('Ctrl Pts',(-2.88654643974598,0.0702232785018827,
1.06706918382192));
#20192=CARTESIAN_POINT('Ctrl Pts',(-2.88922109707321,0.0807651986054815,
1.01185481384779));
#20193=CARTESIAN_POINT('Ctrl Pts',(-2.89185038905304,0.096718663397188,
0.958114462937943));
#20194=CARTESIAN_POINT('Ctrl Pts',(-2.88353005387197,0.0831281904378376,
1.12422135153951));
#20195=CARTESIAN_POINT('Ctrl Pts',(-2.88640514642651,0.08791353187808,1.06981058545882));
#20196=CARTESIAN_POINT('Ctrl Pts',(-2.88903159296831,0.0981988242247885,
1.01577166814133));
#20197=CARTESIAN_POINT('Ctrl Pts',(-2.89160384326392,0.113780711900135,
0.963157446086756));
#20198=CARTESIAN_POINT('',(-2.97150840945859,0.0370763914516166,0.944338415459349));
#20199=CARTESIAN_POINT('',(-2.89160384334168,0.113780712456408,0.963157444496232));
#20200=CARTESIAN_POINT('Origin',(-2.97150840940722,0.113780711900135,0.967063890691585));
#20201=CARTESIAN_POINT('',(-2.88353005387197,0.0831281904378376,1.12422135153951));
#20202=CARTESIAN_POINT('Ctrl Pts',(-2.89160384326392,0.113780711900135,
0.963157446086756));
#20203=CARTESIAN_POINT('Ctrl Pts',(-2.88903159296831,0.0981988242247885,
1.01577166814133));
#20204=CARTESIAN_POINT('Ctrl Pts',(-2.88640514642651,0.08791353187808,1.06981058545882));
#20205=CARTESIAN_POINT('Ctrl Pts',(-2.88353005387197,0.0831281904378376,
1.12422135153951));
#20206=CARTESIAN_POINT('',(-2.96341860243295,0.00343337974884617,1.1214615033794));
#20207=CARTESIAN_POINT('Origin',(-2.96341860243295,0.0831281904378376,1.12844270307901));
#20208=CARTESIAN_POINT('Ctrl Pts',(-2.96341860243295,0.00343337974884617,
1.1214615033794));
#20209=CARTESIAN_POINT('Ctrl Pts',(-2.96630515786593,0.00868558376862438,
1.06150427209154));
#20210=CARTESIAN_POINT('Ctrl Pts',(-2.96893720254462,0.0199743192711058,
1.00206230831012));
#20211=CARTESIAN_POINT('Ctrl Pts',(-2.97150840940722,0.0370763911099046,
0.944338416612715));
#20212=CARTESIAN_POINT('Ctrl Pts',(-2.94220556991652,1.38777878078145E-17,
1.19999999999997));
#20213=CARTESIAN_POINT('Ctrl Pts',(-2.95477525929363,7.99204335707293E-16,
1.17610462613062));
#20214=CARTESIAN_POINT('Ctrl Pts',(-2.96209712200597,0.00102889281907461,
1.14891024269609));
#20215=CARTESIAN_POINT('Ctrl Pts',(-2.96341860243295,0.00343337974884619,
1.1214615033794));
#20216=CARTESIAN_POINT('Ctrl Pts',(-2.92147643432527,4.12491330437235E-16,
1.1880320279863));
#20217=CARTESIAN_POINT('Ctrl Pts',(-2.93233653942741,0.0003274672410604,
1.16750429943543));
#20218=CARTESIAN_POINT('Ctrl Pts',(-2.93864796914417,0.00143185455554525,
1.14395403171255));
#20219=CARTESIAN_POINT('Ctrl Pts',(-2.93958582132551,0.00354285648575692,
1.12021175717555));
#20220=CARTESIAN_POINT('Ctrl Pts',(-2.88559036993739,0.0200923283589629,
1.16731319905181));
#20221=CARTESIAN_POINT('Ctrl Pts',(-2.89349138284601,0.0205972730886243,
1.15311091289949));
#20222=CARTESIAN_POINT('Ctrl Pts',(-2.89801951662537,0.0217263036549144,
1.13650101054829));
#20223=CARTESIAN_POINT('Ctrl Pts',(-2.89832153725836,0.0236238550069256,
1.11979041032883));
#20224=CARTESIAN_POINT('Ctrl Pts',(-2.87292353761376,0.0620480419794871,
1.15999999999999));
#20225=CARTESIAN_POINT('Ctrl Pts',(-2.87941161142243,0.0621984441063758,
1.1487678034684));
#20226=CARTESIAN_POINT('Ctrl Pts',(-2.88316790462212,0.0631932819332653,
1.13573901604496));
#20227=CARTESIAN_POINT('Ctrl Pts',(-2.8836123610279,0.0652969522995559,
1.1226636989343));
#20228=CARTESIAN_POINT('Ctrl Pts',(-2.87292353761376,0.08,1.15999999999999));
#20229=CARTESIAN_POINT('Ctrl Pts',(-2.87920838230231,0.0800000000000008,
1.14911432968172));
#20230=CARTESIAN_POINT('Ctrl Pts',(-2.88286931365848,0.0809374356795997,
1.13672577722824));
#20231=CARTESIAN_POINT('Ctrl Pts',(-2.88353005387198,0.0831281904378377,
1.12422135153951));
#20232=CARTESIAN_POINT('',(-2.87292353761376,0.08,1.15999999999998));
#20233=CARTESIAN_POINT('Ctrl Pts',(-2.88353005387198,0.0831281904378377,
1.12422135153951));
#20234=CARTESIAN_POINT('Ctrl Pts',(-2.88286931365848,0.0809374356795997,
1.13672577722824));
#20235=CARTESIAN_POINT('Ctrl Pts',(-2.87917379579497,0.0800000000000008,
1.14909623365625));
#20236=CARTESIAN_POINT('Ctrl Pts',(-2.87291508431494,0.08,1.15999514568442));
#20237=CARTESIAN_POINT('',(-2.94220556991652,1.81603863891322E-17,1.19999999999998));
#20238=CARTESIAN_POINT('Origin',(-2.94220556991652,0.08,1.19999999999997));
#20239=CARTESIAN_POINT('Ctrl Pts',(-2.94220556991652,1.38777878078145E-17,
1.19999999999997));
#20240=CARTESIAN_POINT('Ctrl Pts',(-2.95477525929363,7.99204335707293E-16,
1.17610462613062));
#20241=CARTESIAN_POINT('Ctrl Pts',(-2.96209712200597,0.00102889281907461,
1.14891024269609));
#20242=CARTESIAN_POINT('Ctrl Pts',(-2.96341860243295,0.00343337974884619,
1.1214615033794));
#20243=CARTESIAN_POINT('Ctrl Pts',(-2.97150840951392,0.0370763918196141,
0.944338414217263));
#20244=CARTESIAN_POINT('Ctrl Pts',(-2.9722976916079,0.0423262056041848,
0.926618942442153));
#20245=CARTESIAN_POINT('Ctrl Pts',(-2.9704006751309,0.0481782537629969,
0.908937053039817));
#20246=CARTESIAN_POINT('Ctrl Pts',(-2.96590341962731,0.0542766412925386,
0.892181871007293));
#20247=CARTESIAN_POINT('Ctrl Pts',(-2.94780986478466,0.0373919537646065,
0.943273311490377));
#20248=CARTESIAN_POINT('Ctrl Pts',(-2.94857578158365,0.0419549531652315,
0.927965726332386));
#20249=CARTESIAN_POINT('Ctrl Pts',(-2.9469952950528,0.0469737957410308,
0.912624042243611));
#20250=CARTESIAN_POINT('Ctrl Pts',(-2.94308190554019,0.0521158688929946,
0.89811854438363));
#20251=CARTESIAN_POINT('Ctrl Pts',(-2.90676705829981,0.056843651940239,
0.947029801368067));
#20252=CARTESIAN_POINT('Ctrl Pts',(-2.90748135565274,0.059940306716287,
0.936220750290145));
#20253=CARTESIAN_POINT('Ctrl Pts',(-2.90645413242085,0.0633115026576812,
0.925322801814758));
#20254=CARTESIAN_POINT('Ctrl Pts',(-2.90355489767837,0.0668278028163856,
0.915117754801607));
#20255=CARTESIAN_POINT('Ctrl Pts',(-2.89185038918151,0.0967186642359907,
0.95811446019075));
#20256=CARTESIAN_POINT('Ctrl Pts',(-2.89236030863334,0.0988989884558824,
0.949564065008555));
#20257=CARTESIAN_POINT('Ctrl Pts',(-2.89145639520232,0.101358036048963,
0.940957760954761));
#20258=CARTESIAN_POINT('Ctrl Pts',(-2.88910171978587,0.104230462691718,
0.932989060257172));
#20259=CARTESIAN_POINT('Ctrl Pts',(-2.89160384339595,0.11378071272758,0.963157443386126));
#20260=CARTESIAN_POINT('Ctrl Pts',(-2.89200506610289,0.115786605025646,
0.954950614685553));
#20261=CARTESIAN_POINT('Ctrl Pts',(-2.89106334819291,0.118074599969182,
0.946756646504643));
#20262=CARTESIAN_POINT('Ctrl Pts',(-2.88881405854803,0.120889693311755,
0.939137268222128));
#20263=CARTESIAN_POINT('',(-2.9659034196274,0.0542766412925467,0.892181871007271));
#20264=CARTESIAN_POINT('',(-2.88881405854801,0.120889693312663,0.939137268222463));
#20265=CARTESIAN_POINT('Origin',(-2.96590341962731,0.129452050955424,0.919543482473312));
#20266=CARTESIAN_POINT('Ctrl Pts',(-2.88881405854803,0.120889693311755,
0.939137268222128));
#20267=CARTESIAN_POINT('Ctrl Pts',(-2.89106334819291,0.118074599969182,
0.946756646504643));
#20268=CARTESIAN_POINT('Ctrl Pts',(-2.89200506610289,0.115786605025646,
0.954950614685553));
#20269=CARTESIAN_POINT('Ctrl Pts',(-2.89160384339595,0.11378071272758,0.963157443386126));
#20270=CARTESIAN_POINT('Ctrl Pts',(-2.97150840951392,0.0370763918196141,
0.944338414217263));
#20271=CARTESIAN_POINT('Ctrl Pts',(-2.9722976916079,0.0423262056041848,
0.926618942442153));
#20272=CARTESIAN_POINT('Ctrl Pts',(-2.9704006751309,0.0481782537629969,
0.908937053039817));
#20273=CARTESIAN_POINT('Ctrl Pts',(-2.96590341962731,0.0542766412925386,
0.892181871007293));
#20274=CARTESIAN_POINT('Ctrl Pts',(-2.803641505311,0.,1.28));
#20275=CARTESIAN_POINT('Ctrl Pts',(-2.83156585186791,0.,1.28));
#20276=CARTESIAN_POINT('Ctrl Pts',(-2.8873697166731,0.,1.26501863102788));
#20277=CARTESIAN_POINT('Ctrl Pts',(-2.92824339663807,0.,1.22418319350235));
#20278=CARTESIAN_POINT('Ctrl Pts',(-2.94220556991652,0.,1.19999999999998));
#20279=CARTESIAN_POINT('Ctrl Pts',(-2.803641505311,0.,1.25606405597265));
#20280=CARTESIAN_POINT('Ctrl Pts',(-2.82737027930954,0.,1.25606405597265));
#20281=CARTESIAN_POINT('Ctrl Pts',(-2.87483488599671,1.25420474925568E-17,
1.24330810087636));
#20282=CARTESIAN_POINT('Ctrl Pts',(-2.90961204732599,-6.04209133589596E-17,
1.20858174906972));
#20283=CARTESIAN_POINT('Ctrl Pts',(-2.92147643432527,-4.86342276316735E-17,
1.1880320279863));
#20284=CARTESIAN_POINT('Ctrl Pts',(-2.803641505311,0.0200923513320623,1.21462642566814));
#20285=CARTESIAN_POINT('Ctrl Pts',(-2.8201635207438,0.0200923513320623,
1.21462642566814));
#20286=CARTESIAN_POINT('Ctrl Pts',(-2.85316323302638,0.0200923513320623,
1.20577244147847));
#20287=CARTESIAN_POINT('Ctrl Pts',(-2.87732938609252,0.0200923513320622,
1.18162169792061));
#20288=CARTESIAN_POINT('Ctrl Pts',(-2.88559039380893,0.0200923513320622,
1.16731321283406));
#20289=CARTESIAN_POINT('Ctrl Pts',(-2.803641505311,0.0620480419794869,1.2));
#20290=CARTESIAN_POINT('Ctrl Pts',(-2.81759233090944,0.0620480419794869,
1.2));
#20291=CARTESIAN_POINT('Ctrl Pts',(-2.84549989357585,0.0620480419794869,
1.19249941381066));
#20292=CARTESIAN_POINT('Ctrl Pts',(-2.86594812481452,0.0620480419794869,
1.17208176937204));
#20293=CARTESIAN_POINT('Ctrl Pts',(-2.87292353761376,0.0620480419794869,
1.15999999999999));
#20294=CARTESIAN_POINT('Ctrl Pts',(-2.803641505311,0.08,1.2));
#20295=CARTESIAN_POINT('Ctrl Pts',(-2.81760367858943,0.08,1.2));
#20296=CARTESIAN_POINT('Ctrl Pts',(-2.84550561099204,0.08,1.19250931551394));
#20297=CARTESIAN_POINT('Ctrl Pts',(-2.86594245097452,0.08,1.17209159675119));
#20298=CARTESIAN_POINT('Ctrl Pts',(-2.87292353761376,0.08,1.15999999999999));
#20299=CARTESIAN_POINT('Ctrl Pts',(-2.87292353215132,0.08,1.1600000094612));
#20300=CARTESIAN_POINT('Ctrl Pts',(-2.86594244564417,0.08,1.17209160207655));
#20301=CARTESIAN_POINT('Ctrl Pts',(-2.84550560735334,0.08,1.1925093164908));
#20302=CARTESIAN_POINT('Ctrl Pts',(-2.81760367858943,0.08,1.2));
#20303=CARTESIAN_POINT('Ctrl Pts',(-2.803641505311,0.08,1.2));
#20304=CARTESIAN_POINT('Ctrl Pts',(-2.803641505311,0.,1.28));
#20305=CARTESIAN_POINT('Ctrl Pts',(-2.83156585186791,0.,1.28));
#20306=CARTESIAN_POINT('Ctrl Pts',(-2.8873697166731,0.,1.26501863102788));
#20307=CARTESIAN_POINT('Ctrl Pts',(-2.92824339663807,0.,1.22418319350235));
#20308=CARTESIAN_POINT('Ctrl Pts',(-2.94220556991652,0.,1.19999999999998));
#20309=CARTESIAN_POINT('Ctrl Pts',(-2.87936339380758,0.129452051231406,
0.919543482573353));
#20310=CARTESIAN_POINT('Ctrl Pts',(-2.88146283528349,0.12700291504183,0.922197454617062));
#20311=CARTESIAN_POINT('Ctrl Pts',(-2.88513307556505,0.12490800002558,0.928743709056956));
#20312=CARTESIAN_POINT('Ctrl Pts',(-2.88777400865552,0.122191365716222,
0.935614140915412));
#20313=CARTESIAN_POINT('Ctrl Pts',(-2.88881405885504,0.120889693194046,
0.939137269378581));
#20314=CARTESIAN_POINT('Ctrl Pts',(-2.87936339372816,0.106959621146319,
0.911356907579326));
#20315=CARTESIAN_POINT('Ctrl Pts',(-2.88181984292263,0.104843095498008,
0.91387702531295));
#20316=CARTESIAN_POINT('Ctrl Pts',(-2.88543932888245,0.102667578804832,
0.920501736474717));
#20317=CARTESIAN_POINT('Ctrl Pts',(-2.88815026196516,0.0999776780681394,
0.927409871210725));
#20318=CARTESIAN_POINT('Ctrl Pts',(-2.88919760708753,0.0986773855985862,
0.930939658748897));
#20319=CARTESIAN_POINT('Ctrl Pts',(-2.89636159093292,0.0716838001108839,
0.8871184305754));
#20320=CARTESIAN_POINT('Ctrl Pts',(-2.89953989153624,0.0700649159705931,
0.890573780537225));
#20321=CARTESIAN_POINT('Ctrl Pts',(-2.90406236399545,0.0671359894824263,
0.898820413092617));
#20322=CARTESIAN_POINT('Ctrl Pts',(-2.90746777995082,0.0639291528782548,
0.907488124439835));
#20323=CARTESIAN_POINT('Ctrl Pts',(-2.90878614712001,0.0623073044369298,
0.911931323621345));
#20324=CARTESIAN_POINT('Ctrl Pts',(-2.93185794276191,0.0655906976416168,
0.861096582782205));
#20325=CARTESIAN_POINT('Ctrl Pts',(-2.93571995395406,0.0636246040882168,
0.866508892071219));
#20326=CARTESIAN_POINT('Ctrl Pts',(-2.94222111396444,0.0594240163271901,
0.87804374409531));
#20327=CARTESIAN_POINT('Ctrl Pts',(-2.94693586861888,0.0549402807148656,
0.890358235333227));
#20328=CARTESIAN_POINT('Ctrl Pts',(-2.94878744727228,0.0526560220635993,
0.896634315718971));
#20329=CARTESIAN_POINT('Ctrl Pts',(-2.94704588059102,0.0688641988014324,
0.852102886147849));
#20330=CARTESIAN_POINT('Ctrl Pts',(-2.95120132743568,0.0666088423893841,
0.858299426813201));
#20331=CARTESIAN_POINT('Ctrl Pts',(-2.95854860928908,0.0618941129944658,
0.871253039452356));
#20332=CARTESIAN_POINT('Ctrl Pts',(-2.96382417230887,0.0568458522077424,
0.885123022035033));
#20333=CARTESIAN_POINT('Ctrl Pts',(-2.965903663846,0.0542766635868824,0.892181809755297));
#20334=CARTESIAN_POINT('',(-2.96041704457315,0.0598643409482463,0.876829792382116));
#20335=CARTESIAN_POINT('',(-2.87936339380758,0.129452050955555,0.919543482472952));
#20336=CARTESIAN_POINT('Ctrl Pts',(-2.96041669789433,0.0598642771869273,
0.876829967575949));
#20337=CARTESIAN_POINT('Ctrl Pts',(-2.96041641286921,0.0598644584628993,
0.876829469535466));
#20338=CARTESIAN_POINT('Ctrl Pts',(-2.96041607078052,0.0598646469725351,
0.87682895162779));
#20339=CARTESIAN_POINT('Ctrl Pts',(-2.96041508469685,0.0598650593064606,
0.876827818832396));
#20340=CARTESIAN_POINT('Ctrl Pts',(-2.96041443818893,0.0598652486069508,
0.876827298805383));
#20341=CARTESIAN_POINT('Ctrl Pts',(-2.96041272590323,0.0598655661020481,
0.876826426772454));
#20342=CARTESIAN_POINT('Ctrl Pts',(-2.96041160620732,0.0598656765852475,
0.87682612344575));
#20343=CARTESIAN_POINT('Ctrl Pts',(-2.96040815324349,0.0598658185101067,
0.876825734520681));
#20344=CARTESIAN_POINT('Ctrl Pts',(-2.96040556214768,0.0598657920045578,
0.876825808324795));
#20345=CARTESIAN_POINT('Ctrl Pts',(-2.96039837346811,0.0598655893040655,
0.876826369399628));
#20346=CARTESIAN_POINT('Ctrl Pts',(-2.9603929165739,0.0598653472112175,
0.876827038754178));
#20347=CARTESIAN_POINT('Ctrl Pts',(-2.96037760633566,0.0598646053374691,
0.876829094693984));
#20348=CARTESIAN_POINT('Ctrl Pts',(-2.96036380015299,0.0598638705770211,
0.876831138211164));
#20349=CARTESIAN_POINT('Ctrl Pts',(-2.96033719264881,0.0598624486708876,
0.876835106182144));
#20350=CARTESIAN_POINT('Ctrl Pts',(-2.96031159368107,0.0598610583320029,
0.87683901584924));
#20351=CARTESIAN_POINT('Ctrl Pts',(-2.96025529525252,0.0598580144693806,
0.876847638168764));
#20352=CARTESIAN_POINT('Ctrl Pts',(-2.96021310455862,0.0598557471926268,
0.876854148091574));
#20353=CARTESIAN_POINT('Ctrl Pts',(-2.96008734802608,0.0598490878769054,
0.876873602790802));
#20354=CARTESIAN_POINT('Ctrl Pts',(-2.96000449353606,0.0598448127019288,
0.876886490315284));
#20355=CARTESIAN_POINT('Ctrl Pts',(-2.95975590153061,0.0598323488694641,
0.876925311717692));
#20356=CARTESIAN_POINT('Ctrl Pts',(-2.95959033691541,0.0598245243488887,
0.876951380460641));
#20357=CARTESIAN_POINT('Ctrl Pts',(-2.95909365784188,0.0598024889557596,
0.877030194875114));
#20358=CARTESIAN_POINT('Ctrl Pts',(-2.95876256633421,0.0597897148429793,
0.87708355225251));
#20359=CARTESIAN_POINT('Ctrl Pts',(-2.95776929650042,0.0597571183908872,
0.877246060040826));
#20360=CARTESIAN_POINT('Ctrl Pts',(-2.9571073199902,0.0597430321504992,
0.877357618292709));
#20361=CARTESIAN_POINT('Ctrl Pts',(-2.95512198401899,0.0597235213942096,
0.877701903024172));
#20362=CARTESIAN_POINT('Ctrl Pts',(-2.95380002536389,0.0597408898589351,
0.877944117676307));
#20363=CARTESIAN_POINT('Ctrl Pts',(-2.94984178410647,0.0598827452244851,
0.878707993952471));
#20364=CARTESIAN_POINT('Ctrl Pts',(-2.94721536727803,0.0600971459470857,
0.879266580845324));
#20365=CARTESIAN_POINT('Ctrl Pts',(-2.93941233445455,0.0610887194259119,
0.881080123930645));
#20366=CARTESIAN_POINT('Ctrl Pts',(-2.93430536722629,0.0622152948597964,
0.882474905957679));
#20367=CARTESIAN_POINT('Ctrl Pts',(-2.92116902241244,0.0664103649549747,
0.886626951401218));
#20368=CARTESIAN_POINT('Ctrl Pts',(-2.91200301339737,0.0707140517326124,
0.890125580532118));
#20369=CARTESIAN_POINT('Ctrl Pts',(-2.8961467184212,0.0842530156264676,
0.898723641095627));
#20370=CARTESIAN_POINT('Ctrl Pts',(-2.89019671334679,0.0919560410529159,
0.90303400223478));
#20371=CARTESIAN_POINT('Ctrl Pts',(-2.88388864657462,0.105006472772146,
0.909426649433165));
#20372=CARTESIAN_POINT('Ctrl Pts',(-2.8822163987365,0.109700228982129,0.911582109267249));
#20373=CARTESIAN_POINT('Ctrl Pts',(-2.87995399962771,0.119400639997362,
0.915722468197169));
#20374=CARTESIAN_POINT('Ctrl Pts',(-2.87936339380758,0.124392439973975,
0.917701934678691));
#20375=CARTESIAN_POINT('Ctrl Pts',(-2.87936339380758,0.129452050955555,
0.919543482472953));
#20376=CARTESIAN_POINT('Ctrl Pts',(-2.87936339380758,0.129452050955555,
0.919543482472952));
#20377=CARTESIAN_POINT('Ctrl Pts',(-2.88146283528787,0.127002914770058,
0.922197454515019));
#20378=CARTESIAN_POINT('Ctrl Pts',(-2.88513307538547,0.124907999857464,
0.928743708628879));
#20379=CARTESIAN_POINT('Ctrl Pts',(-2.8877740083963,0.12219136571519,0.935614140128415));
#20380=CARTESIAN_POINT('Ctrl Pts',(-2.88881405854803,0.120889693311755,
0.939137268222128));
#20381=CARTESIAN_POINT('Origin',(-2.81154186539738,0.0396551669818869,0.932354041514756));
#20382=CARTESIAN_POINT('Ctrl Pts',(-2.87936339380758,-3.,1.2));
#20383=CARTESIAN_POINT('Ctrl Pts',(-2.87936339380758,4.2,1.2));
#20384=CARTESIAN_POINT('Ctrl Pts',(-2.88050601962387,-3.,1.18008118002045));
#20385=CARTESIAN_POINT('Ctrl Pts',(-2.88050601962387,4.2,1.18008118002045));
#20386=CARTESIAN_POINT('Ctrl Pts',(-2.88410012960011,-3.,1.11550336602625));
#20387=CARTESIAN_POINT('Ctrl Pts',(-2.88410012960011,4.2,1.11550336602625));
#20388=CARTESIAN_POINT('Ctrl Pts',(-2.88965455295869,-3.,1.00596877194195));
#20389=CARTESIAN_POINT('Ctrl Pts',(-2.88965455295869,4.2,1.00596877194195));
#20390=CARTESIAN_POINT('Ctrl Pts',(-2.89676647174981,-3.,0.851337038635417));
#20391=CARTESIAN_POINT('Ctrl Pts',(-2.89676647174981,4.2,0.851337038635417));
#20392=CARTESIAN_POINT('Ctrl Pts',(-2.90717911786707,-3.,0.654020230869684));
#20393=CARTESIAN_POINT('Ctrl Pts',(-2.90717911786707,4.2,0.654020230869684));
#20394=CARTESIAN_POINT('Ctrl Pts',(-2.92780415844476,-3.,0.444963858672577));
#20395=CARTESIAN_POINT('Ctrl Pts',(-2.92780415844476,4.2,0.444963858672577));
#20396=CARTESIAN_POINT('Ctrl Pts',(-2.96639254265869,-3.,0.262319630540737));
#20397=CARTESIAN_POINT('Ctrl Pts',(-2.96639254265869,4.2,0.262319630540737));
#20398=CARTESIAN_POINT('Ctrl Pts',(-3.03063129752067,-3.,0.11901737132707));
#20399=CARTESIAN_POINT('Ctrl Pts',(-3.03063129752067,4.2,0.11901737132707));
#20400=CARTESIAN_POINT('Ctrl Pts',(-3.12452733970658,-3.,0.0241851999813871));
#20401=CARTESIAN_POINT('Ctrl Pts',(-3.12452733970658,4.2,0.0241851999813871));
#20402=CARTESIAN_POINT('Ctrl Pts',(-3.24511001026157,-3.,-0.0214179570895714));
#20403=CARTESIAN_POINT('Ctrl Pts',(-3.24511001026157,4.2,-0.0214179570895714));
#20404=CARTESIAN_POINT('Ctrl Pts',(-3.38164698943802,-3.,-0.0263068037112043));
#20405=CARTESIAN_POINT('Ctrl Pts',(-3.38164698943802,4.2,-0.0263068037112043));
#20406=CARTESIAN_POINT('Ctrl Pts',(-3.52045328348989,-3.,-0.00118366394785932));
#20407=CARTESIAN_POINT('Ctrl Pts',(-3.52045328348989,4.2,-0.00118366394785932));
#20408=CARTESIAN_POINT('Ctrl Pts',(-3.64881642260079,-3.,0.0470540298718583));
#20409=CARTESIAN_POINT('Ctrl Pts',(-3.64881642260079,4.2,0.0470540298718583));
#20410=CARTESIAN_POINT('Ctrl Pts',(-3.75872318140663,-3.,0.120497232333251));
#20411=CARTESIAN_POINT('Ctrl Pts',(-3.75872318140663,4.2,0.120497232333251));
#20412=CARTESIAN_POINT('Ctrl Pts',(-3.84598208672296,-3.,0.224659532804408));
#20413=CARTESIAN_POINT('Ctrl Pts',(-3.84598208672296,4.2,0.224659532804408));
#20414=CARTESIAN_POINT('Ctrl Pts',(-3.9098657241983,-3.,0.364350357241515));
#20415=CARTESIAN_POINT('Ctrl Pts',(-3.9098657241983,4.2,0.364350357241515));
#20416=CARTESIAN_POINT('Ctrl Pts',(-3.9525920016999,-3.,0.538436816836325));
#20417=CARTESIAN_POINT('Ctrl Pts',(-3.9525920016999,4.2,0.538436816836325));
#20418=CARTESIAN_POINT('Ctrl Pts',(-3.97841403016126,-3.,0.741129277895169));
#20419=CARTESIAN_POINT('Ctrl Pts',(-3.97841403016126,4.2,0.741129277895169));
#20420=CARTESIAN_POINT('Ctrl Pts',(-3.98977740850458,-3.,0.919671129654853));
#20421=CARTESIAN_POINT('Ctrl Pts',(-3.98977740850458,4.2,0.919671129654853));
#20422=CARTESIAN_POINT('Ctrl Pts',(-3.99545186687387,-3.,1.05866205464795));
#20423=CARTESIAN_POINT('Ctrl Pts',(-3.99545186687387,4.2,1.05866205464795));
#20424=CARTESIAN_POINT('Ctrl Pts',(-3.99855414331415,-3.,1.15256872586734));
#20425=CARTESIAN_POINT('Ctrl Pts',(-3.99855414331415,4.2,1.15256872586734));
#20426=CARTESIAN_POINT('Ctrl Pts',(-3.99999413894399,-3.,1.19980766336825));
#20427=CARTESIAN_POINT('Ctrl Pts',(-3.99999413894399,4.2,1.19980766336825));
#20428=CARTESIAN_POINT('Ctrl Pts',(-4.,-3.,1.2));
#20429=CARTESIAN_POINT('Ctrl Pts',(-4.,4.2,1.2));
#20430=CARTESIAN_POINT('',(-2.89158569656657,0.11486454003439,0.963528635709791));
#20431=CARTESIAN_POINT('Origin',(-2.89391657159917,0.129178635160739,0.915904052326592));
#20432=CARTESIAN_POINT('',(-2.8852657140673,0.5,1.09088035845137));
#20433=CARTESIAN_POINT('Ctrl Pts',(-2.8852657140673,0.5,1.09088035845137));
#20434=CARTESIAN_POINT('Ctrl Pts',(-2.88739518236194,0.371284826357953,
1.04939286925411));
#20435=CARTESIAN_POINT('Ctrl Pts',(-2.88948025018409,0.243010859025609,
1.00659623192935));
#20436=CARTESIAN_POINT('Ctrl Pts',(-2.89158569656657,0.114864540034388,
0.963528635709792));
#20437=CARTESIAN_POINT('',(-2.88353005387197,0.5,1.12422135153951));
#20438=CARTESIAN_POINT('Ctrl Pts',(-2.88353005387198,0.500000000000001,
1.12422135153951));
#20439=CARTESIAN_POINT('Ctrl Pts',(-2.88378350828653,0.500000000000001,
1.11942475852518));
#20440=CARTESIAN_POINT('Ctrl Pts',(-2.88413377322526,0.500000000000001,
1.11275818755601));
#20441=CARTESIAN_POINT('Ctrl Pts',(-2.88448145181725,0.500000000000001,
1.10609021938137));
#20442=CARTESIAN_POINT('Ctrl Pts',(-2.88482670797398,0.500000000000001,
1.09942100077238));
#20443=CARTESIAN_POINT('Ctrl Pts',(-2.885169713669,0.500000000000001,1.09275069176305));
#20444=CARTESIAN_POINT('Ctrl Pts',(-2.8852657140673,0.500000000000001,1.09088035845137));
#20445=CARTESIAN_POINT('',(-2.88353005387198,0.0831281904378376,1.12422135153951));
#20446=CARTESIAN_POINT('Ctrl Pts',(-2.87936280293809,0.129463942239828,
0.919546811122371));
#20447=CARTESIAN_POINT('Ctrl Pts',(-2.87936272551578,0.128996507120314,
0.919376678242473));
#20448=CARTESIAN_POINT('Ctrl Pts',(-2.87936729845633,0.128528665510741,
0.919206397636387));
#20449=CARTESIAN_POINT('Ctrl Pts',(-2.87937652870275,0.128060914565431,
0.919036150256641));
#20450=CARTESIAN_POINT('Ctrl Pts',(-2.88800912722877,0.125219614594593,
0.932602973731212));
#20451=CARTESIAN_POINT('Ctrl Pts',(-2.8880161408965,0.124635052899647,0.932396199243668));
#20452=CARTESIAN_POINT('Ctrl Pts',(-2.88802498402021,0.124050831955124,
0.932186275174002));
#20453=CARTESIAN_POINT('Ctrl Pts',(-2.88803574670127,0.123468016182681,
0.931973542850541));
#20454=CARTESIAN_POINT('Ctrl Pts',(-2.8923362255842,0.120058692271535,0.948176288112179));
#20455=CARTESIAN_POINT('Ctrl Pts',(-2.89234848804188,0.119330898552523,
0.947926692856932));
#20456=CARTESIAN_POINT('Ctrl Pts',(-2.8923610549264,0.118605121800164,0.947669421968552));
#20457=CARTESIAN_POINT('Ctrl Pts',(-2.8923740164996,0.117882286794026,0.94740478025217));
#20458=CARTESIAN_POINT('Ctrl Pts',(-2.89158534139673,0.11488616536118,0.963535900827959));
#20459=CARTESIAN_POINT('Ctrl Pts',(-2.89159964786982,0.114014752657563,
0.963243257015774));
#20460=CARTESIAN_POINT('Ctrl Pts',(-2.89161454709808,0.113147190385347,
0.962938501079936));
#20461=CARTESIAN_POINT('Ctrl Pts',(-2.89163003027391,0.1122839746201,0.962621817739011));
#20462=CARTESIAN_POINT('Origin',(-2.81168112317661,0.114864540034389,0.959622339334904));
#20463=CARTESIAN_POINT('Ctrl Pts',(-3.99945760881125,0.13546233783637,0.903030354983468));
#20464=CARTESIAN_POINT('Ctrl Pts',(-3.9973961162676,0.158008411859628,0.841085525707216));
#20465=CARTESIAN_POINT('Ctrl Pts',(-3.99279290514081,0.203310563544645,
0.716618886899923));
#20466=CARTESIAN_POINT('Ctrl Pts',(-3.97849395981051,0.281987502029712,
0.50045577498038));
#20467=CARTESIAN_POINT('Ctrl Pts',(-3.95509656322196,0.35087941221533,0.311176807362298));
#20468=CARTESIAN_POINT('Ctrl Pts',(-3.90963080113393,0.40951907607415,0.150065655025781));
#20469=CARTESIAN_POINT('Ctrl Pts',(-3.8691416736774,0.444506704555304,0.0539379358135427));
#20470=CARTESIAN_POINT('Ctrl Pts',(-3.80820163959337,0.478469777977808,
-0.0393748415100655));
#20471=CARTESIAN_POINT('Ctrl Pts',(-3.72122359734069,0.507285738389506,
-0.118546042061105));
#20472=CARTESIAN_POINT('Ctrl Pts',(-3.58603043474247,0.533328259831995,
-0.190097281670006));
#20473=CARTESIAN_POINT('Ctrl Pts',(-3.44370085318666,0.546103828098339,
-0.225197867002487));
#20474=CARTESIAN_POINT('Ctrl Pts',(-3.29162344210726,0.547685564166839,
-0.229543651134227));
#20475=CARTESIAN_POINT('Ctrl Pts',(-3.18823564478345,0.539575598601234,
-0.207261703870172));
#20476=CARTESIAN_POINT('Ctrl Pts',(-3.11077137978012,0.523493646274472,
-0.163076902991648));
#20477=CARTESIAN_POINT('Ctrl Pts',(-3.04751283334051,0.502320173155856,
-0.104903263706821));
#20478=CARTESIAN_POINT('Ctrl Pts',(-2.97789574195055,0.460397612655845,
0.0102780246326795));
#20479=CARTESIAN_POINT('Ctrl Pts',(-2.91982931246599,0.377551236111436,
0.237896573472077));
#20480=CARTESIAN_POINT('Ctrl Pts',(-2.89832305986079,0.263668991805047,
0.550785468180695));
#20481=CARTESIAN_POINT('Ctrl Pts',(-2.88684765097271,0.174075173876031,
0.796942459863397));
#20482=CARTESIAN_POINT('Ctrl Pts',(-2.87936339380758,0.129452050955555,
0.919543482472953));
#20483=CARTESIAN_POINT('Ctrl Pts',(-3.99945760881125,0.112969907862324,
0.894843779976599));
#20484=CARTESIAN_POINT('Ctrl Pts',(-3.99739609096167,0.13551625865078,0.832898190294214));
#20485=CARTESIAN_POINT('Ctrl Pts',(-3.9927943517283,0.180816769376243,0.708436059986241));
#20486=CARTESIAN_POINT('Ctrl Pts',(-3.97850103889804,0.259491261707806,
0.492279668818216));
#20487=CARTESIAN_POINT('Ctrl Pts',(-3.95511811012035,0.328375650295247,
0.303021366621285));
#20488=CARTESIAN_POINT('Ctrl Pts',(-3.90966176168135,0.387018886385186,
0.141900399660432));
#20489=CARTESIAN_POINT('Ctrl Pts',(-3.8691813956086,0.422008258304128,0.0457678903922369));
#20490=CARTESIAN_POINT('Ctrl Pts',(-3.80822946486193,0.455982725304131,
-0.0475761905282765));
#20491=CARTESIAN_POINT('Ctrl Pts',(-3.72124990150233,0.484803780244265,
-0.126761388181157));
#20492=CARTESIAN_POINT('Ctrl Pts',(-3.58604191832488,0.510849567633407,
-0.198321600904739));
#20493=CARTESIAN_POINT('Ctrl Pts',(-3.44375381289202,0.523625721203665,
-0.233423794346508));
#20494=CARTESIAN_POINT('Ctrl Pts',(-3.29167170986371,0.525210387234294,
-0.237777628483038));
#20495=CARTESIAN_POINT('Ctrl Pts',(-3.18824858312854,0.517100692154883,
-0.215496424373695));
#20496=CARTESIAN_POINT('Ctrl Pts',(-3.11073783195475,0.501008107849723,
-0.171282412374599));
#20497=CARTESIAN_POINT('Ctrl Pts',(-3.04744355689428,0.479821356105204,
-0.11307229036494));
#20498=CARTESIAN_POINT('Ctrl Pts',(-2.97782462588385,0.437884988863251,
0.00214693168628145));
#20499=CARTESIAN_POINT('Ctrl Pts',(-2.91980546068163,0.355046369978444,
0.229744166531096));
#20500=CARTESIAN_POINT('Ctrl Pts',(-2.89831668227606,0.241171500824311,
0.542612798175426));
#20501=CARTESIAN_POINT('Ctrl Pts',(-2.88684752017467,0.151581964049483,
0.788758027483666));
#20502=CARTESIAN_POINT('Ctrl Pts',(-2.87936339380758,0.106959620981509,
0.911356907466083));
#20503=CARTESIAN_POINT('Ctrl Pts',(-3.97937276807867,0.0738190510046144,
0.881262446761113));
#20504=CARTESIAN_POINT('Ctrl Pts',(-3.97731327142506,0.0963432964334023,
0.819377591055264));
#20505=CARTESIAN_POINT('Ctrl Pts',(-3.97270726831941,0.141579135382642,
0.695093144992142));
#20506=CARTESIAN_POINT('Ctrl Pts',(-3.95848366570773,0.219966739110569,
0.479724973784506));
#20507=CARTESIAN_POINT('Ctrl Pts',(-3.93516955254869,0.288360740578814,
0.291813999124357));
#20508=CARTESIAN_POINT('Ctrl Pts',(-3.89045398807751,0.34598040353968,0.133505276222791));
#20509=CARTESIAN_POINT('Ctrl Pts',(-3.85097180237235,0.380059347708762,
0.0398741466393852));
#20510=CARTESIAN_POINT('Ctrl Pts',(-3.79225425972909,0.412734983723264,
-0.0499014254767779));
#20511=CARTESIAN_POINT('Ctrl Pts',(-3.70917100058941,0.440255377838933,
-0.125513086884069));
#20512=CARTESIAN_POINT('Ctrl Pts',(-3.57908941427417,0.465363375357826,
-0.194496743114952));
#20513=CARTESIAN_POINT('Ctrl Pts',(-3.44018820684967,0.477851863444749,
-0.2288085821369));
#20514=CARTESIAN_POINT('Ctrl Pts',(-3.29321826238141,0.479328003623049,
-0.232864243944729));
#20515=CARTESIAN_POINT('Ctrl Pts',(-3.19543503576692,0.471597152685915,
-0.211623905561783));
#20516=CARTESIAN_POINT('Ctrl Pts',(-3.12325058435565,0.456594508464948,
-0.170404479332566));
#20517=CARTESIAN_POINT('Ctrl Pts',(-3.06397256609718,0.436789352841401,
-0.115990261468086));
#20518=CARTESIAN_POINT('Ctrl Pts',(-2.99722044260985,0.396760213362037,
-0.00601110462833348));
#20519=CARTESIAN_POINT('Ctrl Pts',(-2.9398515643179,0.315401605007014,0.217519834705343));
#20520=CARTESIAN_POINT('Ctrl Pts',(-2.91841241808079,0.201953714096476,
0.529215353266799));
#20521=CARTESIAN_POINT('Ctrl Pts',(-2.90691964577141,0.112314614371736,
0.775496755660762));
#20522=CARTESIAN_POINT('Ctrl Pts',(-2.8994250725072,0.0676299841370301,
0.898266768227296));
#20523=CARTESIAN_POINT('Ctrl Pts',(-3.93743988512382,0.0596235975755129,
0.87749122935701));
#20524=CARTESIAN_POINT('Ctrl Pts',(-3.93538453772238,0.0821024635791913,
0.815731052596958));
#20525=CARTESIAN_POINT('Ctrl Pts',(-3.93077373753047,0.127198705107589,
0.691830147295415));
#20526=CARTESIAN_POINT('Ctrl Pts',(-3.9167113835724,0.20498052425003,0.478126355557454));
#20527=CARTESIAN_POINT('Ctrl Pts',(-3.89358129219178,0.272329724497136,
0.293085948660201));
#20528=CARTESIAN_POINT('Ctrl Pts',(-3.8504385811501,0.327822346713796,0.140621222173602));
#20529=CARTESIAN_POINT('Ctrl Pts',(-3.81306481879868,0.360005373332597,
0.0521990832487384));
#20530=CARTESIAN_POINT('Ctrl Pts',(-3.75897902541619,0.390001101649611,
-0.0302135029823513));
#20531=CARTESIAN_POINT('Ctrl Pts',(-3.68402617998296,0.414820200291004,
-0.0984034160707962));
#20532=CARTESIAN_POINT('Ctrl Pts',(-3.56460608864264,0.4379794000974,-0.162032794591505));
#20533=CARTESIAN_POINT('Ctrl Pts',(-3.43289167818615,0.449868936091557,
-0.194699026263248));
#20534=CARTESIAN_POINT('Ctrl Pts',(-3.29658174994825,0.451126668724512,
-0.198154618272002));
#20535=CARTESIAN_POINT('Ctrl Pts',(-3.21047490685931,0.44418751827955,-0.179089459114268));
#20536=CARTESIAN_POINT('Ctrl Pts',(-3.14928099284796,0.431430785935711,
-0.144040625053544));
#20537=CARTESIAN_POINT('Ctrl Pts',(-3.09828842224605,0.414473076814942,
-0.0974497021585525));
#20538=CARTESIAN_POINT('Ctrl Pts',(-3.03751645364449,0.378387318235333,
0.0016951047028135));
#20539=CARTESIAN_POINT('Ctrl Pts',(-2.98163705203391,0.300140293015244,
0.216677039634506));
#20540=CARTESIAN_POINT('Ctrl Pts',(-2.96035026114277,0.187604410632771,
0.52586683535875));
#20541=CARTESIAN_POINT('Ctrl Pts',(-2.94882561743878,0.097873773732583,
0.772399734075299));
#20542=CARTESIAN_POINT('Ctrl Pts',(-2.94130959805507,0.0530612760548464,
0.895521059554243));
#20543=CARTESIAN_POINT('Ctrl Pts',(-3.91949669889834,0.0594316804308482,
0.878018517378383));
#20544=CARTESIAN_POINT('Ctrl Pts',(-3.91744312474473,0.0818911528271679,
0.81631162411663));
#20545=CARTESIAN_POINT('Ctrl Pts',(-3.91283040143456,0.12692751581812,0.692575233744628));
#20546=CARTESIAN_POINT('Ctrl Pts',(-3.89883754199609,0.204449902882089,
0.479584225784152));
#20547=CARTESIAN_POINT('Ctrl Pts',(-3.87578746756243,0.271351367948194,
0.295773961186595));
#20548=CARTESIAN_POINT('Ctrl Pts',(-3.83331861312405,0.325934138527799,
0.14580903152786));
#20549=CARTESIAN_POINT('Ctrl Pts',(-3.7968478216781,0.3573060507223,0.0596154111683547));
#20550=CARTESIAN_POINT('Ctrl Pts',(-3.74474291823659,0.386156042733723,
-0.0196492904344777));
#20551=CARTESIAN_POINT('Ctrl Pts',(-3.67326896340584,0.409819698696741,
-0.0846646508546109));
#20552=CARTESIAN_POINT('Ctrl Pts',(-3.55840964799874,0.432145290546818,
-0.146003710338657));
#20553=CARTESIAN_POINT('Ctrl Pts',(-3.4297741371024,0.443778584954816,-0.177965924038501));
#20554=CARTESIAN_POINT('Ctrl Pts',(-3.29802524363671,0.444943118366151,
-0.181165453290342));
#20555=CARTESIAN_POINT('Ctrl Pts',(-3.21691164450761,0.438342762365917,
-0.163031124219339));
#20556=CARTESIAN_POINT('Ctrl Pts',(-3.16041651707056,0.426546125464733,
-0.13062013070783));
#20557=CARTESIAN_POINT('Ctrl Pts',(-3.11296616528858,0.410805676990282,
-0.087373603952188));
#20558=CARTESIAN_POINT('Ctrl Pts',(-3.05475295808673,0.37640608565689,0.00713849647477464));
#20559=CARTESIAN_POINT('Ctrl Pts',(-2.99951506785369,0.299491197583846,
0.218460414675343));
#20560=CARTESIAN_POINT('Ctrl Pts',(-2.97829500840806,0.187346215163306,
0.526576221580912));
#20561=CARTESIAN_POINT('Ctrl Pts',(-2.96675727674276,0.0975767861342948,
0.773215700795454));
#20562=CARTESIAN_POINT('Ctrl Pts',(-2.95923209202432,0.0527096423040758,
0.896487165344404));
#20563=CARTESIAN_POINT('',(-3.91949669889834,0.0594316804308483,0.878018517378383));
#20564=CARTESIAN_POINT('Ctrl Pts',(-2.96041766193066,0.0598644374565791,
0.876829527222077));
#20565=CARTESIAN_POINT('Ctrl Pts',(-2.96737439864014,0.102348383545406,
0.760105844653699));
#20566=CARTESIAN_POINT('Ctrl Pts',(-2.9787461837485,0.189730612377242,0.52002514407661));
#20567=CARTESIAN_POINT('Ctrl Pts',(-2.99951506785369,0.299491197583846,
0.218460414675343));
#20568=CARTESIAN_POINT('Ctrl Pts',(-3.05475295808673,0.37640608565689,0.00713849647477464));
#20569=CARTESIAN_POINT('Ctrl Pts',(-3.11296616528858,0.410805676990282,
-0.087373603952188));
#20570=CARTESIAN_POINT('Ctrl Pts',(-3.16041651707056,0.426546125464733,
-0.13062013070783));
#20571=CARTESIAN_POINT('Ctrl Pts',(-3.21691164450761,0.438342762365917,
-0.163031124219339));
#20572=CARTESIAN_POINT('Ctrl Pts',(-3.29802524363671,0.444943118366151,
-0.181165453290342));
#20573=CARTESIAN_POINT('Ctrl Pts',(-3.4297741371024,0.443778584954816,-0.177965924038501));
#20574=CARTESIAN_POINT('Ctrl Pts',(-3.55840964799874,0.432145290546818,
-0.146003710338657));
#20575=CARTESIAN_POINT('Ctrl Pts',(-3.67326896340584,0.409819698696741,
-0.0846646508546109));
#20576=CARTESIAN_POINT('Ctrl Pts',(-3.74474291823659,0.386156042733723,
-0.0196492904344777));
#20577=CARTESIAN_POINT('Ctrl Pts',(-3.7968478216781,0.3573060507223,0.0596154111683547));
#20578=CARTESIAN_POINT('Ctrl Pts',(-3.83331861312405,0.325934138527799,
0.14580903152786));
#20579=CARTESIAN_POINT('Ctrl Pts',(-3.87578746756243,0.271351367948194,
0.295773961186595));
#20580=CARTESIAN_POINT('Ctrl Pts',(-3.89883754199609,0.204449902882089,
0.479584225784152));
#20581=CARTESIAN_POINT('Ctrl Pts',(-3.91283040143456,0.12692751581812,0.692575233744628));
#20582=CARTESIAN_POINT('Ctrl Pts',(-3.91744312474473,0.0818911528271679,
0.81631162411663));
#20583=CARTESIAN_POINT('Ctrl Pts',(-3.91949669889834,0.0594316804308482,
0.878018517378383));
#20584=CARTESIAN_POINT('',(-3.99945760881125,0.135462337836371,0.903030354983466));
#20585=CARTESIAN_POINT('Origin',(-3.91949669889834,0.134607090093721,0.905380128844436));
#20586=CARTESIAN_POINT('Ctrl Pts',(-3.99945760881125,0.135462337836371,
0.903030354983466));
#20587=CARTESIAN_POINT('Ctrl Pts',(-3.99823410537672,0.148843515996691,
0.866265870142289));
#20588=CARTESIAN_POINT('Ctrl Pts',(-3.99689944434567,0.162259022242162,
0.829407069662303));
#20589=CARTESIAN_POINT('Ctrl Pts',(-3.99536024116589,0.17567461573747,0.792548029465364));
#20590=CARTESIAN_POINT('Ctrl Pts',(-3.99427372087306,0.185144655017843,
0.766529310381191));
#20591=CARTESIAN_POINT('Ctrl Pts',(-3.99308470617941,0.194614511215692,
0.740511094312118));
#20592=CARTESIAN_POINT('Ctrl Pts',(-3.99175212990483,0.204067318082626,
0.714539720894749));
#20593=CARTESIAN_POINT('Ctrl Pts',(-3.99025895344394,0.214659363710641,
0.685438314705947));
#20594=CARTESIAN_POINT('Ctrl Pts',(-3.98858683641064,0.225229808869164,
0.65639625531932));
#20595=CARTESIAN_POINT('Ctrl Pts',(-3.98665248763581,0.235815021378387,
0.6273136229701));
#20596=CARTESIAN_POINT('Ctrl Pts',(-3.98481642208428,0.245862404919968,
0.599708663565006));
#20597=CARTESIAN_POINT('Ctrl Pts',(-3.98274441730402,0.255923265448313,
0.572066676443098));
#20598=CARTESIAN_POINT('Ctrl Pts',(-3.98034174674877,0.266015499867288,
0.544338490265121));
#20599=CARTESIAN_POINT('Ctrl Pts',(-3.97939553288731,0.269989999025906,
0.533418643573175));
#20600=CARTESIAN_POINT('Ctrl Pts',(-3.97839766833391,0.273969348433885,
0.522485470930634));
#20601=CARTESIAN_POINT('Ctrl Pts',(-3.9773423211157,0.277949779679242,0.511549325964324));
#20602=CARTESIAN_POINT('Ctrl Pts',(-3.97510642880281,0.286382848407637,
0.488379660056349));
#20603=CARTESIAN_POINT('Ctrl Pts',(-3.97261253876767,0.294829085588724,
0.465173814121954));
#20604=CARTESIAN_POINT('Ctrl Pts',(-3.96977215365409,0.303312662508484,
0.441865378098708));
#20605=CARTESIAN_POINT('Ctrl Pts',(-3.96702053057532,0.311531127649501,
0.419285330701187));
#20606=CARTESIAN_POINT('Ctrl Pts',(-3.96394406722112,0.319784800447935,
0.396608551059925));
#20607=CARTESIAN_POINT('Ctrl Pts',(-3.96043598303906,0.328081168873384,
0.373814466147526));
#20608=CARTESIAN_POINT('Ctrl Pts',(-3.95703752648768,0.336118275785539,
0.351732696388639));
#20609=CARTESIAN_POINT('Ctrl Pts',(-3.9532343129631,0.344195585556897,0.329540470181892));
#20610=CARTESIAN_POINT('Ctrl Pts',(-3.94889948313842,0.352303921980112,
0.307262998949767));
#20611=CARTESIAN_POINT('Ctrl Pts',(-3.94595348495836,0.357814436882015,
0.292122983687222));
#20612=CARTESIAN_POINT('Ctrl Pts',(-3.94276133969239,0.363338951078113,
0.276944505679984));
#20613=CARTESIAN_POINT('Ctrl Pts',(-3.93927383281782,0.368869699153342,
0.261748900230602));
#20614=CARTESIAN_POINT('Ctrl Pts',(-3.93612304217305,0.373866457560057,
0.248020419337682));
#20615=CARTESIAN_POINT('Ctrl Pts',(-3.93273246601248,0.378866861656343,
0.234281921994987));
#20616=CARTESIAN_POINT('Ctrl Pts',(-3.92904932269308,0.383874882287698,
0.220522498394176));
#20617=CARTESIAN_POINT('Ctrl Pts',(-3.9242428496489,0.390410309796705,0.202566558886697));
#20618=CARTESIAN_POINT('Ctrl Pts',(-3.91894049307532,0.396957198804506,
0.184579129170088));
#20619=CARTESIAN_POINT('Ctrl Pts',(-3.9130077333512,0.403499782727413,0.166603527577014));
#20620=CARTESIAN_POINT('Ctrl Pts',(-3.90795034653693,0.409077014774833,
0.15128020846367));
#20621=CARTESIAN_POINT('Ctrl Pts',(-3.90243675237154,0.414649019758862,
0.135971250588961));
#20622=CARTESIAN_POINT('Ctrl Pts',(-3.89635541881929,0.420206121603407,
0.120703238753463));
#20623=CARTESIAN_POINT('Ctrl Pts',(-3.8900374447729,0.425979464723838,0.104841108895317));
#20624=CARTESIAN_POINT('Ctrl Pts',(-3.88310583474409,0.431738296312812,
0.0890188491421691));
#20625=CARTESIAN_POINT('Ctrl Pts',(-3.87540089395165,0.437463615370407,
0.0732886643122535));
#20626=CARTESIAN_POINT('Ctrl Pts',(-3.87075334907403,0.440917071792165,
0.0638003707744014));
#20627=CARTESIAN_POINT('Ctrl Pts',(-3.86582311762319,0.444358520125789,
0.0543450691875513));
#20628=CARTESIAN_POINT('Ctrl Pts',(-3.86057143915063,0.447779999038701,
0.0449446331331839));
#20629=CARTESIAN_POINT('Ctrl Pts',(-3.85175601294152,0.453523266651225,
0.0291651350538899));
#20630=CARTESIAN_POINT('Ctrl Pts',(-3.84204078188016,0.459203303127001,
0.0135593630950167));
#20631=CARTESIAN_POINT('Ctrl Pts',(-3.83132752297138,0.464733701807003,
-0.00163528239887109));
#20632=CARTESIAN_POINT('Ctrl Pts',(-3.82441995626527,0.468299525999133,
-0.0114323038484921));
#20633=CARTESIAN_POINT('Ctrl Pts',(-3.8170977510109,0.471803434497092,-0.0210592133264701));
#20634=CARTESIAN_POINT('Ctrl Pts',(-3.80933982107858,0.475226299554347,
-0.0304634577811197));
#20635=CARTESIAN_POINT('Ctrl Pts',(-3.80343570000945,0.477831248281349,
-0.0376204955873941));
#20636=CARTESIAN_POINT('Ctrl Pts',(-3.79727563639941,0.480390662744171,
-0.0446524290310215));
#20637=CARTESIAN_POINT('Ctrl Pts',(-3.79086906934545,0.482891327150591,
-0.0515229480212962));
#20638=CARTESIAN_POINT('Ctrl Pts',(-3.78176306264065,0.486445659238199,
-0.0612883951732427));
#20639=CARTESIAN_POINT('Ctrl Pts',(-3.77216154255004,0.48987894582093,-0.0707212725338115));
#20640=CARTESIAN_POINT('Ctrl Pts',(-3.76213783752762,0.493157146302368,
-0.0797280543330087));
#20641=CARTESIAN_POINT('Ctrl Pts',(-3.75263674507966,0.496264429065319,
-0.0882652435600765));
#20642=CARTESIAN_POINT('Ctrl Pts',(-3.74275660335202,0.499232588020461,
-0.0964201932666809));
#20643=CARTESIAN_POINT('Ctrl Pts',(-3.73258649467787,0.502043996418041,
-0.104144474355898));
#20644=CARTESIAN_POINT('Ctrl Pts',(-3.72556063050263,0.503986214950349,
-0.10948067591706));
#20645=CARTESIAN_POINT('Ctrl Pts',(-3.71839939185283,0.505853269012534,
-0.114610364793813));
#20646=CARTESIAN_POINT('Ctrl Pts',(-3.7111300071802,0.507644171485729,-0.119530828899364));
#20647=CARTESIAN_POINT('Ctrl Pts',(-3.69305477933714,0.512097226552356,
-0.131765497142509));
#20648=CARTESIAN_POINT('Ctrl Pts',(-3.67428822511307,0.516084784645751,
-0.142721222962874));
#20649=CARTESIAN_POINT('Ctrl Pts',(-3.65509432646411,0.519651775395887,
-0.152521449504278));
#20650=CARTESIAN_POINT('Ctrl Pts',(-3.64440611533146,0.521638070673514,
-0.157978750927925));
#20651=CARTESIAN_POINT('Ctrl Pts',(-3.63358642140285,0.523494019649325,
-0.163077928830628));
#20652=CARTESIAN_POINT('Ctrl Pts',(-3.62268697157354,0.525227290438691,
-0.16784005118621));
#20653=CARTESIAN_POINT('Ctrl Pts',(-3.61375034448887,0.526648425901848,
-0.171744588781219));
#20654=CARTESIAN_POINT('Ctrl Pts',(-3.6047674830026,0.52798607554658,-0.175419750975262));
#20655=CARTESIAN_POINT('Ctrl Pts',(-3.59574600476154,0.52924732199469,-0.178884997111813));
#20656=CARTESIAN_POINT('Ctrl Pts',(-3.58013963908983,0.531429167668471,
-0.184879568833261));
#20657=CARTESIAN_POINT('Ctrl Pts',(-3.56441224699608,0.533384292376045,
-0.190251229819538));
#20658=CARTESIAN_POINT('Ctrl Pts',(-3.5485570527871,0.535140904149324,-0.19507748100137));
#20659=CARTESIAN_POINT('Ctrl Pts',(-3.53268239263572,0.53689967257254,-0.199909657530206));
#20660=CARTESIAN_POINT('Ctrl Pts',(-3.51667900179308,0.538459473597168,
-0.204195175624212));
#20661=CARTESIAN_POINT('Ctrl Pts',(-3.50053180651659,0.539831120837288,
-0.207963745443901));
#20662=CARTESIAN_POINT('Ctrl Pts',(-3.48386348055343,0.541247036289682,
-0.21185394117721));
#20663=CARTESIAN_POINT('Ctrl Pts',(-3.46704135193447,0.542462516150015,
-0.215193444647276));
#20664=CARTESIAN_POINT('Ctrl Pts',(-3.45004930524678,0.543469776899708,
-0.217960870812559));
#20665=CARTESIAN_POINT('Ctrl Pts',(-3.43655982054718,0.544269411500601,
-0.220157848822329));
#20666=CARTESIAN_POINT('Ctrl Pts',(-3.42296310261358,0.544937465463458,
-0.221993312000254));
#20667=CARTESIAN_POINT('Ctrl Pts',(-3.40925535079096,0.545461019899046,
-0.223431765989889));
#20668=CARTESIAN_POINT('Ctrl Pts',(-3.39748261302319,0.545910668328423,
-0.224667164896297));
#20669=CARTESIAN_POINT('Ctrl Pts',(-3.38563650689686,0.546253524649681,
-0.225609154897069));
#20670=CARTESIAN_POINT('Ctrl Pts',(-3.3736853870908,0.546476778145907,-0.226222538836764));
#20671=CARTESIAN_POINT('Ctrl Pts',(-3.36016796810983,0.546729290972858,
-0.226916312126935));
#20672=CARTESIAN_POINT('Ctrl Pts',(-3.34651252112207,0.546829337291431,
-0.227191187128114));
#20673=CARTESIAN_POINT('Ctrl Pts',(-3.33267610475802,0.546744862736256,
-0.226959095195251));
#20674=CARTESIAN_POINT('Ctrl Pts',(-3.32110141125817,0.546674196527682,
-0.226764941382877));
#20675=CARTESIAN_POINT('Ctrl Pts',(-3.3094000957189,0.546474225573401,-0.226215525701441));
#20676=CARTESIAN_POINT('Ctrl Pts',(-3.29755962677078,0.546116630947227,
-0.225233042540711));
#20677=CARTESIAN_POINT('Ctrl Pts',(-3.28814851407603,0.545832405437181,
-0.224452139369827));
#20678=CARTESIAN_POINT('Ctrl Pts',(-3.27864397132647,0.545448060082736,
-0.223396159187217));
#20679=CARTESIAN_POINT('Ctrl Pts',(-3.26907623467603,0.544946536842993,
-0.222018235410691));
#20680=CARTESIAN_POINT('Ctrl Pts',(-3.24982747331958,0.543937552011029,
-0.219246072368296));
#20681=CARTESIAN_POINT('Ctrl Pts',(-3.23033080009046,0.542455134615159,
-0.215173164046936));
#20682=CARTESIAN_POINT('Ctrl Pts',(-3.21094931274948,0.540352353894123,
-0.209395821497827));
#20683=CARTESIAN_POINT('Ctrl Pts',(-3.20077276026693,0.539248256051144,
-0.206362337605374));
#20684=CARTESIAN_POINT('Ctrl Pts',(-3.19062885973354,0.537972925085944,
-0.202858394576155));
#20685=CARTESIAN_POINT('Ctrl Pts',(-3.18057391345523,0.536504701365254,
-0.198824483056852));
#20686=CARTESIAN_POINT('Ctrl Pts',(-3.17465003302617,0.535639696070971,
-0.1964479005431));
#20687=CARTESIAN_POINT('Ctrl Pts',(-3.1687549656581,0.534707371098516,-0.193886358733686));
#20688=CARTESIAN_POINT('Ctrl Pts',(-3.16290756953124,0.533704680892061,
-0.191131490032742));
#20689=CARTESIAN_POINT('Ctrl Pts',(-3.15405708743901,0.532187032433883,
-0.186961785163228));
#20690=CARTESIAN_POINT('Ctrl Pts',(-3.14532752481795,0.530508785283586,
-0.182350839013525));
#20691=CARTESIAN_POINT('Ctrl Pts',(-3.13684553141908,0.528682129286832,
-0.177332142909332));
#20692=CARTESIAN_POINT('Ctrl Pts',(-3.12879381283923,0.526948135951016,
-0.172568035373691));
#20693=CARTESIAN_POINT('Ctrl Pts',(-3.12096520761203,0.525080479341376,
-0.167436691011411));
#20694=CARTESIAN_POINT('Ctrl Pts',(-3.11344649454215,0.523102727922514,
-0.162002863646793));
#20695=CARTESIAN_POINT('Ctrl Pts',(-3.10446773365921,0.520740919869617,
-0.155513849352373));
#20696=CARTESIAN_POINT('Ctrl Pts',(-3.0959270560741,0.518221524243454,-0.148591866758818));
#20697=CARTESIAN_POINT('Ctrl Pts',(-3.08787517326817,0.515585575459487,
-0.141349656996029));
#20698=CARTESIAN_POINT('Ctrl Pts',(-3.08147273160297,0.513489605022683,
-0.135591025549066));
#20699=CARTESIAN_POINT('Ctrl Pts',(-3.0753789290815,0.511320332691276,-0.129630998801876));
#20700=CARTESIAN_POINT('Ctrl Pts',(-3.06960775233313,0.509104574416123,
-0.123543252973923));
#20701=CARTESIAN_POINT('Ctrl Pts',(-3.06372377560279,0.506845508249982,
-0.117336519693398));
#20702=CARTESIAN_POINT('Ctrl Pts',(-3.05817974413936,0.504540843174219,
-0.111004504438334));
#20703=CARTESIAN_POINT('Ctrl Pts',(-3.05293955472372,0.502203600541567,
-0.104582983081335));
#20704=CARTESIAN_POINT('Ctrl Pts',(-3.04420284120351,0.498306829320328,
-0.0938766921421992));
#20705=CARTESIAN_POINT('Ctrl Pts',(-3.03630814797779,0.4943198500131,-0.0829225565237586));
#20706=CARTESIAN_POINT('Ctrl Pts',(-3.02909796092231,0.490287466832876,
-0.0718436747895053));
#20707=CARTESIAN_POINT('Ctrl Pts',(-3.02161999941514,0.48610532759407,-0.0603533416658699));
#20708=CARTESIAN_POINT('Ctrl Pts',(-3.01487803363331,0.481874376480483,
-0.0487288990184732));
#20709=CARTESIAN_POINT('Ctrl Pts',(-3.00872169536913,0.477626257281286,
-0.0370572874435275));
#20710=CARTESIAN_POINT('Ctrl Pts',(-3.00349762266516,0.474021438540117,
-0.0271531293509397));
#20711=CARTESIAN_POINT('Ctrl Pts',(-2.99869545470355,0.470403755285769,
-0.0172136262988795));
#20712=CARTESIAN_POINT('Ctrl Pts',(-2.9942367434548,0.466781597354371,-0.00726182917266559));
#20713=CARTESIAN_POINT('Ctrl Pts',(-2.98835950279235,0.462007057651627,
0.00585611084891477));
#20714=CARTESIAN_POINT('Ctrl Pts',(-2.98308260387313,0.457228034424005,
0.0189863692538536));
#20715=CARTESIAN_POINT('Ctrl Pts',(-2.97827812075261,0.452466276252641,
0.0320691923065807));
#20716=CARTESIAN_POINT('Ctrl Pts',(-2.97325578738024,0.447488605111897,
0.045745231367245));
#20717=CARTESIAN_POINT('Ctrl Pts',(-2.96874974008818,0.442529710065418,
0.0593696835328924));
#20718=CARTESIAN_POINT('Ctrl Pts',(-2.9646429990344,0.437597110787006,0.0729218886695459));
#20719=CARTESIAN_POINT('Ctrl Pts',(-2.96031131519025,0.432394333128475,
0.0872164028048048));
#20720=CARTESIAN_POINT('Ctrl Pts',(-2.95642400398736,0.427220699948731,
0.101430843142691));
#20721=CARTESIAN_POINT('Ctrl Pts',(-2.95287408362541,0.422067771173593,
0.115588398596441));
#20722=CARTESIAN_POINT('Ctrl Pts',(-2.9491044072207,0.416595852922409,0.130622370432671));
#20723=CARTESIAN_POINT('Ctrl Pts',(-2.94571535463065,0.411147158745473,
0.145592534649317));
#20724=CARTESIAN_POINT('Ctrl Pts',(-2.942609760046,0.405694490587329,0.160573617289596));
#20725=CARTESIAN_POINT('Ctrl Pts',(-2.93974684524852,0.400667909064796,
0.174384036519804));
#20726=CARTESIAN_POINT('Ctrl Pts',(-2.93712392796838,0.395632789357454,
0.188217914219976));
#20727=CARTESIAN_POINT('Ctrl Pts',(-2.93470339303712,0.390603676173332,
0.202035289133233));
#20728=CARTESIAN_POINT('Ctrl Pts',(-2.93099979535042,0.382908760593194,
0.223176895934272));
#20729=CARTESIAN_POINT('Ctrl Pts',(-2.92776715655637,0.375226020910854,
0.244285049731048));
#20730=CARTESIAN_POINT('Ctrl Pts',(-2.92488564478655,0.367576098718698,
0.265303038214582));
#20731=CARTESIAN_POINT('Ctrl Pts',(-2.92184968434103,0.35951614163992,0.287447588290298));
#20732=CARTESIAN_POINT('Ctrl Pts',(-2.91920364550544,0.351492503454705,
0.309492353026049));
#20733=CARTESIAN_POINT('Ctrl Pts',(-2.91683841522211,0.34351219560062,0.331418068655445));
#20734=CARTESIAN_POINT('Ctrl Pts',(-2.91432245416582,0.335023320788077,
0.354741060519485));
#20735=CARTESIAN_POINT('Ctrl Pts',(-2.91212444088888,0.326583343686617,
0.377929707026459));
#20736=CARTESIAN_POINT('Ctrl Pts',(-2.91014448265287,0.318183739895187,
0.401007428775779));
#20737=CARTESIAN_POINT('Ctrl Pts',(-2.907919558577,0.308744914184863,0.426940389281062));
#20738=CARTESIAN_POINT('Ctrl Pts',(-2.90597008942706,0.29935700917154,0.452733446321151));
#20739=CARTESIAN_POINT('Ctrl Pts',(-2.90419078248043,0.289988480614236,
0.47847326698586));
#20740=CARTESIAN_POINT('Ctrl Pts',(-2.90291344823327,0.283262973025782,
0.496951447219508));
#20741=CARTESIAN_POINT('Ctrl Pts',(-2.90172462797116,0.276547017573975,
0.515403383173411));
#20742=CARTESIAN_POINT('Ctrl Pts',(-2.90059397675046,0.269824323391606,
0.533873833637369));
#20743=CARTESIAN_POINT('Ctrl Pts',(-2.89983485563977,0.265310695332727,
0.546274924808955));
#20744=CARTESIAN_POINT('Ctrl Pts',(-2.89910178887351,0.26079188236583,0.558690261398245));
#20745=CARTESIAN_POINT('Ctrl Pts',(-2.89838906856979,0.256276445704804,
0.571096321663392));
#20746=CARTESIAN_POINT('Ctrl Pts',(-2.89654063821258,0.244565722498618,
0.603271269237869));
#20747=CARTESIAN_POINT('Ctrl Pts',(-2.89482523118125,0.232869975283629,
0.6354050706147));
#20748=CARTESIAN_POINT('Ctrl Pts',(-2.89314446329961,0.221201583373919,
0.667463713907976));
#20749=CARTESIAN_POINT('Ctrl Pts',(-2.89134078182618,0.208679888652084,
0.70186678740952));
#20750=CARTESIAN_POINT('Ctrl Pts',(-2.88957745244866,0.196189464596047,
0.736183945462895));
#20751=CARTESIAN_POINT('Ctrl Pts',(-2.88776644175644,0.183726850734524,
0.770424695634813));
#20752=CARTESIAN_POINT('Ctrl Pts',(-2.88572744403318,0.169695326018192,
0.808975992953454));
#20753=CARTESIAN_POINT('Ctrl Pts',(-2.88362845669159,0.155698865847008,
0.847430951226077));
#20754=CARTESIAN_POINT('Ctrl Pts',(-2.88137742145133,0.141713015122622,
0.885856760283194));
#20755=CARTESIAN_POINT('Ctrl Pts',(-2.88071953338383,0.137625507232499,
0.897087095913149));
#20756=CARTESIAN_POINT('Ctrl Pts',(-2.88004882973202,0.133538801428664,
0.908315227829142));
#20757=CARTESIAN_POINT('Ctrl Pts',(-2.87936339380758,0.129452050955556,
0.919543482472952));
#20758=CARTESIAN_POINT('Origin',(-3.43968169690379,0.263987455675957,0.316006143873413));
#20759=CARTESIAN_POINT('',(-3.91503635643998,0.0542766412926798,0.892181871006905));
#20760=CARTESIAN_POINT('',(-4.5,0.0542766412926824,0.892181871006898));
#20761=CARTESIAN_POINT('Origin',(-4.07070327333776,0.0413242491918032,0.927768275831754));
#20762=CARTESIAN_POINT('Origin',(-3.2,0.9,1.2));
#20763=CARTESIAN_POINT('',(-4.05408422825637,4.03679607859634E-16,1.1999999999999));
#20764=CARTESIAN_POINT('',(-4.5,0.,1.2));
#20765=CARTESIAN_POINT('',(-3.9178024645294,0.00300376380597895,1.12653061234128));
#20766=CARTESIAN_POINT('Ctrl Pts',(-3.91780246453198,0.00300376306932705,
1.12653061227823));
#20767=CARTESIAN_POINT('Ctrl Pts',(-3.91789635426004,0.00299646731275753,
1.1266196870125));
#20768=CARTESIAN_POINT('Ctrl Pts',(-3.91799025015003,0.0029891856217416,
1.12670875309452));
#20769=CARTESIAN_POINT('Ctrl Pts',(-3.93198424061395,0.00190612082577026,
1.13998060667364));
#20770=CARTESIAN_POINT('Ctrl Pts',(-3.95372016194337,0.000728182714508301,
1.16059376321201));
#20771=CARTESIAN_POINT('Ctrl Pts',(-3.98957829615743,0.000138376987816399,
1.18285735678753));
#20772=CARTESIAN_POINT('Ctrl Pts',(-4.00792465999132,1.58115480707647E-5,
1.19293784769595));
#20773=CARTESIAN_POINT('Ctrl Pts',(-4.03839217161777,-9.33473974974476E-7,
1.19912770931096));
#20774=CARTESIAN_POINT('Ctrl Pts',(-4.04624242871877,7.69055196891966E-18,
1.19999825406822));
#20775=CARTESIAN_POINT('Ctrl Pts',(-4.05408422825637,6.93889390390723E-18,
1.19999999999961));
#20776=CARTESIAN_POINT('',(-3.91070419800688,0.0384900677109038,0.939614446316166));
#20777=CARTESIAN_POINT('Ctrl Pts',(-3.91070419800688,0.0384900677109038,
0.939614446316166));
#20778=CARTESIAN_POINT('Ctrl Pts',(-3.91354706175869,0.0201143993533441,
1.00041206192318));
#20779=CARTESIAN_POINT('Ctrl Pts',(-3.91582848502696,0.00819208764812623,
1.06318918889612));
#20780=CARTESIAN_POINT('Ctrl Pts',(-3.91780246457708,0.0030037652751779,
1.1265306125175));
#20781=CARTESIAN_POINT('Ctrl Pts',(-3.91503635643999,0.0542766412926799,
0.892181871006906));
#20782=CARTESIAN_POINT('Ctrl Pts',(-3.91141850629553,0.0486938803101099,
0.90752038074473));
#20783=CARTESIAN_POINT('Ctrl Pts',(-3.90995323778991,0.043344115284559,
0.923554376403128));
#20784=CARTESIAN_POINT('Ctrl Pts',(-3.91070419800688,0.0384900677109053,
0.939614446316161));
#20785=CARTESIAN_POINT('Ctrl Pts',(4.1,0.,11.7890187209237));
#20786=CARTESIAN_POINT('Ctrl Pts',(4.1778740733922,2.3055357147031E-16,
11.7166528289146));
#20787=CARTESIAN_POINT('Ctrl Pts',(4.25493082441583,0.00976502690773917,
11.6434441359381));
#20788=CARTESIAN_POINT('Ctrl Pts',(4.33293714067645,0.0306667563623946,
11.5737513316985));
#20789=CARTESIAN_POINT('Ctrl Pts',(4.11709141945523,0.,11.8057761908248));
#20790=CARTESIAN_POINT('Ctrl Pts',(4.19446713550167,0.00152406851324286,
11.7325672253649));
#20791=CARTESIAN_POINT('Ctrl Pts',(4.27036703049148,0.0125190657257837,
11.6590157024546));
#20792=CARTESIAN_POINT('Ctrl Pts',(4.34699197838351,0.0344327387772118,
11.5891134622547));
#20793=CARTESIAN_POINT('Ctrl Pts',(4.14667038231247,0.0201034459912815,
11.8347772097913));
#20794=CARTESIAN_POINT('Ctrl Pts',(4.22147162288739,0.0224535142329611,
11.7602048577659));
#20795=CARTESIAN_POINT('Ctrl Pts',(4.29413970444214,0.0340349382796113,
11.6860288143997));
#20796=CARTESIAN_POINT('Ctrl Pts',(4.36741004838275,0.0559487962903834,
11.6158150586253));
#20797=CARTESIAN_POINT('Ctrl Pts',(4.15712386170589,0.062048041979487,11.8450264384616));
#20798=CARTESIAN_POINT('Ctrl Pts',(4.22938050951698,0.0627480300001918,
11.7713116264474));
#20799=CARTESIAN_POINT('Ctrl Pts',(4.2996344178864,0.0724531692081621,11.6980817694637));
#20800=CARTESIAN_POINT('Ctrl Pts',(4.3703722128866,0.0923540347180163,11.6287837175683));
#20801=CARTESIAN_POINT('Ctrl Pts',(4.15712386170589,0.0800000000000001,
11.8450264384616));
#20802=CARTESIAN_POINT('Ctrl Pts',(4.22862937879342,0.0800000000000004,
11.7720959308659));
#20803=CARTESIAN_POINT('Ctrl Pts',(4.29822259191301,0.0888970245159395,
11.6995328113185));
#20804=CARTESIAN_POINT('Ctrl Pts',(4.36824305034239,0.107940822463515,11.6308715500256));
#20805=CARTESIAN_POINT('',(4.15712386170589,0.0800000000000001,11.8450264384616));
#20806=CARTESIAN_POINT('Ctrl Pts',(4.23249000178399,0.0834041484552263,
11.7678256594183));
#20807=CARTESIAN_POINT('Ctrl Pts',(4.20753856027708,0.081116204299734,11.7934084522297));
#20808=CARTESIAN_POINT('Ctrl Pts',(4.18245116805733,0.0800000000000002,
11.8191943994319));
#20809=CARTESIAN_POINT('Ctrl Pts',(4.15712386170589,0.0800000000000001,
11.8450264384616));
#20810=CARTESIAN_POINT('',(4.1,0.,11.7890187209237));
#20811=CARTESIAN_POINT('Origin',(4.1,0.0800000000000001,11.7890187209237));
#20812=CARTESIAN_POINT('Ctrl Pts',(4.1,0.,11.7890187209237));
#20813=CARTESIAN_POINT('Ctrl Pts',(4.1778740733922,2.3055357147031E-16,
11.7166528289146));
#20814=CARTESIAN_POINT('Ctrl Pts',(4.25493082441583,0.00976502690773917,
11.6434441359381));
#20815=CARTESIAN_POINT('Ctrl Pts',(4.33293714067645,0.0306667563623946,
11.5737513316985));
#20816=CARTESIAN_POINT('Ctrl Pts',(4.09999999999981,0.08,11.9026515720696));
#20817=CARTESIAN_POINT('Ctrl Pts',(4.06432399954022,0.08,11.9381300567193));
#20818=CARTESIAN_POINT('Ctrl Pts',(3.98818983778508,0.08,12.0113745379845));
#20819=CARTESIAN_POINT('Ctrl Pts',(3.86893999186953,0.08,12.1091025700166));
#20820=CARTESIAN_POINT('Ctrl Pts',(3.73111116955382,0.08,12.1934030676208));
#20821=CARTESIAN_POINT('Ctrl Pts',(3.52459155666187,0.08,12.2691718924221));
#20822=CARTESIAN_POINT('Ctrl Pts',(3.26513646721023,0.08,12.2978239927277));
#20823=CARTESIAN_POINT('Ctrl Pts',(2.86516691280962,0.08,12.3018717460263));
#20824=CARTESIAN_POINT('Ctrl Pts',(2.3724345221647,0.08,12.2928334043575));
#20825=CARTESIAN_POINT('Ctrl Pts',(1.18525410089388,0.0800000000000001,
12.2925039217734));
#20826=CARTESIAN_POINT('Ctrl Pts',(-0.197223498551522,0.08,12.3061838691053));
#20827=CARTESIAN_POINT('Ctrl Pts',(-1.58273390323592,0.08,12.2905351916681));
#20828=CARTESIAN_POINT('Ctrl Pts',(-2.37158423452643,0.08,12.2934900223558));
#20829=CARTESIAN_POINT('Ctrl Pts',(-2.8649548727089,0.08,12.3017730777117));
#20830=CARTESIAN_POINT('Ctrl Pts',(-3.26529575985038,0.08,12.2978370579524));
#20831=CARTESIAN_POINT('Ctrl Pts',(-3.52422781159081,0.08,12.2692312868616));
#20832=CARTESIAN_POINT('Ctrl Pts',(-3.73122681675827,0.08,12.1933713817583));
#20833=CARTESIAN_POINT('Ctrl Pts',(-3.86889459911728,0.08,12.1090065132441));
#20834=CARTESIAN_POINT('Ctrl Pts',(-3.98631749393431,0.08,12.0130274731947));
#20835=CARTESIAN_POINT('Ctrl Pts',(-4.06432399954019,0.08,11.9381300567181));
#20836=CARTESIAN_POINT('Ctrl Pts',(-4.0999999999998,0.08,11.9026515720685));
#20837=CARTESIAN_POINT('Ctrl Pts',(4.09999999999981,0.0560640559726492,
11.9026515720696));
#20838=CARTESIAN_POINT('Ctrl Pts',(4.06432200541893,0.0560640559726492,
11.9381320398003));
#20839=CARTESIAN_POINT('Ctrl Pts',(3.98819817514749,0.0560640559726492,
12.0113732141449));
#20840=CARTESIAN_POINT('Ctrl Pts',(3.86894130022029,0.0560640559726492,
12.1091110958518));
#20841=CARTESIAN_POINT('Ctrl Pts',(3.73109430755215,0.0560640559726492,
12.1934253732652));
#20842=CARTESIAN_POINT('Ctrl Pts',(3.52453032420505,0.0560640559726492,
12.2692082165472));
#20843=CARTESIAN_POINT('Ctrl Pts',(3.26508176198252,0.0560640559726491,
12.2978447746476));
#20844=CARTESIAN_POINT('Ctrl Pts',(2.86512835900754,0.0560640559726492,
12.301883596069));
#20845=CARTESIAN_POINT('Ctrl Pts',(2.37242466553327,0.0560640559726492,
12.2928361559738));
#20846=CARTESIAN_POINT('Ctrl Pts',(1.18525566090828,0.0560640559726493,
12.2925052045904));
#20847=CARTESIAN_POINT('Ctrl Pts',(-0.197226227294698,0.0560640559726492,
12.3061822863099));
#20848=CARTESIAN_POINT('Ctrl Pts',(-1.58273033360394,0.0560640559726493,
12.2905370248849));
#20849=CARTESIAN_POINT('Ctrl Pts',(-2.37157938813513,0.0560640559726492,
12.2934911038005));
#20850=CARTESIAN_POINT('Ctrl Pts',(-2.86490940365101,0.0560640559726493,
12.301787110831));
#20851=CARTESIAN_POINT('Ctrl Pts',(-3.26524117145924,0.0560640559726493,
12.2978577914992));
#20852=CARTESIAN_POINT('Ctrl Pts',(-3.52416558815914,0.0560640559726493,
12.2692679240856));
#20853=CARTESIAN_POINT('Ctrl Pts',(-3.73120976022586,0.0560640559726493,
12.193393737439));
#20854=CARTESIAN_POINT('Ctrl Pts',(-3.86889559828825,0.0560640559726493,
12.1090151471365));
#20855=CARTESIAN_POINT('Ctrl Pts',(-3.98632550448738,0.0560640559726493,
12.0130263967018));
#20856=CARTESIAN_POINT('Ctrl Pts',(-4.0643220054189,0.0560640559726493,
11.9381320397991));
#20857=CARTESIAN_POINT('Ctrl Pts',(-4.0999999999998,0.0560640559726493,
11.9026515720685));
#20858=CARTESIAN_POINT('Ctrl Pts',(4.08582423633291,0.0146397293840558,
11.8883968890952));
#20859=CARTESIAN_POINT('Ctrl Pts',(4.05030551310779,0.0146397293840558,
11.9237189672565));
#20860=CARTESIAN_POINT('Ctrl Pts',(3.9746955606649,0.0146397293840557,11.9964469996915));
#20861=CARTESIAN_POINT('Ctrl Pts',(3.85709175380371,0.0146397293840558,
12.0927851123546));
#20862=CARTESIAN_POINT('Ctrl Pts',(3.72224943041651,0.0146397293840557,
12.1751948890262));
#20863=CARTESIAN_POINT('Ctrl Pts',(3.52063632363833,0.0146397293840557,
12.2492384843966));
#20864=CARTESIAN_POINT('Ctrl Pts',(3.26439578123385,0.0146397293840557,
12.277728740107));
#20865=CARTESIAN_POINT('Ctrl Pts',(2.8655223444065,0.0146397293840557,12.2817567080134));
#20866=CARTESIAN_POINT('Ctrl Pts',(2.37263681728462,0.0146397293840557,
12.2727335042978));
#20867=CARTESIAN_POINT('Ctrl Pts',(1.18492866445151,0.0146397293840561,
12.2723941790853));
#20868=CARTESIAN_POINT('Ctrl Pts',(-0.197082299090637,0.0146397293840558,
12.286086899881));
#20869=CARTESIAN_POINT('Ctrl Pts',(-1.58260309447466,0.0146397293840562,
12.2704270240485));
#20870=CARTESIAN_POINT('Ctrl Pts',(-2.37177693824149,0.0146397293840558,
12.2733925401474));
#20871=CARTESIAN_POINT('Ctrl Pts',(-2.86532165277665,0.0146397293840561,
12.2816543668416));
#20872=CARTESIAN_POINT('Ctrl Pts',(-3.26455165823213,0.0146397293840562,
12.2777430390883));
#20873=CARTESIAN_POINT('Ctrl Pts',(-3.52028225283393,0.0146397293840561,
12.2492943914395));
#20874=CARTESIAN_POINT('Ctrl Pts',(-3.72236259942317,0.0146397293840561,
12.1751643380234));
#20875=CARTESIAN_POINT('Ctrl Pts',(-3.85705264607581,0.014639729384056,
12.0926856460335));
#20876=CARTESIAN_POINT('Ctrl Pts',(-3.97284413197348,0.014639729384056,
11.998081262117));
#20877=CARTESIAN_POINT('Ctrl Pts',(-4.05030551310777,0.0146397293840561,
11.9237189672553));
#20878=CARTESIAN_POINT('Ctrl Pts',(-4.08582423633293,0.0146397293840561,
11.888396889094));
#20879=CARTESIAN_POINT('Ctrl Pts',(4.05624736761446,-1.09923062066103E-16,
11.8586553600413));
#20880=CARTESIAN_POINT('Ctrl Pts',(4.02105560774433,-1.14986681133505E-16,
11.8936522850402));
#20881=CARTESIAN_POINT('Ctrl Pts',(3.94654553093069,-1.32301790805734E-16,
11.9653008115684));
#20882=CARTESIAN_POINT('Ctrl Pts',(3.83237190384969,-1.17548824419341E-16,
12.0587448002228));
#20883=CARTESIAN_POINT('Ctrl Pts',(3.7037499217885,-1.63179123823165E-16,
12.13721789838));
#20884=CARTESIAN_POINT('Ctrl Pts',(3.51234755170784,-1.2488020255128E-16,
12.207670245142));
#20885=CARTESIAN_POINT('Ctrl Pts',(3.26281784836069,-2.24963096574075E-16,
12.2358135780229));
#20886=CARTESIAN_POINT('Ctrl Pts',(2.86624100045032,-1.52293381882714E-16,
12.2397949525638));
#20887=CARTESIAN_POINT('Ctrl Pts',(2.3730530313914,-1.90334102701785E-16,
12.2307979218616));
#20888=CARTESIAN_POINT('Ctrl Pts',(1.18425058894606,2.83933512305755E-16,
12.2304371870165));
#20889=CARTESIAN_POINT('Ctrl Pts',(-0.19678931795809,-5.0793709047756E-17,
12.2441548545081));
#20890=CARTESIAN_POINT('Ctrl Pts',(-1.58232804686594,4.50897213697133E-16,
12.2284736456218));
#20891=CARTESIAN_POINT('Ctrl Pts',(-2.37217612036961,-3.31978508512746E-17,
12.2314610090552));
#20892=CARTESIAN_POINT('Ctrl Pts',(-2.8660598737781,3.25578437998814E-16,
12.2396862466115));
#20893=CARTESIAN_POINT('Ctrl Pts',(-3.26296666832,4.68732183862947E-16,
12.2358304223918));
#20894=CARTESIAN_POINT('Ctrl Pts',(-3.51201307627747,3.5252554681229E-16,
12.2077190621633));
#20895=CARTESIAN_POINT('Ctrl Pts',(-3.70385780448657,3.19211288769243E-16,
12.1371897449525));
#20896=CARTESIAN_POINT('Ctrl Pts',(-3.83234572555419,2.13429601981668E-16,
12.0586382843544));
#20897=CARTESIAN_POINT('Ctrl Pts',(-3.94473754607314,1.88196963216156E-16,
11.9668962614767));
#20898=CARTESIAN_POINT('Ctrl Pts',(-4.02105560774434,2.57336224836312E-16,
11.893652285039));
#20899=CARTESIAN_POINT('Ctrl Pts',(-4.05624736761451,2.50899420937073E-16,
11.8586553600401));
#20900=CARTESIAN_POINT('Ctrl Pts',(4.0435887019288,-1.11022302462516E-16,
11.8459262210355));
#20901=CARTESIAN_POINT('Ctrl Pts',(4.00853667496432,-1.16081809443283E-16,
11.8807841867429));
#20902=CARTESIAN_POINT('Ctrl Pts',(3.93449839739079,-1.33394172299536E-16,
11.9519703536246));
#20903=CARTESIAN_POINT('Ctrl Pts',(3.82179213813238,-1.18666346909376E-16,
12.0441766918018));
#20904=CARTESIAN_POINT('Ctrl Pts',(3.69583054658886,-1.64263096837451E-16,
12.1209663380819));
#20905=CARTESIAN_POINT('Ctrl Pts',(3.50879373356752,-1.2597952000311E-16,
12.1898830987469));
#20906=CARTESIAN_POINT('Ctrl Pts',(3.26213688664597,-2.26051670054873E-16,
12.2178763550172));
#20907=CARTESIAN_POINT('Ctrl Pts',(2.86654461957332,-1.53389929340232E-16,
12.221836870547));
#20908=CARTESIAN_POINT('Ctrl Pts',(2.37323015533067,-1.91431012567934E-16,
12.212850107161));
#20909=CARTESIAN_POINT('Ctrl Pts',(1.18396053823096,2.82832847689486E-16,
12.212480058298));
#20910=CARTESIAN_POINT('Ctrl Pts',(-0.196664204629831,-5.18915455952868E-17,
12.2262081084424));
#20911=CARTESIAN_POINT('Ctrl Pts',(-1.58220996201918,4.49796397254339E-16,
12.2105181200467));
#20912=CARTESIAN_POINT('Ctrl Pts',(-2.37234646937341,-3.42995743393534E-17,
12.2135147567495));
#20913=CARTESIAN_POINT('Ctrl Pts',(-2.86637115626172,3.24464130618306E-16,
12.2217256647492));
#20914=CARTESIAN_POINT('Ctrl Pts',(-3.26228269824909,4.67598234842018E-16,
12.2178942838233));
#20915=CARTESIAN_POINT('Ctrl Pts',(-3.50846754301617,3.51404355795733E-16,
12.1899289134544));
#20916=CARTESIAN_POINT('Ctrl Pts',(-3.69593614680787,3.18100712493542E-16,
12.1209392159371));
#20917=CARTESIAN_POINT('Ctrl Pts',(-3.82177146177483,2.12368510762661E-16,
12.0440671698819));
#20918=CARTESIAN_POINT('Ctrl Pts',(-3.93270897258269,1.87121689875167E-16,
11.9535492174884));
#20919=CARTESIAN_POINT('Ctrl Pts',(-4.00853667496434,2.56231757211128E-16,
11.8807841867417));
#20920=CARTESIAN_POINT('Ctrl Pts',(-4.04358870192886,2.4980018054066E-16,
11.8459262210343));
#20921=CARTESIAN_POINT('',(-4.04358870192886,0.,11.8459262210343));
#20922=CARTESIAN_POINT('Origin',(-4.04358870192886,0.08,11.8459262210343));
#20923=CARTESIAN_POINT('',(4.0435887019288,0.,11.8459262210355));
#20924=CARTESIAN_POINT('Ctrl Pts',(-4.04358870192886,2.4980018054066E-16,
11.8459262210343));
#20925=CARTESIAN_POINT('Ctrl Pts',(-4.00853667496434,2.56231757211128E-16,
11.8807841867417));
#20926=CARTESIAN_POINT('Ctrl Pts',(-3.93270897258269,1.87121689875167E-16,
11.9535492174884));
#20927=CARTESIAN_POINT('Ctrl Pts',(-3.82177146177483,2.12368510762661E-16,
12.0440671698819));
#20928=CARTESIAN_POINT('Ctrl Pts',(-3.69593614680787,3.18100712493542E-16,
12.1209392159371));
#20929=CARTESIAN_POINT('Ctrl Pts',(-3.50846754301617,3.51404355795733E-16,
12.1899289134544));
#20930=CARTESIAN_POINT('Ctrl Pts',(-3.26228269824909,4.67598234842018E-16,
12.2178942838233));
#20931=CARTESIAN_POINT('Ctrl Pts',(-2.86637115626172,3.24464130618306E-16,
12.2217256647492));
#20932=CARTESIAN_POINT('Ctrl Pts',(-2.37234646937341,-3.42995743393534E-17,
12.2135147567495));
#20933=CARTESIAN_POINT('Ctrl Pts',(-1.58220996201918,4.49796397254339E-16,
12.2105181200467));
#20934=CARTESIAN_POINT('Ctrl Pts',(-0.196664204629831,-5.18915455952868E-17,
12.2262081084424));
#20935=CARTESIAN_POINT('Ctrl Pts',(1.18396053823096,2.82832847689486E-16,
12.212480058298));
#20936=CARTESIAN_POINT('Ctrl Pts',(2.37323015533067,-1.91431012567934E-16,
12.212850107161));
#20937=CARTESIAN_POINT('Ctrl Pts',(2.86654461957332,-1.53389929340232E-16,
12.221836870547));
#20938=CARTESIAN_POINT('Ctrl Pts',(3.26213688664597,-2.26051670054873E-16,
12.2178763550172));
#20939=CARTESIAN_POINT('Ctrl Pts',(3.50879373356752,-1.2597952000311E-16,
12.1898830987469));
#20940=CARTESIAN_POINT('Ctrl Pts',(3.69583054658886,-1.64263096837451E-16,
12.1209663380819));
#20941=CARTESIAN_POINT('Ctrl Pts',(3.82179213813238,-1.18666346909376E-16,
12.0441766918018));
#20942=CARTESIAN_POINT('Ctrl Pts',(3.93449839739079,-1.33394172299536E-16,
11.9519703536246));
#20943=CARTESIAN_POINT('Ctrl Pts',(4.00853667496432,-1.16081809443283E-16,
11.8807841867429));
#20944=CARTESIAN_POINT('Ctrl Pts',(4.0435887019288,-1.11022302462516E-16,
11.8459262210355));
#20945=CARTESIAN_POINT('Origin',(4.0435887019288,0.08,11.8459262210355));
#20946=CARTESIAN_POINT('Ctrl Pts',(4.15712386170585,0.08,11.8450264384616));
#20947=CARTESIAN_POINT('Ctrl Pts',(4.13827843210564,0.08,11.8642474273109));
#20948=CARTESIAN_POINT('Ctrl Pts',(4.11927627294067,0.08,11.8834820198546));
#20949=CARTESIAN_POINT('Ctrl Pts',(4.09999999999983,0.08,11.9026515720696));
#20950=CARTESIAN_POINT('Ctrl Pts',(4.15712386170585,0.0560640559726494,
11.8450264384616));
#20951=CARTESIAN_POINT('Ctrl Pts',(4.13827796583819,0.0560640559726494,
11.8642479028703));
#20952=CARTESIAN_POINT('Ctrl Pts',(4.11927735039403,0.0560640559726492,
11.8834809483664));
#20953=CARTESIAN_POINT('Ctrl Pts',(4.09999999999983,0.0560640559726491,
11.9026515720696));
#20954=CARTESIAN_POINT('Ctrl Pts',(4.14276903578864,0.0146397293927042,
11.8309520917479));
#20955=CARTESIAN_POINT('Ctrl Pts',(4.12396038090976,0.0146397293927042,
11.8501355730145));
#20956=CARTESIAN_POINT('Ctrl Pts',(4.10501553004289,0.0146397293927035,
11.8693118456237));
#20957=CARTESIAN_POINT('Ctrl Pts',(4.08582423632785,0.0146397293927031,
11.88839688909));
#20958=CARTESIAN_POINT('Ctrl Pts',(4.11281856459138,1.07485755671115E-15,
11.8015868233495));
#20959=CARTESIAN_POINT('Ctrl Pts',(4.09408636061341,1.00638808982717E-15,
11.8206923301711));
#20960=CARTESIAN_POINT('Ctrl Pts',(4.07526199817246,7.19794876773123E-16,
11.8397460016581));
#20961=CARTESIAN_POINT('Ctrl Pts',(4.05624736761449,-2.53423937412745E-16,
11.8586553600413));
#20962=CARTESIAN_POINT('Ctrl Pts',(4.09999999999996,1.22124532708767E-15,
11.7890187209237));
#20963=CARTESIAN_POINT('Ctrl Pts',(4.0813004685107,1.13295521928305E-15,
11.8080909041462));
#20964=CARTESIAN_POINT('Ctrl Pts',(4.06252783272243,1.14575066216236E-15,
11.8270919444215));
#20965=CARTESIAN_POINT('Ctrl Pts',(4.04358870192882,-1.11022302462516E-16,
11.8459262210355));
#20966=CARTESIAN_POINT('Ctrl Pts',(4.04358870192882,-1.11022302462516E-16,
11.8459262210355));
#20967=CARTESIAN_POINT('Ctrl Pts',(4.06252783272243,1.14575066216236E-15,
11.8270919444215));
#20968=CARTESIAN_POINT('Ctrl Pts',(4.0813004685107,1.13295521928305E-15,
11.8080909041462));
#20969=CARTESIAN_POINT('Ctrl Pts',(4.09999999999996,1.22124532708767E-15,
11.7890187209237));
#20970=CARTESIAN_POINT('Ctrl Pts',(4.15712386170585,0.08,11.8450264384616));
#20971=CARTESIAN_POINT('Ctrl Pts',(4.13827843210564,0.08,11.8642474273109));
#20972=CARTESIAN_POINT('Ctrl Pts',(4.11927627294067,0.08,11.8834820198546));
#20973=CARTESIAN_POINT('Ctrl Pts',(4.09999999999983,0.08,11.9026515720696));
#20974=CARTESIAN_POINT('Ctrl Pts',(-4.26119373042794,0.014552891884149,
11.638842338191));
#20975=CARTESIAN_POINT('Ctrl Pts',(-4.20740273136266,0.00476035687747917,
11.6883109569019));
#20976=CARTESIAN_POINT('Ctrl Pts',(-4.15394513638752,2.66182811039857E-16,
11.7388892266742));
#20977=CARTESIAN_POINT('Ctrl Pts',(-4.1,0.,11.7890187209227));
#20978=CARTESIAN_POINT('Ctrl Pts',(-4.27643939137202,0.017328331476068,
11.6544471019321));
#20979=CARTESIAN_POINT('Ctrl Pts',(-4.2234768418442,0.00670578391947384,
11.7041521797741));
#20980=CARTESIAN_POINT('Ctrl Pts',(-4.17069133240935,0.00105575681647751,
11.7550626804798));
#20981=CARTESIAN_POINT('Ctrl Pts',(-4.1170914194552,0.,11.8057761908238));
#20982=CARTESIAN_POINT('Ctrl Pts',(-4.29989809966375,0.0386834060206609,
11.6815396961087));
#20983=CARTESIAN_POINT('Ctrl Pts',(-4.24916885028947,0.0278752704198574,
11.7316116548977));
#20984=CARTESIAN_POINT('Ctrl Pts',(-4.19848690136659,0.0217313873072571,
11.7831192542213));
#20985=CARTESIAN_POINT('Ctrl Pts',(-4.14667038594628,0.0201034417498351,
11.8347772133533));
#20986=CARTESIAN_POINT('Ctrl Pts',(-4.3051722926355,0.0768991460759326,
11.6936574822235));
#20987=CARTESIAN_POINT('Ctrl Pts',(-4.25617484947063,0.0674142792550516,
11.7430966000368));
#20988=CARTESIAN_POINT('Ctrl Pts',(-4.20717768002144,0.0625329395532443,
11.7939625167387));
#20989=CARTESIAN_POINT('Ctrl Pts',(-4.15712386170579,0.0620480419794868,
11.8450264384607));
#20990=CARTESIAN_POINT('Ctrl Pts',(-4.3036970099402,0.0932593014944473,
11.695146582961));
#20991=CARTESIAN_POINT('Ctrl Pts',(-4.25517797344347,0.0843372140439259,
11.7441200666597));
#20992=CARTESIAN_POINT('Ctrl Pts',(-4.20665735473779,0.0800000000000001,
11.7945058221931));
#20993=CARTESIAN_POINT('Ctrl Pts',(-4.15712386170579,0.0799999999999999,
11.8450264384607));
#20994=CARTESIAN_POINT('Origin',(-4.1,0.0799999999999999,11.7890187209227));
#20995=CARTESIAN_POINT('Ctrl Pts',(-4.0999999999998,0.08,11.9026515720685));
#20996=CARTESIAN_POINT('Ctrl Pts',(-4.11927627294061,0.08,11.8834820198536));
#20997=CARTESIAN_POINT('Ctrl Pts',(-4.13827843210557,0.08,11.8642474273099));
#20998=CARTESIAN_POINT('Ctrl Pts',(-4.15712386170576,0.08,11.8450264384607));
#20999=CARTESIAN_POINT('Ctrl Pts',(-4.0999999999998,0.0560640559726492,
11.9026515720685));
#21000=CARTESIAN_POINT('Ctrl Pts',(-4.11927735039396,0.0560640559726493,
11.8834809483654));
#21001=CARTESIAN_POINT('Ctrl Pts',(-4.13827796583812,0.0560640559726492,
11.8642479028694));
#21002=CARTESIAN_POINT('Ctrl Pts',(-4.15712386170576,0.0560640559726492,
11.8450264384607));
#21003=CARTESIAN_POINT('Ctrl Pts',(-4.08582423632784,0.0146397293927034,
11.8883968890889));
#21004=CARTESIAN_POINT('Ctrl Pts',(-4.10501553004285,0.0146397293927039,
11.8693118456227));
#21005=CARTESIAN_POINT('Ctrl Pts',(-4.12396038090971,0.0146397293927035,
11.8501355730135));
#21006=CARTESIAN_POINT('Ctrl Pts',(-4.14276903578857,0.0146397293927034,
11.830952091747));
#21007=CARTESIAN_POINT('Ctrl Pts',(-4.05624736761451,1.39140256632356E-16,
11.8586553600401));
#21008=CARTESIAN_POINT('Ctrl Pts',(-4.07526199817246,1.14622689682545E-15,
11.839746001657));
#21009=CARTESIAN_POINT('Ctrl Pts',(-4.0940863606134,5.30685220103077E-16,
11.8206923301701));
#21010=CARTESIAN_POINT('Ctrl Pts',(-4.11281856459137,3.64434135141482E-16,
11.8015868233486));
#21011=CARTESIAN_POINT('Ctrl Pts',(-4.04358870192886,2.77555756156289E-16,
11.8459262210343));
#21012=CARTESIAN_POINT('Ctrl Pts',(-4.06252783272245,1.56490939312256E-15,
11.8270919444204));
#21013=CARTESIAN_POINT('Ctrl Pts',(-4.08130046851071,8.50913911948276E-16,
11.8080909041452));
#21014=CARTESIAN_POINT('Ctrl Pts',(-4.09999999999997,6.38378239159465E-16,
11.7890187209227));
#21015=CARTESIAN_POINT('Ctrl Pts',(-4.09999999999997,6.38378239159465E-16,
11.7890187209227));
#21016=CARTESIAN_POINT('Ctrl Pts',(-4.08130046851071,8.50913911948276E-16,
11.8080909041452));
#21017=CARTESIAN_POINT('Ctrl Pts',(-4.06252783272245,1.56490939312256E-15,
11.8270919444204));
#21018=CARTESIAN_POINT('Ctrl Pts',(-4.04358870192886,2.77555756156289E-16,
11.8459262210343));
#21019=CARTESIAN_POINT('Origin',(4.1,0.9,6.5));
#21020=CARTESIAN_POINT('',(4.10000000000037,6.53231808922516E-18,3.51568653184868));
#21021=CARTESIAN_POINT('',(4.1,0.,-0.5));
#21022=CARTESIAN_POINT('Ctrl Pts',(4.33293714059217,0.0306667563398109,
3.61523506307459));
#21023=CARTESIAN_POINT('Ctrl Pts',(4.31105117291262,0.0248024289745047,
3.63206334799651));
#21024=CARTESIAN_POINT('Ctrl Pts',(4.25303821911669,0.0114738356156513,
3.65326412679659));
#21025=CARTESIAN_POINT('Ctrl Pts',(4.15558369197843,0.000126613028484238,
3.61126292396189));
#21026=CARTESIAN_POINT('Ctrl Pts',(4.11687019564162,1.39427594163973E-14,
3.55256131194227));
#21027=CARTESIAN_POINT('Ctrl Pts',(4.10000000000067,1.11022302462516E-15,
3.51568653184854));
#21028=CARTESIAN_POINT('Origin',(0.,0.,6.75052439809906));
#21029=CARTESIAN_POINT('',(4.02,0.,1.28));
#21030=CARTESIAN_POINT('',(2.05,0.,1.28));
#21031=CARTESIAN_POINT('',(4.02,0.,3.08202325217412));
#21032=CARTESIAN_POINT('',(4.02,0.,9.32658798508426));
#21033=CARTESIAN_POINT('',(4.0212525797096,0.,3.10200465730851));
#21034=CARTESIAN_POINT('Origin',(4.18005218222794,-2.82131847876398E-16,
3.08201998101282));
#21035=CARTESIAN_POINT('',(4.08065440441665,0.,3.45401819866313));
#21036=CARTESIAN_POINT('Ctrl Pts',(4.08065440441665,-1.66533453693773E-16,
3.45401819866313));
#21037=CARTESIAN_POINT('Ctrl Pts',(4.0550039783989,-1.5992419952717E-16,
3.33776776889323));
#21038=CARTESIAN_POINT('Ctrl Pts',(4.03612145990415,4.46335323570744E-16,
3.22013430623041));
#21039=CARTESIAN_POINT('Ctrl Pts',(4.02125257970961,4.44089209850063E-16,
3.10200465730851));
#21040=CARTESIAN_POINT('Origin',(4.41014376905476,-1.89597157664411E-14,
3.2836903911759));
#21041=CARTESIAN_POINT('',(-4.1,-3.46944695195361E-18,1.26933116532693));
#21042=CARTESIAN_POINT('',(-4.1,0.,-0.5));
#21043=CARTESIAN_POINT('',(-4.05989131075898,5.20211316432632E-18,1.20000798754555));
#21044=CARTESIAN_POINT('Ctrl Pts',(-4.05990512546201,5.20005590072221E-18,
1.20001597509111));
#21045=CARTESIAN_POINT('Ctrl Pts',(-4.07021467126473,5.64716117898825E-18,
1.20597960426501));
#21046=CARTESIAN_POINT('Ctrl Pts',(-4.09130896359301,6.56198028176264E-18,
1.22537277009846));
#21047=CARTESIAN_POINT('Ctrl Pts',(-4.1,6.93889390390737E-18,1.25328382445493));
#21048=CARTESIAN_POINT('Ctrl Pts',(-4.1,6.93889390390723E-18,1.26933116532693));
#21049=CARTESIAN_POINT('',(-4.5,0.,1.2));
#21050=CARTESIAN_POINT('',(-3.3,0.,10.7));
#21051=CARTESIAN_POINT('Origin',(-3.,0.,10.7));
#21052=CARTESIAN_POINT('',(2.64,0.,11.7));
#21053=CARTESIAN_POINT('Origin',(3.,0.,11.7));
#21054=CARTESIAN_POINT('',(-3.36,0.,11.7));
#21055=CARTESIAN_POINT('Origin',(-3.,0.,11.7));
#21056=CARTESIAN_POINT('',(2.7,0.,10.7));
#21057=CARTESIAN_POINT('Origin',(3.,0.,10.7));
#21058=CARTESIAN_POINT('Origin',(2.05,0.08,1.28));
#21059=CARTESIAN_POINT('',(4.02,0.08,1.2));
#21060=CARTESIAN_POINT('',(2.05,0.08,1.2));
#21061=CARTESIAN_POINT('Origin',(4.02,0.08,1.28));
#21062=CARTESIAN_POINT('Origin',(4.02,0.,1.28));
#21063=CARTESIAN_POINT('',(4.1,0.08,1.28));
#21064=CARTESIAN_POINT('Origin',(4.02,0.08,1.28));
#21065=CARTESIAN_POINT('',(4.02,0.42,1.2));
#21066=CARTESIAN_POINT('',(4.02,0.,1.2));
#21067=CARTESIAN_POINT('',(4.1,0.42,1.28));
#21068=CARTESIAN_POINT('Origin',(4.02,0.42,1.28));
#21069=CARTESIAN_POINT('',(4.1,0.,1.28));
#21070=CARTESIAN_POINT('Origin',(2.05,0.42,1.28));
#21071=CARTESIAN_POINT('',(4.02,0.5,1.28));
#21072=CARTESIAN_POINT('',(2.05,0.5,1.28));
#21073=CARTESIAN_POINT('Origin',(4.02,0.42,1.28));
#21074=CARTESIAN_POINT('',(2.05,0.42,1.2));
#21075=CARTESIAN_POINT('Origin',(4.02,0.42,1.28));
#21076=CARTESIAN_POINT('Origin',(4.02,0.42,1.28));
#21077=CARTESIAN_POINT('Origin',(4.02,0.08,1.28));
#21078=CARTESIAN_POINT('Origin',(4.02,0.08,1.28));
#21079=CARTESIAN_POINT('Origin',(4.02,0.08,9.32658798508426));
#21080=CARTESIAN_POINT('',(4.1,0.08,3.08202325217433));
#21081=CARTESIAN_POINT('',(4.1,0.08,9.32658798508426));
#21082=CARTESIAN_POINT('Origin',(4.02,0.08,3.08202325217412));
#21083=CARTESIAN_POINT('Origin',(4.1,0.,11.9026515720695));
#21084=CARTESIAN_POINT('',(4.09999995360518,0.420060922767902,2.91110490125779));
#21085=CARTESIAN_POINT('',(4.1,0.42,9.32658798508426));
#21086=CARTESIAN_POINT('',(4.10001562649967,0.307717888808026,3.08199713129763));
#21087=CARTESIAN_POINT('Ctrl Pts',(4.1,0.420108484733097,2.91112675763541));
#21088=CARTESIAN_POINT('Ctrl Pts',(4.1,0.403846880854867,2.94612344156548));
#21089=CARTESIAN_POINT('Ctrl Pts',(4.10000000001308,0.38486882493947,2.98262906973082));
#21090=CARTESIAN_POINT('Ctrl Pts',(4.10000000001308,0.354969676766091,3.02928232732464));
#21091=CARTESIAN_POINT('Ctrl Pts',(4.09999999999961,0.344338937185448,3.04446410228447));
#21092=CARTESIAN_POINT('Ctrl Pts',(4.09999999999961,0.327298117371871,3.06460863705819));
#21093=CARTESIAN_POINT('Ctrl Pts',(4.1,0.317366554193231,3.07555920769984));
#21094=CARTESIAN_POINT('Ctrl Pts',(4.1,0.307684300216189,3.08193081722902));
#21095=CARTESIAN_POINT('',(4.1,0.08,3.08202325217412));
#21096=CARTESIAN_POINT('Origin',(4.02,0.42,9.32658798508426));
#21097=CARTESIAN_POINT('',(4.02,0.5,9.32658798508426));
#21098=CARTESIAN_POINT('Ctrl Pts',(4.08072994232021,0.472075657516576,2.72825956479583));
#21099=CARTESIAN_POINT('Ctrl Pts',(4.08122454955537,0.471498853107479,2.73157912921552));
#21100=CARTESIAN_POINT('Ctrl Pts',(4.0817174163307,0.470907450992412,2.73489656248772));
#21101=CARTESIAN_POINT('Ctrl Pts',(4.08632402965424,0.465210421595644,2.76604215816752));
#21102=CARTESIAN_POINT('Ctrl Pts',(4.090310411307,0.459013812808448,2.79397090075911));
#21103=CARTESIAN_POINT('Ctrl Pts',(4.09495793357299,0.448192539461495,2.83357438640932));
#21104=CARTESIAN_POINT('Ctrl Pts',(4.09626884293072,0.444498335917193,2.84600777143549));
#21105=CARTESIAN_POINT('Ctrl Pts',(4.09809490830362,0.43761039207076,2.86702885206655));
#21106=CARTESIAN_POINT('Ctrl Pts',(4.09874538136808,0.434501757347987,2.87590964228465));
#21107=CARTESIAN_POINT('Ctrl Pts',(4.09945899238873,0.429453602695266,2.88918275571946));
#21108=CARTESIAN_POINT('Ctrl Pts',(4.09965766008674,0.427632208943707,2.89377446083871));
#21109=CARTESIAN_POINT('Ctrl Pts',(4.09992238135085,0.423953166512825,2.9025897644674));
#21110=CARTESIAN_POINT('Ctrl Pts',(4.09999693148384,0.422075613013451,2.90688508225406));
#21111=CARTESIAN_POINT('Ctrl Pts',(4.09999990721035,0.420121845535804,2.91109776321207));
#21112=CARTESIAN_POINT('Origin',(0.,0.5,6.75052439809906));
#21113=CARTESIAN_POINT('',(-2.87936339380758,0.5,1.05441190629352));
#21114=CARTESIAN_POINT('',(-2.88715652190429,0.5,0.898556263634797));
#21115=CARTESIAN_POINT('Ctrl Pts',(-2.87936339380758,0.5,1.05441190629352));
#21116=CARTESIAN_POINT('Ctrl Pts',(-2.88225640305787,0.5,1.00074289678204));
#21117=CARTESIAN_POINT('Ctrl Pts',(-2.88479548403111,0.5,0.94877882392077));
#21118=CARTESIAN_POINT('Ctrl Pts',(-2.88715652190429,0.5,0.898556263634797));
#21119=CARTESIAN_POINT('',(-2.89976430745756,0.500020637206737,1.05079292247917));
#21120=CARTESIAN_POINT('Ctrl Pts',(-2.88715652190429,0.5,0.898556263634783));
#21121=CARTESIAN_POINT('Ctrl Pts',(-2.88603713588444,0.5,0.924909290748928));
#21122=CARTESIAN_POINT('Ctrl Pts',(-2.886491373252,0.499999999978573,0.951912747979301));
#21123=CARTESIAN_POINT('Ctrl Pts',(-2.89056682713583,0.499999999978573,
1.00214907554527));
#21124=CARTESIAN_POINT('Ctrl Pts',(-2.89410001522392,0.5,1.02750911559584));
#21125=CARTESIAN_POINT('Ctrl Pts',(-2.89983611779302,0.5,1.05077445318157));
#21126=CARTESIAN_POINT('',(-2.94907641594456,0.5,1.2));
#21127=CARTESIAN_POINT('Ctrl Pts',(-2.89974754967704,0.5,1.05079644977824));
#21128=CARTESIAN_POINT('Ctrl Pts',(-2.90603688042105,0.5,1.0759238598806));
#21129=CARTESIAN_POINT('Ctrl Pts',(-2.91415049349688,0.499999999999601,
1.10134719163055));
#21130=CARTESIAN_POINT('Ctrl Pts',(-2.93088651158465,0.499999999999601,
1.15007567318975));
#21131=CARTESIAN_POINT('Ctrl Pts',(-2.93983934236369,0.5,1.17435149002438));
#21132=CARTESIAN_POINT('Ctrl Pts',(-2.94896009810987,0.5,1.19967694937972));
#21133=CARTESIAN_POINT('Ctrl Pts',(-2.94901825916661,0.499999999999999,
1.19983846830976));
#21134=CARTESIAN_POINT('Ctrl Pts',(-2.94907641594456,0.499999999999999,
1.2));
#21135=CARTESIAN_POINT('',(-3.91996273602064,0.5,1.19999999999642));
#21136=CARTESIAN_POINT('',(-4.5,0.5,1.2));
#21137=CARTESIAN_POINT('',(-3.9565294294013,0.499872084413071,1.10578825936713));
#21138=CARTESIAN_POINT('Ctrl Pts',(-3.95639036913989,0.5,1.10574453980859));
#21139=CARTESIAN_POINT('Ctrl Pts',(-3.95076346391642,0.5,1.12156459291084));
#21140=CARTESIAN_POINT('Ctrl Pts',(-3.94468196650963,0.5,1.13750333307378));
#21141=CARTESIAN_POINT('Ctrl Pts',(-3.93253478628767,0.5,1.16853559910449));
#21142=CARTESIAN_POINT('Ctrl Pts',(-3.92630639980323,0.5,1.18405004798573));
#21143=CARTESIAN_POINT('Ctrl Pts',(-3.92009288044491,0.5,1.19967272770361));
#21144=CARTESIAN_POINT('Ctrl Pts',(-3.92002780536768,0.5,1.19983636257788));
#21145=CARTESIAN_POINT('Ctrl Pts',(-3.91996273602209,0.5,1.199999999997));
#21146=CARTESIAN_POINT('',(-4.05976551316264,0.500000001208332,1.2));
#21147=CARTESIAN_POINT('Ctrl Pts',(-4.05976550743572,0.5,1.2));
#21148=CARTESIAN_POINT('Ctrl Pts',(-4.04742877842025,0.5,1.19999809186902));
#21149=CARTESIAN_POINT('Ctrl Pts',(-4.035091497052,0.5,1.19762022778872));
#21150=CARTESIAN_POINT('Ctrl Pts',(-4.007915635338,0.5,1.18794866440528));
#21151=CARTESIAN_POINT('Ctrl Pts',(-3.99341012555002,0.500000000024842,
1.1792057307165));
#21152=CARTESIAN_POINT('Ctrl Pts',(-3.97352459100036,0.500000000024842,
1.1611448793698));
#21153=CARTESIAN_POINT('Ctrl Pts',(-3.96617262558927,0.5,1.15272746382386));
#21154=CARTESIAN_POINT('Ctrl Pts',(-3.95707696368493,0.5,1.13661229032071));
#21155=CARTESIAN_POINT('Ctrl Pts',(-3.95543177553355,0.5,1.13081595575233));
#21156=CARTESIAN_POINT('Ctrl Pts',(-3.95416491149362,0.5,1.12308915103081));
#21157=CARTESIAN_POINT('Ctrl Pts',(-3.9540319481804,0.5,1.11975105593971));
#21158=CARTESIAN_POINT('Ctrl Pts',(-3.95465641496988,0.5,1.11277077485612));
#21159=CARTESIAN_POINT('Ctrl Pts',(-3.95546639835865,0.5,1.10925940502722));
#21160=CARTESIAN_POINT('Ctrl Pts',(-3.95666399897708,0.5,1.10584429672409));
#21161=CARTESIAN_POINT('',(-4.05989131075939,0.499999999999496,1.20000798754579));
#21162=CARTESIAN_POINT('',(-4.5,0.5,1.2));
#21163=CARTESIAN_POINT('',(-4.1,0.5,1.26933116532693));
#21164=CARTESIAN_POINT('Ctrl Pts',(-4.1,0.5,1.26933116532693));
#21165=CARTESIAN_POINT('Ctrl Pts',(-4.1,0.5,1.25328382445493));
#21166=CARTESIAN_POINT('Ctrl Pts',(-4.09130896359301,0.5,1.22537277009847));
#21167=CARTESIAN_POINT('Ctrl Pts',(-4.07021467126473,0.5,1.20597960426501));
#21168=CARTESIAN_POINT('Ctrl Pts',(-4.05990512546201,0.5,1.20001597509111));
#21169=CARTESIAN_POINT('',(-4.1,0.5,-0.5));
#21170=CARTESIAN_POINT('',(-4.1,0.5,-0.5));
#21171=CARTESIAN_POINT('',(4.1,0.5,11.7890187209237));
#21172=CARTESIAN_POINT('Ctrl Pts',(4.09999999999996,0.499999999999999,11.7890187209237));
#21173=CARTESIAN_POINT('Ctrl Pts',(4.08130046851069,0.499999999999999,11.8080909041462));
#21174=CARTESIAN_POINT('Ctrl Pts',(4.06252783272241,0.5,11.8270919444215));
#21175=CARTESIAN_POINT('Ctrl Pts',(4.0435887019288,0.500000000000001,11.8459262210355));
#21176=CARTESIAN_POINT('',(4.1,0.5,-0.5));
#21177=CARTESIAN_POINT('',(-4.5,0.5,1.2));
#21178=CARTESIAN_POINT('',(-2.803641505311,0.5,1.2));
#21179=CARTESIAN_POINT('',(-4.5,0.5,1.2));
#21180=CARTESIAN_POINT('Ctrl Pts',(-2.803641505311,0.5,1.2));
#21181=CARTESIAN_POINT('Ctrl Pts',(-2.82677300877682,0.5,1.2));
#21182=CARTESIAN_POINT('Ctrl Pts',(-2.86687236848074,0.5,1.18130984727687));
#21183=CARTESIAN_POINT('Ctrl Pts',(-2.88261462067416,0.5,1.14154581001999));
#21184=CARTESIAN_POINT('Ctrl Pts',(-2.88353005387198,0.5,1.12422135153951));
#21185=CARTESIAN_POINT('Ctrl Pts',(-2.8852657140673,0.5,1.09088035845137));
#21186=CARTESIAN_POINT('Ctrl Pts',(-2.88558432089061,0.5,1.0846730825913));
#21187=CARTESIAN_POINT('Ctrl Pts',(-2.88523738147895,0.500000000000113,
1.07842688666836));
#21188=CARTESIAN_POINT('Ctrl Pts',(-2.88325561528678,0.500000000000113,
1.06618259874669));
#21189=CARTESIAN_POINT('Ctrl Pts',(-2.88162442549406,0.5,1.0601716794206));
#21190=CARTESIAN_POINT('Ctrl Pts',(-2.87936339380758,0.5,1.05441190629352));
#21191=CARTESIAN_POINT('',(2.7,0.5,10.7));
#21192=CARTESIAN_POINT('Origin',(3.,0.5,10.7));
#21193=CARTESIAN_POINT('',(-3.36,0.5,11.7));
#21194=CARTESIAN_POINT('Origin',(-3.,0.5,11.7));
#21195=CARTESIAN_POINT('',(2.64,0.5,11.7));
#21196=CARTESIAN_POINT('Origin',(3.,0.5,11.7));
#21197=CARTESIAN_POINT('',(-3.3,0.5,10.7));
#21198=CARTESIAN_POINT('Origin',(-3.,0.5,10.7));
#21199=CARTESIAN_POINT('Ctrl Pts',(4.1,0.08,3.08202325217412));
#21200=CARTESIAN_POINT('Ctrl Pts',(4.1,0.08,3.08536220394432));
#21201=CARTESIAN_POINT('Ctrl Pts',(4.10020930892952,0.08,3.08870114236636));
#21202=CARTESIAN_POINT('Ctrl Pts',(4.1006262898548,0.08,3.09201395474132));
#21203=CARTESIAN_POINT('Ctrl Pts',(4.1,0.0560640559726492,3.08202325217412));
#21204=CARTESIAN_POINT('Ctrl Pts',(4.1,0.0560640559726492,3.08535153317887));
#21205=CARTESIAN_POINT('Ctrl Pts',(4.10021064153507,0.0560640559726493,
3.0887117295944));
#21206=CARTESIAN_POINT('Ctrl Pts',(4.1006262898548,0.0560640559726493,3.09201395474132));
#21207=CARTESIAN_POINT('Ctrl Pts',(4.07990169691163,0.0146335669363464,
3.08202325217412));
#21208=CARTESIAN_POINT('Ctrl Pts',(4.07990169691163,0.0146335669363464,
3.08620381196858));
#21209=CARTESIAN_POINT('Ctrl Pts',(4.08016324468958,0.0146335669363467,
3.09037607507745));
#21210=CARTESIAN_POINT('Ctrl Pts',(4.08068532880797,0.0146335669363467,
3.09452390684458));
#21211=CARTESIAN_POINT('Ctrl Pts',(4.03795195802051,-4.05341230270309E-17,
3.08202325217412));
#21212=CARTESIAN_POINT('Ctrl Pts',(4.03795195802051,-4.05341230270405E-17,
3.08795342935058));
#21213=CARTESIAN_POINT('Ctrl Pts',(4.03832341566108,4.19890745630692E-16,
3.09387899684106));
#21214=CARTESIAN_POINT('Ctrl Pts',(4.03906399861534,4.17432874630846E-16,
3.09976274889499));
#21215=CARTESIAN_POINT('Ctrl Pts',(4.02,-4.16333634234434E-17,3.08202325217412));
#21216=CARTESIAN_POINT('Ctrl Pts',(4.02,-4.16333634234529E-17,3.08870115571451));
#21217=CARTESIAN_POINT('Ctrl Pts',(4.02041861785905,4.18789509235301E-16,
3.0953790325586));
#21218=CARTESIAN_POINT('Ctrl Pts',(4.0212525797096,4.16333634234434E-16,
3.10200465730851));
#21219=CARTESIAN_POINT('',(4.10062628985479,0.08,3.09201395474128));
#21220=CARTESIAN_POINT('Origin',(4.0212525797096,0.08,3.10200465730851));
#21221=CARTESIAN_POINT('Origin',(4.18002609111314,0.08,3.08202161659353));
#21222=CARTESIAN_POINT('Ctrl Pts',(4.1006262898548,0.08,3.09201395474132));
#21223=CARTESIAN_POINT('Ctrl Pts',(4.11526689217912,0.08,3.20832999131892));
#21224=CARTESIAN_POINT('Ctrl Pts',(4.13379447775995,0.08,3.32356514996729));
#21225=CARTESIAN_POINT('Ctrl Pts',(4.15877532388868,0.08,3.43678097322386));
#21226=CARTESIAN_POINT('Ctrl Pts',(4.1006262898548,0.0560640559726493,3.09201395474132));
#21227=CARTESIAN_POINT('Ctrl Pts',(4.1152661626389,0.0560640559726493,3.20832419529872));
#21228=CARTESIAN_POINT('Ctrl Pts',(4.13379661763211,0.0560640559726492,
3.32357484809309));
#21229=CARTESIAN_POINT('Ctrl Pts',(4.15877532388868,0.0560640559726492,
3.43678097322386));
#21230=CARTESIAN_POINT('Ctrl Pts',(4.08068487271943,0.0146341184962319,
3.09452396425207));
#21231=CARTESIAN_POINT('Ctrl Pts',(4.09538301420591,0.0146341184962319,
3.2112971355255));
#21232=CARTESIAN_POINT('Ctrl Pts',(4.11399903223575,0.0146341184962314,
3.32713084077746));
#21233=CARTESIAN_POINT('Ctrl Pts',(4.13914865103515,0.0146341184962313,
3.44111155953654));
#21234=CARTESIAN_POINT('Ctrl Pts',(4.03906399861534,4.45188450246475E-16,
3.09976274889499));
#21235=CARTESIAN_POINT('Ctrl Pts',(4.05388175816077,4.47436389483802E-16,
3.2174862566513));
#21236=CARTESIAN_POINT('Ctrl Pts',(4.07268421775703,-1.58819587495572E-16,
3.33457931569976));
#21237=CARTESIAN_POINT('Ctrl Pts',(4.09818469775272,-1.65434213297361E-16,
3.45015017431968));
#21238=CARTESIAN_POINT('Ctrl Pts',(4.02125257970961,4.44089209850063E-16,
3.10200465730851));
#21239=CARTESIAN_POINT('Ctrl Pts',(4.03612145990415,4.46335323570744E-16,
3.22013430623041));
#21240=CARTESIAN_POINT('Ctrl Pts',(4.0550039783989,-1.5992419952717E-16,
3.33776776889323));
#21241=CARTESIAN_POINT('Ctrl Pts',(4.08065440441665,-1.66533453693773E-16,
3.45401819866313));
#21242=CARTESIAN_POINT('',(4.15877532388652,0.0799994042033401,3.43678097322434));
#21243=CARTESIAN_POINT('Origin',(4.08065440441665,0.08,3.45401819866313));
#21244=CARTESIAN_POINT('Ctrl Pts',(4.1006262898548,0.08,3.09201395474132));
#21245=CARTESIAN_POINT('Ctrl Pts',(4.11526645524359,0.08,3.20832651997201));
#21246=CARTESIAN_POINT('Ctrl Pts',(4.13379337188534,0.08,3.32355827178816));
#21247=CARTESIAN_POINT('Ctrl Pts',(4.15877308731365,0.08,3.43677083674693));
#21248=CARTESIAN_POINT('Ctrl Pts',(4.17250638811433,0.0648543434789084,
3.48546348151857));
#21249=CARTESIAN_POINT('Ctrl Pts',(4.18266052260979,0.0556405700559915,
3.51444097567126));
#21250=CARTESIAN_POINT('Ctrl Pts',(4.20433589890911,0.0406236453241535,
3.56000713380897));
#21251=CARTESIAN_POINT('Ctrl Pts',(4.25199456808014,0.0336163065688034,
3.59330578207307));
#21252=CARTESIAN_POINT('Ctrl Pts',(4.27729012420774,0.0439150199095526,
3.57845771566606));
#21253=CARTESIAN_POINT('Ctrl Pts',(4.28625335961854,0.0503448666167723,
3.56616535738233));
#21254=CARTESIAN_POINT('Ctrl Pts',(4.16929027892073,0.0467828333657603,
3.48680406174265));
#21255=CARTESIAN_POINT('Ctrl Pts',(4.17796988891339,0.0397461385215758,
3.51697746443788));
#21256=CARTESIAN_POINT('Ctrl Pts',(4.1988611271974,0.0290109791845337,3.56548110876311));
#21257=CARTESIAN_POINT('Ctrl Pts',(4.25263440860521,0.0269453546316361,
3.60149225779319));
#21258=CARTESIAN_POINT('Ctrl Pts',(4.28279509833513,0.036739599270244,3.58519594631708));
#21259=CARTESIAN_POINT('Ctrl Pts',(4.29328883703346,0.0422568691806583,
3.57193401843471));
#21260=CARTESIAN_POINT('Ctrl Pts',(4.15087621691878,0.013238281675356,3.49447964919285));
#21261=CARTESIAN_POINT('Ctrl Pts',(4.16005024766761,0.0114887305890716,
3.52731328970503));
#21262=CARTESIAN_POINT('Ctrl Pts',(4.1844192175266,0.00938090938160887,
3.58082600653567));
#21263=CARTESIAN_POINT('Ctrl Pts',(4.25361565342529,0.0161067146530447,
3.62047517370959));
#21264=CARTESIAN_POINT('Ctrl Pts',(4.29453368233821,0.0258216733838189,
3.60185180708036));
#21265=CARTESIAN_POINT('Ctrl Pts',(4.30919086234588,0.0301620716842713,
3.58693685155031));
#21266=CARTESIAN_POINT('Ctrl Pts',(4.11698762514124,1.35575488646911E-14,
3.50860553025727));
#21267=CARTESIAN_POINT('Ctrl Pts',(4.1313452462753,0.000358144080936645,
3.54413845042102));
#21268=CARTESIAN_POINT('Ctrl Pts',(4.16538066436182,0.00107821606618538,
3.60111646091567));
#21269=CARTESIAN_POINT('Ctrl Pts',(4.25343337329451,0.0118887454562876,
3.64233796301702));
#21270=CARTESIAN_POINT('Ctrl Pts',(4.30590173066008,0.0236297726512944,
3.62199161527088));
#21271=CARTESIAN_POINT('Ctrl Pts',(4.325507636067,0.0286760266021307,3.6057994627788));
#21272=CARTESIAN_POINT('Ctrl Pts',(4.10000000000067,1.11022302462516E-15,
3.51568653184854));
#21273=CARTESIAN_POINT('Ctrl Pts',(4.11687019564162,1.39427594163973E-14,
3.55256131194227));
#21274=CARTESIAN_POINT('Ctrl Pts',(4.15558369197843,0.000126613028484238,
3.61126292396189));
#21275=CARTESIAN_POINT('Ctrl Pts',(4.25303821911669,0.0114738356156513,
3.65326412679659));
#21276=CARTESIAN_POINT('Ctrl Pts',(4.31105117291262,0.0248024289745047,
3.63206334799651));
#21277=CARTESIAN_POINT('Ctrl Pts',(4.33293714059217,0.0306667563398109,
3.61523506307459));
#21278=CARTESIAN_POINT('',(4.17250638811433,0.0648543434789084,3.48546348151857));
#21279=CARTESIAN_POINT('Origin',(4.10000000000061,0.0800000000000007,3.51568653184854));
#21280=CARTESIAN_POINT('',(4.28625335961854,0.0503448666167723,3.56616535738233));
#21281=CARTESIAN_POINT('Ctrl Pts',(4.17250638811433,0.0648543434789084,
3.48546348151857));
#21282=CARTESIAN_POINT('Ctrl Pts',(4.18266052260979,0.0556405700559915,
3.51444097567126));
#21283=CARTESIAN_POINT('Ctrl Pts',(4.20433589890911,0.0406236453241535,
3.56000713380897));
#21284=CARTESIAN_POINT('Ctrl Pts',(4.25199456808014,0.0336163065688034,
3.59330578207307));
#21285=CARTESIAN_POINT('Ctrl Pts',(4.27729012420774,0.0439150199095526,
3.57845771566606));
#21286=CARTESIAN_POINT('Ctrl Pts',(4.28625335961854,0.0503448666167723,
3.56616535738233));
#21287=CARTESIAN_POINT('Origin',(4.31223161698397,0.107940822442937,3.6152350630746));
#21288=CARTESIAN_POINT('Ctrl Pts',(4.15877532388868,0.0800000000000003,
3.43678097322386));
#21289=CARTESIAN_POINT('Ctrl Pts',(4.16246506407796,0.0749031082315837,
3.45350326401334));
#21290=CARTESIAN_POINT('Ctrl Pts',(4.16702335990291,0.069829595641864,3.46981621803132));
#21291=CARTESIAN_POINT('Ctrl Pts',(4.17250638811433,0.064854343478907,3.48546348151857));
#21292=CARTESIAN_POINT('Ctrl Pts',(4.15877532388868,0.0560640559726496,
3.43678097322386));
#21293=CARTESIAN_POINT('Ctrl Pts',(4.16092731617209,0.0519427537625869,
3.45382800899325));
#21294=CARTESIAN_POINT('Ctrl Pts',(4.16431986899145,0.0479680589322419,
3.47067724603867));
#21295=CARTESIAN_POINT('Ctrl Pts',(4.16883083475021,0.0442011890638705,
3.48699557320324));
#21296=CARTESIAN_POINT('Ctrl Pts',(4.13914860105817,0.0146341799039232,
3.44111157056385));
#21297=CARTESIAN_POINT('Ctrl Pts',(4.14071345514682,0.0133927789551764,
3.45945075426926));
#21298=CARTESIAN_POINT('Ctrl Pts',(4.14379087487777,0.0122539493399985,
3.4777024640668));
#21299=CARTESIAN_POINT('Ctrl Pts',(4.14857154686496,0.0111913457409417,
3.49544031156815));
#21300=CARTESIAN_POINT('Ctrl Pts',(4.09818469775272,5.82845227735974E-16,
3.45015017431968));
#21301=CARTESIAN_POINT('Ctrl Pts',(4.10191329035582,1.31426440172898E-5,
3.47039859381559));
#21302=CARTESIAN_POINT('Ctrl Pts',(4.10731252271732,-7.72394405668259E-6,
3.49035786986458));
#21303=CARTESIAN_POINT('Ctrl Pts',(4.11456082154968,8.4635003401468E-17,
3.50961710191317));
#21304=CARTESIAN_POINT('Ctrl Pts',(4.08065440441665,5.82867087928207E-16,
3.45401819866313));
#21305=CARTESIAN_POINT('Ctrl Pts',(4.08530246872869,6.1214364716609E-16,
3.47508371521632));
#21306=CARTESIAN_POINT('Ctrl Pts',(4.0917001731762,2.63948896849449E-16,
3.49577489293594));
#21307=CARTESIAN_POINT('Ctrl Pts',(4.10000000000061,8.32667268468867E-17,
3.51568653184854));
#21308=CARTESIAN_POINT('Origin',(4.24802043123848,0.0859220706677168,3.38337978260087));
#21309=CARTESIAN_POINT('Ctrl Pts',(4.28625335961854,0.0503448666167712,
3.56616535738233));
#21310=CARTESIAN_POINT('Ctrl Pts',(4.28883173298406,0.0521944828250372,
3.56262932516341));
#21311=CARTESIAN_POINT('Ctrl Pts',(4.29121124271805,0.0540999851939356,
3.55876018527392));
#21312=CARTESIAN_POINT('Ctrl Pts',(4.29338985935164,0.0560360920070411,
3.55463300336248));
#21313=CARTESIAN_POINT('Ctrl Pts',(4.30032431444838,0.0341688717445422,
3.5777026794871));
#21314=CARTESIAN_POINT('Ctrl Pts',(4.30358042720995,0.0355310056620428,
3.57365818981285));
#21315=CARTESIAN_POINT('Ctrl Pts',(4.30657676601693,0.0369119378047956,
3.5692595980189));
#21316=CARTESIAN_POINT('Ctrl Pts',(4.30926534633513,0.0382206091540884,
3.56457879573332));
#21317=CARTESIAN_POINT('Ctrl Pts',(4.31807813154184,0.026685296864449,3.59636386248302));
#21318=CARTESIAN_POINT('Ctrl Pts',(4.32262354005804,0.02789161406842,3.59191453262352));
#21319=CARTESIAN_POINT('Ctrl Pts',(4.32687322788778,0.029057244381936,3.58706864094837));
#21320=CARTESIAN_POINT('Ctrl Pts',(4.33079072300035,0.0300916254794634,
3.58191136456955));
#21321=CARTESIAN_POINT('Ctrl Pts',(4.33293714059217,0.0306667563398117,
3.6152350630746));
#21322=CARTESIAN_POINT('Ctrl Pts',(4.33867325889683,0.0322037446072338,
3.61039422161037));
#21323=CARTESIAN_POINT('Ctrl Pts',(4.34406623569343,0.0336487883846835,
3.60510985574939));
#21324=CARTESIAN_POINT('Ctrl Pts',(4.34909964308337,0.0349974858299939,
3.59949138964762));
#21325=CARTESIAN_POINT('',(4.29338985926344,0.0560360920135354,3.55463300342316));
#21326=CARTESIAN_POINT('Origin',(4.32839411947511,0.112271551933105,3.59949138964768));
#21327=CARTESIAN_POINT('Origin',(4.23862664689032,0.0738535158890165,3.44885235882043));
#21328=CARTESIAN_POINT('Origin',(4.32839411947511,0.112271551933102,3.59949138964768));
#21329=CARTESIAN_POINT('Origin',(4.32839411947511,0.112271551933102,3.59949138964768));
#21330=CARTESIAN_POINT('Ctrl Pts',(4.1,0.,11.9026515720695));
#21331=CARTESIAN_POINT('Ctrl Pts',(4.1,0.8496,11.9026515720695));
#21332=CARTESIAN_POINT('Ctrl Pts',(4.11686402271798,0.,11.8858809149492));
#21333=CARTESIAN_POINT('Ctrl Pts',(4.11686402271798,0.8496,11.8858809149492));
#21334=CARTESIAN_POINT('Ctrl Pts',(4.15991130277621,0.,11.842517268502));
#21335=CARTESIAN_POINT('Ctrl Pts',(4.15991130277621,0.8496,11.842517268502));
#21336=CARTESIAN_POINT('Ctrl Pts',(4.22986670297865,0.,11.7703786717735));
#21337=CARTESIAN_POINT('Ctrl Pts',(4.22986670297865,0.8496,11.7703786717735));
#21338=CARTESIAN_POINT('Ctrl Pts',(4.32906075669879,0.,11.667756621275));
#21339=CARTESIAN_POINT('Ctrl Pts',(4.32906075669879,0.8496,11.667756621275));
#21340=CARTESIAN_POINT('Ctrl Pts',(4.46255574628753,0.,11.5373242211525));
#21341=CARTESIAN_POINT('Ctrl Pts',(4.46255574628753,0.8496,11.5373242211525));
#21342=CARTESIAN_POINT('Ctrl Pts',(4.61532593596939,0.,11.4029224160728));
#21343=CARTESIAN_POINT('Ctrl Pts',(4.61532593596939,0.8496,11.4029224160728));
#21344=CARTESIAN_POINT('Ctrl Pts',(4.77596612414944,0.,11.2768795166233));
#21345=CARTESIAN_POINT('Ctrl Pts',(4.77596612414944,0.8496,11.2768795166233));
#21346=CARTESIAN_POINT('Ctrl Pts',(4.94211773226968,0.,11.1598106424589));
#21347=CARTESIAN_POINT('Ctrl Pts',(4.94211773226968,0.8496,11.1598106424589));
#21348=CARTESIAN_POINT('Ctrl Pts',(5.11112998264613,0.,11.051370419133));
#21349=CARTESIAN_POINT('Ctrl Pts',(5.11112998264613,0.8496,11.051370419133));
#21350=CARTESIAN_POINT('Ctrl Pts',(5.28082876351925,0.,10.9511663773825));
#21351=CARTESIAN_POINT('Ctrl Pts',(5.28082876351925,0.8496,10.9511663773825));
#21352=CARTESIAN_POINT('Ctrl Pts',(5.45051506148977,0.,10.8599381259735));
#21353=CARTESIAN_POINT('Ctrl Pts',(5.45051506148977,0.8496,10.8599381259735));
#21354=CARTESIAN_POINT('Ctrl Pts',(5.62101499943423,0.,10.7795199127532));
#21355=CARTESIAN_POINT('Ctrl Pts',(5.62101499943423,0.8496,10.7795199127532));
#21356=CARTESIAN_POINT('Ctrl Pts',(5.7936769541502,0.,10.7114411549111));
#21357=CARTESIAN_POINT('Ctrl Pts',(5.7936769541502,0.8496,10.7114411549111));
#21358=CARTESIAN_POINT('Ctrl Pts',(5.96961932707136,0.,10.6558377434042));
#21359=CARTESIAN_POINT('Ctrl Pts',(5.96961932707136,0.8496,10.6558377434042));
#21360=CARTESIAN_POINT('Ctrl Pts',(6.14893768388704,0.,10.6103475969888));
#21361=CARTESIAN_POINT('Ctrl Pts',(6.14893768388704,0.8496,10.6103475969888));
#21362=CARTESIAN_POINT('Ctrl Pts',(6.32976796473819,0.,10.5687216653907));
#21363=CARTESIAN_POINT('Ctrl Pts',(6.32976796473819,0.8496,10.5687216653907));
#21364=CARTESIAN_POINT('Ctrl Pts',(6.50892555577775,0.,10.5222908830264));
#21365=CARTESIAN_POINT('Ctrl Pts',(6.50892555577775,0.8496,10.5222908830264));
#21366=CARTESIAN_POINT('Ctrl Pts',(6.68288828293941,0.,10.462050267878));
#21367=CARTESIAN_POINT('Ctrl Pts',(6.68288828293941,0.8496,10.462050267878));
#21368=CARTESIAN_POINT('Ctrl Pts',(6.84859008776107,0.,10.3804015453596));
#21369=CARTESIAN_POINT('Ctrl Pts',(6.84859008776107,0.8496,10.3804015453596));
#21370=CARTESIAN_POINT('Ctrl Pts',(7.00445448641038,0.,10.2733319413005));
#21371=CARTESIAN_POINT('Ctrl Pts',(7.00445448641038,0.8496,10.2733319413005));
#21372=CARTESIAN_POINT('Ctrl Pts',(7.15081550722288,0.,10.1414720974144));
#21373=CARTESIAN_POINT('Ctrl Pts',(7.15081550722288,0.8496,10.1414720974144));
#21374=CARTESIAN_POINT('Ctrl Pts',(7.28883796912684,0.,9.98835756998534));
#21375=CARTESIAN_POINT('Ctrl Pts',(7.28883796912684,0.8496,9.98835756998534));
#21376=CARTESIAN_POINT('Ctrl Pts',(7.41967047354988,0.,9.81917361987377));
#21377=CARTESIAN_POINT('Ctrl Pts',(7.41967047354988,0.8496,9.81917361987377));
#21378=CARTESIAN_POINT('Ctrl Pts',(7.54360573526532,0.,9.63939026966049));
#21379=CARTESIAN_POINT('Ctrl Pts',(7.54360573526532,0.8496,9.63939026966049));
#21380=CARTESIAN_POINT('Ctrl Pts',(7.6590003866074,0.,9.45324999450471));
#21381=CARTESIAN_POINT('Ctrl Pts',(7.6590003866074,0.8496,9.45324999450471));
#21382=CARTESIAN_POINT('Ctrl Pts',(7.76209282457502,0.,9.26297089919836));
#21383=CARTESIAN_POINT('Ctrl Pts',(7.76209282457502,0.8496,9.26297089919836));
#21384=CARTESIAN_POINT('Ctrl Pts',(7.84862074946283,0.,9.06945407017055));
#21385=CARTESIAN_POINT('Ctrl Pts',(7.84862074946283,0.8496,9.06945407017055));
#21386=CARTESIAN_POINT('Ctrl Pts',(7.91508259073031,0.,8.87266947141857));
#21387=CARTESIAN_POINT('Ctrl Pts',(7.91508259073031,0.8496,8.87266947141857));
#21388=CARTESIAN_POINT('Ctrl Pts',(7.96007609558387,0.,8.67216210283894));
#21389=CARTESIAN_POINT('Ctrl Pts',(7.96007609558387,0.8496,8.67216210283894));
#21390=CARTESIAN_POINT('Ctrl Pts',(7.98575825096082,0.,8.46752658699496));
#21391=CARTESIAN_POINT('Ctrl Pts',(7.98575825096082,0.8496,8.46752658699496));
#21392=CARTESIAN_POINT('Ctrl Pts',(7.9987984391963,0.,8.25883677791438));
#21393=CARTESIAN_POINT('Ctrl Pts',(7.9987984391963,0.8496,8.25883677791438));
#21394=CARTESIAN_POINT('Ctrl Pts',(8.00781893805568,0.,8.04662057355209));
#21395=CARTESIAN_POINT('Ctrl Pts',(8.00781893805568,0.8496,8.04662057355209));
#21396=CARTESIAN_POINT('Ctrl Pts',(8.02124364536257,0.,7.8318867323277));
#21397=CARTESIAN_POINT('Ctrl Pts',(8.02124364536257,0.8496,7.8318867323277));
#21398=CARTESIAN_POINT('Ctrl Pts',(8.04494633492827,0.,7.61613341658679));
#21399=CARTESIAN_POINT('Ctrl Pts',(8.04494633492827,0.8496,7.61613341658679));
#21400=CARTESIAN_POINT('Ctrl Pts',(8.08008348678094,0.,7.40136016279815));
#21401=CARTESIAN_POINT('Ctrl Pts',(8.08008348678094,0.8496,7.40136016279815));
#21402=CARTESIAN_POINT('Ctrl Pts',(8.12057943633426,0.,7.19009032473197));
#21403=CARTESIAN_POINT('Ctrl Pts',(8.12057943633426,0.8496,7.19009032473197));
#21404=CARTESIAN_POINT('Ctrl Pts',(8.15569042861283,0.,6.98516923427904));
#21405=CARTESIAN_POINT('Ctrl Pts',(8.15569042861283,0.8496,6.98516923427904));
#21406=CARTESIAN_POINT('Ctrl Pts',(8.17293082304204,0.,6.78954489191915));
#21407=CARTESIAN_POINT('Ctrl Pts',(8.17293082304204,0.8496,6.78954489191915));
#21408=CARTESIAN_POINT('Ctrl Pts',(8.16089752265956,0.,6.60605451948904));
#21409=CARTESIAN_POINT('Ctrl Pts',(8.16089752265956,0.8496,6.60605451948904));
#21410=CARTESIAN_POINT('Ctrl Pts',(8.11207116917844,0.,6.43720976255638));
#21411=CARTESIAN_POINT('Ctrl Pts',(8.11207116917844,0.8496,6.43720976255638));
#21412=CARTESIAN_POINT('Ctrl Pts',(8.02580908828092,0.,6.28498018271691));
#21413=CARTESIAN_POINT('Ctrl Pts',(8.02580908828092,0.8496,6.28498018271691));
#21414=CARTESIAN_POINT('Ctrl Pts',(7.90644860448881,0.,6.15052660592943));
#21415=CARTESIAN_POINT('Ctrl Pts',(7.90644860448881,0.8496,6.15052660592943));
#21416=CARTESIAN_POINT('Ctrl Pts',(7.76106756457749,0.,6.03389995867286));
#21417=CARTESIAN_POINT('Ctrl Pts',(7.76106756457749,0.8496,6.03389995867286));
#21418=CARTESIAN_POINT('Ctrl Pts',(7.59751903688427,0.,5.93381436957244));
#21419=CARTESIAN_POINT('Ctrl Pts',(7.59751903688427,0.8496,5.93381436957244));
#21420=CARTESIAN_POINT('Ctrl Pts',(7.42198551710643,0.,5.84723737025948));
#21421=CARTESIAN_POINT('Ctrl Pts',(7.42198551710643,0.8496,5.84723737025948));
#21422=CARTESIAN_POINT('Ctrl Pts',(7.23853768475023,0.,5.76979878895671));
#21423=CARTESIAN_POINT('Ctrl Pts',(7.23853768475023,0.8496,5.76979878895671));
#21424=CARTESIAN_POINT('Ctrl Pts',(7.04976847947264,0.,5.69662713609756));
#21425=CARTESIAN_POINT('Ctrl Pts',(7.04976847947264,0.8496,5.69662713609756));
#21426=CARTESIAN_POINT('Ctrl Pts',(6.85709976037512,0.,5.62308582598972));
#21427=CARTESIAN_POINT('Ctrl Pts',(6.85709976037512,0.8496,5.62308582598972));
#21428=CARTESIAN_POINT('Ctrl Pts',(6.66121503090593,0.,5.54547963906641));
#21429=CARTESIAN_POINT('Ctrl Pts',(6.66121503090593,0.8496,5.54547963906641));
#21430=CARTESIAN_POINT('Ctrl Pts',(6.46246210121974,0.,5.46195513100458));
#21431=CARTESIAN_POINT('Ctrl Pts',(6.46246210121974,0.8496,5.46195513100458));
#21432=CARTESIAN_POINT('Ctrl Pts',(6.26112587698791,0.,5.37226655127806));
#21433=CARTESIAN_POINT('Ctrl Pts',(6.26112587698791,0.8496,5.37226655127806));
#21434=CARTESIAN_POINT('Ctrl Pts',(6.05762450882876,0.,5.27709955371581));
#21435=CARTESIAN_POINT('Ctrl Pts',(6.05762450882876,0.8496,5.27709955371581));
#21436=CARTESIAN_POINT('Ctrl Pts',(5.85274048349253,0.,5.17752467829117));
#21437=CARTESIAN_POINT('Ctrl Pts',(5.85274048349253,0.8496,5.17752467829117));
#21438=CARTESIAN_POINT('Ctrl Pts',(5.6478173738032,0.,5.07442896098936));
#21439=CARTESIAN_POINT('Ctrl Pts',(5.6478173738032,0.8496,5.07442896098936));
#21440=CARTESIAN_POINT('Ctrl Pts',(5.44501860313336,0.,4.96787993373722));
#21441=CARTESIAN_POINT('Ctrl Pts',(5.44501860313336,0.8496,4.96787993373722));
#21442=CARTESIAN_POINT('Ctrl Pts',(5.24741086000008,0.,4.85676111532844));
#21443=CARTESIAN_POINT('Ctrl Pts',(5.24741086000008,0.8496,4.85676111532844));
#21444=CARTESIAN_POINT('Ctrl Pts',(5.05850630701875,0.,4.73929437247794));
#21445=CARTESIAN_POINT('Ctrl Pts',(5.05850630701875,0.8496,4.73929437247794));
#21446=CARTESIAN_POINT('Ctrl Pts',(4.88190185104846,0.,4.61340315498245));
#21447=CARTESIAN_POINT('Ctrl Pts',(4.88190185104846,0.8496,4.61340315498245));
#21448=CARTESIAN_POINT('Ctrl Pts',(4.7208720035032,0.,4.47714872481864));
#21449=CARTESIAN_POINT('Ctrl Pts',(4.7208720035032,0.8496,4.47714872481864));
#21450=CARTESIAN_POINT('Ctrl Pts',(4.57800047823784,0.,4.32911151507775));
#21451=CARTESIAN_POINT('Ctrl Pts',(4.57800047823784,0.8496,4.32911151507775));
#21452=CARTESIAN_POINT('Ctrl Pts',(4.4547451964031,0.,4.16885849319143));
#21453=CARTESIAN_POINT('Ctrl Pts',(4.4547451964031,0.8496,4.16885849319143));
#21454=CARTESIAN_POINT('Ctrl Pts',(4.35148411330737,0.,3.99681013615577));
#21455=CARTESIAN_POINT('Ctrl Pts',(4.35148411330737,0.8496,3.99681013615577));
#21456=CARTESIAN_POINT('Ctrl Pts',(4.26765207024408,0.,3.81399668859083));
#21457=CARTESIAN_POINT('Ctrl Pts',(4.26765207024408,0.8496,3.81399668859083));
#21458=CARTESIAN_POINT('Ctrl Pts',(4.20184334854117,0.,3.62185203209172));
#21459=CARTESIAN_POINT('Ctrl Pts',(4.20184334854117,0.8496,3.62185203209172));
#21460=CARTESIAN_POINT('Ctrl Pts',(4.15193466045737,0.,3.42199345348454));
#21461=CARTESIAN_POINT('Ctrl Pts',(4.15193466045737,0.8496,3.42199345348454));
#21462=CARTESIAN_POINT('Ctrl Pts',(4.11518318246501,0.,3.21600287470933));
#21463=CARTESIAN_POINT('Ctrl Pts',(4.11518318246501,0.8496,3.21600287470933));
#21464=CARTESIAN_POINT('Ctrl Pts',(4.08854433447712,0.,3.00529120729351));
#21465=CARTESIAN_POINT('Ctrl Pts',(4.08854433447712,0.8496,3.00529120729351));
#21466=CARTESIAN_POINT('Ctrl Pts',(4.06899962712481,0.,2.7909834104826));
#21467=CARTESIAN_POINT('Ctrl Pts',(4.06899962712481,0.8496,2.7909834104826));
#21468=CARTESIAN_POINT('Ctrl Pts',(4.05390260344518,0.,2.57377631141663));
#21469=CARTESIAN_POINT('Ctrl Pts',(4.05390260344518,0.8496,2.57377631141663));
#21470=CARTESIAN_POINT('Ctrl Pts',(4.04126813644791,0.,2.35385258470204));
#21471=CARTESIAN_POINT('Ctrl Pts',(4.04126813644791,0.8496,2.35385258470204));
#21472=CARTESIAN_POINT('Ctrl Pts',(4.03021014446877,0.,2.13065748555701));
#21473=CARTESIAN_POINT('Ctrl Pts',(4.03021014446877,0.8496,2.13065748555701));
#21474=CARTESIAN_POINT('Ctrl Pts',(4.02066709528519,0.,1.9033255681334));
#21475=CARTESIAN_POINT('Ctrl Pts',(4.02066709528519,0.8496,1.9033255681334));
#21476=CARTESIAN_POINT('Ctrl Pts',(4.012782399266,0.,1.67142113207676));
#21477=CARTESIAN_POINT('Ctrl Pts',(4.012782399266,0.8496,1.67142113207676));
#21478=CARTESIAN_POINT('Ctrl Pts',(4.00639322616619,0.,1.4355810193293));
#21479=CARTESIAN_POINT('Ctrl Pts',(4.00639322616619,0.8496,1.4355810193293));
#21480=CARTESIAN_POINT('Ctrl Pts',(4.00047520099043,0.,1.19819542279832));
#21481=CARTESIAN_POINT('Ctrl Pts',(4.00047520099043,0.8496,1.19819542279832));
#21482=CARTESIAN_POINT('Ctrl Pts',(3.99260375067002,0.,0.964078729991153));
#21483=CARTESIAN_POINT('Ctrl Pts',(3.99260375067002,0.8496,0.964078729991153));
#21484=CARTESIAN_POINT('Ctrl Pts',(3.97841403016118,0.,0.741129277895168));
#21485=CARTESIAN_POINT('Ctrl Pts',(3.97841403016118,0.8496,0.741129277895168));
#21486=CARTESIAN_POINT('Ctrl Pts',(3.95259200169988,0.,0.538436816836329));
#21487=CARTESIAN_POINT('Ctrl Pts',(3.95259200169988,0.8496,0.538436816836329));
#21488=CARTESIAN_POINT('Ctrl Pts',(3.90986572419832,0.,0.364350357241537));
#21489=CARTESIAN_POINT('Ctrl Pts',(3.90986572419832,0.8496,0.364350357241537));
#21490=CARTESIAN_POINT('Ctrl Pts',(3.84598208672298,0.,0.224659532804428));
#21491=CARTESIAN_POINT('Ctrl Pts',(3.84598208672298,0.8496,0.224659532804428));
#21492=CARTESIAN_POINT('Ctrl Pts',(3.75872318140661,0.,0.120497232333236));
#21493=CARTESIAN_POINT('Ctrl Pts',(3.75872318140661,0.8496,0.120497232333236));
#21494=CARTESIAN_POINT('Ctrl Pts',(3.64881642260075,0.,0.0470540298718229));
#21495=CARTESIAN_POINT('Ctrl Pts',(3.64881642260075,0.8496,0.0470540298718229));
#21496=CARTESIAN_POINT('Ctrl Pts',(3.52045328348988,0.,-0.00118366394786523));
#21497=CARTESIAN_POINT('Ctrl Pts',(3.52045328348988,0.8496,-0.00118366394786523));
#21498=CARTESIAN_POINT('Ctrl Pts',(3.3816469894381,0.,-0.0263068037111615));
#21499=CARTESIAN_POINT('Ctrl Pts',(3.3816469894381,0.8496,-0.0263068037111615));
#21500=CARTESIAN_POINT('Ctrl Pts',(3.2451100102617,0.,-0.0214179570895094));
#21501=CARTESIAN_POINT('Ctrl Pts',(3.2451100102617,0.8496,-0.0214179570895094));
#21502=CARTESIAN_POINT('Ctrl Pts',(3.12452733970665,0.,0.0241851999814078));
#21503=CARTESIAN_POINT('Ctrl Pts',(3.12452733970665,0.8496,0.0241851999814078));
#21504=CARTESIAN_POINT('Ctrl Pts',(3.03063129752059,0.,0.119017371327004));
#21505=CARTESIAN_POINT('Ctrl Pts',(3.03063129752059,0.8496,0.119017371327004));
#21506=CARTESIAN_POINT('Ctrl Pts',(2.96639254265844,0.,0.262319630540593));
#21507=CARTESIAN_POINT('Ctrl Pts',(2.96639254265844,0.8496,0.262319630540593));
#21508=CARTESIAN_POINT('Ctrl Pts',(2.92780415844446,0.,0.444963858672424));
#21509=CARTESIAN_POINT('Ctrl Pts',(2.92780415844446,0.8496,0.444963858672424));
#21510=CARTESIAN_POINT('Ctrl Pts',(2.90717911786689,0.,0.65402023086958));
#21511=CARTESIAN_POINT('Ctrl Pts',(2.90717911786689,0.8496,0.65402023086958));
#21512=CARTESIAN_POINT('Ctrl Pts',(2.89547076625581,0.,0.875890304828918));
#21513=CARTESIAN_POINT('Ctrl Pts',(2.89547076625581,0.8496,0.875890304828918));
#21514=CARTESIAN_POINT('Ctrl Pts',(2.88537704766906,0.,1.10060381648398));
#21515=CARTESIAN_POINT('Ctrl Pts',(2.88537704766906,0.8496,1.10060381648398));
#21516=CARTESIAN_POINT('Ctrl Pts',(2.8728456296504,0.,1.32371934078733));
#21517=CARTESIAN_POINT('Ctrl Pts',(2.8728456296504,0.8496,1.32371934078733));
#21518=CARTESIAN_POINT('Ctrl Pts',(2.85578261679345,0.,1.54401727992264));
#21519=CARTESIAN_POINT('Ctrl Pts',(2.85578261679345,0.8496,1.54401727992264));
#21520=CARTESIAN_POINT('Ctrl Pts',(2.83335686249019,0.,1.76209503442146));
#21521=CARTESIAN_POINT('Ctrl Pts',(2.83335686249019,0.8496,1.76209503442146));
#21522=CARTESIAN_POINT('Ctrl Pts',(2.80505146480345,0.,1.97856787413951));
#21523=CARTESIAN_POINT('Ctrl Pts',(2.80505146480345,0.8496,1.97856787413951));
#21524=CARTESIAN_POINT('Ctrl Pts',(2.76985908233915,0.,2.19251877196071));
#21525=CARTESIAN_POINT('Ctrl Pts',(2.76985908233915,0.8496,2.19251877196071));
#21526=CARTESIAN_POINT('Ctrl Pts',(2.72531955636536,0.,2.39962532458029));
#21527=CARTESIAN_POINT('Ctrl Pts',(2.72531955636536,0.8496,2.39962532458029));
#21528=CARTESIAN_POINT('Ctrl Pts',(2.66797634363184,0.,2.59347738935741));
#21529=CARTESIAN_POINT('Ctrl Pts',(2.66797634363184,0.8496,2.59347738935741));
#21530=CARTESIAN_POINT('Ctrl Pts',(2.59397540849171,0.,2.7672283971178));
#21531=CARTESIAN_POINT('Ctrl Pts',(2.59397540849171,0.8496,2.7672283971178));
#21532=CARTESIAN_POINT('Ctrl Pts',(2.49960870420485,0.,2.91510580081997));
#21533=CARTESIAN_POINT('Ctrl Pts',(2.49960870420485,0.8496,2.91510580081997));
#21534=CARTESIAN_POINT('Ctrl Pts',(2.38189256086504,0.,3.03403241435618));
#21535=CARTESIAN_POINT('Ctrl Pts',(2.38189256086504,0.8496,3.03403241435618));
#21536=CARTESIAN_POINT('Ctrl Pts',(2.23909845280558,0.,3.12505646843308));
#21537=CARTESIAN_POINT('Ctrl Pts',(2.23909845280558,0.8496,3.12505646843308));
#21538=CARTESIAN_POINT('Ctrl Pts',(2.07061055216582,0.,3.19196918412265));
#21539=CARTESIAN_POINT('Ctrl Pts',(2.07061055216582,0.8496,3.19196918412265));
#21540=CARTESIAN_POINT('Ctrl Pts',(1.87681490437036,0.,3.24001322621211));
#21541=CARTESIAN_POINT('Ctrl Pts',(1.87681490437036,0.8496,3.24001322621211));
#21542=CARTESIAN_POINT('Ctrl Pts',(1.65897747541321,0.,3.27464765209773));
#21543=CARTESIAN_POINT('Ctrl Pts',(1.65897747541321,0.8496,3.27464765209773));
#21544=CARTESIAN_POINT('Ctrl Pts',(1.4191255439272,0.,3.30006519349576));
#21545=CARTESIAN_POINT('Ctrl Pts',(1.4191255439272,0.8496,3.30006519349576));
#21546=CARTESIAN_POINT('Ctrl Pts',(1.15993538533448,0.,3.31897283641381));
#21547=CARTESIAN_POINT('Ctrl Pts',(1.15993538533448,0.8496,3.31897283641381));
#21548=CARTESIAN_POINT('Ctrl Pts',(0.884625090385968,0.,3.33300441174764));
#21549=CARTESIAN_POINT('Ctrl Pts',(0.884625090385968,0.8496,3.33300441174764));
#21550=CARTESIAN_POINT('Ctrl Pts',(0.596845720618978,0.,3.34293392264922));
#21551=CARTESIAN_POINT('Ctrl Pts',(0.596845720618978,0.8496,3.34293392264922));
#21552=CARTESIAN_POINT('Ctrl Pts',(0.30057321210183,0.,3.34897162637417));
#21553=CARTESIAN_POINT('Ctrl Pts',(0.30057321210183,0.8496,3.34897162637417));
#21554=CARTESIAN_POINT('Ctrl Pts',(1.66741620510891E-14,0.,3.35102435732185));
#21555=CARTESIAN_POINT('Ctrl Pts',(1.66741620510891E-14,0.8496,3.35102435732185));
#21556=CARTESIAN_POINT('Ctrl Pts',(-0.300573212101791,0.,3.34897162637426));
#21557=CARTESIAN_POINT('Ctrl Pts',(-0.300573212101791,0.8496,3.34897162637426));
#21558=CARTESIAN_POINT('Ctrl Pts',(-0.596845720618908,0.,3.34293392264938));
#21559=CARTESIAN_POINT('Ctrl Pts',(-0.596845720618908,0.8496,3.34293392264938));
#21560=CARTESIAN_POINT('Ctrl Pts',(-0.884625090385886,0.,3.33300441174785));
#21561=CARTESIAN_POINT('Ctrl Pts',(-0.884625090385886,0.8496,3.33300441174785));
#21562=CARTESIAN_POINT('Ctrl Pts',(-1.15993538533442,0.,3.31897283641402));
#21563=CARTESIAN_POINT('Ctrl Pts',(-1.15993538533442,0.8496,3.31897283641402));
#21564=CARTESIAN_POINT('Ctrl Pts',(-1.41912554392716,0.,3.30006519349591));
#21565=CARTESIAN_POINT('Ctrl Pts',(-1.41912554392716,0.8496,3.30006519349591));
#21566=CARTESIAN_POINT('Ctrl Pts',(-1.65897747541319,0.,3.27464765209779));
#21567=CARTESIAN_POINT('Ctrl Pts',(-1.65897747541319,0.8496,3.27464765209779));
#21568=CARTESIAN_POINT('Ctrl Pts',(-1.87681490437034,0.,3.24001322621208));
#21569=CARTESIAN_POINT('Ctrl Pts',(-1.87681490437034,0.8496,3.24001322621208));
#21570=CARTESIAN_POINT('Ctrl Pts',(-2.07061055216576,0.,3.19196918412254));
#21571=CARTESIAN_POINT('Ctrl Pts',(-2.07061055216576,0.8496,3.19196918412254));
#21572=CARTESIAN_POINT('Ctrl Pts',(-2.23909845280547,0.,3.12505646843295));
#21573=CARTESIAN_POINT('Ctrl Pts',(-2.23909845280547,0.8496,3.12505646843295));
#21574=CARTESIAN_POINT('Ctrl Pts',(-2.38189256086493,0.,3.03403241435609));
#21575=CARTESIAN_POINT('Ctrl Pts',(-2.38189256086493,0.8496,3.03403241435609));
#21576=CARTESIAN_POINT('Ctrl Pts',(-2.49960870420481,0.,2.91510580081997));
#21577=CARTESIAN_POINT('Ctrl Pts',(-2.49960870420481,0.8496,2.91510580081997));
#21578=CARTESIAN_POINT('Ctrl Pts',(-2.59397540849182,0.,2.76722839711793));
#21579=CARTESIAN_POINT('Ctrl Pts',(-2.59397540849182,0.8496,2.76722839711793));
#21580=CARTESIAN_POINT('Ctrl Pts',(-2.66797634363209,0.,2.59347738935767));
#21581=CARTESIAN_POINT('Ctrl Pts',(-2.66797634363209,0.8496,2.59347738935767));
#21582=CARTESIAN_POINT('Ctrl Pts',(-2.72531955636566,0.,2.39962532458057));
#21583=CARTESIAN_POINT('Ctrl Pts',(-2.72531955636566,0.8496,2.39962532458057));
#21584=CARTESIAN_POINT('Ctrl Pts',(-2.76985908233936,0.,2.19251877196088));
#21585=CARTESIAN_POINT('Ctrl Pts',(-2.76985908233936,0.8496,2.19251877196088));
#21586=CARTESIAN_POINT('Ctrl Pts',(-2.80505146480344,0.,1.97856787413951));
#21587=CARTESIAN_POINT('Ctrl Pts',(-2.80505146480344,0.8496,1.97856787413951));
#21588=CARTESIAN_POINT('Ctrl Pts',(-2.8333568624899,0.,1.76209503442131));
#21589=CARTESIAN_POINT('Ctrl Pts',(-2.8333568624899,0.8496,1.76209503442131));
#21590=CARTESIAN_POINT('Ctrl Pts',(-2.85578261679294,0.,1.54401727992238));
#21591=CARTESIAN_POINT('Ctrl Pts',(-2.85578261679294,0.8496,1.54401727992238));
#21592=CARTESIAN_POINT('Ctrl Pts',(-2.87284562964987,0.,1.32371934078708));
#21593=CARTESIAN_POINT('Ctrl Pts',(-2.87284562964987,0.8496,1.32371934078708));
#21594=CARTESIAN_POINT('Ctrl Pts',(-2.88537704766869,0.,1.10060381648384));
#21595=CARTESIAN_POINT('Ctrl Pts',(-2.88537704766869,0.8496,1.10060381648384));
#21596=CARTESIAN_POINT('Ctrl Pts',(-2.89547076625573,0.,0.875890304828914));
#21597=CARTESIAN_POINT('Ctrl Pts',(-2.89547076625573,0.8496,0.875890304828914));
#21598=CARTESIAN_POINT('Ctrl Pts',(-2.90717911786707,0.,0.654020230869684));
#21599=CARTESIAN_POINT('Ctrl Pts',(-2.90717911786707,0.8496,0.654020230869684));
#21600=CARTESIAN_POINT('Ctrl Pts',(-2.92780415844476,0.,0.444963858672577));
#21601=CARTESIAN_POINT('Ctrl Pts',(-2.92780415844476,0.8496,0.444963858672577));
#21602=CARTESIAN_POINT('Ctrl Pts',(-2.96639254265869,0.,0.262319630540737));
#21603=CARTESIAN_POINT('Ctrl Pts',(-2.96639254265869,0.8496,0.262319630540737));
#21604=CARTESIAN_POINT('Ctrl Pts',(-3.03063129752067,0.,0.11901737132707));
#21605=CARTESIAN_POINT('Ctrl Pts',(-3.03063129752067,0.8496,0.11901737132707));
#21606=CARTESIAN_POINT('Ctrl Pts',(-3.12452733970658,0.,0.0241851999813871));
#21607=CARTESIAN_POINT('Ctrl Pts',(-3.12452733970658,0.8496,0.0241851999813871));
#21608=CARTESIAN_POINT('Ctrl Pts',(-3.24511001026157,0.,-0.0214179570895714));
#21609=CARTESIAN_POINT('Ctrl Pts',(-3.24511001026157,0.8496,-0.0214179570895714));
#21610=CARTESIAN_POINT('Ctrl Pts',(-3.38164698943802,0.,-0.0263068037112043));
#21611=CARTESIAN_POINT('Ctrl Pts',(-3.38164698943802,0.8496,-0.0263068037112043));
#21612=CARTESIAN_POINT('Ctrl Pts',(-3.52045328348989,0.,-0.00118366394785932));
#21613=CARTESIAN_POINT('Ctrl Pts',(-3.52045328348989,0.8496,-0.00118366394785932));
#21614=CARTESIAN_POINT('Ctrl Pts',(-3.64881642260079,0.,0.0470540298718583));
#21615=CARTESIAN_POINT('Ctrl Pts',(-3.64881642260079,0.8496,0.0470540298718583));
#21616=CARTESIAN_POINT('Ctrl Pts',(-3.75872318140663,0.,0.120497232333251));
#21617=CARTESIAN_POINT('Ctrl Pts',(-3.75872318140663,0.8496,0.120497232333251));
#21618=CARTESIAN_POINT('Ctrl Pts',(-3.84598208672296,0.,0.224659532804408));
#21619=CARTESIAN_POINT('Ctrl Pts',(-3.84598208672296,0.8496,0.224659532804408));
#21620=CARTESIAN_POINT('Ctrl Pts',(-3.9098657241983,0.,0.364350357241515));
#21621=CARTESIAN_POINT('Ctrl Pts',(-3.9098657241983,0.8496,0.364350357241515));
#21622=CARTESIAN_POINT('Ctrl Pts',(-3.9525920016999,0.,0.538436816836325));
#21623=CARTESIAN_POINT('Ctrl Pts',(-3.9525920016999,0.8496,0.538436816836325));
#21624=CARTESIAN_POINT('Ctrl Pts',(-3.97841403016126,0.,0.741129277895169));
#21625=CARTESIAN_POINT('Ctrl Pts',(-3.97841403016126,0.8496,0.741129277895169));
#21626=CARTESIAN_POINT('Ctrl Pts',(-3.99260375067011,0.,0.964078729991154));
#21627=CARTESIAN_POINT('Ctrl Pts',(-3.99260375067011,0.8496,0.964078729991154));
#21628=CARTESIAN_POINT('Ctrl Pts',(-4.00047520099045,0.,1.1981954227983));
#21629=CARTESIAN_POINT('Ctrl Pts',(-4.00047520099045,0.8496,1.1981954227983));
#21630=CARTESIAN_POINT('Ctrl Pts',(-4.00639322616607,0.,1.43558101932923));
#21631=CARTESIAN_POINT('Ctrl Pts',(-4.00639322616607,0.8496,1.43558101932923));
#21632=CARTESIAN_POINT('Ctrl Pts',(-4.01278239926574,0.,1.67142113207667));
#21633=CARTESIAN_POINT('Ctrl Pts',(-4.01278239926574,0.8496,1.67142113207667));
#21634=CARTESIAN_POINT('Ctrl Pts',(-4.02066709528487,0.,1.90332556813333));
#21635=CARTESIAN_POINT('Ctrl Pts',(-4.02066709528487,0.8496,1.90332556813333));
#21636=CARTESIAN_POINT('Ctrl Pts',(-4.0302101444685,0.,2.130657485557));
#21637=CARTESIAN_POINT('Ctrl Pts',(-4.0302101444685,0.8496,2.130657485557));
#21638=CARTESIAN_POINT('Ctrl Pts',(-4.04126813644779,0.,2.35385258470204));
#21639=CARTESIAN_POINT('Ctrl Pts',(-4.04126813644779,0.8496,2.35385258470204));
#21640=CARTESIAN_POINT('Ctrl Pts',(-4.05390260344525,0.,2.57377631141659));
#21641=CARTESIAN_POINT('Ctrl Pts',(-4.05390260344525,0.8496,2.57377631141659));
#21642=CARTESIAN_POINT('Ctrl Pts',(-4.06899962712502,0.,2.7909834104825));
#21643=CARTESIAN_POINT('Ctrl Pts',(-4.06899962712502,0.8496,2.7909834104825));
#21644=CARTESIAN_POINT('Ctrl Pts',(-4.08854433447739,0.,3.00529120729338));
#21645=CARTESIAN_POINT('Ctrl Pts',(-4.08854433447739,0.8496,3.00529120729338));
#21646=CARTESIAN_POINT('Ctrl Pts',(-4.11518318246524,0.,3.21600287470921));
#21647=CARTESIAN_POINT('Ctrl Pts',(-4.11518318246524,0.8496,3.21600287470921));
#21648=CARTESIAN_POINT('Ctrl Pts',(-4.15193466045748,0.,3.42199345348447));
#21649=CARTESIAN_POINT('Ctrl Pts',(-4.15193466045748,0.8496,3.42199345348447));
#21650=CARTESIAN_POINT('Ctrl Pts',(-4.20184334854115,0.,3.62185203209171));
#21651=CARTESIAN_POINT('Ctrl Pts',(-4.20184334854115,0.8496,3.62185203209171));
#21652=CARTESIAN_POINT('Ctrl Pts',(-4.26765207024395,0.,3.81399668859083));
#21653=CARTESIAN_POINT('Ctrl Pts',(-4.26765207024395,0.8496,3.81399668859083));
#21654=CARTESIAN_POINT('Ctrl Pts',(-4.35148411330718,0.,3.99681013615577));
#21655=CARTESIAN_POINT('Ctrl Pts',(-4.35148411330718,0.8496,3.99681013615577));
#21656=CARTESIAN_POINT('Ctrl Pts',(-4.45474519640294,0.,4.16885849319142));
#21657=CARTESIAN_POINT('Ctrl Pts',(-4.45474519640294,0.8496,4.16885849319142));
#21658=CARTESIAN_POINT('Ctrl Pts',(-4.57800047823775,0.,4.32911151507774));
#21659=CARTESIAN_POINT('Ctrl Pts',(-4.57800047823775,0.8496,4.32911151507774));
#21660=CARTESIAN_POINT('Ctrl Pts',(-4.7208720035032,0.,4.47714872481861));
#21661=CARTESIAN_POINT('Ctrl Pts',(-4.7208720035032,0.8496,4.47714872481861));
#21662=CARTESIAN_POINT('Ctrl Pts',(-4.88190185104852,0.,4.61340315498244));
#21663=CARTESIAN_POINT('Ctrl Pts',(-4.88190185104852,0.8496,4.61340315498244));
#21664=CARTESIAN_POINT('Ctrl Pts',(-5.05850630701885,0.,4.73929437247796));
#21665=CARTESIAN_POINT('Ctrl Pts',(-5.05850630701885,0.8496,4.73929437247796));
#21666=CARTESIAN_POINT('Ctrl Pts',(-5.24741086000019,0.,4.8567611153285));
#21667=CARTESIAN_POINT('Ctrl Pts',(-5.24741086000019,0.8496,4.8567611153285));
#21668=CARTESIAN_POINT('Ctrl Pts',(-5.44501860313342,0.,4.96787993373728));
#21669=CARTESIAN_POINT('Ctrl Pts',(-5.44501860313342,0.8496,4.96787993373728));
#21670=CARTESIAN_POINT('Ctrl Pts',(-5.64781737380319,0.,5.07442896098937));
#21671=CARTESIAN_POINT('Ctrl Pts',(-5.64781737380319,0.8496,5.07442896098937));
#21672=CARTESIAN_POINT('Ctrl Pts',(-5.85274048349242,0.,5.17752467829109));
#21673=CARTESIAN_POINT('Ctrl Pts',(-5.85274048349242,0.8496,5.17752467829109));
#21674=CARTESIAN_POINT('Ctrl Pts',(-6.05762450882858,0.,5.27709955371564));
#21675=CARTESIAN_POINT('Ctrl Pts',(-6.05762450882858,0.8496,5.27709955371564));
#21676=CARTESIAN_POINT('Ctrl Pts',(-6.26112587698772,0.,5.37226655127787));
#21677=CARTESIAN_POINT('Ctrl Pts',(-6.26112587698772,0.8496,5.37226655127787));
#21678=CARTESIAN_POINT('Ctrl Pts',(-6.46246210121964,0.,5.46195513100446));
#21679=CARTESIAN_POINT('Ctrl Pts',(-6.46246210121964,0.8496,5.46195513100446));
#21680=CARTESIAN_POINT('Ctrl Pts',(-6.66121503090592,0.,5.54547963906637));
#21681=CARTESIAN_POINT('Ctrl Pts',(-6.66121503090592,0.8496,5.54547963906637));
#21682=CARTESIAN_POINT('Ctrl Pts',(-6.8570997603751,0.,5.62308582598972));
#21683=CARTESIAN_POINT('Ctrl Pts',(-6.8570997603751,0.8496,5.62308582598972));
#21684=CARTESIAN_POINT('Ctrl Pts',(-7.04976847947249,0.,5.69662713609756));
#21685=CARTESIAN_POINT('Ctrl Pts',(-7.04976847947249,0.8496,5.69662713609756));
#21686=CARTESIAN_POINT('Ctrl Pts',(-7.23853768475,0.,5.76979878895672));
#21687=CARTESIAN_POINT('Ctrl Pts',(-7.23853768475,0.8496,5.76979878895672));
#21688=CARTESIAN_POINT('Ctrl Pts',(-7.42198551710617,0.,5.84723737025949));
#21689=CARTESIAN_POINT('Ctrl Pts',(-7.42198551710617,0.8496,5.84723737025949));
#21690=CARTESIAN_POINT('Ctrl Pts',(-7.59751903688412,0.,5.93381436957244));
#21691=CARTESIAN_POINT('Ctrl Pts',(-7.59751903688412,0.8496,5.93381436957244));
#21692=CARTESIAN_POINT('Ctrl Pts',(-7.76106756457753,0.,6.03389995867283));
#21693=CARTESIAN_POINT('Ctrl Pts',(-7.76106756457753,0.8496,6.03389995867283));
#21694=CARTESIAN_POINT('Ctrl Pts',(-7.90644860448901,0.,6.15052660592937));
#21695=CARTESIAN_POINT('Ctrl Pts',(-7.90644860448901,0.8496,6.15052660592937));
#21696=CARTESIAN_POINT('Ctrl Pts',(-8.02580908828117,0.,6.28498018271686));
#21697=CARTESIAN_POINT('Ctrl Pts',(-8.02580908828117,0.8496,6.28498018271686));
#21698=CARTESIAN_POINT('Ctrl Pts',(-8.11207116917861,0.,6.43720976255636));
#21699=CARTESIAN_POINT('Ctrl Pts',(-8.11207116917861,0.8496,6.43720976255636));
#21700=CARTESIAN_POINT('Ctrl Pts',(-8.16089752265956,0.,6.60605451948903));
#21701=CARTESIAN_POINT('Ctrl Pts',(-8.16089752265956,0.8496,6.60605451948903));
#21702=CARTESIAN_POINT('Ctrl Pts',(-8.17293082304181,0.,6.78954489191904));
#21703=CARTESIAN_POINT('Ctrl Pts',(-8.17293082304181,0.8496,6.78954489191904));
#21704=CARTESIAN_POINT('Ctrl Pts',(-8.15569042861244,0.,6.9851692342788));
#21705=CARTESIAN_POINT('Ctrl Pts',(-8.15569042861244,0.8496,6.9851692342788));
#21706=CARTESIAN_POINT('Ctrl Pts',(-8.12057943633387,0.,7.19009032473164));
#21707=CARTESIAN_POINT('Ctrl Pts',(-8.12057943633387,0.8496,7.19009032473164));
#21708=CARTESIAN_POINT('Ctrl Pts',(-8.08008348678073,0.,7.40136016279791));
#21709=CARTESIAN_POINT('Ctrl Pts',(-8.08008348678073,0.8496,7.40136016279791));
#21710=CARTESIAN_POINT('Ctrl Pts',(-8.04494633492831,0.,7.61613341658677));
#21711=CARTESIAN_POINT('Ctrl Pts',(-8.04494633492831,0.8496,7.61613341658677));
#21712=CARTESIAN_POINT('Ctrl Pts',(-8.02124364536279,0.,7.83188673232793));
#21713=CARTESIAN_POINT('Ctrl Pts',(-8.02124364536279,0.8496,7.83188673232793));
#21714=CARTESIAN_POINT('Ctrl Pts',(-8.007818938056,0.,8.04662057355248));
#21715=CARTESIAN_POINT('Ctrl Pts',(-8.007818938056,0.8496,8.04662057355248));
#21716=CARTESIAN_POINT('Ctrl Pts',(-7.99879843919661,0.,8.25883677791483));
#21717=CARTESIAN_POINT('Ctrl Pts',(-7.99879843919661,0.8496,8.25883677791483));
#21718=CARTESIAN_POINT('Ctrl Pts',(-7.98575825096101,0.,8.46752658699528));
#21719=CARTESIAN_POINT('Ctrl Pts',(-7.98575825096101,0.8496,8.46752658699528));
#21720=CARTESIAN_POINT('Ctrl Pts',(-7.96007609558389,0.,8.67216210283896));
#21721=CARTESIAN_POINT('Ctrl Pts',(-7.96007609558389,0.8496,8.67216210283896));
#21722=CARTESIAN_POINT('Ctrl Pts',(-7.91508259073019,0.,8.87266947141823));
#21723=CARTESIAN_POINT('Ctrl Pts',(-7.91508259073019,0.8496,8.87266947141823));
#21724=CARTESIAN_POINT('Ctrl Pts',(-7.84862074946261,0.,9.06945407016992));
#21725=CARTESIAN_POINT('Ctrl Pts',(-7.84862074946261,0.8496,9.06945407016992));
#21726=CARTESIAN_POINT('Ctrl Pts',(-7.76209282457479,0.,9.26297089919765));
#21727=CARTESIAN_POINT('Ctrl Pts',(-7.76209282457479,0.8496,9.26297089919765));
#21728=CARTESIAN_POINT('Ctrl Pts',(-7.65900038660722,0.,9.4532499945042));
#21729=CARTESIAN_POINT('Ctrl Pts',(-7.65900038660722,0.8496,9.4532499945042));
#21730=CARTESIAN_POINT('Ctrl Pts',(-7.5436057352653,0.,9.63939026966035));
#21731=CARTESIAN_POINT('Ctrl Pts',(-7.5436057352653,0.8496,9.63939026966035));
#21732=CARTESIAN_POINT('Ctrl Pts',(-7.41967047355001,0.,9.81917361987397));
#21733=CARTESIAN_POINT('Ctrl Pts',(-7.41967047355001,0.8496,9.81917361987397));
#21734=CARTESIAN_POINT('Ctrl Pts',(-7.28883796912703,0.,9.98835756998572));
#21735=CARTESIAN_POINT('Ctrl Pts',(-7.28883796912703,0.8496,9.98835756998572));
#21736=CARTESIAN_POINT('Ctrl Pts',(-7.15081550722306,0.,10.1414720974148));
#21737=CARTESIAN_POINT('Ctrl Pts',(-7.15081550722306,0.8496,10.1414720974148));
#21738=CARTESIAN_POINT('Ctrl Pts',(-7.0044544864105,0.,10.2733319413008));
#21739=CARTESIAN_POINT('Ctrl Pts',(-7.0044544864105,0.8496,10.2733319413008));
#21740=CARTESIAN_POINT('Ctrl Pts',(-6.84859008776113,0.,10.3804015453596));
#21741=CARTESIAN_POINT('Ctrl Pts',(-6.84859008776113,0.8496,10.3804015453596));
#21742=CARTESIAN_POINT('Ctrl Pts',(-6.68288828293938,0.,10.4620502678778));
#21743=CARTESIAN_POINT('Ctrl Pts',(-6.68288828293938,0.8496,10.4620502678778));
#21744=CARTESIAN_POINT('Ctrl Pts',(-6.50892555577766,0.,10.522290883026));
#21745=CARTESIAN_POINT('Ctrl Pts',(-6.50892555577766,0.8496,10.522290883026));
#21746=CARTESIAN_POINT('Ctrl Pts',(-6.32976796473811,0.,10.5687216653902));
#21747=CARTESIAN_POINT('Ctrl Pts',(-6.32976796473811,0.8496,10.5687216653902));
#21748=CARTESIAN_POINT('Ctrl Pts',(-6.14893768388701,0.,10.6103475969885));
#21749=CARTESIAN_POINT('Ctrl Pts',(-6.14893768388701,0.8496,10.6103475969885));
#21750=CARTESIAN_POINT('Ctrl Pts',(-5.96961932707142,0.,10.6558377434043));
#21751=CARTESIAN_POINT('Ctrl Pts',(-5.96961932707142,0.8496,10.6558377434043));
#21752=CARTESIAN_POINT('Ctrl Pts',(-5.79367695415031,0.,10.7114411549114));
#21753=CARTESIAN_POINT('Ctrl Pts',(-5.79367695415031,0.8496,10.7114411549114));
#21754=CARTESIAN_POINT('Ctrl Pts',(-5.62101499943431,0.,10.7795199127535));
#21755=CARTESIAN_POINT('Ctrl Pts',(-5.62101499943431,0.8496,10.7795199127535));
#21756=CARTESIAN_POINT('Ctrl Pts',(-5.45051506148982,0.,10.8599381259737));
#21757=CARTESIAN_POINT('Ctrl Pts',(-5.45051506148982,0.8496,10.8599381259737));
#21758=CARTESIAN_POINT('Ctrl Pts',(-5.28082876351929,0.,10.9511663773826));
#21759=CARTESIAN_POINT('Ctrl Pts',(-5.28082876351929,0.8496,10.9511663773826));
#21760=CARTESIAN_POINT('Ctrl Pts',(-5.11112998264616,0.,11.0513704191329));
#21761=CARTESIAN_POINT('Ctrl Pts',(-5.11112998264616,0.8496,11.0513704191329));
#21762=CARTESIAN_POINT('Ctrl Pts',(-4.94211773226973,0.,11.1598106424589));
#21763=CARTESIAN_POINT('Ctrl Pts',(-4.94211773226973,0.8496,11.1598106424589));
#21764=CARTESIAN_POINT('Ctrl Pts',(-4.77596612414951,0.,11.2768795166235));
#21765=CARTESIAN_POINT('Ctrl Pts',(-4.77596612414951,0.8496,11.2768795166235));
#21766=CARTESIAN_POINT('Ctrl Pts',(-4.61532593596946,0.,11.4029224160731));
#21767=CARTESIAN_POINT('Ctrl Pts',(-4.61532593596946,0.8496,11.4029224160731));
#21768=CARTESIAN_POINT('Ctrl Pts',(-4.46255574628757,0.,11.5373242211527));
#21769=CARTESIAN_POINT('Ctrl Pts',(-4.46255574628757,0.8496,11.5373242211527));
#21770=CARTESIAN_POINT('Ctrl Pts',(-4.31893584999241,0.,11.6776492463597));
#21771=CARTESIAN_POINT('Ctrl Pts',(-4.31893584999241,0.8496,11.6776492463597));
#21772=CARTESIAN_POINT('Ctrl Pts',(-4.18369962429796,0.,11.8183570873721));
#21773=CARTESIAN_POINT('Ctrl Pts',(-4.18369962429796,0.8496,11.8183570873721));
#21774=CARTESIAN_POINT('Ctrl Pts',(-4.05395481372655,0.,11.9514202619522));
#21775=CARTESIAN_POINT('Ctrl Pts',(-4.05395481372655,0.8496,11.9514202619522));
#21776=CARTESIAN_POINT('Ctrl Pts',(-3.92533033057354,0.,12.0684942936867));
#21777=CARTESIAN_POINT('Ctrl Pts',(-3.92533033057354,0.8496,12.0684942936867));
#21778=CARTESIAN_POINT('Ctrl Pts',(-3.79241297762166,0.,12.1626050652586));
#21779=CARTESIAN_POINT('Ctrl Pts',(-3.79241297762166,0.8496,12.1626050652586));
#21780=CARTESIAN_POINT('Ctrl Pts',(-3.64927048315908,0.,12.2301117722809));
#21781=CARTESIAN_POINT('Ctrl Pts',(-3.64927048315908,0.8496,12.2301117722809));
#21782=CARTESIAN_POINT('Ctrl Pts',(-3.48993681214334,0.,12.2723364229645));
#21783=CARTESIAN_POINT('Ctrl Pts',(-3.48993681214334,0.8496,12.2723364229645));
#21784=CARTESIAN_POINT('Ctrl Pts',(-3.30884480305534,0.,12.2938762651139));
#21785=CARTESIAN_POINT('Ctrl Pts',(-3.30884480305534,0.8496,12.2938762651139));
#21786=CARTESIAN_POINT('Ctrl Pts',(-3.10127560868576,0.,12.3010487961981));
#21787=CARTESIAN_POINT('Ctrl Pts',(-3.10127560868576,0.8496,12.3010487961981));
#21788=CARTESIAN_POINT('Ctrl Pts',(-2.86376302967345,0.,12.300400839059));
#21789=CARTESIAN_POINT('Ctrl Pts',(-2.86376302967345,0.8496,12.300400839059));
#21790=CARTESIAN_POINT('Ctrl Pts',(-2.59461297443094,0.,12.2969132923574));
#21791=CARTESIAN_POINT('Ctrl Pts',(-2.59461297443094,0.8496,12.2969132923574));
#21792=CARTESIAN_POINT('Ctrl Pts',(-2.29394197380209,0.,12.2935845551224));
#21793=CARTESIAN_POINT('Ctrl Pts',(-2.29394197380209,0.8496,12.2935845551224));
#21794=CARTESIAN_POINT('Ctrl Pts',(-1.96338745719135,0.,12.2919684497906));
#21795=CARTESIAN_POINT('Ctrl Pts',(-1.96338745719135,0.8496,12.2919684497906));
#21796=CARTESIAN_POINT('Ctrl Pts',(-1.60591558979456,0.,12.2924280531798));
#21797=CARTESIAN_POINT('Ctrl Pts',(-1.60591558979456,0.8496,12.2924280531798));
#21798=CARTESIAN_POINT('Ctrl Pts',(-1.22558901314075,0.,12.2945066442122));
#21799=CARTESIAN_POINT('Ctrl Pts',(-1.22558901314075,0.8496,12.2945066442122));
#21800=CARTESIAN_POINT('Ctrl Pts',(-0.827351903312651,0.,12.2972483292773));
#21801=CARTESIAN_POINT('Ctrl Pts',(-0.827351903312651,0.8496,12.2972483292773));
#21802=CARTESIAN_POINT('Ctrl Pts',(-0.498916532526571,0.,12.299081889758));
#21803=CARTESIAN_POINT('Ctrl Pts',(-0.498916532526571,0.8496,12.299081889758));
#21804=CARTESIAN_POINT('Ctrl Pts',(-0.249771440080693,0.,12.2998330708668));
#21805=CARTESIAN_POINT('Ctrl Pts',(-0.249771440080693,0.8496,12.2998330708668));
#21806=CARTESIAN_POINT('Ctrl Pts',(-0.0832571466935557,0.,12.2999999999989));
#21807=CARTESIAN_POINT('Ctrl Pts',(-0.0832571466935557,0.8496,12.2999999999989));
#21808=CARTESIAN_POINT('Ctrl Pts',(0.,0.,12.3));
#21809=CARTESIAN_POINT('Ctrl Pts',(0.,0.8496,12.3));
#21810=CARTESIAN_POINT('Ctrl Pts',(0.0832571466935396,0.,12.3000000000011));
#21811=CARTESIAN_POINT('Ctrl Pts',(0.0832571466935396,0.8496,12.3000000000011));
#21812=CARTESIAN_POINT('Ctrl Pts',(0.24977144008061,0.,12.2998330708736));
#21813=CARTESIAN_POINT('Ctrl Pts',(0.24977144008061,0.8496,12.2998330708736));
#21814=CARTESIAN_POINT('Ctrl Pts',(0.498916532526534,0.,12.2990818897713));
#21815=CARTESIAN_POINT('Ctrl Pts',(0.498916532526534,0.8496,12.2990818897713));
#21816=CARTESIAN_POINT('Ctrl Pts',(0.827351903312438,0.,12.2972483292974));
#21817=CARTESIAN_POINT('Ctrl Pts',(0.827351903312438,0.8496,12.2972483292974));
#21818=CARTESIAN_POINT('Ctrl Pts',(1.22558901314046,0.,12.2945066442369));
#21819=CARTESIAN_POINT('Ctrl Pts',(1.22558901314046,0.8496,12.2945066442369));
#21820=CARTESIAN_POINT('Ctrl Pts',(1.60591558979418,0.,12.2924280532047));
#21821=CARTESIAN_POINT('Ctrl Pts',(1.60591558979418,0.8496,12.2924280532047));
#21822=CARTESIAN_POINT('Ctrl Pts',(1.96338745719096,0.,12.291968449812));
#21823=CARTESIAN_POINT('Ctrl Pts',(1.96338745719096,0.8496,12.291968449812));
#21824=CARTESIAN_POINT('Ctrl Pts',(2.29394197380175,0.,12.2935845551378));
#21825=CARTESIAN_POINT('Ctrl Pts',(2.29394197380175,0.8496,12.2935845551378));
#21826=CARTESIAN_POINT('Ctrl Pts',(2.59461297443069,0.,12.2969132923658));
#21827=CARTESIAN_POINT('Ctrl Pts',(2.59461297443069,0.8496,12.2969132923658));
#21828=CARTESIAN_POINT('Ctrl Pts',(2.86376302967335,0.,12.3004008390612));
#21829=CARTESIAN_POINT('Ctrl Pts',(2.86376302967335,0.8496,12.3004008390612));
#21830=CARTESIAN_POINT('Ctrl Pts',(3.10127560868576,0.,12.3010487961961));
#21831=CARTESIAN_POINT('Ctrl Pts',(3.10127560868576,0.8496,12.3010487961961));
#21832=CARTESIAN_POINT('Ctrl Pts',(3.30884480305537,0.,12.2938762651102));
#21833=CARTESIAN_POINT('Ctrl Pts',(3.30884480305537,0.8496,12.2938762651102));
#21834=CARTESIAN_POINT('Ctrl Pts',(3.48993681214337,0.,12.2723364229612));
#21835=CARTESIAN_POINT('Ctrl Pts',(3.48993681214337,0.8496,12.2723364229612));
#21836=CARTESIAN_POINT('Ctrl Pts',(3.64927048315907,0.,12.2301117722792));
#21837=CARTESIAN_POINT('Ctrl Pts',(3.64927048315907,0.8496,12.2301117722792));
#21838=CARTESIAN_POINT('Ctrl Pts',(3.79241297762162,0.,12.1626050652587));
#21839=CARTESIAN_POINT('Ctrl Pts',(3.79241297762162,0.8496,12.1626050652587));
#21840=CARTESIAN_POINT('Ctrl Pts',(3.90811725944041,0.,12.0806818325566));
#21841=CARTESIAN_POINT('Ctrl Pts',(3.90811725944041,0.8496,12.0806818325566));
#21842=CARTESIAN_POINT('Ctrl Pts',(3.99482565231282,0.,12.0046763352305));
#21843=CARTESIAN_POINT('Ctrl Pts',(3.99482565231282,0.8496,12.0046763352305));
#21844=CARTESIAN_POINT('Ctrl Pts',(4.05565687163389,0.,11.9465013108381));
#21845=CARTESIAN_POINT('Ctrl Pts',(4.05565687163389,0.8496,11.9465013108381));
#21846=CARTESIAN_POINT('Ctrl Pts',(4.0908196144603,0.,11.9117811315282));
#21847=CARTESIAN_POINT('Ctrl Pts',(4.0908196144603,0.8496,11.9117811315282));
#21848=CARTESIAN_POINT('Ctrl Pts',(4.1,0.,11.9026515720695));
#21849=CARTESIAN_POINT('Ctrl Pts',(4.1,0.8496,11.9026515720695));
#21850=CARTESIAN_POINT('',(4.10063757647074,0.292307308198873,3.09202603079313));
#21851=CARTESIAN_POINT('',(4.1006262898548,0.292339670981987,3.09201395474132));
#21852=CARTESIAN_POINT('Ctrl Pts',(4.15877746029711,0.0799982138568305,
3.43674861413894));
#21853=CARTESIAN_POINT('Ctrl Pts',(4.14646117554196,0.124733851720112,3.38095797208512));
#21854=CARTESIAN_POINT('Ctrl Pts',(4.12508521221268,0.202624969870674,3.27000814202033));
#21855=CARTESIAN_POINT('Ctrl Pts',(4.10791209946146,0.265571898245336,3.14988703412665));
#21856=CARTESIAN_POINT('Ctrl Pts',(4.1006381376306,0.292296403815986,3.09203050838626));
#21857=CARTESIAN_POINT('Origin',(4.18004567262241,0.307776805703052,3.08202038908219));
#21858=CARTESIAN_POINT('Origin',(4.36136464669403,0.283715212921747,3.04584783530248));
#21859=CARTESIAN_POINT('Origin',(4.1,0.,1.2));
#21860=CARTESIAN_POINT('Ctrl Pts',(4.29339835604888,0.0559939529287135,
3.55467920026169));
#21861=CARTESIAN_POINT('Ctrl Pts',(4.25584474784527,0.150162334098852,3.46593762044134));
#21862=CARTESIAN_POINT('Ctrl Pts',(4.17638455329654,0.33726205850833,3.22405277301241));
#21863=CARTESIAN_POINT('Ctrl Pts',(4.13042338687859,0.443584832494149,2.92533348324746));
#21864=CARTESIAN_POINT('Ctrl Pts',(4.11051138672739,0.490305829863764,2.74803482597387));
#21865=CARTESIAN_POINT('Ctrl Pts',(4.3060475661543,0.0550570568185274,3.54597738315241));
#21866=CARTESIAN_POINT('Ctrl Pts',(4.26914663034547,0.150354528702341,3.45998535295299));
#21867=CARTESIAN_POINT('Ctrl Pts',(4.18859964481653,0.340124295101877,3.22265812391974));
#21868=CARTESIAN_POINT('Ctrl Pts',(4.14050849741124,0.447815386226925,2.92485200908127));
#21869=CARTESIAN_POINT('Ctrl Pts',(4.11965690824515,0.495007873940908,2.74784464353325));
#21870=CARTESIAN_POINT('Ctrl Pts',(4.33523822515995,0.0596089270271733,
3.53376471245904));
#21871=CARTESIAN_POINT('Ctrl Pts',(4.29744618195624,0.156949697666454,3.45282690279432));
#21872=CARTESIAN_POINT('Ctrl Pts',(4.21178168150148,0.35100840785864,3.22251980707619));
#21873=CARTESIAN_POINT('Ctrl Pts',(4.15902952625075,0.460249382405453,2.92536481676328));
#21874=CARTESIAN_POINT('Ctrl Pts',(4.13617464437627,0.507855044332698,2.74857164914344));
#21875=CARTESIAN_POINT('Ctrl Pts',(4.38400568703593,0.0874022066366798,
3.53702215045297));
#21876=CARTESIAN_POINT('Ctrl Pts',(4.3397963041374,0.186814587951356,3.45970264916118));
#21877=CARTESIAN_POINT('Ctrl Pts',(4.24053830160474,0.383996027912259,3.23126786608819));
#21878=CARTESIAN_POINT('Ctrl Pts',(4.18058055549715,0.492294479045333,2.93123150415905));
#21879=CARTESIAN_POINT('Ctrl Pts',(4.15478642497044,0.539079251837051,2.75350788240694));
#21880=CARTESIAN_POINT('Ctrl Pts',(4.40199170668536,0.116954263196119,3.56084440742005));
#21881=CARTESIAN_POINT('Ctrl Pts',(4.35269219239138,0.217003436097948,3.48044613277936));
#21882=CARTESIAN_POINT('Ctrl Pts',(4.24528014220526,0.413945938159646,3.24416115246424));
#21883=CARTESIAN_POINT('Ctrl Pts',(4.18297157398144,0.519676492843704,2.93904329627266));
#21884=CARTESIAN_POINT('Ctrl Pts',(4.15627962724123,0.565091367558406,2.75968239072319));
#21885=CARTESIAN_POINT('Ctrl Pts',(4.4028813462376,0.132178376897717,3.57815186105023));
#21886=CARTESIAN_POINT('Ctrl Pts',(4.35199587562355,0.232956026703696,3.49496809556833));
#21887=CARTESIAN_POINT('Ctrl Pts',(4.24197300931968,0.430310911915843,3.25270142258189));
#21888=CARTESIAN_POINT('Ctrl Pts',(4.17940016830811,0.534808403083364,2.94423234285935));
#21889=CARTESIAN_POINT('Ctrl Pts',(4.15273910526043,0.579540791776975,2.76375542954464));
#21890=CARTESIAN_POINT('',(4.11092960039253,0.489270313943276,2.7535990262568));
#21891=CARTESIAN_POINT('Ctrl Pts',(4.29338839752952,0.0560337429176049,
3.55463113046212));
#21892=CARTESIAN_POINT('Ctrl Pts',(4.28200201425128,0.0845703603400842,
3.52772622977568));
#21893=CARTESIAN_POINT('Ctrl Pts',(4.2709089389845,0.111840202565025,3.49944329913683));
#21894=CARTESIAN_POINT('Ctrl Pts',(4.26022466516199,0.137812970890808,3.46992665998807));
#21895=CARTESIAN_POINT('Ctrl Pts',(4.24925651305979,0.164475828680185,3.43962577168181));
#21896=CARTESIAN_POINT('Ctrl Pts',(4.23871834098693,0.189772252648034,3.40802535345698));
#21897=CARTESIAN_POINT('Ctrl Pts',(4.22869342338732,0.213651455574615,3.37524966812642));
#21898=CARTESIAN_POINT('Ctrl Pts',(4.22022011266837,0.233834754250891,3.34754684034024));
#21899=CARTESIAN_POINT('Ctrl Pts',(4.21211246977426,0.253005453813316,3.31900381508105));
#21900=CARTESIAN_POINT('Ctrl Pts',(4.20440515624013,0.271118966485284,3.28967551860074));
#21901=CARTESIAN_POINT('Ctrl Pts',(4.20081384008402,0.279559177255812,3.27600964338828));
#21902=CARTESIAN_POINT('Ctrl Pts',(4.19730929252788,0.287769629485392,3.26217300268237));
#21903=CARTESIAN_POINT('Ctrl Pts',(4.19388960090582,0.295760962667081,3.24817707975791));
#21904=CARTESIAN_POINT('Ctrl Pts',(4.1836826106382,0.319613247909556,3.2064024799213));
#21905=CARTESIAN_POINT('Ctrl Pts',(4.17426127019943,0.341554919196119,3.16314473495888));
#21906=CARTESIAN_POINT('Ctrl Pts',(4.16557077913211,0.36180048426393,3.11876022001722));
#21907=CARTESIAN_POINT('Ctrl Pts',(4.15562425095267,0.384972141871765,3.06796080889318));
#21908=CARTESIAN_POINT('Ctrl Pts',(4.14663412018599,0.405922678178319,3.01568449521542));
#21909=CARTESIAN_POINT('Ctrl Pts',(4.13847959221096,0.424941648061345,2.96242067986732));
#21910=CARTESIAN_POINT('Ctrl Pts',(4.13793497928194,0.426211859767844,2.95886337249452));
#21911=CARTESIAN_POINT('Ctrl Pts',(4.13739408426757,0.427473443573063,2.9553016503188));
#21912=CARTESIAN_POINT('Ctrl Pts',(4.13685686763256,0.428726480598055,2.95173565560756));
#21913=CARTESIAN_POINT('Ctrl Pts',(4.12711395055437,0.451451457888153,2.88706306635978));
#21914=CARTESIAN_POINT('Ctrl Pts',(4.1185832632104,0.471366282144737,2.82098952702215));
#21915=CARTESIAN_POINT('Ctrl Pts',(4.11092961016103,0.48927029109206,2.75359911226844));
#21916=CARTESIAN_POINT('Ctrl Pts',(4.11092959062404,0.489270336794493,2.75359894024517));
#21917=CARTESIAN_POINT('Ctrl Pts',(4.1107363463406,0.48972238856588,2.75189742393957));
#21918=CARTESIAN_POINT('Ctrl Pts',(4.11054370257317,0.490173111237358,2.75019527901328));
#21919=CARTESIAN_POINT('Ctrl Pts',(4.11035165498701,0.490622516758464,2.74849251651165));
#21920=CARTESIAN_POINT('Ctrl Pts',(4.29852898837605,0.0372770987405308,
3.57383899454876));
#21921=CARTESIAN_POINT('Ctrl Pts',(4.27477346003042,0.123982026893121,3.48643046936511));
#21922=CARTESIAN_POINT('Ctrl Pts',(4.23193632460675,0.280581959460234,3.29066087065414));
#21923=CARTESIAN_POINT('Ctrl Pts',(4.1817587479489,0.465308268502128,2.89185740177477));
#21924=CARTESIAN_POINT('Ctrl Pts',(4.16266015813344,0.536354908261444,2.59271405704707));
#21925=CARTESIAN_POINT('Ctrl Pts',(4.15265762140395,0.573560196368465,2.41375802693634));
#21926=CARTESIAN_POINT('Ctrl Pts',(4.27990542769405,0.0415912017479113,
3.58302567652478));
#21927=CARTESIAN_POINT('Ctrl Pts',(4.25574518298946,0.128851626852539,3.49496679687017));
#21928=CARTESIAN_POINT('Ctrl Pts',(4.21217417030772,0.286596632409413,3.29758018724282));
#21929=CARTESIAN_POINT('Ctrl Pts',(4.16134218460521,0.472536053380556,2.89573250617543));
#21930=CARTESIAN_POINT('Ctrl Pts',(4.14218738993462,0.543679227290343,2.59573641962871));
#21931=CARTESIAN_POINT('Ctrl Pts',(4.13215107098433,0.580950336455741,2.4164357799317));
#21932=CARTESIAN_POINT('Ctrl Pts',(4.2425246107023,0.0384093103467611,3.58977350532038));
#21933=CARTESIAN_POINT('Ctrl Pts',(4.21784750090365,0.125768723447587,3.50101955140993));
#21934=CARTESIAN_POINT('Ctrl Pts',(4.17340163251863,0.283772364998772,3.30214121155968));
#21935=CARTESIAN_POINT('Ctrl Pts',(4.12188632167338,0.469965279517223,2.89820958314819));
#21936=CARTESIAN_POINT('Ctrl Pts',(4.10266098140499,0.541170438724443,2.59763356171415));
#21937=CARTESIAN_POINT('Ctrl Pts',(4.09259095256892,0.578455090364732,2.41812014531828));
#21938=CARTESIAN_POINT('Ctrl Pts',(4.20079672067991,0.0123622460192512,
3.57509535012891));
#21939=CARTESIAN_POINT('Ctrl Pts',(4.17648320323078,0.0980364595359651,
3.48663488226387));
#21940=CARTESIAN_POINT('Ctrl Pts',(4.1329090360641,0.2524767319253,3.28946784706272));
#21941=CARTESIAN_POINT('Ctrl Pts',(4.08235693904747,0.435012022130954,2.8906393693344));
#21942=CARTESIAN_POINT('Ctrl Pts',(4.06323935395148,0.50581699413431,2.59179524992414));
#21943=CARTESIAN_POINT('Ctrl Pts',(4.0532219348772,0.542904670388583,2.41292428466811));
#21944=CARTESIAN_POINT('Ctrl Pts',(4.18838200131568,-0.00802902932684357,
3.55824631789071));
#21945=CARTESIAN_POINT('Ctrl Pts',(4.16482172696645,0.0761931109747066,
3.47052062622828));
#21946=CARTESIAN_POINT('Ctrl Pts',(4.12272687827244,0.227572559537098,3.2758060231306));
#21947=CARTESIAN_POINT('Ctrl Pts',(4.07356897734373,0.406942533188969,2.88269695569247));
#21948=CARTESIAN_POINT('Ctrl Pts',(4.05459109477352,0.477418672060344,2.58565061480296));
#21949=CARTESIAN_POINT('Ctrl Pts',(4.04464671888026,0.514335567712338,2.40746452010013));
#21950=CARTESIAN_POINT('Ctrl Pts',(4.1858850014514,-0.0182571874063626,
3.54880807404773));
#21951=CARTESIAN_POINT('Ctrl Pts',(4.16280303442141,0.0652367320815442,
3.46156265250184));
#21952=CARTESIAN_POINT('Ctrl Pts',(4.12161403444145,0.215078388014765,3.26830977903833));
#21953=CARTESIAN_POINT('Ctrl Pts',(4.07328088856278,0.392860332120455,2.87837605543618));
#21954=CARTESIAN_POINT('Ctrl Pts',(4.05438293677277,0.463168756286503,2.58230694074878));
#21955=CARTESIAN_POINT('Ctrl Pts',(4.04448133058357,0.5000000000037,2.4044944869251));
#21956=CARTESIAN_POINT('Ctrl Pts',(4.13468980447943,0.501507067233083,11.7463816858832));
#21957=CARTESIAN_POINT('Ctrl Pts',(4.12315670636567,0.500503082254402,11.7605952205767));
#21958=CARTESIAN_POINT('Ctrl Pts',(4.11159548058617,0.5,11.7748268489774));
#21959=CARTESIAN_POINT('Ctrl Pts',(4.1,0.5,11.7890187209237));
#21960=CARTESIAN_POINT('Ctrl Pts',(4.15241805382695,0.503050355590439,11.7637744947979));
#21961=CARTESIAN_POINT('Ctrl Pts',(4.14072380658156,0.501498211900196,11.7777465183035));
#21962=CARTESIAN_POINT('Ctrl Pts',(4.1289422172797,0.500510602421279,11.7917766549303));
#21963=CARTESIAN_POINT('Ctrl Pts',(4.11709141945523,0.5,11.8057761908248));
#21964=CARTESIAN_POINT('Ctrl Pts',(4.18493513822404,0.483966152642229,11.7938187431267));
#21965=CARTESIAN_POINT('Ctrl Pts',(4.17228908000075,0.482051425256797,11.80741030448));
#21966=CARTESIAN_POINT('Ctrl Pts',(4.15953538207889,0.480683792904307,11.8210795723414));
#21967=CARTESIAN_POINT('Ctrl Pts',(4.14667030106967,0.479896459182794,11.8347771301359));
#21968=CARTESIAN_POINT('Ctrl Pts',(4.19815579876099,0.440436692354107,11.8030020113162));
#21969=CARTESIAN_POINT('Ctrl Pts',(4.1845616929059,0.439020641370625,11.8169554560875));
#21970=CARTESIAN_POINT('Ctrl Pts',(4.17089559391198,0.438186472135287,11.830986356775));
#21971=CARTESIAN_POINT('Ctrl Pts',(4.15712386170588,0.437951958020513,11.8450264384616));
#21972=CARTESIAN_POINT('Ctrl Pts',(4.19894501008271,0.421808480679699,11.8021914830442));
#21973=CARTESIAN_POINT('Ctrl Pts',(4.18508246714534,0.420603698705282,11.8164284594574));
#21974=CARTESIAN_POINT('Ctrl Pts',(4.17114700318572,0.42,11.8307238382166));
#21975=CARTESIAN_POINT('Ctrl Pts',(4.15712386170588,0.42,11.8450264384616));
#21976=CARTESIAN_POINT('Origin',(4.03743041112843,1.49645215763755,11.737916375275));
#21977=CARTESIAN_POINT('',(4.15712386170589,0.42,11.8450264384616));
#21978=CARTESIAN_POINT('Origin',(4.1,0.42,11.7890187209237));
#21979=CARTESIAN_POINT('Ctrl Pts',(4.15712386170588,0.42,11.8450264384616));
#21980=CARTESIAN_POINT('Ctrl Pts',(4.17114700318572,0.42,11.8307238382166));
#21981=CARTESIAN_POINT('Ctrl Pts',(4.18508246714534,0.420603698705282,11.8164284594574));
#21982=CARTESIAN_POINT('Ctrl Pts',(4.19894501008271,0.421808480679699,11.8021914830442));
#21983=CARTESIAN_POINT('Ctrl Pts',(4.09999999999981,0.42,11.9026515720696));
#21984=CARTESIAN_POINT('Ctrl Pts',(4.11927627294066,0.42,11.8834820198546));
#21985=CARTESIAN_POINT('Ctrl Pts',(4.13827843210563,0.42,11.8642474273109));
#21986=CARTESIAN_POINT('Ctrl Pts',(4.15712386170585,0.42,11.8450264384616));
#21987=CARTESIAN_POINT('Ctrl Pts',(4.09999999999981,0.443935944027351,11.9026515720696));
#21988=CARTESIAN_POINT('Ctrl Pts',(4.11927735039401,0.44393594402735,11.8834809483665));
#21989=CARTESIAN_POINT('Ctrl Pts',(4.13827796583818,0.44393594402735,11.8642479028703));
#21990=CARTESIAN_POINT('Ctrl Pts',(4.15712386170585,0.44393594402735,11.8450264384616));
#21991=CARTESIAN_POINT('Ctrl Pts',(4.08582416465968,0.485360148657719,11.8883968170229));
#21992=CARTESIAN_POINT('Ctrl Pts',(4.10501545837473,0.485360148657719,11.8693117735566));
#21993=CARTESIAN_POINT('Ctrl Pts',(4.12396030833632,0.485360148657719,11.8501355018591));
#21994=CARTESIAN_POINT('Ctrl Pts',(4.14276896321521,0.485360148657719,11.8309520205925));
#21995=CARTESIAN_POINT('Ctrl Pts',(4.05624736761447,0.5,11.8586553600413));
#21996=CARTESIAN_POINT('Ctrl Pts',(4.07526199817245,0.5,11.8397460016581));
#21997=CARTESIAN_POINT('Ctrl Pts',(4.0940863606134,0.499999999999999,11.8206923301711));
#21998=CARTESIAN_POINT('Ctrl Pts',(4.11281856459138,0.499999999999999,11.8015868233495));
#21999=CARTESIAN_POINT('Ctrl Pts',(4.0435887019288,0.500000000000001,11.8459262210355));
#22000=CARTESIAN_POINT('Ctrl Pts',(4.06252783272241,0.5,11.8270919444215));
#22001=CARTESIAN_POINT('Ctrl Pts',(4.08130046851069,0.499999999999999,11.8080909041462));
#22002=CARTESIAN_POINT('Ctrl Pts',(4.09999999999996,0.499999999999999,11.7890187209237));
#22003=CARTESIAN_POINT('Ctrl Pts',(4.09999999999981,0.42,11.9026515720696));
#22004=CARTESIAN_POINT('Ctrl Pts',(4.11927627294066,0.42,11.8834820198546));
#22005=CARTESIAN_POINT('Ctrl Pts',(4.13827843210563,0.42,11.8642474273109));
#22006=CARTESIAN_POINT('Ctrl Pts',(4.15712386170585,0.42,11.8450264384616));
#22007=CARTESIAN_POINT('Origin',(-4.1,0.9,6.5));
#22008=CARTESIAN_POINT('Origin',(4.1,0.9,6.5));
#22009=CARTESIAN_POINT('Ctrl Pts',(-4.1,-1.17961196366423E-16,1.26933116532693));
#22010=CARTESIAN_POINT('Ctrl Pts',(-4.1,0.6,1.26933116532693));
#22011=CARTESIAN_POINT('Ctrl Pts',(-4.1,-1.17961196366423E-16,1.25328382445493));
#22012=CARTESIAN_POINT('Ctrl Pts',(-4.1,0.6,1.25328382445493));
#22013=CARTESIAN_POINT('Ctrl Pts',(-4.09002305366,-1.18393877442287E-16,
1.22124310128144));
#22014=CARTESIAN_POINT('Ctrl Pts',(-4.09002305366,0.6,1.22124310128144));
#22015=CARTESIAN_POINT('Ctrl Pts',(-4.06370099763855,-1.19535414655197E-16,
1.2004273196109));
#22016=CARTESIAN_POINT('Ctrl Pts',(-4.06370099763855,0.6,1.2004273196109));
#22017=CARTESIAN_POINT('Ctrl Pts',(-4.04872369693346,-1.20184951533693E-16,
1.19466558266346));
#22018=CARTESIAN_POINT('Ctrl Pts',(-4.04872369693346,0.6,1.19466558266346));
#22019=CARTESIAN_POINT('',(-4.05991477685645,0.499739255703113,1.19999999917294));
#22020=CARTESIAN_POINT('',(-4.04872369689169,0.425808996579714,1.19466558264739));
#22021=CARTESIAN_POINT('Ctrl Pts',(-4.05991477685645,0.499739255703113,
1.19999999917294));
#22022=CARTESIAN_POINT('Ctrl Pts',(-4.05991218030895,0.474962555580598,
1.19999833336884));
#22023=CARTESIAN_POINT('Ctrl Pts',(-4.05598720035336,0.449889989994391,
1.19748057630533));
#22024=CARTESIAN_POINT('Ctrl Pts',(-4.04884919779574,0.426222308101129,
1.19471395377504));
#22025=CARTESIAN_POINT('Ctrl Pts',(-4.04878657689504,0.426015612511084,
1.19468977245607));
#22026=CARTESIAN_POINT('Ctrl Pts',(-4.04872369693346,0.425808996580428,
1.19466558266346));
#22027=CARTESIAN_POINT('',(-4.04872369674582,0.083386841251265,1.19466558259128));
#22028=CARTESIAN_POINT('',(-4.04872369693346,0.425808996578679,1.19466558266346));
#22029=CARTESIAN_POINT('',(-4.05990543157618,0.0103940914527843,1.2000161521659));
#22030=CARTESIAN_POINT('Ctrl Pts',(-4.04872369693346,0.0833868071488794,
1.19466558266346));
#22031=CARTESIAN_POINT('Ctrl Pts',(-4.04880141653304,0.0831338820732446,
1.19469548123446));
#22032=CARTESIAN_POINT('Ctrl Pts',(-4.04887876782991,0.0828807524790114,
1.19472538210338));
#22033=CARTESIAN_POINT('Ctrl Pts',(-4.04895570042065,0.0826275846881222,
1.19475526183619));
#22034=CARTESIAN_POINT('Ctrl Pts',(-4.05194285075349,0.0727975472034251,
1.19591543664592));
#22035=CARTESIAN_POINT('Ctrl Pts',(-4.05436347175601,0.062687010783333,
1.19706577060194));
#22036=CARTESIAN_POINT('Ctrl Pts',(-4.05616232857013,0.0524346246710381,
1.19798196717376));
#22037=CARTESIAN_POINT('Ctrl Pts',(-4.05766721379084,0.043857697249005,
1.19874843767289));
#22038=CARTESIAN_POINT('Ctrl Pts',(-4.05873866585706,0.0351814943549607,
1.19935076478133));
#22039=CARTESIAN_POINT('Ctrl Pts',(-4.05934068619687,0.0264871938955073,
1.19969251928842));
#22040=CARTESIAN_POINT('Ctrl Pts',(-4.05971209465163,0.0211233606736628,
1.19990336019361));
#22041=CARTESIAN_POINT('Ctrl Pts',(-4.05990465511051,0.0157526393208265,
1.20001570300931));
#22042=CARTESIAN_POINT('Ctrl Pts',(-4.05990543157618,0.0103940914527843,
1.2000161521659));
#22043=CARTESIAN_POINT('Ctrl Pts',(-4.05987749605595,0.0103667322106564,
1.2));
#22044=CARTESIAN_POINT('Ctrl Pts',(-4.05987749605595,-1.19701232604091E-16,
1.2));
#22045=CARTESIAN_POINT('',(-4.1,-1.17961196366423E-16,1.26933116532693));
#22046=CARTESIAN_POINT('Ctrl Pts',(-4.05987749605677,0.499999999998992,
1.20000000000048));
#22047=CARTESIAN_POINT('Ctrl Pts',(-4.05987749605924,0.499960642899619,
1.2000000000019));
#22048=CARTESIAN_POINT('Ctrl Pts',(-4.05987749606638,0.499921285800245,
1.20000000000603));
#22049=CARTESIAN_POINT('Ctrl Pts',(-4.05987749606638,0.499834371718783,
1.20000000000603));
#22050=CARTESIAN_POINT('Ctrl Pts',(-4.0598774960573,0.499786814736695,1.20000000000078));
#22051=CARTESIAN_POINT('Ctrl Pts',(-4.05987749605608,0.499739257754606,
1.20000000000008));
#22052=CARTESIAN_POINT('Ctrl Pts',(-3.99749546403561,0.425808662442754,
1.12277288952037));
#22053=CARTESIAN_POINT('Ctrl Pts',(-3.99741900307445,0.440723737997244,
1.12056649920249));
#22054=CARTESIAN_POINT('Ctrl Pts',(-3.98925783839562,0.470755634285058,
1.11503732261258));
#22055=CARTESIAN_POINT('Ctrl Pts',(-3.9675518325465,0.493430715073795,1.10823883346629));
#22056=CARTESIAN_POINT('Ctrl Pts',(-3.95471619020724,0.501221222100498,
1.10539530861746));
#22057=CARTESIAN_POINT('Ctrl Pts',(-3.99790114239118,0.425808660873484,
1.13447013611379));
#22058=CARTESIAN_POINT('Ctrl Pts',(-3.99750830618296,0.440793786014735,
1.13248513004705));
#22059=CARTESIAN_POINT('Ctrl Pts',(-3.98845020395956,0.470610844054392,
1.12748649040356));
#22060=CARTESIAN_POINT('Ctrl Pts',(-3.96623032097253,0.491977735388082,
1.12119921453367));
#22061=CARTESIAN_POINT('Ctrl Pts',(-3.95352414898529,0.499091855265921,
1.11853791734794));
#22062=CARTESIAN_POINT('Ctrl Pts',(-4.00394093236138,0.42580863679589,1.15764284313999));
#22063=CARTESIAN_POINT('Ctrl Pts',(-4.00311371590923,0.441868527536911,
1.15623651208263));
#22064=CARTESIAN_POINT('Ctrl Pts',(-3.99226601725672,0.473314772733068,
1.15266048766281));
#22065=CARTESIAN_POINT('Ctrl Pts',(-3.9678344720362,0.49415299798259,1.14800581947106));
#22066=CARTESIAN_POINT('Ctrl Pts',(-3.95443818406651,0.500724592612001,
1.14600324261257));
#22067=CARTESIAN_POINT('Ctrl Pts',(-4.030731649599,0.425808530009691,1.18998205823776));
#22068=CARTESIAN_POINT('Ctrl Pts',(-4.02989922071593,0.446635090392047,
1.18960843288307));
#22069=CARTESIAN_POINT('Ctrl Pts',(-4.01635066531951,0.487487150831074,
1.18865363029091));
#22070=CARTESIAN_POINT('Ctrl Pts',(-3.98472526989518,0.514749615707155,
1.18735776371463));
#22071=CARTESIAN_POINT('Ctrl Pts',(-3.96711397890226,0.523367319030488,
1.18678687783788));
#22072=CARTESIAN_POINT('Ctrl Pts',(-4.05989190797289,0.425808413866688,
1.19999999986964));
#22073=CARTESIAN_POINT('Ctrl Pts',(-4.05957479390507,0.451819306042337,
1.20000581905524));
#22074=CARTESIAN_POINT('Ctrl Pts',(-4.04452566782116,0.503506810044701,
1.1999930990205));
#22075=CARTESIAN_POINT('Ctrl Pts',(-4.00584874486514,0.540239318982905,
1.19998873486588));
#22076=CARTESIAN_POINT('Ctrl Pts',(-3.98334410647183,0.552359067730285,
1.20000004480259));
#22077=CARTESIAN_POINT('Ctrl Pts',(-4.0774473938656,0.425808343825508,1.2));
#22078=CARTESIAN_POINT('Ctrl Pts',(-4.07744751278487,0.454945698277075,
1.2));
#22079=CARTESIAN_POINT('Ctrl Pts',(-4.06151247834833,0.513148697855926,
1.2));
#22080=CARTESIAN_POINT('Ctrl Pts',(-4.018597248821,0.555602008566458,1.2));
#22081=CARTESIAN_POINT('Ctrl Pts',(-3.99313806728599,0.569854029665374,
1.2));
#22082=CARTESIAN_POINT('',(-4.05989001907265,0.49975147889953,1.2));
#22083=CARTESIAN_POINT('',(-3.99749495051979,0.425816408369019,1.12277588236388));
#22084=CARTESIAN_POINT('Ctrl Pts',(-3.95658932953199,0.499868627057285,
1.10580990849871));
#22085=CARTESIAN_POINT('Ctrl Pts',(-3.96360335567988,0.495368835792349,
1.10742680652405));
#22086=CARTESIAN_POINT('Ctrl Pts',(-3.9700453297573,0.489837933598796,1.10919755141692));
#22087=CARTESIAN_POINT('Ctrl Pts',(-3.97558141221856,0.483497827408914,
1.11098169097766));
#22088=CARTESIAN_POINT('Ctrl Pts',(-3.97694492583232,0.481936286163253,
1.11142111697916));
#22089=CARTESIAN_POINT('Ctrl Pts',(-3.97825354811615,0.480325670155073,
1.11186112444703));
#22090=CARTESIAN_POINT('Ctrl Pts',(-3.97950242686639,0.478669304998406,
1.11229909409945));
#22091=CARTESIAN_POINT('Ctrl Pts',(-3.9818456702272,0.475561503976319,1.11312084679567));
#22092=CARTESIAN_POINT('Ctrl Pts',(-3.98397855806195,0.472292666317773,
1.11393570752481));
#22093=CARTESIAN_POINT('Ctrl Pts',(-3.98588913947764,0.468903558492556,
1.11472661791731));
#22094=CARTESIAN_POINT('Ctrl Pts',(-3.98989952307469,0.46178969131097,1.11638676913556));
#22095=CARTESIAN_POINT('Ctrl Pts',(-3.99293173507827,0.454148826888769,
1.11794762353363));
#22096=CARTESIAN_POINT('Ctrl Pts',(-3.99489269458943,0.446280500947391,
1.11938837303024));
#22097=CARTESIAN_POINT('Ctrl Pts',(-3.99656653497968,0.439564236950421,
1.12061817134373));
#22098=CARTESIAN_POINT('Ctrl Pts',(-3.997459613396,0.432681349848232,1.12175934133402));
#22099=CARTESIAN_POINT('Ctrl Pts',(-3.99749495051979,0.425816408369019,
1.12277588236388));
#22100=CARTESIAN_POINT('Origin',(-4.07744739386693,0.425808996578679,1.12));
#22101=CARTESIAN_POINT('Origin',(4.1,0.,1.2));
#22102=CARTESIAN_POINT('Origin',(-3.91744442112685,0.0831608766898327,1.20000000000032));
#22103=CARTESIAN_POINT('Origin',(4.1,0.,1.2));
#22104=CARTESIAN_POINT('Origin',(-4.1,0.,1.2));
#22105=CARTESIAN_POINT('Ctrl Pts',(-4.04872369777422,0.425808996578679,
1.1946655829869));
#22106=CARTESIAN_POINT('Ctrl Pts',(-4.04872369777422,0.0149024691460445,
1.1946655829869));
#22107=CARTESIAN_POINT('Ctrl Pts',(-4.03417809695481,0.425808996578679,
1.18906992029053));
#22108=CARTESIAN_POINT('Ctrl Pts',(-4.03417809695481,0.0149024691460445,
1.18906992029053));
#22109=CARTESIAN_POINT('Ctrl Pts',(-4.00850642174527,0.425808996578679,
1.16912611569929));
#22110=CARTESIAN_POINT('Ctrl Pts',(-4.00850642174527,0.0149024691460445,
1.16912611569929));
#22111=CARTESIAN_POINT('Ctrl Pts',(-3.9980360657665,0.425808996578679,1.1383501202594));
#22112=CARTESIAN_POINT('Ctrl Pts',(-3.9980360657665,0.0149024691460445,
1.1383501202594));
#22113=CARTESIAN_POINT('Ctrl Pts',(-3.99749552679662,0.425808996578679,
1.12277469853698));
#22114=CARTESIAN_POINT('Ctrl Pts',(-3.99749552679662,0.0149024691460445,
1.12277469853698));
#22115=CARTESIAN_POINT('',(-3.99749552930111,0.08338687277103,1.12277470064702));
#22116=CARTESIAN_POINT('',(-3.99749552679662,0.425808996578679,1.12277469853698));
#22117=CARTESIAN_POINT('Origin',(-4.07744739386693,0.0833868903848169,1.12));
#22118=CARTESIAN_POINT('Ctrl Pts',(-3.91780246449684,0.00300376307205705,
1.1265306122449));
#22119=CARTESIAN_POINT('Ctrl Pts',(-3.93576025037965,0.00296202866725982,
1.12704015241118));
#22120=CARTESIAN_POINT('Ctrl Pts',(-3.96555870066537,0.0134692513665733,
1.12719733238845));
#22121=CARTESIAN_POINT('Ctrl Pts',(-3.99216195295547,0.0472952052376165,
1.12560552323969));
#22122=CARTESIAN_POINT('Ctrl Pts',(-3.99753261370091,0.0713291405834686,
1.12384334179573));
#22123=CARTESIAN_POINT('Ctrl Pts',(-3.99749552679548,0.0833868069155861,
1.12277469850418));
#22124=CARTESIAN_POINT('Ctrl Pts',(-3.91780246449684,0.00115146656907868,
1.14914551409197));
#22125=CARTESIAN_POINT('Ctrl Pts',(-3.93613149057372,0.000969237935352311,
1.14954546365303));
#22126=CARTESIAN_POINT('Ctrl Pts',(-3.96686365991627,0.0118424389758149,
1.14966515106411));
#22127=CARTESIAN_POINT('Ctrl Pts',(-3.99366630482309,0.0466900216982605,
1.14841701955119));
#22128=CARTESIAN_POINT('Ctrl Pts',(-3.99865916988022,0.0712429843090682,
1.14702096166311));
#22129=CARTESIAN_POINT('Ctrl Pts',(-3.99830738013179,0.0833868069192833,
1.14616793922152));
#22130=CARTESIAN_POINT('Ctrl Pts',(-3.91780246449684,-0.0199489376043931,
1.18690998941925));
#22131=CARTESIAN_POINT('Ctrl Pts',(-3.94093194698948,-0.0201921648247794,
1.18702695697395));
#22132=CARTESIAN_POINT('Ctrl Pts',(-3.97951730409342,-0.00666843160596345,
1.18706431777373));
#22133=CARTESIAN_POINT('Ctrl Pts',(-4.01329298538155,0.0373349474711074,
1.18669970306998));
#22134=CARTESIAN_POINT('Ctrl Pts',(-4.01937761864352,0.0681485596815143,
1.18628923992153));
#22135=CARTESIAN_POINT('Ctrl Pts',(-4.01886907034338,0.0833868070129213,
1.18603556032283));
#22136=CARTESIAN_POINT('Ctrl Pts',(-3.91780246449684,-0.0597112616448693,
1.2));
#22137=CARTESIAN_POINT('Ctrl Pts',(-3.94986432816707,-0.0597837540420209,
1.19999893991423));
#22138=CARTESIAN_POINT('Ctrl Pts',(-4.00315043136341,-0.0410040343800299,
1.19999296250002));
#22139=CARTESIAN_POINT('Ctrl Pts',(-4.05061466200189,0.0193832087506108,
1.19999621445595));
#22140=CARTESIAN_POINT('Ctrl Pts',(-4.0600434134887,0.0620661620497311,
1.19999748313998));
#22141=CARTESIAN_POINT('Ctrl Pts',(-4.0598919008628,0.0833868071997395,
1.2));
#22142=CARTESIAN_POINT('Ctrl Pts',(-3.91780246449684,-0.0767292357659823,
1.2));
#22143=CARTESIAN_POINT('Ctrl Pts',(-3.95368317895231,-0.0767292357659822,
1.2));
#22144=CARTESIAN_POINT('Ctrl Pts',(-4.01326936269294,-0.0556897214928556,
1.2));
#22145=CARTESIAN_POINT('Ctrl Pts',(-4.06658466073547,0.0117033247253155,
1.2));
#22146=CARTESIAN_POINT('Ctrl Pts',(-4.07744739397586,0.0594663309760329,
1.2));
#22147=CARTESIAN_POINT('Ctrl Pts',(-4.07744739386693,0.0833868072796873,
1.2));
#22148=CARTESIAN_POINT('Ctrl Pts',(-3.99749552679548,0.0833868069155861,
1.12277469850418));
#22149=CARTESIAN_POINT('Ctrl Pts',(-3.99753261370091,0.0713291405834686,
1.12384334179573));
#22150=CARTESIAN_POINT('Ctrl Pts',(-3.99216195295547,0.0472952052376165,
1.12560552323969));
#22151=CARTESIAN_POINT('Ctrl Pts',(-3.96555870066537,0.0134692513665733,
1.12719733238845));
#22152=CARTESIAN_POINT('Ctrl Pts',(-3.93576025037965,0.00296202866725982,
1.12704015241118));
#22153=CARTESIAN_POINT('Ctrl Pts',(-3.91780246449684,0.00300376307205705,
1.1265306122449));
#22154=CARTESIAN_POINT('Ctrl Pts',(-3.9199627360209,0.5,1.2));
#22155=CARTESIAN_POINT('Ctrl Pts',(-3.91859147059112,0.5,1.16263028970545));
#22156=CARTESIAN_POINT('Ctrl Pts',(-3.91708574929206,0.505271087920178,
1.12526784524295));
#22157=CARTESIAN_POINT('Ctrl Pts',(-3.91539217619132,0.515604560956495,
1.08936480468426));
#22158=CARTESIAN_POINT('Ctrl Pts',(-3.94388749707654,0.5,1.1992684093282));
#22159=CARTESIAN_POINT('Ctrl Pts',(-3.94255922360763,0.500070437490442,
1.16187406103769));
#22160=CARTESIAN_POINT('Ctrl Pts',(-3.94110090415831,0.505425615700251,
1.12441169682652));
#22161=CARTESIAN_POINT('Ctrl Pts',(-3.93947649219532,0.515856199601771,
1.08849050110252));
#22162=CARTESIAN_POINT('Ctrl Pts',(-3.98530151225888,0.479904100518027,
1.19800201811456));
#22163=CARTESIAN_POINT('Ctrl Pts',(-3.98404149316127,0.480012713029783,
1.15861674257998));
#22164=CARTESIAN_POINT('Ctrl Pts',(-3.98266889977967,0.485680432111213,
1.11922733796895));
#22165=CARTESIAN_POINT('Ctrl Pts',(-3.98115396081513,0.496695221132957,
1.08133736541183));
#22166=CARTESIAN_POINT('Ctrl Pts',(-3.99992535969115,0.437951958020513,
1.19755483829351));
#22167=CARTESIAN_POINT('Ctrl Pts',(-3.99860101206523,0.437984309190483,
1.15422623809305));
#22168=CARTESIAN_POINT('Ctrl Pts',(-3.9971480185017,0.444112318340178,1.11085352703736));
#22169=CARTESIAN_POINT('Ctrl Pts',(-3.99552667887377,0.456097443939778,
1.06908769510471));
#22170=CARTESIAN_POINT('Ctrl Pts',(-3.99992535969115,0.42,1.19755483829351));
#22171=CARTESIAN_POINT('Ctrl Pts',(-3.99854929471383,0.42,1.15255422928056));
#22172=CARTESIAN_POINT('Ctrl Pts',(-3.99703626487076,0.426325305504265,
1.10749080430861));
#22173=CARTESIAN_POINT('Ctrl Pts',(-3.99533043997794,0.438725473147794,
1.06409547620398));
#22174=CARTESIAN_POINT('',(-3.91539217619132,0.515604560956495,1.08936480468426));
#22175=CARTESIAN_POINT('Ctrl Pts',(-3.9199627360209,0.5,1.2));
#22176=CARTESIAN_POINT('Ctrl Pts',(-3.91859147059112,0.5,1.16263028970545));
#22177=CARTESIAN_POINT('Ctrl Pts',(-3.91708574929206,0.505271087920178,
1.12526784524295));
#22178=CARTESIAN_POINT('Ctrl Pts',(-3.91539217619132,0.515604560956495,
1.08936480468426));
#22179=CARTESIAN_POINT('',(-3.99533043998062,0.438725473135619,1.06409547624199));
#22180=CARTESIAN_POINT('Origin',(-3.91539217619132,0.438725473147794,1.06723776562112));
#22181=CARTESIAN_POINT('Origin',(-3.98259956593766,0.90718624733336,1.19842150873233));
#22182=CARTESIAN_POINT('Ctrl Pts',(-3.99642658272504,0.44384037918325,1.04839302148096));
#22183=CARTESIAN_POINT('Ctrl Pts',(-3.99548774892012,0.44179052725272,1.05345171612862));
#22184=CARTESIAN_POINT('Ctrl Pts',(-3.99511937952587,0.440067061234499,
1.05872620436003));
#22185=CARTESIAN_POINT('Ctrl Pts',(-3.99533043997794,0.438725473147794,
1.06409547620398));
#22186=CARTESIAN_POINT('Ctrl Pts',(-3.99657534106213,0.466413555729877,
1.05663619619587));
#22187=CARTESIAN_POINT('Ctrl Pts',(-3.99579563594237,0.464642772895823,
1.06121182233657));
#22188=CARTESIAN_POINT('Ctrl Pts',(-3.99546531235558,0.463114794501233,
1.06596374902201));
#22189=CARTESIAN_POINT('Ctrl Pts',(-3.99559209183904,0.461888100870439,
1.07075176807162));
#22190=CARTESIAN_POINT('Ctrl Pts',(-3.97685954371716,0.50677512210794,1.06772025968478));
#22191=CARTESIAN_POINT('Ctrl Pts',(-3.97592643102433,0.505042447302577,
1.07279579186463));
#22192=CARTESIAN_POINT('Ctrl Pts',(-3.97553510541324,0.503447592943445,
1.07789416781835));
#22193=CARTESIAN_POINT('Ctrl Pts',(-3.97566885922969,0.501970835818075,
1.08307138584241));
#22194=CARTESIAN_POINT('Ctrl Pts',(-3.93534760874179,0.523078681693286,
1.06606105089355));
#22195=CARTESIAN_POINT('Ctrl Pts',(-3.93375572569525,0.520454986989424,
1.07347568016643));
#22196=CARTESIAN_POINT('Ctrl Pts',(-3.93312277810201,0.518010117677892,
1.08106604861408));
#22197=CARTESIAN_POINT('Ctrl Pts',(-3.93345541319432,0.515793289940452,
1.08870907699796));
#22198=CARTESIAN_POINT('Ctrl Pts',(-3.91758436243186,0.524122951685319,
1.06319194267061));
#22199=CARTESIAN_POINT('Ctrl Pts',(-3.91571147604617,0.521017369008945,
1.07172446094826));
#22200=CARTESIAN_POINT('Ctrl Pts',(-3.91497483111678,0.518151025630959,
1.08051726386549));
#22201=CARTESIAN_POINT('Ctrl Pts',(-3.91539217619132,0.515604560956495,
1.08936480468426));
#22202=CARTESIAN_POINT('',(-3.91758436243186,0.524122951685478,1.06319194267017));
#22203=CARTESIAN_POINT('Origin',(-4.02330412568762,0.546067694126366,1.09055042993106));
#22204=CARTESIAN_POINT('',(-3.99642658272504,0.443840379183073,1.04839302148084));
#22205=CARTESIAN_POINT('Origin',(-3.91758436243186,0.448947542022383,1.03583033120473));
#22206=CARTESIAN_POINT('Origin',(-4.05033769991219,0.474821566285832,1.0709707385159));
#22207=CARTESIAN_POINT('Ctrl Pts',(-2.87962408435655,0.450506079619966,
1.031548284348));
#22208=CARTESIAN_POINT('Ctrl Pts',(-2.88706985293045,0.495141499993335,
0.908913474764299));
#22209=CARTESIAN_POINT('Ctrl Pts',(-2.89830085190713,0.584802360144796,
0.662572286089282));
#22210=CARTESIAN_POINT('Ctrl Pts',(-2.92033299964242,0.698627090634836,
0.349841409292389));
#22211=CARTESIAN_POINT('Ctrl Pts',(-2.97414103030473,0.773765776974324,
0.143399565247164));
#22212=CARTESIAN_POINT('Ctrl Pts',(-3.02113993649286,0.805536061367637,
0.0561114262668838));
#22213=CARTESIAN_POINT('Ctrl Pts',(-3.04982829439264,0.821130183736138,
0.0132669271832156));
#22214=CARTESIAN_POINT('Ctrl Pts',(-3.09662700629875,0.839948596127357,
-0.0384362359316435));
#22215=CARTESIAN_POINT('Ctrl Pts',(-3.20078875895428,0.862136521381471,
-0.0993970595518691));
#22216=CARTESIAN_POINT('Ctrl Pts',(-3.33746877961289,0.868528535167059,
-0.116958973092616));
#22217=CARTESIAN_POINT('Ctrl Pts',(-3.48441332396274,0.862274358796636,
-0.0997757647375922));
#22218=CARTESIAN_POINT('Ctrl Pts',(-3.61382529190729,0.84783025941325,-0.0600909278373817));
#22219=CARTESIAN_POINT('Ctrl Pts',(-3.72587585229285,0.825571951670826,
0.0010632700802009));
#22220=CARTESIAN_POINT('Ctrl Pts',(-3.84060061269669,0.786540385741618,
0.108301616116654));
#22221=CARTESIAN_POINT('Ctrl Pts',(-3.90217403729928,0.738739795172645,
0.239632659341502));
#22222=CARTESIAN_POINT('Ctrl Pts',(-3.93815958139645,0.692207019220546,
0.367480410534435));
#22223=CARTESIAN_POINT('Ctrl Pts',(-3.96327795090667,0.645584422821145,
0.495574941378137));
#22224=CARTESIAN_POINT('Ctrl Pts',(-3.988190288963,0.56591300759988,0.714470355674555));
#22225=CARTESIAN_POINT('Ctrl Pts',(-3.99552195740115,0.49833669404846,0.900134751247067));
#22226=CARTESIAN_POINT('Ctrl Pts',(-3.99961373290197,0.453243799876031,
1.02402645976367));
#22227=CARTESIAN_POINT('Ctrl Pts',(-2.87962408435655,0.472998509594012,
1.03973485935487));
#22228=CARTESIAN_POINT('Ctrl Pts',(-2.88706972471758,0.517633161364987,
0.917102161488891));
#22229=CARTESIAN_POINT('Ctrl Pts',(-2.89829720228894,0.607291613669455,
0.670767588319117));
#22230=CARTESIAN_POINT('Ctrl Pts',(-2.92029355131071,0.72110022589572,0.358080996087986));
#22231=CARTESIAN_POINT('Ctrl Pts',(-2.9740705062357,0.796239021043994,0.151638853093076));
#22232=CARTESIAN_POINT('Ctrl Pts',(-3.02108238010733,0.828022541036071,
0.0643143496040615));
#22233=CARTESIAN_POINT('Ctrl Pts',(-3.04978340300042,0.843624632566539,
0.0214479554278384));
#22234=CARTESIAN_POINT('Ctrl Pts',(-3.096592410354,0.862452712083289,-0.0302817678961312));
#22235=CARTESIAN_POINT('Ctrl Pts',(-3.20082556389089,0.884655834508208,
-0.0912843453999811));
#22236=CARTESIAN_POINT('Ctrl Pts',(-3.33748082734155,0.891040050440225,
-0.108824834514122));
#22237=CARTESIAN_POINT('Ctrl Pts',(-3.48443609473601,0.884781674811433,
-0.0916300887915507));
#22238=CARTESIAN_POINT('Ctrl Pts',(-3.61385184322647,0.870335933837343,
-0.051940741657948));
#22239=CARTESIAN_POINT('Ctrl Pts',(-3.72590622690082,0.84807391828105,0.00922364339451449));
#22240=CARTESIAN_POINT('Ctrl Pts',(-3.84068731705383,0.809022827244695,
0.116515634221966));
#22241=CARTESIAN_POINT('Ctrl Pts',(-3.90219876188619,0.761230212281178,
0.247824764650918));
#22242=CARTESIAN_POINT('Ctrl Pts',(-3.93818741165077,0.714691426981262,
0.375689026391285));
#22243=CARTESIAN_POINT('Ctrl Pts',(-3.96329567170119,0.668068278176157,
0.503785074957183));
#22244=CARTESIAN_POINT('Ctrl Pts',(-3.98820643523393,0.588393873042911,
0.722688703969256));
#22245=CARTESIAN_POINT('Ctrl Pts',(-3.99552190872555,0.520829660445818,
0.908319852442999));
#22246=CARTESIAN_POINT('Ctrl Pts',(-3.99961373290197,0.475736229850077,
1.03221303477054));
#22247=CARTESIAN_POINT('Ctrl Pts',(-2.89968712497522,0.511541907490879,
1.05498163579157));
#22248=CARTESIAN_POINT('Ctrl Pts',(-2.90714300575565,0.556237947877504,
0.932180274090282));
#22249=CARTESIAN_POINT('Ctrl Pts',(-2.9183967840909,0.645941625439093,0.685721445547777));
#22250=CARTESIAN_POINT('Ctrl Pts',(-2.94035557430995,0.759332481137342,
0.374182629944202));
#22251=CARTESIAN_POINT('Ctrl Pts',(-2.99348007913718,0.833071760243458,
0.171585625673285));
#22252=CARTESIAN_POINT('Ctrl Pts',(-3.03867906787114,0.863582657829508,
0.0877576235083202));
#22253=CARTESIAN_POINT('Ctrl Pts',(-3.06601334262966,0.878445385572726,
0.0469226146423277));
#22254=CARTESIAN_POINT('Ctrl Pts',(-3.11011593586453,0.896118505150049,
-0.00163388232768946));
#22255=CARTESIAN_POINT('Ctrl Pts',(-3.20700850686946,0.916796373054912,
-0.058445857478767));
#22256=CARTESIAN_POINT('Ctrl Pts',(-3.33712049077176,0.923017161010362,
-0.0755373319175819));
#22257=CARTESIAN_POINT('Ctrl Pts',(-3.48002463105222,0.916949465597777,
-0.0588664757833766));
#22258=CARTESIAN_POINT('Ctrl Pts',(-3.60584634368539,0.9028960189969,-0.0202549485819569));
#22259=CARTESIAN_POINT('Ctrl Pts',(-3.71361989979722,0.881446144267468,
0.0386780978872879));
#22260=CARTESIAN_POINT('Ctrl Pts',(-3.82318598076471,0.844187728138539,
0.141044754886167));
#22261=CARTESIAN_POINT('Ctrl Pts',(-3.88312165251306,0.797918873417564,
0.26816738845607));
#22262=CARTESIAN_POINT('Ctrl Pts',(-3.91850643383034,0.752156053042667,
0.393899704086659));
#22263=CARTESIAN_POINT('Ctrl Pts',(-3.94333901415249,0.70609879889664,0.52044096985495));
#22264=CARTESIAN_POINT('Ctrl Pts',(-3.96810955084563,0.626950470316382,
0.737899215416785));
#22265=CARTESIAN_POINT('Ctrl Pts',(-3.97543979982371,0.559508505904016,
0.923194489763422));
#22266=CARTESIAN_POINT('Ctrl Pts',(-3.97952773625812,0.514457919677186,
1.04696995815483));
#22267=CARTESIAN_POINT('Ctrl Pts',(-2.9415713861866,0.524472685894761,1.06223105582735));
#22268=CARTESIAN_POINT('Ctrl Pts',(-2.94904828921471,0.569294749116044,
0.93908344923351));
#22269=CARTESIAN_POINT('Ctrl Pts',(-2.96034719658121,0.659086154935045,
0.692383589284719));
#22270=CARTESIAN_POINT('Ctrl Pts',(-2.98212818142746,0.77156013548705,0.383363867441909));
#22271=CARTESIAN_POINT('Ctrl Pts',(-3.03380432716909,0.84237804114237,0.188793270760848));
#22272=CARTESIAN_POINT('Ctrl Pts',(-3.07525468269643,0.870268919584971,
0.112163712031047));
#22273=CARTESIAN_POINT('Ctrl Pts',(-3.0997708540493,0.883610253909479,0.0755086972290682));
#22274=CARTESIAN_POINT('Ctrl Pts',(-3.13825203413196,0.898899082374074,
0.0335029862526778));
#22275=CARTESIAN_POINT('Ctrl Pts',(-3.22001841149168,0.916434974427251,
-0.0146764811934207));
#22276=CARTESIAN_POINT('Ctrl Pts',(-3.33640169127941,0.922292933767806,
-0.0307710922056808));
#22277=CARTESIAN_POINT('Ctrl Pts',(-3.47087833872087,0.916611649236276,
-0.0151618912418065));
#22278=CARTESIAN_POINT('Ctrl Pts',(-3.58920752111338,0.903372611293106,
0.0212120665623573));
#22279=CARTESIAN_POINT('Ctrl Pts',(-3.68805489678656,0.883607893498353,
0.0755151824053357));
#22280=CARTESIAN_POINT('Ctrl Pts',(-3.78689035517007,0.85003771211992,0.167748497709577));
#22281=CARTESIAN_POINT('Ctrl Pts',(-3.84336430236995,0.8069720537749,0.286070421566467));
#22282=CARTESIAN_POINT('Ctrl Pts',(-3.87749705111799,0.762812478046415,
0.407397858733175));
#22283=CARTESIAN_POINT('Ctrl Pts',(-3.90172604413317,0.717935070365446,
0.530697522980297));
#22284=CARTESIAN_POINT('Ctrl Pts',(-3.92619946695966,0.639876694845063,
0.745161147121859));
#22285=CARTESIAN_POINT('Ctrl Pts',(-3.93351559588986,0.572723538474725,
0.929662927894466));
#22286=CARTESIAN_POINT('Ctrl Pts',(-3.93759555129614,0.527760906158602,
1.05319674490226));
#22287=CARTESIAN_POINT('Ctrl Pts',(-2.9594941977123,0.524122950641471,1.06319194553855));
#22288=CARTESIAN_POINT('Ctrl Pts',(-2.96698008492688,0.568998871692987,
0.939896365772286));
#22289=CARTESIAN_POINT('Ctrl Pts',(-2.9782979876664,0.658827601540248,0.693093958898646));
#22290=CARTESIAN_POINT('Ctrl Pts',(-2.99999967569416,0.770907793456571,
0.38515616244041));
#22291=CARTESIAN_POINT('Ctrl Pts',(-3.05105326213358,0.840475615777891,
0.194020141491951));
#22292=CARTESIAN_POINT('Ctrl Pts',(-3.09090069290084,0.867246541900823,
0.12046762647131));
#22293=CARTESIAN_POINT('Ctrl Pts',(-3.11421209795167,0.879937567446779,
0.0855993203540729));
#22294=CARTESIAN_POINT('Ctrl Pts',(-3.15028872702707,0.894206994493787,
0.0463943917538627));
#22295=CARTESIAN_POINT('Ctrl Pts',(-3.22558881811219,0.910399758249608,
0.00190513897618206));
#22296=CARTESIAN_POINT('Ctrl Pts',(-3.3360951886178,0.916101759009581,-0.0137609793575587));
#22297=CARTESIAN_POINT('Ctrl Pts',(-3.46696656599506,0.910585447910795,
0.00139496082504257));
#22298=CARTESIAN_POINT('Ctrl Pts',(-3.58208993795251,0.897694758584722,
0.0368118386696318));
#22299=CARTESIAN_POINT('Ctrl Pts',(-3.67711802975361,0.878650808373231,
0.089134661852922));
#22300=CARTESIAN_POINT('Ctrl Pts',(-3.77136677090444,0.846657118193748,
0.177036603186079));
#22301=CARTESIAN_POINT('Ctrl Pts',(-3.82635384144273,0.804962864100056,
0.2915906248295));
#22302=CARTESIAN_POINT('Ctrl Pts',(-3.85995110804723,0.761488798159762,
0.411034639332341));
#22303=CARTESIAN_POINT('Ctrl Pts',(-3.88392091137359,0.717116212326026,
0.532947316953341));
#22304=CARTESIAN_POINT('Ctrl Pts',(-3.90826705411741,0.639523973437174,
0.746130241225391));
#22305=CARTESIAN_POINT('Ctrl Pts',(-3.91557568799506,0.572495487342456,
0.930289493230857));
#22306=CARTESIAN_POINT('Ctrl Pts',(-3.91965223258409,0.527570443506261,
1.05372003673881));
#22307=CARTESIAN_POINT('',(-2.88729704002952,0.500000000328437,0.895564854801195));
#22308=CARTESIAN_POINT('Ctrl Pts',(-2.88715652162958,0.500000000004701,
0.898556263621882));
#22309=CARTESIAN_POINT('Ctrl Pts',(-2.88720339858619,0.499999999361646,
0.897559129110793));
#22310=CARTESIAN_POINT('Ctrl Pts',(-2.88725023764408,0.499999999368085,
0.896561992815236));
#22311=CARTESIAN_POINT('Ctrl Pts',(-2.88729704002392,0.500000000000096,
0.895564854800933));
#22312=CARTESIAN_POINT('',(-3.99961373290197,0.453243799876042,1.02402645976365));
#22313=CARTESIAN_POINT('Ctrl Pts',(-2.88729704002952,0.500000000328437,
0.895564854801195));
#22314=CARTESIAN_POINT('Ctrl Pts',(-2.88906965512591,0.512137783677987,
0.862216569126075));
#22315=CARTESIAN_POINT('Ctrl Pts',(-2.89078934467508,0.52428817848214,0.828833633764207));
#22316=CARTESIAN_POINT('Ctrl Pts',(-2.89253615105346,0.536464830009127,
0.795378558649242));
#22317=CARTESIAN_POINT('Ctrl Pts',(-2.89381761055983,0.545397637931103,
0.770835870591288));
#22318=CARTESIAN_POINT('Ctrl Pts',(-2.89511395407221,0.554344395792644,
0.746254855389374));
#22319=CARTESIAN_POINT('Ctrl Pts',(-2.89646663063639,0.563304917550206,
0.721636024193941));
#22320=CARTESIAN_POINT('Ctrl Pts',(-2.89734121067155,0.569098389279699,
0.705718591436909));
#22321=CARTESIAN_POINT('Ctrl Pts',(-2.89823953190499,0.574897507579613,
0.689785644855149));
#22322=CARTESIAN_POINT('Ctrl Pts',(-2.89917526582012,0.580700853337509,
0.673841083428042));
#22323=CARTESIAN_POINT('Ctrl Pts',(-2.89971479707597,0.584046982375097,
0.664647669454688));
#22324=CARTESIAN_POINT('Ctrl Pts',(-2.90026689066681,0.587394941514684,
0.655449227317415));
#22325=CARTESIAN_POINT('Ctrl Pts',(-2.90083359406858,0.590739208495519,
0.646260929302945));
#22326=CARTESIAN_POINT('Ctrl Pts',(-2.90240528294206,0.600014161120397,
0.620778206399581));
#22327=CARTESIAN_POINT('Ctrl Pts',(-2.90408968664164,0.609274396150569,
0.595335919755338));
#22328=CARTESIAN_POINT('Ctrl Pts',(-2.90597098506406,0.618563414427602,
0.56981455179029));
#22329=CARTESIAN_POINT('Ctrl Pts',(-2.90768551128761,0.627028985459456,
0.546555586537481));
#22330=CARTESIAN_POINT('Ctrl Pts',(-2.90956331501266,0.635518588868317,
0.523230592871512));
#22331=CARTESIAN_POINT('Ctrl Pts',(-2.91168894974053,0.644054012119428,
0.499779710223596));
#22332=CARTESIAN_POINT('Ctrl Pts',(-2.91366705538124,0.651997036693419,
0.477956429564381));
#22333=CARTESIAN_POINT('Ctrl Pts',(-2.91585960531524,0.659979843146529,
0.456023849090585));
#22334=CARTESIAN_POINT('Ctrl Pts',(-2.9183567293491,0.668008257167524,0.43396596285387));
#22335=CARTESIAN_POINT('Ctrl Pts',(-2.92077093488793,0.675770082905733,
0.412640521904397));
#22336=CARTESIAN_POINT('Ctrl Pts',(-2.92346955517842,0.683574699361931,
0.391197514423489));
#22337=CARTESIAN_POINT('Ctrl Pts',(-2.92655871267213,0.691414026493946,
0.369659140144562));
#22338=CARTESIAN_POINT('Ctrl Pts',(-2.92955133399416,0.699008374653085,
0.348793840061851));
#22339=CARTESIAN_POINT('Ctrl Pts',(-2.93291025093034,0.70663544629957,0.327838632936568));
#22340=CARTESIAN_POINT('Ctrl Pts',(-2.9367590113504,0.714272904796163,0.306854888175159));
#22341=CARTESIAN_POINT('Ctrl Pts',(-2.93885689266313,0.718435928655275,
0.295417074125599));
#22342=CARTESIAN_POINT('Ctrl Pts',(-2.94110120212796,0.722602382083406,
0.283969837412598));
#22343=CARTESIAN_POINT('Ctrl Pts',(-2.94351389087306,0.726763244431991,
0.272537962064403));
#22344=CARTESIAN_POINT('Ctrl Pts',(-2.94661866850662,0.732117665876711,
0.25782681005079));
#22345=CARTESIAN_POINT('Ctrl Pts',(-2.95000336005515,0.737468874357662,
0.243124485582583));
#22346=CARTESIAN_POINT('Ctrl Pts',(-2.95376109050901,0.742841037534281,
0.228364588561198));
#22347=CARTESIAN_POINT('Ctrl Pts',(-2.95729395081782,0.747891719665993,
0.214487953451476));
#22348=CARTESIAN_POINT('Ctrl Pts',(-2.96115642045917,0.752961014265982,
0.200560181005442));
#22349=CARTESIAN_POINT('Ctrl Pts',(-2.96544977445503,0.758055775150981,
0.186562440516388));
#22350=CARTESIAN_POINT('Ctrl Pts',(-2.96952289573906,0.762889194202305,
0.173282730814113));
#22351=CARTESIAN_POINT('Ctrl Pts',(-2.97398373546562,0.767745620448862,
0.159939809362452));
#22352=CARTESIAN_POINT('Ctrl Pts',(-2.97894249446087,0.772617350031455,
0.14655484234059));
#22353=CARTESIAN_POINT('Ctrl Pts',(-2.98370439589809,0.777295677032889,
0.133701244543323));
#22354=CARTESIAN_POINT('Ctrl Pts',(-2.98892541390208,0.781988195935133,
0.120808654819044));
#22355=CARTESIAN_POINT('Ctrl Pts',(-2.99472675076426,0.78667401504634,0.107934472619355));
#22356=CARTESIAN_POINT('Ctrl Pts',(-2.99762127725687,0.789011963674251,
0.101511011556323));
#22357=CARTESIAN_POINT('Ctrl Pts',(-3.00066060816065,0.791347981754224,
0.0950928546301593));
#22358=CARTESIAN_POINT('Ctrl Pts',(-3.00386228892887,0.793678090217947,
0.0886909342412002));
#22359=CARTESIAN_POINT('Ctrl Pts',(-3.00948082270016,0.797767127833499,
0.0774563957251705));
#22360=CARTESIAN_POINT('Ctrl Pts',(-3.01561191556197,0.801849220402643,
0.0662409385673262));
#22361=CARTESIAN_POINT('Ctrl Pts',(-3.0223851741983,0.805900395663406,0.055110426016126));
#22362=CARTESIAN_POINT('Ctrl Pts',(-3.02782556918369,0.809154367607626,
0.0461702115758429));
#22363=CARTESIAN_POINT('Ctrl Pts',(-3.03368223245992,0.812389485062581,
0.0372817994190711));
#22364=CARTESIAN_POINT('Ctrl Pts',(-3.0400481045814,0.81559153492332,0.0284842397307234));
#22365=CARTESIAN_POINT('Ctrl Pts',(-3.04611577676524,0.818643589457321,
0.0200987888156099));
#22366=CARTESIAN_POINT('Ctrl Pts',(-3.05265301996243,0.821667341345101,
0.0117910987819022));
#22367=CARTESIAN_POINT('Ctrl Pts',(-3.05969044973315,0.824619391171969,
0.00368040854147765));
#22368=CARTESIAN_POINT('Ctrl Pts',(-3.06690597848203,0.82764614967441,-0.0046355420981232));
#22369=CARTESIAN_POINT('Ctrl Pts',(-3.07464711940229,0.83059711117744,-0.0127432421933774));
#22370=CARTESIAN_POINT('Ctrl Pts',(-3.08293432214086,0.833428549750499,
-0.0205225557374285));
#22371=CARTESIAN_POINT('Ctrl Pts',(-3.08900359713866,0.835502202330433,
-0.0262198693765905));
#22372=CARTESIAN_POINT('Ctrl Pts',(-3.09536426361141,0.837511450702421,
-0.0317402339087038));
#22373=CARTESIAN_POINT('Ctrl Pts',(-3.102023294888,0.839442269732748,-0.0370451155955819));
#22374=CARTESIAN_POINT('Ctrl Pts',(-3.1094340557817,0.841591056480911,-0.0429488586653822));
#22375=CARTESIAN_POINT('Ctrl Pts',(-3.11722060609208,0.8436428828278,-0.0485862052221031));
#22376=CARTESIAN_POINT('Ctrl Pts',(-3.12529583871742,0.845562886609632,
-0.0538613722579536));
#22377=CARTESIAN_POINT('Ctrl Pts',(-3.13341782061337,0.847494005709194,
-0.0591670783782781));
#22378=CARTESIAN_POINT('Ctrl Pts',(-3.14183173807261,0.849291747731165,
-0.0641063339896468));
#22379=CARTESIAN_POINT('Ctrl Pts',(-3.15042212018654,0.850936379853183,
-0.0686249236082001));
#22380=CARTESIAN_POINT('Ctrl Pts',(-3.15734806920517,0.852262355587489,
-0.0722680119969508));
#22381=CARTESIAN_POINT('Ctrl Pts',(-3.1643881120949,0.853489141241828,-0.0756385778807585));
#22382=CARTESIAN_POINT('Ctrl Pts',(-3.17147060890108,0.854613538175338,
-0.0787278330660827));
#22383=CARTESIAN_POINT('Ctrl Pts',(-3.18024623377992,0.856006731278484,
-0.0825555996579158));
#22384=CARTESIAN_POINT('Ctrl Pts',(-3.18907687523737,0.857242188179029,
-0.0859499895948705));
#22385=CARTESIAN_POINT('Ctrl Pts',(-3.19793312265248,0.858337868433289,
-0.0889603463523945));
#22386=CARTESIAN_POINT('Ctrl Pts',(-3.2131925497421,0.860225739465991,-0.0941472293855846));
#22387=CARTESIAN_POINT('Ctrl Pts',(-3.22852785907475,0.86169972756608,-0.0981969784071248));
#22388=CARTESIAN_POINT('Ctrl Pts',(-3.24381982804354,0.862842315550003,
-0.101336213092694));
#22389=CARTESIAN_POINT('Ctrl Pts',(-3.25916182043291,0.863988641192523,
-0.104485716910859));
#22390=CARTESIAN_POINT('Ctrl Pts',(-3.27446023005863,0.864801422853929,
-0.106718816172519));
#22391=CARTESIAN_POINT('Ctrl Pts',(-3.28962546932607,0.865349158675545,
-0.108223707974235));
#22392=CARTESIAN_POINT('Ctrl Pts',(-3.30345932201092,0.865848807677636,
-0.109596482325133));
#22393=CARTESIAN_POINT('Ctrl Pts',(-3.31718287702708,0.866127684895366,
-0.110362691183646));
#22394=CARTESIAN_POINT('Ctrl Pts',(-3.33074870214876,0.866227388645556,
-0.110636624985929));
#22395=CARTESIAN_POINT('Ctrl Pts',(-3.33884111261622,0.866286864841397,
-0.110800034490998));
#22396=CARTESIAN_POINT('Ctrl Pts',(-3.34687301046511,0.86628237775275,-0.11078770631626));
#22397=CARTESIAN_POINT('Ctrl Pts',(-3.35484001959732,0.866221349813515,
-0.110620033431256));
#22398=CARTESIAN_POINT('Ctrl Pts',(-3.36947366066627,0.866109254930338,
-0.110312055270891));
#22399=CARTESIAN_POINT('Ctrl Pts',(-3.38389482814325,0.865807432300713,
-0.109482804411314));
#22400=CARTESIAN_POINT('Ctrl Pts',(-3.39813942762288,0.865348115847427,
-0.108220842827527));
#22401=CARTESIAN_POINT('Ctrl Pts',(-3.41318766118658,0.864862886250162,
-0.106887685465791));
#22402=CARTESIAN_POINT('Ctrl Pts',(-3.42803949559875,0.864201828823164,
-0.105071445112153));
#22403=CARTESIAN_POINT('Ctrl Pts',(-3.44275393648476,0.863384196034785,
-0.102825017488676));
#22404=CARTESIAN_POINT('Ctrl Pts',(-3.45532171030314,0.862685846431803,
-0.100906317723598));
#22405=CARTESIAN_POINT('Ctrl Pts',(-3.4677897761167,0.861872922343871,-0.0986728271482742));
#22406=CARTESIAN_POINT('Ctrl Pts',(-3.48019827523262,0.860947876601344,
-0.0961312848587167));
#22407=CARTESIAN_POINT('Ctrl Pts',(-3.49513963286312,0.8598340078623,-0.0930709556499571));
#22408=CARTESIAN_POINT('Ctrl Pts',(-3.50998931624428,0.858557840967348,
-0.089564715922621));
#22409=CARTESIAN_POINT('Ctrl Pts',(-3.52473645223634,0.857117620036816,
-0.0856077414369611));
#22410=CARTESIAN_POINT('Ctrl Pts',(-3.54127412363113,0.855502533521181,
-0.0811703277047876));
#22411=CARTESIAN_POINT('Ctrl Pts',(-3.55768510248944,0.853681303099851,
-0.0761665382465599));
#22412=CARTESIAN_POINT('Ctrl Pts',(-3.57395757994887,0.851634209192849,
-0.070542193961567));
#22413=CARTESIAN_POINT('Ctrl Pts',(-3.58761668013831,0.849915880754991,
-0.0658211253793454));
#22414=CARTESIAN_POINT('Ctrl Pts',(-3.60117829038003,0.848038110914512,
-0.060661995143698));
#22415=CARTESIAN_POINT('Ctrl Pts',(-3.6146298930802,0.84597971447189,-0.0550065973973076));
#22416=CARTESIAN_POINT('Ctrl Pts',(-3.62657049822057,0.844152534492555,
-0.0499864616628069));
#22417=CARTESIAN_POINT('Ctrl Pts',(-3.63843162632087,0.842181318652093,
-0.0445705906522641));
#22418=CARTESIAN_POINT('Ctrl Pts',(-3.65014896992634,0.8400553704926,-0.0387295960891255));
#22419=CARTESIAN_POINT('Ctrl Pts',(-3.66894272975055,0.836645505556185,
-0.0293610691729366));
#22420=CARTESIAN_POINT('Ctrl Pts',(-3.68735920610381,0.832838066824895,
-0.0189002172327613));
#22421=CARTESIAN_POINT('Ctrl Pts',(-3.70514280927609,0.828591806062877,
-0.00723371167200015));
#22422=CARTESIAN_POINT('Ctrl Pts',(-3.71362054925493,0.826567542797777,
-0.00167209406010711));
#22423=CARTESIAN_POINT('Ctrl Pts',(-3.72195672266957,0.824443138391217,
0.00416465907670791));
#22424=CARTESIAN_POINT('Ctrl Pts',(-3.73012282927105,0.822215961845034,
0.0102837763464823));
#22425=CARTESIAN_POINT('Ctrl Pts',(-3.74073718401333,0.819321064302234,
0.0182374419769606));
#22426=CARTESIAN_POINT('Ctrl Pts',(-3.75105335567548,0.816254009126217,
0.026664106817291));
#22427=CARTESIAN_POINT('Ctrl Pts',(-3.76096038332406,0.813036383310419,
0.0355044610904482));
#22428=CARTESIAN_POINT('Ctrl Pts',(-3.77048021789542,0.809944510897677,
0.0439993107282911));
#22429=CARTESIAN_POINT('Ctrl Pts',(-3.77962242626167,0.806713575795501,
0.0528762319652448));
#22430=CARTESIAN_POINT('Ctrl Pts',(-3.78831696314315,0.803374869806503,
0.062049251280213));
#22431=CARTESIAN_POINT('Ctrl Pts',(-3.79496379746781,0.800822482500531,
0.0690618777690747));
#22432=CARTESIAN_POINT('Ctrl Pts',(-3.80134959436443,0.798207357924017,
0.0762468734921084));
#22433=CARTESIAN_POINT('Ctrl Pts',(-3.80745376791091,0.795548593922769,
0.0835517675491962));
#22434=CARTESIAN_POINT('Ctrl Pts',(-3.82454823836735,0.788102841877238,
0.10400880316515));
#22435=CARTESIAN_POINT('Ctrl Pts',(-3.83946221950595,0.780306519377066,
0.125429023189158));
#22436=CARTESIAN_POINT('Ctrl Pts',(-3.85260231893967,0.772297204784702,
0.147434434176986));
#22437=CARTESIAN_POINT('Ctrl Pts',(-3.86512430791641,0.764664648460241,
0.168404710331158));
#22438=CARTESIAN_POINT('Ctrl Pts',(-3.87603724729861,0.756840228025687,
0.189902128795414));
#22439=CARTESIAN_POINT('Ctrl Pts',(-3.88566793707772,0.748948363478614,
0.211584848435892));
#22440=CARTESIAN_POINT('Ctrl Pts',(-3.89335476066421,0.742649399236893,
0.228891110455972));
#22441=CARTESIAN_POINT('Ctrl Pts',(-3.90022423734518,0.736307637874966,
0.246314956597437));
#22442=CARTESIAN_POINT('Ctrl Pts',(-3.90642254620822,0.729981049634948,
0.263697114929073));
#22443=CARTESIAN_POINT('Ctrl Pts',(-3.91059554935688,0.725721682567389,
0.275399629768361));
#22444=CARTESIAN_POINT('Ctrl Pts',(-3.91446234610801,0.721471283238569,
0.287077505947959));
#22445=CARTESIAN_POINT('Ctrl Pts',(-3.91807359617238,0.717231425397062,
0.298726419629196));
#22446=CARTESIAN_POINT('Ctrl Pts',(-3.92287656539946,0.711592406670298,
0.314219496248863));
#22447=CARTESIAN_POINT('Ctrl Pts',(-3.9272292236022,0.705971453373679,0.329662938507133));
#22448=CARTESIAN_POINT('Ctrl Pts',(-3.93123176207092,0.700356158170212,
0.34509083528223));
#22449=CARTESIAN_POINT('Ctrl Pts',(-3.93386883168704,0.696656524929363,
0.355255494071726));
#22450=CARTESIAN_POINT('Ctrl Pts',(-3.93635393272922,0.692958190829683,
0.365416583500196));
#22451=CARTESIAN_POINT('Ctrl Pts',(-3.93870841662801,0.689257829337623,
0.375583243143451));
#22452=CARTESIAN_POINT('Ctrl Pts',(-3.94382390749327,0.681218205273688,
0.397671928720016));
#22453=CARTESIAN_POINT('Ctrl Pts',(-3.94831885241916,0.673177794435633,
0.41976277594071));
#22454=CARTESIAN_POINT('Ctrl Pts',(-3.9523304703066,0.665170889075466,0.44176156761748));
#22455=CARTESIAN_POINT('Ctrl Pts',(-3.95613817456041,0.657570980894964,
0.462642143733336));
#22456=CARTESIAN_POINT('Ctrl Pts',(-3.95950945349948,0.650003104747759,
0.483434712561013));
#22457=CARTESIAN_POINT('Ctrl Pts',(-3.96254420999663,0.642468554647117,
0.504135718828276));
#22458=CARTESIAN_POINT('Ctrl Pts',(-3.96597393742826,0.633953389364699,
0.527530943164642));
#22459=CARTESIAN_POINT('Ctrl Pts',(-3.96897347355073,0.625481816767219,
0.55080639758349));
#22460=CARTESIAN_POINT('Ctrl Pts',(-3.97165158136693,0.617042978738954,
0.573991914512582));
#22461=CARTESIAN_POINT('Ctrl Pts',(-3.97412494043032,0.609249313227979,
0.595404834518768));
#22462=CARTESIAN_POINT('Ctrl Pts',(-3.97632347848357,0.601483217612124,
0.616742006860656));
#22463=CARTESIAN_POINT('Ctrl Pts',(-3.97831229220852,0.593724774977134,
0.638058152810425));
#22464=CARTESIAN_POINT('Ctrl Pts',(-3.97974379269629,0.588140433780633,
0.653401004150341));
#22465=CARTESIAN_POINT('Ctrl Pts',(-3.98106661594193,0.582557871569018,
0.668738967769455));
#22466=CARTESIAN_POINT('Ctrl Pts',(-3.98229809143707,0.576976592903405,
0.68407340487491));
#22467=CARTESIAN_POINT('Ctrl Pts',(-3.98480909968719,0.56559623102785,0.715340692153218));
#22468=CARTESIAN_POINT('Ctrl Pts',(-3.98694117105561,0.554226106519258,
0.746579852496963));
#22469=CARTESIAN_POINT('Ctrl Pts',(-3.9888095252893,0.542876129547436,0.777763657938374));
#22470=CARTESIAN_POINT('Ctrl Pts',(-3.99076772011234,0.530980384218651,
0.810446949616796));
#22471=CARTESIAN_POINT('Ctrl Pts',(-3.99243593368405,0.519106627018567,
0.843069829408114));
#22472=CARTESIAN_POINT('Ctrl Pts',(-3.99391540185511,0.507248820519574,
0.87564888500836));
#22473=CARTESIAN_POINT('Ctrl Pts',(-3.99551021095321,0.494466566694838,
0.91076783876156));
#22474=CARTESIAN_POINT('Ctrl Pts',(-3.99688550405414,0.481702741944058,
0.945836159050202));
#22475=CARTESIAN_POINT('Ctrl Pts',(-3.99813625458243,0.468931928776515,
0.980923679856098));
#22476=CARTESIAN_POINT('Ctrl Pts',(-3.99864819727412,0.463704727731907,
0.995285296693106));
#22477=CARTESIAN_POINT('Ctrl Pts',(-3.99913894233745,0.458476169216874,
1.00965064314946));
#22478=CARTESIAN_POINT('Ctrl Pts',(-3.99961373290197,0.453243799876032,
1.02402645976366));
#22479=CARTESIAN_POINT('',(-3.91965223258409,0.527570443506261,1.05372003673881));
#22480=CARTESIAN_POINT('Origin',(-3.91965223258409,0.452395033843389,1.02635842527276));
#22481=CARTESIAN_POINT('',(-2.95949419761707,0.524122950903392,1.06319194481893));
#22482=CARTESIAN_POINT('Ctrl Pts',(-3.91965223258409,0.527570443506261,
1.05372003673881));
#22483=CARTESIAN_POINT('Ctrl Pts',(-3.91557568799506,0.572495487342456,
0.930289493230857));
#22484=CARTESIAN_POINT('Ctrl Pts',(-3.90826705411741,0.639523973437174,
0.746130241225391));
#22485=CARTESIAN_POINT('Ctrl Pts',(-3.88392091137359,0.717116212326026,
0.532947316953341));
#22486=CARTESIAN_POINT('Ctrl Pts',(-3.85995110804723,0.761488798159762,
0.411034639332341));
#22487=CARTESIAN_POINT('Ctrl Pts',(-3.82635384144273,0.804962864100056,
0.2915906248295));
#22488=CARTESIAN_POINT('Ctrl Pts',(-3.77136677090444,0.846657118193748,
0.177036603186079));
#22489=CARTESIAN_POINT('Ctrl Pts',(-3.67711802975361,0.878650808373231,
0.089134661852922));
#22490=CARTESIAN_POINT('Ctrl Pts',(-3.58208993795251,0.897694758584722,
0.0368118386696318));
#22491=CARTESIAN_POINT('Ctrl Pts',(-3.46696656599506,0.910585447910795,
0.00139496082504257));
#22492=CARTESIAN_POINT('Ctrl Pts',(-3.3360951886178,0.916101759009581,-0.0137609793575587));
#22493=CARTESIAN_POINT('Ctrl Pts',(-3.22558881811219,0.910399758249608,
0.00190513897618206));
#22494=CARTESIAN_POINT('Ctrl Pts',(-3.15028872702707,0.894206994493787,
0.0463943917538627));
#22495=CARTESIAN_POINT('Ctrl Pts',(-3.11421209795167,0.879937567446779,
0.0855993203540729));
#22496=CARTESIAN_POINT('Ctrl Pts',(-3.09090069290084,0.867246541900823,
0.12046762647131));
#22497=CARTESIAN_POINT('Ctrl Pts',(-3.05105326213358,0.840475615777891,
0.194020141491951));
#22498=CARTESIAN_POINT('Ctrl Pts',(-2.99999967569416,0.770907793456571,
0.38515616244041));
#22499=CARTESIAN_POINT('Ctrl Pts',(-2.9782979876664,0.658827601540248,0.693093958898646));
#22500=CARTESIAN_POINT('Ctrl Pts',(-2.96698008492688,0.568998871692987,
0.939896365772286));
#22501=CARTESIAN_POINT('Ctrl Pts',(-2.9594941977123,0.524122950641471,1.06319194553855));
#22502=CARTESIAN_POINT('Origin',(-2.9594941977123,0.448947540978598,1.0358303340725));
#22503=CARTESIAN_POINT('Ctrl Pts',(-2.89005284851791,0.473859726879199,
1.19608230823957));
#22504=CARTESIAN_POINT('Ctrl Pts',(-2.89347901133131,0.474015979945485,
1.14661220793332));
#22505=CARTESIAN_POINT('Ctrl Pts',(-2.8967631553832,0.48293057760256,1.09714693603063));
#22506=CARTESIAN_POINT('Ctrl Pts',(-2.8997444856637,0.500000000116261,1.0507842073536));
#22507=CARTESIAN_POINT('Ctrl Pts',(-2.90496083257667,0.490269001123116,
1.19707182630597));
#22508=CARTESIAN_POINT('Ctrl Pts',(-2.90839510354824,0.490488270635738,
1.14949416876069));
#22509=CARTESIAN_POINT('Ctrl Pts',(-2.91169011394851,0.49911244823268,1.10190390404276));
#22510=CARTESIAN_POINT('Ctrl Pts',(-2.91467642669419,0.515552148620265,
1.05735131869985));
#22511=CARTESIAN_POINT('Ctrl Pts',(-2.92693299276352,0.499999999999999,
1.19853022935878));
#22512=CARTESIAN_POINT('Ctrl Pts',(-2.9304999693179,0.500173738497183,1.15205198095784));
#22513=CARTESIAN_POINT('Ctrl Pts',(-2.93391047394094,0.508550849038461,
1.10553353033146));
#22514=CARTESIAN_POINT('Ctrl Pts',(-2.9369928411141,0.524562029109686,1.06198558733789));
#22515=CARTESIAN_POINT('Ctrl Pts',(-2.94907641594456,0.499999999999999,
1.2));
#22516=CARTESIAN_POINT('Ctrl Pts',(-2.95278203038302,0.499999999999999,
1.15347630759795));
#22517=CARTESIAN_POINT('Ctrl Pts',(-2.95631131108945,0.508222479010737,
1.10687813316721));
#22518=CARTESIAN_POINT('Ctrl Pts',(-2.9594941977123,0.5241229508155,1.06319194506041));
#22519=CARTESIAN_POINT('Ctrl Pts',(-2.95949419767749,0.524122950641611,
1.06319194553817));
#22520=CARTESIAN_POINT('Ctrl Pts',(-2.95631131106372,0.508222478950789,
1.10687813350695));
#22521=CARTESIAN_POINT('Ctrl Pts',(-2.95278203036951,0.499999999999999,
1.15347630776754));
#22522=CARTESIAN_POINT('Ctrl Pts',(-2.94907641594456,0.499999999999999,
1.2));
#22523=CARTESIAN_POINT('Origin',(-3.91965223258409,0.452395033843409,1.0263584252727));
#22524=CARTESIAN_POINT('',(-3.99746275444911,0.445738635713984,1.04371397372222));
#22525=CARTESIAN_POINT('Origin',(-3.91965223258409,0.452395033843409,1.0263584252727));
#22526=CARTESIAN_POINT('Origin',(-3.91965223258409,0.452395033843409,1.0263584252727));
#22527=CARTESIAN_POINT('Ctrl Pts',(-3.99746275438256,0.445738635719676,
1.04371397370738));
#22528=CARTESIAN_POINT('Ctrl Pts',(-3.99706351813064,0.445109606322813,
1.0452626260641));
#22529=CARTESIAN_POINT('Ctrl Pts',(-3.99671788877829,0.44447641750283,1.04682338437936));
#22530=CARTESIAN_POINT('Ctrl Pts',(-3.99642658272506,0.443840379183309,
1.04839302148081));
#22531=CARTESIAN_POINT('Ctrl Pts',(-3.99755582933675,0.468280384206874,
1.0519421574563));
#22532=CARTESIAN_POINT('Ctrl Pts',(-3.9971768724252,0.467663343351554,1.05349202747387));
#22533=CARTESIAN_POINT('Ctrl Pts',(-3.99684651829552,0.46703688980806,1.05506776196706));
#22534=CARTESIAN_POINT('Ctrl Pts',(-3.99657534106215,0.466413555729912,
1.05663619619577));
#22535=CARTESIAN_POINT('Ctrl Pts',(-3.97806581626837,0.508977365274313,
1.06180057527797));
#22536=CARTESIAN_POINT('Ctrl Pts',(-3.97759566678914,0.508247059602534,
1.06376320056323));
#22537=CARTESIAN_POINT('Ctrl Pts',(-3.97719426482472,0.507513520656082,
1.06573512393595));
#22538=CARTESIAN_POINT('Ctrl Pts',(-3.97685956385479,0.50677514383455,1.06772027127607));
#22539=CARTESIAN_POINT('Ctrl Pts',(-3.93715733927913,0.526140389499051,
1.05764907783222));
#22540=CARTESIAN_POINT('Ctrl Pts',(-3.93645817327013,0.525126591517723,
1.06043493280982));
#22541=CARTESIAN_POINT('Ctrl Pts',(-3.93585500062643,0.524105540900254,
1.0632393122251));
#22542=CARTESIAN_POINT('Ctrl Pts',(-3.93534760874183,0.523078681693311,
1.06606105089346));
#22543=CARTESIAN_POINT('Ctrl Pts',(-3.91965223258409,0.527570443506282,
1.05372003673876));
#22544=CARTESIAN_POINT('Ctrl Pts',(-3.91885525761101,0.526429247151133,
1.05685544795569));
#22545=CARTESIAN_POINT('Ctrl Pts',(-3.91816549099621,0.525279290574345,
1.06001492768377));
#22546=CARTESIAN_POINT('Ctrl Pts',(-3.91758436243191,0.524122951685363,
1.06319194267048));
#22547=CARTESIAN_POINT('Origin',(-4.05559523088995,0.440984362651786,1.05744795078647));
#22548=CARTESIAN_POINT('Origin',(-4.03591301597994,0.517624494217011,1.08104630782635));
#22549=CARTESIAN_POINT('Ctrl Pts',(-3.99500090812059,0.125168749047044,
0.930078956913999));
#22550=CARTESIAN_POINT('Ctrl Pts',(-3.99593963459395,0.232006196698264,
0.968035837491526));
#22551=CARTESIAN_POINT('Ctrl Pts',(-3.99674494883676,0.33885382942011,1.00593844604213));
#22552=CARTESIAN_POINT('Ctrl Pts',(-3.99746275438256,0.445738635719677,
1.04371397370738));
#22553=CARTESIAN_POINT('Ctrl Pts',(-3.99824520675537,0.128463087592629,
0.921420039511872));
#22554=CARTESIAN_POINT('Ctrl Pts',(-3.99857533133843,0.235036780014703,
0.960065081373451));
#22555=CARTESIAN_POINT('Ctrl Pts',(-3.99885884426554,0.341611566532603,
0.998688309789087));
#22556=CARTESIAN_POINT('Ctrl Pts',(-3.99910791850814,0.448191320810768,
1.0372788540661));
#22557=CARTESIAN_POINT('Ctrl Pts',(-3.99976439851731,0.131971946808211,
0.91219976288192));
#22558=CARTESIAN_POINT('Ctrl Pts',(-3.99978611058741,0.238221660879987,
0.95169039150062));
#22559=CARTESIAN_POINT('Ctrl Pts',(-3.99981055015748,0.344480567483035,
0.991147371513851));
#22560=CARTESIAN_POINT('Ctrl Pts',(-3.99983334587227,0.450722471820515,
1.03063914975585));
#22561=CARTESIAN_POINT('Ctrl Pts',(-3.99945760881125,0.135462337836371,
0.903030354983464));
#22562=CARTESIAN_POINT('Ctrl Pts',(-3.99950970007112,0.241391193737631,
0.943357929054413));
#22563=CARTESIAN_POINT('Ctrl Pts',(-3.99956010118928,0.347337150066848,
0.983640596922404));
#22564=CARTESIAN_POINT('Ctrl Pts',(-3.99961373290197,0.453243799876052,
1.02402645976362));
#22565=CARTESIAN_POINT('Ctrl Pts',(-3.99961373290197,0.453243799876052,
1.02402645976362));
#22566=CARTESIAN_POINT('Ctrl Pts',(-3.99956010118928,0.347337150066848,
0.983640596922404));
#22567=CARTESIAN_POINT('Ctrl Pts',(-3.99950970007112,0.241391193737631,
0.943357929054413));
#22568=CARTESIAN_POINT('Ctrl Pts',(-3.99945760881125,0.135462337836371,
0.903030354983464));
#22569=CARTESIAN_POINT('',(-3.99500090813004,0.125168749022039,0.930078956989209));
#22570=CARTESIAN_POINT('Origin',(-3.91949669889834,0.134607090093723,0.905380128844431));
#22571=CARTESIAN_POINT('Ctrl Pts',(-3.99500090812059,0.125168749047044,
0.930078956913999));
#22572=CARTESIAN_POINT('Ctrl Pts',(-3.99593963459395,0.232006196698264,
0.968035837491526));
#22573=CARTESIAN_POINT('Ctrl Pts',(-3.99674494883676,0.33885382942011,1.00593844604213));
#22574=CARTESIAN_POINT('Ctrl Pts',(-3.99746275438256,0.445738635719677,
1.04371397370738));
#22575=CARTESIAN_POINT('Ctrl Pts',(-2.87936339380758,0.054276641292682,
0.892181871006899));
#22576=CARTESIAN_POINT('Ctrl Pts',(-2.87936339380758,0.618092213764237,
1.0973939570023));
#22577=CARTESIAN_POINT('Ctrl Pts',(-2.88050601962387,0.061089278956966,
0.873464302857353));
#22578=CARTESIAN_POINT('Ctrl Pts',(-2.88050601962387,0.624904851428521,
1.07867638885275));
#22579=CARTESIAN_POINT('Ctrl Pts',(-2.88410012960011,0.0831761921549222,
0.812781007580514));
#22580=CARTESIAN_POINT('Ctrl Pts',(-2.88410012960011,0.646991764626477,
1.01799309357591));
#22581=CARTESIAN_POINT('Ctrl Pts',(-2.88965455295869,0.120639229722751,
0.709852157798725));
#22582=CARTESIAN_POINT('Ctrl Pts',(-2.88965455295869,0.684454802194306,
0.915064243794126));
#22583=CARTESIAN_POINT('Ctrl Pts',(-2.89676647174981,0.173526397310949,
0.564545859071238));
#22584=CARTESIAN_POINT('Ctrl Pts',(-2.89676647174981,0.737341969782504,
0.769757945066639));
#22585=CARTESIAN_POINT('Ctrl Pts',(-2.90717911786707,0.241012720183549,
0.379128710856747));
#22586=CARTESIAN_POINT('Ctrl Pts',(-2.90717911786707,0.804828292655104,
0.584340796852148));
#22587=CARTESIAN_POINT('Ctrl Pts',(-2.92780415844476,0.312514210565547,
0.182679980574853));
#22588=CARTESIAN_POINT('Ctrl Pts',(-2.92780415844476,0.876329783037102,
0.387892066570254));
#22589=CARTESIAN_POINT('Ctrl Pts',(-2.96639254265869,0.374982215648805,
0.0110505471702249));
#22590=CARTESIAN_POINT('Ctrl Pts',(-2.96639254265869,0.93879778812036,0.216262633165626));
#22591=CARTESIAN_POINT('Ctrl Pts',(-3.03063129752067,0.423994474883956,
-0.123609528354807));
#22592=CARTESIAN_POINT('Ctrl Pts',(-3.03063129752067,0.987810047355511,
0.0816025576405938));
#22593=CARTESIAN_POINT('Ctrl Pts',(-3.12452733970658,0.456428987719491,
-0.212722619981451));
#22594=CARTESIAN_POINT('Ctrl Pts',(-3.12452733970658,1.02024456019105,-0.00751053398605017));
#22595=CARTESIAN_POINT('Ctrl Pts',(-3.24511001026157,0.472026186037003,
-0.255575570165571));
#22596=CARTESIAN_POINT('Ctrl Pts',(-3.24511001026157,1.03584175850856,-0.0503634841701701));
#22597=CARTESIAN_POINT('Ctrl Pts',(-3.38164698943802,0.473698270059231,
-0.260169583260074));
#22598=CARTESIAN_POINT('Ctrl Pts',(-3.38164698943802,1.03751384253079,-0.0549574972646732));
#22599=CARTESIAN_POINT('Ctrl Pts',(-3.52045328348989,0.465105650196581,
-0.236561554213485));
#22600=CARTESIAN_POINT('Ctrl Pts',(-3.52045328348989,1.02892122266814,-0.0313494682180842));
#22601=CARTESIAN_POINT('Ctrl Pts',(-3.64881642260079,0.448607387242662,
-0.191232949287367));
#22602=CARTESIAN_POINT('Ctrl Pts',(-3.64881642260079,1.01242295971422,0.0139791367080338));
#22603=CARTESIAN_POINT('Ctrl Pts',(-3.75872318140663,0.42348833261052,-0.122218913887511));
#22604=CARTESIAN_POINT('Ctrl Pts',(-3.75872318140663,0.987303905082075,
0.0829931721078898));
#22605=CARTESIAN_POINT('Ctrl Pts',(-3.84598208672296,0.387862727674243,
-0.0243383687706796));
#22606=CARTESIAN_POINT('Ctrl Pts',(-3.84598208672296,0.951678300145798,
0.180873717224721));
#22607=CARTESIAN_POINT('Ctrl Pts',(-3.9098657241983,0.340085651878983,0.10692806814437));
#22608=CARTESIAN_POINT('Ctrl Pts',(-3.9098657241983,0.903901224350538,0.312140154139771));
#22609=CARTESIAN_POINT('Ctrl Pts',(-3.9525920016999,0.280544576017308,0.270515829604357));
#22610=CARTESIAN_POINT('Ctrl Pts',(-3.9525920016999,0.844360148488863,0.475727915599758));
#22611=CARTESIAN_POINT('Ctrl Pts',(-3.97841403016126,0.21121967143493,0.460984439550287));
#22612=CARTESIAN_POINT('Ctrl Pts',(-3.97841403016126,0.775035243906485,
0.666196525545688));
#22613=CARTESIAN_POINT('Ctrl Pts',(-3.98977740850458,0.150154761706452,
0.628758900150314));
#22614=CARTESIAN_POINT('Ctrl Pts',(-3.98977740850458,0.713970334178007,
0.833970986145715));
#22615=CARTESIAN_POINT('Ctrl Pts',(-3.99545186687387,0.102617065619347,
0.759367646722532));
#22616=CARTESIAN_POINT('Ctrl Pts',(-3.99545186687387,0.666432638090902,
0.964579732717933));
#22617=CARTESIAN_POINT('Ctrl Pts',(-3.99855414331415,0.0704990924696529,
0.847611052709967));
#22618=CARTESIAN_POINT('Ctrl Pts',(-3.99855414331415,0.634314664941208,
1.05282313870537));
#22619=CARTESIAN_POINT('Ctrl Pts',(-3.99999413894399,0.054342424295042,
0.892001133693331));
#22620=CARTESIAN_POINT('Ctrl Pts',(-3.99999413894399,0.618157996766597,
1.09721321968873));
#22621=CARTESIAN_POINT('Ctrl Pts',(-4.,0.0542766412926824,0.892181871006898));
#22622=CARTESIAN_POINT('Ctrl Pts',(-4.,0.618092213764237,1.0973939570023));
#22623=CARTESIAN_POINT('',(-2.87936339380758,0.0542766412926824,0.892181871006898));
#22624=CARTESIAN_POINT('Ctrl Pts',(-2.87936339380758,0.510402750471661,
1.0581981978197));
#22625=CARTESIAN_POINT('Ctrl Pts',(-2.87936339380758,0.38345364991127,1.01199250394885));
#22626=CARTESIAN_POINT('Ctrl Pts',(-2.87936339380758,0.25645519700216,0.965768847292079));
#22627=CARTESIAN_POINT('Ctrl Pts',(-2.87936339380758,0.129452050955553,
0.919543482472951));
#22628=CARTESIAN_POINT('Ctrl Pts',(-2.88380565711847,0.507160352260398,
1.06851837583814));
#22629=CARTESIAN_POINT('Ctrl Pts',(-2.885256581924,0.379732217321614,1.02359703230995));
#22630=CARTESIAN_POINT('Ctrl Pts',(-2.88661730605277,0.252436541519274,
0.978175521115242));
#22631=CARTESIAN_POINT('Ctrl Pts',(-2.88800949912464,0.125204871749137,
0.932598552100246));
#22632=CARTESIAN_POINT('Ctrl Pts',(-2.88583635958945,0.503581269771104,
1.07976272406583));
#22633=CARTESIAN_POINT('Ctrl Pts',(-2.88803975294752,0.375510613992429,
1.03657431850542));
#22634=CARTESIAN_POINT('Ctrl Pts',(-2.8901570753878,0.247726768638573,0.992479117588928));
#22635=CARTESIAN_POINT('Ctrl Pts',(-2.89233651283672,0.120040512706022,
0.948170442679049));
#22636=CARTESIAN_POINT('Ctrl Pts',(-2.8852657140673,0.5,1.09088035845137));
#22637=CARTESIAN_POINT('Ctrl Pts',(-2.88739518236194,0.371284826357953,
1.04939286925411));
#22638=CARTESIAN_POINT('Ctrl Pts',(-2.88948025018409,0.243010859025609,
1.00659623192935));
#22639=CARTESIAN_POINT('Ctrl Pts',(-2.89158569656657,0.114864540034388,
0.963528635709792));
#22640=CARTESIAN_POINT('Ctrl Pts',(-2.803641505311,0.08,1.2));
#22641=CARTESIAN_POINT('Ctrl Pts',(-2.803641505311,0.584,1.2));
#22642=CARTESIAN_POINT('Ctrl Pts',(-2.82677300877682,0.08,1.2));
#22643=CARTESIAN_POINT('Ctrl Pts',(-2.82677300877682,0.584,1.2));
#22644=CARTESIAN_POINT('Ctrl Pts',(-2.86687236848073,0.08,1.18130984727688));
#22645=CARTESIAN_POINT('Ctrl Pts',(-2.86687236848073,0.584,1.18130984727688));
#22646=CARTESIAN_POINT('Ctrl Pts',(-2.88261462067416,0.08,1.14154581001999));
#22647=CARTESIAN_POINT('Ctrl Pts',(-2.88261462067416,0.584,1.14154581001999));
#22648=CARTESIAN_POINT('Ctrl Pts',(-2.88353005387198,0.08,1.12422135153951));
#22649=CARTESIAN_POINT('Ctrl Pts',(-2.88353005387198,0.584,1.12422135153951));
#22650=CARTESIAN_POINT('',(-2.803641505311,0.5,1.2));
#22651=CARTESIAN_POINT('Ctrl Pts',(-3.9106833422892,0.0384897740707112,
0.939615427909197));
#22652=CARTESIAN_POINT('Ctrl Pts',(-3.91354391573668,0.0199991968201913,
1.00079349366622));
#22653=CARTESIAN_POINT('Ctrl Pts',(-3.9158360335454,0.00804296821746633,
1.06397598649794));
#22654=CARTESIAN_POINT('Ctrl Pts',(-3.91781846660453,0.00290707172437443,
1.12772087043234));
#22655=CARTESIAN_POINT('Ctrl Pts',(-3.93437185463721,0.0388201352419867,
0.938499550671921));
#22656=CARTESIAN_POINT('Ctrl Pts',(-3.93732958055613,0.0201980578537388,
0.999813489629965));
#22657=CARTESIAN_POINT('Ctrl Pts',(-3.93967836210679,0.00816932330334512,
1.06306801873905));
#22658=CARTESIAN_POINT('Ctrl Pts',(-3.94170600662187,0.00296563685502545,
1.12691026059145));
#22659=CARTESIAN_POINT('Ctrl Pts',(-3.97540039704606,0.0582587635086386,
0.942269104078657));
#22660=CARTESIAN_POINT('Ctrl Pts',(-3.97851429576965,0.0399886969010512,
1.00247500534244));
#22661=CARTESIAN_POINT('Ctrl Pts',(-3.98096563012735,0.0281607199544487,
1.06457282534426));
#22662=CARTESIAN_POINT('Ctrl Pts',(-3.98306565367973,0.0230377862102752,
1.12711565157154));
#22663=CARTESIAN_POINT('Ctrl Pts',(-3.99034065233881,0.0980581224574643,
0.953531437079163));
#22664=CARTESIAN_POINT('Ctrl Pts',(-3.99333584061565,0.0807856567863764,
1.01108170025839));
#22665=CARTESIAN_POINT('Ctrl Pts',(-3.9957069693143,0.0696117321811971,
1.07033813817931));
#22666=CARTESIAN_POINT('Ctrl Pts',(-3.99774875287515,0.0647997910680151,
1.12997927823579));
#22667=CARTESIAN_POINT('Ctrl Pts',(-3.990599354584,0.115088570413461,0.958665497906023));
#22668=CARTESIAN_POINT('Ctrl Pts',(-3.9934922166161,0.0982419908213599,
1.01503404648247));
#22669=CARTESIAN_POINT('Ctrl Pts',(-3.99580030401545,0.087348807066054,
1.07303953608064));
#22670=CARTESIAN_POINT('Ctrl Pts',(-3.99779298688,0.0826695349261019,1.13141756172706));
#22671=CARTESIAN_POINT('',(-3.99059905039462,0.115068728348614,0.9586595164214));
#22672=CARTESIAN_POINT('Ctrl Pts',(-3.99749553673965,0.0833869626360487,
1.12277470481743));
#22673=CARTESIAN_POINT('Ctrl Pts',(-3.99557092677476,0.088417954777819,
1.0673144474751));
#22674=CARTESIAN_POINT('Ctrl Pts',(-3.99334924695252,0.0990531491906679,
1.01224727331911));
#22675=CARTESIAN_POINT('Ctrl Pts',(-3.99059905039179,0.115068728358824,
0.958659516390688));
#22676=CARTESIAN_POINT('Origin',(-3.91070419800688,0.115068728358824,0.96275982886584));
#22677=CARTESIAN_POINT('Ctrl Pts',(-3.99059905039179,0.115068728358825,
0.958659516390683));
#22678=CARTESIAN_POINT('Ctrl Pts',(-3.99022032406425,0.117088541529883,
0.951280009531972));
#22679=CARTESIAN_POINT('Ctrl Pts',(-3.99095351851113,0.11955866968438,0.943986539572236));
#22680=CARTESIAN_POINT('Ctrl Pts',(-3.99276651177431,0.122341921457849,
0.937078276746861));
#22681=CARTESIAN_POINT('Ctrl Pts',(-3.99024788717857,0.0923702555515019,
0.951817078587972));
#22682=CARTESIAN_POINT('Ctrl Pts',(-3.98978566864749,0.0945716870691454,
0.944022370054385));
#22683=CARTESIAN_POINT('Ctrl Pts',(-3.99058029988189,0.0971825638221607,
0.93620230647329));
#22684=CARTESIAN_POINT('Ctrl Pts',(-3.99256871721073,0.0999892111837481,
0.928891350782428));
#22685=CARTESIAN_POINT('Ctrl Pts',(-3.96997099994117,0.0530616659229667,
0.940976960505986));
#22686=CARTESIAN_POINT('Ctrl Pts',(-3.96936836234513,0.0561827488203104,
0.930609204971929));
#22687=CARTESIAN_POINT('Ctrl Pts',(-3.97037966405284,0.0595786334866178,
0.920227936342186));
#22688=CARTESIAN_POINT('Ctrl Pts',(-3.97292637392248,0.0630513948986112,
0.910362103819981));
#22689=CARTESIAN_POINT('Ctrl Pts',(-3.92846526015161,0.0387425083350586,
0.938779222925522));
#22690=CARTESIAN_POINT('Ctrl Pts',(-3.92775891147314,0.0431208469974308,
0.924351545690715));
#22691=CARTESIAN_POINT('Ctrl Pts',(-3.9290879339547,0.047896842751599,0.909937955493114));
#22692=CARTESIAN_POINT('Ctrl Pts',(-3.9323846422143,0.0528332298852771,
0.896147611255728));
#22693=CARTESIAN_POINT('Ctrl Pts',(-3.91070419800688,0.0384900677109053,
0.939614446316161));
#22694=CARTESIAN_POINT('Ctrl Pts',(-3.90995323778991,0.043344115284559,
0.923554376403128));
#22695=CARTESIAN_POINT('Ctrl Pts',(-3.91141850629553,0.0486938803101099,
0.90752038074473));
#22696=CARTESIAN_POINT('Ctrl Pts',(-3.91503635643999,0.0542766412926799,
0.892181871006906));
#22697=CARTESIAN_POINT('',(-3.99276651177429,0.122341921455471,0.93707827674599));
#22698=CARTESIAN_POINT('Origin',(-3.91503635643999,0.129452050955553,0.919543482472958));
#22699=CARTESIAN_POINT('Ctrl Pts',(-3.99059905039179,0.115068728358825,
0.958659516390683));
#22700=CARTESIAN_POINT('Ctrl Pts',(-3.99022032406425,0.117088541529883,
0.951280009531972));
#22701=CARTESIAN_POINT('Ctrl Pts',(-3.99095351851113,0.11955866968438,0.943986539572236));
#22702=CARTESIAN_POINT('Ctrl Pts',(-3.99276651177431,0.122341921457849,
0.937078276746861));
#22703=CARTESIAN_POINT('Ctrl Pts',(-3.91949669889834,0.0594316804308502,
0.878018517378377));
#22704=CARTESIAN_POINT('Ctrl Pts',(-3.91776450002014,0.0577396751765171,
0.882667263608256));
#22705=CARTESIAN_POINT('Ctrl Pts',(-3.91627531395221,0.0560185533163472,
0.887396007055203));
#22706=CARTESIAN_POINT('Ctrl Pts',(-3.91503635643999,0.0542766412926799,
0.892181871006905));
#22707=CARTESIAN_POINT('Ctrl Pts',(-3.94201201831921,0.0567353225932654,
0.885426699651911));
#22708=CARTESIAN_POINT('Ctrl Pts',(-3.9405226858886,0.0552989731010419,
0.889375045120937));
#22709=CARTESIAN_POINT('Ctrl Pts',(-3.93923778894123,0.053832019954493,
0.893401502356153));
#22710=CARTESIAN_POINT('Ctrl Pts',(-3.93816740413907,0.052352092749476,
0.897469524672002));
#22711=CARTESIAN_POINT('Ctrl Pts',(-3.98099331223824,0.070815773798773,
0.905076632451692));
#22712=CARTESIAN_POINT('Ctrl Pts',(-3.97992327128341,0.069788483816893,
0.907811358142667));
#22713=CARTESIAN_POINT('Ctrl Pts',(-3.97899701572105,0.068744459577118,
0.91059438223949));
#22714=CARTESIAN_POINT('Ctrl Pts',(-3.97821832116159,0.0676852936406248,
0.913418676649671));
#22715=CARTESIAN_POINT('Ctrl Pts',(-3.99491190730368,0.108366920859318,
0.923930428412372));
#22716=CARTESIAN_POINT('Ctrl Pts',(-3.99402530924208,0.107450746899103,
0.926226086767676));
#22717=CARTESIAN_POINT('Ctrl Pts',(-3.99325856149151,0.106518326821552,
0.928569719091837));
#22718=CARTESIAN_POINT('Ctrl Pts',(-3.99261816585162,0.105577388752273,
0.930938082273536));
#22719=CARTESIAN_POINT('Ctrl Pts',(-3.99500090812059,0.125168749047044,
0.930078956913999));
#22720=CARTESIAN_POINT('Ctrl Pts',(-3.99413338741396,0.124238863836765,
0.932375620181965));
#22721=CARTESIAN_POINT('Ctrl Pts',(-3.99338738371022,0.123295065052931,
0.934712494920036));
#22722=CARTESIAN_POINT('Ctrl Pts',(-3.99276651177431,0.122341921457849,
0.937078276746861));
#22723=CARTESIAN_POINT('Origin',(-3.91949669889834,0.134607090093723,0.905380128844431));
#22724=CARTESIAN_POINT('Origin',(-4.0510872574969,0.118364537007352,0.949600376125361));
#22725=CARTESIAN_POINT('Origin',(-3.91949669889834,0.134607090093723,0.905380128844431));
#22726=CARTESIAN_POINT('Ctrl Pts',(-3.99499168547955,0.124132806141263,
0.929711262728432));
#22727=CARTESIAN_POINT('Ctrl Pts',(-3.99594631188109,0.231310970463683,
0.9677529322264));
#22728=CARTESIAN_POINT('Ctrl Pts',(-3.99676075730698,0.338517926331372,
1.00575284837914));
#22729=CARTESIAN_POINT('Ctrl Pts',(-3.99748245955517,0.445763956511613,
1.04363554723628));
#22730=CARTESIAN_POINT('Ctrl Pts',(-3.9915949893774,0.121141354506694,0.938941135546907));
#22731=CARTESIAN_POINT('Ctrl Pts',(-3.99320655831758,0.22857262587258,0.976182588452333));
#22732=CARTESIAN_POINT('Ctrl Pts',(-3.99457441210398,0.336045551741593,
1.01337043101945));
#22733=CARTESIAN_POINT('Ctrl Pts',(-3.99578832520602,0.443592156028746,
1.05036245459742));
#22734=CARTESIAN_POINT('Ctrl Pts',(-3.99009222817804,0.117914157270493,
0.948787406604446));
#22735=CARTESIAN_POINT('Ctrl Pts',(-3.9920041082913,0.225667811748472,0.985047957459691));
#22736=CARTESIAN_POINT('Ctrl Pts',(-3.99362608533509,0.333454367731145,
1.02129852328768));
#22737=CARTESIAN_POINT('Ctrl Pts',(-3.99506362287769,0.441337300197856,
1.05730597317919));
#22738=CARTESIAN_POINT('Ctrl Pts',(-3.99059262862431,0.114685780139278,
0.958534409222154));
#22739=CARTESIAN_POINT('Ctrl Pts',(-3.9924053082979,0.2227624802018,0.993842518267836));
#22740=CARTESIAN_POINT('Ctrl Pts',(-3.99395808870925,0.330862808266828,
1.02917430286131));
#22741=CARTESIAN_POINT('Ctrl Pts',(-3.99533497979657,0.439082237595944,
1.06421098217699));
#22742=CARTESIAN_POINT('Ctrl Pts',(-3.99059905040313,0.115068728317981,
0.958659516513544));
#22743=CARTESIAN_POINT('Ctrl Pts',(-3.9924069847619,0.22289907004185,0.993887178660277));
#22744=CARTESIAN_POINT('Ctrl Pts',(-3.99395630241674,0.330753044397502,
1.02913803372068));
#22745=CARTESIAN_POINT('Ctrl Pts',(-3.99533043998868,0.438725473099098,
1.06409547635602));
#22746=CARTESIAN_POINT('Ctrl Pts',(-2.87936339380758,-3.,1.2));
#22747=CARTESIAN_POINT('Ctrl Pts',(-2.87936339380758,4.2,1.2));
#22748=CARTESIAN_POINT('Ctrl Pts',(-2.88050601962387,-3.,1.18008118002045));
#22749=CARTESIAN_POINT('Ctrl Pts',(-2.88050601962387,4.2,1.18008118002045));
#22750=CARTESIAN_POINT('Ctrl Pts',(-2.88410012960011,-3.,1.11550336602625));
#22751=CARTESIAN_POINT('Ctrl Pts',(-2.88410012960011,4.2,1.11550336602625));
#22752=CARTESIAN_POINT('Ctrl Pts',(-2.88965455295869,-3.,1.00596877194195));
#22753=CARTESIAN_POINT('Ctrl Pts',(-2.88965455295869,4.2,1.00596877194195));
#22754=CARTESIAN_POINT('Ctrl Pts',(-2.89676647174981,-3.,0.851337038635417));
#22755=CARTESIAN_POINT('Ctrl Pts',(-2.89676647174981,4.2,0.851337038635417));
#22756=CARTESIAN_POINT('Ctrl Pts',(-2.90717911786707,-3.,0.654020230869684));
#22757=CARTESIAN_POINT('Ctrl Pts',(-2.90717911786707,4.2,0.654020230869684));
#22758=CARTESIAN_POINT('Ctrl Pts',(-2.92780415844476,-3.,0.444963858672577));
#22759=CARTESIAN_POINT('Ctrl Pts',(-2.92780415844476,4.2,0.444963858672577));
#22760=CARTESIAN_POINT('Ctrl Pts',(-2.96639254265869,-3.,0.262319630540737));
#22761=CARTESIAN_POINT('Ctrl Pts',(-2.96639254265869,4.2,0.262319630540737));
#22762=CARTESIAN_POINT('Ctrl Pts',(-3.03063129752067,-3.,0.11901737132707));
#22763=CARTESIAN_POINT('Ctrl Pts',(-3.03063129752067,4.2,0.11901737132707));
#22764=CARTESIAN_POINT('Ctrl Pts',(-3.12452733970658,-3.,0.0241851999813871));
#22765=CARTESIAN_POINT('Ctrl Pts',(-3.12452733970658,4.2,0.0241851999813871));
#22766=CARTESIAN_POINT('Ctrl Pts',(-3.24511001026157,-3.,-0.0214179570895714));
#22767=CARTESIAN_POINT('Ctrl Pts',(-3.24511001026157,4.2,-0.0214179570895714));
#22768=CARTESIAN_POINT('Ctrl Pts',(-3.38164698943802,-3.,-0.0263068037112043));
#22769=CARTESIAN_POINT('Ctrl Pts',(-3.38164698943802,4.2,-0.0263068037112043));
#22770=CARTESIAN_POINT('Ctrl Pts',(-3.52045328348989,-3.,-0.00118366394785932));
#22771=CARTESIAN_POINT('Ctrl Pts',(-3.52045328348989,4.2,-0.00118366394785932));
#22772=CARTESIAN_POINT('Ctrl Pts',(-3.64881642260079,-3.,0.0470540298718583));
#22773=CARTESIAN_POINT('Ctrl Pts',(-3.64881642260079,4.2,0.0470540298718583));
#22774=CARTESIAN_POINT('Ctrl Pts',(-3.75872318140663,-3.,0.120497232333251));
#22775=CARTESIAN_POINT('Ctrl Pts',(-3.75872318140663,4.2,0.120497232333251));
#22776=CARTESIAN_POINT('Ctrl Pts',(-3.84598208672296,-3.,0.224659532804408));
#22777=CARTESIAN_POINT('Ctrl Pts',(-3.84598208672296,4.2,0.224659532804408));
#22778=CARTESIAN_POINT('Ctrl Pts',(-3.9098657241983,-3.,0.364350357241515));
#22779=CARTESIAN_POINT('Ctrl Pts',(-3.9098657241983,4.2,0.364350357241515));
#22780=CARTESIAN_POINT('Ctrl Pts',(-3.9525920016999,-3.,0.538436816836325));
#22781=CARTESIAN_POINT('Ctrl Pts',(-3.9525920016999,4.2,0.538436816836325));
#22782=CARTESIAN_POINT('Ctrl Pts',(-3.97841403016126,-3.,0.741129277895169));
#22783=CARTESIAN_POINT('Ctrl Pts',(-3.97841403016126,4.2,0.741129277895169));
#22784=CARTESIAN_POINT('Ctrl Pts',(-3.98977740850458,-3.,0.919671129654853));
#22785=CARTESIAN_POINT('Ctrl Pts',(-3.98977740850458,4.2,0.919671129654853));
#22786=CARTESIAN_POINT('Ctrl Pts',(-3.99545186687387,-3.,1.05866205464795));
#22787=CARTESIAN_POINT('Ctrl Pts',(-3.99545186687387,4.2,1.05866205464795));
#22788=CARTESIAN_POINT('Ctrl Pts',(-3.99855414331415,-3.,1.15256872586734));
#22789=CARTESIAN_POINT('Ctrl Pts',(-3.99855414331415,4.2,1.15256872586734));
#22790=CARTESIAN_POINT('Ctrl Pts',(-3.99999413894399,-3.,1.19980766336825));
#22791=CARTESIAN_POINT('Ctrl Pts',(-3.99999413894399,4.2,1.19980766336825));
#22792=CARTESIAN_POINT('Ctrl Pts',(-4.,-3.,1.2));
#22793=CARTESIAN_POINT('Ctrl Pts',(-4.,4.2,1.2));
#22794=CARTESIAN_POINT('Origin',(-3.2,0.9,1.2));
#22795=CARTESIAN_POINT('',(-4.5,0.524122951685637,1.06319194266973));
#22796=CARTESIAN_POINT('Origin',(4.1,0.,1.2));
#22797=CARTESIAN_POINT('Origin',(3.2,0.9,1.2));
#22798=CARTESIAN_POINT('',(-4.5,0.524122951685637,1.06319194266973));
#22799=CARTESIAN_POINT('Ctrl Pts',(4.08617023400024,-0.552060840994624,
11.9163435012344));
#22800=CARTESIAN_POINT('Ctrl Pts',(4.08617023400024,1.61522066995007,11.9163435012344));
#22801=CARTESIAN_POINT('Ctrl Pts',(4.10576511646638,-0.552060840994624,
11.8970344456328));
#22802=CARTESIAN_POINT('Ctrl Pts',(4.10576511646638,1.61522066995007,11.8970344456328));
#22803=CARTESIAN_POINT('Ctrl Pts',(4.15149421914094,-0.552060840994624,
11.8511956487512));
#22804=CARTESIAN_POINT('Ctrl Pts',(4.15149421914094,1.61522066995007,11.8511956487512));
#22805=CARTESIAN_POINT('Ctrl Pts',(4.22408937937455,-0.552060840994624,
11.7763607682953));
#22806=CARTESIAN_POINT('Ctrl Pts',(4.22408937937455,1.61522066995007,11.7763607682953));
#22807=CARTESIAN_POINT('Ctrl Pts',(4.3260071847331,-0.552060840994624,11.6707401393954));
#22808=CARTESIAN_POINT('Ctrl Pts',(4.3260071847331,1.61522066995007,11.6707401393954));
#22809=CARTESIAN_POINT('Ctrl Pts',(4.46255574628753,-0.552060840994624,
11.5373242211525));
#22810=CARTESIAN_POINT('Ctrl Pts',(4.46255574628753,1.61522066995007,11.5373242211525));
#22811=CARTESIAN_POINT('Ctrl Pts',(4.61532593596939,-0.552060840994624,
11.4029224160728));
#22812=CARTESIAN_POINT('Ctrl Pts',(4.61532593596939,1.61522066995007,11.4029224160728));
#22813=CARTESIAN_POINT('Ctrl Pts',(4.77596612414944,-0.552060840994624,
11.2768795166233));
#22814=CARTESIAN_POINT('Ctrl Pts',(4.77596612414944,1.61522066995007,11.2768795166233));
#22815=CARTESIAN_POINT('Ctrl Pts',(4.94211773226968,-0.552060840994624,
11.1598106424589));
#22816=CARTESIAN_POINT('Ctrl Pts',(4.94211773226968,1.61522066995007,11.1598106424589));
#22817=CARTESIAN_POINT('Ctrl Pts',(5.11112998264613,-0.552060840994624,
11.051370419133));
#22818=CARTESIAN_POINT('Ctrl Pts',(5.11112998264613,1.61522066995007,11.051370419133));
#22819=CARTESIAN_POINT('Ctrl Pts',(5.28082876351925,-0.552060840994624,
10.9511663773825));
#22820=CARTESIAN_POINT('Ctrl Pts',(5.28082876351925,1.61522066995007,10.9511663773825));
#22821=CARTESIAN_POINT('Ctrl Pts',(5.45051506148977,-0.552060840994624,
10.8599381259735));
#22822=CARTESIAN_POINT('Ctrl Pts',(5.45051506148977,1.61522066995007,10.8599381259735));
#22823=CARTESIAN_POINT('Ctrl Pts',(5.62101499943423,-0.552060840994624,
10.7795199127532));
#22824=CARTESIAN_POINT('Ctrl Pts',(5.62101499943423,1.61522066995007,10.7795199127532));
#22825=CARTESIAN_POINT('Ctrl Pts',(5.7936769541502,-0.552060840994624,10.7114411549111));
#22826=CARTESIAN_POINT('Ctrl Pts',(5.7936769541502,1.61522066995007,10.7114411549111));
#22827=CARTESIAN_POINT('Ctrl Pts',(5.96961932707136,-0.552060840994624,
10.6558377434042));
#22828=CARTESIAN_POINT('Ctrl Pts',(5.96961932707136,1.61522066995007,10.6558377434042));
#22829=CARTESIAN_POINT('Ctrl Pts',(6.14893768388704,-0.552060840994624,
10.6103475969888));
#22830=CARTESIAN_POINT('Ctrl Pts',(6.14893768388704,1.61522066995007,10.6103475969888));
#22831=CARTESIAN_POINT('Ctrl Pts',(6.32976796473819,-0.552060840994624,
10.5687216653907));
#22832=CARTESIAN_POINT('Ctrl Pts',(6.32976796473819,1.61522066995007,10.5687216653907));
#22833=CARTESIAN_POINT('Ctrl Pts',(6.50892555577775,-0.552060840994624,
10.5222908830264));
#22834=CARTESIAN_POINT('Ctrl Pts',(6.50892555577775,1.61522066995007,10.5222908830264));
#22835=CARTESIAN_POINT('Ctrl Pts',(6.68288828293941,-0.552060840994624,
10.462050267878));
#22836=CARTESIAN_POINT('Ctrl Pts',(6.68288828293941,1.61522066995007,10.462050267878));
#22837=CARTESIAN_POINT('Ctrl Pts',(6.84859008776107,-0.552060840994624,
10.3804015453596));
#22838=CARTESIAN_POINT('Ctrl Pts',(6.84859008776107,1.61522066995007,10.3804015453596));
#22839=CARTESIAN_POINT('Ctrl Pts',(7.00445448641038,-0.552060840994624,
10.2733319413005));
#22840=CARTESIAN_POINT('Ctrl Pts',(7.00445448641038,1.61522066995007,10.2733319413005));
#22841=CARTESIAN_POINT('Ctrl Pts',(7.15081550722288,-0.552060840994624,
10.1414720974144));
#22842=CARTESIAN_POINT('Ctrl Pts',(7.15081550722288,1.61522066995007,10.1414720974144));
#22843=CARTESIAN_POINT('Ctrl Pts',(7.28883796912684,-0.552060840994624,
9.98835756998534));
#22844=CARTESIAN_POINT('Ctrl Pts',(7.28883796912684,1.61522066995007,9.98835756998534));
#22845=CARTESIAN_POINT('Ctrl Pts',(7.41967047354988,-0.552060840994624,
9.81917361987377));
#22846=CARTESIAN_POINT('Ctrl Pts',(7.41967047354988,1.61522066995007,9.81917361987377));
#22847=CARTESIAN_POINT('Ctrl Pts',(7.54360573526532,-0.552060840994624,
9.63939026966049));
#22848=CARTESIAN_POINT('Ctrl Pts',(7.54360573526532,1.61522066995007,9.63939026966049));
#22849=CARTESIAN_POINT('Ctrl Pts',(7.6590003866074,-0.552060840994624,9.45324999450471));
#22850=CARTESIAN_POINT('Ctrl Pts',(7.6590003866074,1.61522066995007,9.45324999450471));
#22851=CARTESIAN_POINT('Ctrl Pts',(7.76209282457502,-0.552060840994624,
9.26297089919836));
#22852=CARTESIAN_POINT('Ctrl Pts',(7.76209282457502,1.61522066995007,9.26297089919836));
#22853=CARTESIAN_POINT('Ctrl Pts',(7.84862074946283,-0.552060840994624,
9.06945407017055));
#22854=CARTESIAN_POINT('Ctrl Pts',(7.84862074946283,1.61522066995007,9.06945407017055));
#22855=CARTESIAN_POINT('Ctrl Pts',(7.91508259073031,-0.552060840994624,
8.87266947141857));
#22856=CARTESIAN_POINT('Ctrl Pts',(7.91508259073031,1.61522066995007,8.87266947141857));
#22857=CARTESIAN_POINT('Ctrl Pts',(7.96007609558387,-0.552060840994624,
8.67216210283894));
#22858=CARTESIAN_POINT('Ctrl Pts',(7.96007609558387,1.61522066995007,8.67216210283894));
#22859=CARTESIAN_POINT('Ctrl Pts',(7.98575825096082,-0.552060840994624,
8.46752658699496));
#22860=CARTESIAN_POINT('Ctrl Pts',(7.98575825096082,1.61522066995007,8.46752658699496));
#22861=CARTESIAN_POINT('Ctrl Pts',(7.9987984391963,-0.552060840994624,8.25883677791438));
#22862=CARTESIAN_POINT('Ctrl Pts',(7.9987984391963,1.61522066995007,8.25883677791438));
#22863=CARTESIAN_POINT('Ctrl Pts',(8.00781893805568,-0.552060840994624,
8.04662057355209));
#22864=CARTESIAN_POINT('Ctrl Pts',(8.00781893805568,1.61522066995007,8.04662057355209));
#22865=CARTESIAN_POINT('Ctrl Pts',(8.02124364536257,-0.552060840994624,
7.8318867323277));
#22866=CARTESIAN_POINT('Ctrl Pts',(8.02124364536257,1.61522066995007,7.8318867323277));
#22867=CARTESIAN_POINT('Ctrl Pts',(8.04494633492827,-0.552060840994624,
7.61613341658679));
#22868=CARTESIAN_POINT('Ctrl Pts',(8.04494633492827,1.61522066995007,7.61613341658679));
#22869=CARTESIAN_POINT('Ctrl Pts',(8.08008348678094,-0.552060840994624,
7.40136016279815));
#22870=CARTESIAN_POINT('Ctrl Pts',(8.08008348678094,1.61522066995007,7.40136016279815));
#22871=CARTESIAN_POINT('Ctrl Pts',(8.12057943633426,-0.552060840994624,
7.19009032473197));
#22872=CARTESIAN_POINT('Ctrl Pts',(8.12057943633426,1.61522066995007,7.19009032473197));
#22873=CARTESIAN_POINT('Ctrl Pts',(8.15569042861283,-0.552060840994624,
6.98516923427904));
#22874=CARTESIAN_POINT('Ctrl Pts',(8.15569042861283,1.61522066995007,6.98516923427904));
#22875=CARTESIAN_POINT('Ctrl Pts',(8.17293082304204,-0.552060840994624,
6.78954489191915));
#22876=CARTESIAN_POINT('Ctrl Pts',(8.17293082304204,1.61522066995007,6.78954489191915));
#22877=CARTESIAN_POINT('Ctrl Pts',(8.16089752265956,-0.552060840994624,
6.60605451948904));
#22878=CARTESIAN_POINT('Ctrl Pts',(8.16089752265956,1.61522066995007,6.60605451948904));
#22879=CARTESIAN_POINT('Ctrl Pts',(8.11207116917844,-0.552060840994624,
6.43720976255638));
#22880=CARTESIAN_POINT('Ctrl Pts',(8.11207116917844,1.61522066995007,6.43720976255638));
#22881=CARTESIAN_POINT('Ctrl Pts',(8.02580908828092,-0.552060840994624,
6.28498018271691));
#22882=CARTESIAN_POINT('Ctrl Pts',(8.02580908828092,1.61522066995007,6.28498018271691));
#22883=CARTESIAN_POINT('Ctrl Pts',(7.90644860448881,-0.552060840994624,
6.15052660592943));
#22884=CARTESIAN_POINT('Ctrl Pts',(7.90644860448881,1.61522066995007,6.15052660592943));
#22885=CARTESIAN_POINT('Ctrl Pts',(7.76106756457749,-0.552060840994624,
6.03389995867286));
#22886=CARTESIAN_POINT('Ctrl Pts',(7.76106756457749,1.61522066995007,6.03389995867286));
#22887=CARTESIAN_POINT('Ctrl Pts',(7.59751903688427,-0.552060840994624,
5.93381436957244));
#22888=CARTESIAN_POINT('Ctrl Pts',(7.59751903688427,1.61522066995007,5.93381436957244));
#22889=CARTESIAN_POINT('Ctrl Pts',(7.42198551710643,-0.552060840994624,
5.84723737025948));
#22890=CARTESIAN_POINT('Ctrl Pts',(7.42198551710643,1.61522066995007,5.84723737025948));
#22891=CARTESIAN_POINT('Ctrl Pts',(7.23853768475023,-0.552060840994624,
5.76979878895671));
#22892=CARTESIAN_POINT('Ctrl Pts',(7.23853768475023,1.61522066995007,5.76979878895671));
#22893=CARTESIAN_POINT('Ctrl Pts',(7.04976847947264,-0.552060840994624,
5.69662713609756));
#22894=CARTESIAN_POINT('Ctrl Pts',(7.04976847947264,1.61522066995007,5.69662713609756));
#22895=CARTESIAN_POINT('Ctrl Pts',(6.85709976037512,-0.552060840994624,
5.62308582598972));
#22896=CARTESIAN_POINT('Ctrl Pts',(6.85709976037512,1.61522066995007,5.62308582598972));
#22897=CARTESIAN_POINT('Ctrl Pts',(6.66121503090593,-0.552060840994624,
5.54547963906641));
#22898=CARTESIAN_POINT('Ctrl Pts',(6.66121503090593,1.61522066995007,5.54547963906641));
#22899=CARTESIAN_POINT('Ctrl Pts',(6.46246210121974,-0.552060840994624,
5.46195513100458));
#22900=CARTESIAN_POINT('Ctrl Pts',(6.46246210121974,1.61522066995007,5.46195513100458));
#22901=CARTESIAN_POINT('Ctrl Pts',(6.26112587698791,-0.552060840994624,
5.37226655127806));
#22902=CARTESIAN_POINT('Ctrl Pts',(6.26112587698791,1.61522066995007,5.37226655127806));
#22903=CARTESIAN_POINT('Ctrl Pts',(6.05762450882876,-0.552060840994624,
5.27709955371581));
#22904=CARTESIAN_POINT('Ctrl Pts',(6.05762450882876,1.61522066995007,5.27709955371581));
#22905=CARTESIAN_POINT('Ctrl Pts',(5.85274048349253,-0.552060840994624,
5.17752467829117));
#22906=CARTESIAN_POINT('Ctrl Pts',(5.85274048349253,1.61522066995007,5.17752467829117));
#22907=CARTESIAN_POINT('Ctrl Pts',(5.6478173738032,-0.552060840994624,5.07442896098936));
#22908=CARTESIAN_POINT('Ctrl Pts',(5.6478173738032,1.61522066995007,5.07442896098936));
#22909=CARTESIAN_POINT('Ctrl Pts',(5.44501860313336,-0.552060840994624,
4.96787993373722));
#22910=CARTESIAN_POINT('Ctrl Pts',(5.44501860313336,1.61522066995007,4.96787993373722));
#22911=CARTESIAN_POINT('Ctrl Pts',(5.24741086000008,-0.552060840994624,
4.85676111532844));
#22912=CARTESIAN_POINT('Ctrl Pts',(5.24741086000008,1.61522066995007,4.85676111532844));
#22913=CARTESIAN_POINT('Ctrl Pts',(5.05850630701875,-0.552060840994624,
4.73929437247794));
#22914=CARTESIAN_POINT('Ctrl Pts',(5.05850630701875,1.61522066995007,4.73929437247794));
#22915=CARTESIAN_POINT('Ctrl Pts',(4.88190185104846,-0.552060840994624,
4.61340315498245));
#22916=CARTESIAN_POINT('Ctrl Pts',(4.88190185104846,1.61522066995007,4.61340315498245));
#22917=CARTESIAN_POINT('Ctrl Pts',(4.7208720035032,-0.552060840994624,4.47714872481864));
#22918=CARTESIAN_POINT('Ctrl Pts',(4.7208720035032,1.61522066995007,4.47714872481864));
#22919=CARTESIAN_POINT('Ctrl Pts',(4.57800047823784,-0.552060840994624,
4.32911151507775));
#22920=CARTESIAN_POINT('Ctrl Pts',(4.57800047823784,1.61522066995007,4.32911151507775));
#22921=CARTESIAN_POINT('Ctrl Pts',(4.4547451964031,-0.552060840994624,4.16885849319143));
#22922=CARTESIAN_POINT('Ctrl Pts',(4.4547451964031,1.61522066995007,4.16885849319143));
#22923=CARTESIAN_POINT('Ctrl Pts',(4.35148411330737,-0.552060840994624,
3.99681013615577));
#22924=CARTESIAN_POINT('Ctrl Pts',(4.35148411330737,1.61522066995007,3.99681013615577));
#22925=CARTESIAN_POINT('Ctrl Pts',(4.26765207024408,-0.552060840994624,
3.81399668859083));
#22926=CARTESIAN_POINT('Ctrl Pts',(4.26765207024408,1.61522066995007,3.81399668859083));
#22927=CARTESIAN_POINT('Ctrl Pts',(4.20184334854117,-0.552060840994624,
3.62185203209172));
#22928=CARTESIAN_POINT('Ctrl Pts',(4.20184334854117,1.61522066995007,3.62185203209172));
#22929=CARTESIAN_POINT('Ctrl Pts',(4.15193466045737,-0.552060840994624,
3.42199345348454));
#22930=CARTESIAN_POINT('Ctrl Pts',(4.15193466045737,1.61522066995007,3.42199345348454));
#22931=CARTESIAN_POINT('Ctrl Pts',(4.11518318246501,-0.552060840994624,
3.21600287470933));
#22932=CARTESIAN_POINT('Ctrl Pts',(4.11518318246501,1.61522066995007,3.21600287470933));
#22933=CARTESIAN_POINT('Ctrl Pts',(4.08854433447712,-0.552060840994624,
3.00529120729351));
#22934=CARTESIAN_POINT('Ctrl Pts',(4.08854433447712,1.61522066995007,3.00529120729351));
#22935=CARTESIAN_POINT('Ctrl Pts',(4.06899962712481,-0.552060840994624,
2.7909834104826));
#22936=CARTESIAN_POINT('Ctrl Pts',(4.06899962712481,1.61522066995007,2.7909834104826));
#22937=CARTESIAN_POINT('Ctrl Pts',(4.05390260344518,-0.552060840994624,
2.57377631141663));
#22938=CARTESIAN_POINT('Ctrl Pts',(4.05390260344518,1.61522066995007,2.57377631141663));
#22939=CARTESIAN_POINT('Ctrl Pts',(4.04126813644791,-0.552060840994624,
2.35385258470204));
#22940=CARTESIAN_POINT('Ctrl Pts',(4.04126813644791,1.61522066995007,2.35385258470204));
#22941=CARTESIAN_POINT('Ctrl Pts',(4.03021014446877,-0.552060840994624,
2.13065748555701));
#22942=CARTESIAN_POINT('Ctrl Pts',(4.03021014446877,1.61522066995007,2.13065748555701));
#22943=CARTESIAN_POINT('Ctrl Pts',(4.02066709528519,-0.552060840994624,
1.9033255681334));
#22944=CARTESIAN_POINT('Ctrl Pts',(4.02066709528519,1.61522066995007,1.9033255681334));
#22945=CARTESIAN_POINT('Ctrl Pts',(4.012782399266,-0.552060840994624,1.67142113207676));
#22946=CARTESIAN_POINT('Ctrl Pts',(4.012782399266,1.61522066995007,1.67142113207676));
#22947=CARTESIAN_POINT('Ctrl Pts',(4.00639322616619,-0.552060840994624,
1.4355810193293));
#22948=CARTESIAN_POINT('Ctrl Pts',(4.00639322616619,1.61522066995007,1.4355810193293));
#22949=CARTESIAN_POINT('Ctrl Pts',(4.00047520099043,-0.552060840994624,
1.19819542279832));
#22950=CARTESIAN_POINT('Ctrl Pts',(4.00047520099043,1.61522066995007,1.19819542279832));
#22951=CARTESIAN_POINT('Ctrl Pts',(3.99260375067002,-0.552060840994624,
0.964078729991153));
#22952=CARTESIAN_POINT('Ctrl Pts',(3.99260375067002,1.61522066995007,0.964078729991153));
#22953=CARTESIAN_POINT('Ctrl Pts',(3.97841403016118,-0.552060840994624,
0.741129277895168));
#22954=CARTESIAN_POINT('Ctrl Pts',(3.97841403016118,1.61522066995007,0.741129277895168));
#22955=CARTESIAN_POINT('Ctrl Pts',(3.95259200169988,-0.552060840994624,
0.538436816836329));
#22956=CARTESIAN_POINT('Ctrl Pts',(3.95259200169988,1.61522066995007,0.538436816836329));
#22957=CARTESIAN_POINT('Ctrl Pts',(3.90986572419832,-0.552060840994624,
0.364350357241537));
#22958=CARTESIAN_POINT('Ctrl Pts',(3.90986572419832,1.61522066995007,0.364350357241537));
#22959=CARTESIAN_POINT('Ctrl Pts',(3.84598208672298,-0.552060840994624,
0.224659532804428));
#22960=CARTESIAN_POINT('Ctrl Pts',(3.84598208672298,1.61522066995007,0.224659532804428));
#22961=CARTESIAN_POINT('Ctrl Pts',(3.75872318140661,-0.552060840994624,
0.120497232333236));
#22962=CARTESIAN_POINT('Ctrl Pts',(3.75872318140661,1.61522066995007,0.120497232333236));
#22963=CARTESIAN_POINT('Ctrl Pts',(3.64881642260075,-0.552060840994624,
0.0470540298718229));
#22964=CARTESIAN_POINT('Ctrl Pts',(3.64881642260075,1.61522066995007,0.0470540298718229));
#22965=CARTESIAN_POINT('Ctrl Pts',(3.52045328348988,-0.552060840994624,
-0.00118366394786523));
#22966=CARTESIAN_POINT('Ctrl Pts',(3.52045328348988,1.61522066995007,-0.00118366394786523));
#22967=CARTESIAN_POINT('Ctrl Pts',(3.3816469894381,-0.552060840994624,-0.0263068037111615));
#22968=CARTESIAN_POINT('Ctrl Pts',(3.3816469894381,1.61522066995007,-0.0263068037111615));
#22969=CARTESIAN_POINT('Ctrl Pts',(3.2451100102617,-0.552060840994624,-0.0214179570895094));
#22970=CARTESIAN_POINT('Ctrl Pts',(3.2451100102617,1.61522066995007,-0.0214179570895094));
#22971=CARTESIAN_POINT('Ctrl Pts',(3.12452733970665,-0.552060840994624,
0.0241851999814078));
#22972=CARTESIAN_POINT('Ctrl Pts',(3.12452733970665,1.61522066995007,0.0241851999814078));
#22973=CARTESIAN_POINT('Ctrl Pts',(3.03063129752059,-0.552060840994624,
0.119017371327004));
#22974=CARTESIAN_POINT('Ctrl Pts',(3.03063129752059,1.61522066995007,0.119017371327004));
#22975=CARTESIAN_POINT('Ctrl Pts',(2.96639254265844,-0.552060840994624,
0.262319630540593));
#22976=CARTESIAN_POINT('Ctrl Pts',(2.96639254265844,1.61522066995007,0.262319630540593));
#22977=CARTESIAN_POINT('Ctrl Pts',(2.92780415844446,-0.552060840994624,
0.444963858672424));
#22978=CARTESIAN_POINT('Ctrl Pts',(2.92780415844446,1.61522066995007,0.444963858672424));
#22979=CARTESIAN_POINT('Ctrl Pts',(2.90717911786689,-0.552060840994624,
0.65402023086958));
#22980=CARTESIAN_POINT('Ctrl Pts',(2.90717911786689,1.61522066995007,0.65402023086958));
#22981=CARTESIAN_POINT('Ctrl Pts',(2.89547076625581,-0.552060840994624,
0.875890304828918));
#22982=CARTESIAN_POINT('Ctrl Pts',(2.89547076625581,1.61522066995007,0.875890304828918));
#22983=CARTESIAN_POINT('Ctrl Pts',(2.88537704766906,-0.552060840994624,
1.10060381648398));
#22984=CARTESIAN_POINT('Ctrl Pts',(2.88537704766906,1.61522066995007,1.10060381648398));
#22985=CARTESIAN_POINT('Ctrl Pts',(2.8728456296504,-0.552060840994624,1.32371934078733));
#22986=CARTESIAN_POINT('Ctrl Pts',(2.8728456296504,1.61522066995007,1.32371934078733));
#22987=CARTESIAN_POINT('Ctrl Pts',(2.85578261679345,-0.552060840994624,
1.54401727992264));
#22988=CARTESIAN_POINT('Ctrl Pts',(2.85578261679345,1.61522066995007,1.54401727992264));
#22989=CARTESIAN_POINT('Ctrl Pts',(2.83335686249019,-0.552060840994624,
1.76209503442146));
#22990=CARTESIAN_POINT('Ctrl Pts',(2.83335686249019,1.61522066995007,1.76209503442146));
#22991=CARTESIAN_POINT('Ctrl Pts',(2.80505146480345,-0.552060840994624,
1.97856787413951));
#22992=CARTESIAN_POINT('Ctrl Pts',(2.80505146480345,1.61522066995007,1.97856787413951));
#22993=CARTESIAN_POINT('Ctrl Pts',(2.76985908233915,-0.552060840994624,
2.19251877196071));
#22994=CARTESIAN_POINT('Ctrl Pts',(2.76985908233915,1.61522066995007,2.19251877196071));
#22995=CARTESIAN_POINT('Ctrl Pts',(2.72531955636536,-0.552060840994624,
2.39962532458029));
#22996=CARTESIAN_POINT('Ctrl Pts',(2.72531955636536,1.61522066995007,2.39962532458029));
#22997=CARTESIAN_POINT('Ctrl Pts',(2.66797634363184,-0.552060840994624,
2.59347738935741));
#22998=CARTESIAN_POINT('Ctrl Pts',(2.66797634363184,1.61522066995007,2.59347738935741));
#22999=CARTESIAN_POINT('Ctrl Pts',(2.59397540849171,-0.552060840994624,
2.7672283971178));
#23000=CARTESIAN_POINT('Ctrl Pts',(2.59397540849171,1.61522066995007,2.7672283971178));
#23001=CARTESIAN_POINT('Ctrl Pts',(2.49960870420485,-0.552060840994624,
2.91510580081997));
#23002=CARTESIAN_POINT('Ctrl Pts',(2.49960870420485,1.61522066995007,2.91510580081997));
#23003=CARTESIAN_POINT('Ctrl Pts',(2.38189256086504,-0.552060840994624,
3.03403241435618));
#23004=CARTESIAN_POINT('Ctrl Pts',(2.38189256086504,1.61522066995007,3.03403241435618));
#23005=CARTESIAN_POINT('Ctrl Pts',(2.23909845280558,-0.552060840994624,
3.12505646843308));
#23006=CARTESIAN_POINT('Ctrl Pts',(2.23909845280558,1.61522066995007,3.12505646843308));
#23007=CARTESIAN_POINT('Ctrl Pts',(2.07061055216582,-0.552060840994624,
3.19196918412265));
#23008=CARTESIAN_POINT('Ctrl Pts',(2.07061055216582,1.61522066995007,3.19196918412265));
#23009=CARTESIAN_POINT('Ctrl Pts',(1.87681490437036,-0.552060840994624,
3.24001322621211));
#23010=CARTESIAN_POINT('Ctrl Pts',(1.87681490437036,1.61522066995007,3.24001322621211));
#23011=CARTESIAN_POINT('Ctrl Pts',(1.65897747541321,-0.552060840994624,
3.27464765209773));
#23012=CARTESIAN_POINT('Ctrl Pts',(1.65897747541321,1.61522066995007,3.27464765209773));
#23013=CARTESIAN_POINT('Ctrl Pts',(1.4191255439272,-0.552060840994624,3.30006519349576));
#23014=CARTESIAN_POINT('Ctrl Pts',(1.4191255439272,1.61522066995007,3.30006519349576));
#23015=CARTESIAN_POINT('Ctrl Pts',(1.15993538533448,-0.552060840994624,
3.31897283641381));
#23016=CARTESIAN_POINT('Ctrl Pts',(1.15993538533448,1.61522066995007,3.31897283641381));
#23017=CARTESIAN_POINT('Ctrl Pts',(0.884625090385968,-0.552060840994624,
3.33300441174764));
#23018=CARTESIAN_POINT('Ctrl Pts',(0.884625090385968,1.61522066995007,3.33300441174764));
#23019=CARTESIAN_POINT('Ctrl Pts',(0.596845720618978,-0.552060840994624,
3.34293392264922));
#23020=CARTESIAN_POINT('Ctrl Pts',(0.596845720618978,1.61522066995007,3.34293392264922));
#23021=CARTESIAN_POINT('Ctrl Pts',(0.30057321210183,-0.552060840994624,
3.34897162637417));
#23022=CARTESIAN_POINT('Ctrl Pts',(0.30057321210183,1.61522066995007,3.34897162637417));
#23023=CARTESIAN_POINT('Ctrl Pts',(1.66741620510891E-14,-0.552060840994624,
3.35102435732185));
#23024=CARTESIAN_POINT('Ctrl Pts',(1.66741620510891E-14,1.61522066995007,
3.35102435732185));
#23025=CARTESIAN_POINT('Ctrl Pts',(-0.300573212101791,-0.552060840994624,
3.34897162637426));
#23026=CARTESIAN_POINT('Ctrl Pts',(-0.300573212101791,1.61522066995007,
3.34897162637426));
#23027=CARTESIAN_POINT('Ctrl Pts',(-0.596845720618908,-0.552060840994624,
3.34293392264938));
#23028=CARTESIAN_POINT('Ctrl Pts',(-0.596845720618908,1.61522066995007,
3.34293392264938));
#23029=CARTESIAN_POINT('Ctrl Pts',(-0.884625090385886,-0.552060840994624,
3.33300441174785));
#23030=CARTESIAN_POINT('Ctrl Pts',(-0.884625090385886,1.61522066995007,
3.33300441174785));
#23031=CARTESIAN_POINT('Ctrl Pts',(-1.15993538533442,-0.552060840994624,
3.31897283641402));
#23032=CARTESIAN_POINT('Ctrl Pts',(-1.15993538533442,1.61522066995007,3.31897283641402));
#23033=CARTESIAN_POINT('Ctrl Pts',(-1.41912554392716,-0.552060840994624,
3.30006519349591));
#23034=CARTESIAN_POINT('Ctrl Pts',(-1.41912554392716,1.61522066995007,3.30006519349591));
#23035=CARTESIAN_POINT('Ctrl Pts',(-1.65897747541319,-0.552060840994624,
3.27464765209779));
#23036=CARTESIAN_POINT('Ctrl Pts',(-1.65897747541319,1.61522066995007,3.27464765209779));
#23037=CARTESIAN_POINT('Ctrl Pts',(-1.87681490437034,-0.552060840994624,
3.24001322621208));
#23038=CARTESIAN_POINT('Ctrl Pts',(-1.87681490437034,1.61522066995007,3.24001322621208));
#23039=CARTESIAN_POINT('Ctrl Pts',(-2.07061055216576,-0.552060840994624,
3.19196918412254));
#23040=CARTESIAN_POINT('Ctrl Pts',(-2.07061055216576,1.61522066995007,3.19196918412254));
#23041=CARTESIAN_POINT('Ctrl Pts',(-2.23909845280547,-0.552060840994624,
3.12505646843295));
#23042=CARTESIAN_POINT('Ctrl Pts',(-2.23909845280547,1.61522066995007,3.12505646843295));
#23043=CARTESIAN_POINT('Ctrl Pts',(-2.38189256086493,-0.552060840994624,
3.03403241435609));
#23044=CARTESIAN_POINT('Ctrl Pts',(-2.38189256086493,1.61522066995007,3.03403241435609));
#23045=CARTESIAN_POINT('Ctrl Pts',(-2.49960870420481,-0.552060840994624,
2.91510580081997));
#23046=CARTESIAN_POINT('Ctrl Pts',(-2.49960870420481,1.61522066995007,2.91510580081997));
#23047=CARTESIAN_POINT('Ctrl Pts',(-2.59397540849182,-0.552060840994624,
2.76722839711793));
#23048=CARTESIAN_POINT('Ctrl Pts',(-2.59397540849182,1.61522066995007,2.76722839711793));
#23049=CARTESIAN_POINT('Ctrl Pts',(-2.66797634363209,-0.552060840994624,
2.59347738935767));
#23050=CARTESIAN_POINT('Ctrl Pts',(-2.66797634363209,1.61522066995007,2.59347738935767));
#23051=CARTESIAN_POINT('Ctrl Pts',(-2.72531955636566,-0.552060840994624,
2.39962532458057));
#23052=CARTESIAN_POINT('Ctrl Pts',(-2.72531955636566,1.61522066995007,2.39962532458057));
#23053=CARTESIAN_POINT('Ctrl Pts',(-2.76985908233936,-0.552060840994624,
2.19251877196088));
#23054=CARTESIAN_POINT('Ctrl Pts',(-2.76985908233936,1.61522066995007,2.19251877196088));
#23055=CARTESIAN_POINT('Ctrl Pts',(-2.80505146480344,-0.552060840994624,
1.97856787413951));
#23056=CARTESIAN_POINT('Ctrl Pts',(-2.80505146480344,1.61522066995007,1.97856787413951));
#23057=CARTESIAN_POINT('Ctrl Pts',(-2.8333568624899,-0.552060840994624,
1.76209503442131));
#23058=CARTESIAN_POINT('Ctrl Pts',(-2.8333568624899,1.61522066995007,1.76209503442131));
#23059=CARTESIAN_POINT('Ctrl Pts',(-2.85578261679294,-0.552060840994624,
1.54401727992238));
#23060=CARTESIAN_POINT('Ctrl Pts',(-2.85578261679294,1.61522066995007,1.54401727992238));
#23061=CARTESIAN_POINT('Ctrl Pts',(-2.87284562964987,-0.552060840994624,
1.32371934078708));
#23062=CARTESIAN_POINT('Ctrl Pts',(-2.87284562964987,1.61522066995007,1.32371934078708));
#23063=CARTESIAN_POINT('Ctrl Pts',(-2.88537704766869,-0.552060840994624,
1.10060381648384));
#23064=CARTESIAN_POINT('Ctrl Pts',(-2.88537704766869,1.61522066995007,1.10060381648384));
#23065=CARTESIAN_POINT('Ctrl Pts',(-2.89547076625573,-0.552060840994624,
0.875890304828914));
#23066=CARTESIAN_POINT('Ctrl Pts',(-2.89547076625573,1.61522066995007,0.875890304828914));
#23067=CARTESIAN_POINT('Ctrl Pts',(-2.90717911786707,-0.552060840994624,
0.654020230869684));
#23068=CARTESIAN_POINT('Ctrl Pts',(-2.90717911786707,1.61522066995007,0.654020230869684));
#23069=CARTESIAN_POINT('Ctrl Pts',(-2.92780415844476,-0.552060840994624,
0.444963858672577));
#23070=CARTESIAN_POINT('Ctrl Pts',(-2.92780415844476,1.61522066995007,0.444963858672577));
#23071=CARTESIAN_POINT('Ctrl Pts',(-2.96639254265869,-0.552060840994624,
0.262319630540737));
#23072=CARTESIAN_POINT('Ctrl Pts',(-2.96639254265869,1.61522066995007,0.262319630540737));
#23073=CARTESIAN_POINT('Ctrl Pts',(-3.03063129752067,-0.552060840994624,
0.11901737132707));
#23074=CARTESIAN_POINT('Ctrl Pts',(-3.03063129752067,1.61522066995007,0.11901737132707));
#23075=CARTESIAN_POINT('Ctrl Pts',(-3.12452733970658,-0.552060840994624,
0.0241851999813871));
#23076=CARTESIAN_POINT('Ctrl Pts',(-3.12452733970658,1.61522066995007,0.0241851999813871));
#23077=CARTESIAN_POINT('Ctrl Pts',(-3.24511001026157,-0.552060840994624,
-0.0214179570895714));
#23078=CARTESIAN_POINT('Ctrl Pts',(-3.24511001026157,1.61522066995007,-0.0214179570895714));
#23079=CARTESIAN_POINT('Ctrl Pts',(-3.38164698943802,-0.552060840994624,
-0.0263068037112043));
#23080=CARTESIAN_POINT('Ctrl Pts',(-3.38164698943802,1.61522066995007,-0.0263068037112043));
#23081=CARTESIAN_POINT('Ctrl Pts',(-3.52045328348989,-0.552060840994624,
-0.00118366394785932));
#23082=CARTESIAN_POINT('Ctrl Pts',(-3.52045328348989,1.61522066995007,-0.00118366394785932));
#23083=CARTESIAN_POINT('Ctrl Pts',(-3.64881642260079,-0.552060840994624,
0.0470540298718583));
#23084=CARTESIAN_POINT('Ctrl Pts',(-3.64881642260079,1.61522066995007,0.0470540298718583));
#23085=CARTESIAN_POINT('Ctrl Pts',(-3.75872318140663,-0.552060840994624,
0.120497232333251));
#23086=CARTESIAN_POINT('Ctrl Pts',(-3.75872318140663,1.61522066995007,0.120497232333251));
#23087=CARTESIAN_POINT('Ctrl Pts',(-3.84598208672296,-0.552060840994624,
0.224659532804408));
#23088=CARTESIAN_POINT('Ctrl Pts',(-3.84598208672296,1.61522066995007,0.224659532804408));
#23089=CARTESIAN_POINT('Ctrl Pts',(-3.9098657241983,-0.552060840994624,
0.364350357241515));
#23090=CARTESIAN_POINT('Ctrl Pts',(-3.9098657241983,1.61522066995007,0.364350357241515));
#23091=CARTESIAN_POINT('Ctrl Pts',(-3.9525920016999,-0.552060840994624,
0.538436816836325));
#23092=CARTESIAN_POINT('Ctrl Pts',(-3.9525920016999,1.61522066995007,0.538436816836325));
#23093=CARTESIAN_POINT('Ctrl Pts',(-3.97841403016126,-0.552060840994624,
0.741129277895169));
#23094=CARTESIAN_POINT('Ctrl Pts',(-3.97841403016126,1.61522066995007,0.741129277895169));
#23095=CARTESIAN_POINT('Ctrl Pts',(-3.99260375067011,-0.552060840994624,
0.964078729991154));
#23096=CARTESIAN_POINT('Ctrl Pts',(-3.99260375067011,1.61522066995007,0.964078729991154));
#23097=CARTESIAN_POINT('Ctrl Pts',(-4.00047520099045,-0.552060840994624,
1.1981954227983));
#23098=CARTESIAN_POINT('Ctrl Pts',(-4.00047520099045,1.61522066995007,1.1981954227983));
#23099=CARTESIAN_POINT('Ctrl Pts',(-4.00639322616607,-0.552060840994624,
1.43558101932923));
#23100=CARTESIAN_POINT('Ctrl Pts',(-4.00639322616607,1.61522066995007,1.43558101932923));
#23101=CARTESIAN_POINT('Ctrl Pts',(-4.01278239926574,-0.552060840994624,
1.67142113207667));
#23102=CARTESIAN_POINT('Ctrl Pts',(-4.01278239926574,1.61522066995007,1.67142113207667));
#23103=CARTESIAN_POINT('Ctrl Pts',(-4.02066709528487,-0.552060840994624,
1.90332556813333));
#23104=CARTESIAN_POINT('Ctrl Pts',(-4.02066709528487,1.61522066995007,1.90332556813333));
#23105=CARTESIAN_POINT('Ctrl Pts',(-4.0302101444685,-0.552060840994624,
2.130657485557));
#23106=CARTESIAN_POINT('Ctrl Pts',(-4.0302101444685,1.61522066995007,2.130657485557));
#23107=CARTESIAN_POINT('Ctrl Pts',(-4.04126813644779,-0.552060840994624,
2.35385258470204));
#23108=CARTESIAN_POINT('Ctrl Pts',(-4.04126813644779,1.61522066995007,2.35385258470204));
#23109=CARTESIAN_POINT('Ctrl Pts',(-4.05390260344525,-0.552060840994624,
2.57377631141659));
#23110=CARTESIAN_POINT('Ctrl Pts',(-4.05390260344525,1.61522066995007,2.57377631141659));
#23111=CARTESIAN_POINT('Ctrl Pts',(-4.06899962712502,-0.552060840994624,
2.7909834104825));
#23112=CARTESIAN_POINT('Ctrl Pts',(-4.06899962712502,1.61522066995007,2.7909834104825));
#23113=CARTESIAN_POINT('Ctrl Pts',(-4.08854433447739,-0.552060840994624,
3.00529120729338));
#23114=CARTESIAN_POINT('Ctrl Pts',(-4.08854433447739,1.61522066995007,3.00529120729338));
#23115=CARTESIAN_POINT('Ctrl Pts',(-4.11518318246524,-0.552060840994624,
3.21600287470921));
#23116=CARTESIAN_POINT('Ctrl Pts',(-4.11518318246524,1.61522066995007,3.21600287470921));
#23117=CARTESIAN_POINT('Ctrl Pts',(-4.15193466045748,-0.552060840994624,
3.42199345348447));
#23118=CARTESIAN_POINT('Ctrl Pts',(-4.15193466045748,1.61522066995007,3.42199345348447));
#23119=CARTESIAN_POINT('Ctrl Pts',(-4.20184334854115,-0.552060840994624,
3.62185203209171));
#23120=CARTESIAN_POINT('Ctrl Pts',(-4.20184334854115,1.61522066995007,3.62185203209171));
#23121=CARTESIAN_POINT('Ctrl Pts',(-4.26765207024395,-0.552060840994624,
3.81399668859083));
#23122=CARTESIAN_POINT('Ctrl Pts',(-4.26765207024395,1.61522066995007,3.81399668859083));
#23123=CARTESIAN_POINT('Ctrl Pts',(-4.35148411330718,-0.552060840994624,
3.99681013615577));
#23124=CARTESIAN_POINT('Ctrl Pts',(-4.35148411330718,1.61522066995007,3.99681013615577));
#23125=CARTESIAN_POINT('Ctrl Pts',(-4.45474519640294,-0.552060840994624,
4.16885849319142));
#23126=CARTESIAN_POINT('Ctrl Pts',(-4.45474519640294,1.61522066995007,4.16885849319142));
#23127=CARTESIAN_POINT('Ctrl Pts',(-4.57800047823775,-0.552060840994624,
4.32911151507774));
#23128=CARTESIAN_POINT('Ctrl Pts',(-4.57800047823775,1.61522066995007,4.32911151507774));
#23129=CARTESIAN_POINT('Ctrl Pts',(-4.7208720035032,-0.552060840994624,
4.47714872481861));
#23130=CARTESIAN_POINT('Ctrl Pts',(-4.7208720035032,1.61522066995007,4.47714872481861));
#23131=CARTESIAN_POINT('Ctrl Pts',(-4.88190185104852,-0.552060840994624,
4.61340315498244));
#23132=CARTESIAN_POINT('Ctrl Pts',(-4.88190185104852,1.61522066995007,4.61340315498244));
#23133=CARTESIAN_POINT('Ctrl Pts',(-5.05850630701885,-0.552060840994624,
4.73929437247796));
#23134=CARTESIAN_POINT('Ctrl Pts',(-5.05850630701885,1.61522066995007,4.73929437247796));
#23135=CARTESIAN_POINT('Ctrl Pts',(-5.24741086000019,-0.552060840994624,
4.8567611153285));
#23136=CARTESIAN_POINT('Ctrl Pts',(-5.24741086000019,1.61522066995007,4.8567611153285));
#23137=CARTESIAN_POINT('Ctrl Pts',(-5.44501860313342,-0.552060840994624,
4.96787993373728));
#23138=CARTESIAN_POINT('Ctrl Pts',(-5.44501860313342,1.61522066995007,4.96787993373728));
#23139=CARTESIAN_POINT('Ctrl Pts',(-5.64781737380319,-0.552060840994624,
5.07442896098937));
#23140=CARTESIAN_POINT('Ctrl Pts',(-5.64781737380319,1.61522066995007,5.07442896098937));
#23141=CARTESIAN_POINT('Ctrl Pts',(-5.85274048349242,-0.552060840994624,
5.17752467829109));
#23142=CARTESIAN_POINT('Ctrl Pts',(-5.85274048349242,1.61522066995007,5.17752467829109));
#23143=CARTESIAN_POINT('Ctrl Pts',(-6.05762450882858,-0.552060840994624,
5.27709955371564));
#23144=CARTESIAN_POINT('Ctrl Pts',(-6.05762450882858,1.61522066995007,5.27709955371564));
#23145=CARTESIAN_POINT('Ctrl Pts',(-6.26112587698772,-0.552060840994624,
5.37226655127787));
#23146=CARTESIAN_POINT('Ctrl Pts',(-6.26112587698772,1.61522066995007,5.37226655127787));
#23147=CARTESIAN_POINT('Ctrl Pts',(-6.46246210121964,-0.552060840994624,
5.46195513100446));
#23148=CARTESIAN_POINT('Ctrl Pts',(-6.46246210121964,1.61522066995007,5.46195513100446));
#23149=CARTESIAN_POINT('Ctrl Pts',(-6.66121503090592,-0.552060840994624,
5.54547963906637));
#23150=CARTESIAN_POINT('Ctrl Pts',(-6.66121503090592,1.61522066995007,5.54547963906637));
#23151=CARTESIAN_POINT('Ctrl Pts',(-6.8570997603751,-0.552060840994624,
5.62308582598972));
#23152=CARTESIAN_POINT('Ctrl Pts',(-6.8570997603751,1.61522066995007,5.62308582598972));
#23153=CARTESIAN_POINT('Ctrl Pts',(-7.04976847947249,-0.552060840994624,
5.69662713609756));
#23154=CARTESIAN_POINT('Ctrl Pts',(-7.04976847947249,1.61522066995007,5.69662713609756));
#23155=CARTESIAN_POINT('Ctrl Pts',(-7.23853768475,-0.552060840994624,5.76979878895672));
#23156=CARTESIAN_POINT('Ctrl Pts',(-7.23853768475,1.61522066995007,5.76979878895672));
#23157=CARTESIAN_POINT('Ctrl Pts',(-7.42198551710617,-0.552060840994624,
5.84723737025949));
#23158=CARTESIAN_POINT('Ctrl Pts',(-7.42198551710617,1.61522066995007,5.84723737025949));
#23159=CARTESIAN_POINT('Ctrl Pts',(-7.59751903688412,-0.552060840994624,
5.93381436957244));
#23160=CARTESIAN_POINT('Ctrl Pts',(-7.59751903688412,1.61522066995007,5.93381436957244));
#23161=CARTESIAN_POINT('Ctrl Pts',(-7.76106756457753,-0.552060840994624,
6.03389995867283));
#23162=CARTESIAN_POINT('Ctrl Pts',(-7.76106756457753,1.61522066995007,6.03389995867283));
#23163=CARTESIAN_POINT('Ctrl Pts',(-7.90644860448901,-0.552060840994624,
6.15052660592937));
#23164=CARTESIAN_POINT('Ctrl Pts',(-7.90644860448901,1.61522066995007,6.15052660592937));
#23165=CARTESIAN_POINT('Ctrl Pts',(-8.02580908828117,-0.552060840994624,
6.28498018271686));
#23166=CARTESIAN_POINT('Ctrl Pts',(-8.02580908828117,1.61522066995007,6.28498018271686));
#23167=CARTESIAN_POINT('Ctrl Pts',(-8.11207116917861,-0.552060840994624,
6.43720976255636));
#23168=CARTESIAN_POINT('Ctrl Pts',(-8.11207116917861,1.61522066995007,6.43720976255636));
#23169=CARTESIAN_POINT('Ctrl Pts',(-8.16089752265956,-0.552060840994624,
6.60605451948903));
#23170=CARTESIAN_POINT('Ctrl Pts',(-8.16089752265956,1.61522066995007,6.60605451948903));
#23171=CARTESIAN_POINT('Ctrl Pts',(-8.17293082304181,-0.552060840994624,
6.78954489191904));
#23172=CARTESIAN_POINT('Ctrl Pts',(-8.17293082304181,1.61522066995007,6.78954489191904));
#23173=CARTESIAN_POINT('Ctrl Pts',(-8.15569042861244,-0.552060840994624,
6.9851692342788));
#23174=CARTESIAN_POINT('Ctrl Pts',(-8.15569042861244,1.61522066995007,6.9851692342788));
#23175=CARTESIAN_POINT('Ctrl Pts',(-8.12057943633387,-0.552060840994624,
7.19009032473164));
#23176=CARTESIAN_POINT('Ctrl Pts',(-8.12057943633387,1.61522066995007,7.19009032473164));
#23177=CARTESIAN_POINT('Ctrl Pts',(-8.08008348678073,-0.552060840994624,
7.40136016279791));
#23178=CARTESIAN_POINT('Ctrl Pts',(-8.08008348678073,1.61522066995007,7.40136016279791));
#23179=CARTESIAN_POINT('Ctrl Pts',(-8.04494633492831,-0.552060840994624,
7.61613341658677));
#23180=CARTESIAN_POINT('Ctrl Pts',(-8.04494633492831,1.61522066995007,7.61613341658677));
#23181=CARTESIAN_POINT('Ctrl Pts',(-8.02124364536279,-0.552060840994624,
7.83188673232793));
#23182=CARTESIAN_POINT('Ctrl Pts',(-8.02124364536279,1.61522066995007,7.83188673232793));
#23183=CARTESIAN_POINT('Ctrl Pts',(-8.007818938056,-0.552060840994624,8.04662057355248));
#23184=CARTESIAN_POINT('Ctrl Pts',(-8.007818938056,1.61522066995007,8.04662057355248));
#23185=CARTESIAN_POINT('Ctrl Pts',(-7.99879843919661,-0.552060840994624,
8.25883677791483));
#23186=CARTESIAN_POINT('Ctrl Pts',(-7.99879843919661,1.61522066995007,8.25883677791483));
#23187=CARTESIAN_POINT('Ctrl Pts',(-7.98575825096101,-0.552060840994624,
8.46752658699528));
#23188=CARTESIAN_POINT('Ctrl Pts',(-7.98575825096101,1.61522066995007,8.46752658699528));
#23189=CARTESIAN_POINT('Ctrl Pts',(-7.96007609558389,-0.552060840994624,
8.67216210283896));
#23190=CARTESIAN_POINT('Ctrl Pts',(-7.96007609558389,1.61522066995007,8.67216210283896));
#23191=CARTESIAN_POINT('Ctrl Pts',(-7.91508259073019,-0.552060840994624,
8.87266947141823));
#23192=CARTESIAN_POINT('Ctrl Pts',(-7.91508259073019,1.61522066995007,8.87266947141823));
#23193=CARTESIAN_POINT('Ctrl Pts',(-7.84862074946261,-0.552060840994624,
9.06945407016992));
#23194=CARTESIAN_POINT('Ctrl Pts',(-7.84862074946261,1.61522066995007,9.06945407016992));
#23195=CARTESIAN_POINT('Ctrl Pts',(-7.76209282457479,-0.552060840994624,
9.26297089919765));
#23196=CARTESIAN_POINT('Ctrl Pts',(-7.76209282457479,1.61522066995007,9.26297089919765));
#23197=CARTESIAN_POINT('Ctrl Pts',(-7.65900038660722,-0.552060840994624,
9.4532499945042));
#23198=CARTESIAN_POINT('Ctrl Pts',(-7.65900038660722,1.61522066995007,9.4532499945042));
#23199=CARTESIAN_POINT('Ctrl Pts',(-7.5436057352653,-0.552060840994624,
9.63939026966035));
#23200=CARTESIAN_POINT('Ctrl Pts',(-7.5436057352653,1.61522066995007,9.63939026966035));
#23201=CARTESIAN_POINT('Ctrl Pts',(-7.41967047355001,-0.552060840994624,
9.81917361987397));
#23202=CARTESIAN_POINT('Ctrl Pts',(-7.41967047355001,1.61522066995007,9.81917361987397));
#23203=CARTESIAN_POINT('Ctrl Pts',(-7.28883796912703,-0.552060840994624,
9.98835756998572));
#23204=CARTESIAN_POINT('Ctrl Pts',(-7.28883796912703,1.61522066995007,9.98835756998572));
#23205=CARTESIAN_POINT('Ctrl Pts',(-7.15081550722306,-0.552060840994624,
10.1414720974148));
#23206=CARTESIAN_POINT('Ctrl Pts',(-7.15081550722306,1.61522066995007,10.1414720974148));
#23207=CARTESIAN_POINT('Ctrl Pts',(-7.0044544864105,-0.552060840994624,
10.2733319413008));
#23208=CARTESIAN_POINT('Ctrl Pts',(-7.0044544864105,1.61522066995007,10.2733319413008));
#23209=CARTESIAN_POINT('Ctrl Pts',(-6.84859008776113,-0.552060840994624,
10.3804015453596));
#23210=CARTESIAN_POINT('Ctrl Pts',(-6.84859008776113,1.61522066995007,10.3804015453596));
#23211=CARTESIAN_POINT('Ctrl Pts',(-6.68288828293938,-0.552060840994624,
10.4620502678778));
#23212=CARTESIAN_POINT('Ctrl Pts',(-6.68288828293938,1.61522066995007,10.4620502678778));
#23213=CARTESIAN_POINT('Ctrl Pts',(-6.50892555577766,-0.552060840994624,
10.522290883026));
#23214=CARTESIAN_POINT('Ctrl Pts',(-6.50892555577766,1.61522066995007,10.522290883026));
#23215=CARTESIAN_POINT('Ctrl Pts',(-6.32976796473811,-0.552060840994624,
10.5687216653902));
#23216=CARTESIAN_POINT('Ctrl Pts',(-6.32976796473811,1.61522066995007,10.5687216653902));
#23217=CARTESIAN_POINT('Ctrl Pts',(-6.14893768388701,-0.552060840994624,
10.6103475969885));
#23218=CARTESIAN_POINT('Ctrl Pts',(-6.14893768388701,1.61522066995007,10.6103475969885));
#23219=CARTESIAN_POINT('Ctrl Pts',(-5.96961932707142,-0.552060840994624,
10.6558377434043));
#23220=CARTESIAN_POINT('Ctrl Pts',(-5.96961932707142,1.61522066995007,10.6558377434043));
#23221=CARTESIAN_POINT('Ctrl Pts',(-5.79367695415031,-0.552060840994624,
10.7114411549114));
#23222=CARTESIAN_POINT('Ctrl Pts',(-5.79367695415031,1.61522066995007,10.7114411549114));
#23223=CARTESIAN_POINT('Ctrl Pts',(-5.62101499943431,-0.552060840994624,
10.7795199127535));
#23224=CARTESIAN_POINT('Ctrl Pts',(-5.62101499943431,1.61522066995007,10.7795199127535));
#23225=CARTESIAN_POINT('Ctrl Pts',(-5.45051506148982,-0.552060840994624,
10.8599381259737));
#23226=CARTESIAN_POINT('Ctrl Pts',(-5.45051506148982,1.61522066995007,10.8599381259737));
#23227=CARTESIAN_POINT('Ctrl Pts',(-5.28082876351929,-0.552060840994624,
10.9511663773826));
#23228=CARTESIAN_POINT('Ctrl Pts',(-5.28082876351929,1.61522066995007,10.9511663773826));
#23229=CARTESIAN_POINT('Ctrl Pts',(-5.11112998264616,-0.552060840994624,
11.0513704191329));
#23230=CARTESIAN_POINT('Ctrl Pts',(-5.11112998264616,1.61522066995007,11.0513704191329));
#23231=CARTESIAN_POINT('Ctrl Pts',(-4.94211773226973,-0.552060840994624,
11.1598106424589));
#23232=CARTESIAN_POINT('Ctrl Pts',(-4.94211773226973,1.61522066995007,11.1598106424589));
#23233=CARTESIAN_POINT('Ctrl Pts',(-4.77596612414951,-0.552060840994624,
11.2768795166235));
#23234=CARTESIAN_POINT('Ctrl Pts',(-4.77596612414951,1.61522066995007,11.2768795166235));
#23235=CARTESIAN_POINT('Ctrl Pts',(-4.61532593596946,-0.552060840994624,
11.4029224160731));
#23236=CARTESIAN_POINT('Ctrl Pts',(-4.61532593596946,1.61522066995007,11.4029224160731));
#23237=CARTESIAN_POINT('Ctrl Pts',(-4.46255574628757,-0.552060840994624,
11.5373242211527));
#23238=CARTESIAN_POINT('Ctrl Pts',(-4.46255574628757,1.61522066995007,11.5373242211527));
#23239=CARTESIAN_POINT('Ctrl Pts',(-4.31893584999241,-0.552060840994624,
11.6776492463597));
#23240=CARTESIAN_POINT('Ctrl Pts',(-4.31893584999241,1.61522066995007,11.6776492463597));
#23241=CARTESIAN_POINT('Ctrl Pts',(-4.18369962429796,-0.552060840994624,
11.8183570873721));
#23242=CARTESIAN_POINT('Ctrl Pts',(-4.18369962429796,1.61522066995007,11.8183570873721));
#23243=CARTESIAN_POINT('Ctrl Pts',(-4.05395481372655,-0.552060840994624,
11.9514202619522));
#23244=CARTESIAN_POINT('Ctrl Pts',(-4.05395481372655,1.61522066995007,11.9514202619522));
#23245=CARTESIAN_POINT('Ctrl Pts',(-3.92533033057354,-0.552060840994624,
12.0684942936867));
#23246=CARTESIAN_POINT('Ctrl Pts',(-3.92533033057354,1.61522066995007,12.0684942936867));
#23247=CARTESIAN_POINT('Ctrl Pts',(-3.79241297762166,-0.552060840994624,
12.1626050652586));
#23248=CARTESIAN_POINT('Ctrl Pts',(-3.79241297762166,1.61522066995007,12.1626050652586));
#23249=CARTESIAN_POINT('Ctrl Pts',(-3.64927048315908,-0.552060840994624,
12.2301117722809));
#23250=CARTESIAN_POINT('Ctrl Pts',(-3.64927048315908,1.61522066995007,12.2301117722809));
#23251=CARTESIAN_POINT('Ctrl Pts',(-3.48993681214334,-0.552060840994624,
12.2723364229645));
#23252=CARTESIAN_POINT('Ctrl Pts',(-3.48993681214334,1.61522066995007,12.2723364229645));
#23253=CARTESIAN_POINT('Ctrl Pts',(-3.30884480305534,-0.552060840994624,
12.2938762651139));
#23254=CARTESIAN_POINT('Ctrl Pts',(-3.30884480305534,1.61522066995007,12.2938762651139));
#23255=CARTESIAN_POINT('Ctrl Pts',(-3.10127560868576,-0.552060840994624,
12.3010487961981));
#23256=CARTESIAN_POINT('Ctrl Pts',(-3.10127560868576,1.61522066995007,12.3010487961981));
#23257=CARTESIAN_POINT('Ctrl Pts',(-2.86376302967345,-0.552060840994624,
12.300400839059));
#23258=CARTESIAN_POINT('Ctrl Pts',(-2.86376302967345,1.61522066995007,12.300400839059));
#23259=CARTESIAN_POINT('Ctrl Pts',(-2.59461297443094,-0.552060840994624,
12.2969132923574));
#23260=CARTESIAN_POINT('Ctrl Pts',(-2.59461297443094,1.61522066995007,12.2969132923574));
#23261=CARTESIAN_POINT('Ctrl Pts',(-2.29394197380209,-0.552060840994624,
12.2935845551224));
#23262=CARTESIAN_POINT('Ctrl Pts',(-2.29394197380209,1.61522066995007,12.2935845551224));
#23263=CARTESIAN_POINT('Ctrl Pts',(-1.96338745719135,-0.552060840994624,
12.2919684497906));
#23264=CARTESIAN_POINT('Ctrl Pts',(-1.96338745719135,1.61522066995007,12.2919684497906));
#23265=CARTESIAN_POINT('Ctrl Pts',(-1.60591558979456,-0.552060840994624,
12.2924280531798));
#23266=CARTESIAN_POINT('Ctrl Pts',(-1.60591558979456,1.61522066995007,12.2924280531798));
#23267=CARTESIAN_POINT('Ctrl Pts',(-1.22558901314075,-0.552060840994624,
12.2945066442122));
#23268=CARTESIAN_POINT('Ctrl Pts',(-1.22558901314075,1.61522066995007,12.2945066442122));
#23269=CARTESIAN_POINT('Ctrl Pts',(-0.827351903312651,-0.552060840994624,
12.2972483292773));
#23270=CARTESIAN_POINT('Ctrl Pts',(-0.827351903312651,1.61522066995007,
12.2972483292773));
#23271=CARTESIAN_POINT('Ctrl Pts',(-0.498916532526571,-0.552060840994624,
12.299081889758));
#23272=CARTESIAN_POINT('Ctrl Pts',(-0.498916532526571,1.61522066995007,
12.299081889758));
#23273=CARTESIAN_POINT('Ctrl Pts',(-0.249771440080693,-0.552060840994624,
12.2998330708668));
#23274=CARTESIAN_POINT('Ctrl Pts',(-0.249771440080693,1.61522066995007,
12.2998330708668));
#23275=CARTESIAN_POINT('Ctrl Pts',(-0.0832571466935557,-0.552060840994624,
12.2999999999989));
#23276=CARTESIAN_POINT('Ctrl Pts',(-0.0832571466935557,1.61522066995007,
12.2999999999989));
#23277=CARTESIAN_POINT('Ctrl Pts',(0.,-0.552060840994624,12.3));
#23278=CARTESIAN_POINT('Ctrl Pts',(0.,1.61522066995007,12.3));
#23279=CARTESIAN_POINT('Ctrl Pts',(0.0832571466935396,-0.552060840994624,
12.3000000000011));
#23280=CARTESIAN_POINT('Ctrl Pts',(0.0832571466935396,1.61522066995007,
12.3000000000011));
#23281=CARTESIAN_POINT('Ctrl Pts',(0.24977144008061,-0.552060840994624,
12.2998330708736));
#23282=CARTESIAN_POINT('Ctrl Pts',(0.24977144008061,1.61522066995007,12.2998330708736));
#23283=CARTESIAN_POINT('Ctrl Pts',(0.498916532526534,-0.552060840994624,
12.2990818897713));
#23284=CARTESIAN_POINT('Ctrl Pts',(0.498916532526534,1.61522066995007,12.2990818897713));
#23285=CARTESIAN_POINT('Ctrl Pts',(0.827351903312438,-0.552060840994624,
12.2972483292974));
#23286=CARTESIAN_POINT('Ctrl Pts',(0.827351903312438,1.61522066995007,12.2972483292974));
#23287=CARTESIAN_POINT('Ctrl Pts',(1.22558901314046,-0.552060840994624,
12.2945066442369));
#23288=CARTESIAN_POINT('Ctrl Pts',(1.22558901314046,1.61522066995007,12.2945066442369));
#23289=CARTESIAN_POINT('Ctrl Pts',(1.60591558979418,-0.552060840994624,
12.2924280532047));
#23290=CARTESIAN_POINT('Ctrl Pts',(1.60591558979418,1.61522066995007,12.2924280532047));
#23291=CARTESIAN_POINT('Ctrl Pts',(1.96338745719096,-0.552060840994624,
12.291968449812));
#23292=CARTESIAN_POINT('Ctrl Pts',(1.96338745719096,1.61522066995007,12.291968449812));
#23293=CARTESIAN_POINT('Ctrl Pts',(2.29394197380175,-0.552060840994624,
12.2935845551378));
#23294=CARTESIAN_POINT('Ctrl Pts',(2.29394197380175,1.61522066995007,12.2935845551378));
#23295=CARTESIAN_POINT('Ctrl Pts',(2.59461297443069,-0.552060840994624,
12.2969132923658));
#23296=CARTESIAN_POINT('Ctrl Pts',(2.59461297443069,1.61522066995007,12.2969132923658));
#23297=CARTESIAN_POINT('Ctrl Pts',(2.86376302967335,-0.552060840994624,
12.3004008390612));
#23298=CARTESIAN_POINT('Ctrl Pts',(2.86376302967335,1.61522066995007,12.3004008390612));
#23299=CARTESIAN_POINT('Ctrl Pts',(3.10127560868576,-0.552060840994624,
12.3010487961961));
#23300=CARTESIAN_POINT('Ctrl Pts',(3.10127560868576,1.61522066995007,12.3010487961961));
#23301=CARTESIAN_POINT('Ctrl Pts',(3.30884480305537,-0.552060840994624,
12.2938762651102));
#23302=CARTESIAN_POINT('Ctrl Pts',(3.30884480305537,1.61522066995007,12.2938762651102));
#23303=CARTESIAN_POINT('Ctrl Pts',(3.48993681214337,-0.552060840994624,
12.2723364229612));
#23304=CARTESIAN_POINT('Ctrl Pts',(3.48993681214337,1.61522066995007,12.2723364229612));
#23305=CARTESIAN_POINT('Ctrl Pts',(3.64927048315907,-0.552060840994624,
12.2301117722792));
#23306=CARTESIAN_POINT('Ctrl Pts',(3.64927048315907,1.61522066995007,12.2301117722792));
#23307=CARTESIAN_POINT('Ctrl Pts',(3.79241297762162,-0.552060840994624,
12.1626050652587));
#23308=CARTESIAN_POINT('Ctrl Pts',(3.79241297762162,1.61522066995007,12.1626050652587));
#23309=CARTESIAN_POINT('Ctrl Pts',(3.90529123941674,-0.552060840994624,
12.0826827671148));
#23310=CARTESIAN_POINT('Ctrl Pts',(3.90529123941674,1.61522066995007,12.0826827671148));
#23311=CARTESIAN_POINT('Ctrl Pts',(3.98932418204563,-0.552060840994624,
12.0094836266392));
#23312=CARTESIAN_POINT('Ctrl Pts',(3.98932418204563,1.61522066995007,12.0094836266392));
#23313=CARTESIAN_POINT('Ctrl Pts',(4.04740991713241,-0.552060840994624,
11.9543581845679));
#23314=CARTESIAN_POINT('Ctrl Pts',(4.04740991713241,1.61522066995007,11.9543581845679));
#23315=CARTESIAN_POINT('Ctrl Pts',(4.07977092452996,-0.552060840994624,
11.9226494651812));
#23316=CARTESIAN_POINT('Ctrl Pts',(4.07977092452996,1.61522066995007,11.9226494651812));
#23317=CARTESIAN_POINT('Ctrl Pts',(4.08617023400024,-0.552060840994624,
11.9163435012344));
#23318=CARTESIAN_POINT('Ctrl Pts',(4.08617023400024,1.61522066995007,11.9163435012344));
#23319=CARTESIAN_POINT('Origin',(3.,0.,10.7));
#23320=CARTESIAN_POINT('',(2.7,0.,10.7));
#23321=CARTESIAN_POINT('Origin',(-3.,0.,11.7));
#23322=CARTESIAN_POINT('',(-3.36,0.,11.7));
#23323=CARTESIAN_POINT('Origin',(3.,0.,11.7));
#23324=CARTESIAN_POINT('',(2.64,0.,11.7));
#23325=CARTESIAN_POINT('Origin',(-3.,0.,10.7));
#23326=CARTESIAN_POINT('',(-3.3,0.,10.7));
#23327=CARTESIAN_POINT('Origin',(3.43968169690401,0.733833766068903,0.487016215536267));
#23328=CARTESIAN_POINT('Origin',(-4.33293714059227,0.0306667563398384,11.9026515720683));
#23329=CARTESIAN_POINT('Origin',(-3.43968169690379,0.733833766068911,0.487016215536247));
#23330=CARTESIAN_POINT('',(0.,0.,0.));
#23331=CARTESIAN_POINT('Origin',(4.14610847673285,3.66,10.5297906787748));
#23332=CARTESIAN_POINT('',(3.82,3.7,11.2854932334582));
#23333=CARTESIAN_POINT('',(3.53330081745645,3.7,12.0500243869077));
#23334=CARTESIAN_POINT('',(4.10865530963009,3.7,10.5157457411113));
#23335=CARTESIAN_POINT('',(3.6,3.62,12.1));
#23336=CARTESIAN_POINT('',(3.53330081745645,3.7,12.0500243869077));
#23337=CARTESIAN_POINT('',(3.9,3.62,11.3));
#23338=CARTESIAN_POINT('',(4.18356164383562,3.62,10.5438356164384));
#23339=CARTESIAN_POINT('',(3.82,3.7,11.2854932334582));
#23340=CARTESIAN_POINT('Origin',(3.2,3.66,12.35));
#23341=CARTESIAN_POINT('',(2.77333333333333,3.7,12.62));
#23342=CARTESIAN_POINT('',(3.176,3.7,12.318));
#23343=CARTESIAN_POINT('',(2.8,3.62,12.7));
#23344=CARTESIAN_POINT('',(2.77333333333333,3.7,12.62));
#23345=CARTESIAN_POINT('',(3.224,3.62,12.382));
#23346=CARTESIAN_POINT('Origin',(-1.4,3.66,12.66));
#23347=CARTESIAN_POINT('',(-2.77333333333333,3.7,12.62));
#23348=CARTESIAN_POINT('',(-1.4,3.7,12.62));
#23349=CARTESIAN_POINT('',(-2.8,3.62,12.7));
#23350=CARTESIAN_POINT('',(-2.77333333333333,3.7,12.62));
#23351=CARTESIAN_POINT('',(-1.4,3.62,12.7));
#23352=CARTESIAN_POINT('Origin',(-3.6,3.66,12.05));
#23353=CARTESIAN_POINT('',(-3.53330081745645,3.7,12.0500243869077));
#23354=CARTESIAN_POINT('',(-3.576,3.7,12.018));
#23355=CARTESIAN_POINT('',(-3.6,3.62,12.1));
#23356=CARTESIAN_POINT('',(-3.53330081745645,3.7,12.0500243869077));
#23357=CARTESIAN_POINT('',(-3.624,3.62,12.082));
#23358=CARTESIAN_POINT('Origin',(-4.29610847673285,3.66,10.1297906787748));
#23359=CARTESIAN_POINT('',(-3.82,3.7,11.2854932334582));
#23360=CARTESIAN_POINT('',(-4.25865530963009,3.7,10.1157457411113));
#23361=CARTESIAN_POINT('',(-3.9,3.62,11.3));
#23362=CARTESIAN_POINT('',(-3.82,3.7,11.2854932334582));
#23363=CARTESIAN_POINT('',(-4.33356164383562,3.62,10.1438356164384));
#23364=CARTESIAN_POINT('Origin',(-3.86,3.66,4.45));
#23365=CARTESIAN_POINT('',(-3.9,3.62,1.7));
#23366=CARTESIAN_POINT('',(-3.9,3.62,4.45));
#23367=CARTESIAN_POINT('',(-3.82,3.7,1.78));
#23368=CARTESIAN_POINT('',(-3.82,3.7,4.45));
#23369=CARTESIAN_POINT('',(-3.82,3.7,1.78));
#23370=CARTESIAN_POINT('Origin',(1.95,3.66,1.74));
#23371=CARTESIAN_POINT('',(3.9,3.62,1.7));
#23372=CARTESIAN_POINT('',(1.95,3.62,1.7));
#23373=CARTESIAN_POINT('',(3.82,3.7,1.78));
#23374=CARTESIAN_POINT('',(1.95,3.7,1.78));
#23375=CARTESIAN_POINT('',(3.82,3.7,1.78));
#23376=CARTESIAN_POINT('Origin',(3.86,3.66,9.25));
#23377=CARTESIAN_POINT('',(3.9,3.62,9.25));
#23378=CARTESIAN_POINT('',(3.82,3.7,9.25));
#23379=CARTESIAN_POINT('Origin',(-3.9,0.5,1.7));
#23380=CARTESIAN_POINT('',(-3.9,0.5,1.7));
#23381=CARTESIAN_POINT('',(-3.9,0.5,1.7));
#23382=CARTESIAN_POINT('',(-3.9,0.5,11.3));
#23383=CARTESIAN_POINT('',(-3.9,0.5,11.3));
#23384=CARTESIAN_POINT('',(-3.9,0.5,11.3));
#23385=CARTESIAN_POINT('Origin',(3.9,0.5,1.7));
#23386=CARTESIAN_POINT('',(3.9,0.5,1.7));
#23387=CARTESIAN_POINT('',(3.9,0.5,1.7));
#23388=CARTESIAN_POINT('',(-3.9,0.5,1.7));
#23389=CARTESIAN_POINT('Origin',(3.9,0.5,11.3));
#23390=CARTESIAN_POINT('',(3.9,0.5,11.3));
#23391=CARTESIAN_POINT('',(3.9,0.5,11.3));
#23392=CARTESIAN_POINT('',(3.9,0.5,1.7));
#23393=CARTESIAN_POINT('Origin',(3.6,0.5,12.1));
#23394=CARTESIAN_POINT('',(3.6,0.5,12.1));
#23395=CARTESIAN_POINT('',(3.6,0.5,12.1));
#23396=CARTESIAN_POINT('',(3.9,0.5,11.3));
#23397=CARTESIAN_POINT('Origin',(0.,3.7,7.2));
#23398=CARTESIAN_POINT('',(-3.2,3.7,9.5));
#23399=CARTESIAN_POINT('',(-3.2,3.7,3.7));
#23400=CARTESIAN_POINT('',(-3.2,3.7,8.35));
#23401=CARTESIAN_POINT('',(-1.2,3.7,3.7));
#23402=CARTESIAN_POINT('',(-1.6,3.7,3.7));
#23403=CARTESIAN_POINT('',(-1.2,3.7,3.));
#23404=CARTESIAN_POINT('',(-1.2,3.7,5.45));
#23405=CARTESIAN_POINT('',(1.2,3.7,3.));
#23406=CARTESIAN_POINT('',(-0.6,3.7,3.));
#23407=CARTESIAN_POINT('',(1.2,3.7,3.7));
#23408=CARTESIAN_POINT('',(1.2,3.7,5.1));
#23409=CARTESIAN_POINT('',(3.2,3.7,3.7));
#23410=CARTESIAN_POINT('',(0.6,3.7,3.7));
#23411=CARTESIAN_POINT('',(3.2,3.7,9.5));
#23412=CARTESIAN_POINT('',(3.2,3.7,5.45));
#23413=CARTESIAN_POINT('',(1.2,3.7,9.5));
#23414=CARTESIAN_POINT('',(1.6,3.7,9.5));
#23415=CARTESIAN_POINT('',(1.2,3.7,12.4));
#23416=CARTESIAN_POINT('',(1.2,3.7,8.35));
#23417=CARTESIAN_POINT('',(-1.2,3.7,12.4));
#23418=CARTESIAN_POINT('',(0.6,3.7,12.4));
#23419=CARTESIAN_POINT('',(-1.2,3.7,9.5));
#23420=CARTESIAN_POINT('',(-1.2,3.7,9.8));
#23421=CARTESIAN_POINT('',(-0.6,3.7,9.5));
#23422=CARTESIAN_POINT('',(-3.36,3.7,11.7));
#23423=CARTESIAN_POINT('Origin',(-3.,3.7,11.7));
#23424=CARTESIAN_POINT('',(2.64,3.7,11.7));
#23425=CARTESIAN_POINT('Origin',(3.,3.7,11.7));
#23426=CARTESIAN_POINT('',(3.805,3.7,2.5));
#23427=CARTESIAN_POINT('Origin',(3.55,3.7,2.5));
#23428=CARTESIAN_POINT('',(-3.295,3.7,2.5));
#23429=CARTESIAN_POINT('Origin',(-3.55,3.7,2.5));
#23430=CARTESIAN_POINT('',(3.805,3.7,10.));
#23431=CARTESIAN_POINT('Origin',(3.55,3.7,10.));
#23432=CARTESIAN_POINT('',(-3.295,3.7,10.));
#23433=CARTESIAN_POINT('Origin',(-3.55,3.7,10.));
#23434=CARTESIAN_POINT('Origin',(-3.55,2.63841178654968,10.));
#23435=CARTESIAN_POINT('',(-3.55,2.57682357309935,10.));
#23436=CARTESIAN_POINT('',(-3.345,2.7,10.));
#23437=CARTESIAN_POINT('',(-3.4475,2.63841178654968,10.));
#23438=CARTESIAN_POINT('Origin',(-3.55,2.7,10.));
#23439=CARTESIAN_POINT('Origin',(-3.55,3.175,10.));
#23440=CARTESIAN_POINT('',(-3.345,3.65,10.));
#23441=CARTESIAN_POINT('',(-3.345,3.175,10.));
#23442=CARTESIAN_POINT('Origin',(-3.55,3.65,10.));
#23443=CARTESIAN_POINT('Origin',(-3.55,3.7,10.));
#23444=CARTESIAN_POINT('',(-3.295,3.7,10.));
#23445=CARTESIAN_POINT('Origin',(3.55,2.63841178654968,10.));
#23446=CARTESIAN_POINT('',(3.55,2.57682357309935,10.));
#23447=CARTESIAN_POINT('',(3.755,2.7,10.));
#23448=CARTESIAN_POINT('',(3.6525,2.63841178654968,10.));
#23449=CARTESIAN_POINT('Origin',(3.55,2.7,10.));
#23450=CARTESIAN_POINT('Origin',(3.55,3.175,10.));
#23451=CARTESIAN_POINT('',(3.755,3.65,10.));
#23452=CARTESIAN_POINT('',(3.755,3.175,10.));
#23453=CARTESIAN_POINT('Origin',(3.55,3.65,10.));
#23454=CARTESIAN_POINT('Origin',(3.55,3.7,10.));
#23455=CARTESIAN_POINT('',(3.805,3.7,10.));
#23456=CARTESIAN_POINT('Origin',(-3.55,2.63841178654968,2.5));
#23457=CARTESIAN_POINT('',(-3.55,2.57682357309935,2.5));
#23458=CARTESIAN_POINT('',(-3.345,2.7,2.5));
#23459=CARTESIAN_POINT('',(-3.4475,2.63841178654968,2.5));
#23460=CARTESIAN_POINT('Origin',(-3.55,2.7,2.5));
#23461=CARTESIAN_POINT('Origin',(-3.55,3.175,2.5));
#23462=CARTESIAN_POINT('',(-3.345,3.65,2.5));
#23463=CARTESIAN_POINT('',(-3.345,3.175,2.5));
#23464=CARTESIAN_POINT('Origin',(-3.55,3.65,2.5));
#23465=CARTESIAN_POINT('Origin',(-3.55,3.7,2.5));
#23466=CARTESIAN_POINT('',(-3.295,3.7,2.5));
#23467=CARTESIAN_POINT('Origin',(3.55,2.63841178654968,2.5));
#23468=CARTESIAN_POINT('',(3.55,2.57682357309935,2.5));
#23469=CARTESIAN_POINT('',(3.755,2.7,2.5));
#23470=CARTESIAN_POINT('',(3.6525,2.63841178654968,2.5));
#23471=CARTESIAN_POINT('Origin',(3.55,2.7,2.5));
#23472=CARTESIAN_POINT('Origin',(3.55,3.175,2.5));
#23473=CARTESIAN_POINT('',(3.755,3.65,2.5));
#23474=CARTESIAN_POINT('',(3.755,3.175,2.5));
#23475=CARTESIAN_POINT('Origin',(3.55,3.65,2.5));
#23476=CARTESIAN_POINT('Origin',(3.55,3.7,2.5));
#23477=CARTESIAN_POINT('',(3.805,3.7,2.5));
#23478=CARTESIAN_POINT('Origin',(-3.,1.74012909285413,10.7));
#23479=CARTESIAN_POINT('',(-3.,1.83025818570827,10.7));
#23480=CARTESIAN_POINT('',(-3.3,1.65,10.7));
#23481=CARTESIAN_POINT('',(-3.15,1.74012909285413,10.7));
#23482=CARTESIAN_POINT('Origin',(-3.,1.65,10.7));
#23483=CARTESIAN_POINT('Origin',(-3.,1.05,10.7));
#23484=CARTESIAN_POINT('',(-3.3,0.5,10.7));
#23485=CARTESIAN_POINT('',(-3.3,1.05,10.7));
#23486=CARTESIAN_POINT('Origin',(-3.,0.5,10.7));
#23487=CARTESIAN_POINT('Origin',(3.,1.74012909285413,10.7));
#23488=CARTESIAN_POINT('',(3.,1.83025818570827,10.7));
#23489=CARTESIAN_POINT('',(2.7,1.65,10.7));
#23490=CARTESIAN_POINT('',(2.85,1.74012909285413,10.7));
#23491=CARTESIAN_POINT('Origin',(3.,1.65,10.7));
#23492=CARTESIAN_POINT('Origin',(3.,1.05,10.7));
#23493=CARTESIAN_POINT('',(2.7,0.5,10.7));
#23494=CARTESIAN_POINT('',(2.7,1.05,10.7));
#23495=CARTESIAN_POINT('Origin',(3.,0.5,10.7));
#23496=CARTESIAN_POINT('Origin',(3.,0.5,11.7));
#23497=CARTESIAN_POINT('',(2.64,0.5,11.7));
#23498=CARTESIAN_POINT('Origin',(3.,0.5,11.7));
#23499=CARTESIAN_POINT('',(2.64,0.5,11.7));
#23500=CARTESIAN_POINT('Origin',(-3.,0.5,11.7));
#23501=CARTESIAN_POINT('',(-3.36,0.5,11.7));
#23502=CARTESIAN_POINT('Origin',(-3.,0.5,11.7));
#23503=CARTESIAN_POINT('',(-3.36,0.5,11.7));
#23504=CARTESIAN_POINT('Origin',(0.,2.1,12.7));
#23505=CARTESIAN_POINT('',(-0.5,2.1,12.7));
#23506=CARTESIAN_POINT('Origin',(0.,2.1,12.7));
#23507=CARTESIAN_POINT('',(-0.5,2.1,12.4));
#23508=CARTESIAN_POINT('',(-0.5,2.1,12.7));
#23509=CARTESIAN_POINT('Origin',(0.,2.1,12.4));
#23510=CARTESIAN_POINT('Origin',(-3.2,3.7,9.5));
#23511=CARTESIAN_POINT('',(-3.2,0.7,9.5));
#23512=CARTESIAN_POINT('',(-3.2,3.7,9.5));
#23513=CARTESIAN_POINT('',(-3.2,0.7,3.7));
#23514=CARTESIAN_POINT('',(-3.2,0.7,9.5));
#23515=CARTESIAN_POINT('',(-3.2,3.7,3.7));
#23516=CARTESIAN_POINT('Origin',(-1.2,3.7,9.5));
#23517=CARTESIAN_POINT('',(-1.2,0.7,9.5));
#23518=CARTESIAN_POINT('',(-1.2,3.7,9.5));
#23519=CARTESIAN_POINT('',(-1.2,0.7,9.5));
#23520=CARTESIAN_POINT('Origin',(-1.2,3.7,12.4));
#23521=CARTESIAN_POINT('',(-1.2,0.7,12.4));
#23522=CARTESIAN_POINT('',(-1.2,3.7,12.4));
#23523=CARTESIAN_POINT('',(-1.2,0.7,12.4));
#23524=CARTESIAN_POINT('Origin',(1.2,3.7,12.4));
#23525=CARTESIAN_POINT('',(1.2,0.7,12.4));
#23526=CARTESIAN_POINT('',(1.2,3.7,12.4));
#23527=CARTESIAN_POINT('',(1.2,0.7,12.4));
#23528=CARTESIAN_POINT('Origin',(1.2,3.7,9.5));
#23529=CARTESIAN_POINT('',(1.2,0.7,9.5));
#23530=CARTESIAN_POINT('',(1.2,3.7,9.5));
#23531=CARTESIAN_POINT('',(1.2,0.7,9.5));
#23532=CARTESIAN_POINT('Origin',(3.2,3.7,9.5));
#23533=CARTESIAN_POINT('',(3.2,0.7,9.5));
#23534=CARTESIAN_POINT('',(3.2,3.7,9.5));
#23535=CARTESIAN_POINT('',(3.2,0.7,9.5));
#23536=CARTESIAN_POINT('Origin',(3.2,3.7,3.7));
#23537=CARTESIAN_POINT('',(3.2,0.7,3.7));
#23538=CARTESIAN_POINT('',(3.2,3.7,3.7));
#23539=CARTESIAN_POINT('',(3.2,0.7,3.7));
#23540=CARTESIAN_POINT('Origin',(1.2,3.7,3.7));
#23541=CARTESIAN_POINT('',(1.2,0.7,3.7));
#23542=CARTESIAN_POINT('',(1.2,3.7,3.7));
#23543=CARTESIAN_POINT('',(1.2,0.7,3.7));
#23544=CARTESIAN_POINT('Origin',(1.2,3.7,3.));
#23545=CARTESIAN_POINT('',(1.2,0.7,3.));
#23546=CARTESIAN_POINT('',(1.2,3.7,3.));
#23547=CARTESIAN_POINT('',(1.2,0.7,3.));
#23548=CARTESIAN_POINT('Origin',(-1.2,3.7,3.));
#23549=CARTESIAN_POINT('',(-1.2,0.7,3.));
#23550=CARTESIAN_POINT('',(-1.2,3.7,3.));
#23551=CARTESIAN_POINT('',(-1.2,0.7,3.));
#23552=CARTESIAN_POINT('Origin',(-1.2,3.7,3.7));
#23553=CARTESIAN_POINT('',(-1.2,0.7,3.7));
#23554=CARTESIAN_POINT('',(-1.2,3.7,3.7));
#23555=CARTESIAN_POINT('',(-1.2,0.7,3.7));
#23556=CARTESIAN_POINT('Origin',(-3.2,3.7,3.7));
#23557=CARTESIAN_POINT('',(-3.2,0.7,3.7));
#23558=CARTESIAN_POINT('Origin',(0.,0.7,7.7));
#23559=CARTESIAN_POINT('Origin',(2.8,0.5,12.7));
#23560=CARTESIAN_POINT('',(2.8,0.5,12.7));
#23561=CARTESIAN_POINT('',(2.8,0.5,12.7));
#23562=CARTESIAN_POINT('',(3.6,0.5,12.1));
#23563=CARTESIAN_POINT('Origin',(-2.8,0.5,12.7));
#23564=CARTESIAN_POINT('',(-2.8,0.5,12.7));
#23565=CARTESIAN_POINT('',(-2.8,0.5,12.7));
#23566=CARTESIAN_POINT('',(2.8,0.5,12.7));
#23567=CARTESIAN_POINT('Origin',(-3.6,0.5,12.1));
#23568=CARTESIAN_POINT('',(-3.6,0.5,12.1));
#23569=CARTESIAN_POINT('',(-3.6,0.5,12.1));
#23570=CARTESIAN_POINT('',(-2.8,0.5,12.7));
#23571=CARTESIAN_POINT('Origin',(-3.9,0.5,11.3));
#23572=CARTESIAN_POINT('',(-3.6,0.5,12.1));
#23573=CARTESIAN_POINT('Origin',(0.,0.5,7.2));
#23574=CARTESIAN_POINT('',(0.,0.,0.));
#23575=CARTESIAN_POINT('Origin',(2.9,3.7,9.1));
#23576=CARTESIAN_POINT('',(3.1,3.7,9.1));
#23577=CARTESIAN_POINT('',(2.9,3.7,9.3));
#23578=CARTESIAN_POINT('Origin',(2.9,3.7,9.1));
#23579=CARTESIAN_POINT('',(2.9,3.85,9.3));
#23580=CARTESIAN_POINT('',(2.9,3.7,9.3));
#23581=CARTESIAN_POINT('',(3.1,3.85,9.1));
#23582=CARTESIAN_POINT('Origin',(2.9,3.85,9.1));
#23583=CARTESIAN_POINT('',(3.1,3.7,9.1));
#23584=CARTESIAN_POINT('Origin',(1.5,3.7,9.3));
#23585=CARTESIAN_POINT('',(1.7,3.7,9.3));
#23586=CARTESIAN_POINT('',(0.75,3.7,9.3));
#23587=CARTESIAN_POINT('',(1.7,3.85,9.3));
#23588=CARTESIAN_POINT('',(1.7,3.7,9.3));
#23589=CARTESIAN_POINT('',(0.75,3.85,9.3));
#23590=CARTESIAN_POINT('Origin',(2.9,3.7,4.2));
#23591=CARTESIAN_POINT('',(2.9,3.7,4.));
#23592=CARTESIAN_POINT('',(3.1,3.7,4.2));
#23593=CARTESIAN_POINT('Origin',(2.9,3.7,4.2));
#23594=CARTESIAN_POINT('',(3.1,3.85,4.2));
#23595=CARTESIAN_POINT('',(3.1,3.7,4.2));
#23596=CARTESIAN_POINT('',(2.9,3.85,4.));
#23597=CARTESIAN_POINT('Origin',(2.9,3.85,4.2));
#23598=CARTESIAN_POINT('',(2.9,3.7,4.));
#23599=CARTESIAN_POINT('Origin',(3.1,3.7,9.3));
#23600=CARTESIAN_POINT('',(3.1,3.85,8.25));
#23601=CARTESIAN_POINT('',(3.1,3.7,8.25));
#23602=CARTESIAN_POINT('Origin',(1.7,3.7,9.1));
#23603=CARTESIAN_POINT('',(1.5,3.7,9.1));
#23604=CARTESIAN_POINT('Origin',(1.7,3.7,9.1));
#23605=CARTESIAN_POINT('',(1.5,3.85,9.1));
#23606=CARTESIAN_POINT('',(1.5,3.7,9.1));
#23607=CARTESIAN_POINT('Origin',(1.7,3.85,9.1));
#23608=CARTESIAN_POINT('Origin',(1.5,3.7,4.));
#23609=CARTESIAN_POINT('',(1.5,3.7,4.2));
#23610=CARTESIAN_POINT('',(1.5,3.7,5.6));
#23611=CARTESIAN_POINT('',(1.5,3.85,4.2));
#23612=CARTESIAN_POINT('',(1.5,3.7,4.2));
#23613=CARTESIAN_POINT('',(1.5,3.85,5.6));
#23614=CARTESIAN_POINT('Origin',(1.7,3.7,4.2));
#23615=CARTESIAN_POINT('',(1.7,3.7,4.));
#23616=CARTESIAN_POINT('Origin',(1.7,3.7,4.2));
#23617=CARTESIAN_POINT('',(1.7,3.85,4.));
#23618=CARTESIAN_POINT('',(1.7,3.7,4.));
#23619=CARTESIAN_POINT('Origin',(1.7,3.85,4.2));
#23620=CARTESIAN_POINT('Origin',(3.1,3.7,4.));
#23621=CARTESIAN_POINT('',(1.55,3.85,4.));
#23622=CARTESIAN_POINT('',(1.55,3.7,4.));
#23623=CARTESIAN_POINT('Origin',(-1.7,3.7,4.2));
#23624=CARTESIAN_POINT('',(-1.7,3.7,4.));
#23625=CARTESIAN_POINT('',(-1.5,3.7,4.2));
#23626=CARTESIAN_POINT('Origin',(-1.7,3.7,4.2));
#23627=CARTESIAN_POINT('',(-1.5,3.85,4.2));
#23628=CARTESIAN_POINT('',(-1.5,3.7,4.2));
#23629=CARTESIAN_POINT('',(-1.7,3.85,4.));
#23630=CARTESIAN_POINT('Origin',(-1.7,3.85,4.2));
#23631=CARTESIAN_POINT('',(-1.7,3.7,4.));
#23632=CARTESIAN_POINT('Origin',(-1.5,3.7,9.3));
#23633=CARTESIAN_POINT('',(-1.5,3.7,9.1));
#23634=CARTESIAN_POINT('',(-1.5,3.7,8.25));
#23635=CARTESIAN_POINT('',(-1.5,3.85,9.1));
#23636=CARTESIAN_POINT('',(-1.5,3.7,9.1));
#23637=CARTESIAN_POINT('',(-1.5,3.85,8.25));
#23638=CARTESIAN_POINT('Origin',(-2.9,3.7,4.2));
#23639=CARTESIAN_POINT('',(-3.1,3.7,4.2));
#23640=CARTESIAN_POINT('',(-2.9,3.7,4.));
#23641=CARTESIAN_POINT('Origin',(-2.9,3.7,4.2));
#23642=CARTESIAN_POINT('',(-2.9,3.85,4.));
#23643=CARTESIAN_POINT('',(-2.9,3.7,4.));
#23644=CARTESIAN_POINT('',(-3.1,3.85,4.2));
#23645=CARTESIAN_POINT('Origin',(-2.9,3.85,4.2));
#23646=CARTESIAN_POINT('',(-3.1,3.7,4.2));
#23647=CARTESIAN_POINT('Origin',(-1.5,3.7,4.));
#23648=CARTESIAN_POINT('',(-0.75,3.85,4.));
#23649=CARTESIAN_POINT('',(-0.75,3.7,4.));
#23650=CARTESIAN_POINT('Origin',(-1.7,3.7,9.1));
#23651=CARTESIAN_POINT('',(-1.7,3.7,9.3));
#23652=CARTESIAN_POINT('Origin',(-1.7,3.7,9.1));
#23653=CARTESIAN_POINT('',(-1.7,3.85,9.3));
#23654=CARTESIAN_POINT('',(-1.7,3.7,9.3));
#23655=CARTESIAN_POINT('Origin',(-1.7,3.85,9.1));
#23656=CARTESIAN_POINT('Origin',(-3.1,3.7,9.3));
#23657=CARTESIAN_POINT('',(-2.9,3.7,9.3));
#23658=CARTESIAN_POINT('',(-1.55,3.7,9.3));
#23659=CARTESIAN_POINT('',(-2.9,3.85,9.3));
#23660=CARTESIAN_POINT('',(-2.9,3.7,9.3));
#23661=CARTESIAN_POINT('',(-1.55,3.85,9.3));
#23662=CARTESIAN_POINT('Origin',(-2.9,3.7,9.1));
#23663=CARTESIAN_POINT('',(-3.1,3.7,9.1));
#23664=CARTESIAN_POINT('Origin',(-2.9,3.7,9.1));
#23665=CARTESIAN_POINT('',(-3.1,3.85,9.1));
#23666=CARTESIAN_POINT('',(-3.1,3.7,9.1));
#23667=CARTESIAN_POINT('Origin',(-2.9,3.85,9.1));
#23668=CARTESIAN_POINT('Origin',(-3.1,3.7,4.));
#23669=CARTESIAN_POINT('',(-3.1,3.85,5.6));
#23670=CARTESIAN_POINT('',(-3.1,3.7,5.6));
#23671=CARTESIAN_POINT('Origin',(1.1,3.7,12.));
#23672=CARTESIAN_POINT('',(1.3,3.7,12.));
#23673=CARTESIAN_POINT('',(1.1,3.7,12.2));
#23674=CARTESIAN_POINT('Origin',(1.1,3.7,12.));
#23675=CARTESIAN_POINT('',(1.1,3.85,12.2));
#23676=CARTESIAN_POINT('',(1.1,3.7,12.2));
#23677=CARTESIAN_POINT('',(1.3,3.85,12.));
#23678=CARTESIAN_POINT('Origin',(1.1,3.85,12.));
#23679=CARTESIAN_POINT('',(1.3,3.7,12.));
#23680=CARTESIAN_POINT('Origin',(-1.3,3.7,12.2));
#23681=CARTESIAN_POINT('',(-1.1,3.7,12.2));
#23682=CARTESIAN_POINT('',(-0.65,3.7,12.2));
#23683=CARTESIAN_POINT('',(-1.1,3.85,12.2));
#23684=CARTESIAN_POINT('',(-1.1,3.7,12.2));
#23685=CARTESIAN_POINT('',(-0.65,3.85,12.2));
#23686=CARTESIAN_POINT('Origin',(1.1,3.7,4.2));
#23687=CARTESIAN_POINT('',(1.1,3.7,4.));
#23688=CARTESIAN_POINT('',(1.3,3.7,4.2));
#23689=CARTESIAN_POINT('Origin',(1.1,3.7,4.2));
#23690=CARTESIAN_POINT('',(1.3,3.85,4.2));
#23691=CARTESIAN_POINT('',(1.3,3.7,4.2));
#23692=CARTESIAN_POINT('',(1.1,3.85,4.));
#23693=CARTESIAN_POINT('Origin',(1.1,3.85,4.2));
#23694=CARTESIAN_POINT('',(1.1,3.7,4.));
#23695=CARTESIAN_POINT('Origin',(1.3,3.7,12.2));
#23696=CARTESIAN_POINT('',(1.3,3.85,9.7));
#23697=CARTESIAN_POINT('',(1.3,3.7,9.7));
#23698=CARTESIAN_POINT('Origin',(-1.1,3.7,12.));
#23699=CARTESIAN_POINT('',(-1.3,3.7,12.));
#23700=CARTESIAN_POINT('Origin',(-1.1,3.7,12.));
#23701=CARTESIAN_POINT('',(-1.3,3.85,12.));
#23702=CARTESIAN_POINT('',(-1.3,3.7,12.));
#23703=CARTESIAN_POINT('Origin',(-1.1,3.85,12.));
#23704=CARTESIAN_POINT('Origin',(-1.3,3.7,4.));
#23705=CARTESIAN_POINT('',(-1.3,3.7,4.2));
#23706=CARTESIAN_POINT('',(-1.3,3.7,5.6));
#23707=CARTESIAN_POINT('',(-1.3,3.85,4.2));
#23708=CARTESIAN_POINT('',(-1.3,3.7,4.2));
#23709=CARTESIAN_POINT('',(-1.3,3.85,5.6));
#23710=CARTESIAN_POINT('Origin',(-1.1,3.7,4.2));
#23711=CARTESIAN_POINT('',(-1.1,3.7,4.));
#23712=CARTESIAN_POINT('Origin',(-1.1,3.7,4.2));
#23713=CARTESIAN_POINT('',(-1.1,3.85,4.));
#23714=CARTESIAN_POINT('',(-1.1,3.7,4.));
#23715=CARTESIAN_POINT('Origin',(-1.1,3.85,4.2));
#23716=CARTESIAN_POINT('Origin',(1.3,3.7,4.));
#23717=CARTESIAN_POINT('',(0.65,3.85,4.));
#23718=CARTESIAN_POINT('',(0.65,3.7,4.));
#23719=CARTESIAN_POINT('Origin',(3.55,3.7,10.));
#23720=CARTESIAN_POINT('',(3.325,3.7,10.));
#23721=CARTESIAN_POINT('Origin',(3.55,3.7,10.));
#23722=CARTESIAN_POINT('',(3.325,3.85,10.));
#23723=CARTESIAN_POINT('',(3.325,3.7,10.));
#23724=CARTESIAN_POINT('Origin',(3.55,3.85,10.));
#23725=CARTESIAN_POINT('Origin',(3.,3.7,11.7));
#23726=CARTESIAN_POINT('',(2.64,3.7,11.7));
#23727=CARTESIAN_POINT('Origin',(3.,3.7,11.7));
#23728=CARTESIAN_POINT('',(2.64,3.85,11.7));
#23729=CARTESIAN_POINT('',(2.64,3.7,11.7));
#23730=CARTESIAN_POINT('Origin',(3.,3.85,11.7));
#23731=CARTESIAN_POINT('Origin',(-3.,3.7,11.7));
#23732=CARTESIAN_POINT('',(-3.36,3.7,11.7));
#23733=CARTESIAN_POINT('Origin',(-3.,3.7,11.7));
#23734=CARTESIAN_POINT('',(-3.36,3.85,11.7));
#23735=CARTESIAN_POINT('',(-3.36,3.7,11.7));
#23736=CARTESIAN_POINT('Origin',(-3.,3.85,11.7));
#23737=CARTESIAN_POINT('Origin',(3.55,3.7,2.5));
#23738=CARTESIAN_POINT('',(3.325,3.7,2.5));
#23739=CARTESIAN_POINT('Origin',(3.55,3.7,2.5));
#23740=CARTESIAN_POINT('',(3.325,3.85,2.5));
#23741=CARTESIAN_POINT('',(3.325,3.7,2.5));
#23742=CARTESIAN_POINT('Origin',(3.55,3.85,2.5));
#23743=CARTESIAN_POINT('Origin',(-3.55,3.7,2.5));
#23744=CARTESIAN_POINT('',(-3.775,3.7,2.5));
#23745=CARTESIAN_POINT('Origin',(-3.55,3.7,2.5));
#23746=CARTESIAN_POINT('',(-3.775,3.85,2.5));
#23747=CARTESIAN_POINT('',(-3.775,3.7,2.5));
#23748=CARTESIAN_POINT('Origin',(-3.55,3.85,2.5));
#23749=CARTESIAN_POINT('Origin',(-3.55,3.7,10.));
#23750=CARTESIAN_POINT('',(-3.775,3.7,10.));
#23751=CARTESIAN_POINT('Origin',(-3.55,3.7,10.));
#23752=CARTESIAN_POINT('',(-3.775,3.85,10.));
#23753=CARTESIAN_POINT('',(-3.775,3.7,10.));
#23754=CARTESIAN_POINT('Origin',(-3.55,3.85,10.));
#23755=CARTESIAN_POINT('Origin',(-3.9,3.7,1.7));
#23756=CARTESIAN_POINT('',(-3.9,3.7,11.3));
#23757=CARTESIAN_POINT('',(-3.9,3.7,1.7));
#23758=CARTESIAN_POINT('',(-3.9,3.7,11.3));
#23759=CARTESIAN_POINT('',(-3.9,3.85,11.3));
#23760=CARTESIAN_POINT('',(-3.9,3.7,11.3));
#23761=CARTESIAN_POINT('',(-3.9,3.85,1.7));
#23762=CARTESIAN_POINT('',(-3.9,3.85,11.3));
#23763=CARTESIAN_POINT('',(-3.9,3.7,1.7));
#23764=CARTESIAN_POINT('Origin',(3.9,3.7,1.7));
#23765=CARTESIAN_POINT('',(3.9,3.7,1.7));
#23766=CARTESIAN_POINT('',(-3.9,3.7,1.7));
#23767=CARTESIAN_POINT('',(3.9,3.85,1.7));
#23768=CARTESIAN_POINT('',(-3.9,3.85,1.7));
#23769=CARTESIAN_POINT('',(3.9,3.7,1.7));
#23770=CARTESIAN_POINT('Origin',(3.9,3.7,11.3));
#23771=CARTESIAN_POINT('',(3.9,3.7,11.3));
#23772=CARTESIAN_POINT('',(3.9,3.7,1.7));
#23773=CARTESIAN_POINT('',(3.9,3.85,11.3));
#23774=CARTESIAN_POINT('',(3.9,3.85,1.7));
#23775=CARTESIAN_POINT('',(3.9,3.7,11.3));
#23776=CARTESIAN_POINT('Origin',(3.6,3.7,12.1));
#23777=CARTESIAN_POINT('',(3.6,3.7,12.1));
#23778=CARTESIAN_POINT('',(3.9,3.7,11.3));
#23779=CARTESIAN_POINT('',(3.6,3.85,12.1));
#23780=CARTESIAN_POINT('',(3.9,3.85,11.3));
#23781=CARTESIAN_POINT('',(3.6,3.7,12.1));
#23782=CARTESIAN_POINT('Origin',(2.8,3.7,12.7));
#23783=CARTESIAN_POINT('',(2.8,3.7,12.7));
#23784=CARTESIAN_POINT('',(3.6,3.7,12.1));
#23785=CARTESIAN_POINT('',(2.8,3.85,12.7));
#23786=CARTESIAN_POINT('',(3.6,3.85,12.1));
#23787=CARTESIAN_POINT('',(2.8,3.7,12.7));
#23788=CARTESIAN_POINT('Origin',(-2.8,3.7,12.7));
#23789=CARTESIAN_POINT('',(-2.8,3.7,12.7));
#23790=CARTESIAN_POINT('',(2.8,3.7,12.7));
#23791=CARTESIAN_POINT('',(-2.8,3.85,12.7));
#23792=CARTESIAN_POINT('',(2.8,3.85,12.7));
#23793=CARTESIAN_POINT('',(-2.8,3.7,12.7));
#23794=CARTESIAN_POINT('Origin',(-3.6,3.7,12.1));
#23795=CARTESIAN_POINT('',(-3.6,3.7,12.1));
#23796=CARTESIAN_POINT('',(-2.8,3.7,12.7));
#23797=CARTESIAN_POINT('',(-3.6,3.85,12.1));
#23798=CARTESIAN_POINT('',(-2.8,3.85,12.7));
#23799=CARTESIAN_POINT('',(-3.6,3.7,12.1));
#23800=CARTESIAN_POINT('Origin',(-3.9,3.7,11.3));
#23801=CARTESIAN_POINT('',(-3.6,3.7,12.1));
#23802=CARTESIAN_POINT('',(-3.6,3.85,12.1));
#23803=CARTESIAN_POINT('Origin',(0.,3.85,7.2));
#23804=CARTESIAN_POINT('Origin',(0.,3.7,7.2));
#23805=CARTESIAN_POINT('',(0.,0.,0.));
#23806=CARTESIAN_POINT('Origin',(5.77,-0.37,11.));
#23807=CARTESIAN_POINT('',(5.74,-0.4,12.3751471862576));
#23808=CARTESIAN_POINT('',(5.74,-0.4,10.46));
#23809=CARTESIAN_POINT('',(5.74,-0.4,11.));
#23810=CARTESIAN_POINT('',(5.8,-0.34,10.4));
#23811=CARTESIAN_POINT('',(5.74,-0.4,10.46));
#23812=CARTESIAN_POINT('',(5.8,-0.34,12.4));
#23813=CARTESIAN_POINT('',(5.8,-0.34,11.));
#23814=CARTESIAN_POINT('',(5.74,-0.4,12.3751471862576));
#23815=CARTESIAN_POINT('Origin',(-2.9,-0.37,10.43));
#23816=CARTESIAN_POINT('',(-5.74,-0.4,10.46));
#23817=CARTESIAN_POINT('',(-2.9,-0.4,10.46));
#23818=CARTESIAN_POINT('',(-5.8,-0.34,10.4));
#23819=CARTESIAN_POINT('',(-5.74,-0.4,10.46));
#23820=CARTESIAN_POINT('',(-2.9,-0.34,10.4));
#23821=CARTESIAN_POINT('Origin',(-5.77,-0.37,12.));
#23822=CARTESIAN_POINT('',(-5.74,-0.4,12.3751471862576));
#23823=CARTESIAN_POINT('',(-5.74,-0.4,12.));
#23824=CARTESIAN_POINT('',(-5.8,-0.34,12.4));
#23825=CARTESIAN_POINT('',(-5.74,-0.4,12.3751471862576));
#23826=CARTESIAN_POINT('',(-5.8,-0.34,12.));
#23827=CARTESIAN_POINT('Origin',(-4.32878679656441,-0.37,13.8287867965644));
#23828=CARTESIAN_POINT('',(-5.37514718625761,-0.4,12.74));
#23829=CARTESIAN_POINT('',(-4.30757359312881,-0.4,13.8075735931288));
#23830=CARTESIAN_POINT('',(-5.4,-0.34,12.8));
#23831=CARTESIAN_POINT('',(-5.37514718625761,-0.4,12.74));
#23832=CARTESIAN_POINT('',(-4.35,-0.34,13.85));
#23833=CARTESIAN_POINT('Origin',(2.7,-0.37,12.77));
#23834=CARTESIAN_POINT('',(5.4,-0.34,12.8));
#23835=CARTESIAN_POINT('',(2.7,-0.34,12.8));
#23836=CARTESIAN_POINT('',(5.37514718625761,-0.4,12.74));
#23837=CARTESIAN_POINT('',(2.7,-0.4,12.74));
#23838=CARTESIAN_POINT('',(5.37514718625761,-0.4,12.74));
#23839=CARTESIAN_POINT('Origin',(4.52878679656441,-0.37,13.6287867965644));
#23840=CARTESIAN_POINT('',(4.55,-0.34,13.65));
#23841=CARTESIAN_POINT('',(4.50757359312881,-0.4,13.6075735931288));
#23842=CARTESIAN_POINT('Origin',(5.4,0.,12.8));
#23843=CARTESIAN_POINT('',(5.4,0.,12.8));
#23844=CARTESIAN_POINT('',(5.4,0.,12.8));
#23845=CARTESIAN_POINT('',(-5.4,0.,12.8));
#23846=CARTESIAN_POINT('',(5.4,0.,12.8));
#23847=CARTESIAN_POINT('',(-5.4,0.,12.8));
#23848=CARTESIAN_POINT('Origin',(5.8,0.,12.4));
#23849=CARTESIAN_POINT('',(5.8,0.,12.4));
#23850=CARTESIAN_POINT('',(5.8,0.,12.4));
#23851=CARTESIAN_POINT('',(5.8,0.,12.4));
#23852=CARTESIAN_POINT('Origin',(5.8,0.,10.4));
#23853=CARTESIAN_POINT('',(5.8,0.,10.4));
#23854=CARTESIAN_POINT('',(5.8,0.,10.4));
#23855=CARTESIAN_POINT('',(5.8,0.,10.4));
#23856=CARTESIAN_POINT('Origin',(0.,-0.4,11.6));
#23857=CARTESIAN_POINT('',(-3.36,-0.4,11.7));
#23858=CARTESIAN_POINT('Origin',(-3.,-0.4,11.7));
#23859=CARTESIAN_POINT('',(4.7,-0.4,12.1));
#23860=CARTESIAN_POINT('Origin',(5.,-0.4,12.1));
#23861=CARTESIAN_POINT('',(-5.3,-0.4,12.1));
#23862=CARTESIAN_POINT('Origin',(-5.,-0.4,12.1));
#23863=CARTESIAN_POINT('',(2.64,-0.4,11.7));
#23864=CARTESIAN_POINT('Origin',(3.,-0.4,11.7));
#23865=CARTESIAN_POINT('Origin',(3.,0.,11.7));
#23866=CARTESIAN_POINT('',(2.64,0.,11.7));
#23867=CARTESIAN_POINT('Origin',(3.,0.,11.7));
#23868=CARTESIAN_POINT('',(2.64,0.,11.7));
#23869=CARTESIAN_POINT('Origin',(-5.,0.,12.1));
#23870=CARTESIAN_POINT('',(-5.3,0.,12.1));
#23871=CARTESIAN_POINT('Origin',(-5.,0.,12.1));
#23872=CARTESIAN_POINT('',(-5.3,0.,12.1));
#23873=CARTESIAN_POINT('Origin',(5.,0.,12.1));
#23874=CARTESIAN_POINT('',(4.7,0.,12.1));
#23875=CARTESIAN_POINT('Origin',(5.,0.,12.1));
#23876=CARTESIAN_POINT('',(4.7,0.,12.1));
#23877=CARTESIAN_POINT('Origin',(-3.,0.,11.7));
#23878=CARTESIAN_POINT('',(-3.36,0.,11.7));
#23879=CARTESIAN_POINT('Origin',(-3.,0.,11.7));
#23880=CARTESIAN_POINT('',(-3.36,0.,11.7));
#23881=CARTESIAN_POINT('Origin',(-5.8,0.,10.4));
#23882=CARTESIAN_POINT('',(-5.8,0.,10.4));
#23883=CARTESIAN_POINT('',(-5.8,0.,10.4));
#23884=CARTESIAN_POINT('',(-5.8,0.,10.4));
#23885=CARTESIAN_POINT('Origin',(-5.8,0.,12.4));
#23886=CARTESIAN_POINT('',(-5.8,0.,12.4));
#23887=CARTESIAN_POINT('',(-5.8,0.,12.4));
#23888=CARTESIAN_POINT('',(-5.8,0.,12.4));
#23889=CARTESIAN_POINT('Origin',(-5.4,0.,12.8));
#23890=CARTESIAN_POINT('',(-5.4,0.,12.8));
#23891=CARTESIAN_POINT('Origin',(0.,0.,11.6));
#23892=CARTESIAN_POINT('',(0.,0.,0.));
#23893=CARTESIAN_POINT('Origin',(0.,2.1,8.275));
#23894=CARTESIAN_POINT('',(-0.3933,2.1,3.1433));
#23895=CARTESIAN_POINT('Origin',(0.,2.1,3.1433));
#23896=CARTESIAN_POINT('',(0.384471428898077,2.18286501288886,13.3567));
#23897=CARTESIAN_POINT('',(0.29316324943834,1.83781647805639,13.3567));
#23898=CARTESIAN_POINT('Origin',(0.,2.1,13.3567));
#23899=CARTESIAN_POINT('',(-0.392808029221009,2.09981557082489,13.3087163522035));
#23900=CARTESIAN_POINT('Ctrl Pts',(0.293163249438369,1.83781647805643,13.3567));
#23901=CARTESIAN_POINT('Ctrl Pts',(0.205874279401571,1.74021340252209,13.3500765521591));
#23902=CARTESIAN_POINT('Ctrl Pts',(-0.0723649223063588,1.64076470611477,
13.3368296564771));
#23903=CARTESIAN_POINT('Ctrl Pts',(-0.357038552261128,1.85969648354392,
13.3208351072118));
#23904=CARTESIAN_POINT('Ctrl Pts',(-0.393052229550994,2.04530970055771,
13.3114640057871));
#23905=CARTESIAN_POINT('Ctrl Pts',(-0.392808029221009,2.09981557082489,
13.3087163522035));
#23906=CARTESIAN_POINT('',(-0.393251878202368,2.10034280740082,13.1837163495333));
#23907=CARTESIAN_POINT('Ctrl Pts',(-0.392808029221009,2.09981557082489,
13.3087163522035));
#23908=CARTESIAN_POINT('Ctrl Pts',(-0.392463564313855,2.1767006411361,13.3048405579462));
#23909=CARTESIAN_POINT('Ctrl Pts',(-0.333298288113736,2.38542484271478,
13.2943413158479));
#23910=CARTESIAN_POINT('Ctrl Pts',(0.00570651033598579,2.56500954775341,
13.2772186259089));
#23911=CARTESIAN_POINT('Ctrl Pts',(0.394173573742321,2.34685779795354,13.257348282386));
#23912=CARTESIAN_POINT('Ctrl Pts',(0.420885805445878,1.90223262684733,13.2374779388633));
#23913=CARTESIAN_POINT('Ctrl Pts',(0.0615726668307027,1.63903988954688,
13.2176075953405));
#23914=CARTESIAN_POINT('Ctrl Pts',(-0.313461573621718,1.7830432015364,13.1996870664539));
#23915=CARTESIAN_POINT('Ctrl Pts',(-0.392298178424971,2.00783384627357,
13.1883899854082));
#23916=CARTESIAN_POINT('Ctrl Pts',(-0.39306562301603,2.1003425921784,13.1837163522035));
#23917=CARTESIAN_POINT('',(-0.393299999901611,2.10000879729578,13.0587163522061));
#23918=CARTESIAN_POINT('Ctrl Pts',(-0.393299850553082,2.10034286283405,
13.1837163488456));
#23919=CARTESIAN_POINT('Ctrl Pts',(-0.393277891496654,2.12553221774172,
13.1824445054716));
#23920=CARTESIAN_POINT('Ctrl Pts',(-0.390832020267695,2.15061417421091,
13.1811726620976));
#23921=CARTESIAN_POINT('Ctrl Pts',(-0.386046962715129,2.17518399150367,
13.1799008187235));
#23922=CARTESIAN_POINT('Ctrl Pts',(-0.383496234992751,2.18828120369264,
13.1792228485807));
#23923=CARTESIAN_POINT('Ctrl Pts',(-0.380281645786825,2.20123326940233,
13.1785448784378));
#23924=CARTESIAN_POINT('Ctrl Pts',(-0.376421488055696,2.21398137273228,
13.1778669082949));
#23925=CARTESIAN_POINT('Ctrl Pts',(-0.370477346392613,2.23361179651466,
13.1768229223095));
#23926=CARTESIAN_POINT('Ctrl Pts',(-0.362975776245312,2.25283444432371,
13.1757789363242));
#23927=CARTESIAN_POINT('Ctrl Pts',(-0.353993350086029,2.27138727518363,
13.1747349503388));
#23928=CARTESIAN_POINT('Ctrl Pts',(-0.345027440958812,2.28990599079487,
13.1736928840519));
#23929=CARTESIAN_POINT('Ctrl Pts',(-0.334586344420496,2.30775665364154,
13.172650817765));
#23930=CARTESIAN_POINT('Ctrl Pts',(-0.322795237567398,2.32469562657917,
13.1716087514782));
#23931=CARTESIAN_POINT('Ctrl Pts',(-0.311016785982873,2.34161641909875,
13.1705678036299));
#23932=CARTESIAN_POINT('Ctrl Pts',(-0.297891595095139,2.35762684698715,
13.1695268557816));
#23933=CARTESIAN_POINT('Ctrl Pts',(-0.283588888680998,2.3725109763233,13.1684859079333));
#23934=CARTESIAN_POINT('Ctrl Pts',(-0.269278826679315,2.38740276026083,
13.1674444247469));
#23935=CARTESIAN_POINT('Ctrl Pts',(-0.253790537533736,2.40116654681418,
13.1664029415606));
#23936=CARTESIAN_POINT('Ctrl Pts',(-0.237331461545412,2.4136218540866,13.1653614583742));
#23937=CARTESIAN_POINT('Ctrl Pts',(-0.220867349369152,2.42608097246411,
13.1643196565123));
#23938=CARTESIAN_POINT('Ctrl Pts',(-0.203432467039979,2.43723039977957,
13.1632778546504));
#23939=CARTESIAN_POINT('Ctrl Pts',(-0.185264047611803,2.44693244682862,
13.1622360527885));
#23940=CARTESIAN_POINT('Ctrl Pts',(-0.167056352371871,2.45665546740126,
13.1611919987982));
#23941=CARTESIAN_POINT('Ctrl Pts',(-0.148112629136325,2.46492456641514,
13.1601479448079));
#23942=CARTESIAN_POINT('Ctrl Pts',(-0.128691628157987,2.47164950537038,
13.1591038908176));
#23943=CARTESIAN_POINT('Ctrl Pts',(-0.121825642167522,2.47402700057286,
13.1587347821357));
#23944=CARTESIAN_POINT('Ctrl Pts',(-0.114900135186391,2.47621195498811,
13.1583656734539));
#23945=CARTESIAN_POINT('Ctrl Pts',(-0.107926882296612,2.47820190120851,
13.1579965647721));
#23946=CARTESIAN_POINT('Ctrl Pts',(-0.0882047006351017,2.4838299892007,
13.1569526289518));
#23947=CARTESIAN_POINT('Ctrl Pts',(-0.067982306282485,2.48792801563734,
13.1559086931315));
#23948=CARTESIAN_POINT('Ctrl Pts',(-0.0475214463151485,2.49041849615524,
13.1548647573111));
#23949=CARTESIAN_POINT('Ctrl Pts',(-0.0270982382722515,2.49290439370915,
13.1538227425339));
#23950=CARTESIAN_POINT('Ctrl Pts',(-0.0064381506447005,2.49378847026311,
13.1527807277566));
#23951=CARTESIAN_POINT('Ctrl Pts',(0.0141862272639498,2.49304406999218,
13.1517387129793));
#23952=CARTESIAN_POINT('Ctrl Pts',(0.0347884451167996,2.49230046954908,
13.1506978178046));
#23953=CARTESIAN_POINT('Ctrl Pts',(0.0553542967653325,2.48993186339393,
13.1496569226298));
#23954=CARTESIAN_POINT('Ctrl Pts',(0.0756106380122407,2.48596362706787,
13.1486160274551));
#23955=CARTESIAN_POINT('Ctrl Pts',(0.0958773755848161,2.48199335409181,
13.1475745980533));
#23956=CARTESIAN_POINT('Ctrl Pts',(0.115833560205196,2.47642193640849,13.1465331686515));
#23957=CARTESIAN_POINT('Ctrl Pts',(0.135215165358773,2.46932607416347,13.1454917392497));
#23958=CARTESIAN_POINT('Ctrl Pts',(0.154602688013568,2.46222804544291,13.1444499918835));
#23959=CARTESIAN_POINT('Ctrl Pts',(0.173414604016691,2.45360493232044,13.1434082445174));
#23960=CARTESIAN_POINT('Ctrl Pts',(0.191406737712538,2.44358165078805,13.1423664971512));
#23961=CARTESIAN_POINT('Ctrl Pts',(0.209437763911716,2.43353670253637,13.141322497903));
#23962=CARTESIAN_POINT('Ctrl Pts',(0.226644856785306,2.42208595134131,13.1402784986548));
#23963=CARTESIAN_POINT('Ctrl Pts',(0.242812088822247,2.40939809230468,13.1392344994066));
#23964=CARTESIAN_POINT('Ctrl Pts',(0.248532971016366,2.40490840930401,13.1388650733542));
#23965=CARTESIAN_POINT('Ctrl Pts',(0.254123961662768,2.4002641822085,13.1384956473018));
#23966=CARTESIAN_POINT('Ctrl Pts',(0.259576589738731,2.39547399895695,13.1381262212494));
#23967=CARTESIAN_POINT('Ctrl Pts',(0.274985324271206,2.38193728582399,13.1370822498118));
#23968=CARTESIAN_POINT('Ctrl Pts',(0.289378219602958,2.36715166976236,13.1360382783743));
#23969=CARTESIAN_POINT('Ctrl Pts',(0.302548435357331,2.35129531285488,13.1349943069367));
#23970=CARTESIAN_POINT('Ctrl Pts',(0.315694424602928,2.3354681235918,13.1339522558764));
#23971=CARTESIAN_POINT('Ctrl Pts',(0.327621688123889,2.31857462470843,13.1329102048162));
#23972=CARTESIAN_POINT('Ctrl Pts',(0.33816025659571,2.30082960653032,13.1318681537559));
#23973=CARTESIAN_POINT('Ctrl Pts',(0.348687507651402,2.28310364480713,13.130827221759));
#23974=CARTESIAN_POINT('Ctrl Pts',(0.357828625639041,2.26452859383173,13.129786289762));
#23975=CARTESIAN_POINT('Ctrl Pts',(0.365457091351407,2.24534787367199,13.1287453577651));
#23976=CARTESIAN_POINT('Ctrl Pts',(0.373089474834909,2.22615730281952,13.1277038911739));
#23977=CARTESIAN_POINT('Ctrl Pts',(0.37920736717172,2.2063611190848,13.1266624245828));
#23978=CARTESIAN_POINT('Ctrl Pts',(0.383732340163726,2.18622285725067,13.1256209579917));
#23979=CARTESIAN_POINT('Ctrl Pts',(0.388258695777645,2.1660784420976,13.1245791731767));
#23980=CARTESIAN_POINT('Ctrl Pts',(0.391191037230872,2.14559246595596,13.1235373883617));
#23981=CARTESIAN_POINT('Ctrl Pts',(0.392502222912741,2.12503787148615,13.1224956035467));
#23982=CARTESIAN_POINT('Ctrl Pts',(0.393816242581397,2.10443885047177,13.1214515670258));
#23983=CARTESIAN_POINT('Ctrl Pts',(0.393502122194069,2.08377165141165,13.120407530505));
#23984=CARTESIAN_POINT('Ctrl Pts',(0.39158482157553,2.06330916311038,13.1193634939842));
#23985=CARTESIAN_POINT('Ctrl Pts',(0.390906801444503,2.05607295880053,13.118994288565));
#23986=CARTESIAN_POINT('Ctrl Pts',(0.390028765919873,2.04886228550099,13.1186250831458));
#23987=CARTESIAN_POINT('Ctrl Pts',(0.388953345278611,2.04168889302562,13.1182558777266));
#23988=CARTESIAN_POINT('Ctrl Pts',(0.38591248675788,2.02140541436217,13.1172119127868));
#23989=CARTESIAN_POINT('Ctrl Pts',(0.381271655761468,2.00130000996013,13.1161679478471));
#23990=CARTESIAN_POINT('Ctrl Pts',(0.375068685372782,1.9816430346252,13.1151239829074));
#23991=CARTESIAN_POINT('Ctrl Pts',(0.368877125441056,1.96202221859088,13.1140819383568));
#23992=CARTESIAN_POINT('Ctrl Pts',(0.361129292266942,1.94284890588497,13.1130398938062));
#23993=CARTESIAN_POINT('Ctrl Pts',(0.351913775661758,1.92438227737644,13.1119978492557));
#23994=CARTESIAN_POINT('Ctrl Pts',(0.342708155609275,1.90593548019913,13.1109569237578));
#23995=CARTESIAN_POINT('Ctrl Pts',(0.332038282154381,1.88819452852851,13.1099159982599));
#23996=CARTESIAN_POINT('Ctrl Pts',(0.320040337939026,1.87139756761602,13.1088750727621));
#23997=CARTESIAN_POINT('Ctrl Pts',(0.308036230796624,1.85459197868835,13.1078336125769));
#23998=CARTESIAN_POINT('Ctrl Pts',(0.294703104591166,1.83873195732152,13.1067921523918));
#23999=CARTESIAN_POINT('Ctrl Pts',(0.280220087396299,1.82402610156102,13.1057506922067));
#24000=CARTESIAN_POINT('Ctrl Pts',(0.265732644198551,1.80931575169828,13.1047089137518));
#24001=CARTESIAN_POINT('Ctrl Pts',(0.250095152073664,1.79576076800596,13.103667135297));
#24002=CARTESIAN_POINT('Ctrl Pts',(0.233522411733559,1.78353171846433,13.1026253568422));
#24003=CARTESIAN_POINT('Ctrl Pts',(0.216913848346639,1.77127623504361,13.101581326516));
#24004=CARTESIAN_POINT('Ctrl Pts',(0.199366625946405,1.76035279699869,13.1005372961899));
#24005=CARTESIAN_POINT('Ctrl Pts',(0.181123703314227,1.75088813526645,13.0994932658637));
#24006=CARTESIAN_POINT('Ctrl Pts',(0.17467169949027,1.74754075311063,13.0991240219771));
#24007=CARTESIAN_POINT('Ctrl Pts',(0.168132872239832,1.74437540547865,13.0987547780904));
#24008=CARTESIAN_POINT('Ctrl Pts',(0.161518528472187,1.7413962424065,13.0983855342038));
#24009=CARTESIAN_POINT('Ctrl Pts',(0.142817870497033,1.73297328895537,13.0973415752146));
#24010=CARTESIAN_POINT('Ctrl Pts',(0.123400847963987,1.72599199312796,13.0962976162254));
#24011=CARTESIAN_POINT('Ctrl Pts',(0.10351525561347,1.72056689409689,13.0952536572363));
#24012=CARTESIAN_POINT('Ctrl Pts',(0.0836662466095349,1.71515177557205,
13.0942116188091));
#24013=CARTESIAN_POINT('Ctrl Pts',(0.0633510650414822,1.71128741990603,
13.093169580382));
#24014=CARTESIAN_POINT('Ctrl Pts',(0.0428355866410116,1.70903964073436,
13.0921275419548));
#24015=CARTESIAN_POINT('Ctrl Pts',(0.022342142943603,1.70679427579577,13.0910866227318));
#24016=CARTESIAN_POINT('Ctrl Pts',(0.00164955404500148,1.70616214888769,
13.0900457035087));
#24017=CARTESIAN_POINT('Ctrl Pts',(-0.0189682279706726,1.70715766988822,
13.0890047842856));
#24018=CARTESIAN_POINT('Ctrl Pts',(-0.0395965976908121,1.70815370211164,
13.0879633305267));
#24019=CARTESIAN_POINT('Ctrl Pts',(-0.0601493480777889,1.71077903267315,
13.0869218767677));
#24020=CARTESIAN_POINT('Ctrl Pts',(-0.0803541232532163,1.71499596771435,
13.0858804230087));
#24021=CARTESIAN_POINT('Ctrl Pts',(-0.100565071178656,1.71921419106912,
13.0848386510757));
#24022=CARTESIAN_POINT('Ctrl Pts',(-0.120427119989594,1.72502480129605,
13.0837968791428));
#24023=CARTESIAN_POINT('Ctrl Pts',(-0.139680579560224,1.73233952388961,
13.0827551072098));
#24024=CARTESIAN_POINT('Ctrl Pts',(-0.158975656144607,1.73967005750714,
13.0817110834511));
#24025=CARTESIAN_POINT('Ctrl Pts',(-0.177658851470548,1.74851087932031,
13.0806670596923));
#24026=CARTESIAN_POINT('Ctrl Pts',(-0.195492091675046,1.75872630911171,
13.0796230359336));
#24027=CARTESIAN_POINT('Ctrl Pts',(-0.201799888898195,1.76233960983175,
13.0792537541827));
#24028=CARTESIAN_POINT('Ctrl Pts',(-0.20800160610377,1.7661244877695,13.0788844724318));
#24029=CARTESIAN_POINT('Ctrl Pts',(-0.214087630197371,1.7700736800489,13.078515190681));
#24030=CARTESIAN_POINT('Ctrl Pts',(-0.231281785301351,1.78123088605782,
13.0774719007426));
#24031=CARTESIAN_POINT('Ctrl Pts',(-0.247652961663615,1.79376928691335,
13.0764286108042));
#24032=CARTESIAN_POINT('Ctrl Pts',(-0.262970887533086,1.80754281969823,
13.0753853208659));
#24033=CARTESIAN_POINT('Ctrl Pts',(-0.2782606347176,1.82129101484639,13.074343950152));
#24034=CARTESIAN_POINT('Ctrl Pts',(-0.29250039560478,1.83626938927644,13.0733025794381));
#24035=CARTESIAN_POINT('Ctrl Pts',(-0.305491059368287,1.85229028552348,
13.0722612087243));
#24036=CARTESIAN_POINT('Ctrl Pts',(-0.318467806746011,1.86829401921617,
13.0712209535898));
#24037=CARTESIAN_POINT('Ctrl Pts',(-0.330197629191986,1.88533750641536,
13.0701806984553));
#24038=CARTESIAN_POINT('Ctrl Pts',(-0.340520257307395,1.90319846453011,
13.0691404433208));
#24039=CARTESIAN_POINT('Ctrl Pts',(-0.350848207924016,1.9210686320216,13.0680996518152));
#24040=CARTESIAN_POINT('Ctrl Pts',(-0.359767132357192,1.93975648239246,
13.0670588603096));
#24041=CARTESIAN_POINT('Ctrl Pts',(-0.367161437262072,1.95901287651828,
13.0660180688041));
#24042=CARTESIAN_POINT('Ctrl Pts',(-0.374558056424921,1.97827529748018,
13.0649769515532));
#24043=CARTESIAN_POINT('Ctrl Pts',(-0.380428876601272,1.99810591598814,
13.0639358343023));
#24044=CARTESIAN_POINT('Ctrl Pts',(-0.384707693247568,2.01823887992367,
13.0628947170515));
#24045=CARTESIAN_POINT('Ctrl Pts',(-0.388995726059894,2.03841520835778,
13.0618513573326));
#24046=CARTESIAN_POINT('Ctrl Pts',(-0.3916848148126,2.05889445100123,13.0608079976137));
#24047=CARTESIAN_POINT('Ctrl Pts',(-0.392760317080386,2.07940331757505,
13.0597646378949));
#24048=CARTESIAN_POINT('Ctrl Pts',(-0.393120510410699,2.08627188231304,
13.0594152093319));
#24049=CARTESIAN_POINT('Ctrl Pts',(-0.393300153457839,2.09314377131058,
13.059065780769));
#24050=CARTESIAN_POINT('Ctrl Pts',(-0.393299999901611,2.10000879729578,
13.0587163522061));
#24051=CARTESIAN_POINT('',(-0.393299846364205,2.09965236528803,12.9337163522064));
#24052=CARTESIAN_POINT('Ctrl Pts',(-0.39329999990161,2.10000879734644,13.0587163522035));
#24053=CARTESIAN_POINT('Ctrl Pts',(-0.393299989427263,2.10047707045121,
13.0586925171884));
#24054=CARTESIAN_POINT('Ctrl Pts',(-0.393299142646321,2.10094534245175,
13.0586686821733));
#24055=CARTESIAN_POINT('Ctrl Pts',(-0.393297459568052,2.10141361144476,
13.0586448471582));
#24056=CARTESIAN_POINT('Ctrl Pts',(-0.393223741505037,2.12192358044329,
13.057600884333));
#24057=CARTESIAN_POINT('Ctrl Pts',(-0.391541130597174,2.14248887778938,
13.0565569215078));
#24058=CARTESIAN_POINT('Ctrl Pts',(-0.388247938399845,2.16283652065694,
13.0555129586825));
#24059=CARTESIAN_POINT('Ctrl Pts',(-0.384960804350849,2.18314673205032,
13.0544709163288));
#24060=CARTESIAN_POINT('Ctrl Pts',(-0.380069027615285,2.20323935611151,
13.053428873975));
#24061=CARTESIAN_POINT('Ctrl Pts',(-0.37362275919439,2.22284512123797,13.0523868316213));
#24062=CARTESIAN_POINT('Ctrl Pts',(-0.367183413903594,2.24242983026595,
13.0513459083948));
#24063=CARTESIAN_POINT('Ctrl Pts',(-0.359193092431404,2.26152801393411,
13.0503049851684));
#24064=CARTESIAN_POINT('Ctrl Pts',(-0.349752081724406,2.27988432763708,
13.0492640619419));
#24065=CARTESIAN_POINT('Ctrl Pts',(-0.34030622225204,2.29825006887498,13.0482226041124));
#24066=CARTESIAN_POINT('Ctrl Pts',(-0.329408507284762,2.31587251728544,
13.047181146283));
#24067=CARTESIAN_POINT('Ctrl Pts',(-0.317205992928561,2.33251934984041,
13.0461396884535));
#24068=CARTESIAN_POINT('Ctrl Pts',(-0.304999750088171,2.34917126884315,
13.0450979124061));
#24069=CARTESIAN_POINT('Ctrl Pts',(-0.29148837798416,2.36484640701149,13.0440561363587));
#24070=CARTESIAN_POINT('Ctrl Pts',(-0.276859733177765,2.37934490892933,
13.0430143603113));
#24071=CARTESIAN_POINT('Ctrl Pts',(-0.262199468123118,2.39387474978772,
13.0419703324342));
#24072=CARTESIAN_POINT('Ctrl Pts',(-0.246417671226193,2.40722240116009,
13.0409263045571));
#24073=CARTESIAN_POINT('Ctrl Pts',(-0.229736404323014,2.41922730855729,
13.0398822766799));
#24074=CARTESIAN_POINT('Ctrl Pts',(-0.223836479544724,2.42347327206983,
13.0395130189984));
#24075=CARTESIAN_POINT('Ctrl Pts',(-0.21782429496167,2.42755166837154,13.0391437613169));
#24076=CARTESIAN_POINT('Ctrl Pts',(-0.211710439165922,2.43145675426543,
13.0387745036354));
#24077=CARTESIAN_POINT('Ctrl Pts',(-0.194425398337294,2.44249717971381,
13.0377305414756));
#24078=CARTESIAN_POINT('Ctrl Pts',(-0.176222914177312,2.45221477202946,
13.0366865793157));
#24079=CARTESIAN_POINT('Ctrl Pts',(-0.157331601041175,2.46046034083352,
13.0356426171559));
#24080=CARTESIAN_POINT('Ctrl Pts',(-0.138475040730624,2.46869074092949,
13.0346005754891));
#24081=CARTESIAN_POINT('Ctrl Pts',(-0.11893280968917,2.47545414719846,13.0335585338223));
#24082=CARTESIAN_POINT('Ctrl Pts',(-0.0989584635155615,2.48064696570266,
13.0325164921555));
#24083=CARTESIAN_POINT('Ctrl Pts',(-0.0790055696679896,2.48583420715144,
13.0314755696351));
#24084=CARTESIAN_POINT('Ctrl Pts',(-0.0586221832361915,2.48945399735763,
13.0304346471147));
#24085=CARTESIAN_POINT('Ctrl Pts',(-0.0380772893152163,2.49145243649568,
13.0293937245942));
#24086=CARTESIAN_POINT('Ctrl Pts',(-0.017521844227084,2.49345190196492,
13.028352267491));
#24087=CARTESIAN_POINT('Ctrl Pts',(0.00319454329350911,2.49382826559513,
13.0273108103878));
#24088=CARTESIAN_POINT('Ctrl Pts',(0.023796928057364,2.49257941389613,13.0262693532845));
#24089=CARTESIAN_POINT('Ctrl Pts',(0.0444056076453001,2.49133018062472,
13.0252275779759));
#24090=CARTESIAN_POINT('Ctrl Pts',(0.0648994835106651,2.48845482407434,
13.0241858026673));
#24091=CARTESIAN_POINT('Ctrl Pts',(0.0850088237426345,2.48400311181798,
13.0231440273587));
#24092=CARTESIAN_POINT('Ctrl Pts',(0.1051616307887,2.47954177708039,13.0221000002282));
#24093=CARTESIAN_POINT('Ctrl Pts',(0.124927538499802,2.47349749943457,13.0210559730976));
#24094=CARTESIAN_POINT('Ctrl Pts',(0.144051343921903,2.46597008117371,13.0200119459671));
#24095=CARTESIAN_POINT('Ctrl Pts',(0.150815242582771,2.46330770864008,13.0196426840156));
#24096=CARTESIAN_POINT('Ctrl Pts',(0.157499014214537,2.46046023452778,13.0192734220641));
#24097=CARTESIAN_POINT('Ctrl Pts',(0.164092097660787,2.45743345322631,13.0189041601126));
#24098=CARTESIAN_POINT('Ctrl Pts',(0.182731804010363,2.4488762561115,13.0178601972387));
#24099=CARTESIAN_POINT('Ctrl Pts',(0.200755875449437,2.43883158084948,13.0168162343649));
#24100=CARTESIAN_POINT('Ctrl Pts',(0.217915116787653,2.42741089150397,13.0157722714911));
#24101=CARTESIAN_POINT('Ctrl Pts',(0.235042791917278,2.41601121170398,13.0147302290955));
#24102=CARTESIAN_POINT('Ctrl Pts',(0.251308156361853,2.40324089595244,13.0136881866999));
#24103=CARTESIAN_POINT('Ctrl Pts',(0.266486852156776,2.38925706149993,13.0126461443043));
#24104=CARTESIAN_POINT('Ctrl Pts',(0.28164924631423,2.37528824542599,13.0116052210429));
#24105=CARTESIAN_POINT('Ctrl Pts',(0.295726730730443,2.36010897274665,13.0105642977815));
#24106=CARTESIAN_POINT('Ctrl Pts',(0.308528378921624,2.34391623439204,13.0095233745201));
#24107=CARTESIAN_POINT('Ctrl Pts',(0.321336601720315,2.32771517985053,13.0084819166665));
#24108=CARTESIAN_POINT('Ctrl Pts',(0.332867210316033,2.31050018700096,13.0074404588128));
#24109=CARTESIAN_POINT('Ctrl Pts',(0.34296959482452,2.29250129097205,13.0063990009592));
#24110=CARTESIAN_POINT('Ctrl Pts',(0.353075066061434,2.27449689547873,13.0053572248938));
#24111=CARTESIAN_POINT('Ctrl Pts',(0.36175111619616,2.25570877877258,13.0043154488284));
#24112=CARTESIAN_POINT('Ctrl Pts',(0.368893579926101,2.23639067669495,13.003273672763));
#24113=CARTESIAN_POINT('Ctrl Pts',(0.376051482236477,2.21703081814727,13.0022296448774));
#24114=CARTESIAN_POINT('Ctrl Pts',(0.381668979991324,2.19713939590162,13.0011856169919));
#24115=CARTESIAN_POINT('Ctrl Pts',(0.385691842767505,2.17698501427295,13.0001415891064));
#24116=CARTESIAN_POINT('Ctrl Pts',(0.387114670926065,2.16985670209948,12.9997723316008));
#24117=CARTESIAN_POINT('Ctrl Pts',(0.388338492958074,2.16269556421669,12.9994030740953));
#24118=CARTESIAN_POINT('Ctrl Pts',(0.389362463971912,2.15551361679554,12.9990338165898));
#24119=CARTESIAN_POINT('Ctrl Pts',(0.392257428810782,2.13520885720969,12.9979898539379));
#24120=CARTESIAN_POINT('Ctrl Pts',(0.393568441845717,2.11461653557569,12.9969458912861));
#24121=CARTESIAN_POINT('Ctrl Pts',(0.393254330125343,2.09400651706701,12.9959019286342));
#24122=CARTESIAN_POINT('Ctrl Pts',(0.392940796247009,2.07343441288748,12.9948598864631));
#24123=CARTESIAN_POINT('Ctrl Pts',(0.391008023454439,2.05284540474457,12.993817844292));
#24124=CARTESIAN_POINT('Ctrl Pts',(0.387466669650576,2.03251318714081,12.9927758021209));
#24125=CARTESIAN_POINT('Ctrl Pts',(0.383929119201573,2.0122028059993,12.9917348790857));
#24126=CARTESIAN_POINT('Ctrl Pts',(0.378786514539462,1.99214939404301,12.9906939560505));
#24127=CARTESIAN_POINT('Ctrl Pts',(0.372101137137044,1.97262012034345,12.9896530330153));
#24128=CARTESIAN_POINT('Ctrl Pts',(0.365412326289747,1.95308081689078,12.9886115753877));
#24129=CARTESIAN_POINT('Ctrl Pts',(0.357179382852222,1.93406689080609,12.9875701177601));
#24130=CARTESIAN_POINT('Ctrl Pts',(0.347514196557822,1.9158294996728,12.9865286601325));
#24131=CARTESIAN_POINT('Ctrl Pts',(0.337846057119786,1.89758653620661,12.9854868842933));
#24132=CARTESIAN_POINT('Ctrl Pts',(0.326745179860557,1.88012121266505,12.9844451084542));
#24133=CARTESIAN_POINT('Ctrl Pts',(0.314368523790327,1.86365846482285,12.983403332615));
#24134=CARTESIAN_POINT('Ctrl Pts',(0.301965115283709,1.84716013235974,12.9823593049526));
#24135=CARTESIAN_POINT('Ctrl Pts',(0.288280910085889,1.83166925404743,12.9813152772902));
#24136=CARTESIAN_POINT('Ctrl Pts',(0.273512399539091,1.81737682809372,12.9802712496278));
#24137=CARTESIAN_POINT('Ctrl Pts',(0.268288971587627,1.81232178500157,12.9799019907742));
#24138=CARTESIAN_POINT('Ctrl Pts',(0.262930216575671,1.80741630175329,12.9795327319206));
#24139=CARTESIAN_POINT('Ctrl Pts',(0.257445780669388,1.80266759339835,12.979163473067));
#24140=CARTESIAN_POINT('Ctrl Pts',(0.2419402732851,1.78924212289936,12.9781195104829));
#24141=CARTESIAN_POINT('Ctrl Pts',(0.225335556935778,1.77699280464536,12.9770755478987));
#24142=CARTESIAN_POINT('Ctrl Pts',(0.207836251371787,1.76610034049774,12.9760315853146));
#24143=CARTESIAN_POINT('Ctrl Pts',(0.190369137693771,1.75522791422892,12.9749895432138));
#24144=CARTESIAN_POINT('Ctrl Pts',(0.17201128761171,1.74570782235724,12.973947501113));
#24145=CARTESIAN_POINT('Ctrl Pts',(0.152998597630337,1.73767925932518,12.9729054590122));
#24146=CARTESIAN_POINT('Ctrl Pts',(0.13400632700451,1.72965931885433,12.9718645360496));
#24147=CARTESIAN_POINT('Ctrl Pts',(0.114361275810847,1.72312803852619,12.970823613087));
#24148=CARTESIAN_POINT('Ctrl Pts',(0.0943217986337186,1.71817767443155,
12.9697826901245));
#24149=CARTESIAN_POINT('Ctrl Pts',(0.074272029725231,1.71322476796432,12.9687412325721));
#24150=CARTESIAN_POINT('Ctrl Pts',(0.0538281405908412,1.70985459186216,
12.9676997750198));
#24151=CARTESIAN_POINT('Ctrl Pts',(0.0332618769233426,1.70810902339613,
12.9666583174674));
#24152=CARTESIAN_POINT('Ctrl Pts',(0.0126893293803217,1.70636292158407,
12.9656165417051));
#24153=CARTESIAN_POINT('Ctrl Pts',(-0.00800493154724586,1.70624244172002,
12.9645747659428));
#24154=CARTESIAN_POINT('Ctrl Pts',(-0.0285468111130381,1.70773737168158,
12.9635329901805));
#24155=CARTESIAN_POINT('Ctrl Pts',(-0.0491330924183241,1.70923553296822,
12.9624889625963));
#24156=CARTESIAN_POINT('Ctrl Pts',(-0.0695656067424458,1.71235596399375,
12.961444935012));
#24157=CARTESIAN_POINT('Ctrl Pts',(-0.0895773950829874,1.71703684212428,
12.9604009074277));
#24158=CARTESIAN_POINT('Ctrl Pts',(-0.0966553104131074,1.71869240925874,
12.9600316481332));
#24159=CARTESIAN_POINT('Ctrl Pts',(-0.103680728015908,1.72054272172845,
12.9596623888388));
#24160=CARTESIAN_POINT('Ctrl Pts',(-0.110642359662777,1.72258357448535,
12.9592931295443));
#24161=CARTESIAN_POINT('Ctrl Pts',(-0.130324149002113,1.72835343363211,
12.9582491668622));
#24162=CARTESIAN_POINT('Ctrl Pts',(-0.149612029943242,1.73568420011201,
12.9572052041802));
#24163=CARTESIAN_POINT('Ctrl Pts',(-0.168243300725745,1.74450164309676,
12.9561612414981));
#24164=CARTESIAN_POINT('Ctrl Pts',(-0.186840297289561,1.75330286545046,
12.9551191992973));
#24165=CARTESIAN_POINT('Ctrl Pts',(-0.204782398349391,1.76358507820212,
12.9540771570964));
#24166=CARTESIAN_POINT('Ctrl Pts',(-0.221824871663632,1.77522528375593,
12.9530351148956));
#24167=CARTESIAN_POINT('Ctrl Pts',(-0.238849041637425,1.78685298791742,
12.9519941918312));
#24168=CARTESIAN_POINT('Ctrl Pts',(-0.254974881161543,1.79983540048527,
12.9509532687668));
#24169=CARTESIAN_POINT('Ctrl Pts',(-0.269984967643882,1.81400523213469,
12.9499123457024));
#24170=CARTESIAN_POINT('Ctrl Pts',(-0.285002762918998,1.8281823410437,12.9488708880468));
#24171=CARTESIAN_POINT('Ctrl Pts',(-0.298903114282888,1.84354759397336,
12.9478294303912));
#24172=CARTESIAN_POINT('Ctrl Pts',(-0.311503709712774,1.85989517115397,
12.9467879727356));
#24173=CARTESIAN_POINT('Ctrl Pts',(-0.324108155176177,1.87624774323506,
12.9457461968691));
#24174=CARTESIAN_POINT('Ctrl Pts',(-0.335411633959992,1.8935826327288,12.9447044210026));
#24175=CARTESIAN_POINT('Ctrl Pts',(-0.34527436015343,1.91166384781291,12.9436626451361));
#24176=CARTESIAN_POINT('Ctrl Pts',(-0.35515840485029,1.92978414584813,12.9426186174477));
#24177=CARTESIAN_POINT('Ctrl Pts',(-0.363595178957836,1.94865331781493,
12.9415745897594));
#24178=CARTESIAN_POINT('Ctrl Pts',(-0.370492154315508,1.96801343405235,
12.940530562071));
#24179=CARTESIAN_POINT('Ctrl Pts',(-0.372931522607136,1.97486084921953,
12.9401613033878));
#24180=CARTESIAN_POINT('Ctrl Pts',(-0.37517872820195,1.98176954231094,12.9397920447047));
#24181=CARTESIAN_POINT('Ctrl Pts',(-0.377231196270089,1.98872774577354,
12.9394227860215));
#24182=CARTESIAN_POINT('Ctrl Pts',(-0.384364369069022,2.01291037177361,
12.9381394598467));
#24183=CARTESIAN_POINT('Ctrl Pts',(-0.389176175554744,2.03780721766341,
12.936856133672));
#24184=CARTESIAN_POINT('Ctrl Pts',(-0.391557233824522,2.06301591369671,
12.9355728074972));
#24185=CARTESIAN_POINT('Ctrl Pts',(-0.392705377429683,2.07517151841772,
12.9349539890669));
#24186=CARTESIAN_POINT('Ctrl Pts',(-0.393289015992787,2.08739932130897,
12.9343351706367));
#24187=CARTESIAN_POINT('Ctrl Pts',(-0.393299846364205,2.09965236528802,
12.9337163522064));
#24188=CARTESIAN_POINT('',(-0.39329996604184,2.10016343649383,12.8087163521999));
#24189=CARTESIAN_POINT('Ctrl Pts',(-0.393299846364255,2.09965236534526,
12.9337163522035));
#24190=CARTESIAN_POINT('Ctrl Pts',(-0.393317930215556,2.12011170632657,
12.9326830891799));
#24191=CARTESIAN_POINT('Ctrl Pts',(-0.391735263661162,2.14060277128025,
12.9316498261563));
#24192=CARTESIAN_POINT('Ctrl Pts',(-0.388563460451927,2.16085496858617,
12.9306165631326));
#24193=CARTESIAN_POINT('Ctrl Pts',(-0.385390688312413,2.18111335258335,
12.9295829844653));
#24194=CARTESIAN_POINT('Ctrl Pts',(-0.380627895954077,2.20113197993515,
12.9285494057979));
#24195=CARTESIAN_POINT('Ctrl Pts',(-0.374338427906584,2.22064672143257,
12.9275158271306));
#24196=CARTESIAN_POINT('Ctrl Pts',(-0.368048185872011,2.24016386443002,
12.9264821212702));
#24197=CARTESIAN_POINT('Ctrl Pts',(-0.360231150982646,2.25917629499611,
12.9254484154098));
#24198=CARTESIAN_POINT('Ctrl Pts',(-0.350999807899556,2.27743738291148,
12.9244147095494));
#24199=CARTESIAN_POINT('Ctrl Pts',(-0.341747795418505,2.2957393582351,12.9233786891745));
#24200=CARTESIAN_POINT('Ctrl Pts',(-0.331075534220016,2.31328598694484,
12.9223426687996));
#24201=CARTESIAN_POINT('Ctrl Pts',(-0.319140661220974,2.32985675616662,
12.9213066484246));
#24202=CARTESIAN_POINT('Ctrl Pts',(-0.312404556588541,2.3392093848311,12.920721913116));
#24203=CARTESIAN_POINT('Ctrl Pts',(-0.305267016299046,2.34825170990766,
12.9201371778073));
#24204=CARTESIAN_POINT('Ctrl Pts',(-0.297761766329719,2.35694906209637,
12.9195524424987));
#24205=CARTESIAN_POINT('Ctrl Pts',(-0.284362198264628,2.3724769609825,12.9185084798591));
#24206=CARTESIAN_POINT('Ctrl Pts',(-0.269704794752743,2.3870001484392,12.9174645172196));
#24207=CARTESIAN_POINT('Ctrl Pts',(-0.253965873338599,2.40031021491012,
12.9164205545801));
#24208=CARTESIAN_POINT('Ctrl Pts',(-0.238255905369688,2.41359579607672,
12.9153785124225));
#24209=CARTESIAN_POINT('Ctrl Pts',(-0.22146888578192,2.42567217086989,12.9143364702649));
#24210=CARTESIAN_POINT('Ctrl Pts',(-0.20381808603056,2.43636747435928,12.9132944281074));
#24211=CARTESIAN_POINT('Ctrl Pts',(-0.186186242963999,2.44705129125882,
12.9122535050869));
#24212=CARTESIAN_POINT('Ctrl Pts',(-0.167693072504943,2.45635657735828,
12.9112125820665));
#24213=CARTESIAN_POINT('Ctrl Pts',(-0.148580860049953,2.46415466223408,
12.910171659046));
#24214=CARTESIAN_POINT('Ctrl Pts',(-0.129458832063715,2.47195675200183,
12.9091302014348));
#24215=CARTESIAN_POINT('Ctrl Pts',(-0.109717802104711,2.47824980126081,
12.9080887438235));
#24216=CARTESIAN_POINT('Ctrl Pts',(-0.0896205958273914,2.4829530503907,
12.9070472862123));
#24217=CARTESIAN_POINT('Ctrl Pts',(-0.0695172489793877,2.48765773656778,
12.9060055103905));
#24218=CARTESIAN_POINT('Ctrl Pts',(-0.0490582332257658,2.49077152330589,
12.9049637345686));
#24219=CARTESIAN_POINT('Ctrl Pts',(-0.0285162361747516,2.49226485220374,
12.9039219587468));
#24220=CARTESIAN_POINT('Ctrl Pts',(-0.00792983713114693,2.49376140896588,
12.9028779311029));
#24221=CARTESIAN_POINT('Ctrl Pts',(0.0127391648422252,2.49363051966932,
12.901833903459));
#24222=CARTESIAN_POINT('Ctrl Pts',(0.0332176744469679,2.49189472579295,
12.9007898758151));
#24223=CARTESIAN_POINT('Ctrl Pts',(0.0404606559185965,2.4912807981621,12.9004206168687));
#24224=CARTESIAN_POINT('Ctrl Pts',(0.0476798729945234,2.4904665786042,12.9000513579223));
#24225=CARTESIAN_POINT('Ctrl Pts',(0.0548635477976874,2.48945459443053,
12.8996820989759));
#24226=CARTESIAN_POINT('Ctrl Pts',(0.075173111794499,2.48659352987763,12.8986381363232));
#24227=CARTESIAN_POINT('Ctrl Pts',(0.0953187854656397,2.48213098626654,
12.8975941736705));
#24228=CARTESIAN_POINT('Ctrl Pts',(0.115029890446542,2.47610239869463,12.8965502110178));
#24229=CARTESIAN_POINT('Ctrl Pts',(0.13470473472776,2.4700849013586,12.8955081688468));
#24230=CARTESIAN_POINT('Ctrl Pts',(0.153945884114854,2.4625072344424,12.8944661266759));
#24231=CARTESIAN_POINT('Ctrl Pts',(0.172493383800945,2.4534556868193,12.8934240845049));
#24232=CARTESIAN_POINT('Ctrl Pts',(0.191020963765159,2.44441386041546,12.8923831614707));
#24233=CARTESIAN_POINT('Ctrl Pts',(0.208855702399793,2.43390159085845,12.8913422384366));
#24234=CARTESIAN_POINT('Ctrl Pts',(0.225758257843078,2.42205294442942,12.8903013154024));
#24235=CARTESIAN_POINT('Ctrl Pts',(0.242669493999045,2.41019821284388,12.8892598577773));
#24236=CARTESIAN_POINT('Ctrl Pts',(0.258646978794167,2.39700614239969,12.8882184001522));
#24237=CARTESIAN_POINT('Ctrl Pts',(0.273480535815841,2.38265400497761,12.8871769425271));
#24238=CARTESIAN_POINT('Ctrl Pts',(0.288318625136341,2.36829748235138,12.8861351666912));
#24239=CARTESIAN_POINT('Ctrl Pts',(0.302011587692007,2.35278072431232,12.8850933908553));
#24240=CARTESIAN_POINT('Ctrl Pts',(0.314386959518568,2.33631701099301,12.8840516150195));
#24241=CARTESIAN_POINT('Ctrl Pts',(0.326789080991684,2.31981771098439,12.8830075873615));
#24242=CARTESIAN_POINT('Ctrl Pts',(0.337867531099198,2.30236799098489,12.8819635597036));
#24243=CARTESIAN_POINT('Ctrl Pts',(0.347493431699077,2.2842096765265,12.8809195320456));
#24244=CARTESIAN_POINT('Ctrl Pts',(0.35089798625785,2.27778731930107,12.8805502731815));
#24245=CARTESIAN_POINT('Ctrl Pts',(0.354121267761971,2.27127652200698,12.8801810143173));
#24246=CARTESIAN_POINT('Ctrl Pts',(0.357159025645194,2.26468855576565,12.8798117554531));
#24247=CARTESIAN_POINT('Ctrl Pts',(0.365747325257615,2.24606316490433,12.8787677928062));
#24248=CARTESIAN_POINT('Ctrl Pts',(0.3729003558302,2.22670866641481,12.8777238301594));
#24249=CARTESIAN_POINT('Ctrl Pts',(0.378501388736522,2.20687183316723,12.8766798675126));
#24250=CARTESIAN_POINT('Ctrl Pts',(0.384092117939278,2.18707149191191,12.8756378253475));
#24251=CARTESIAN_POINT('Ctrl Pts',(0.388136261762029,2.16679126110359,12.8745957831825));
#24252=CARTESIAN_POINT('Ctrl Pts',(0.390565655198947,2.14629642512136,12.8735537410174));
#24253=CARTESIAN_POINT('Ctrl Pts',(0.392992439505489,2.12582360027092,12.8725128179893));
#24254=CARTESIAN_POINT('Ctrl Pts',(0.393807801369165,2.10513735136339,12.8714718949611));
#24255=CARTESIAN_POINT('Ctrl Pts',(0.392994906043685,2.08451149381913,12.870430971933));
#24256=CARTESIAN_POINT('Ctrl Pts',(0.392181593236339,2.06387504337163,12.8693895143139));
#24257=CARTESIAN_POINT('Ctrl Pts',(0.389738365505875,2.04329978209165,12.8683480566948));
#24258=CARTESIAN_POINT('Ctrl Pts',(0.385700503932339,2.02305839053971,12.8673065990757));
#24259=CARTESIAN_POINT('Ctrl Pts',(0.381661408616018,2.00281081436001,12.8662648232459));
#24260=CARTESIAN_POINT('Ctrl Pts',(0.376026888797889,1.9828980248649,12.865223047416));
#24261=CARTESIAN_POINT('Ctrl Pts',(0.368882916370616,1.96358048523063,12.8641812715862));
#24262=CARTESIAN_POINT('Ctrl Pts',(0.36172350208465,1.94422119029561,12.8631372439343));
#24263=CARTESIAN_POINT('Ctrl Pts',(0.353048430440259,1.92546038241904,12.8620932162823));
#24264=CARTESIAN_POINT('Ctrl Pts',(0.342991268606171,1.90753732917802,12.8610491886304));
#24265=CARTESIAN_POINT('Ctrl Pts',(0.339434182249748,1.90119818010189,12.8606799297304));
#24266=CARTESIAN_POINT('Ctrl Pts',(0.335704607486352,1.89496357446836,12.8603106708303));
#24267=CARTESIAN_POINT('Ctrl Pts',(0.331809720370535,1.88884318749416,12.8599414119303));
#24268=CARTESIAN_POINT('Ctrl Pts',(0.320798160023472,1.87153973080601,12.8588974492837));
#24269=CARTESIAN_POINT('Ctrl Pts',(0.30839661586408,1.85504839488947,12.8578534866371));
#24270=CARTESIAN_POINT('Ctrl Pts',(0.294749391624824,1.83960090987717,12.8568095239905));
#24271=CARTESIAN_POINT('Ctrl Pts',(0.281127272925502,1.82418184217854,12.8557674818258));
#24272=CARTESIAN_POINT('Ctrl Pts',(0.266264459886931,1.80980339827059,12.854725439661));
#24273=CARTESIAN_POINT('Ctrl Pts',(0.250347109415109,1.7966664957386,12.8536833974962));
#24274=CARTESIAN_POINT('Ctrl Pts',(0.234446853928001,1.78354370203386,12.8526424744684));
#24275=CARTESIAN_POINT('Ctrl Pts',(0.217494855587536,1.77166029087087,12.8516015514406));
#24276=CARTESIAN_POINT('Ctrl Pts',(0.199712230348975,1.76117863844049,12.8505606284128));
#24277=CARTESIAN_POINT('Ctrl Pts',(0.181920472417946,1.75069160290684,12.849519170794));
#24278=CARTESIAN_POINT('Ctrl Pts',(0.163297861035636,1.74160815182395,12.8484777131753));
#24279=CARTESIAN_POINT('Ctrl Pts',(0.144092769185384,1.73404622714271,12.8474362555565));
#24280=CARTESIAN_POINT('Ctrl Pts',(0.124881809342569,1.72648199196391,12.8463944797271));
#24281=CARTESIAN_POINT('Ctrl Pts',(0.105088712027454,1.72044044435186,12.8453527038977));
#24282=CARTESIAN_POINT('Ctrl Pts',(0.0849790174808098,1.71599029102379,
12.8443109280682));
#24283=CARTESIAN_POINT('Ctrl Pts',(0.0648258553731176,1.71153051858832,
12.8432669004167));
#24284=CARTESIAN_POINT('Ctrl Pts',(0.0443554591847135,1.70866910985458,
12.8422228727652));
#24285=CARTESIAN_POINT('Ctrl Pts',(0.0238413117000786,1.70742327901871,
12.8411788451136));
#24286=CARTESIAN_POINT('Ctrl Pts',(0.0165857265000572,1.70698264497427,
12.8408095862116));
#24287=CARTESIAN_POINT('Ctrl Pts',(0.00932467220683392,1.70674363352745,
12.8404403273095));
#24288=CARTESIAN_POINT('Ctrl Pts',(0.00207016844406672,1.70670544829274,
12.8400710684075));
#24289=CARTESIAN_POINT('Ctrl Pts',(-0.018439644367605,1.70659749163,12.8390271057592));
#24290=CARTESIAN_POINT('Ctrl Pts',(-0.0390190348449233,1.70809787389726,
12.8379831431109));
#24291=CARTESIAN_POINT('Ctrl Pts',(-0.05939504592475,1.71121070163957,12.8369391804626));
#24292=CARTESIAN_POINT('Ctrl Pts',(-0.0797335731368521,1.71431780299987,
12.8358971382961));
#24293=CARTESIAN_POINT('Ctrl Pts',(-0.0998687354948376,1.71903141084047,
12.8348550961295));
#24294=CARTESIAN_POINT('Ctrl Pts',(-0.119530827798182,1.72530376142016,
12.833813053963));
#24295=CARTESIAN_POINT('Ctrl Pts',(-0.139171803323475,1.73156937559392,
12.8327721309334));
#24296=CARTESIAN_POINT('Ctrl Pts',(-0.158340011223974,1.73939021415808,
12.8317312079038));
#24297=CARTESIAN_POINT('Ctrl Pts',(-0.176779228628762,1.74866825602371,
12.8306902848741));
#24298=CARTESIAN_POINT('Ctrl Pts',(-0.195227915935204,1.75795106284992,
12.8296488272536));
#24299=CARTESIAN_POINT('Ctrl Pts',(-0.21294620028672,1.76869225176188,12.828607369633));
#24300=CARTESIAN_POINT('Ctrl Pts',(-0.229700465195227,1.78074683041652,
12.8275659120124));
#24301=CARTESIAN_POINT('Ctrl Pts',(-0.246459849262177,1.79280509227054,
12.8265241361812));
#24302=CARTESIAN_POINT('Ctrl Pts',(-0.262254051887945,1.80617708403007,
12.8254823603499));
#24303=CARTESIAN_POINT('Ctrl Pts',(-0.276881561503866,1.82067672689305,
12.8244405845186));
#24304=CARTESIAN_POINT('Ctrl Pts',(-0.291540688813689,1.83520771106304,
12.8233965568652));
#24305=CARTESIAN_POINT('Ctrl Pts',(-0.305027607840395,1.85087065448245,
12.8223525292119));
#24306=CARTESIAN_POINT('Ctrl Pts',(-0.317179803406605,1.86744492628423,
12.8213085015585));
#24307=CARTESIAN_POINT('Ctrl Pts',(-0.321477875633597,1.87330702889159,
12.8209392426672));
#24308=CARTESIAN_POINT('Ctrl Pts',(-0.325609380499227,1.87928287195875,
12.820569983776));
#24309=CARTESIAN_POINT('Ctrl Pts',(-0.329568481179749,1.885361918074,12.8202007248847));
#24310=CARTESIAN_POINT('Ctrl Pts',(-0.340996590095234,1.90290933773148,
12.8191348437243));
#24311=CARTESIAN_POINT('Ctrl Pts',(-0.351050771947492,1.9214196059709,12.818068962564));
#24312=CARTESIAN_POINT('Ctrl Pts',(-0.359575330480823,1.94065612120446,
12.8170030814036));
#24313=CARTESIAN_POINT('Ctrl Pts',(-0.368081184057702,1.95985042684109,
12.815939539046));
#24314=CARTESIAN_POINT('Ctrl Pts',(-0.375063746194578,1.97976721269897,
12.8148759966883));
#24315=CARTESIAN_POINT('Ctrl Pts',(-0.380412644867909,2.00014455635969,
12.8138124543307));
#24316=CARTESIAN_POINT('Ctrl Pts',(-0.385752843557379,2.02048875627031,
12.8127506418247));
#24317=CARTESIAN_POINT('Ctrl Pts',(-0.389464444032076,2.0412913688329,12.8116888293188));
#24318=CARTESIAN_POINT('Ctrl Pts',(-0.391486464389773,2.06227417065729,
12.8106270168128));
#24319=CARTESIAN_POINT('Ctrl Pts',(-0.392699297074441,2.07485991331397,
12.8099901286097));
#24320=CARTESIAN_POINT('Ctrl Pts',(-0.393305224118923,2.08751018874901,
12.8093532404066));
#24321=CARTESIAN_POINT('Ctrl Pts',(-0.39329996604187,2.10016343642201,12.8087163522035));
#24322=CARTESIAN_POINT('',(-0.39342120080697,2.10027707468048,12.6837163522035));
#24323=CARTESIAN_POINT('Ctrl Pts',(-0.39329996604184,2.10016343649382,12.8087163521999));
#24324=CARTESIAN_POINT('Ctrl Pts',(-0.393290593258356,2.12271846896977,
12.8075810678464));
#24325=CARTESIAN_POINT('Ctrl Pts',(-0.391336792531897,2.14521105601326,
12.8064457834928));
#24326=CARTESIAN_POINT('Ctrl Pts',(-0.387495400099244,2.16732165254899,
12.8053104991393));
#24327=CARTESIAN_POINT('Ctrl Pts',(-0.38362857989576,2.1895786082999,12.8041676998675));
#24328=CARTESIAN_POINT('Ctrl Pts',(-0.377849299340276,2.21144802287218,
12.8030249005957));
#24329=CARTESIAN_POINT('Ctrl Pts',(-0.370265105169706,2.23262217723166,
12.8018821013238));
#24330=CARTESIAN_POINT('Ctrl Pts',(-0.366832438914899,2.24220576693271,
12.8013648613365));
#24331=CARTESIAN_POINT('Ctrl Pts',(-0.363030680309679,2.25164721999182,
12.8008476213493));
#24332=CARTESIAN_POINT('Ctrl Pts',(-0.358872916032692,2.26091960768717,
12.800330381362));
#24333=CARTESIAN_POINT('Ctrl Pts',(-0.350481162284677,2.27963437577207,
12.7992864187145));
#24334=CARTESIAN_POINT('Ctrl Pts',(-0.34059653621493,2.29774670930704,12.7982424560671));
#24335=CARTESIAN_POINT('Ctrl Pts',(-0.32932829007445,2.31500643561679,12.7971984934196));
#24336=CARTESIAN_POINT('Ctrl Pts',(-0.318080773087009,2.3322344108001,12.796156451254));
#24337=CARTESIAN_POINT('Ctrl Pts',(-0.305455036274669,2.34861225044094,
12.7951144090883));
#24338=CARTESIAN_POINT('Ctrl Pts',(-0.291606203295323,2.36391421371288,
12.7940723669227));
#24339=CARTESIAN_POINT('Ctrl Pts',(-0.27777224374508,2.37919974291661,12.7930314438939));
#24340=CARTESIAN_POINT('Ctrl Pts',(-0.262718265589452,2.39341112747198,
12.7919905208652));
#24341=CARTESIAN_POINT('Ctrl Pts',(-0.246639560738822,2.4063557035189,12.7909495978364));
#24342=CARTESIAN_POINT('Ctrl Pts',(-0.230552598284487,2.41930692756267,
12.7899081402168));
#24343=CARTESIAN_POINT('Ctrl Pts',(-0.213440420774801,2.43098956937945,
12.7888666825971));
#24344=CARTESIAN_POINT('Ctrl Pts',(-0.19553172014492,2.44125098742299,12.7878252249774));
#24345=CARTESIAN_POINT('Ctrl Pts',(-0.177617547626279,2.45151554077709,
12.786783449147));
#24346=CARTESIAN_POINT('Ctrl Pts',(-0.15890702334585,2.460357671781,12.7857416733166));
#24347=CARTESIAN_POINT('Ctrl Pts',(-0.139652950420971,2.46767097171074,
12.7846998974863));
#24348=CARTESIAN_POINT('Ctrl Pts',(-0.120357259380547,2.47500007950423,
12.7836558698338));
#24349=CARTESIAN_POINT('Ctrl Pts',(-0.10051638103565,2.48079355231629,12.7826118421813));
#24350=CARTESIAN_POINT('Ctrl Pts',(-0.0803984287066173,2.48499478264193,
12.7815678145288));
#24351=CARTESIAN_POINT('Ctrl Pts',(-0.0732829726542685,2.48648070274249,
12.7811985556322));
#24352=CARTESIAN_POINT('Ctrl Pts',(-0.0661329291528956,2.48776791378742,
12.7808292967356));
#24353=CARTESIAN_POINT('Ctrl Pts',(-0.0589603065575513,2.48885546447316,
12.7804600378391));
#24354=CARTESIAN_POINT('Ctrl Pts',(-0.0386819865373434,2.49193016979197,
12.7794160751914));
#24355=CARTESIAN_POINT('Ctrl Pts',(-0.018102085510851,2.49342353262573,
12.7783721125437));
#24356=CARTESIAN_POINT('Ctrl Pts',(0.00250990663971027,2.49329199123382,
12.7773281498961));
#24357=CARTESIAN_POINT('Ctrl Pts',(0.0230839808096885,2.49316069182646,
12.7762861077302));
#24358=CARTESIAN_POINT('Ctrl Pts',(0.0436893010881905,2.49141036678333,
12.7752440655643));
#24359=CARTESIAN_POINT('Ctrl Pts',(0.0640520893075922,2.48804924926526,
12.7742020233985));
#24360=CARTESIAN_POINT('Ctrl Pts',(0.0843930082123747,2.48469174153459,
12.7731611003695));
#24361=CARTESIAN_POINT('Ctrl Pts',(0.104491185179972,2.4797269664095,12.7721201773406));
#24362=CARTESIAN_POINT('Ctrl Pts',(0.124078909947421,2.47321483639622,12.7710792543116));
#24363=CARTESIAN_POINT('Ctrl Pts',(0.14367669445982,2.46669936192269,12.7700377966917));
#24364=CARTESIAN_POINT('Ctrl Pts',(0.162762799756044,2.45863516179295,12.7689963390718));
#24365=CARTESIAN_POINT('Ctrl Pts',(0.181085087014295,2.44913189665372,12.7679548814519));
#24366=CARTESIAN_POINT('Ctrl Pts',(0.199412972530104,2.43962572785268,12.7669131056213));
#24367=CARTESIAN_POINT('Ctrl Pts',(0.216975939463557,2.42867998931199,12.7658713297907));
#24368=CARTESIAN_POINT('Ctrl Pts',(0.233547670559036,2.41644964145413,12.7648295539601));
#24369=CARTESIAN_POINT('Ctrl Pts',(0.250155221827326,2.40419285742184,12.7637855263074));
#24370=CARTESIAN_POINT('Ctrl Pts',(0.265766703446861,2.39064640317974,12.7627414986547));
#24371=CARTESIAN_POINT('Ctrl Pts',(0.280189384229086,2.37600507054278,12.761697471002));
#24372=CARTESIAN_POINT('Ctrl Pts',(0.285290497363255,2.37082662311377,12.7613282121068));
#24373=CARTESIAN_POINT('Ctrl Pts',(0.290243255177885,2.36551152913714,12.7609589532116));
#24374=CARTESIAN_POINT('Ctrl Pts',(0.295040357460439,2.36006937049491,12.7605896943164));
#24375=CARTESIAN_POINT('Ctrl Pts',(0.308602645774295,2.34468338949881,12.7595457316689));
#24376=CARTESIAN_POINT('Ctrl Pts',(0.320998564262121,2.32818782453299,12.7585017690214));
#24377=CARTESIAN_POINT('Ctrl Pts',(0.332045605689831,2.31078568675807,12.7574578063738));
#24378=CARTESIAN_POINT('Ctrl Pts',(0.343072324894443,2.29341556209079,12.7564157642081));
#24379=CARTESIAN_POINT('Ctrl Pts',(0.3527546524404,2.27514275730554,12.7553737220423));
#24380=CARTESIAN_POINT('Ctrl Pts',(0.360951309847737,2.25620192674613,12.7543316798766));
#24381=CARTESIAN_POINT('Ctrl Pts',(0.369139164173787,2.23728143834118,12.7532907568478));
#24382=CARTESIAN_POINT('Ctrl Pts',(0.375844198701232,2.21769500882111,12.7522498338189));
#24383=CARTESIAN_POINT('Ctrl Pts',(0.380971872535446,2.19770016549032,12.7512089107901));
#24384=CARTESIAN_POINT('Ctrl Pts',(0.386102179809297,2.17769505332912,12.7501674531704));
#24385=CARTESIAN_POINT('Ctrl Pts',(0.389653309617672,2.15728181703275,12.7491259955506));
#24386=CARTESIAN_POINT('Ctrl Pts',(0.391580979295629,2.1367318207264,12.7480845379308));
#24387=CARTESIAN_POINT('Ctrl Pts',(0.393509237960712,2.11617554550027,12.7470427621003));
#24388=CARTESIAN_POINT('Ctrl Pts',(0.393813016364664,2.09548316240203,12.7460009862699));
#24389=CARTESIAN_POINT('Ctrl Pts',(0.392500098385387,2.07492884590887,12.7449592104394));
#24390=CARTESIAN_POINT('Ctrl Pts',(0.391184342504103,2.05433010079415,12.7439151827868));
#24391=CARTESIAN_POINT('Ctrl Pts',(0.388245018321332,2.03387074708653,12.7428711551342));
#24392=CARTESIAN_POINT('Ctrl Pts',(0.383741581407897,2.01381828094911,12.7418271274817));
#24393=CARTESIAN_POINT('Ctrl Pts',(0.382148774800765,2.00672598651557,12.7414578685856));
#24394=CARTESIAN_POINT('Ctrl Pts',(0.380360765913862,1.99968446264585,12.7410886096896));
#24395=CARTESIAN_POINT('Ctrl Pts',(0.378381659628227,1.9927050343353,12.7407193507936));
#24396=CARTESIAN_POINT('Ctrl Pts',(0.372786363049382,1.97297290997607,12.739675388146));
#24397=CARTESIAN_POINT('Ctrl Pts',(0.36562673134054,1.953620852398,12.7386314254985));
#24398=CARTESIAN_POINT('Ctrl Pts',(0.356974665456834,1.93491221056062,12.7375874628509));
#24399=CARTESIAN_POINT('Ctrl Pts',(0.348338515980635,1.91623798528587,12.7365454206852));
#24400=CARTESIAN_POINT('Ctrl Pts',(0.33821563340283,1.89820551153,12.7355033785194));
#24401=CARTESIAN_POINT('Ctrl Pts',(0.326726842703097,1.88106060140471,12.7344613363537));
#24402=CARTESIAN_POINT('Ctrl Pts',(0.315250390784098,1.86393410464357,12.7334204133248));
#24403=CARTESIAN_POINT('Ctrl Pts',(0.302411326502362,1.84769390335969,12.732379490296));
#24404=CARTESIAN_POINT('Ctrl Pts',(0.288375006731796,1.83255889341308,12.7313385672671));
#24405=CARTESIAN_POINT('Ctrl Pts',(0.274331478273237,1.81741611051983,12.7302971096474));
#24406=CARTESIAN_POINT('Ctrl Pts',(0.259089954438587,1.80338020334509,12.7292556520276));
#24407=CARTESIAN_POINT('Ctrl Pts',(0.242854632036266,1.7906352998506,12.7282141944078));
#24408=CARTESIAN_POINT('Ctrl Pts',(0.226614349035148,1.77788650223246,12.7271724185773));
#24409=CARTESIAN_POINT('Ctrl Pts',(0.209380263580363,1.76642991905275,12.7261306427468));
#24410=CARTESIAN_POINT('Ctrl Pts',(0.191387120035008,1.7564074210861,12.7250888669163));
#24411=CARTESIAN_POINT('Ctrl Pts',(0.173355083901566,1.74636325926265,12.7240448392638));
#24412=CARTESIAN_POINT('Ctrl Pts',(0.154561383701292,1.73775967782343,12.7230008116112));
#24413=CARTESIAN_POINT('Ctrl Pts',(0.135263119372274,1.73069148596643,12.7219567839586));
#24414=CARTESIAN_POINT('Ctrl Pts',(0.128437576234481,1.72819155915417,12.7215875250627));
#24415=CARTESIAN_POINT('Ctrl Pts',(0.121549055374674,1.72588324493719,12.7212182661667));
#24416=CARTESIAN_POINT('Ctrl Pts',(0.114609301097982,1.72376922228261,12.7208490072708));
#24417=CARTESIAN_POINT('Ctrl Pts',(0.0949893425059211,1.71779249237378,
12.7198050446232));
#24418=CARTESIAN_POINT('Ctrl Pts',(0.0748421479967187,1.71333682046681,
12.7187610819756));
#24419=CARTESIAN_POINT('Ctrl Pts',(0.054428067376843,1.71048430650149,12.7177171193281));
#24420=CARTESIAN_POINT('Ctrl Pts',(0.0340515406579967,1.70763704004299,
12.7166750771623));
#24421=CARTESIAN_POINT('Ctrl Pts',(0.0134098146149503,1.70638723708833,
12.7156330349965));
#24422=CARTESIAN_POINT('Ctrl Pts',(-0.00722502278297791,1.7067663683689,
12.7145909928307));
#24423=CARTESIAN_POINT('Ctrl Pts',(-0.0278376986897041,1.70714509246843,
12.7135500698018));
#24424=CARTESIAN_POINT('Ctrl Pts',(-0.0484427681833268,1.70914929319555,
12.712509146773));
#24425=CARTESIAN_POINT('Ctrl Pts',(-0.0687666690419001,1.71275842781426,
12.7114682237441));
#24426=CARTESIAN_POINT('Ctrl Pts',(-0.0891010077262566,1.71636941599046,
12.7104267661243));
#24427=CARTESIAN_POINT('Ctrl Pts',(-0.109153162032004,1.7215868719547,12.7093853085045));
#24428=CARTESIAN_POINT('Ctrl Pts',(-0.128657778450192,1.72833877516714,
12.7083438508847));
#24429=CARTESIAN_POINT('Ctrl Pts',(-0.14816835437902,1.73509274138037,12.7073020750542));
#24430=CARTESIAN_POINT('Ctrl Pts',(-0.167130376496693,1.74338181351447,
12.7062602992237));
#24431=CARTESIAN_POINT('Ctrl Pts',(-0.185297485950494,1.75308541151974,
12.7052185233931));
#24432=CARTESIAN_POINT('Ctrl Pts',(-0.203503864023646,1.76280998407231,
12.7041744957405));
#24433=CARTESIAN_POINT('Ctrl Pts',(-0.220911278838742,1.77395478960106,
12.7031304680879));
#24434=CARTESIAN_POINT('Ctrl Pts',(-0.237300840282622,1.78635497580679,
12.7020864404353));
#24435=CARTESIAN_POINT('Ctrl Pts',(-0.243097613333569,1.79074075912809,
12.7017171815395));
#24436=CARTESIAN_POINT('Ctrl Pts',(-0.248767366062678,1.79528321860555,
12.7013479226437));
#24437=CARTESIAN_POINT('Ctrl Pts',(-0.254301488541851,1.79997392959045,
12.700978663748));
#24438=CARTESIAN_POINT('Ctrl Pts',(-0.269725217596206,1.81304705104297,
12.699949530551));
#24439=CARTESIAN_POINT('Ctrl Pts',(-0.284190372762731,1.82735715623177,
12.698920397354));
#24440=CARTESIAN_POINT('Ctrl Pts',(-0.297489980694176,1.8427363193403,12.697891264157));
#24441=CARTESIAN_POINT('Ctrl Pts',(-0.310764998574633,1.8580870474448,12.6968640337558));
#24442=CARTESIAN_POINT('Ctrl Pts',(-0.322878205604673,1.87450238736961,
12.6958368033546));
#24443=CARTESIAN_POINT('Ctrl Pts',(-0.333658479324258,1.89177678041337,
12.6948095729534));
#24444=CARTESIAN_POINT('Ctrl Pts',(-0.344434541860459,1.90904442542467,
12.6937827438273));
#24445=CARTESIAN_POINT('Ctrl Pts',(-0.353878263301965,1.92716984179229,
12.6927559147013));
#24446=CARTESIAN_POINT('Ctrl Pts',(-0.361861105604863,1.94591745637345,
12.6917290855752));
#24447=CARTESIAN_POINT('Ctrl Pts',(-0.369841686340488,1.96465975968954,
12.6907025473534));
#24448=CARTESIAN_POINT('Ctrl Pts',(-0.376361921247464,1.98402320961346,
12.6896760091316));
#24449=CARTESIAN_POINT('Ctrl Pts',(-0.38134134509607,2.00375204666945,12.6886494709098));
#24450=CARTESIAN_POINT('Ctrl Pts',(-0.386329346774736,2.02351486970789,
12.6876211643167));
#24451=CARTESIAN_POINT('Ctrl Pts',(-0.389771084541329,2.04364359186479,
12.6865928577236));
#24452=CARTESIAN_POINT('Ctrl Pts',(-0.391637110626739,2.06387156826072,
12.6855645511305));
#24453=CARTESIAN_POINT('Ctrl Pts',(-0.392755061061598,2.07599030292631,
12.6849484848215));
#24454=CARTESIAN_POINT('Ctrl Pts',(-0.393308446986103,2.08814453182548,
12.6843324185125));
#24455=CARTESIAN_POINT('Ctrl Pts',(-0.393299902462425,2.10027698925372,
12.6837163522035));
#24456=CARTESIAN_POINT('',(-0.393370510321481,2.0996853138986,12.5587163522035));
#24457=CARTESIAN_POINT('Ctrl Pts',(-0.393690665213019,2.10027726445613,
12.6837163522035));
#24458=CARTESIAN_POINT('Ctrl Pts',(-0.393827751509988,2.11741474265097,
12.6828470082107));
#24459=CARTESIAN_POINT('Ctrl Pts',(-0.385020221980793,2.26497915337671,
12.6753542163767));
#24460=CARTESIAN_POINT('Ctrl Pts',(-0.198467542194671,2.52057776709468,
12.6612379767026));
#24461=CARTESIAN_POINT('Ctrl Pts',(0.246195250088315,2.49454140760323,12.6413676331794));
#24462=CARTESIAN_POINT('Ctrl Pts',(0.465007416872288,2.10656701859771,12.6214972896568));
#24463=CARTESIAN_POINT('Ctrl Pts',(0.257238583719243,1.71256828404793,12.6016269461339));
#24464=CARTESIAN_POINT('Ctrl Pts',(-0.18651163012543,1.67398540481866,12.5817566026112));
#24465=CARTESIAN_POINT('Ctrl Pts',(-0.382777726348084,1.9275339801708,12.5674530713011));
#24466=CARTESIAN_POINT('Ctrl Pts',(-0.39377123766665,2.07884159406489,12.5597729878318));
#24467=CARTESIAN_POINT('Ctrl Pts',(-0.393589312541075,2.09968513886256,
12.5587163522035));
#24468=CARTESIAN_POINT('',(-0.393063587406926,2.09989359760973,12.4337163554286));
#24469=CARTESIAN_POINT('Ctrl Pts',(-0.393299874152304,2.09968537040569,
12.5587163522035));
#24470=CARTESIAN_POINT('Ctrl Pts',(-0.393316073204164,2.11993484843599,
12.5576890687256));
#24471=CARTESIAN_POINT('Ctrl Pts',(-0.391764136452784,2.14024179843025,
12.5566617852476));
#24472=CARTESIAN_POINT('Ctrl Pts',(-0.388643851428118,2.16033942945636,
12.5556345017697));
#24473=CARTESIAN_POINT('Ctrl Pts',(-0.385527866712678,2.18040936236277,
12.5546086340715));
#24474=CARTESIAN_POINT('Ctrl Pts',(-0.380847892929046,2.20026979672838,
12.5535827663734));
#24475=CARTESIAN_POINT('Ctrl Pts',(-0.374655546270946,2.21965831207409,
12.5525568986753));
#24476=CARTESIAN_POINT('Ctrl Pts',(-0.368461716593899,2.23905147081868,
12.5515307852898));
#24477=CARTESIAN_POINT('Ctrl Pts',(-0.360754992450185,2.25797175237034,
12.5505046719044));
#24478=CARTESIAN_POINT('Ctrl Pts',(-0.351637115186527,2.27617102265497,
12.5494785585189));
#24479=CARTESIAN_POINT('Ctrl Pts',(-0.342518065902537,2.29437263229054,
12.5484523132359));
#24480=CARTESIAN_POINT('Ctrl Pts',(-0.331987870839673,2.31185238142415,
12.5474260679528));
#24481=CARTESIAN_POINT('Ctrl Pts',(-0.320194088805975,2.32838703004705,
12.5463998226698));
#24482=CARTESIAN_POINT('Ctrl Pts',(-0.308375411432332,2.34495658144305,
12.545371411099));
#24483=CARTESIAN_POINT('Ctrl Pts',(-0.295288311023228,2.3605764668794,12.5443429995283));
#24484=CARTESIAN_POINT('Ctrl Pts',(-0.281120681691834,2.37505645297851,
12.5433145879575));
#24485=CARTESIAN_POINT('Ctrl Pts',(-0.275157080608436,2.38115153485624,
12.5428816971602));
#24486=CARTESIAN_POINT('Ctrl Pts',(-0.269002461012857,2.38704511247016,
12.5424488063629));
#24487=CARTESIAN_POINT('Ctrl Pts',(-0.262672555761914,2.39272515855236,
12.5420159155656));
#24488=CARTESIAN_POINT('Ctrl Pts',(-0.247407309456433,2.40642319968154,
12.540971952918));
#24489=CARTESIAN_POINT('Ctrl Pts',(-0.231022191321355,2.41896474513736,
12.5399279902705));
#24490=CARTESIAN_POINT('Ctrl Pts',(-0.213718587953237,2.43016549662749,
12.5388840276229));
#24491=CARTESIAN_POINT('Ctrl Pts',(-0.196446816428079,2.4413456431283,12.5378419854572));
#24492=CARTESIAN_POINT('Ctrl Pts',(-0.178260491938778,2.45118944640849,
12.5367999432914));
#24493=CARTESIAN_POINT('Ctrl Pts',(-0.159393008216892,2.45955355502563,
12.5357579011256));
#24494=CARTESIAN_POINT('Ctrl Pts',(-0.140545787876112,2.46790868072152,
12.5347169780968));
#24495=CARTESIAN_POINT('Ctrl Pts',(-0.121019518127539,2.47478694351721,
12.5336760550679));
#24496=CARTESIAN_POINT('Ctrl Pts',(-0.101070878754924,2.48009152511955,
12.5326351320391));
#24497=CARTESIAN_POINT('Ctrl Pts',(-0.081111994281074,2.48539883101675,
12.5315936744193));
#24498=CARTESIAN_POINT('Ctrl Pts',(-0.0607310137548827,2.48913063645375,
12.5305522167995));
#24499=CARTESIAN_POINT('Ctrl Pts',(-0.040198898411932,2.49124025683264,
12.5295107591797));
#24500=CARTESIAN_POINT('Ctrl Pts',(-0.0196605096126161,2.49335052179252,
12.5284689833493));
#24501=CARTESIAN_POINT('Ctrl Pts',(0.0010283709272217,2.49383757582712,
12.5274272075188));
#24502=CARTESIAN_POINT('Ctrl Pts',(0.0215935105388922,2.4927067739454,12.5263854316883));
#24503=CARTESIAN_POINT('Ctrl Pts',(0.0422031021665188,2.49157352780976,
12.5253414040357));
#24504=CARTESIAN_POINT('Ctrl Pts',(0.0626876889855271,2.4888155423744,12.5242973763831));
#24505=CARTESIAN_POINT('Ctrl Pts',(0.0827792586853799,2.48448990146882,
12.5232533487305));
#24506=CARTESIAN_POINT('Ctrl Pts',(0.0898853835329845,2.48295997897992,
12.5228840898346));
#24507=CARTESIAN_POINT('Ctrl Pts',(0.0969424688577103,2.48123441215734,
12.5225148309388));
#24508=CARTESIAN_POINT('Ctrl Pts',(0.103939153748573,2.47931720540734,12.5221455720429));
#24509=CARTESIAN_POINT('Ctrl Pts',(0.123720065635645,2.47389691016998,12.5211016093953));
#24510=CARTESIAN_POINT('Ctrl Pts',(0.143134782110379,2.46690897464314,12.5200576467478));
#24511=CARTESIAN_POINT('Ctrl Pts',(0.161919327665279,2.4584229642872,12.5190136841002));
#24512=CARTESIAN_POINT('Ctrl Pts',(0.180669317024478,2.44995256486173,12.5179716419345));
#24513=CARTESIAN_POINT('Ctrl Pts',(0.198790749121794,2.439989806198,12.5169295997687));
#24514=CARTESIAN_POINT('Ctrl Pts',(0.216036751253761,2.42865333119827,12.5158875576029));
#24515=CARTESIAN_POINT('Ctrl Pts',(0.233264231450364,2.41732903139461,12.5148466345741));
#24516=CARTESIAN_POINT('Ctrl Pts',(0.24961752059224,2.40463432211781,12.5138057115452));
#24517=CARTESIAN_POINT('Ctrl Pts',(0.264876266720187,2.39073261483428,12.5127647885164));
#24518=CARTESIAN_POINT('Ctrl Pts',(0.280142849342448,2.37682376799621,12.5117233308966));
#24519=CARTESIAN_POINT('Ctrl Pts',(0.294313211189345,2.36170716837339,12.5106818732768));
#24520=CARTESIAN_POINT('Ctrl Pts',(0.307201422802289,2.34558537380766,12.509640415657));
#24521=CARTESIAN_POINT('Ctrl Pts',(0.320093572325771,2.32945865333083,12.5085986398265));
#24522=CARTESIAN_POINT('Ctrl Pts',(0.33170236093904,2.3123267233007,12.507556863996));
#24523=CARTESIAN_POINT('Ctrl Pts',(0.341883844130885,2.29442306221817,12.5065150881655));
#24524=CARTESIAN_POINT('Ctrl Pts',(0.35208733482969,2.27648070196593,12.5054710605129));
#24525=CARTESIAN_POINT('Ctrl Pts',(0.360857048273736,2.2577639472548,12.5044270328603));
#24526=CARTESIAN_POINT('Ctrl Pts',(0.368095901662538,2.23852904814241,12.5033830052077));
#24527=CARTESIAN_POINT('Ctrl Pts',(0.370656189221089,2.23172591645258,12.5030137463118));
#24528=CARTESIAN_POINT('Ctrl Pts',(0.37302542954117,2.22485811225872,12.5026444874159));
#24529=CARTESIAN_POINT('Ctrl Pts',(0.375200839732851,2.21793735567564,12.5022752285201));
#24530=CARTESIAN_POINT('Ctrl Pts',(0.381351123473112,2.19837110704542,12.5012312658725));
#24531=CARTESIAN_POINT('Ctrl Pts',(0.385985078996909,2.17826417006023,12.5001873032249));
#24532=CARTESIAN_POINT('Ctrl Pts',(0.389018303476915,2.15787615709377,12.4991433405774));
#24533=CARTESIAN_POINT('Ctrl Pts',(0.392045948013639,2.13752565007411,12.4981012984116));
#24534=CARTESIAN_POINT('Ctrl Pts',(0.393478540779884,2.11689580423328,12.4970592562458));
#24535=CARTESIAN_POINT('Ctrl Pts',(0.393282202197022,2.0962584181072,12.4960172140801));
#24536=CARTESIAN_POINT('Ctrl Pts',(0.393086074478714,2.07564319620961,12.4949762910512));
#24537=CARTESIAN_POINT('Ctrl Pts',(0.391264466525502,2.05502118239317,12.4939353680224));
#24538=CARTESIAN_POINT('Ctrl Pts',(0.387835497127093,2.03466611010983,12.4928944449935));
#24539=CARTESIAN_POINT('Ctrl Pts',(0.38440476669937,2.01430058399189,12.4918529873737));
#24540=CARTESIAN_POINT('Ctrl Pts',(0.379365131992984,1.99420300152393,12.4908115297539));
#24541=CARTESIAN_POINT('Ctrl Pts',(0.372786260292589,1.97463934374348,12.4897700721341));
#24542=CARTESIAN_POINT('Ctrl Pts',(0.366205378460076,1.95506970841268,12.4887282963036));
#24543=CARTESIAN_POINT('Ctrl Pts',(0.358084591987923,1.93603500781878,12.4876865204731));
#24544=CARTESIAN_POINT('Ctrl Pts',(0.348542294015158,1.91778265921529,12.4866447446426));
#24545=CARTESIAN_POINT('Ctrl Pts',(0.338979370148784,1.8994908577461,12.4856007169901));
#24546=CARTESIAN_POINT('Ctrl Pts',(0.327989192021601,1.88198540815059,12.4845566893375));
#24547=CARTESIAN_POINT('Ctrl Pts',(0.315734666595995,1.86548665217196,12.4835126616849));
#24548=CARTESIAN_POINT('Ctrl Pts',(0.311400401582283,1.85965125844398,12.483143402789));
#24549=CARTESIAN_POINT('Ctrl Pts',(0.306908341447079,1.8539414922597,12.4827741438931));
#24550=CARTESIAN_POINT('Ctrl Pts',(0.302266834244163,1.8483660378327,12.4824048849973));
#24551=CARTESIAN_POINT('Ctrl Pts',(0.289144441791431,1.83260320522365,12.4813609223497));
#24552=CARTESIAN_POINT('Ctrl Pts',(0.274746613027273,1.81782264415175,12.4803169597022));
#24553=CARTESIAN_POINT('Ctrl Pts',(0.259245945908198,1.8042358548942,12.4792729970546));
#24554=CARTESIAN_POINT('Ctrl Pts',(0.243773793936582,1.79067405999955,12.4782309548888));
#24555=CARTESIAN_POINT('Ctrl Pts',(0.227203338538617,1.7783022020407,12.4771889127231));
#24556=CARTESIAN_POINT('Ctrl Pts',(0.20974477316162,1.76729589703254,12.4761468705573));
#24557=CARTESIAN_POINT('Ctrl Pts',(0.192304958009566,1.75630141262306,12.4751059475284));
#24558=CARTESIAN_POINT('Ctrl Pts',(0.173979530268808,1.74666998450989,12.4740650244996));
#24559=CARTESIAN_POINT('Ctrl Pts',(0.155008457955053,1.73853455495387,12.4730241014707));
#24560=CARTESIAN_POINT('Ctrl Pts',(0.136027642593012,1.73039494725327,12.4719826438509));
#24561=CARTESIAN_POINT('Ctrl Pts',(0.11640119009215,1.72375317781577,12.4709411862312));
#24562=CARTESIAN_POINT('Ctrl Pts',(0.0963904542310355,1.71869464948268,
12.4698997286114));
#24563=CARTESIAN_POINT('Ctrl Pts',(0.0763736042177105,1.71363457554865,
12.4688579527809));
#24564=CARTESIAN_POINT('Ctrl Pts',(0.0559729587031034,1.71015885084542,
12.4678161769504));
#24565=CARTESIAN_POINT('Ctrl Pts',(0.0354606388891938,1.7083018597318,12.4667744011199));
#24566=CARTESIAN_POINT('Ctrl Pts',(0.0149039812305196,1.70644085468974,
12.4657303734673));
#24567=CARTESIAN_POINT('Ctrl Pts',(-0.00576409621383964,1.70620557706198,
12.4646863458147));
#24568=CARTESIAN_POINT('Ctrl Pts',(-0.0262701416788386,1.70757832672472,
12.4636423181621));
#24569=CARTESIAN_POINT('Ctrl Pts',(-0.0335228611716422,1.70806385028676,
12.4632730592662));
#24570=CARTESIAN_POINT('Ctrl Pts',(-0.0407553681268636,1.70875005527154,
12.4629038003703));
#24571=CARTESIAN_POINT('Ctrl Pts',(-0.0479558417498726,1.70963462340768,
12.4625345414745));
#24572=CARTESIAN_POINT('Ctrl Pts',(-0.0683129017726483,1.7121354598227,
12.4614905788269));
#24573=CARTESIAN_POINT('Ctrl Pts',(-0.0885344670210547,1.71624042725586,
12.4604466161794));
#24574=CARTESIAN_POINT('Ctrl Pts',(-0.108349273882756,1.72191889117667,
12.4594026535318));
#24575=CARTESIAN_POINT('Ctrl Pts',(-0.128127629272081,1.72758690895121,
12.458360611366));
#24576=CARTESIAN_POINT('Ctrl Pts',(-0.147499995870457,1.73482253427522,
12.4573185692003));
#24577=CARTESIAN_POINT('Ctrl Pts',(-0.166204931077286,1.74354409685686,
12.4562765270345));
#24578=CARTESIAN_POINT('Ctrl Pts',(-0.184889777477541,1.75225629261729,
12.4552356040056));
#24579=CARTESIAN_POINT('Ctrl Pts',(-0.202907939835433,1.76245097430072,
12.4541946809768));
#24580=CARTESIAN_POINT('Ctrl Pts',(-0.220017738894964,1.77399833655095,
12.4531537579479));
#24581=CARTESIAN_POINT('Ctrl Pts',(-0.237136325101362,1.78555162922548,
12.4521123003281));
#24582=CARTESIAN_POINT('Ctrl Pts',(-0.253344997127429,1.79845859208211,
12.4510708427083));
#24583=CARTESIAN_POINT('Ctrl Pts',(-0.268430471212415,1.81254570428557,
12.4500293850885));
#24584=CARTESIAN_POINT('Ctrl Pts',(-0.283520554567386,1.82663712071593,
12.448987609258));
#24585=CARTESIAN_POINT('Ctrl Pts',(-0.297486244161894,1.8419088761414,12.4479458334275));
#24586=CARTESIAN_POINT('Ctrl Pts',(-0.310151324887868,1.8581507790579,12.4469040575971));
#24587=CARTESIAN_POINT('Ctrl Pts',(-0.322843781473253,1.87442778921615,
12.4458600299445));
#24588=CARTESIAN_POINT('Ctrl Pts',(-0.334229610884264,1.8916785187495,12.4448160022919));
#24589=CARTESIAN_POINT('Ctrl Pts',(-0.344175671320527,1.90966346312107,
12.4437719746393));
#24590=CARTESIAN_POINT('Ctrl Pts',(-0.347693462526264,1.91602450220297,
12.4434027157434));
#24591=CARTESIAN_POINT('Ctrl Pts',(-0.351031575786892,1.92247717870157,
12.4430334568475));
#24592=CARTESIAN_POINT('Ctrl Pts',(-0.354185561536747,1.92901029855895,
12.4426641979517));
#24593=CARTESIAN_POINT('Ctrl Pts',(-0.363789505481296,1.94890376729011,
12.441539797901));
#24594=CARTESIAN_POINT('Ctrl Pts',(-0.371733180364064,1.96964892991815,
12.4404153978504));
#24595=CARTESIAN_POINT('Ctrl Pts',(-0.377883062466265,1.99096201991454,
12.4392909977998));
#24596=CARTESIAN_POINT('Ctrl Pts',(-0.384000616375438,2.01216307301722,
12.4381725084026));
#24597=CARTESIAN_POINT('Ctrl Pts',(-0.388342935182014,2.03392560141778,
12.4370540190054));
#24598=CARTESIAN_POINT('Ctrl Pts',(-0.390825227665587,2.05594853668558,
12.4359355296082));
#24599=CARTESIAN_POINT('Ctrl Pts',(-0.392466916440398,2.07051362353847,
12.4351958055425));
#24600=CARTESIAN_POINT('Ctrl Pts',(-0.393296004457353,2.08519217356933,
12.4344560814769));
#24601=CARTESIAN_POINT('Ctrl Pts',(-0.393299985579107,2.09989349425388,
12.4337163574112));
#24602=CARTESIAN_POINT('',(-0.393299835296684,2.10035993832925,12.3087163506447));
#24603=CARTESIAN_POINT('Ctrl Pts',(-0.392679023151022,2.09989376574539,
12.4337163522035));
#24604=CARTESIAN_POINT('Ctrl Pts',(-0.392504708819361,2.17213770239946,
12.430075519612));
#24605=CARTESIAN_POINT('Ctrl Pts',(-0.338763420378901,2.37604995535533,
12.4198112391793));
#24606=CARTESIAN_POINT('Ctrl Pts',(-0.0106856712490616,2.5649310055368,
12.4029235109061));
#24607=CARTESIAN_POINT('Ctrl Pts',(0.385137966833689,2.3606602577738,12.3830531673834));
#24608=CARTESIAN_POINT('Ctrl Pts',(0.427649952146105,1.91726920919309,12.3631828238606));
#24609=CARTESIAN_POINT('Ctrl Pts',(0.0778513256483007,1.64150878462692,
12.3433124803378));
#24610=CARTESIAN_POINT('Ctrl Pts',(-0.30701340218317,1.77385138595576,12.3251569897854));
#24611=CARTESIAN_POINT('Ctrl Pts',(-0.39232831653515,2.0032839961273,12.313624947074));
#24612=CARTESIAN_POINT('Ctrl Pts',(-0.393198689398899,2.10035981493551,
12.3087163522035));
#24613=CARTESIAN_POINT('',(-0.393299992424556,2.09992280645213,12.183716352199));
#24614=CARTESIAN_POINT('Ctrl Pts',(-0.393299835296684,2.10035993832925,
12.3087163506447));
#24615=CARTESIAN_POINT('Ctrl Pts',(-0.393275675193132,2.1267593628298,12.3073818069068));
#24616=CARTESIAN_POINT('Ctrl Pts',(-0.390589636175855,2.15303871333908,
12.306047263169));
#24617=CARTESIAN_POINT('Ctrl Pts',(-0.38533610283396,2.17874628786639,12.3047127194312));
#24618=CARTESIAN_POINT('Ctrl Pts',(-0.383838988541392,2.18607224827196,
12.3043324107182));
#24619=CARTESIAN_POINT('Ctrl Pts',(-0.382133660681373,2.19335192324089,
12.3039521020052));
#24620=CARTESIAN_POINT('Ctrl Pts',(-0.380222989607752,2.20057518667019,
12.3035717932922));
#24621=CARTESIAN_POINT('Ctrl Pts',(-0.374978120993316,2.22040333405629,
12.3025278306446));
#24622=CARTESIAN_POINT('Ctrl Pts',(-0.368162429928449,2.23987918613092,
12.3014838679971));
#24623=CARTESIAN_POINT('Ctrl Pts',(-0.359843140920602,2.25873816155038,
12.3004399053495));
#24624=CARTESIAN_POINT('Ctrl Pts',(-0.351539156141341,2.27756244385239,
12.2993978631838));
#24625=CARTESIAN_POINT('Ctrl Pts',(-0.341737303079051,2.29577141246672,
12.298355821018));
#24626=CARTESIAN_POINT('Ctrl Pts',(-0.330554033249778,2.313117153468,12.2973137788522));
#24627=CARTESIAN_POINT('Ctrl Pts',(-0.319382774076619,2.33044426541594,
12.2962728558234));
#24628=CARTESIAN_POINT('Ctrl Pts',(-0.306833415843539,2.34690935932156,
12.2952319327945));
#24629=CARTESIAN_POINT('Ctrl Pts',(-0.293067411788011,2.36229064441546,
12.2941910097657));
#24630=CARTESIAN_POINT('Ctrl Pts',(-0.27929433787158,2.3776798289365,12.2931495521459));
#24631=CARTESIAN_POINT('Ctrl Pts',(-0.264303848523121,2.39198353363584,
12.2921080945261));
#24632=CARTESIAN_POINT('Ctrl Pts',(-0.248296846725069,2.40501404214624,
12.2910666369062));
#24633=CARTESIAN_POINT('Ctrl Pts',(-0.232284954090124,2.41804853204507,
12.2900248610757));
#24634=CARTESIAN_POINT('Ctrl Pts',(-0.215256523671905,2.42980861525563,
12.2889830852452));
#24635=CARTESIAN_POINT('Ctrl Pts',(-0.197443749790202,2.44014828482411,
12.2879413094147));
#24636=CARTESIAN_POINT('Ctrl Pts',(-0.179592473193528,2.45051030382301,
12.2868972817621));
#24637=CARTESIAN_POINT('Ctrl Pts',(-0.160954132505601,2.45944546119213,
12.2858532541095));
#24638=CARTESIAN_POINT('Ctrl Pts',(-0.14178410779799,2.46685440814569,12.2848092264569));
#24639=CARTESIAN_POINT('Ctrl Pts',(-0.13500392133518,2.4694748555684,12.284439967561));
#24640=CARTESIAN_POINT('Ctrl Pts',(-0.128157372660572,2.47190483609913,
12.2840707086652));
#24641=CARTESIAN_POINT('Ctrl Pts',(-0.121256156779108,2.4741414631435,12.2837014497693));
#24642=CARTESIAN_POINT('Ctrl Pts',(-0.101745153296427,2.4804648181583,12.2826574871218));
#24643=CARTESIAN_POINT('Ctrl Pts',(-0.0816800514438771,2.48527669371452,
12.2816135244742));
#24644=CARTESIAN_POINT('Ctrl Pts',(-0.0613197057929595,2.4884903907196,
12.2805695618267));
#24645=CARTESIAN_POINT('Ctrl Pts',(-0.0409968151918136,2.49169817578274,
12.2795275196609));
#24646=CARTESIAN_POINT('Ctrl Pts',(-0.0203804681897151,2.49331344595796,
12.2784854774951));
#24647=CARTESIAN_POINT('Ctrl Pts',(0.000257847436364005,2.49329991547762,
12.2774434353294));
#24648=CARTESIAN_POINT('Ctrl Pts',(0.0208739978356784,2.4932863995288,12.2764025123005));
#24649=CARTESIAN_POINT('Ctrl Pts',(0.0415113379529104,2.4916475272744,12.2753615892717));
#24650=CARTESIAN_POINT('Ctrl Pts',(0.0618959845834157,2.48839899213624,
12.2743206662428));
#24651=CARTESIAN_POINT('Ctrl Pts',(0.0822911002371422,2.4851487886351,12.273279208623));
#24652=CARTESIAN_POINT('Ctrl Pts',(0.102432533992589,2.48028737060078,12.2722377510032));
#24653=CARTESIAN_POINT('Ctrl Pts',(0.122053698152773,2.47388204659656,12.2711962933835));
#24654=CARTESIAN_POINT('Ctrl Pts',(0.141680857434022,2.4674747654866,12.270154517553));
#24655=CARTESIAN_POINT('Ctrl Pts',(0.160786743024064,2.45952290184056,12.2691127417225));
#24656=CARTESIAN_POINT('Ctrl Pts',(0.179122898681202,2.45014265259754,12.268070965892));
#24657=CARTESIAN_POINT('Ctrl Pts',(0.197498688354888,2.44074212773292,12.2670269382394));
#24658=CARTESIAN_POINT('Ctrl Pts',(0.215100799237128,2.42990743930654,12.2659829105868));
#24659=CARTESIAN_POINT('Ctrl Pts',(0.231707455242898,2.41779953616212,12.2649388829342));
#24660=CARTESIAN_POINT('Ctrl Pts',(0.237581011796238,2.41351712952731,12.2645696240383));
#24661=CARTESIAN_POINT('Ctrl Pts',(0.243330343440933,2.40907582118649,12.2642003651425));
#24662=CARTESIAN_POINT('Ctrl Pts',(0.24894669235926,2.4044838819435,12.2638311062466));
#24663=CARTESIAN_POINT('Ctrl Pts',(0.264825141198124,2.39150162720805,12.262787143599));
#24664=CARTESIAN_POINT('Ctrl Pts',(0.279732654505629,2.37723528550078,12.2617431809515));
#24665=CARTESIAN_POINT('Ctrl Pts',(0.29345621147571,2.36185557459471,12.2606992183039));
#24666=CARTESIAN_POINT('Ctrl Pts',(0.307154522483946,2.3465041563241,12.2596571761382));
#24667=CARTESIAN_POINT('Ctrl Pts',(0.319672671713673,2.33004393757367,12.2586151339724));
#24668=CARTESIAN_POINT('Ctrl Pts',(0.330833188202641,2.31268354798544,12.2575730918066));
#24669=CARTESIAN_POINT('Ctrl Pts',(0.341981718472226,2.29534180318291,12.2565321687778));
#24670=CARTESIAN_POINT('Ctrl Pts',(0.351775090436263,2.27710240694963,12.2554912457489));
#24671=CARTESIAN_POINT('Ctrl Pts',(0.360078241477362,2.25820414032057,12.2544503227201));
#24672=CARTESIAN_POINT('Ctrl Pts',(0.368385656800428,2.23929616803432,12.2534088651003));
#24673=CARTESIAN_POINT('Ctrl Pts',(0.375201011500912,2.21972931649054,12.2523674074805));
#24674=CARTESIAN_POINT('Ctrl Pts',(0.380436591086625,2.19976417273945,12.2513259498607));
#24675=CARTESIAN_POINT('Ctrl Pts',(0.385673770370154,2.17979292876655,12.2502841740302));
#24676=CARTESIAN_POINT('Ctrl Pts',(0.389330062134675,2.15942387061067,12.2492423981997));
#24677=CARTESIAN_POINT('Ctrl Pts',(0.391368672994078,2.13892880423099,12.2482006223692));
#24678=CARTESIAN_POINT('Ctrl Pts',(0.393411690357115,2.11838943730023,12.2471565947166));
#24679=CARTESIAN_POINT('Ctrl Pts',(0.393830031010305,2.09772425469989,12.246112567064));
#24680=CARTESIAN_POINT('Ctrl Pts',(0.392638972221088,2.07720685425029,12.2450685394114));
#24681=CARTESIAN_POINT('Ctrl Pts',(0.392217710339444,2.06995011864823,12.2446992805155));
#24682=CARTESIAN_POINT('Ctrl Pts',(0.39159559587069,2.06271181720889,12.2443300216196));
#24683=CARTESIAN_POINT('Ctrl Pts',(0.390774842289819,2.05550379079779,12.2439607627238));
#24684=CARTESIAN_POINT('Ctrl Pts',(0.388454421330812,2.03512537765745,12.2429168000762));
#24685=CARTESIAN_POINT('Ctrl Pts',(0.384528732108304,2.01486824501606,12.2418728374286));
#24686=CARTESIAN_POINT('Ctrl Pts',(0.379026005171062,1.99500391719656,12.2408288747811));
#24687=CARTESIAN_POINT('Ctrl Pts',(0.373533401092972,1.97517613194859,12.2397868326153));
#24688=CARTESIAN_POINT('Ctrl Pts',(0.366469654824172,1.95574043411958,12.2387447904496));
#24689=CARTESIAN_POINT('Ctrl Pts',(0.357914117664509,1.93695897946702,12.2377027482838));
#24690=CARTESIAN_POINT('Ctrl Pts',(0.349367769017353,1.91819769580171,12.2366618252549));
#24691=CARTESIAN_POINT('Ctrl Pts',(0.339333087298376,1.90008993856399,12.2356209022261));
#24692=CARTESIAN_POINT('Ctrl Pts',(0.327937732041783,1.8828785273095,12.2345799791972));
#24693=CARTESIAN_POINT('Ctrl Pts',(0.316536524427733,1.86565827672278,12.2335385215774));
#24694=CARTESIAN_POINT('Ctrl Pts',(0.303773639962304,1.84933591417466,12.2324970639576));
#24695=CARTESIAN_POINT('Ctrl Pts',(0.289820703463437,1.83412625205944,12.2314556063378));
#24696=CARTESIAN_POINT('Ctrl Pts',(0.27586350373417,1.81891194272936,12.2304138305073));
#24697=CARTESIAN_POINT('Ctrl Pts',(0.260716051738381,1.80481152792479,12.2293720546768));
#24698=CARTESIAN_POINT('Ctrl Pts',(0.244586969868335,1.79200307766046,12.2283302788464));
#24699=CARTESIAN_POINT('Ctrl Pts',(0.22842302462181,1.77916694164022,12.2272862511938));
#24700=CARTESIAN_POINT('Ctrl Pts',(0.211273824448557,1.76762875659117,12.2262422235412));
#24701=CARTESIAN_POINT('Ctrl Pts',(0.19337768515542,1.75752378055706,12.2251981958886));
#24702=CARTESIAN_POINT('Ctrl Pts',(0.187048055265674,1.75394978298735,12.2248289369927));
#24703=CARTESIAN_POINT('Ctrl Pts',(0.180625200015419,1.7505546446144,12.2244596780968));
#24704=CARTESIAN_POINT('Ctrl Pts',(0.174120273610395,1.74734291398323,12.224090419201));
#24705=CARTESIAN_POINT('Ctrl Pts',(0.155729653186621,1.73826276222385,12.2230464565534));
#24706=CARTESIAN_POINT('Ctrl Pts',(0.136572046861426,1.73059800008724,12.2220024939059));
#24707=CARTESIAN_POINT('Ctrl Pts',(0.11689103885316,1.72447187184469,12.2209585312583));
#24708=CARTESIAN_POINT('Ctrl Pts',(0.0972462361798775,1.71835701327518,
12.2199164890925));
#24709=CARTESIAN_POINT('Ctrl Pts',(0.0770806199719689,1.71377544319439,
12.2188744469268));
#24710=CARTESIAN_POINT('Ctrl Pts',(0.0566575697764722,1.71080235125707,
12.217832404761));
#24711=CARTESIAN_POINT('Ctrl Pts',(0.0362564536160493,1.70783245237379,
12.2167914817321));
#24712=CARTESIAN_POINT('Ctrl Pts',(0.0155991725926806,1.70646773624871,
12.2157505587033));
#24713=CARTESIAN_POINT('Ctrl Pts',(-0.00504100185119109,1.70673230707273,
12.2147096356744));
#24714=CARTESIAN_POINT('Ctrl Pts',(-0.0256917765507166,1.70699701377344,
12.2136681780547));
#24715=CARTESIAN_POINT('Ctrl Pts',(-0.0463246911948396,1.70889268576987,
12.2126267204349));
#24716=CARTESIAN_POINT('Ctrl Pts',(-0.0666662240613439,1.71239129967272,
12.2115852628151));
#24717=CARTESIAN_POINT('Ctrl Pts',(-0.0870139721529581,1.71589098255464,
12.2105434869846));
#24718=CARTESIAN_POINT('Ctrl Pts',(-0.107069442842288,1.72099442208645,
12.2095017111541));
#24719=CARTESIAN_POINT('Ctrl Pts',(-0.126569980602219,1.72762259734195,
12.2084599353236));
#24720=CARTESIAN_POINT('Ctrl Pts',(-0.146112669217038,1.73426509954868,
12.207415907671));
#24721=CARTESIAN_POINT('Ctrl Pts',(-0.165097353710535,1.74243862605138,
12.2063718800184));
#24722=CARTESIAN_POINT('Ctrl Pts',(-0.183281302045478,1.75201601427578,
12.2053278523658));
#24723=CARTESIAN_POINT('Ctrl Pts',(-0.189712726220865,1.75540341095272,
12.2049585934699));
#24724=CARTESIAN_POINT('Ctrl Pts',(-0.196044226953382,1.75896601289691,
12.2045893345741));
#24725=CARTESIAN_POINT('Ctrl Pts',(-0.202265941771804,1.76269690366206,
12.2042200756782));
#24726=CARTESIAN_POINT('Ctrl Pts',(-0.219855871078453,1.77324481637183,
12.2031761130306));
#24727=CARTESIAN_POINT('Ctrl Pts',(-0.23667089877559,1.7852038005372,12.2021321503831));
#24728=CARTESIAN_POINT('Ctrl Pts',(-0.25247554233462,1.7984357605371,12.2010881877355));
#24729=CARTESIAN_POINT('Ctrl Pts',(-0.268251111548774,1.81164337892074,
12.2000461455698));
#24730=CARTESIAN_POINT('Ctrl Pts',(-0.283019390125813,1.82611890341287,
12.199004103404));
#24731=CARTESIAN_POINT('Ctrl Pts',(-0.296574585150023,1.84168158129337,
12.1979620612382));
#24732=CARTESIAN_POINT('Ctrl Pts',(-0.310115222107724,1.85722754510232,
12.1969211382094));
#24733=CARTESIAN_POINT('Ctrl Pts',(-0.322444859331438,1.87385781134533,
12.1958802151805));
#24734=CARTESIAN_POINT('Ctrl Pts',(-0.333395302816379,1.89135565653492,
12.1948392921517));
#24735=CARTESIAN_POINT('Ctrl Pts',(-0.344351370163691,1.90886248816175,
12.1937978345319));
#24736=CARTESIAN_POINT('Ctrl Pts',(-0.35392642471822,1.92723717371848,12.1927563769121));
#24737=CARTESIAN_POINT('Ctrl Pts',(-0.361995966796987,1.94623456167684,
12.1917149192923));
#24738=CARTESIAN_POINT('Ctrl Pts',(-0.37006797447266,1.96523775416543,12.1906731434618));
#24739=CARTESIAN_POINT('Ctrl Pts',(-0.376633299803859,1.98486333703376,
12.1896313676313));
#24740=CARTESIAN_POINT('Ctrl Pts',(-0.381616204817429,2.00484768935679,
12.1885895918008));
#24741=CARTESIAN_POINT('Ctrl Pts',(-0.386609880493262,2.02487523831087,
12.1875455641482));
#24742=CARTESIAN_POINT('Ctrl Pts',(-0.390014185815633,2.04526237852428,
12.1865015364956));
#24743=CARTESIAN_POINT('Ctrl Pts',(-0.391804646116096,2.06573618115503,
12.185457508843));
#24744=CARTESIAN_POINT('Ctrl Pts',(-0.392437908455446,2.07297749677984,
12.1850882499471));
#24745=CARTESIAN_POINT('Ctrl Pts',(-0.392869764704041,2.08022963676174,
12.1847189910513));
#24746=CARTESIAN_POINT('Ctrl Pts',(-0.39310069159986,2.08748056456099,12.1843497321554));
#24747=CARTESIAN_POINT('Ctrl Pts',(-0.393232725851723,2.09162633902301,
12.1841386055047));
#24748=CARTESIAN_POINT('Ctrl Pts',(-0.393299178173347,2.0957742132399,12.1839274788541));
#24749=CARTESIAN_POINT('Ctrl Pts',(-0.393299992424539,2.09992280636392,
12.1837163522035));
#24750=CARTESIAN_POINT('',(-0.393299871729038,2.09968235566726,12.0587163522076));
#24751=CARTESIAN_POINT('Ctrl Pts',(-0.393299992424556,2.09992280645214,
12.183716352199));
#24752=CARTESIAN_POINT('Ctrl Pts',(-0.393303997505547,2.12032863526799,
12.1826778762235));
#24753=CARTESIAN_POINT('Ctrl Pts',(-0.391715603864827,2.14079812773611,
12.1816394002479));
#24754=CARTESIAN_POINT('Ctrl Pts',(-0.388531187097256,2.1610606800879,12.1806009242724));
#24755=CARTESIAN_POINT('Ctrl Pts',(-0.385352552134374,2.18128644261952,
12.1795643338118));
#24756=CARTESIAN_POINT('Ctrl Pts',(-0.380583699187246,2.2013052743376,12.1785277433511));
#24757=CARTESIAN_POINT('Ctrl Pts',(-0.374272869640994,2.22084994435537,
12.1774911528905));
#24758=CARTESIAN_POINT('Ctrl Pts',(-0.367671498009194,2.24129442463527,
12.1764068392023));
#24759=CARTESIAN_POINT('Ctrl Pts',(-0.359382669624518,2.26121911750468,
12.1753225255142));
#24760=CARTESIAN_POINT('Ctrl Pts',(-0.349520709452778,2.28033347904265,
12.174238211826));
#24761=CARTESIAN_POINT('Ctrl Pts',(-0.340097295564756,2.29859785416087,
12.173202115909));
#24762=CARTESIAN_POINT('Ctrl Pts',(-0.329238279185668,2.31612184059859,
12.1721660199919));
#24763=CARTESIAN_POINT('Ctrl Pts',(-0.317090954891824,2.33267620489812,
12.1711299240749));
#24764=CARTESIAN_POINT('Ctrl Pts',(-0.304938571797175,2.34923746332753,
12.1700933966717));
#24765=CARTESIAN_POINT('Ctrl Pts',(-0.291497287948853,2.36482772302869,
12.1690568692684));
#24766=CARTESIAN_POINT('Ctrl Pts',(-0.276954855100894,2.37925060113819,
12.1680203418652));
#24767=CARTESIAN_POINT('Ctrl Pts',(-0.262382049761107,2.39370360204435,
12.1669816496302));
#24768=CARTESIAN_POINT('Ctrl Pts',(-0.246704081486891,2.40698388492101,
12.1659429573952));
#24769=CARTESIAN_POINT('Ctrl Pts',(-0.230142255229364,2.41893484030119,
12.1649042651603));
#24770=CARTESIAN_POINT('Ctrl Pts',(-0.227884053041853,2.42056435103042,
12.164762639651));
#24771=CARTESIAN_POINT('Ctrl Pts',(-0.225609459681919,2.42216921581425,
12.1646210141418));
#24772=CARTESIAN_POINT('Ctrl Pts',(-0.223319072711738,2.4237491031079,12.1644793886326));
#24773=CARTESIAN_POINT('Ctrl Pts',(-0.206435966987021,2.43539490993406,
12.1634354259851));
#24774=CARTESIAN_POINT('Ctrl Pts',(-0.18858913326125,2.44575121162367,12.1623914633375));
#24775=CARTESIAN_POINT('Ctrl Pts',(-0.17000175783156,2.45466081307945,12.16134750069));
#24776=CARTESIAN_POINT('Ctrl Pts',(-0.151448575881872,2.4635540243633,12.1603054585242));
#24777=CARTESIAN_POINT('Ctrl Pts',(-0.132158186645935,2.47100545003735,
12.1592634163584));
#24778=CARTESIAN_POINT('Ctrl Pts',(-0.112380317171347,2.4769025793391,12.1582213741927));
#24779=CARTESIAN_POINT('Ctrl Pts',(-0.0926236888178818,2.48279337521662,
12.1571804511638));
#24780=CARTESIAN_POINT('Ctrl Pts',(-0.0723813128532868,2.48713295177294,
12.156139528135));
#24781=CARTESIAN_POINT('Ctrl Pts',(-0.0519200964590137,2.48985791460952,
12.1550986051061));
#24782=CARTESIAN_POINT('Ctrl Pts',(-0.0314483717172843,2.492584276916,12.1540571474863));
#24783=CARTESIAN_POINT('Ctrl Pts',(-0.0107583092250953,2.49369425578895,
12.1530156898665));
#24784=CARTESIAN_POINT('Ctrl Pts',(0.00987539303740517,2.49317599953756,
12.1519742322468));
#24785=CARTESIAN_POINT('Ctrl Pts',(0.0305153997955036,2.49265758493628,
12.1509324564163));
#24786=CARTESIAN_POINT('Ctrl Pts',(0.0510982780238676,2.49050999944065,
12.1498906805858));
#24787=CARTESIAN_POINT('Ctrl Pts',(0.0713527019384991,2.48677342453441,
12.1488489047553));
#24788=CARTESIAN_POINT('Ctrl Pts',(0.0916509062500565,2.48302877293671,
12.1478048771027));
#24789=CARTESIAN_POINT('Ctrl Pts',(0.111618527372682,2.47768846512622,12.1467608494501));
#24790=CARTESIAN_POINT('Ctrl Pts',(0.130996986946167,2.47084320057273,12.1457168217975));
#24791=CARTESIAN_POINT('Ctrl Pts',(0.13785089408932,2.46842212022617,12.1453475629016));
#24792=CARTESIAN_POINT('Ctrl Pts',(0.144631282693188,2.46581321920853,12.1449783040057));
#24793=CARTESIAN_POINT('Ctrl Pts',(0.151327393242926,2.46302191401388,12.1446090451099));
#24794=CARTESIAN_POINT('Ctrl Pts',(0.170258526320522,2.45513038210031,12.1435650824623));
#24795=CARTESIAN_POINT('Ctrl Pts',(0.188627103771938,2.44573049799819,12.1425211198148));
#24796=CARTESIAN_POINT('Ctrl Pts',(0.206180138369548,2.43492482819569,12.1414771571672));
#24797=CARTESIAN_POINT('Ctrl Pts',(0.223700882268574,2.42413903658717,12.1404351150014));
#24798=CARTESIAN_POINT('Ctrl Pts',(0.240408410637133,2.41195292329113,12.1393930728357));
#24799=CARTESIAN_POINT('Ctrl Pts',(0.256072940648541,2.39851555917173,12.1383510306699));
#24800=CARTESIAN_POINT('Ctrl Pts',(0.271720647200798,2.38509262657029,12.1373101076411));
#24801=CARTESIAN_POINT('Ctrl Pts',(0.286327004732961,2.37042156563308,12.1362691846122));
#24802=CARTESIAN_POINT('Ctrl Pts',(0.29969422841969,2.35469248016368,12.1352282615833));
#24803=CARTESIAN_POINT('Ctrl Pts',(0.313068317164112,2.33895531664594,12.1341868039635));
#24804=CARTESIAN_POINT('Ctrl Pts',(0.325201511946711,2.32215959327964,12.1331453463438));
#24805=CARTESIAN_POINT('Ctrl Pts',(0.335935148673514,2.3045298655104,12.132103888724));
#24806=CARTESIAN_POINT('Ctrl Pts',(0.346672064994279,2.28689475109076,12.1310621128935));
#24807=CARTESIAN_POINT('Ctrl Pts',(0.356008220552377,2.26842577171939,12.130020337063));
#24808=CARTESIAN_POINT('Ctrl Pts',(0.363830527109338,2.24937281393661,12.1289785612325));
#24809=CARTESIAN_POINT('Ctrl Pts',(0.371669741759436,2.2302786727532,12.1279345335799));
#24810=CARTESIAN_POINT('Ctrl Pts',(0.377988349443145,2.21059873429428,12.1268905059273));
#24811=CARTESIAN_POINT('Ctrl Pts',(0.38272263875999,2.19059951313661,12.1258464782747));
#24812=CARTESIAN_POINT('Ctrl Pts',(0.384397094835468,2.18352605075797,12.1254772193788));
#24813=CARTESIAN_POINT('Ctrl Pts',(0.385873831014179,2.17641273336051,12.1251079604829));
#24814=CARTESIAN_POINT('Ctrl Pts',(0.387151577261523,2.16927153978305,12.1247387015871));
#24815=CARTESIAN_POINT('Ctrl Pts',(0.390764000334346,2.14908207532537,12.1236947389395));
#24816=CARTESIAN_POINT('Ctrl Pts',(0.392803652355737,2.12854911941653,12.122650776292));
#24817=CARTESIAN_POINT('Ctrl Pts',(0.393219826507829,2.10794090934042,12.1216068136444));
#24818=CARTESIAN_POINT('Ctrl Pts',(0.393635235062723,2.0873706102874,12.1205647714786));
#24819=CARTESIAN_POINT('Ctrl Pts',(0.39243301981034,2.06672605798086,12.1195227293129));
#24820=CARTESIAN_POINT('Ctrl Pts',(0.389614136606284,2.0462811526879,12.1184806871471));
#24821=CARTESIAN_POINT('Ctrl Pts',(0.386798280838503,2.02585820490205,12.1174397641182));
#24822=CARTESIAN_POINT('Ctrl Pts',(0.382369275378471,2.00563520759659,12.1163988410894));
#24823=CARTESIAN_POINT('Ctrl Pts',(0.376379898408236,1.98588136841775,12.1153579180605));
#24824=CARTESIAN_POINT('Ctrl Pts',(0.370387445450093,1.96611738418195,12.1143164604407));
#24825=CARTESIAN_POINT('Ctrl Pts',(0.362833218095359,1.94682374823372,12.1132750028209));
#24826=CARTESIAN_POINT('Ctrl Pts',(0.353820138842289,1.92825542410421,12.1122335452011));
#24827=CARTESIAN_POINT('Ctrl Pts',(0.344804305700569,1.90968142654217,12.1111917693707));
#24828=CARTESIAN_POINT('Ctrl Pts',(0.334329086866636,1.8918338275438,12.1101499935402));
#24829=CARTESIAN_POINT('Ctrl Pts',(0.322543374710771,1.87494298182419,12.1091082177097));
#24830=CARTESIAN_POINT('Ctrl Pts',(0.310732187470628,1.85801562615826,12.1080641900571));
#24831=CARTESIAN_POINT('Ctrl Pts',(0.297605319366354,1.84204972140527,12.1070201624045));
#24832=CARTESIAN_POINT('Ctrl Pts',(0.28335237249362,1.82724310640749,12.1059761347519));
#24833=CARTESIAN_POINT('Ctrl Pts',(0.278311292008886,1.82200620076427,12.105606875856));
#24834=CARTESIAN_POINT('Ctrl Pts',(0.273129671358055,1.81691396730848,12.1052376169601));
#24835=CARTESIAN_POINT('Ctrl Pts',(0.267816895070616,1.81197395826986,12.1048683580643));
#24836=CARTESIAN_POINT('Ctrl Pts',(0.25279670175634,1.79800764636061,12.1038243954167));
#24837=CARTESIAN_POINT('Ctrl Pts',(0.236636325291627,1.78517781038189,12.1027804327692));
#24838=CARTESIAN_POINT('Ctrl Pts',(0.219533855870652,1.77367228722255,12.1017364701216));
#24839=CARTESIAN_POINT('Ctrl Pts',(0.202462848285074,1.76218792971285,12.1006944279558));
#24840=CARTESIAN_POINT('Ctrl Pts',(0.184453758238992,1.75202350463506,12.0996523857901));
#24841=CARTESIAN_POINT('Ctrl Pts',(0.165737403402908,1.74332647545232,12.0986103436243));
#24842=CARTESIAN_POINT('Ctrl Pts',(0.147041149637887,1.7346387867423,12.0975694205954));
#24843=CARTESIAN_POINT('Ctrl Pts',(0.1276397907406,1.7274156999839,12.0965284975666));
#24844=CARTESIAN_POINT('Ctrl Pts',(0.107788251103555,1.72175856529984,12.0954875745377));
#24845=CARTESIAN_POINT('Ctrl Pts',(0.0879265162331535,1.71609852525885,
12.0944461169179));
#24846=CARTESIAN_POINT('Ctrl Pts',(0.0676148419238802,1.71200626111984,
12.0934046592982));
#24847=CARTESIAN_POINT('Ctrl Pts',(0.0471233198857042,1.70953325016981,
12.0923632016784));
#24848=CARTESIAN_POINT('Ctrl Pts',(0.0266255367941799,1.70705948360713,
12.0913214258479));
#24849=CARTESIAN_POINT('Ctrl Pts',(0.00594853077608295,1.70620600733156,
12.0902796500174));
#24850=CARTESIAN_POINT('Ctrl Pts',(-0.0146334136694206,1.70697232514188,
12.0892378741869));
#24851=CARTESIAN_POINT('Ctrl Pts',(-0.0352598464549025,1.70774029936554,
12.0881938465343));
#24852=CARTESIAN_POINT('Ctrl Pts',(-0.0557900759231901,1.7101349723677,
12.0871498188817));
#24853=CARTESIAN_POINT('Ctrl Pts',(-0.0759551205932514,1.71410401705166,
12.0861057912291));
#24854=CARTESIAN_POINT('Ctrl Pts',(-0.0830872325746495,1.71550781613113,
12.0857365323332));
#24855=CARTESIAN_POINT('Ctrl Pts',(-0.0901737785218994,1.71710809756765,
12.0853672734373));
#24856=CARTESIAN_POINT('Ctrl Pts',(-0.0972033283696397,1.71890105883922,
12.0849980145415));
#24857=CARTESIAN_POINT('Ctrl Pts',(-0.117077155519838,1.72397008931346,
12.0839540518939));
#24858=CARTESIAN_POINT('Ctrl Pts',(-0.136612615100873,1.73061300115087,
12.0829100892464));
#24859=CARTESIAN_POINT('Ctrl Pts',(-0.15554454069214,1.73876491607144,12.0818661265988));
#24860=CARTESIAN_POINT('Ctrl Pts',(-0.174441638966242,1.7469018346661,12.080824084433));
#24861=CARTESIAN_POINT('Ctrl Pts',(-0.192736715404961,1.75654201306439,
12.0797820422673));
#24862=CARTESIAN_POINT('Ctrl Pts',(-0.210180834312592,1.76757120027341,
12.0787400001015));
#24863=CARTESIAN_POINT('Ctrl Pts',(-0.227606218510548,1.77858854230862,
12.0776990770726));
#24864=CARTESIAN_POINT('Ctrl Pts',(-0.24418182531333,1.7909915648636,12.0766581540438));
#24865=CARTESIAN_POINT('Ctrl Pts',(-0.259684442543274,1.80462078559758,
12.0756172310149));
#24866=CARTESIAN_POINT('Ctrl Pts',(-0.275195021513392,1.81825700594412,
12.0745757733951));
#24867=CARTESIAN_POINT('Ctrl Pts',(-0.289630946783222,1.8331202088504,12.0735343157754));
#24868=CARTESIAN_POINT('Ctrl Pts',(-0.302802729805314,1.84901116195645,
12.0724928581556));
#24869=CARTESIAN_POINT('Ctrl Pts',(-0.315978537381359,1.86490697044146,
12.0714510823251));
#24870=CARTESIAN_POINT('Ctrl Pts',(-0.327888992482206,1.88183056518122,
12.0704093064946));
#24871=CARTESIAN_POINT('Ctrl Pts',(-0.338386037167328,1.89955105425522,
12.0693675306641));
#24872=CARTESIAN_POINT('Ctrl Pts',(-0.34890577145275,1.9173098465685,12.0683235030115));
#24873=CARTESIAN_POINT('Ctrl Pts',(-0.358005671686283,1.93586831085162,
12.0672794753589));
#24874=CARTESIAN_POINT('Ctrl Pts',(-0.365584130891856,1.95497195705642,
12.0662354477063));
#24875=CARTESIAN_POINT('Ctrl Pts',(-0.368264532576321,1.96172866631324,
12.0658661888104));
#24876=CARTESIAN_POINT('Ctrl Pts',(-0.370755062659463,1.96855342228281,
12.0654969299145));
#24877=CARTESIAN_POINT('Ctrl Pts',(-0.373052731068955,1.97543455598765,
12.0651276710187));
#24878=CARTESIAN_POINT('Ctrl Pts',(-0.380724672436183,1.99841074093475,
12.0638947112988));
#24879=CARTESIAN_POINT('Ctrl Pts',(-0.386280054004908,2.02212718864926,
12.062661751579));
#24880=CARTESIAN_POINT('Ctrl Pts',(-0.38960581650926,2.04622084286498,12.0614287918592));
#24881=CARTESIAN_POINT('Ctrl Pts',(-0.392044644516216,2.06388905537695,
12.0605246453087));
#24882=CARTESIAN_POINT('Ctrl Pts',(-0.393285396653957,2.08175965223396,
12.0596204987581));
#24883=CARTESIAN_POINT('Ctrl Pts',(-0.393299871729038,2.09968235566726,
12.0587163522076));
#24884=CARTESIAN_POINT('',(-0.393117616260674,2.10022922555168,11.9337163003311));
#24885=CARTESIAN_POINT('Ctrl Pts',(-0.393299871729104,2.09968235574893,
12.0587163522035));
#24886=CARTESIAN_POINT('Ctrl Pts',(-0.393316492993478,2.12026242645436,
12.0576781494565));
#24887=CARTESIAN_POINT('Ctrl Pts',(-0.391713458209966,2.14086461331921,
12.0566399467095));
#24888=CARTESIAN_POINT('Ctrl Pts',(-0.388506753042148,2.16121595250135,
12.0556017439626));
#24889=CARTESIAN_POINT('Ctrl Pts',(-0.385298042103967,2.18158002129561,
12.0545628918274));
#24890=CARTESIAN_POINT('Ctrl Pts',(-0.380483759796851,2.20169219674375,
12.0535240396923));
#24891=CARTESIAN_POINT('Ctrl Pts',(-0.374131492706927,2.22128691670946,
12.0524851875572));
#24892=CARTESIAN_POINT('Ctrl Pts',(-0.367776788637376,2.24088915398083,
12.0514459368775));
#24893=CARTESIAN_POINT('Ctrl Pts',(-0.359883191796895,2.2599728509145,12.0504066861978));
#24894=CARTESIAN_POINT('Ctrl Pts',(-0.350567110264477,2.27829074906123,
12.0493674355182));
#24895=CARTESIAN_POINT('Ctrl Pts',(-0.341230137865095,2.29664972421785,
12.0483258543686));
#24896=CARTESIAN_POINT('Ctrl Pts',(-0.330464703739848,2.31423884457759,
12.047284273219));
#24897=CARTESIAN_POINT('Ctrl Pts',(-0.318431833598604,2.33083772947902,
12.0462426920694));
#24898=CARTESIAN_POINT('Ctrl Pts',(-0.314637357620361,2.33607206420422,
12.0459142372116));
#24899=CARTESIAN_POINT('Ctrl Pts',(-0.310717146896181,2.34120817816899,
12.0455857823537));
#24900=CARTESIAN_POINT('Ctrl Pts',(-0.306677039555868,2.34623988996352,
12.0452573274959));
#24901=CARTESIAN_POINT('Ctrl Pts',(-0.293835941137391,2.36223270919443,
12.0442133648483));
#24902=CARTESIAN_POINT('Ctrl Pts',(-0.279702205837368,2.37726600508028,
12.0431694022008));
#24903=CARTESIAN_POINT('Ctrl Pts',(-0.264444657850618,2.39112525299992,
12.0421254395532));
#24904=CARTESIAN_POINT('Ctrl Pts',(-0.249215177767485,2.4049590053396,12.0410833973875));
#24905=CARTESIAN_POINT('Ctrl Pts',(-0.232866487148554,2.41762246365465,
12.0400413552217));
#24906=CARTESIAN_POINT('Ctrl Pts',(-0.215605635461306,2.42893631595998,
12.0389993130559));
#24907=CARTESIAN_POINT('Ctrl Pts',(-0.198363321657604,2.44023801736568,
12.0379583900271));
#24908=CARTESIAN_POINT('Ctrl Pts',(-0.180211388011673,2.45019256478358,
12.0369174669982));
#24909=CARTESIAN_POINT('Ctrl Pts',(-0.161387409842751,2.45866278583685,
12.0358765439693));
#24910=CARTESIAN_POINT('Ctrl Pts',(-0.14255376416926,2.46713735697488,12.0348350863495));
#24911=CARTESIAN_POINT('Ctrl Pts',(-0.123048048815827,2.47412576219931,
12.0337936287298));
#24912=CARTESIAN_POINT('Ctrl Pts',(-0.103130063658391,2.47953798224923,
12.03275217111));
#24913=CARTESIAN_POINT('Ctrl Pts',(-0.083205992688135,2.48495185596832,
12.0317103952795));
#24914=CARTESIAN_POINT('Ctrl Pts',(-0.062870120066094,2.48878842791809,
12.030668619449));
#24915=CARTESIAN_POINT('Ctrl Pts',(-0.042393915182467,2.49100849857196,
12.0296268436185));
#24916=CARTESIAN_POINT('Ctrl Pts',(-0.0218734505173167,2.49323336795894,
12.0285828159659));
#24917=CARTESIAN_POINT('Ctrl Pts',(-0.00121278417029519,2.49383473881415,
12.0275387883133));
#24918=CARTESIAN_POINT('Ctrl Pts',(0.0193143614497235,2.49282546435,12.0264947606607));
#24919=CARTESIAN_POINT('Ctrl Pts',(0.0265745437907052,2.49246849720135,
12.0261255017648));
#24920=CARTESIAN_POINT('Ctrl Pts',(0.0338180717901917,2.4919105220603,12.0257562428689));
#24921=CARTESIAN_POINT('Ctrl Pts',(0.0410330854408241,2.49115364743181,
12.0253869839731));
#24922=CARTESIAN_POINT('Ctrl Pts',(0.0614312527895902,2.48901382399119,
12.0243430213255));
#24923=CARTESIAN_POINT('Ctrl Pts',(0.0817223634306081,2.48526772099253,
12.023299058678));
#24924=CARTESIAN_POINT('Ctrl Pts',(0.101634653634368,2.4799411627879,12.0222550960304));
#24925=CARTESIAN_POINT('Ctrl Pts',(0.121510313034625,2.47462440336105,12.0212130538647));
#24926=CARTESIAN_POINT('Ctrl Pts',(0.141007817151458,2.46773309037553,12.0201710116989));
#24927=CARTESIAN_POINT('Ctrl Pts',(0.159864317639446,2.45934424991319,12.0191289695331));
#24928=CARTESIAN_POINT('Ctrl Pts',(0.178700566542123,2.45096441893373,12.0180880465043));
#24929=CARTESIAN_POINT('Ctrl Pts',(0.196896497908281,2.44109052450962,12.0170471234754));
#24930=CARTESIAN_POINT('Ctrl Pts',(0.214208170934481,2.42984807033679,12.0160062004466));
#24931=CARTESIAN_POINT('Ctrl Pts',(0.23152873478477,2.4185998423325,12.0149647428268));
#24932=CARTESIAN_POINT('Ctrl Pts',(0.247963507187296,2.40598203764596,12.013923285207));
#24933=CARTESIAN_POINT('Ctrl Pts',(0.263296163968612,2.39216437161196,12.0128818275872));
#24934=CARTESIAN_POINT('Ctrl Pts',(0.278633505545024,2.37834248367859,12.0118400517567));
#24935=CARTESIAN_POINT('Ctrl Pts',(0.292867539228064,2.36332052359557,12.0107982759262));
#24936=CARTESIAN_POINT('Ctrl Pts',(0.305818354067898,2.34730552827465,12.0097565000958));
#24937=CARTESIAN_POINT('Ctrl Pts',(0.318797162387892,2.33125591617792,12.0087124724432));
#24938=CARTESIAN_POINT('Ctrl Pts',(0.330486797778318,2.31420959090686,12.0076684447906));
#24939=CARTESIAN_POINT('Ctrl Pts',(0.340749896564524,2.29640366083978,12.006624417138));
#24940=CARTESIAN_POINT('Ctrl Pts',(0.344379820079021,2.29010593677082,12.0062551582421));
#24941=CARTESIAN_POINT('Ctrl Pts',(0.347831717178603,2.2837134067121,12.0058858993462));
#24942=CARTESIAN_POINT('Ctrl Pts',(0.351100940695715,2.277237184142,12.0055166404504));
#24943=CARTESIAN_POINT('Ctrl Pts',(0.360343635391998,2.25892771472598,12.0044726778028));
#24944=CARTESIAN_POINT('Ctrl Pts',(0.368177789746147,2.23983875235823,12.0034287151553));
#24945=CARTESIAN_POINT('Ctrl Pts',(0.374478006718493,2.22021278003667,12.0023847525077));
#24946=CARTESIAN_POINT('Ctrl Pts',(0.380766633762833,2.200622911806,12.001342710342));
#24947=CARTESIAN_POINT('Ctrl Pts',(0.385526645695877,2.18049866901658,12.0003006681762));
#24948=CARTESIAN_POINT('Ctrl Pts',(0.388680522867616,2.16010275487327,11.9992586260104));
#24949=CARTESIAN_POINT('Ctrl Pts',(0.391831012824818,2.13972874562135,11.9982177029816));
#24950=CARTESIAN_POINT('Ctrl Pts',(0.393378652035149,2.11908436328001,11.9971767799527));
#24951=CARTESIAN_POINT('Ctrl Pts',(0.393296916688583,2.09844265506273,11.9961358569238));
#24952=CARTESIAN_POINT('Ctrl Pts',(0.393215139364874,2.07779034580209,11.9950943993041));
#24953=CARTESIAN_POINT('Ctrl Pts',(0.391502302529403,2.05714144924551,11.9940529416843));
#24954=CARTESIAN_POINT('Ctrl Pts',(0.38818400569048,2.03676972460843,11.9930114840645));
#24955=CARTESIAN_POINT('Ctrl Pts',(0.384864694967206,2.01639177552135,11.991969708234));
#24956=CARTESIAN_POINT('Ctrl Pts',(0.379939101595768,1.99629188672652,11.9909279324035));
#24957=CARTESIAN_POINT('Ctrl Pts',(0.373483916870504,1.97673340339303,11.989886156573));
#24958=CARTESIAN_POINT('Ctrl Pts',(0.367014779116969,1.95713264395397,11.9888421289204));
#24959=CARTESIAN_POINT('Ctrl Pts',(0.359009734480259,1.93807630534519,11.9877981012678));
#24960=CARTESIAN_POINT('Ctrl Pts',(0.349593790491062,1.91980823645324,11.9867540736152));
#24961=CARTESIAN_POINT('Ctrl Pts',(0.346263494523937,1.91334705993946,11.9863848147193));
#24962=CARTESIAN_POINT('Ctrl Pts',(0.34275711506805,1.90698425102751,11.9860155558234));
#24963=CARTESIAN_POINT('Ctrl Pts',(0.339081480939228,1.90072973306572,11.9856462969276));
#24964=CARTESIAN_POINT('Ctrl Pts',(0.328689788878464,1.88304706325432,11.98460233428));
#24965=CARTESIAN_POINT('Ctrl Pts',(0.316880216849635,1.86612676576232,11.9835583716324));
#24966=CARTESIAN_POINT('Ctrl Pts',(0.303788769215543,1.85020553709398,11.9825144089849));
#24967=CARTESIAN_POINT('Ctrl Pts',(0.290721404710059,1.8343135972414,11.9814723668191));
#24968=CARTESIAN_POINT('Ctrl Pts',(0.276377261527864,1.81941767773911,11.9804303246534));
#24969=CARTESIAN_POINT('Ctrl Pts',(0.260935262439899,1.80572516448833,11.9793882824876));
#24970=CARTESIAN_POINT('Ctrl Pts',(0.245509847816362,1.79204735678167,11.9783473594587));
#24971=CARTESIAN_POINT('Ctrl Pts',(0.228989446587432,1.77957089684241,11.9773064364299));
#24972=CARTESIAN_POINT('Ctrl Pts',(0.211589283921301,1.76846589175521,11.976265513401));
#24973=CARTESIAN_POINT('Ctrl Pts',(0.194180184985127,1.75735518342682,11.9752240557812));
#24974=CARTESIAN_POINT('Ctrl Pts',(0.175891033526532,1.7476177464974,11.9741825981614));
#24975=CARTESIAN_POINT('Ctrl Pts',(0.156965868671762,1.73938024725187,11.9731411405417));
#24976=CARTESIAN_POINT('Ctrl Pts',(0.138034921354045,1.7311402310912,11.9720993647112));
#24977=CARTESIAN_POINT('Ctrl Pts',(0.118468262287423,1.72440132520103,11.9710575888807));
#24978=CARTESIAN_POINT('Ctrl Pts',(0.098528831188428,1.71924159966635,11.9700158130502));
#24979=CARTESIAN_POINT('Ctrl Pts',(0.0785463005566409,1.71407072126784,
11.9689717853976));
#24980=CARTESIAN_POINT('Ctrl Pts',(0.0581901145585439,1.71048596570866,
11.967927757745));
#24981=CARTESIAN_POINT('Ctrl Pts',(0.0377329745389964,1.70851422422719,
11.9668837300924));
#24982=CARTESIAN_POINT('Ctrl Pts',(0.0304975522612305,1.70781684511029,
11.9665144711965));
#24983=CARTESIAN_POINT('Ctrl Pts',(0.0232495220501961,1.70732076830367,
11.9661452123006));
#24984=CARTESIAN_POINT('Ctrl Pts',(0.0160009241962401,1.70702562370446,
11.9657759534048));
#24985=CARTESIAN_POINT('Ctrl Pts',(-0.00449219185696926,1.70619119577152,
11.9647319907572));
#24986=CARTESIAN_POINT('Ctrl Pts',(-0.0251118156604017,1.70696163261368,
11.9636880281097));
#24987=CARTESIAN_POINT('Ctrl Pts',(-0.0455853069363327,1.70935070742222,
11.9626440654621));
#24988=CARTESIAN_POINT('Ctrl Pts',(-0.0660211350189228,1.71173538727021,
11.9616020232963));
#24989=CARTESIAN_POINT('Ctrl Pts',(-0.0863106347254772,1.71573276930209,
11.9605599811306));
#24990=CARTESIAN_POINT('Ctrl Pts',(-0.106182578148309,1.72130467378408,
11.9595179389648));
#24991=CARTESIAN_POINT('Ctrl Pts',(-0.126033179416082,1.7268705941282,11.9584770159359));
#24992=CARTESIAN_POINT('Ctrl Pts',(-0.145466402006288,1.73400751006866,
11.9574360929071));
#24993=CARTESIAN_POINT('Ctrl Pts',(-0.164222711564067,1.74262653846915,
11.9563951698782));
#24994=CARTESIAN_POINT('Ctrl Pts',(-0.182988653873587,1.75124999337798,
11.9553537122584));
#24995=CARTESIAN_POINT('Ctrl Pts',(-0.201076313335196,1.76135678882616,
11.9543122546386));
#24996=CARTESIAN_POINT('Ctrl Pts',(-0.218247083880113,1.77281029909573,
11.9532707970188));
#24997=CARTESIAN_POINT('Ctrl Pts',(-0.235423100844017,1.78426730891201,
11.9522290211883));
#24998=CARTESIAN_POINT('Ctrl Pts',(-0.251681079672283,1.79707141466158,
11.9511872453578));
#24999=CARTESIAN_POINT('Ctrl Pts',(-0.266813043620092,1.81104379267061,
11.9501454695273));
#25000=CARTESIAN_POINT('Ctrl Pts',(-0.281977715651357,1.82504637229179,
11.9491014418747));
#25001=CARTESIAN_POINT('Ctrl Pts',(-0.296011013602061,1.84022172498738,
11.9480574142221));
#25002=CARTESIAN_POINT('Ctrl Pts',(-0.308742708672144,1.85635511529731,
11.9470133865695));
#25003=CARTESIAN_POINT('Ctrl Pts',(-0.313245742334435,1.86206128397733,
11.9466441276737));
#25004=CARTESIAN_POINT('Ctrl Pts',(-0.317586342312149,1.86788702221123,
11.9462748687778));
#25005=CARTESIAN_POINT('Ctrl Pts',(-0.321758302167676,1.87382200596394,
11.945905609882));
#25006=CARTESIAN_POINT('Ctrl Pts',(-0.333683180404073,1.890786205294,11.9448501425421));
#25007=CARTESIAN_POINT('Ctrl Pts',(-0.34429731941234,1.90874491298018,11.9437946752022));
#25008=CARTESIAN_POINT('Ctrl Pts',(-0.35343870890053,1.92747183113843,11.9427392078623));
#25009=CARTESIAN_POINT('Ctrl Pts',(-0.362561452952742,1.94616055252648,
11.9416858933295));
#25010=CARTESIAN_POINT('Ctrl Pts',(-0.370217046306243,1.96561376671549,
11.9406325787968));
#25011=CARTESIAN_POINT('Ctrl Pts',(-0.376287829472357,1.98557815160127,
11.9395792642641));
#25012=CARTESIAN_POINT('Ctrl Pts',(-0.382352060450643,2.00552098895421,
11.9385270865723));
#25013=CARTESIAN_POINT('Ctrl Pts',(-0.386834628806233,2.02597323466799,
11.9374749088804));
#25014=CARTESIAN_POINT('Ctrl Pts',(-0.389666644633754,2.0466633703739,11.9364227311886));
#25015=CARTESIAN_POINT('Ctrl Pts',(-0.392094785869053,2.06440287987213,
11.9355206048602));
#25016=CARTESIAN_POINT('Ctrl Pts',(-0.393310331065654,2.08231670296114,
11.9346184785319));
#25017=CARTESIAN_POINT('Ctrl Pts',(-0.393299933737381,2.10022830280689,
11.9337163522035));
#25018=CARTESIAN_POINT('',(-0.393476660747021,2.10021501587443,11.8087164144524));
#25019=CARTESIAN_POINT('Ctrl Pts',(-0.392787134589716,2.10023089818476,
11.9337162063036));
#25020=CARTESIAN_POINT('Ctrl Pts',(-0.393054107309642,2.15099946965231,
11.9311558929888));
#25021=CARTESIAN_POINT('Ctrl Pts',(-0.360302360717907,2.33277278484366,
11.9219721318331));
#25022=CARTESIAN_POINT('Ctrl Pts',(-0.0859611737152024,2.55704015151082,
11.9061649228363));
#25023=CARTESIAN_POINT('Ctrl Pts',(0.337755205860749,2.41968178614589,11.8862945793136));
#25024=CARTESIAN_POINT('Ctrl Pts',(0.4516271652787,1.98905890273745,11.8664242357908));
#25025=CARTESIAN_POINT('Ctrl Pts',(0.15119268404004,1.66020937280082,11.846553892268));
#25026=CARTESIAN_POINT('Ctrl Pts',(-0.273919395647392,1.7324260119291,11.8273179899681));
#25027=CARTESIAN_POINT('Ctrl Pts',(-0.393020217355167,1.98223813255993,
11.8147055355092));
#25028=CARTESIAN_POINT('Ctrl Pts',(-0.393801543951838,2.10021294015016,
11.8087165288911));
#25029=CARTESIAN_POINT('',(-0.393301967689671,2.09965328553757,11.6837163511551));
#25030=CARTESIAN_POINT('Ctrl Pts',(-0.393299940606853,2.10021614496415,
11.8087163522035));
#25031=CARTESIAN_POINT('Ctrl Pts',(-0.393293081754006,2.11269659496315,
11.8080819698765));
#25032=CARTESIAN_POINT('Ctrl Pts',(-0.392692218482795,2.12516040435568,
11.8074475875494));
#25033=CARTESIAN_POINT('Ctrl Pts',(-0.391501762296877,2.1375667421856,11.8068132052223));
#25034=CARTESIAN_POINT('Ctrl Pts',(-0.389542704267171,2.15798306328373,
11.8057692425746));
#25035=CARTESIAN_POINT('Ctrl Pts',(-0.385976481415077,2.17830655986508,
11.804725279927));
#25036=CARTESIAN_POINT('Ctrl Pts',(-0.380826509869729,2.19826525011641,
11.8036813172794));
#25037=CARTESIAN_POINT('Ctrl Pts',(-0.37568601225198,2.21818722420636,11.8026392751136));
#25038=CARTESIAN_POINT('Ctrl Pts',(-0.368967673248511,2.23774500481882,
11.8015972329478));
#25039=CARTESIAN_POINT('Ctrl Pts',(-0.360746187679668,2.25667507164379,
11.8005551907821));
#25040=CARTESIAN_POINT('Ctrl Pts',(-0.352533531857171,2.27558480787437,
11.7995142677532));
#25041=CARTESIAN_POINT('Ctrl Pts',(-0.342821199442785,2.2938674856994,11.7984733447244));
#25042=CARTESIAN_POINT('Ctrl Pts',(-0.331732528447031,2.31127806220746,
11.7974324216956));
#25043=CARTESIAN_POINT('Ctrl Pts',(-0.320638162598855,2.32869758033385,
11.7963909640758));
#25044=CARTESIAN_POINT('Ctrl Pts',(-0.308166427695835,2.34524347310334,
11.7953495064561));
#25045=CARTESIAN_POINT('Ctrl Pts',(-0.294485116273548,2.36069792153632,
11.7943080488364));
#25046=CARTESIAN_POINT('Ctrl Pts',(-0.280799624614169,2.37615709197704,
11.7932662730059));
#25047=CARTESIAN_POINT('Ctrl Pts',(-0.265904335080789,2.3905236277231,11.7922244971755));
#25048=CARTESIAN_POINT('Ctrl Pts',(-0.250004682860337,2.40361579100551,
11.7911827213451));
#25049=CARTESIAN_POINT('Ctrl Pts',(-0.234070663180799,2.41673625329596,
11.7901386936925));
#25050=CARTESIAN_POINT('Ctrl Pts',(-0.217128550282337,2.42857642184816,
11.78909466604));
#25051=CARTESIAN_POINT('Ctrl Pts',(-0.19941422651103,2.43899683813423,11.7880506383874));
#25052=CARTESIAN_POINT('Ctrl Pts',(-0.193148902388196,2.44268240278632,
11.7876813794916));
#25053=CARTESIAN_POINT('Ctrl Pts',(-0.186787199084921,2.44619078777344,
11.7873121205957));
#25054=CARTESIAN_POINT('Ctrl Pts',(-0.180340188480231,2.44951724767015,
11.7869428616999));
#25055=CARTESIAN_POINT('Ctrl Pts',(-0.162113306649872,2.45892176011297,
11.7858988990524));
#25056=CARTESIAN_POINT('Ctrl Pts',(-0.143094485977205,2.46692469200966,
11.7848549364048));
#25057=CARTESIAN_POINT('Ctrl Pts',(-0.123525089214268,2.47339850339096,
11.7838109737573));
#25058=CARTESIAN_POINT('Ctrl Pts',(-0.103991692465394,2.47986040549863,
11.7827689315915));
#25059=CARTESIAN_POINT('Ctrl Pts',(-0.0839104020611678,2.48479848580899,
11.7817268894257));
#25060=CARTESIAN_POINT('Ctrl Pts',(-0.0635432242523246,2.48813290075903,
11.78068484726));
#25061=CARTESIAN_POINT('Ctrl Pts',(-0.0431979204724972,2.4914637345998,
11.7796439242311));
#25062=CARTESIAN_POINT('Ctrl Pts',(-0.0225680565905233,2.49319417546617,
11.7786030012022));
#25063=CARTESIAN_POINT('Ctrl Pts',(-0.00192643416733575,2.49329528201009,
11.7775620781733));
#25064=CARTESIAN_POINT('Ctrl Pts',(0.0187257892551426,2.4933964404797,11.7765206205535));
#25065=CARTESIAN_POINT('Ctrl Pts',(0.0393890475926803,2.49186657319596,
11.7754791629337));
#25066=CARTESIAN_POINT('Ctrl Pts',(0.059789365615982,2.48872885377759,11.7744377053139));
#25067=CARTESIAN_POINT('Ctrl Pts',(0.0801959168258219,2.48559017564915,
11.7733959294833));
#25068=CARTESIAN_POINT('Ctrl Pts',(0.100338646670289,2.48084281490468,11.7723541536528));
#25069=CARTESIAN_POINT('Ctrl Pts',(0.11995354100067,2.47456112718941,11.7713123778223));
#25070=CARTESIAN_POINT('Ctrl Pts',(0.139610833370268,2.46826586146359,11.7702683501696));
#25071=CARTESIAN_POINT('Ctrl Pts',(0.158737330916367,2.46042992677606,11.769224322517));
#25072=CARTESIAN_POINT('Ctrl Pts',(0.177088087035754,2.45117616580574,11.7681802948644));
#25073=CARTESIAN_POINT('Ctrl Pts',(0.183578508937987,2.44790323184655,11.7678110359685));
#25074=CARTESIAN_POINT('Ctrl Pts',(0.189972126797455,2.44445334999276,11.7674417770726));
#25075=CARTESIAN_POINT('Ctrl Pts',(0.196258957167312,2.44083326089394,11.7670725181768));
#25076=CARTESIAN_POINT('Ctrl Pts',(0.214032980084853,2.43059860482395,11.7660285555292));
#25077=CARTESIAN_POINT('Ctrl Pts',(0.231057219789549,2.41893937152159,11.7649845928816));
#25078=CARTESIAN_POINT('Ctrl Pts',(0.247093784372878,2.40598946342038,11.7639406302341));
#25079=CARTESIAN_POINT('Ctrl Pts',(0.263100847967622,2.39306337807054,11.7628985880683));
#25080=CARTESIAN_POINT('Ctrl Pts',(0.278123239647553,2.37885174165299,11.7618565459025));
#25081=CARTESIAN_POINT('Ctrl Pts',(0.291951996797666,2.36353163295107,11.7608145037368));
#25082=CARTESIAN_POINT('Ctrl Pts',(0.305765902079843,2.34822797780522,11.7597735807079));
#25083=CARTESIAN_POINT('Ctrl Pts',(0.318388205820068,2.33181873779631,11.7587326576791));
#25084=CARTESIAN_POINT('Ctrl Pts',(0.329646901200572,2.31451762288647,11.7576917346502));
#25085=CARTESIAN_POINT('Ctrl Pts',(0.340911378753586,2.29720762257493,11.7566502770305));
#25086=CARTESIAN_POINT('Ctrl Pts',(0.350810434049579,2.27900544019819,11.7556088194107));
#25087=CARTESIAN_POINT('Ctrl Pts',(0.359215244140055,2.26015398333292,11.7545673617909));
#25088=CARTESIAN_POINT('Ctrl Pts',(0.367622622266434,2.24129676652572,11.7535255859604));
#25089=CARTESIAN_POINT('Ctrl Pts',(0.374534579974763,2.22179056647898,11.75248381013));
#25090=CARTESIAN_POINT('Ctrl Pts',(0.379870721193706,2.20189762107024,11.7514420342995));
#25091=CARTESIAN_POINT('Ctrl Pts',(0.385218396602986,2.18196167660856,11.7503980066469));
#25092=CARTESIAN_POINT('Ctrl Pts',(0.388983321135715,2.16163804199095,11.7493539789943));
#25093=CARTESIAN_POINT('Ctrl Pts',(0.391136189093529,2.14119916966871,11.7483099513417));
#25094=CARTESIAN_POINT('Ctrl Pts',(0.391897630270952,2.13397020843597,11.7479406924459));
#25095=CARTESIAN_POINT('Ctrl Pts',(0.392457888712955,2.126726856683,11.74757143355));
#25096=CARTESIAN_POINT('Ctrl Pts',(0.392817227858228,2.11948115750609,11.7472021746541));
#25097=CARTESIAN_POINT('Ctrl Pts',(0.393833145550843,2.09899623654488,11.7461582120066));
#25098=CARTESIAN_POINT('Ctrl Pts',(0.393245381999473,2.07837059733709,11.745114249359));
#25099=CARTESIAN_POINT('Ctrl Pts',(0.391037749579127,2.05787674746542,11.7440702867115));
#25100=CARTESIAN_POINT('Ctrl Pts',(0.388834178336504,2.03742059823893,11.7430282445457));
#25101=CARTESIAN_POINT('Ctrl Pts',(0.385016672039765,2.01709648676696,11.7419862023799));
#25102=CARTESIAN_POINT('Ctrl Pts',(0.379621006461212,1.99717596850261,11.7409441602142));
#25103=CARTESIAN_POINT('Ctrl Pts',(0.374231135742727,1.97727684456193,11.7399032371853));
#25104=CARTESIAN_POINT('Ctrl Pts',(0.367266634031029,1.95778116746959,11.7388623141564));
#25105=CARTESIAN_POINT('Ctrl Pts',(0.358814082090202,1.93894924870164,11.7378213911276));
#25106=CARTESIAN_POINT('Ctrl Pts',(0.350357189138998,1.92010765835103,11.7367799335078));
#25107=CARTESIAN_POINT('Ctrl Pts',(0.340411005794053,1.90193118520857,11.735738475888));
#25108=CARTESIAN_POINT('Ctrl Pts',(0.329110038905254,1.88465963617616,11.7346970182682));
#25109=CARTESIAN_POINT('Ctrl Pts',(0.317805619078393,1.86738280993256,11.7336552424377));
#25110=CARTESIAN_POINT('Ctrl Pts',(0.305146024431257,1.85101205359708,11.7326134666072));
#25111=CARTESIAN_POINT('Ctrl Pts',(0.291308229420404,1.83575691972741,11.7315716907767));
#25112=CARTESIAN_POINT('Ctrl Pts',(0.277440523701614,1.82046881153968,11.730527663124));
#25113=CARTESIAN_POINT('Ctrl Pts',(0.26239006951038,1.80630164494062,11.7294836354714));
#25114=CARTESIAN_POINT('Ctrl Pts',(0.246370086041824,1.7934275441209,11.7284396078188));
#25115=CARTESIAN_POINT('Ctrl Pts',(0.240704027875007,1.78887414341152,11.728070348923));
#25116=CARTESIAN_POINT('Ctrl Pts',(0.234916966051311,1.78448211089951,11.7277010900271));
#25117=CARTESIAN_POINT('Ctrl Pts',(0.229019169225829,1.78025774422652,11.7273318311312));
#25118=CARTESIAN_POINT('Ctrl Pts',(0.212345015515231,1.76831468458585,11.7262878684837));
#25119=CARTESIAN_POINT('Ctrl Pts',(0.19468444174938,1.75764385551856,11.7252439058361));
#25120=CARTESIAN_POINT('Ctrl Pts',(0.176257814528997,1.74840638114798,11.7241999431886));
#25121=CARTESIAN_POINT('Ctrl Pts',(0.157865085074963,1.73918590010689,11.7231579010228));
#25122=CARTESIAN_POINT('Ctrl Pts',(0.138709723122247,1.73139391897812,11.722115858857));
#25123=CARTESIAN_POINT('Ctrl Pts',(0.1190394234298,1.72514735472522,11.7210738166913));
#25124=CARTESIAN_POINT('Ctrl Pts',(0.0993902493302116,1.71890749918419,
11.7200328936624));
#25125=CARTESIAN_POINT('Ctrl Pts',(0.0792279243557716,1.71421001464389,
11.7189919706336));
#25126=CARTESIAN_POINT('Ctrl Pts',(0.0588181907882767,1.7111230137532,11.7179510476047));
#25127=CARTESIAN_POINT('Ctrl Pts',(0.0383979753135636,1.70803442745931,
11.7169095899849));
#25128=CARTESIAN_POINT('Ctrl Pts',(0.0177308224960689,1.70655810315599,
11.7158681323651));
#25129=CARTESIAN_POINT('Ctrl Pts',(-0.00290882273925296,1.70671075688462,
11.7148266747453));
#25130=CARTESIAN_POINT('Ctrl Pts',(-0.02355477428601,1.70686345725561,11.7137848989148));
#25131=CARTESIAN_POINT('Ctrl Pts',(-0.0441724666480545,1.70864608489199,
11.7127431230843));
#25132=CARTESIAN_POINT('Ctrl Pts',(-0.0644899048119323,1.71202327108788,
11.7117013472538));
#25133=CARTESIAN_POINT('Ctrl Pts',(-0.0848512595794584,1.71540775714838,
11.7106573196013));
#25134=CARTESIAN_POINT('Ctrl Pts',(-0.104910349708517,1.72039350523695,
11.7096132919487));
#25135=CARTESIAN_POINT('Ctrl Pts',(-0.12440703069485,1.72689441077131,11.7085692642961));
#25136=CARTESIAN_POINT('Ctrl Pts',(-0.131302751201956,1.72919369584652,
11.7082000054002));
#25137=CARTESIAN_POINT('Ctrl Pts',(-0.138128291905378,1.7316820744839,11.7078307465043));
#25138=CARTESIAN_POINT('Ctrl Pts',(-0.144872799026719,1.73435432164161,
11.7074614876085));
#25139=CARTESIAN_POINT('Ctrl Pts',(-0.163940758092109,1.74190925464105,
11.7064175249609));
#25140=CARTESIAN_POINT('Ctrl Pts',(-0.182472969912289,1.7509822686813,11.7053735623134));
#25141=CARTESIAN_POINT('Ctrl Pts',(-0.200214670016784,1.76147529497824,
11.7043295996658));
#25142=CARTESIAN_POINT('Ctrl Pts',(-0.217923732352159,1.77194901822262,
11.7032875575001));
#25143=CARTESIAN_POINT('Ctrl Pts',(-0.234844513136281,1.78383724934025,
11.7022455153343));
#25144=CARTESIAN_POINT('Ctrl Pts',(-0.25074462484429,1.7969950114079,11.7012034731685));
#25145=CARTESIAN_POINT('Ctrl Pts',(-0.266627660082109,1.8101386422458,11.7001625501397));
#25146=CARTESIAN_POINT('Ctrl Pts',(-0.281491620007923,1.82454865281849,
11.6991216271108));
#25147=CARTESIAN_POINT('Ctrl Pts',(-0.29513538318823,1.84003847286505,11.6980807040819));
#25148=CARTESIAN_POINT('Ctrl Pts',(-0.308786153449707,1.85553624807947,
11.6970392464622));
#25149=CARTESIAN_POINT('Ctrl Pts',(-0.321214976608486,1.87211439918018,
11.6959977888424));
#25150=CARTESIAN_POINT('Ctrl Pts',(-0.332259235520891,1.88955121665576,
11.6949563312226));
#25151=CARTESIAN_POINT('Ctrl Pts',(-0.343306868935889,1.90699336183926,
11.6939145553921));
#25152=CARTESIAN_POINT('Ctrl Pts',(-0.352968733116018,1.92529405527396,
11.6928727795616));
#25153=CARTESIAN_POINT('Ctrl Pts',(-0.361127330886994,1.94420545296309,
11.6918310037311));
#25154=CARTESIAN_POINT('Ctrl Pts',(-0.369303563652189,1.96315772806747,
11.6907869760785));
#25155=CARTESIAN_POINT('Ctrl Pts',(-0.375969805324185,1.98272264572074,
11.6897429484259));
#25156=CARTESIAN_POINT('Ctrl Pts',(-0.381057633256767,2.00263486179976,
11.6886989207733));
#25157=CARTESIAN_POINT('Ctrl Pts',(-0.382857131306516,2.00967755162245,
11.6883296618774));
#25158=CARTESIAN_POINT('Ctrl Pts',(-0.384459646507782,2.01676359277159,
11.6879604029816));
#25159=CARTESIAN_POINT('Ctrl Pts',(-0.385863696822932,2.02388103078641,
11.6875911440857));
#25160=CARTESIAN_POINT('Ctrl Pts',(-0.390774797430378,2.04877647347876,
11.6862995467917));
#25161=CARTESIAN_POINT('Ctrl Pts',(-0.393277374005961,2.07416195048142,
11.6850079494976));
#25162=CARTESIAN_POINT('Ctrl Pts',(-0.393299847159929,2.09965326670688,
11.6837163522035));
#25163=CARTESIAN_POINT('',(-0.393051472227529,2.09996900767188,11.5587163606577));
#25164=CARTESIAN_POINT('Ctrl Pts',(-0.393452248457544,2.09965462005821,
11.6837162768534));
#25165=CARTESIAN_POINT('Ctrl Pts',(-0.392482851514261,2.20492670250052,
11.6783844514232));
#25166=CARTESIAN_POINT('Ctrl Pts',(-0.294736079347038,2.44255991631743,
11.6664291781522));
#25167=CARTESIAN_POINT('Ctrl Pts',(0.106936353373341,2.55259213405307,11.64785045704));
#25168=CARTESIAN_POINT('Ctrl Pts',(0.438434149993482,2.25508229943799,11.6279801135175));
#25169=CARTESIAN_POINT('Ctrl Pts',(0.367728301414394,1.81530556763727,11.6081097699945));
#25170=CARTESIAN_POINT('Ctrl Pts',(-0.0403182020246674,1.63669721988207,
11.5882394264718));
#25171=CARTESIAN_POINT('Ctrl Pts',(-0.347776659907118,1.84087036089522,
11.5717749611909));
#25172=CARTESIAN_POINT('Ctrl Pts',(-0.392699212427442,2.03611368051729,
11.561933943751));
#25173=CARTESIAN_POINT('Ctrl Pts',(-0.392654779593065,2.09996877097556,
11.5587163741521));
#25174=CARTESIAN_POINT('',(-0.393299835490125,2.10035972689682,11.4337163522035));
#25175=CARTESIAN_POINT('Ctrl Pts',(-0.393299998790548,2.0999691559613,11.5587163522035));
#25176=CARTESIAN_POINT('Ctrl Pts',(-0.393301690756094,2.12154382889946,
11.5576310176873));
#25177=CARTESIAN_POINT('Ctrl Pts',(-0.391523838488396,2.14308824023429,
11.5565456831711));
#25178=CARTESIAN_POINT('Ctrl Pts',(-0.388007014089908,2.16430744138149,
11.5554603486549));
#25179=CARTESIAN_POINT('Ctrl Pts',(-0.384483973544393,2.18556414843151,
11.5543730957606));
#25180=CARTESIAN_POINT('Ctrl Pts',(-0.379216005892341,2.20649387877415,
11.5532858428664));
#25181=CARTESIAN_POINT('Ctrl Pts',(-0.37229422929348,2.22681441887567,11.5521985899721));
#25182=CARTESIAN_POINT('Ctrl Pts',(-0.365349330818397,2.24720283880635,
11.5511077051595));
#25183=CARTESIAN_POINT('Ctrl Pts',(-0.356739858367749,2.26697741933563,
11.550016820347));
#25184=CARTESIAN_POINT('Ctrl Pts',(-0.346604715814774,2.2858764669746,11.5489259355344));
#25185=CARTESIAN_POINT('Ctrl Pts',(-0.345281724482195,2.28834345508944,
11.5487835368316));
#25186=CARTESIAN_POINT('Ctrl Pts',(-0.343932797815208,2.29079556406499,
11.5486411381289));
#25187=CARTESIAN_POINT('Ctrl Pts',(-0.342558298755806,2.29323224874106,
11.5484987394261));
#25188=CARTESIAN_POINT('Ctrl Pts',(-0.332481481697149,2.31109623019849,
11.5474547767786));
#25189=CARTESIAN_POINT('Ctrl Pts',(-0.320973501915486,2.3282230763783,11.546410814131));
#25190=CARTESIAN_POINT('Ctrl Pts',(-0.308166149408896,2.34437371863295,
11.5453668514835));
#25191=CARTESIAN_POINT('Ctrl Pts',(-0.295382357407313,2.36049465004083,
11.5443248093177));
#25192=CARTESIAN_POINT('Ctrl Pts',(-0.281304342812541,2.37564233522766,
11.5432827671519));
#25193=CARTESIAN_POINT('Ctrl Pts',(-0.266107326526554,2.38960625126003,
11.5422407249862));
#25194=CARTESIAN_POINT('Ctrl Pts',(-0.25092663159731,2.40355517026596,11.5411998019573));
#25195=CARTESIAN_POINT('Ctrl Pts',(-0.234629840292544,2.41632232744953,
11.5401588789284));
#25196=CARTESIAN_POINT('Ctrl Pts',(-0.217429130600451,2.42773382975569,
11.5391179558996));
#25197=CARTESIAN_POINT('Ctrl Pts',(-0.200219587072171,2.43915119271201,
11.5380764982798));
#25198=CARTESIAN_POINT('Ctrl Pts',(-0.182105801937319,2.44921108968555,
11.53703504066));
#25199=CARTESIAN_POINT('Ctrl Pts',(-0.163329532164277,2.4577825511718,11.5359935830402));
#25200=CARTESIAN_POINT('Ctrl Pts',(-0.144547525422253,2.46635663161321,
11.5349518072097));
#25201=CARTESIAN_POINT('Ctrl Pts',(-0.125103314869879,2.4734410988211,11.5339100313793));
#25202=CARTESIAN_POINT('Ctrl Pts',(-0.105258415970256,2.47895323704572,
11.5328682555488));
#25203=CARTESIAN_POINT('Ctrl Pts',(-0.0853706218713133,2.48447728988221,
11.5318242278962));
#25204=CARTESIAN_POINT('Ctrl Pts',(-0.06508113324532,2.48842208798903,11.5307802002436));
#25205=CARTESIAN_POINT('Ctrl Pts',(-0.044662132273192,2.49075591350716,
11.529736172591));
#25206=CARTESIAN_POINT('Ctrl Pts',(-0.0374401992765492,2.49158135700171,
11.5293669136951));
#25207=CARTESIAN_POINT('Ctrl Pts',(-0.0302020943018215,2.49220575312069,
11.5289976547992));
#25208=CARTESIAN_POINT('Ctrl Pts',(-0.0229598623062941,2.49262925861794,
11.5286283959034));
#25209=CARTESIAN_POINT('Ctrl Pts',(-0.00248474370291479,2.49382658636039,
11.5275844332558));
#25210=CARTESIAN_POINT('Ctrl Pts',(0.0181452926025266,2.49342154221628,
11.5265404706083));
#25211=CARTESIAN_POINT('Ctrl Pts',(0.0386578931035386,2.491395525397,11.5254965079607));
#25212=CARTESIAN_POINT('Ctrl Pts',(0.0591327584655686,2.48937323565398,
11.524454465795));
#25213=CARTESIAN_POINT('Ctrl Pts',(0.0794898870543711,2.48573590461745,
11.5234124236292));
#25214=CARTESIAN_POINT('Ctrl Pts',(0.0994574171779764,2.48051690129124,
11.5223703814634));
#25215=CARTESIAN_POINT('Ctrl Pts',(0.119403502487916,2.47530350309261,11.5213294584346));
#25216=CARTESIAN_POINT('Ctrl Pts',(0.138960104433556,2.46851196205091,11.5202885354057));
#25217=CARTESIAN_POINT('Ctrl Pts',(0.157866154841925,2.46022654976476,11.5192476123768));
#25218=CARTESIAN_POINT('Ctrl Pts',(0.176781914905033,2.45193688230681,11.518206154757));
#25219=CARTESIAN_POINT('Ctrl Pts',(0.195045775585474,2.44215209145183,11.5171646971373));
#25220=CARTESIAN_POINT('Ctrl Pts',(0.212416747963671,2.43100455462809,11.5161232395175));
#25221=CARTESIAN_POINT('Ctrl Pts',(0.229793027931236,2.41985361174585,11.515081463687));
#25222=CARTESIAN_POINT('Ctrl Pts',(0.246275277309255,2.40733952148462,11.5140396878565));
#25223=CARTESIAN_POINT('Ctrl Pts',(0.2616523841689,2.39363739519811,11.512997912026));
#25224=CARTESIAN_POINT('Ctrl Pts',(0.277062728993971,2.37990565145469,11.5119538843733));
#25225=CARTESIAN_POINT('Ctrl Pts',(0.291362652672405,2.36498127664035,11.5109098567208));
#25226=CARTESIAN_POINT('Ctrl Pts',(0.304378149127902,2.34907595695585,11.5098658290682));
#25227=CARTESIAN_POINT('Ctrl Pts',(0.308981559620264,2.34345045386649,11.5094965701723));
#25228=CARTESIAN_POINT('Ctrl Pts',(0.313424680063558,2.33770252251131,11.5091273112764));
#25229=CARTESIAN_POINT('Ctrl Pts',(0.317701122106218,2.33184237535975,11.5087580523806));
#25230=CARTESIAN_POINT('Ctrl Pts',(0.329791408371408,2.31527466418496,11.507714089733));
#25231=CARTESIAN_POINT('Ctrl Pts',(0.340618251416212,2.29770930257737,11.5066701270854));
#25232=CARTESIAN_POINT('Ctrl Pts',(0.350018581490352,2.27936522129856,11.5056261644379));
#25233=CARTESIAN_POINT('Ctrl Pts',(0.359401618644376,2.26105488593396,11.5045841222721));
#25234=CARTESIAN_POINT('Ctrl Pts',(0.367362967119777,2.24196929472217,11.5035420801064));
#25235=CARTESIAN_POINT('Ctrl Pts',(0.373783520526344,2.22235509708603,11.5025000379406));
#25236=CARTESIAN_POINT('Ctrl Pts',(0.380197178359417,2.20276196479003,11.5014591149117));
#25237=CARTESIAN_POINT('Ctrl Pts',(0.385073071051741,2.18264203984399,11.5004181918829));
#25238=CARTESIAN_POINT('Ctrl Pts',(0.38834073475305,2.16226045078106,11.499377268854));
#25239=CARTESIAN_POINT('Ctrl Pts',(0.391610076641271,2.1418683942652,11.4983358112342));
#25240=CARTESIAN_POINT('Ctrl Pts',(0.393269407093095,2.12121512911217,11.4972943536144));
#25241=CARTESIAN_POINT('Ctrl Pts',(0.393299579763786,2.10057494141412,11.4962528959946));
#25242=CARTESIAN_POINT('Ctrl Pts',(0.393329761653542,2.07992844723888,11.4952111201641));
#25243=CARTESIAN_POINT('Ctrl Pts',(0.391729829908486,2.05929577368364,11.4941693443337));
#25244=CARTESIAN_POINT('Ctrl Pts',(0.388532742588471,2.03894921837781,11.4931275685032));
#25245=CARTESIAN_POINT('Ctrl Pts',(0.385328744691665,2.01855868353097,11.4920835408506));
#25246=CARTESIAN_POINT('Ctrl Pts',(0.380520870206384,1.99845621791746,11.491039513198));
#25247=CARTESIAN_POINT('Ctrl Pts',(0.374192916047162,1.97890271852712,11.4899954855454));
#25248=CARTESIAN_POINT('Ctrl Pts',(0.371954801606327,1.97198690209526,11.4896262266495));
#25249=CARTESIAN_POINT('Ctrl Pts',(0.369526979387773,1.96513958777413,11.4892569677536));
#25250=CARTESIAN_POINT('Ctrl Pts',(0.366914578088518,1.95837167519834,11.4888877088578));
#25251=CARTESIAN_POINT('Ctrl Pts',(0.35952884031106,1.939237544619,11.4878437462102));
#25252=CARTESIAN_POINT('Ctrl Pts',(0.350620335543212,1.92062569351484,11.4867997835627));
#25253=CARTESIAN_POINT('Ctrl Pts',(0.340284872086845,1.90279174502866,11.4857558209151));
#25254=CARTESIAN_POINT('Ctrl Pts',(0.329968421829214,1.88499060401244,11.4847137787493));
#25255=CARTESIAN_POINT('Ctrl Pts',(0.318230536804764,1.86796518429359,11.4836717365836));
#25256=CARTESIAN_POINT('Ctrl Pts',(0.305214129823192,1.85194914844679,11.4826296944178));
#25257=CARTESIAN_POINT('Ctrl Pts',(0.292211702258247,1.8359503135709,11.4815887713889));
#25258=CARTESIAN_POINT('Ctrl Pts',(0.277933917944923,1.82095929677809,11.4805478483601));
#25259=CARTESIAN_POINT('Ctrl Pts',(0.26256555834549,1.80717886420082,11.4795069253312));
#25260=CARTESIAN_POINT('Ctrl Pts',(0.247189305957109,1.79339135435254,11.4784654677114));
#25261=CARTESIAN_POINT('Ctrl Pts',(0.230721896388231,1.7808161739912,11.4774240100917));
#25262=CARTESIAN_POINT('Ctrl Pts',(0.213383590033715,1.76961789772398,11.4763825524719));
#25263=CARTESIAN_POINT('Ctrl Pts',(0.196039986070725,1.75841619989516,11.4753407766414));
#25264=CARTESIAN_POINT('Ctrl Pts',(0.177825592767668,1.74859261214799,11.4742990008109));
#25265=CARTESIAN_POINT('Ctrl Pts',(0.158987203639996,1.74026682238257,11.4732572249804));
#25266=CARTESIAN_POINT('Ctrl Pts',(0.140108094906718,1.73192303623363,11.4722131973278));
#25267=CARTESIAN_POINT('Ctrl Pts',(0.120602992564972,1.72508375531778,11.4711691696752));
#25268=CARTESIAN_POINT('Ctrl Pts',(0.100736624258962,1.71981974994365,11.4701251420226));
#25269=CARTESIAN_POINT('Ctrl Pts',(0.0937101501925314,1.71795794024209,
11.4697558831267));
#25270=CARTESIAN_POINT('Ctrl Pts',(0.0866385816794043,1.71629272166694,
11.4693866242308));
#25271=CARTESIAN_POINT('Ctrl Pts',(0.0795338595838778,1.71482568208707,
11.469017365335));
#25272=CARTESIAN_POINT('Ctrl Pts',(0.0594475066971782,1.71067809203304,
11.4679734026874));
#25273=CARTESIAN_POINT('Ctrl Pts',(0.0389759944577575,1.70809359104565,
11.4669294400399));
#25274=CARTESIAN_POINT('Ctrl Pts',(0.0183861181457955,1.7071299952153,11.4658854773923));
#25275=CARTESIAN_POINT('Ctrl Pts',(-0.00216588087000324,1.70616817202332,
11.4648434352265));
#25276=CARTESIAN_POINT('Ctrl Pts',(-0.0228350878531295,1.70682142858785,
11.4638013930608));
#25277=CARTESIAN_POINT('Ctrl Pts',(-0.0433476738410554,1.70909608703344,
11.462759350895));
#25278=CARTESIAN_POINT('Ctrl Pts',(-0.0638382296338581,1.71136830253158,
11.4617184278661));
#25279=CARTESIAN_POINT('Ctrl Pts',(-0.0841717675901777,1.71525841095673,
11.4606775048373));
#25280=CARTESIAN_POINT('Ctrl Pts',(-0.104077772771117,1.72072080571826,
11.4596365818084));
#25281=CARTESIAN_POINT('Ctrl Pts',(-0.123994001157526,1.72618600582338,
11.4585951241886));
#25282=CARTESIAN_POINT('Ctrl Pts',(-0.143481544303063,1.73322492627905,
11.4575536665688));
#25283=CARTESIAN_POINT('Ctrl Pts',(-0.162282793999812,1.74174145541018,
11.4565122089491));
#25284=CARTESIAN_POINT('Ctrl Pts',(-0.181089788298018,1.75026058671226,
11.4554704331186));
#25285=CARTESIAN_POINT('Ctrl Pts',(-0.199209416969298,1.76025788917048,
11.4544286572881));
#25286=CARTESIAN_POINT('Ctrl Pts',(-0.216407450495129,1.77159064360132,
11.4533868814576));
#25287=CARTESIAN_POINT('Ctrl Pts',(-0.233642657960676,1.78294789403801,
11.452342853805));
#25288=CARTESIAN_POINT('Ctrl Pts',(-0.24995171214025,1.79564590697609,11.4512988261524));
#25289=CARTESIAN_POINT('Ctrl Pts',(-0.26513180623412,1.80950040391933,11.4502547984998));
#25290=CARTESIAN_POINT('Ctrl Pts',(-0.270500806538165,1.8144005578868,11.4498855396039));
#25291=CARTESIAN_POINT('Ctrl Pts',(-0.275728919942093,1.81944504640133,
11.449516280708));
#25292=CARTESIAN_POINT('Ctrl Pts',(-0.280808347531718,1.82462468891256,
11.4491470218122));
#25293=CARTESIAN_POINT('Ctrl Pts',(-0.294977119330179,1.83907300448438,
11.4481169953106));
#25294=CARTESIAN_POINT('Ctrl Pts',(-0.308075501102544,1.85466661177501,
11.4470869688091));
#25295=CARTESIAN_POINT('Ctrl Pts',(-0.319912636152642,1.8712188923231,11.4460569423075));
#25296=CARTESIAN_POINT('Ctrl Pts',(-0.331731227406607,1.88774524243155,
11.4450285294229));
#25297=CARTESIAN_POINT('Ctrl Pts',(-0.342291997362797,1.90522671952452,
11.4440001165382));
#25298=CARTESIAN_POINT('Ctrl Pts',(-0.351443142374184,1.92344233894232,
11.4429717036536));
#25299=CARTESIAN_POINT('Ctrl Pts',(-0.360584777984027,1.94163902962069,
11.441944359443));
#25300=CARTESIAN_POINT('Ctrl Pts',(-0.368319331334013,1.96056768695691,
11.4409170152324));
#25301=CARTESIAN_POINT('Ctrl Pts',(-0.374540414687944,1.97998180235738,
11.4398896710218));
#25302=CARTESIAN_POINT('Ctrl Pts',(-0.380770837192769,1.99942506241688,
11.4388607845521));
#25303=CARTESIAN_POINT('Ctrl Pts',(-0.385482997449294,2.01935451861674,
11.4378318980824));
#25304=CARTESIAN_POINT('Ctrl Pts',(-0.388619909072765,2.03950656008892,
11.4368030116127));
#25305=CARTESIAN_POINT('Ctrl Pts',(-0.391756820696237,2.0596586015611,11.4357741251429));
#25306=CARTESIAN_POINT('Ctrl Pts',(-0.393318427568166,2.08003246947057,
11.4347452386732));
#25307=CARTESIAN_POINT('Ctrl Pts',(-0.393299835490125,2.10035972689682,
11.4337163522035));
#25308=CARTESIAN_POINT('',(-0.393451104642905,2.0998418228525,11.3087163522035));
#25309=CARTESIAN_POINT('Ctrl Pts',(-0.393338930018346,2.10035976265415,
11.4337163522035));
#25310=CARTESIAN_POINT('Ctrl Pts',(-0.393609748993565,2.12960050264535,
11.4322364608988));
#25311=CARTESIAN_POINT('Ctrl Pts',(-0.377272507462022,2.28941218116513,
11.4241331217531));
#25312=CARTESIAN_POINT('Ctrl Pts',(-0.158959746935375,2.53704327283899,
11.4094063347668));
#25313=CARTESIAN_POINT('Ctrl Pts',(0.28142602555706,2.4702356217581,11.3895359912438));
#25314=CARTESIAN_POINT('Ctrl Pts',(0.463641732294656,2.06378719074286,11.3696656477211));
#25315=CARTESIAN_POINT('Ctrl Pts',(0.220529268774129,1.69055908229216,11.3497953041983));
#25316=CARTESIAN_POINT('Ctrl Pts',(-0.224888776497657,1.69293727549082,
11.3299249606755));
#25317=CARTESIAN_POINT('Ctrl Pts',(-0.38966566303918,1.95190924956916,11.3162319766772));
#25318=CARTESIAN_POINT('Ctrl Pts',(-0.39391722199241,2.09105853526501,11.3091624405199));
#25319=CARTESIAN_POINT('Ctrl Pts',(-0.393872410819306,2.09984165347692,
11.3087163522035));
#25320=CARTESIAN_POINT('',(-0.393214805503193,2.09972692384377,11.1837163561346));
#25321=CARTESIAN_POINT('Ctrl Pts',(-0.393299968216638,2.09984188361311,
11.3087163522035));
#25322=CARTESIAN_POINT('Ctrl Pts',(-0.393308138253223,2.12016409810585,
11.3076826968398));
#25323=CARTESIAN_POINT('Ctrl Pts',(-0.391736909333096,2.14055070961828,
11.3066490414762));
#25324=CARTESIAN_POINT('Ctrl Pts',(-0.388582538022818,2.16073303173517,
11.3056153861125));
#25325=CARTESIAN_POINT('Ctrl Pts',(-0.385433660037181,2.18088020642124,
11.3045835308554));
#25326=CARTESIAN_POINT('Ctrl Pts',(-0.380707166298691,2.20082305413041,
11.3035516755983));
#25327=CARTESIAN_POINT('Ctrl Pts',(-0.374451184500351,2.22029630262932,
11.3025198203412));
#25328=CARTESIAN_POINT('Ctrl Pts',(-0.368195759830996,2.23976781693022,
11.3014880569763));
#25329=CARTESIAN_POINT('Ctrl Pts',(-0.360411297107628,2.25876908537834,
11.3004562936115));
#25330=CARTESIAN_POINT('Ctrl Pts',(-0.35119635464645,2.27704804569112,11.2994245302467));
#25331=CARTESIAN_POINT('Ctrl Pts',(-0.341983499361973,2.29532286583479,
11.2983930005754));
#25332=CARTESIAN_POINT('Ctrl Pts',(-0.33134115609013,2.31287503586723,11.2973614709041));
#25333=CARTESIAN_POINT('Ctrl Pts',(-0.319414312760897,2.32947633168474,
11.2963299412328));
#25334=CARTESIAN_POINT('Ctrl Pts',(-0.30745977490038,2.3461161762694,11.2952960163149));
#25335=CARTESIAN_POINT('Ctrl Pts',(-0.294215240158087,2.36180013753523,
11.294262091397));
#25336=CARTESIAN_POINT('Ctrl Pts',(-0.279867280661049,2.37633167609847,
11.2932281664791));
#25337=CARTESIAN_POINT('Ctrl Pts',(-0.265787066982277,2.3905920430931,11.2922135355294));
#25338=CARTESIAN_POINT('Ctrl Pts',(-0.250644892116299,2.40374230168349,
11.2911989045796));
#25339=CARTESIAN_POINT('Ctrl Pts',(-0.234647390926508,2.41563506131509,
11.2901842736299));
#25340=CARTESIAN_POINT('Ctrl Pts',(-0.218187422205484,2.42787162558976,
11.2891403109823));
#25341=CARTESIAN_POINT('Ctrl Pts',(-0.200718650950658,2.43885363312795,
11.2880963483347));
#25342=CARTESIAN_POINT('Ctrl Pts',(-0.182458554907021,2.44841608134706,
11.2870523856872));
#25343=CARTESIAN_POINT('Ctrl Pts',(-0.164232050277696,2.45796093841225,
11.2860103435214));
#25344=CARTESIAN_POINT('Ctrl Pts',(-0.145217727279964,2.46609102957953,
11.2849683013556));
#25345=CARTESIAN_POINT('Ctrl Pts',(-0.12566117064822,2.4726850683772,11.2839262591899));
#25346=CARTESIAN_POINT('Ctrl Pts',(-0.106125617451067,2.4792720252808,11.282885336161));
#25347=CARTESIAN_POINT('Ctrl Pts',(-0.08604967116135,2.48432594355809,11.2818444131322));
#25348=CARTESIAN_POINT('Ctrl Pts',(-0.0656978257613062,2.48777401368611,
11.2808034901033));
#25349=CARTESIAN_POINT('Ctrl Pts',(-0.0453355281838982,2.49122385465308,
11.2797620324835));
#25350=CARTESIAN_POINT('Ctrl Pts',(-0.0246977711695951,2.4930660610608,
11.2787205748637));
#25351=CARTESIAN_POINT('Ctrl Pts',(-0.0040586604570363,2.49327905776343,
11.277679117244));
#25352=CARTESIAN_POINT('Ctrl Pts',(0.0165867564036378,2.49349211954584,
11.2766373414135));
#25353=CARTESIAN_POINT('Ctrl Pts',(0.0372327922934162,2.49207500922423,
11.275595565583));
#25354=CARTESIAN_POINT('Ctrl Pts',(0.0576068683316351,2.48905827162653,
11.2745537897525));
#25355=CARTESIAN_POINT('Ctrl Pts',(0.0780249833975529,2.48603501328205,
11.2735097620999));
#25356=CARTESIAN_POINT('Ctrl Pts',(0.0981692472374602,2.48140538963035,
11.2724657344473));
#25357=CARTESIAN_POINT('Ctrl Pts',(0.117778030846165,2.4752508833434,11.2714217067947));
#25358=CARTESIAN_POINT('Ctrl Pts',(0.124713400581441,2.47307411514146,11.2710524478988));
#25359=CARTESIAN_POINT('Ctrl Pts',(0.131581951273689,2.4707070398309,11.270683189003));
#25360=CARTESIAN_POINT('Ctrl Pts',(0.13837273828728,2.46815468936152,11.2703139301071));
#25361=CARTESIAN_POINT('Ctrl Pts',(0.157571539099015,2.46093872629785,11.2692699674596));
#25362=CARTESIAN_POINT('Ctrl Pts',(0.176261569184111,2.45219542977191,11.268226004812));
#25363=CARTESIAN_POINT('Ctrl Pts',(0.194186366783898,2.44201834008613,11.2671820421645));
#25364=CARTESIAN_POINT('Ctrl Pts',(0.212078189786992,2.43185997225346,11.2661399999987));
#25365=CARTESIAN_POINT('Ctrl Pts',(0.229206912610394,2.4202733542875,11.2650979578329));
#25366=CARTESIAN_POINT('Ctrl Pts',(0.245337615962998,2.40739932367133,11.2640559156672));
#25367=CARTESIAN_POINT('Ctrl Pts',(0.261450995193613,2.3945391195618,11.2630149926383));
#25368=CARTESIAN_POINT('Ctrl Pts',(0.276567892644409,2.38039468175596,11.2619740696095));
#25369=CARTESIAN_POINT('Ctrl Pts',(0.290483913393173,2.36514898841932,11.2609331465806));
#25370=CARTESIAN_POINT('Ctrl Pts',(0.304407081047498,2.34989546529193,11.2598916889608));
#25371=CARTESIAN_POINT('Ctrl Pts',(0.317127631951129,2.33354008930304,11.258850231341));
#25372=CARTESIAN_POINT('Ctrl Pts',(0.328479046946049,2.31630165444909,11.2578087737212));
#25373=CARTESIAN_POINT('Ctrl Pts',(0.339833930293128,2.29905795250178,11.2567669978907));
#25374=CARTESIAN_POINT('Ctrl Pts',(0.349818470839558,2.28093128844845,11.2557252220603));
#25375=CARTESIAN_POINT('Ctrl Pts',(0.358310799350261,2.26216738595962,11.2546834462298));
#25376=CARTESIAN_POINT('Ctrl Pts',(0.366821484221758,2.24336292486975,11.2536394185772));
#25377=CARTESIAN_POINT('Ctrl Pts',(0.373833267765141,2.22391916822786,11.2525953909246));
#25378=CARTESIAN_POINT('Ctrl Pts',(0.379273037562057,2.20410020642847,11.251551363272));
#25379=CARTESIAN_POINT('Ctrl Pts',(0.38119701283606,2.19709049942211,11.2511821043761));
#25380=CARTESIAN_POINT('Ctrl Pts',(0.382924804130471,2.19003395838695,11.2508128454802));
#25381=CARTESIAN_POINT('Ctrl Pts',(0.384454717869747,2.18294250965394,11.2504435865844));
#25382=CARTESIAN_POINT('Ctrl Pts',(0.388780064708143,2.16289368299819,11.2493996239368));
#25383=CARTESIAN_POINT('Ctrl Pts',(0.391545795438273,2.14244586667834,11.2483556612893));
#25384=CARTESIAN_POINT('Ctrl Pts',(0.392691733037251,2.12186533338873,11.2473116986417));
#25385=CARTESIAN_POINT('Ctrl Pts',(0.393835562560534,2.10132266020778,11.2462696564759));
#25386=CARTESIAN_POINT('Ctrl Pts',(0.393365413884186,2.08064847771675,11.2452276143102));
#25387=CARTESIAN_POINT('Ctrl Pts',(0.391272539628604,2.06011654813607,11.2441855721444));
#25388=CARTESIAN_POINT('Ctrl Pts',(0.389181913087094,2.03960666952521,11.2431446491156));
#25389=CARTESIAN_POINT('Ctrl Pts',(0.385472066267624,2.01923947173177,11.2421037260867));
#25390=CARTESIAN_POINT('Ctrl Pts',(0.380186207823277,1.99928586305312,11.2410628030578));
#25391=CARTESIAN_POINT('Ctrl Pts',(0.3748976346998,1.97932200672109,11.240021345438));
#25392=CARTESIAN_POINT('Ctrl Pts',(0.368031605785315,1.95977287922202,11.2389798878183));
#25393=CARTESIAN_POINT('Ctrl Pts',(0.359681947160373,1.94089692998901,11.2379384301985));
#25394=CARTESIAN_POINT('Ctrl Pts',(0.351329737350708,1.92201521333059,11.236896654368));
#25395=CARTESIAN_POINT('Ctrl Pts',(0.34149332587491,1.90380774209201,11.2358548785375));
#25396=CARTESIAN_POINT('Ctrl Pts',(0.330313351575673,1.88651000077089,11.234813102707));
#25397=CARTESIAN_POINT('Ctrl Pts',(0.319109211508281,1.86917486998937,11.2337690750544));
#25398=CARTESIAN_POINT('Ctrl Pts',(0.306556157922229,1.85275398004779,11.2327250474018));
#25399=CARTESIAN_POINT('Ctrl Pts',(0.292836665676481,1.83745176207889,11.2316810197492));
#25400=CARTESIAN_POINT('Ctrl Pts',(0.287984261100866,1.83203956816097,11.2313117608533));
#25401=CARTESIAN_POINT('Ctrl Pts',(0.282986279702331,1.82676697713963,11.2309425019574));
#25402=CARTESIAN_POINT('Ctrl Pts',(0.277851832590422,1.82164186894193,11.2305732430616));
#25403=CARTESIAN_POINT('Ctrl Pts',(0.263335808574053,1.80715224774946,11.229529280414));
#25404=CARTESIAN_POINT('Ctrl Pts',(0.247640058524564,1.79375799939032,11.2284853177665));
#25405=CARTESIAN_POINT('Ctrl Pts',(0.230955894380986,1.78165386000349,11.2274413551189));
#25406=CARTESIAN_POINT('Ctrl Pts',(0.214302422555172,1.76957198748535,11.2263993129531));
#25407=CARTESIAN_POINT('Ctrl Pts',(0.196664699784659,1.75877598836898,11.2253572707874));
#25408=CARTESIAN_POINT('Ctrl Pts',(0.178268175131284,1.74942141004425,11.2243152286216));
#25409=CARTESIAN_POINT('Ctrl Pts',(0.159891408056386,1.74007687838968,11.2232743055927));
#25410=CARTESIAN_POINT('Ctrl Pts',(0.140758096373477,1.73217105184052,11.2222333825639));
#25411=CARTESIAN_POINT('Ctrl Pts',(0.121119414254062,1.72581424734398,11.221192459535));
#25412=CARTESIAN_POINT('Ctrl Pts',(0.10147064621935,1.71945417815833,11.2201510019152));
#25413=CARTESIAN_POINT('Ctrl Pts',(0.081316684290351,1.71464496225607,11.2191095442954));
#25414=CARTESIAN_POINT('Ctrl Pts',(0.0609256271305449,1.71144761233683,
11.2180680866757));
#25415=CARTESIAN_POINT('Ctrl Pts',(0.0405283396137982,1.7082492854878,11.2170263108452));
#25416=CARTESIAN_POINT('Ctrl Pts',(0.0198945445382996,1.70666388320196,
11.2159845350147));
#25417=CARTESIAN_POINT('Ctrl Pts',(-0.000701628167408186,1.70670062583585,
11.2149427591842));
#25418=CARTESIAN_POINT('Ctrl Pts',(-0.0213423199677942,1.70673744788977,
11.2138987315316));
#25419=CARTESIAN_POINT('Ctrl Pts',(-0.0419444929620127,1.70840335566758,
11.212854703879));
#25420=CARTESIAN_POINT('Ctrl Pts',(-0.0622374808551683,1.71165558330677,
11.2118106762264));
#25421=CARTESIAN_POINT('Ctrl Pts',(-0.0694148446774901,1.71280585359336,
11.2114414173305));
#25422=CARTESIAN_POINT('Ctrl Pts',(-0.0765536312495216,1.71415409704949,
11.2110721584346));
#25423=CARTESIAN_POINT('Ctrl Pts',(-0.0836422829792746,1.71569691843804,
11.2107028995388));
#25424=CARTESIAN_POINT('Ctrl Pts',(-0.103683201993579,1.72005875756914,
11.2096589368912));
#25425=CARTESIAN_POINT('Ctrl Pts',(-0.123441718935667,1.72600547657797,
11.2086149742437));
#25426=CARTESIAN_POINT('Ctrl Pts',(-0.142650535563883,1.73348163115154,
11.2075710115961));
#25427=CARTESIAN_POINT('Ctrl Pts',(-0.161824015504042,1.74094403253317,
11.2065289694303));
#25428=CARTESIAN_POINT('Ctrl Pts',(-0.180449102885875,1.74993007623814,
11.2054869272646));
#25429=CARTESIAN_POINT('Ctrl Pts',(-0.198272971028225,1.76033440127143,
11.2044448850988));
#25430=CARTESIAN_POINT('Ctrl Pts',(-0.216077696616201,1.77072755222308,
11.20340396207));
#25431=CARTESIAN_POINT('Ctrl Pts',(-0.233082264458637,1.78253561649592,
11.2023630390411));
#25432=CARTESIAN_POINT('Ctrl Pts',(-0.249057952973691,1.79560711890625,
11.2013221160122));
#25433=CARTESIAN_POINT('Ctrl Pts',(-0.265041846185989,1.80868533449953,
11.2002806583925));
#25434=CARTESIAN_POINT('Ctrl Pts',(-0.279995224773786,1.82302783106876,
11.1992392007727));
#25435=CARTESIAN_POINT('Ctrl Pts',(-0.29372166151608,1.83844221373426,11.1981977431529));
#25436=CARTESIAN_POINT('Ctrl Pts',(-0.307452292283217,1.85386130616568,
11.1971559673224));
#25437=CARTESIAN_POINT('Ctrl Pts',(-0.319954773014172,1.87035236359677,
11.1961141914919));
#25438=CARTESIAN_POINT('Ctrl Pts',(-0.331072959584572,1.88768988382107,
11.1950724156614));
#25439=CARTESIAN_POINT('Ctrl Pts',(-0.342215178367549,1.90506487948877,
11.1940283880088));
#25440=CARTESIAN_POINT('Ctrl Pts',(-0.351966781780331,1.92328934139265,
11.1929843603562));
#25441=CARTESIAN_POINT('Ctrl Pts',(-0.360217211569774,1.94211253853172,
11.1919403327036));
#25442=CARTESIAN_POINT('Ctrl Pts',(-0.363135280441789,1.94877005663019,
11.1915710738077));
#25443=CARTESIAN_POINT('Ctrl Pts',(-0.365866007365618,1.95550230473974,
11.1912018149119));
#25444=CARTESIAN_POINT('Ctrl Pts',(-0.368405990784053,1.96229772712689,
11.190832556016));
#25445=CARTESIAN_POINT('Ctrl Pts',(-0.376614512448147,1.98425864682296,
11.1896392137192));
#25446=CARTESIAN_POINT('Ctrl Pts',(-0.382867824574344,2.00698821532882,
11.1884458714223));
#25447=CARTESIAN_POINT('Ctrl Pts',(-0.387048135574983,2.03015280429445,
11.1872525291255));
#25448=CARTESIAN_POINT('Ctrl Pts',(-0.39117723833591,2.05303363020408,11.1860738051091));
#25449=CARTESIAN_POINT('Ctrl Pts',(-0.393283661585075,2.07633860235924,
11.1848950810926));
#25450=CARTESIAN_POINT('Ctrl Pts',(-0.393299905144833,2.0997268460775,11.1837163570762));
#25451=CARTESIAN_POINT('',(-0.39323593112807,2.10028300833082,11.058716348113));
#25452=CARTESIAN_POINT('Ctrl Pts',(-0.392859536202407,2.09972724849813,
11.1837163522035));
#25453=CARTESIAN_POINT('Ctrl Pts',(-0.392322465415884,2.18398909790107,
11.1794649723));
#25454=CARTESIAN_POINT('Ctrl Pts',(-0.324387757795137,2.40031688674488,
11.1685901445557));
#25455=CARTESIAN_POINT('Ctrl Pts',(0.0321045751991462,2.56394430671225,
11.1510918689703));
#25456=CARTESIAN_POINT('Ctrl Pts',(0.407471466368896,2.32414733452502,11.1312215254476));
#25457=CARTESIAN_POINT('Ctrl Pts',(0.409038759376262,1.87872569781509,11.1113511819248));
#25458=CARTESIAN_POINT('Ctrl Pts',(0.0353686762546443,1.63629310958381,
11.091480838402));
#25459=CARTESIAN_POINT('Ctrl Pts',(-0.32322012530308,1.79783743961437,11.0739358951616));
#25460=CARTESIAN_POINT('Ctrl Pts',(-0.392314997973443,2.01510676408243,
11.0630143997621));
#25461=CARTESIAN_POINT('Ctrl Pts',(-0.39287953052133,2.10028267075746,11.0587163522035));
#25462=CARTESIAN_POINT('',(-0.393447242236147,2.10014273833465,10.9337163522035));
#25463=CARTESIAN_POINT('Ctrl Pts',(-0.393299898133711,2.1002830689187,11.0587163473789));
#25464=CARTESIAN_POINT('Ctrl Pts',(-0.393282756740734,2.12409955906082,
11.0575158255002));
#25465=CARTESIAN_POINT('Ctrl Pts',(-0.391098152989675,2.14782821277761,
11.0563153036215));
#25466=CARTESIAN_POINT('Ctrl Pts',(-0.386817917864597,2.17111109912593,
11.0551147817429));
#25467=CARTESIAN_POINT('Ctrl Pts',(-0.382807381066406,2.19292692693431,
11.0539899049474));
#25468=CARTESIAN_POINT('Ctrl Pts',(-0.376957620305677,2.21435139802366,
11.0528650281519));
#25469=CARTESIAN_POINT('Ctrl Pts',(-0.369365914877162,2.23510629491981,
11.0517401513565));
#25470=CARTESIAN_POINT('Ctrl Pts',(-0.362320292698361,2.25436825960839,
11.0506961887089));
#25471=CARTESIAN_POINT('Ctrl Pts',(-0.353742890421406,2.2731350022375,11.0496522260614));
#25472=CARTESIAN_POINT('Ctrl Pts',(-0.343724973009998,2.29114924255481,
11.0486082634138));
#25473=CARTESIAN_POINT('Ctrl Pts',(-0.333725484637158,2.3091303437359,11.0475662212481));
#25474=CARTESIAN_POINT('Ctrl Pts',(-0.322291042826342,2.32636102572852,
11.0465241790823));
#25475=CARTESIAN_POINT('Ctrl Pts',(-0.309560398683813,2.34260513095712,
11.0454821369165));
#25476=CARTESIAN_POINT('Ctrl Pts',(-0.2968434270531,2.35883179027188,11.0444412138876));
#25477=CARTESIAN_POINT('Ctrl Pts',(-0.282833445540318,2.37407338229495,
11.0434002908588));
#25478=CARTESIAN_POINT('Ctrl Pts',(-0.267711614657557,2.38812389935138,
11.0423593678299));
#25479=CARTESIAN_POINT('Ctrl Pts',(-0.252582017596578,2.40218163238717,
11.0413179102101));
#25480=CARTESIAN_POINT('Ctrl Pts',(-0.236339958445469,2.41504655576692,
11.0402764525903));
#25481=CARTESIAN_POINT('Ctrl Pts',(-0.219202747635513,2.42655021884703,
11.0392349949705));
#25482=CARTESIAN_POINT('Ctrl Pts',(-0.202060300660533,2.43805739679772,
11.03819321914));
#25483=CARTESIAN_POINT('Ctrl Pts',(-0.184022788091632,2.44820210674712,
11.0371514433095));
#25484=CARTESIAN_POINT('Ctrl Pts',(-0.165334844474637,2.45686030768712,
11.036109667479));
#25485=CARTESIAN_POINT('Ctrl Pts',(-0.146606506443435,2.46553722352494,
11.0350656398263));
#25486=CARTESIAN_POINT('Ctrl Pts',(-0.127225621076391,2.47272095954478,
11.0340216121737));
#25487=CARTESIAN_POINT('Ctrl Pts',(-0.107455620797547,2.47833606695505,
11.0329775845211));
#25488=CARTESIAN_POINT('Ctrl Pts',(-0.100463230839971,2.4803220568444,11.0326083256253));
#25489=CARTESIAN_POINT('Ctrl Pts',(-0.0934222709461556,2.48211228529378,
11.0322390667295));
#25490=CARTESIAN_POINT('Ctrl Pts',(-0.0863446519779231,2.48370495315387,
11.0318698078336));
#25491=CARTESIAN_POINT('Ctrl Pts',(-0.066334924602597,2.48820771740592,
11.0308258451861));
#25492=CARTESIAN_POINT('Ctrl Pts',(-0.0459124085568853,2.49115446087699,
11.0297818825385));
#25493=CARTESIAN_POINT('Ctrl Pts',(-0.0253428330572904,2.49248265033327,
11.028737919891));
#25494=CARTESIAN_POINT('Ctrl Pts',(-0.00481109750832695,2.49380839644193,
11.0276958777252));
#25495=CARTESIAN_POINT('Ctrl Pts',(0.015866438375116,2.49352139254206,11.0266538355594));
#25496=CARTESIAN_POINT('Ctrl Pts',(0.0364161005943682,2.49161046668533,
11.0256117933937));
#25497=CARTESIAN_POINT('Ctrl Pts',(0.0569436927992294,2.48970159313294,
11.0245708703648));
#25498=CARTESIAN_POINT('Ctrl Pts',(0.077342952400591,2.48617229899716,11.023529947336));
#25499=CARTESIAN_POINT('Ctrl Pts',(0.0973425989983654,2.48106339160334,
11.0224890243071));
#25500=CARTESIAN_POINT('Ctrl Pts',(0.117352516893378,2.47595186040784,11.0214475666873));
#25501=CARTESIAN_POINT('Ctrl Pts',(0.136961694903382,2.46925926174951,11.0204061090675));
#25502=CARTESIAN_POINT('Ctrl Pts',(0.15591086264823,2.46107712875269,11.0193646514477));
#25503=CARTESIAN_POINT('Ctrl Pts',(0.174865820189927,2.45289249575753,11.0183228756173));
#25504=CARTESIAN_POINT('Ctrl Pts',(0.193159705420792,2.44321774703808,11.0172810997868));
#25505=CARTESIAN_POINT('Ctrl Pts',(0.210555797340428,2.43219143006155,11.0162393239563));
#25506=CARTESIAN_POINT('Ctrl Pts',(0.227989491307518,2.42114127945065,11.0151952963037));
#25507=CARTESIAN_POINT('Ctrl Pts',(0.244520928612884,2.40873417014082,11.0141512686511));
#25508=CARTESIAN_POINT('Ctrl Pts',(0.259944069830627,2.39515075903662,11.0131072409985));
#25509=CARTESIAN_POINT('Ctrl Pts',(0.265399032716648,2.39034648457703,11.0127379821026));
#25510=CARTESIAN_POINT('Ctrl Pts',(0.270715687663013,2.38539540244076,11.0123687232067));
#25511=CARTESIAN_POINT('Ctrl Pts',(0.275886074348036,2.38030655358166,11.0119994643109));
#25512=CARTESIAN_POINT('Ctrl Pts',(0.290503706131458,2.36591944419209,11.0109555016633));
#25513=CARTESIAN_POINT('Ctrl Pts',(0.304036457748546,2.35034295253348,11.0099115390158));
#25514=CARTESIAN_POINT('Ctrl Pts',(0.316287906110368,2.33376665811941,11.0088675763682));
#25515=CARTESIAN_POINT('Ctrl Pts',(0.328516816612759,2.31722085758512,11.0078255342025));
#25516=CARTESIAN_POINT('Ctrl Pts',(0.339468622388193,2.29967945479898,11.0067834920367));
#25517=CARTESIAN_POINT('Ctrl Pts',(0.348985785182018,2.28136651218152,11.0057414498709));
#25518=CARTESIAN_POINT('Ctrl Pts',(0.358492726692516,2.26307323737675,11.0047005268421));
#25519=CARTESIAN_POINT('Ctrl Pts',(0.366567720806767,2.24401070398177,11.0036596038132));
#25520=CARTESIAN_POINT('Ctrl Pts',(0.373098230072271,2.22442909915666,11.0026186807844));
#25521=CARTESIAN_POINT('Ctrl Pts',(0.379632093237126,2.20483743772968,11.0015772231646));
#25522=CARTESIAN_POINT('Ctrl Pts',(0.384619638830534,2.18472686518731,11.0005357655448));
#25523=CARTESIAN_POINT('Ctrl Pts',(0.387997481800792,2.16436492924135,10.999494307925));
#25524=CARTESIAN_POINT('Ctrl Pts',(0.391376356849339,2.14399677183626,10.9984525320945));
#25525=CARTESIAN_POINT('Ctrl Pts',(0.39314446553063,2.12337782929996,10.997410756264));
#25526=CARTESIAN_POINT('Ctrl Pts',(0.393290159680905,2.10278213913533,10.9963689804335));
#25527=CARTESIAN_POINT('Ctrl Pts',(0.393436168752392,2.08214193091904,10.9953249527809));
#25528=CARTESIAN_POINT('Ctrl Pts',(0.391952814820575,2.06152580999585,10.9942809251283));
#25529=CARTESIAN_POINT('Ctrl Pts',(0.388880464581221,2.04120481085077,10.9932368974757));
#25530=CARTESIAN_POINT('Ctrl Pts',(0.387793814573136,2.03401753981557,10.9928676385798));
#25531=CARTESIAN_POINT('Ctrl Pts',(0.386508857455187,2.02686709092432,10.9924983796839));
#25532=CARTESIAN_POINT('Ctrl Pts',(0.385028885957275,2.01976505138969,10.9921291207881));
#25533=CARTESIAN_POINT('Ctrl Pts',(0.380844734998389,1.99968628259529,10.9910851581405));
#25534=CARTESIAN_POINT('Ctrl Pts',(0.375073264895953,1.97987586635585,10.990041195493));
#25535=CARTESIAN_POINT('Ctrl Pts',(0.367767550132113,1.96060158153758,10.9889972328454));
#25536=CARTESIAN_POINT('Ctrl Pts',(0.360475275017815,1.94136275384315,10.9879551906796));
#25537=CARTESIAN_POINT('Ctrl Pts',(0.351654559839988,1.9226588011806,10.9869131485139));
#25538=CARTESIAN_POINT('Ctrl Pts',(0.341408521989746,1.90474347357187,10.9858711063481));
#25539=CARTESIAN_POINT('Ctrl Pts',(0.331173488223197,1.88684738674356,10.9848301833192));
#25540=CARTESIAN_POINT('Ctrl Pts',(0.319516509061671,1.86973889334966,10.9837892602904));
#25541=CARTESIAN_POINT('Ctrl Pts',(0.306587027792332,1.85364804772549,10.9827483372615));
#25542=CARTESIAN_POINT('Ctrl Pts',(0.293650906278391,1.83754893826237,10.9817068796417));
#25543=CARTESIAN_POINT('Ctrl Pts',(0.279441425366232,1.82246910433631,10.9806654220219));
#25544=CARTESIAN_POINT('Ctrl Pts',(0.264149232488438,1.80860666964433,10.9796239644021));
#25545=CARTESIAN_POINT('Ctrl Pts',(0.248852367179039,1.7947399993742,10.9785821885716));
#25546=CARTESIAN_POINT('Ctrl Pts',(0.232472700301874,1.78209193578253,10.9775404127411));
#25547=CARTESIAN_POINT('Ctrl Pts',(0.215234342134315,1.7708206143058,10.9764986369106));
#25548=CARTESIAN_POINT('Ctrl Pts',(0.197958722864387,1.75952492961193,10.9754546092581));
#25549=CARTESIAN_POINT('Ctrl Pts',(0.179821352987357,1.74961228139096,10.9744105816055));
#25550=CARTESIAN_POINT('Ctrl Pts',(0.161071974372725,1.74119544446639,10.9733665539529));
#25551=CARTESIAN_POINT('Ctrl Pts',(0.154440564919061,1.73821851957204,10.972997295057));
#25552=CARTESIAN_POINT('Ctrl Pts',(0.147732768961565,1.73542826733806,10.9726280361611));
#25553=CARTESIAN_POINT('Ctrl Pts',(0.140960111650303,1.73282819154579,10.9722587772653));
#25554=CARTESIAN_POINT('Ctrl Pts',(0.121812566833145,1.72547730023794,10.9712148146177));
#25555=CARTESIAN_POINT('Ctrl Pts',(0.102031413115449,1.71960631937277,10.9701708519702));
#25556=CARTESIAN_POINT('Ctrl Pts',(0.0818705339385076,1.71531557651417,
10.9691268893226));
#25557=CARTESIAN_POINT('Ctrl Pts',(0.0617467428712652,1.71103272693941,
10.9680848471568));
#25558=CARTESIAN_POINT('Ctrl Pts',(0.0412453120838937,1.70832455465519,
10.9670428049911));
#25559=CARTESIAN_POINT('Ctrl Pts',(0.02063541844509,1.70724171618463,10.9660007628253));
#25560=CARTESIAN_POINT('Ctrl Pts',(4.76595082905158E-5,1.70616004066558,
10.9649598397964));
#25561=CARTESIAN_POINT('Ctrl Pts',(-0.020647601502705,1.70670030085064,
10.9639189167676));
#25562=CARTESIAN_POINT('Ctrl Pts',(-0.0411760344321745,1.70886137471679,
10.9628779937387));
#25563=CARTESIAN_POINT('Ctrl Pts',(-0.0617150102297682,1.71102355845416,
10.9618365361189));
#25564=CARTESIAN_POINT('Ctrl Pts',(-0.0820862533567069,1.71480815783761,
10.9607950784992));
#25565=CARTESIAN_POINT('Ctrl Pts',(-0.102019976961212,1.72016212102947,
10.9597536208794));
#25566=CARTESIAN_POINT('Ctrl Pts',(-0.121959791187311,1.72551772009049,
10.9587118450489));
#25567=CARTESIAN_POINT('Ctrl Pts',(-0.141461119153378,1.73244341191047,
10.9576700692184));
#25568=CARTESIAN_POINT('Ctrl Pts',(-0.160269682810538,1.74083636212471,
10.9566282933879));
#25569=CARTESIAN_POINT('Ctrl Pts',(-0.179118901604866,1.74924745389131,
10.9555842657353));
#25570=CARTESIAN_POINT('Ctrl Pts',(-0.197271719744822,1.75913178363014,
10.9545402380827));
#25571=CARTESIAN_POINT('Ctrl Pts',(-0.214498124353156,1.77034041095552,
10.9534962104301));
#25572=CARTESIAN_POINT('Ctrl Pts',(-0.220590877863647,1.77430475552057,
10.9531269515342));
#25573=CARTESIAN_POINT('Ctrl Pts',(-0.226568023053773,1.77843437650973,
10.9527576926384));
#25574=CARTESIAN_POINT('Ctrl Pts',(-0.232420375109476,1.7827214800306,10.9523884337425));
#25575=CARTESIAN_POINT('Ctrl Pts',(-0.248819573639561,1.79473460929704,
10.9513537130209));
#25576=CARTESIAN_POINT('Ctrl Pts',(-0.264337975346716,1.80806158770309,
10.9503189922992));
#25577=CARTESIAN_POINT('Ctrl Pts',(-0.278755922944686,1.8225472555132,10.9492842715776));
#25578=CARTESIAN_POINT('Ctrl Pts',(-0.293147344501958,1.83700627269144,
10.948251454528));
#25579=CARTESIAN_POINT('Ctrl Pts',(-0.306441761726816,1.8526192683248,10.9472186374785));
#25580=CARTESIAN_POINT('Ctrl Pts',(-0.318452741495019,1.86919111491473,
10.9461858204289));
#25581=CARTESIAN_POINT('Ctrl Pts',(-0.330537047765084,1.88586413189735,
10.9451466980768));
#25582=CARTESIAN_POINT('Ctrl Pts',(-0.341321657094338,1.90350719523694,
10.9441075757247));
#25583=CARTESIAN_POINT('Ctrl Pts',(-0.350657800144795,1.92188768375653,
10.9430684533726));
#25584=CARTESIAN_POINT('Ctrl Pts',(-0.35993220757721,1.94014663056317,10.9420362022584));
#25585=CARTESIAN_POINT('Ctrl Pts',(-0.367776946782641,1.95913258149407,
10.9410039511443));
#25586=CARTESIAN_POINT('Ctrl Pts',(-0.374092750276984,1.97859364023989,
10.9399717000301));
#25587=CARTESIAN_POINT('Ctrl Pts',(-0.380471616026515,1.99824901444437,
10.938929142059));
#25588=CARTESIAN_POINT('Ctrl Pts',(-0.385290591659725,2.018388300583,10.9378865840879));
#25589=CARTESIAN_POINT('Ctrl Pts',(-0.388499540705839,2.03873829196511,
10.9368440261168));
#25590=CARTESIAN_POINT('Ctrl Pts',(-0.391708489751952,2.05908828334722,
10.9358014681457));
#25591=CARTESIAN_POINT('Ctrl Pts',(-0.393307409292416,2.07964819771871,
10.9347589101746));
#25592=CARTESIAN_POINT('Ctrl Pts',(-0.393299974117743,2.10014268490739,
10.9337163522035));
#25593=CARTESIAN_POINT('',(-0.393299834164626,2.09963882680431,10.8087163522035));
#25594=CARTESIAN_POINT('Ctrl Pts',(-0.39388694406762,2.10014289785364,10.9337163522035));
#25595=CARTESIAN_POINT('Ctrl Pts',(-0.393923666401966,2.10800639674678,
10.9333169315422));
#25596=CARTESIAN_POINT('Ctrl Pts',(-0.393708632815697,2.11586784849621,
10.932917510881));
#25597=CARTESIAN_POINT('Ctrl Pts',(-0.38538959090996,2.25381922960492,10.9258946423788));
#25598=CARTESIAN_POINT('Ctrl Pts',(-0.227747813468656,2.50547004444192,
10.9126477466968));
#25599=CARTESIAN_POINT('Ctrl Pts',(0.217642466485707,2.51098270068397,10.8927774031741));
#25600=CARTESIAN_POINT('Ctrl Pts',(0.46337541278574,2.13947467929094,10.8729070596514));
#25601=CARTESIAN_POINT('Ctrl Pts',(0.284024500720983,1.73175401364076,10.8530367161285));
#25602=CARTESIAN_POINT('Ctrl Pts',(-0.155880224311077,1.66184890831106,
10.8331663726058));
#25603=CARTESIAN_POINT('Ctrl Pts',(-0.376627538569165,1.90871737413284,
10.8183929179641));
#25604=CARTESIAN_POINT('Ctrl Pts',(-0.393589382880225,2.06947046398226,
10.8102429111633));
#25605=CARTESIAN_POINT('Ctrl Pts',(-0.393310804513336,2.09963881673007,
10.8087163522035));
#25606=CARTESIAN_POINT('',(-0.393052814201458,2.10004628639809,10.6837163396379));
#25607=CARTESIAN_POINT('Ctrl Pts',(-0.393299834164626,2.09963882680431,
10.8087163522035));
#25608=CARTESIAN_POINT('Ctrl Pts',(-0.393318497199042,2.11996195274014,
10.8076879366028));
#25609=CARTESIAN_POINT('Ctrl Pts',(-0.391757613702059,2.14033015283819,
10.8066595210021));
#25610=CARTESIAN_POINT('Ctrl Pts',(-0.388622714666593,2.1604754135593,10.8056311054015));
#25611=CARTESIAN_POINT('Ctrl Pts',(-0.385488191001509,2.18061826210248,
10.8046028129425));
#25612=CARTESIAN_POINT('Ctrl Pts',(-0.380780088998554,2.20053747030646,
10.8035745204835));
#25613=CARTESIAN_POINT('Ctrl Pts',(-0.374555819724814,2.21997011257089,
10.8025462280245));
#25614=CARTESIAN_POINT('Ctrl Pts',(-0.36833302776285,2.23939814255555,10.8015181796277));
#25615=CARTESIAN_POINT('Ctrl Pts',(-0.360595024438406,2.25833911782682,
10.8004901312308));
#25616=CARTESIAN_POINT('Ctrl Pts',(-0.35144880686354,2.27654638527649,10.799462082834));
#25617=CARTESIAN_POINT('Ctrl Pts',(-0.342281589741461,2.29479545627711,
10.7984316740569));
#25618=CARTESIAN_POINT('Ctrl Pts',(-0.331700065682448,2.31230678743153,
10.7974012652799));
#25619=CARTESIAN_POINT('Ctrl Pts',(-0.31985720867979,2.3288585940173,10.7963708565029));
#25620=CARTESIAN_POINT('Ctrl Pts',(-0.308573907301469,2.34462835481243,
10.7953891328553));
#25621=CARTESIAN_POINT('Ctrl Pts',(-0.296146369165086,2.35952691372295,
10.7944074092077));
#25622=CARTESIAN_POINT('Ctrl Pts',(-0.282739281461414,2.37339237136153,
10.7934256855602));
#25623=CARTESIAN_POINT('Ctrl Pts',(-0.268482215524499,2.38813686682304,
10.7923817229126));
#25624=CARTESIAN_POINT('Ctrl Pts',(-0.253026204402658,2.40180705990591,
10.7913377602651));
#25625=CARTESIAN_POINT('Ctrl Pts',(-0.236559080309437,2.41420485598277,
10.7902937976175));
#25626=CARTESIAN_POINT('Ctrl Pts',(-0.220122249265415,2.42657984497781,
10.7892517554518));
#25627=CARTESIAN_POINT('Ctrl Pts',(-0.202678542778262,2.43768659812352,
10.788209713286));
#25628=CARTESIAN_POINT('Ctrl Pts',(-0.18445061904708,2.44736559866105,10.7871676711202));
#25629=CARTESIAN_POINT('Ctrl Pts',(-0.166242271819633,2.45703420410405,
10.7861267480914));
#25630=CARTESIAN_POINT('Ctrl Pts',(-0.147252012376544,2.46527773221188,
10.7850858250625));
#25631=CARTESIAN_POINT('Ctrl Pts',(-0.127729021236514,2.47198143385653,
10.7840449020336));
#25632=CARTESIAN_POINT('Ctrl Pts',(-0.108196003597072,2.47868857834763,
10.7830034444139));
#25633=CARTESIAN_POINT('Ctrl Pts',(-0.0881303983353836,2.48385406230473,
10.7819619867941));
#25634=CARTESIAN_POINT('Ctrl Pts',(-0.0677991812195428,2.48741213329729,
10.7809205291743));
#25635=CARTESIAN_POINT('Ctrl Pts',(-0.0474617520304963,2.49097129143566,
10.7798787533438));
#25636=CARTESIAN_POINT('Ctrl Pts',(-0.0268592798146348,2.49292196778493,
10.7788369775133));
#25637=CARTESIAN_POINT('Ctrl Pts',(-0.00626568814791708,2.49325008728802,
10.7777952016828));
#25638=CARTESIAN_POINT('Ctrl Pts',(0.014372417034512,2.49357891602885,10.7767511740302));
#25639=CARTESIAN_POINT('Ctrl Pts',(0.0350008683268066,2.4922782323283,10.7757071463776));
#25640=CARTESIAN_POINT('Ctrl Pts',(0.0553482843194677,2.48938600054816,
10.774663118725));
#25641=CARTESIAN_POINT('Ctrl Pts',(0.0625448986472379,2.48836305607817,
10.7742938598291));
#25642=CARTESIAN_POINT('Ctrl Pts',(0.0697064488265022,2.48714148611739,
10.7739246009332));
#25643=CARTESIAN_POINT('Ctrl Pts',(0.0768213189330443,2.48572448063014,
10.7735553420374));
#25644=CARTESIAN_POINT('Ctrl Pts',(0.0969363621086848,2.48171834613584,
10.7725113793898));
#25645=CARTESIAN_POINT('Ctrl Pts',(0.116797123301805,2.4761225777747,10.7714674167423));
#25646=CARTESIAN_POINT('Ctrl Pts',(0.13613536403185,2.46898787603377,10.7704234540947));
#25647=CARTESIAN_POINT('Ctrl Pts',(0.155438029984263,2.4618662993455,10.7693814119289));
#25648=CARTESIAN_POINT('Ctrl Pts',(0.174219380398024,2.45321160477635,10.7683393697632));
#25649=CARTESIAN_POINT('Ctrl Pts',(0.192224761819899,2.44312465802283,10.7672973275974));
#25650=CARTESIAN_POINT('Ctrl Pts',(0.210210805744975,2.43304854449166,10.7662564045685));
#25651=CARTESIAN_POINT('Ctrl Pts',(0.227421882342083,2.42154356505889,10.7652154815397));
#25652=CARTESIAN_POINT('Ctrl Pts',(0.24362662257272,2.40875711938967,10.7641745585108));
#25653=CARTESIAN_POINT('Ctrl Pts',(0.259839685135593,2.39596410693522,10.763133100891));
#25654=CARTESIAN_POINT('Ctrl Pts',(0.275044791222169,2.38188875656924,10.7620916432713));
#25655=CARTESIAN_POINT('Ctrl Pts',(0.289042136204373,2.36671995331886,10.7610501856515));
#25656=CARTESIAN_POINT('Ctrl Pts',(0.303043757985698,2.35154651533778,10.760008409821));
#25657=CARTESIAN_POINT('Ctrl Pts',(0.315836412059314,2.33527952417846,10.7589666339905));
#25658=CARTESIAN_POINT('Ctrl Pts',(0.327259984084065,2.31814168060528,10.75792485816));
#25659=CARTESIAN_POINT('Ctrl Pts',(0.338708248418983,2.30096679319431,10.7568808305074));
#25660=CARTESIAN_POINT('Ctrl Pts',(0.348781163692602,2.28291793841907,10.7558368028548));
#25661=CARTESIAN_POINT('Ctrl Pts',(0.357363747359534,2.26424384942259,10.7547927752022));
#25662=CARTESIAN_POINT('Ctrl Pts',(0.360399294704181,2.2576390689198,10.7544235163063));
#25663=CARTESIAN_POINT('Ctrl Pts',(0.363248853322744,2.25095625141377,10.7540542574104));
#25664=CARTESIAN_POINT('Ctrl Pts',(0.365908817484673,2.24420689056688,10.7536849985146));
#25665=CARTESIAN_POINT('Ctrl Pts',(0.373429024201246,2.2251252091293,10.752641035867));
#25666=CARTESIAN_POINT('Ctrl Pts',(0.379474990869443,2.2053968350004,10.7515970732195));
#25667=CARTESIAN_POINT('Ctrl Pts',(0.38394414503024,2.18527475298703,10.7505531105719));
#25668=CARTESIAN_POINT('Ctrl Pts',(0.388405077700381,2.16518968771178,10.7495110684061));
#25669=CARTESIAN_POINT('Ctrl Pts',(0.391294739886095,2.14471304946467,10.7484690262404));
#25670=CARTESIAN_POINT('Ctrl Pts',(0.392560092755418,2.12411355585263,10.7474269840746));
#25671=CARTESIAN_POINT('Ctrl Pts',(0.393824086655637,2.10353618577312,10.7463860610457));
#25672=CARTESIAN_POINT('Ctrl Pts',(0.393467160705411,2.08283695116777,10.7453451380169));
#25673=CARTESIAN_POINT('Ctrl Pts',(0.391488006941209,2.06229018136877,10.744304214988));
#25674=CARTESIAN_POINT('Ctrl Pts',(0.389507836735216,2.04173285928432,10.7432627573682));
#25675=CARTESIAN_POINT('Ctrl Pts',(0.385903828800499,2.0213288923701,10.7422212997484));
#25676=CARTESIAN_POINT('Ctrl Pts',(0.380726643194315,2.00134852681288,10.7411798421287));
#25677=CARTESIAN_POINT('Ctrl Pts',(0.375547875732224,1.98136205638293,10.7401380662982));
#25678=CARTESIAN_POINT('Ctrl Pts',(0.368795193113627,1.9618001475528,10.7390962904676));
#25679=CARTESIAN_POINT('Ctrl Pts',(0.360569173342583,1.94291797927501,10.7380545146372));
#25680=CARTESIAN_POINT('Ctrl Pts',(0.352325372843132,1.92399499676199,10.7370104869846));
#25681=CARTESIAN_POINT('Ctrl Pts',(0.342602223638086,1.90575533803863,10.735966459332));
#25682=CARTESIAN_POINT('Ctrl Pts',(0.331546622878107,1.88843032623241,10.7349224316794));
#25683=CARTESIAN_POINT('Ctrl Pts',(0.327636401803429,1.8823026966486,10.7345531727835));
#25684=CARTESIAN_POINT('Ctrl Pts',(0.3235598867612,1.87628920687579,10.7341839138876));
#25685=CARTESIAN_POINT('Ctrl Pts',(0.319324789981441,1.87039911040393,10.7338146549918));
#25686=CARTESIAN_POINT('Ctrl Pts',(0.307351394360173,1.85374672700571,10.7327706923442));
#25687=CARTESIAN_POINT('Ctrl Pts',(0.294036215169403,1.83798384459672,10.7317267296967));
#25688=CARTESIAN_POINT('Ctrl Pts',(0.279536442238813,1.82333365318408,10.7306827670491));
#25689=CARTESIAN_POINT('Ctrl Pts',(0.265063343202964,1.80871041237719,10.7296407248833));
#25690=CARTESIAN_POINT('Ctrl Pts',(0.249410445497218,1.79519635840129,10.7285986827176));
#25691=CARTESIAN_POINT('Ctrl Pts',(0.232774980818624,1.78298154895198,10.7275566405518));
#25692=CARTESIAN_POINT('Ctrl Pts',(0.216157382367754,1.77077985801612,10.7265157175229));
#25693=CARTESIAN_POINT('Ctrl Pts',(0.198559884838435,1.75987509804229,10.7254747944941));
#25694=CARTESIAN_POINT('Ctrl Pts',(0.180212441220589,1.75041686821399,10.7244338714652));
#25695=CARTESIAN_POINT('Ctrl Pts',(0.1618555748339,1.74095378088536,10.7233924138454));
#25696=CARTESIAN_POINT('Ctrl Pts',(0.142748639516621,1.73293905931746,10.7223509562257));
#25697=CARTESIAN_POINT('Ctrl Pts',(0.123146286305556,1.72647639677103,10.7213094986059));
#25698=CARTESIAN_POINT('Ctrl Pts',(0.103537943720977,1.72001175959945,10.7202677227754));
#25699=CARTESIAN_POINT('Ctrl Pts',(0.0834345914179953,1.71510032133677,
10.7192259469449));
#25700=CARTESIAN_POINT('Ctrl Pts',(0.0631052331196161,1.71179564717417,
10.7181841711144));
#25701=CARTESIAN_POINT('Ctrl Pts',(0.0427319324519695,1.70848382988339,
10.7171401434618));
#25702=CARTESIAN_POINT('Ctrl Pts',(0.0221323844766809,1.7067857709853,10.7160961158092));
#25703=CARTESIAN_POINT('Ctrl Pts',(0.00158060790296777,1.7067031761142,
10.7150520881566));
#25704=CARTESIAN_POINT('Ctrl Pts',(-0.005688286083539,1.70667396339093,
10.7146828292607));
#25705=CARTESIAN_POINT('Ctrl Pts',(-0.0129512272027228,1.70684635955504,
10.7143135703649));
#25706=CARTESIAN_POINT('Ctrl Pts',(-0.0201962601851129,1.70721888910675,
10.713944311469));
#25707=CARTESIAN_POINT('Ctrl Pts',(-0.0406792976923341,1.70827209849846,
10.7129003488214));
#25708=CARTESIAN_POINT('Ctrl Pts',(-0.0611407585325059,1.71093500649694,
10.7118563861739));
#25709=CARTESIAN_POINT('Ctrl Pts',(-0.081307890856511,1.71519626186267,
10.7108124235263));
#25710=CARTESIAN_POINT('Ctrl Pts',(-0.101437923567479,1.71944967818997,
10.7097703813606));
#25711=CARTESIAN_POINT('Ctrl Pts',(-0.121273978469272,1.72529551323584,
10.7087283391948));
#25712=CARTESIAN_POINT('Ctrl Pts',(-0.140549486567197,1.73267081272284,
10.707686297029));
#25713=CARTESIAN_POINT('Ctrl Pts',(-0.159804293072227,1.74003819125405,
10.7066453740002));
#25714=CARTESIAN_POINT('Ctrl Pts',(-0.178499053880445,1.74893153863871,
10.7056044509713));
#25715=CARTESIAN_POINT('Ctrl Pts',(-0.196383505611462,1.75923848702685,
10.7045635279425));
#25716=CARTESIAN_POINT('Ctrl Pts',(-0.21427714233077,1.76955072879504,10.7035220703227));
#25717=CARTESIAN_POINT('Ctrl Pts',(-0.231358993051381,1.78127766850619,
10.7024806127029));
#25718=CARTESIAN_POINT('Ctrl Pts',(-0.247404023415605,1.79426132204484,
10.7014391550831));
#25719=CARTESIAN_POINT('Ctrl Pts',(-0.263453956236107,1.80724894265568,
10.7003973792526));
#25720=CARTESIAN_POINT('Ctrl Pts',(-0.278465889309764,1.82149355093451,
10.6993556034221));
#25721=CARTESIAN_POINT('Ctrl Pts',(-0.29224916748893,1.83679795954053,10.6983138275916));
#25722=CARTESIAN_POINT('Ctrl Pts',(-0.306062238536659,1.85213544897305,
10.697269799939));
#25723=CARTESIAN_POINT('Ctrl Pts',(-0.318640904390109,1.86853672776939,
10.6962257722865));
#25724=CARTESIAN_POINT('Ctrl Pts',(-0.329835399642932,1.88577231938335,
10.6951817446339));
#25725=CARTESIAN_POINT('Ctrl Pts',(-0.333794745879168,1.89186832221732,
10.694812485738));
#25726=CARTESIAN_POINT('Ctrl Pts',(-0.337581353358565,1.89806845430745,
10.6944432268421));
#25727=CARTESIAN_POINT('Ctrl Pts',(-0.341189991104376,1.90436186473441,
10.6940739679463));
#25728=CARTESIAN_POINT('Ctrl Pts',(-0.351815332896677,1.92289230240535,
10.6929867150118));
#25729=CARTESIAN_POINT('Ctrl Pts',(-0.360953204524888,1.94233564316304,
10.6918994620774));
#25730=CARTESIAN_POINT('Ctrl Pts',(-0.368457924284301,1.96243674897668,
10.690812209143));
#25731=CARTESIAN_POINT('Ctrl Pts',(-0.375943138005039,1.98248560860926,
10.6897277821632));
#25732=CARTESIAN_POINT('Ctrl Pts',(-0.381803353160854,2.00318825710798,
10.6886433551834));
#25733=CARTESIAN_POINT('Ctrl Pts',(-0.385939644202044,2.02426704130169,
10.6875589282036));
#25734=CARTESIAN_POINT('Ctrl Pts',(-0.390065058944618,2.04529039923331,
10.686477352704));
#25735=CARTESIAN_POINT('Ctrl Pts',(-0.392475396073696,2.06668730305621,
10.6853957772043));
#25736=CARTESIAN_POINT('Ctrl Pts',(-0.393121944047708,2.0881666949608,10.6843142017047));
#25737=CARTESIAN_POINT('Ctrl Pts',(-0.393241072234284,2.09212433013901,
10.6841149185376));
#25738=CARTESIAN_POINT('Ctrl Pts',(-0.393300461280009,2.09608473789163,
10.6839156353706));
#25739=CARTESIAN_POINT('Ctrl Pts',(-0.393299997302219,2.10004606598081,
10.6837163522035));
#25740=CARTESIAN_POINT('',(-0.393315863656476,2.10034160400655,10.558716360067));
#25741=CARTESIAN_POINT('Ctrl Pts',(-0.392657465061904,2.10004663893747,
10.6837163195403));
#25742=CARTESIAN_POINT('Ctrl Pts',(-0.392722889128489,2.16297443070521,
10.680545421168));
#25743=CARTESIAN_POINT('Ctrl Pts',(-0.348724163651497,2.357260709504,10.6707510749546));
#25744=CARTESIAN_POINT('Ctrl Pts',(-0.0435775851074158,2.56300757829187,
10.6543332809008));
#25745=CARTESIAN_POINT('Ctrl Pts',(0.365715727477674,2.38727518193357,10.6344629373778));
#25746=CARTESIAN_POINT('Ctrl Pts',(0.439514647802459,1.94800691513575,10.6145925938551));
#25747=CARTESIAN_POINT('Ctrl Pts',(0.110118713284817,1.64817161171085,10.5947222503322));
#25748=CARTESIAN_POINT('Ctrl Pts',(-0.293328879552519,1.75564368824555,
10.5760968659443));
#25749=CARTESIAN_POINT('Ctrl Pts',(-0.392508382890038,1.99416607365442,
10.5640949293972));
#25750=CARTESIAN_POINT('Ctrl Pts',(-0.39348003609742,2.1003401551118,10.558716440691));
#25751=CARTESIAN_POINT('',(-0.393299933137644,2.09977066634666,10.433716352199));
#25752=CARTESIAN_POINT('Ctrl Pts',(-0.393299851525698,2.10034174532072,
10.5587163522035));
#25753=CARTESIAN_POINT('Ctrl Pts',(-0.393278507363976,2.12490581431345,
10.5574714225646));
#25754=CARTESIAN_POINT('Ctrl Pts',(-0.390954482254135,2.14937301694214,
10.5562264929256));
#25755=CARTESIAN_POINT('Ctrl Pts',(-0.386389811003518,2.17340166178409,
10.5549815632866));
#25756=CARTESIAN_POINT('Ctrl Pts',(-0.382562007298867,2.19355140109584,
10.553937600639));
#25757=CARTESIAN_POINT('Ctrl Pts',(-0.377142379728278,2.21346094894873,
10.5528936379915));
#25758=CARTESIAN_POINT('Ctrl Pts',(-0.370179250805663,2.2328616282941,10.5518496753439));
#25759=CARTESIAN_POINT('Ctrl Pts',(-0.363228931309024,2.25222661799925,
10.5508076331781));
#25760=CARTESIAN_POINT('Ctrl Pts',(-0.354740936404027,2.27108389256192,
10.5497655910124));
#25761=CARTESIAN_POINT('Ctrl Pts',(-0.344813872178568,2.2891779150779,10.5487235488466));
#25762=CARTESIAN_POINT('Ctrl Pts',(-0.334897469464141,2.30725250489794,
10.5476826258178));
#25763=CARTESIAN_POINT('Ctrl Pts',(-0.323545392451628,2.32456481430114,
10.546641702789));
#25764=CARTESIAN_POINT('Ctrl Pts',(-0.310902985619106,2.34088217769924,
10.5456007797601));
#25765=CARTESIAN_POINT('Ctrl Pts',(-0.298254085975937,2.35720792126989,
10.5445593221404));
#25766=CARTESIAN_POINT('Ctrl Pts',(-0.284313970521364,2.37253710651023,
10.5435178645206));
#25767=CARTESIAN_POINT('Ctrl Pts',(-0.269269747056953,2.38666826353799,
10.5424764069009));
#25768=CARTESIAN_POINT('Ctrl Pts',(-0.254220926926409,2.40080373825028,
10.5414346310704));
#25769=CARTESIAN_POINT('Ctrl Pts',(-0.238067887808363,2.41373997908236,
10.5403928552399));
#25770=CARTESIAN_POINT('Ctrl Pts',(-0.221031903480885,2.42531490535113,
10.5393510794095));
#25771=CARTESIAN_POINT('Ctrl Pts',(-0.203959095486683,2.43691485108571,
10.5383070517569));
#25772=CARTESIAN_POINT('Ctrl Pts',(-0.18600017194333,2.44714724308179,10.5372630241043));
#25773=CARTESIAN_POINT('Ctrl Pts',(-0.167402837751568,2.45589490009372,
10.5362189964518));
#25774=CARTESIAN_POINT('Ctrl Pts',(-0.160825204415708,2.45898883171742,
10.5358497375558));
#25775=CARTESIAN_POINT('Ctrl Pts',(-0.154167889700035,2.46189747314211,
10.5354804786599));
#25776=CARTESIAN_POINT('Ctrl Pts',(-0.147442354877446,2.46461711697093,
10.535111219764));
#25777=CARTESIAN_POINT('Ctrl Pts',(-0.128428033985807,2.47230604905385,
10.5340672571164));
#25778=CARTESIAN_POINT('Ctrl Pts',(-0.108753987352186,2.47852652715294,
10.5330232944689));
#25779=CARTESIAN_POINT('Ctrl Pts',(-0.0886722812995241,2.48317374196197,
10.5319793318213));
#25780=CARTESIAN_POINT('Ctrl Pts',(-0.0686275177090747,2.48781240771859,
10.5309372896556));
#25781=CARTESIAN_POINT('Ctrl Pts',(-0.0481772786181898,2.49088333308022,
10.5298952474898));
#25782=CARTESIAN_POINT('Ctrl Pts',(-0.0275898012882309,2.49233110106755,
10.528853205324));
#25783=CARTESIAN_POINT('Ctrl Pts',(-0.00702443458549785,2.49377731417481,
10.5278122822952));
#25784=CARTESIAN_POINT('Ctrl Pts',(0.0136771495331234,2.49360375046415,
10.5267713592663));
#25785=CARTESIAN_POINT('Ctrl Pts',(0.0342406440830859,2.49180667208813,
10.5257304362375));
#25786=CARTESIAN_POINT('Ctrl Pts',(0.0548146995078923,2.49000867077949,
10.5246889786177));
#25787=CARTESIAN_POINT('Ctrl Pts',(0.0752497892952924,2.4865855370673,10.5236475209979));
#25788=CARTESIAN_POINT('Ctrl Pts',(0.0952752291272609,2.48158553525356,
10.5226060633781));
#25789=CARTESIAN_POINT('Ctrl Pts',(0.115306787604137,2.47658400572129,10.5215642875475));
#25790=CARTESIAN_POINT('Ctrl Pts',(0.13492774245287,2.47000486212578,10.520522511717));
#25791=CARTESIAN_POINT('Ctrl Pts',(0.153882033838918,2.46194641821905,10.5194807358865));
#25792=CARTESIAN_POINT('Ctrl Pts',(0.172877295355929,2.45387055580294,10.5184367082339));
#25793=CARTESIAN_POINT('Ctrl Pts',(0.191202363562223,2.44430935001895,10.5173926805813));
#25794=CARTESIAN_POINT('Ctrl Pts',(0.208624623229872,2.43340764325701,10.5163486529287));
#25795=CARTESIAN_POINT('Ctrl Pts',(0.214786648107508,2.42955185247228,10.5159793940328));
#25796=CARTESIAN_POINT('Ctrl Pts',(0.220836010639008,2.42552876322413,10.515610135137));
#25797=CARTESIAN_POINT('Ctrl Pts',(0.226763389384609,2.4213460054751,10.5152408762411));
#25798=CARTESIAN_POINT('Ctrl Pts',(0.24352117661115,2.40952058189637,10.5141969135936));
#25799=CARTESIAN_POINT('Ctrl Pts',(0.259401382900948,2.39634554842707,10.513152950946));
#25800=CARTESIAN_POINT('Ctrl Pts',(0.27417943465761,2.38197611177338,10.5121089882984));
#25801=CARTESIAN_POINT('Ctrl Pts',(0.288930300595645,2.3676331092468,10.5110669461327));
#25802=CARTESIAN_POINT('Ctrl Pts',(0.302582473555006,2.35210052945659,10.5100249039669));
#25803=CARTESIAN_POINT('Ctrl Pts',(0.314944156270969,2.33557391288249,10.5089828618011));
#25804=CARTESIAN_POINT('Ctrl Pts',(0.32729256273389,2.31906504563497,10.5079419387722));
#25805=CARTESIAN_POINT('Ctrl Pts',(0.338352768795716,2.30156482988624,10.5069010157434));
#25806=CARTESIAN_POINT('Ctrl Pts',(0.347973144280237,2.28330188449584,10.5058600927145));
#25807=CARTESIAN_POINT('Ctrl Pts',(0.35759846053887,2.26502955973267,10.5048186350947));
#25808=CARTESIAN_POINT('Ctrl Pts',(0.365782111765119,2.24599436623121,10.5037771774749));
#25809=CARTESIAN_POINT('Ctrl Pts',(0.37241815313595,2.22645002655123,10.5027357198551));
#25810=CARTESIAN_POINT('Ctrl Pts',(0.379056222106729,2.20689971522342,10.5016939440246));
#25811=CARTESIAN_POINT('Ctrl Pts',(0.384145537763884,2.18684065577966,10.5006521681941));
#25812=CARTESIAN_POINT('Ctrl Pts',(0.387630154255204,2.16654136692379,10.4996103923636));
#25813=CARTESIAN_POINT('Ctrl Pts',(0.391122302824145,2.14619820069441,10.498566364711));
#25814=CARTESIAN_POINT('Ctrl Pts',(0.393002760346493,2.1256145017966,10.4975223370585));
#25815=CARTESIAN_POINT('Ctrl Pts',(0.393267394071057,2.10506426308162,10.4964783094059));
#25816=CARTESIAN_POINT('Ctrl Pts',(0.393360991550679,2.09779591301583,10.49610905051));
#25817=CARTESIAN_POINT('Ctrl Pts',(0.393252935323244,2.09053172978668,10.4957397916141));
#25818=CARTESIAN_POINT('Ctrl Pts',(0.392944594934099,2.08328368126421,10.4953705327183));
#25819=CARTESIAN_POINT('Ctrl Pts',(0.39207286008191,2.06279211827132,10.4943265700707));
#25820=CARTESIAN_POINT('Ctrl Pts',(0.389591298651868,2.04230787282293,10.4932826074232));
#25821=CARTESIAN_POINT('Ctrl Pts',(0.385508845475885,2.02210378661417,10.4922386447756));
#25822=CARTESIAN_POINT('Ctrl Pts',(0.381433902412427,2.00193686799911,10.4911966026099));
#25823=CARTESIAN_POINT('Ctrl Pts',(0.375763999125586,1.98204981044483,10.4901545604441));
#25824=CARTESIAN_POINT('Ctrl Pts',(0.368559726226817,1.9627097301204,10.4891125182784));
#25825=CARTESIAN_POINT('Ctrl Pts',(0.361363190603966,1.94339042073842,10.4880715952495));
#25826=CARTESIAN_POINT('Ctrl Pts',(0.3526357852584,1.92461761846187,10.4870306722207));
#25827=CARTESIAN_POINT('Ctrl Pts',(0.342487656866335,1.90664257217731,10.4859897491918));
#25828=CARTESIAN_POINT('Ctrl Pts',(0.332334316660019,1.88865829437746,10.484948291572));
#25829=CARTESIAN_POINT('Ctrl Pts',(0.320759143428588,1.87147323971675,10.4839068339522));
#25830=CARTESIAN_POINT('Ctrl Pts',(0.307918121796048,1.85531383310536,10.4828653763325));
#25831=CARTESIAN_POINT('Ctrl Pts',(0.295073176671582,1.83914948909075,10.481823600502));
#25832=CARTESIAN_POINT('Ctrl Pts',(0.280962098869543,1.82401197004405,10.4807818246715));
#25833=CARTESIAN_POINT('Ctrl Pts',(0.26578037922311,1.81009367026569,10.479740048841));
#25834=CARTESIAN_POINT('Ctrl Pts',(0.250565843945142,1.7961452857665,10.4786960211884));
#25835=CARTESIAN_POINT('Ctrl Pts',(0.234276627008033,1.78342183527605,10.4776519935358));
#25836=CARTESIAN_POINT('Ctrl Pts',(0.217140869373926,1.77207511096665,10.4766079658832));
#25837=CARTESIAN_POINT('Ctrl Pts',(0.21108017650993,1.76806192330841,10.4762387069873));
#25838=CARTESIAN_POINT('Ctrl Pts',(0.204913828401495,1.76422054528154,10.4758694480915));
#25839=CARTESIAN_POINT('Ctrl Pts',(0.198652629207673,1.76055630377207,10.4755001891956));
#25840=CARTESIAN_POINT('Ctrl Pts',(0.180951070327685,1.75019682073656,10.474456226548));
#25841=CARTESIAN_POINT('Ctrl Pts',(0.162384235955808,1.74119486982972,10.4734122639005));
#25842=CARTESIAN_POINT('Ctrl Pts',(0.143186372860344,1.73369063262442,10.4723683012529));
#25843=CARTESIAN_POINT('Ctrl Pts',(0.124023826302726,1.72620020027209,10.4713262590872));
#25844=CARTESIAN_POINT('Ctrl Pts',(0.104233211147734,1.72020233288133,10.4702842169214));
#25845=CARTESIAN_POINT('Ctrl Pts',(0.0840719222456602,1.71579067958999,
10.4692421747556));
#25846=CARTESIAN_POINT('Ctrl Pts',(0.0639322862511359,1.71138376434499,
10.4682012517268));
#25847=CARTESIAN_POINT('Ctrl Pts',(0.0434234757737663,1.70855986594305,
10.4671603286979));
#25848=CARTESIAN_POINT('Ctrl Pts',(0.0228163697618803,1.70736237664879,
10.466119405669));
#25849=CARTESIAN_POINT('Ctrl Pts',(0.00219868047744025,1.70616427235523,
10.4650779480493));
#25850=CARTESIAN_POINT('Ctrl Pts',(-0.0185166715893972,1.7065943046525,
10.4640364904295));
#25851=CARTESIAN_POINT('Ctrl Pts',(-0.0390548670247227,1.70864388677104,
10.4629950328097));
#25852=CARTESIAN_POINT('Ctrl Pts',(-0.0595993377741394,1.71069409512627,
10.4619532569792));
#25853=CARTESIAN_POINT('Ctrl Pts',(-0.079965816201812,1.7143647294148,10.4609114811487));
#25854=CARTESIAN_POINT('Ctrl Pts',(-0.0998867110149369,1.71959556395513,
10.4598697053182));
#25855=CARTESIAN_POINT('Ctrl Pts',(-0.119850665294266,1.72483770506302,
10.4588256776656));
#25856=CARTESIAN_POINT('Ctrl Pts',(-0.139366417727724,1.73164653666351,
10.457781650013));
#25857=CARTESIAN_POINT('Ctrl Pts',(-0.158182841914016,1.73991240159649,
10.4567376223604));
#25858=CARTESIAN_POINT('Ctrl Pts',(-0.164837964507673,1.74283592967638,
10.4563683634645));
#25859=CARTESIAN_POINT('Ctrl Pts',(-0.171405819580025,1.74594129823533,
10.4559991045686));
#25860=CARTESIAN_POINT('Ctrl Pts',(-0.177876079703393,1.74922230648265,
10.4556298456728));
#25861=CARTESIAN_POINT('Ctrl Pts',(-0.196168692188443,1.75849831877336,
10.4545858830252));
#25862=CARTESIAN_POINT('Ctrl Pts',(-0.213788256612227,1.76923672686017,
10.4535419203776));
#25863=CARTESIAN_POINT('Ctrl Pts',(-0.23049010379015,1.78131645468458,10.4524979577301));
#25864=CARTESIAN_POINT('Ctrl Pts',(-0.247161226120462,1.79337396054799,
10.4514559155643));
#25865=CARTESIAN_POINT('Ctrl Pts',(-0.262917357987864,1.80676751011588,
10.4504138733986));
#25866=CARTESIAN_POINT('Ctrl Pts',(-0.277540425037224,1.82133137516011,
10.4493718312328));
#25867=CARTESIAN_POINT('Ctrl Pts',(-0.292147787142294,1.83587959884206,
10.4483309082039));
#25868=CARTESIAN_POINT('Ctrl Pts',(-0.305623961160892,1.85159514665949,
10.4472899851751));
#25869=CARTESIAN_POINT('Ctrl Pts',(-0.31778583043083,1.86827374775959,10.4462490621462));
#25870=CARTESIAN_POINT('Ctrl Pts',(-0.329953945719849,1.88496091455451,
10.4452076045264));
#25871=CARTESIAN_POINT('Ctrl Pts',(-0.340805961241281,1.90261153772065,
10.4441661469066));
#25872=CARTESIAN_POINT('Ctrl Pts',(-0.350200332190293,1.92098989600079,
10.4431246892868));
#25873=CARTESIAN_POINT('Ctrl Pts',(-0.359597573529192,1.93937386967062,
10.4420829134563));
#25874=CARTESIAN_POINT('Ctrl Pts',(-0.367535981270759,1.95848535004642,
10.4410411376258));
#25875=CARTESIAN_POINT('Ctrl Pts',(-0.373921342244449,1.97806674032853,
10.4399993617953));
#25876=CARTESIAN_POINT('Ctrl Pts',(-0.380320505320784,1.99769045623009,
10.4389553341427));
#25877=CARTESIAN_POINT('Ctrl Pts',(-0.385159747222649,2.01778539386682,
10.4379113064901));
#25878=CARTESIAN_POINT('Ctrl Pts',(-0.388395330395011,2.03808104226208,
10.4368672788375));
#25879=CARTESIAN_POINT('Ctrl Pts',(-0.389539713751837,2.04525934706906,
10.4364980199417));
#25880=CARTESIAN_POINT('Ctrl Pts',(-0.390483962892018,2.05246270931861,
10.4361287610458));
#25881=CARTESIAN_POINT('Ctrl Pts',(-0.391227701128192,2.05967908892461,
10.4357595021499));
#25882=CARTESIAN_POINT('Ctrl Pts',(-0.392599429522958,2.07298876204814,
10.4350784521678));
#25883=CARTESIAN_POINT('Ctrl Pts',(-0.393292118961807,2.08636960809798,
10.4343974021856));
#25884=CARTESIAN_POINT('Ctrl Pts',(-0.393299933137593,2.09977066625803,
10.4337163522035));
#25885=CARTESIAN_POINT('',(-0.393113345386621,2.09978390338552,10.3087163551585));
#25886=CARTESIAN_POINT('Ctrl Pts',(-0.393299933137644,2.09977066634666,
10.433716352199));
#25887=CARTESIAN_POINT('Ctrl Pts',(-0.393311752893345,2.12004117204569,
10.4326861926862));
#25888=CARTESIAN_POINT('Ctrl Pts',(-0.391752186310895,2.14037481072923,
10.4316560331735));
#25889=CARTESIAN_POINT('Ctrl Pts',(-0.388618245869949,2.16050412363603,
10.4306258736607));
#25890=CARTESIAN_POINT('Ctrl Pts',(-0.385489406275611,2.18060067378317,
10.4295973908504));
#25891=CARTESIAN_POINT('Ctrl Pts',(-0.380791337052907,2.20049280953543,
10.4285689080402));
#25892=CARTESIAN_POINT('Ctrl Pts',(-0.374572916412325,2.2199167223133,10.4275404252299));
#25893=CARTESIAN_POINT('Ctrl Pts',(-0.3683544003717,2.23934093308357,10.4265119266411));
#25894=CARTESIAN_POINT('Ctrl Pts',(-0.360615672076591,2.25829617333842,
10.4254834280523));
#25895=CARTESIAN_POINT('Ctrl Pts',(-0.351455954974451,2.27653215489818,
10.4244549294635));
#25896=CARTESIAN_POINT('Ctrl Pts',(-0.342297215870464,2.29476618937202,
10.4234265406892));
#25897=CARTESIAN_POINT('Ctrl Pts',(-0.331718144692482,2.31228044926094,
10.4223981519149));
#25898=CARTESIAN_POINT('Ctrl Pts',(-0.319864204852919,2.32884881571424,
10.4213697631407));
#25899=CARTESIAN_POINT('Ctrl Pts',(-0.307983831395344,2.34545412869129,
10.4203390811173));
#25900=CARTESIAN_POINT('Ctrl Pts',(-0.294823383852538,2.36110874111289,
10.419308399094));
#25901=CARTESIAN_POINT('Ctrl Pts',(-0.280569475804279,2.37561868450254,
10.4182777170707));
#25902=CARTESIAN_POINT('Ctrl Pts',(-0.269558549170975,2.38682739453322,
10.4174815309229));
#25903=CARTESIAN_POINT('Ctrl Pts',(-0.257896023166036,2.39735367684374,
10.416685344775));
#25904=CARTESIAN_POINT('Ctrl Pts',(-0.245681167609966,2.40712481808184,
10.4158891586271));
#25905=CARTESIAN_POINT('Ctrl Pts',(-0.229664997296023,2.41993677983715,
10.4148451959796));
#25906=CARTESIAN_POINT('Ctrl Pts',(-0.212596216216608,2.43153070804052,
10.413801233332));
#25907=CARTESIAN_POINT('Ctrl Pts',(-0.194686320575257,2.44173399974376,
10.4127572706845));
#25908=CARTESIAN_POINT('Ctrl Pts',(-0.176809372116842,2.45191852139245,
10.4117152285187));
#25909=CARTESIAN_POINT('Ctrl Pts',(-0.158094983118191,2.46071707274236,
10.4106731863529));
#25910=CARTESIAN_POINT('Ctrl Pts',(-0.138784287729845,2.46799974385768,
10.4096311441872));
#25911=CARTESIAN_POINT('Ctrl Pts',(-0.119494331724977,2.47527459349864,
10.4085902211583));
#25912=CARTESIAN_POINT('Ctrl Pts',(-0.0996100154754499,2.48103650955752,
10.4075492981295));
#25913=CARTESIAN_POINT('Ctrl Pts',(-0.0793930877577652,2.48520335878116,
10.4065083751006));
#25914=CARTESIAN_POINT('Ctrl Pts',(-0.059165777152929,2.48937234798996,
10.4054669174808));
#25915=CARTESIAN_POINT('Ctrl Pts',(-0.0386062311956818,2.49194446949978,
10.404425459861));
#25916=CARTESIAN_POINT('Ctrl Pts',(-0.0179876193114655,2.49288845179199,
10.4033840022412));
#25917=CARTESIAN_POINT('Ctrl Pts',(0.00263729245758782,2.49383272251194,
10.4023422264108));
#25918=CARTESIAN_POINT('Ctrl Pts',(0.0233205700375492,2.49314786619447,
10.4013004505803));
#25919=CARTESIAN_POINT('Ctrl Pts',(0.0437887236061861,2.49085475267027,
10.4002586747498));
#25920=CARTESIAN_POINT('Ctrl Pts',(0.0643011195532388,2.48855668252915,
10.3992146470972));
#25921=CARTESIAN_POINT('Ctrl Pts',(0.0845967399894148,2.48464355437913,
10.3981706194446));
#25922=CARTESIAN_POINT('Ctrl Pts',(0.104411233674789,2.4791875318131,10.397126591792));
#25923=CARTESIAN_POINT('Ctrl Pts',(0.111419360367839,2.47725780814768,10.3967573328961));
#25924=CARTESIAN_POINT('Ctrl Pts',(0.118367451388828,2.47513552981942,10.3963880740002));
#25925=CARTESIAN_POINT('Ctrl Pts',(0.125244390719619,2.47282533791746,10.3960188151044));
#25926=CARTESIAN_POINT('Ctrl Pts',(0.144686759938549,2.46629400155344,10.3949748524568));
#25927=CARTESIAN_POINT('Ctrl Pts',(0.163674781965691,2.45821826764132,10.3939308898093));
#25928=CARTESIAN_POINT('Ctrl Pts',(0.181948842435384,2.44868253288116,10.3928869271617));
#25929=CARTESIAN_POINT('Ctrl Pts',(0.2001892858017,2.43916434013263,10.3918448849959));
#25930=CARTESIAN_POINT('Ctrl Pts',(0.217717702221878,2.42819176161839,10.3908028428302));
#25931=CARTESIAN_POINT('Ctrl Pts',(0.23429433082323,2.41589722465399,10.3897608006644));
#25932=CARTESIAN_POINT('Ctrl Pts',(0.25085315638588,2.40361589182915,10.3887198776355));
#25933=CARTESIAN_POINT('Ctrl Pts',(0.266461618244414,2.39001583198399,10.3876789546067));
#25934=CARTESIAN_POINT('Ctrl Pts',(0.280908967946815,2.37527266796225,10.3866380315778));
#25935=CARTESIAN_POINT('Ctrl Pts',(0.295363737431475,2.36052193223573,10.385596573958));
#25936=CARTESIAN_POINT('Ctrl Pts',(0.308655676963265,2.34462743373741,10.3845551163382));
#25937=CARTESIAN_POINT('Ctrl Pts',(0.320610621343578,2.32780193037304,10.3835136587185));
#25938=CARTESIAN_POINT('Ctrl Pts',(0.332569218480592,2.31097128608387,10.382471882888));
#25939=CARTESIAN_POINT('Ctrl Pts',(0.343189610904075,2.29320969087407,10.3814301070575));
#25940=CARTESIAN_POINT('Ctrl Pts',(0.352341301358908,2.27475839709929,10.380388331227));
#25941=CARTESIAN_POINT('Ctrl Pts',(0.361512773400334,2.2562672204343,10.3793443035744));
#25942=CARTESIAN_POINT('Ctrl Pts',(0.369208931250333,2.23708405241762,10.3783002759218));
#25943=CARTESIAN_POINT('Ctrl Pts',(0.375347353247155,2.21747022776157,10.3772562482692));
#25944=CARTESIAN_POINT('Ctrl Pts',(0.377518432646495,2.21053307507395,10.3768869893733));
#25945=CARTESIAN_POINT('Ctrl Pts',(0.379495110243685,2.20354216813606,10.3765177304774));
#25946=CARTESIAN_POINT('Ctrl Pts',(0.381275271048106,2.19650936580039,10.3761484715816));
#25947=CARTESIAN_POINT('Ctrl Pts',(0.386308112253202,2.17662634326987,10.375104508934));
#25948=CARTESIAN_POINT('Ctrl Pts',(0.389796450003931,2.15628933369475,10.3740605462865));
#25949=CARTESIAN_POINT('Ctrl Pts',(0.391670712609699,2.13576231094058,10.3730165836389));
#25950=CARTESIAN_POINT('Ctrl Pts',(0.39354152730744,2.11527304985668,10.3719745414731));
#25951=CARTESIAN_POINT('Ctrl Pts',(0.393804035362039,2.09459518848343,10.3709324993074));
#25952=CARTESIAN_POINT('Ctrl Pts',(0.392439797138852,2.07400200735409,10.3698904571416));
#25953=CARTESIAN_POINT('Ctrl Pts',(0.391077024086084,2.05343094297776,10.3688495341127));
#25954=CARTESIAN_POINT('Ctrl Pts',(0.388090992698617,2.03294511065555,10.3678086110839));
#25955=CARTESIAN_POINT('Ctrl Pts',(0.383515287862834,2.01281677927785,10.366767688055));
#25956=CARTESIAN_POINT('Ctrl Pts',(0.378937233064304,1.99267811051376,10.3657262304352));
#25957=CARTESIAN_POINT('Ctrl Pts',(0.372768021184381,1.97289803053894,10.3646847728154));
#25958=CARTESIAN_POINT('Ctrl Pts',(0.365092264110561,1.95373815026937,10.3636433151957));
#25959=CARTESIAN_POINT('Ctrl Pts',(0.357414161758318,1.93457241582108,10.3626015393652));
#25960=CARTESIAN_POINT('Ctrl Pts',(0.348228904812652,1.91602792730111,10.3615597635347));
#25961=CARTESIAN_POINT('Ctrl Pts',(0.337668702051527,1.89834500339729,10.3605179877042));
#25962=CARTESIAN_POINT('Ctrl Pts',(0.327085673172499,1.88062385745219,10.3594739600516));
#25963=CARTESIAN_POINT('Ctrl Pts',(0.315122191346237,1.86376859467168,10.358429932399));
#25964=CARTESIAN_POINT('Ctrl Pts',(0.301953375143129,1.84798998186645,10.3573859047464));
#25965=CARTESIAN_POINT('Ctrl Pts',(0.297295737465664,1.84240929333938,10.3570166458505));
#25966=CARTESIAN_POINT('Ctrl Pts',(0.29248766904401,1.83696296318126,10.3566473869546));
#25967=CARTESIAN_POINT('Ctrl Pts',(0.287537996131034,1.83165918912519,10.3562781280588));
#25968=CARTESIAN_POINT('Ctrl Pts',(0.273544362676087,1.81666444677083,10.3552341654112));
#25969=CARTESIAN_POINT('Ctrl Pts',(0.258332941158418,1.80272259918402,10.3541902027637));
#25970=CARTESIAN_POINT('Ctrl Pts',(0.242088025117285,1.79003503731097,10.3531462401161));
#25971=CARTESIAN_POINT('Ctrl Pts',(0.225872993349701,1.77737081557515,10.3521041979503));
#25972=CARTESIAN_POINT('Ctrl Pts',(0.208628777635873,1.76595679411621,10.3510621557846));
#25973=CARTESIAN_POINT('Ctrl Pts',(0.190575175433659,1.75595640899963,10.3500201136188));
#25974=CARTESIAN_POINT('Ctrl Pts',(0.172540962516603,1.74596676413956,10.3489791905899));
#25975=CARTESIAN_POINT('Ctrl Pts',(0.153699715169682,1.73738812160169,10.3479382675611));
#25976=CARTESIAN_POINT('Ctrl Pts',(0.134298542056594,1.73033962668218,10.3468973445322));
#25977=CARTESIAN_POINT('Ctrl Pts',(0.114887405006638,1.72328751183938,10.3458558869124));
#25978=CARTESIAN_POINT('Ctrl Pts',(0.0949164537524642,1.71776738095022,
10.3448144292927));
#25979=CARTESIAN_POINT('Ctrl Pts',(0.0746514573797654,1.71384970554061,
10.3437729716729));
#25980=CARTESIAN_POINT('Ctrl Pts',(0.0543802691671996,1.70993083311036,
10.3427311958424));
#25981=CARTESIAN_POINT('Ctrl Pts',(0.0338155856402103,1.70761549489314,
10.3416894200119));
#25982=CARTESIAN_POINT('Ctrl Pts',(0.0132310380546688,1.70692261622933,
10.3406476441814));
#25983=CARTESIAN_POINT('Ctrl Pts',(-0.00739800349760471,1.70622823989256,
10.3396036165288));
#25984=CARTESIAN_POINT('Ctrl Pts',(-0.0280462591055306,1.70716329131249,
10.3385595888762));
#25985=CARTESIAN_POINT('Ctrl Pts',(-0.0484417174146762,1.7096946195427,
10.3375155612236));
#25986=CARTESIAN_POINT('Ctrl Pts',(-0.0556553236799815,1.7105899171577,
10.3371463023277));
#25987=CARTESIAN_POINT('Ctrl Pts',(-0.0628373899030118,1.71168443024859,
10.3367770434319));
#25988=CARTESIAN_POINT('Ctrl Pts',(-0.0699762454728388,1.712975175125,10.336407784536));
#25989=CARTESIAN_POINT('Ctrl Pts',(-0.0901590999540693,1.71662434770709,
10.3353638218884));
#25990=CARTESIAN_POINT('Ctrl Pts',(-0.110115872345704,1.72186740925833,
10.3343198592409));
#25991=CARTESIAN_POINT('Ctrl Pts',(-0.129577468111601,1.72865841902934,
10.3332758965933));
#25992=CARTESIAN_POINT('Ctrl Pts',(-0.149003262174993,1.73543693600612,
10.3322338544276));
#25993=CARTESIAN_POINT('Ctrl Pts',(-0.167934981327794,1.74375756527136,
10.3311918122618));
#25994=CARTESIAN_POINT('Ctrl Pts',(-0.186116225264505,1.75352396808251,
10.330149770096));
#25995=CARTESIAN_POINT('Ctrl Pts',(-0.204277942830833,1.76327988193045,
10.3291088470672));
#25996=CARTESIAN_POINT('Ctrl Pts',(-0.221690126700608,1.77447816582868,
10.3280679240384));
#25997=CARTESIAN_POINT('Ctrl Pts',(-0.238118832990956,1.78697554189005,
10.3270270010095));
#25998=CARTESIAN_POINT('Ctrl Pts',(-0.25455597663667,1.79947933627805,10.3259855433897));
#25999=CARTESIAN_POINT('Ctrl Pts',(-0.270008038288877,1.81328312306739,
10.3249440857699));
#26000=CARTESIAN_POINT('Ctrl Pts',(-0.284271898618622,1.82820158636268,
10.3239026281501));
#26001=CARTESIAN_POINT('Ctrl Pts',(-0.298540117179546,1.8431246078989,10.3228608523196));
#26002=CARTESIAN_POINT('Ctrl Pts',(-0.311618929780691,1.85916242759387,
10.3218190764891));
#26003=CARTESIAN_POINT('Ctrl Pts',(-0.323344302114012,1.87609521601716,
10.3207773006586));
#26004=CARTESIAN_POINT('Ctrl Pts',(-0.335095019105724,1.8930646050469,10.319733273006));
#26005=CARTESIAN_POINT('Ctrl Pts',(-0.345486084981204,1.91093218828524,
10.3186892453535));
#26006=CARTESIAN_POINT('Ctrl Pts',(-0.354398128988664,1.92945130850888,
10.3176452177008));
#26007=CARTESIAN_POINT('Ctrl Pts',(-0.35755020213726,1.93600127858799,10.317275958805));
#26008=CARTESIAN_POINT('Ctrl Pts',(-0.360517698152115,1.94263256817154,
10.3169066999091));
#26009=CARTESIAN_POINT('Ctrl Pts',(-0.363296808260951,1.94933374927541,
10.3165374410132));
#26010=CARTESIAN_POINT('Ctrl Pts',(-0.372070135350239,1.97048859791629,
10.3153717336655));
#26011=CARTESIAN_POINT('Ctrl Pts',(-0.379006803815233,1.99244781540974,
10.3142060263177));
#26012=CARTESIAN_POINT('Ctrl Pts',(-0.383982339767975,2.01489739871008,
10.3130403189699));
#26013=CARTESIAN_POINT('Ctrl Pts',(-0.38891919674824,2.03717246275805,10.3118836736334));
#26014=CARTESIAN_POINT('Ctrl Pts',(-0.391925091309735,2.05992990768128,
10.3107270282968));
#26015=CARTESIAN_POINT('Ctrl Pts',(-0.392925589507551,2.08284275342185,
10.3095703829602));
#26016=CARTESIAN_POINT('Ctrl Pts',(-0.393171833720999,2.08848209958914,
10.3092857075637));
#26017=CARTESIAN_POINT('Ctrl Pts',(-0.393296832619217,2.09413077860865,
10.3090010321673));
#26018=CARTESIAN_POINT('Ctrl Pts',(-0.393299940559465,2.09978376882535,
10.3087163567708));
#26019=CARTESIAN_POINT('',(-0.393225507384553,2.10032482688042,10.1837163490571));
#26020=CARTESIAN_POINT('Ctrl Pts',(-0.392771343913059,2.09978415001449,
10.3087163522035));
#26021=CARTESIAN_POINT('Ctrl Pts',(-0.392375286529236,2.17943390890476,
10.3046999339658));
#26022=CARTESIAN_POINT('Ctrl Pts',(-0.330116542795512,2.39100262904427,
10.2940600678871));
#26023=CARTESIAN_POINT('Ctrl Pts',(0.0156496755916217,2.56479039483764,
10.2767967539677));
#26024=CARTESIAN_POINT('Ctrl Pts',(0.399275537934642,2.33844091151996,10.2569264104448));
#26025=CARTESIAN_POINT('Ctrl Pts',(0.416620450678848,1.89335435268158,10.2370560669221));
#26026=CARTESIAN_POINT('Ctrl Pts',(0.0517728176779485,1.63783704299332,
10.2171857233993));
#26027=CARTESIAN_POINT('Ctrl Pts',(-0.31718930511009,1.78856927240169,10.1994058184931));
#26028=CARTESIAN_POINT('Ctrl Pts',(-0.392294407528429,2.01055654884596,
10.1882493614278));
#26029=CARTESIAN_POINT('Ctrl Pts',(-0.392991088827784,2.10032457091715,
10.1837163522035));
#26030=CARTESIAN_POINT('',(-0.393299995369781,2.10006035006603,10.0587163522072));
#26031=CARTESIAN_POINT('Ctrl Pts',(-0.393299865795482,2.10032490807289,
10.1837163480591));
#26032=CARTESIAN_POINT('Ctrl Pts',(-0.39327953168376,2.12493926542058,10.1824743656741));
#26033=CARTESIAN_POINT('Ctrl Pts',(-0.390944445826951,2.14945349782272,
10.1812323832891));
#26034=CARTESIAN_POINT('Ctrl Pts',(-0.386374291577607,2.17348330972338,
10.1799904009042));
#26035=CARTESIAN_POINT('Ctrl Pts',(-0.383252210631985,2.1898991709326,10.179141946054));
#26036=CARTESIAN_POINT('Ctrl Pts',(-0.379088103166932,2.2060893872349,10.1782934912039));
#26037=CARTESIAN_POINT('Ctrl Pts',(-0.373920092839562,2.22193709103818,
10.1774450363537));
#26038=CARTESIAN_POINT('Ctrl Pts',(-0.367561227965505,2.24143655033984,
10.1764010737061));
#26039=CARTESIAN_POINT('Ctrl Pts',(-0.359654001645914,2.2604953601309,10.1753571110586));
#26040=CARTESIAN_POINT('Ctrl Pts',(-0.350280507675885,2.27885316866727,
10.174313148411));
#26041=CARTESIAN_POINT('Ctrl Pts',(-0.340924257258063,2.29717720603669,
10.1732711062453));
#26042=CARTESIAN_POINT('Ctrl Pts',(-0.330107371188117,2.31480212694996,
10.1722290640795));
#26043=CARTESIAN_POINT('Ctrl Pts',(-0.317960147849274,2.33148700693488,
10.1711870219137));
#26044=CARTESIAN_POINT('Ctrl Pts',(-0.305825970437466,2.34815396762081,
10.1701460988849));
#26045=CARTESIAN_POINT('Ctrl Pts',(-0.292364699674248,2.3638822828141,10.169105175856));
#26046=CARTESIAN_POINT('Ctrl Pts',(-0.277750084760658,2.37845965671071,
10.1680642528272));
#26047=CARTESIAN_POINT('Ctrl Pts',(-0.263127964161756,2.39304451716662,
10.1670227952074));
#26048=CARTESIAN_POINT('Ctrl Pts',(-0.247351825627305,2.40647672443016,
10.1659813375876));
#26049=CARTESIAN_POINT('Ctrl Pts',(-0.230632876008127,2.41858023558316,
10.1649398799678));
#26050=CARTESIAN_POINT('Ctrl Pts',(-0.213908818020965,2.43068744488648,
10.1638981041373));
#26051=CARTESIAN_POINT('Ctrl Pts',(-0.196241992178396,2.44146474808682,
10.1628563283068));
#26052=CARTESIAN_POINT('Ctrl Pts',(-0.177872485462133,2.45077951610025,
10.1618145524763));
#26053=CARTESIAN_POINT('Ctrl Pts',(-0.159463272640243,2.46011441819611,
10.1607705248237));
#26054=CARTESIAN_POINT('Ctrl Pts',(-0.140349027678615,2.46798019345056,
10.1597264971711));
#26055=CARTESIAN_POINT('Ctrl Pts',(-0.120790344968437,2.4742921086029,10.1586824695185));
#26056=CARTESIAN_POINT('Ctrl Pts',(-0.113872695264071,2.47652455025731,
10.1583132106226));
#26057=CARTESIAN_POINT('Ctrl Pts',(-0.106899571459506,2.47856307387668,
10.1579439517267));
#26058=CARTESIAN_POINT('Ctrl Pts',(-0.099882813207992,2.48040545951085,
10.1575746928309));
#26059=CARTESIAN_POINT('Ctrl Pts',(-0.080045150247591,2.48561422172605,
10.1565307301833));
#26060=CARTESIAN_POINT('Ctrl Pts',(-0.0597398372576802,2.48928256237326,
10.1554867675358));
#26061=CARTESIAN_POINT('Ctrl Pts',(-0.0392302215007405,2.49133857428192,
10.1544428048882));
#26062=CARTESIAN_POINT('Ctrl Pts',(-0.0187583353920246,2.49339080393512,
10.1534007627224));
#26063=CARTESIAN_POINT('Ctrl Pts',(0.00191638955361917,2.49383646061028,
10.1523587205567));
#26064=CARTESIAN_POINT('Ctrl Pts',(0.0225208468571737,2.49265468475091,
10.1513166783909));
#26065=CARTESIAN_POINT('Ctrl Pts',(0.0431031752972776,2.49147417810024,
10.150275755362));
#26066=CARTESIAN_POINT('Ctrl Pts',(0.0636146534114712,2.4886697218335,10.1492348323332));
#26067=CARTESIAN_POINT('Ctrl Pts',(0.0837827255047211,2.48427248783513,
10.1481939093043));
#26068=CARTESIAN_POINT('Ctrl Pts',(0.103961155394147,2.47987299553198,10.1471524516845));
#26069=CARTESIAN_POINT('Ctrl Pts',(0.123795104602177,2.47387923228649,10.1461109940647));
#26070=CARTESIAN_POINT('Ctrl Pts',(0.143022223006656,2.46637348938786,10.145069536445));
#26071=CARTESIAN_POINT('Ctrl Pts',(0.162255216134042,2.45886545315754,10.1440277606145));
#26072=CARTESIAN_POINT('Ctrl Pts',(0.180880337673762,2.4498448186313,10.142985984784));
#26073=CARTESIAN_POINT('Ctrl Pts',(0.198656107296091,2.43944166072238,10.1419442089535));
#26074=CARTESIAN_POINT('Ctrl Pts',(0.216470299647844,2.42901601615155,10.1409001813009));
#26075=CARTESIAN_POINT('Ctrl Pts',(0.233430870483884,2.41720230302976,10.1398561536483));
#26076=CARTESIAN_POINT('Ctrl Pts',(0.249325510108922,2.40417376614186,10.1388121259957));
#26077=CARTESIAN_POINT('Ctrl Pts',(0.254947235801275,2.39956574341947,10.1384428670998));
#26078=CARTESIAN_POINT('Ctrl Pts',(0.260435940870581,2.39480610574416,10.138073608204));
#26079=CARTESIAN_POINT('Ctrl Pts',(0.265783349724765,2.38990360640924,10.1377043493081));
#26080=CARTESIAN_POINT('Ctrl Pts',(0.280901455659281,2.37604334131444,10.1366603866605));
#26081=CARTESIAN_POINT('Ctrl Pts',(0.294977494970005,2.36095600967344,10.135616424013));
#26082=CARTESIAN_POINT('Ctrl Pts',(0.307808452188906,2.3448241139289,10.1345724613654));
#26083=CARTESIAN_POINT('Ctrl Pts',(0.320615805479391,2.32872189454488,10.1335304191997));
#26084=CARTESIAN_POINT('Ctrl Pts',(0.332182123772735,2.31157945765313,10.1324883770339));
#26085=CARTESIAN_POINT('Ctrl Pts',(0.342342030508542,2.29361514441615,10.1314463348681));
#26086=CARTESIAN_POINT('Ctrl Pts',(0.352491025664119,2.27567012456939,10.1304054118393));
#26087=CARTESIAN_POINT('Ctrl Pts',(0.361236222345084,2.2569056036751,10.1293644888104));
#26088=CARTESIAN_POINT('Ctrl Pts',(0.368456291107496,2.23756762534589,10.1283235657816));
#26089=CARTESIAN_POINT('Ctrl Pts',(0.375680067909047,2.21821971553502,10.1272821081618));
#26090=CARTESIAN_POINT('Ctrl Pts',(0.381376879540625,2.19829844358105,10.126240650542));
#26091=CARTESIAN_POINT('Ctrl Pts',(0.385473903130076,2.17806894392564,10.1251991929222));
#26092=CARTESIAN_POINT('Ctrl Pts',(0.389572178538849,2.15783326327616,10.1241574170917));
#26093=CARTESIAN_POINT('Ctrl Pts',(0.392069582344319,2.13728989515265,10.1231156412612));
#26094=CARTESIAN_POINT('Ctrl Pts',(0.392944766196695,2.11671229244075,10.1220738654308));
#26095=CARTESIAN_POINT('Ctrl Pts',(0.393821841778828,2.09609021077361,10.1210298377782));
#26096=CARTESIAN_POINT('Ctrl Pts',(0.393069723720385,2.07543448277302,10.1199858101256));
#26097=CARTESIAN_POINT('Ctrl Pts',(0.390719152264053,2.0550174027644,10.118941782473));
#26098=CARTESIAN_POINT('Ctrl Pts',(0.389887785950664,2.04779614918746,10.1185725235771));
#26099=CARTESIAN_POINT('Ctrl Pts',(0.388856932603512,2.0406046698185,10.1182032646812));
#26100=CARTESIAN_POINT('Ctrl Pts',(0.387629472420801,2.03345466123934,10.1178340057854));
#26101=CARTESIAN_POINT('Ctrl Pts',(0.384159217278783,2.01324027515433,10.1167900431378));
#26102=CARTESIAN_POINT('Ctrl Pts',(0.379093133122442,1.99323784405101,10.1157460804903));
#26103=CARTESIAN_POINT('Ctrl Pts',(0.372474775332054,1.97371685883961,10.1147021178427));
#26104=CARTESIAN_POINT('Ctrl Pts',(0.365868592723991,1.954231784584,10.113660075677));
#26105=CARTESIAN_POINT('Ctrl Pts',(0.35771598194294,1.93522710624149,10.1126180335112));
#26106=CARTESIAN_POINT('Ctrl Pts',(0.348111006827302,1.91696006740145,10.1115759913454));
#26107=CARTESIAN_POINT('Ctrl Pts',(0.338516347304046,1.89871264707415,10.1105350683166));
#26108=CARTESIAN_POINT('Ctrl Pts',(0.327472735148029,1.88120195491398,10.1094941452877));
#26109=CARTESIAN_POINT('Ctrl Pts',(0.315121370413706,1.86466319474297,10.1084532222588));
#26110=CARTESIAN_POINT('Ctrl Pts',(0.302763662340371,1.84811594069578,10.107411764639));
#26111=CARTESIAN_POINT('Ctrl Pts',(0.2890972872744,1.83254221501481,10.1063703070193));
#26112=CARTESIAN_POINT('Ctrl Pts',(0.274305754664904,1.81814677053878,10.1053288493995));
#26113=CARTESIAN_POINT('Ctrl Pts',(0.259509702597341,1.80374692762688,10.104287073569));
#26114=CARTESIAN_POINT('Ctrl Pts',(0.243588360667883,1.7905265694324,10.1032452977385));
#26115=CARTESIAN_POINT('Ctrl Pts',(0.226760096711288,1.77865167101806,10.102203521908));
#26116=CARTESIAN_POINT('Ctrl Pts',(0.209895458080266,1.76675110474131,10.1011594942554));
#26117=CARTESIAN_POINT('Ctrl Pts',(0.19212061705435,1.75620218027901,10.1001154666028));
#26118=CARTESIAN_POINT('Ctrl Pts',(0.173681163826441,1.74712644852314,10.0990714389502));
#26119=CARTESIAN_POINT('Ctrl Pts',(0.167159370919507,1.74391648116353,10.0987021800543));
#26120=CARTESIAN_POINT('Ctrl Pts',(0.16055462676386,1.74089036339037,10.0983329211584));
#26121=CARTESIAN_POINT('Ctrl Pts',(0.153878325158237,1.73805200505253,10.0979636622626));
#26122=CARTESIAN_POINT('Ctrl Pts',(0.135003195599921,1.73002744527012,10.096919699615));
#26123=CARTESIAN_POINT('Ctrl Pts',(0.115442430504887,1.72345942215667,10.0958757369675));
#26124=CARTESIAN_POINT('Ctrl Pts',(0.0954461999698468,1.71845719386769,
10.0948317743199));
#26125=CARTESIAN_POINT('Ctrl Pts',(0.0754867546555941,1.71346416771667,
10.0937897321541));
#26126=CARTESIAN_POINT('Ctrl Pts',(0.0550941253140348,1.7100314530493,10.0927476899884));
#26127=CARTESIAN_POINT('Ctrl Pts',(0.03453552541627,1.70821920990914,10.0917056478226));
#26128=CARTESIAN_POINT('Ctrl Pts',(0.0139990051318226,1.70640891308963,
10.0906647247937));
#26129=CARTESIAN_POINT('Ctrl Pts',(-0.00670240516006667,1.70621572585505,
10.0896238017649));
#26130=CARTESIAN_POINT('Ctrl Pts',(-0.0272945077338579,1.70764824475024,
10.088582878736));
#26131=CARTESIAN_POINT('Ctrl Pts',(-0.0478971858748285,1.7090814993498,
10.0875414211162));
#26132=CARTESIAN_POINT('Ctrl Pts',(-0.0683897090242782,1.71214209308282,
10.0864999634964));
#26133=CARTESIAN_POINT('Ctrl Pts',(-0.0885005803488368,1.71678656433011,
10.0854585058767));
#26134=CARTESIAN_POINT('Ctrl Pts',(-0.108617596421348,1.72143245466585,
10.0844167300462));
#26135=CARTESIAN_POINT('Ctrl Pts',(-0.128352020360443,1.72766298525457,
10.0833749542157));
#26136=CARTESIAN_POINT('Ctrl Pts',(-0.147446090907105,1.73538439381149,
10.0823331783852));
#26137=CARTESIAN_POINT('Ctrl Pts',(-0.166581433720556,1.74312249236823,
10.0812891507326));
#26138=CARTESIAN_POINT('Ctrl Pts',(-0.185073000898774,1.75235757353198,
10.08024512308));
#26139=CARTESIAN_POINT('Ctrl Pts',(-0.202685647866543,1.76294893836554,
10.0792010954274));
#26140=CARTESIAN_POINT('Ctrl Pts',(-0.208915010236842,1.76669496527818,
10.0788318365315));
#26141=CARTESIAN_POINT('Ctrl Pts',(-0.215034691592898,1.77061026018904,
10.0784625776356));
#26142=CARTESIAN_POINT('Ctrl Pts',(-0.221035236794658,1.77468735945997,
10.0780933187398));
#26143=CARTESIAN_POINT('Ctrl Pts',(-0.237929542875462,1.78616627690643,
10.0770536844065));
#26144=CARTESIAN_POINT('Ctrl Pts',(-0.253979647592879,1.79900042839638,
10.0760140500733));
#26145=CARTESIAN_POINT('Ctrl Pts',(-0.268959324569773,1.81304047022799,
10.0749744157401));
#26146=CARTESIAN_POINT('Ctrl Pts',(-0.283911446583697,1.8270546855459,10.0739366938036));
#26147=CARTESIAN_POINT('Ctrl Pts',(-0.297796471253918,1.84226993153282,
10.0728989718671));
#26148=CARTESIAN_POINT('Ctrl Pts',(-0.310420097793868,1.85849585327443,
10.0718612499306));
#26149=CARTESIAN_POINT('Ctrl Pts',(-0.323030379202652,1.87470462170014,
10.0708246250272));
#26150=CARTESIAN_POINT('Ctrl Pts',(-0.334381432834109,1.89192137966887,
10.0697880001237));
#26151=CARTESIAN_POINT('Ctrl Pts',(-0.34431848351851,1.90992193207128,10.0687513752203));
#26152=CARTESIAN_POINT('Ctrl Pts',(-0.354260684373736,1.9279318137931,10.0677142130553));
#26153=CARTESIAN_POINT('Ctrl Pts',(-0.362787047567585,1.94672565788657,
10.0666770508903));
#26154=CARTESIAN_POINT('Ctrl Pts',(-0.369788047242238,1.9660534057291,10.0656398887253));
#26155=CARTESIAN_POINT('Ctrl Pts',(-0.376791509495614,1.98538795204368,
10.0646023617419));
#26156=CARTESIAN_POINT('Ctrl Pts',(-0.382268325512055,2.00525606498279,
10.0635648347585));
#26157=CARTESIAN_POINT('Ctrl Pts',(-0.386158716662584,2.02539212142471,
10.0625273077751));
#26158=CARTESIAN_POINT('Ctrl Pts',(-0.390057259454706,2.04557036948923,
10.0614876068334));
#26159=CARTESIAN_POINT('Ctrl Pts',(-0.392362666939148,2.06601694301546,
10.0604479058917));
#26160=CARTESIAN_POINT('Ctrl Pts',(-0.393066867638244,2.08646014900158,
10.05940820495));
#26161=CARTESIAN_POINT('Ctrl Pts',(-0.393223067421461,2.09099468631091,
10.0591775873691));
#26162=CARTESIAN_POINT('Ctrl Pts',(-0.393300690674402,2.09552906580875,
10.0589469697881));
#26163=CARTESIAN_POINT('Ctrl Pts',(-0.393299995369781,2.10006035006604,
10.0587163522072));
#26164=CARTESIAN_POINT('',(-0.393299837194678,2.09964214159272,9.93371635220721));
#26165=CARTESIAN_POINT('Ctrl Pts',(-0.393299995369769,2.10006035013941,
10.0587163522035));
#26166=CARTESIAN_POINT('Ctrl Pts',(-0.393299499530562,2.10329171894644,
10.058551893208));
#26167=CARTESIAN_POINT('Ctrl Pts',(-0.393259180895846,2.10652274228517,
10.0583874342125));
#26168=CARTESIAN_POINT('Ctrl Pts',(-0.39317906021876,2.10975277424596,10.058222975217));
#26169=CARTESIAN_POINT('Ctrl Pts',(-0.392670465392941,2.13025656430656,
10.0571790125694));
#26170=CARTESIAN_POINT('Ctrl Pts',(-0.390552166972687,2.15078155567138,
10.0561350499219));
#26171=CARTESIAN_POINT('Ctrl Pts',(-0.386828265061194,2.17105479118079,
10.0550910872743));
#26172=CARTESIAN_POINT('Ctrl Pts',(-0.383111213668542,2.19129073188892,
10.0540490451085));
#26173=CARTESIAN_POINT('Ctrl Pts',(-0.377794494658613,2.21127510979819,
10.0530070029428));
#26174=CARTESIAN_POINT('Ctrl Pts',(-0.370933957234741,2.23073977730658,
10.051964960777));
#26175=CARTESIAN_POINT('Ctrl Pts',(-0.364080787920287,2.25018354006785,
10.0509240377481));
#26176=CARTESIAN_POINT('Ctrl Pts',(-0.355687307860049,2.26910800047918,
10.0498831147193));
#26177=CARTESIAN_POINT('Ctrl Pts',(-0.345859195631034,2.28725999785713,
10.0488421916904));
#26178=CARTESIAN_POINT('Ctrl Pts',(-0.33602603593973,2.30542131762784,10.0478007340706));
#26179=CARTESIAN_POINT('Ctrl Pts',(-0.324757108285042,2.32280872711126,
10.0467592764508));
#26180=CARTESIAN_POINT('Ctrl Pts',(-0.312204361749858,2.33919307369647,
10.045717818831));
#26181=CARTESIAN_POINT('Ctrl Pts',(-0.299647779803347,2.35558242641387,
10.0446760430005));
#26182=CARTESIAN_POINT('Ctrl Pts',(-0.285807073895645,2.37096754453505,
10.04363426717));
#26183=CARTESIAN_POINT('Ctrl Pts',(-0.270874295963819,2.38515260087558,
10.0425924913395));
#26184=CARTESIAN_POINT('Ctrl Pts',(-0.255909240493629,2.39936831853728,
10.041548463687));
#26185=CARTESIAN_POINT('Ctrl Pts',(-0.239847972583205,2.41237833213905,
10.0405044360344));
#26186=CARTESIAN_POINT('Ctrl Pts',(-0.222915908432341,2.42402683186394,
10.0394604083818));
#26187=CARTESIAN_POINT('Ctrl Pts',(-0.216927259283587,2.42814675353092,
10.0390911494859));
#26188=CARTESIAN_POINT('Ctrl Pts',(-0.210829927902349,2.43209676418458,
10.03872189059));
#26189=CARTESIAN_POINT('Ctrl Pts',(-0.204634622387762,2.43587134638164,
10.0383526316942));
#26190=CARTESIAN_POINT('Ctrl Pts',(-0.187119357028162,2.44654278278578,
10.0373086690466));
#26191=CARTESIAN_POINT('Ctrl Pts',(-0.168714903591213,2.45587222823603,
10.0362647063991));
#26192=CARTESIAN_POINT('Ctrl Pts',(-0.149652988803798,2.46371537353003,
10.0352207437515));
#26193=CARTESIAN_POINT('Ctrl Pts',(-0.130626140462668,2.47154409051312,
10.0341787015857));
#26194=CARTESIAN_POINT('Ctrl Pts',(-0.110944881641507,2.47789160283408,
10.03313665942));
#26195=CARTESIAN_POINT('Ctrl Pts',(-0.0908649078280011,2.48265971636091,
10.0320946172542));
#26196=CARTESIAN_POINT('Ctrl Pts',(-0.070806499590917,2.48742270900871,
10.0310536942253));
#26197=CARTESIAN_POINT('Ctrl Pts',(-0.0503509320291084,2.49060947305793,
10.0300127711965));
#26198=CARTESIAN_POINT('Ctrl Pts',(-0.0297682729011165,2.49217182449595,
10.0289718481676));
#26199=CARTESIAN_POINT('Ctrl Pts',(-0.00917504305586029,2.49373497831695,
10.0279303905478));
#26200=CARTESIAN_POINT('Ctrl Pts',(0.0115446763047099,2.49367198110561,
10.0268889329281));
#26201=CARTESIAN_POINT('Ctrl Pts',(0.0321159567783998,2.49198654992258,
10.0258474753083));
#26202=CARTESIAN_POINT('Ctrl Pts',(0.0526935226751098,2.49030060376684,
10.0248056994778));
#26203=CARTESIAN_POINT('Ctrl Pts',(0.0731218296459621,2.48699133286079,
10.0237639236473));
#26204=CARTESIAN_POINT('Ctrl Pts',(0.0931322615044203,2.48211421311837,
10.0227221478168));
#26205=CARTESIAN_POINT('Ctrl Pts',(0.113185946365438,2.47722655137095,10.0216781201642));
#26206=CARTESIAN_POINT('Ctrl Pts',(0.132819253266682,2.47076450518345,10.0206340925116));
#26207=CARTESIAN_POINT('Ctrl Pts',(0.151779152662418,2.46283326586337,10.019590064859));
#26208=CARTESIAN_POINT('Ctrl Pts',(0.158485020557026,2.46002809047658,10.0192208059631));
#26209=CARTESIAN_POINT('Ctrl Pts',(0.165106855885699,2.45703955722122,10.0188515470672));
#26210=CARTESIAN_POINT('Ctrl Pts',(0.171634222995775,2.45387368296701,10.0184822881714));
#26211=CARTESIAN_POINT('Ctrl Pts',(0.190088287409788,2.4449231755988,10.0174383255238));
#26212=CARTESIAN_POINT('Ctrl Pts',(0.207895315375127,2.4344985790232,10.0163943628763));
#26213=CARTESIAN_POINT('Ctrl Pts',(0.22480853126639,2.42271661604239,10.0153504002287));
#26214=CARTESIAN_POINT('Ctrl Pts',(0.241690633474522,2.41095632725205,10.0143083580629));
#26215=CARTESIAN_POINT('Ctrl Pts',(0.257681556499956,2.39784399556599,10.0132663158972));
#26216=CARTESIAN_POINT('Ctrl Pts',(0.272560324370808,2.38354146007045,10.0122242737314));
#26217=CARTESIAN_POINT('Ctrl Pts',(0.287423112678699,2.36925428527334,10.0111833507025));
#26218=CARTESIAN_POINT('Ctrl Pts',(0.301175569278181,2.35377993078405,10.0101424276737));
#26219=CARTESIAN_POINT('Ctrl Pts',(0.313630987631237,2.33731939153271,10.0091015046448));
#26220=CARTESIAN_POINT('Ctrl Pts',(0.326092802762532,2.32085039857742,10.008060047025));
#26221=CARTESIAN_POINT('Ctrl Pts',(0.337255792050764,2.30339478603645,10.0070185894052));
#26222=CARTESIAN_POINT('Ctrl Pts',(0.346974257155323,2.28518573074487,10.0059771317855));
#26223=CARTESIAN_POINT('Ctrl Pts',(0.356695691674663,2.26697111179305,10.004935355955));
#26224=CARTESIAN_POINT('Ctrl Pts',(0.364971409125805,2.24800325739952,10.0038935801245));
#26225=CARTESIAN_POINT('Ctrl Pts',(0.371702647855097,2.22853805497793,10.002851804294));
#26226=CARTESIAN_POINT('Ctrl Pts',(0.378448436309655,2.20903077807958,10.0018077766414));
#26227=CARTESIAN_POINT('Ctrl Pts',(0.383642895953234,2.18902471975168,10.0007637489888));
#26228=CARTESIAN_POINT('Ctrl Pts',(0.387237504055506,2.16878957372206,9.99971972133617));
#26229=CARTESIAN_POINT('Ctrl Pts',(0.388508869824041,2.16163266780869,9.99935046244031));
#26230=CARTESIAN_POINT('Ctrl Pts',(0.389580576667465,2.15444716305399,9.99898120354444));
#26231=CARTESIAN_POINT('Ctrl Pts',(0.390452034670221,2.14724509098186,9.99861194464858));
#26232=CARTESIAN_POINT('Ctrl Pts',(0.392915806332796,2.12688351185009,9.99756798200102));
#26233=CARTESIAN_POINT('Ctrl Pts',(0.393789884876273,2.10626802142608,9.99652401935347));
#26234=CARTESIAN_POINT('Ctrl Pts',(0.393038828817571,2.08566929723592,9.99548005670592));
#26235=CARTESIAN_POINT('Ctrl Pts',(0.392289154407419,2.06510846661853,9.99443801454015));
#26236=CARTESIAN_POINT('Ctrl Pts',(0.389920246728875,2.04456507016466,9.99339597237438));
#26237=CARTESIAN_POINT('Ctrl Pts',(0.385948564696898,2.02431251484952,9.99235393020861));
#26238=CARTESIAN_POINT('Ctrl Pts',(0.38198114818903,2.00408171046063,9.99131300717976));
#26239=CARTESIAN_POINT('Ctrl Pts',(0.376414487124075,1.98414185103363,9.99027208415091));
#26240=CARTESIAN_POINT('Ctrl Pts',(0.369316514015366,1.96475872495596,9.98923116112205));
#26241=CARTESIAN_POINT('Ctrl Pts',(0.362214895572662,1.94536564420992,9.98818970350226));
#26242=CARTESIAN_POINT('Ctrl Pts',(0.353580631820356,1.92653056447859,9.98714824588247));
#26243=CARTESIAN_POINT('Ctrl Pts',(0.343530912871894,1.90850221436945,9.98610678826268));
#26244=CARTESIAN_POINT('Ctrl Pts',(0.333478123296164,1.8904683558134,9.98506501243218));
#26245=CARTESIAN_POINT('Ctrl Pts',(0.322009407103362,1.87324234209825,9.98402323660169));
#26246=CARTESIAN_POINT('Ctrl Pts',(0.309286457544761,1.85704573027129,9.98298146077119));
#26247=CARTESIAN_POINT('Ctrl Pts',(0.296536007041966,1.8408141091003,9.98193743311859));
#26248=CARTESIAN_POINT('Ctrl Pts',(0.282526409866713,1.82561687356895,9.980893405466));
#26249=CARTESIAN_POINT('Ctrl Pts',(0.267458163103384,1.8116408125456,9.9798493778134));
#26250=CARTESIAN_POINT('Ctrl Pts',(0.26212872173407,1.80669766295641,9.97948011891753));
#26251=CARTESIAN_POINT('Ctrl Pts',(0.256667154963148,1.80190690909666,9.97911086002167));
#26252=CARTESIAN_POINT('Ctrl Pts',(0.251083259779382,1.7972755598592,9.9787416011258));
#26253=CARTESIAN_POINT('Ctrl Pts',(0.23529656360233,1.78418188583857,9.97769763847825));
#26254=CARTESIAN_POINT('Ctrl Pts',(0.218435844655353,1.77228740748459,9.9766536758307));
#26255=CARTESIAN_POINT('Ctrl Pts',(0.200709508333495,1.76176844726648,9.97560971318314));
#26256=CARTESIAN_POINT('Ctrl Pts',(0.183015781517424,1.75126883780917,9.97456767101737));
#26257=CARTESIAN_POINT('Ctrl Pts',(0.164460193432313,1.74214014610303,9.9735256288516));
#26258=CARTESIAN_POINT('Ctrl Pts',(0.145281539066169,1.7345165333335,9.97248358668583));
#26259=CARTESIAN_POINT('Ctrl Pts',(0.126123482273526,1.72690110820432,9.97144266365698));
#26260=CARTESIAN_POINT('Ctrl Pts',(0.106344357238756,1.72078785029713,9.97040174062812));
#26261=CARTESIAN_POINT('Ctrl Pts',(0.0862044166937409,1.71626351679506,
9.96936081759927));
#26262=CARTESIAN_POINT('Ctrl Pts',(0.0660541328001721,1.71173685971323,
9.96831935997948));
#26263=CARTESIAN_POINT('Ctrl Pts',(0.0455433775512048,1.70880093428048,
9.96727790235969));
#26264=CARTESIAN_POINT('Ctrl Pts',(0.0249447235392476,1.70749184624068,
9.9662364447399));
#26265=CARTESIAN_POINT('Ctrl Pts',(0.00433977574046094,1.70618235821742,
9.9651946689094));
#26266=CARTESIAN_POINT('Ctrl Pts',(-0.0163523883141121,1.7065007076543,
9.9641528930789));
#26267=CARTESIAN_POINT('Ctrl Pts',(-0.036857952013767,1.7084308728036,9.9631111172484));
#26268=CARTESIAN_POINT('Ctrl Pts',(-0.0574078389546922,1.71036521004867,
9.9620670895958));
#26269=CARTESIAN_POINT('Ctrl Pts',(-0.0777695947749148,1.71391819199709,
9.96102306194321));
#26270=CARTESIAN_POINT('Ctrl Pts',(-0.0976776313550497,1.71902234930003,
9.95997903429061));
#26271=CARTESIAN_POINT('Ctrl Pts',(-0.104718842943808,1.72082762283405,
9.95960977539474));
#26272=CARTESIAN_POINT('Ctrl Pts',(-0.111703439341944,1.72282648433332,
9.95924051649888));
#26273=CARTESIAN_POINT('Ctrl Pts',(-0.118620224059825,1.72501449035463,
9.95887125760301));
#26274=CARTESIAN_POINT('Ctrl Pts',(-0.138175243498682,1.73120038481633,
9.95782729495546));
#26275=CARTESIAN_POINT('Ctrl Pts',(-0.157303345681881,1.73893848313514,
9.9567833323079));
#26276=CARTESIAN_POINT('Ctrl Pts',(-0.175743461914374,1.74814900086208,
9.95573936966035));
#26277=CARTESIAN_POINT('Ctrl Pts',(-0.194149655566013,1.75734257484917,
9.95469732749458));
#26278=CARTESIAN_POINT('Ctrl Pts',(-0.211869698104813,1.76800291977198,
9.95365528532881));
#26279=CARTESIAN_POINT('Ctrl Pts',(-0.228661520362214,1.78000187640294,
9.95261324316304));
#26280=CARTESIAN_POINT('Ctrl Pts',(-0.245435308466308,1.79198794634298,
9.95157232013418));
#26281=CARTESIAN_POINT('Ctrl Pts',(-0.261282242936222,1.80530937184055,
9.95053139710533));
#26282=CARTESIAN_POINT('Ctrl Pts',(-0.275988497272819,1.81979429096985,
9.94949047407648));
#26283=CARTESIAN_POINT('Ctrl Pts',(-0.290702304358352,1.83428664917609,
9.94844901645669));
#26284=CARTESIAN_POINT('Ctrl Pts',(-0.304273725450247,1.84994318993631,
9.94740755883689));
#26285=CARTESIAN_POINT('Ctrl Pts',(-0.316524853723257,1.86655427402612,
9.9463661012171));
#26286=CARTESIAN_POINT('Ctrl Pts',(-0.328779725250061,1.88317043352631,
9.9453243253866));
#26287=CARTESIAN_POINT('Ctrl Pts',(-0.3397130936301,1.90074110384625,9.9442825495561));
#26288=CARTESIAN_POINT('Ctrl Pts',(-0.349190208356797,1.9190273822156,9.9432407737256));
#26289=CARTESIAN_POINT('Ctrl Pts',(-0.358687808082036,1.93735318679062,
9.94219674607301));
#26290=CARTESIAN_POINT('Ctrl Pts',(-0.366722583584917,1.95639700897595,
9.94115271842041));
#26291=CARTESIAN_POINT('Ctrl Pts',(-0.37320749665403,1.97589901514802,9.94010869076781));
#26292=CARTESIAN_POINT('Ctrl Pts',(-0.375501125403926,1.98279661910357,
9.93973943187195));
#26293=CARTESIAN_POINT('Ctrl Pts',(-0.377601335100905,1.98975141265669,
9.93937017297608));
#26294=CARTESIAN_POINT('Ctrl Pts',(-0.379505801009439,1.99675157628233,
9.93900091408021));
#26295=CARTESIAN_POINT('Ctrl Pts',(-0.386317014682717,2.02178726213446,
9.93768028070514));
#26296=CARTESIAN_POINT('Ctrl Pts',(-0.390653742797625,2.0475233829174,9.93635964733007));
#26297=CARTESIAN_POINT('Ctrl Pts',(-0.392408023018093,2.07352674045321,
9.935039013955));
#26298=CARTESIAN_POINT('Ctrl Pts',(-0.392993681229854,2.08220783922894,
9.93459812670574));
#26299=CARTESIAN_POINT('Ctrl Pts',(-0.393291899704221,2.09091854130528,
9.93415723945647));
#26300=CARTESIAN_POINT('Ctrl Pts',(-0.393299837194678,2.09964214159272,
9.93371635220721));
#26301=CARTESIAN_POINT('',(-0.393067570229214,2.10012154744265,9.80871631880887));
#26302=CARTESIAN_POINT('Ctrl Pts',(-0.393299837194745,2.09964214166643,
9.93371635220349));
#26303=CARTESIAN_POINT('Ctrl Pts',(-0.39331839913374,2.12004241434374,9.93268533062886));
#26304=CARTESIAN_POINT('Ctrl Pts',(-0.391745421875908,2.14047972199369,
9.93165430905423));
#26305=CARTESIAN_POINT('Ctrl Pts',(-0.388590103262886,2.16068460798373,
9.93062328747959));
#26306=CARTESIAN_POINT('Ctrl Pts',(-0.385434358167012,2.18089222493012,
9.92959212654882));
#26307=CARTESIAN_POINT('Ctrl Pts',(-0.380695920873502,2.20086660921189,
9.92856096561805));
#26308=CARTESIAN_POINT('Ctrl Pts',(-0.37443578397093,2.22034422994924,9.92752980468727));
#26309=CARTESIAN_POINT('Ctrl Pts',(-0.368175768378373,2.23982147324589,
9.92649866373852));
#26310=CARTESIAN_POINT('Ctrl Pts',(-0.360394362374816,2.25880126237412,
9.92546752278976));
#26311=CARTESIAN_POINT('Ctrl Pts',(-0.351201875568091,2.27703709384605,
9.924436381841));
#26312=CARTESIAN_POINT('Ctrl Pts',(-0.341988688502122,2.29531398998818,
9.92340291889979));
#26313=CARTESIAN_POINT('Ctrl Pts',(-0.331358451623212,2.31284292897447,
9.92236945595858));
#26314=CARTESIAN_POINT('Ctrl Pts',(-0.31946694191771,2.32940305800435,9.92133599301738));
#26315=CARTESIAN_POINT('Ctrl Pts',(-0.311008066570381,2.34118289678585,
9.92060085219739));
#26316=CARTESIAN_POINT('Ctrl Pts',(-0.30191195304697,2.35247308549262,9.91986571137741));
#26317=CARTESIAN_POINT('Ctrl Pts',(-0.29224647058237,2.36320503496732,9.91913057055742));
#26318=CARTESIAN_POINT('Ctrl Pts',(-0.278520661336955,2.3784453183014,9.91808660790987));
#26319=CARTESIAN_POINT('Ctrl Pts',(-0.263558603338637,2.39265444491696,
9.91704264526232));
#26320=CARTESIAN_POINT('Ctrl Pts',(-0.247540993614156,2.40562779075293,
9.91599868261476));
#26321=CARTESIAN_POINT('Ctrl Pts',(-0.231552850008755,2.41857727072128,
9.914956640449));
#26322=CARTESIAN_POINT('Ctrl Pts',(-0.214513536950555,2.43029497834499,
9.91391459828323));
#26323=CARTESIAN_POINT('Ctrl Pts',(-0.196639922175481,2.44061360954434,
9.91287255611746));
#26324=CARTESIAN_POINT('Ctrl Pts',(-0.17878550338189,2.45092115869587,9.9118316330886));
#26325=CARTESIAN_POINT('Ctrl Pts',(-0.160099181221913,2.45983222336371,
9.91079071005975));
#26326=CARTESIAN_POINT('Ctrl Pts',(-0.140825914952268,2.46722329947575,
9.9097497870309));
#26327=CARTESIAN_POINT('Ctrl Pts',(-0.121542750435389,2.47461817145185,
9.90870832941111));
#26328=CARTESIAN_POINT('Ctrl Pts',(-0.101672720823039,2.48049121684875,
9.90766687179132));
#26329=CARTESIAN_POINT('Ctrl Pts',(-0.0814803051101876,2.48476726716179,
9.90662541417152));
#26330=CARTESIAN_POINT('Ctrl Pts',(-0.0612817197340254,2.48904462399462,
9.90558363834103));
#26331=CARTESIAN_POINT('Ctrl Pts',(-0.0407612788656792,2.49172389743974,
9.90454186251053));
#26332=CARTESIAN_POINT('Ctrl Pts',(-0.0201922355651711,2.49278131781295,
9.90350008668003));
#26333=CARTESIAN_POINT('Ctrl Pts',(0.000421268189205144,2.4938410238243,
9.90245605902744));
#26334=CARTESIAN_POINT('Ctrl Pts',(0.0210828479149291,2.49327189813925,
9.90141203137484));
#26335=CARTESIAN_POINT('Ctrl Pts',(0.041519947680011,2.49110226788482,9.90036800372224));
#26336=CARTESIAN_POINT('Ctrl Pts',(0.0487482819824797,2.49033489810281,
9.89999874482638));
#26337=CARTESIAN_POINT('Ctrl Pts',(0.0559486102473542,2.48936778538109,
9.89962948593051));
#26338=CARTESIAN_POINT('Ctrl Pts',(0.0631092108396671,2.48820370619971,
9.89926022703464));
#26339=CARTESIAN_POINT('Ctrl Pts',(0.0833535424890364,2.48491264077719,
9.89821626438709));
#26340=CARTESIAN_POINT('Ctrl Pts',(0.103400062894784,2.4800239315054,9.89717230173954));
#26341=CARTESIAN_POINT('Ctrl Pts',(0.122978905917147,2.47357874497811,9.89612833909198));
#26342=CARTESIAN_POINT('Ctrl Pts',(0.14252173154802,2.46714541506595,9.89508629692621));
#26343=CARTESIAN_POINT('Ctrl Pts',(0.161597877955621,2.45916146243047,9.89404425476044));
#26344=CARTESIAN_POINT('Ctrl Pts',(0.179949278450231,2.44971866862557,9.89300221259468));
#26345=CARTESIAN_POINT('Ctrl Pts',(0.198280969829021,2.44028601623286,9.89196128956582));
#26346=CARTESIAN_POINT('Ctrl Pts',(0.215888796374484,2.42939794231108,9.89092036653697));
#26347=CARTESIAN_POINT('Ctrl Pts',(0.23253631277975,2.41719355800331,9.88987944350811));
#26348=CARTESIAN_POINT('Ctrl Pts',(0.249192378915542,2.40498290584185,9.88883798588832));
#26349=CARTESIAN_POINT('Ctrl Pts',(0.26488654669633,2.39145501477568,9.88779652826853));
#26350=CARTESIAN_POINT('Ctrl Pts',(0.279412445838746,2.37679157340933,9.88675507064874));
#26351=CARTESIAN_POINT('Ctrl Pts',(0.293942783276634,2.36212365172235,9.88571329481824));
#26352=CARTESIAN_POINT('Ctrl Pts',(0.307303649782911,2.34632003676162,9.88467151898774));
#26353=CARTESIAN_POINT('Ctrl Pts',(0.319327142562771,2.32959761763288,9.88362974315724));
#26354=CARTESIAN_POINT('Ctrl Pts',(0.33137662439511,2.31283905261574,9.88258571550464));
#26355=CARTESIAN_POINT('Ctrl Pts',(0.342082579765853,2.29515834843272,9.88154168785205));
#26356=CARTESIAN_POINT('Ctrl Pts',(0.351321287179832,2.27680000897711,9.88049766019945));
#26357=CARTESIAN_POINT('Ctrl Pts',(0.354588896893459,2.27030690494824,9.88012840130359));
#26358=CARTESIAN_POINT('Ctrl Pts',(0.357673398992924,2.26372922443483,9.87975914240772));
#26359=CARTESIAN_POINT('Ctrl Pts',(0.360570782859558,2.25707832615624,9.87938988351185));
#26360=CARTESIAN_POINT('Ctrl Pts',(0.368762218641469,2.23827501646417,9.8783459208643));
#26361=CARTESIAN_POINT('Ctrl Pts',(0.375503248069686,2.21877319652422,9.87730195821674));
#26362=CARTESIAN_POINT('Ctrl Pts',(0.380682401335698,2.19882205883954,9.87625799556919));
#26363=CARTESIAN_POINT('Ctrl Pts',(0.385852026991192,2.1789076234225,9.87521595340342));
#26364=CARTESIAN_POINT('Ctrl Pts',(0.389465239402053,2.15854620015387,9.87417391123765));
#26365=CARTESIAN_POINT('Ctrl Pts',(0.391459513979982,2.13800445914042,9.87313186907188));
#26366=CARTESIAN_POINT('Ctrl Pts',(0.393451646738343,2.11748477963413,9.87209094604303));
#26367=CARTESIAN_POINT('Ctrl Pts',(0.393828193902946,2.09678589266856,9.87105002301418));
#26368=CARTESIAN_POINT('Ctrl Pts',(0.392578130496698,2.07618190906648,9.87000909998532));
#26369=CARTESIAN_POINT('Ctrl Pts',(0.391327425090465,2.05556734379542,9.86896764236553));
#26370=CARTESIAN_POINT('Ctrl Pts',(0.38844846866883,2.03504851466331,9.86792618474574));
#26371=CARTESIAN_POINT('Ctrl Pts',(0.383982316300243,2.0148972928239,9.86688472712595));
#26372=CARTESIAN_POINT('Ctrl Pts',(0.379514799327402,1.99473991390771,9.86584295129545));
#26373=CARTESIAN_POINT('Ctrl Pts',(0.373459315369822,1.97495107579972,9.86480117546495));
#26374=CARTESIAN_POINT('Ctrl Pts',(0.365907339854241,1.95578936016787,9.86375939963446));
#26375=CARTESIAN_POINT('Ctrl Pts',(0.358339040572202,1.93658622605283,9.86271537198186));
#26376=CARTESIAN_POINT('Ctrl Pts',(0.349268115019523,1.91801358244924,9.86167134432926));
#26377=CARTESIAN_POINT('Ctrl Pts',(0.338833173766516,1.90030781098072,9.86062731667666));
#26378=CARTESIAN_POINT('Ctrl Pts',(0.335142471823961,1.89404551169519,9.8602580577808));
#26379=CARTESIAN_POINT('Ctrl Pts',(0.331281536998818,1.88789138979079,9.85988879888493));
#26380=CARTESIAN_POINT('Ctrl Pts',(0.327257748885349,1.88185496614753,9.85951953998906));
#26381=CARTESIAN_POINT('Ctrl Pts',(0.315881761633185,1.86478888898893,9.85847557734151));
#26382=CARTESIAN_POINT('Ctrl Pts',(0.303133323291774,1.84856422324269,9.85743161469396));
#26383=CARTESIAN_POINT('Ctrl Pts',(0.289161618757924,1.83340958712419,9.85638765204641));
#26384=CARTESIAN_POINT('Ctrl Pts',(0.275215616680097,1.81828282959182,9.85534560988064));
#26385=CARTESIAN_POINT('Ctrl Pts',(0.2600512646017,1.80422276958154,9.85430356771487));
#26386=CARTESIAN_POINT('Ctrl Pts',(0.24385893783366,1.79142633223387,9.8532615255491));
#26387=CARTESIAN_POINT('Ctrl Pts',(0.227684001370201,1.7786436380589,9.85222060252025));
#26388=CARTESIAN_POINT('Ctrl Pts',(0.210483838392706,1.76712234894144,9.85117967949139));
#26389=CARTESIAN_POINT('Ctrl Pts',(0.192482958169429,1.75702011602086,9.85013875646254));
#26390=CARTESIAN_POINT('Ctrl Pts',(0.174472833163229,1.74691269485675,9.84909729884275));
#26391=CARTESIAN_POINT('Ctrl Pts',(0.155661803121502,1.73822616000108,9.84805584122296));
#26392=CARTESIAN_POINT('Ctrl Pts',(0.136300686028357,1.73107316038515,9.84701438360317));
#26393=CARTESIAN_POINT('Ctrl Pts',(0.116933653269857,1.72391797521599,9.84597260777267));
#26394=CARTESIAN_POINT('Ctrl Pts',(0.0970169009997988,1.71829747891776,
9.84493083194217));
#26395=CARTESIAN_POINT('Ctrl Pts',(0.0768173666156927,1.71427473224297,
9.84388905611167));
#26396=CARTESIAN_POINT('Ctrl Pts',(0.0565741704796338,1.71024329030996,
9.84284502845908));
#26397=CARTESIAN_POINT('Ctrl Pts',(0.0360477033031119,1.70781657935499,
9.84180100080648));
#26398=CARTESIAN_POINT('Ctrl Pts',(0.0155117513937795,1.70700601077281,
9.84075697315388));
#26399=CARTESIAN_POINT('Ctrl Pts',(0.00824845438361141,1.70671932329003,
9.84038771425801));
#26400=CARTESIAN_POINT('Ctrl Pts',(0.000983964717090274,1.70663432903389,
9.84001845536215));
#26401=CARTESIAN_POINT('Ctrl Pts',(-0.00626971757168497,1.70674997693379,
9.83964919646628));
#26402=CARTESIAN_POINT('Ctrl Pts',(-0.0267772082548701,1.70707693476506,
9.83860523381873));
#26403=CARTESIAN_POINT('Ctrl Pts',(-0.0473201577308162,1.70901334524591,
9.83756127117117));
#26404=CARTESIAN_POINT('Ctrl Pts',(-0.0676255832305279,1.71255752621488,
9.83651730852362));
#26405=CARTESIAN_POINT('Ctrl Pts',(-0.0878936547119969,1.71609518728106,
9.83547526635785));
#26406=CARTESIAN_POINT('Ctrl Pts',(-0.107924342687827,1.72123468148423,
9.83443322419208));
#26407=CARTESIAN_POINT('Ctrl Pts',(-0.127449015378381,1.72792253699118,
9.83339118202631));
#26408=CARTESIAN_POINT('Ctrl Pts',(-0.146952718877181,1.73460320984638,
9.83235025899746));
#26409=CARTESIAN_POINT('Ctrl Pts',(-0.165950784055656,1.7428287328604,9.83130933596861));
#26410=CARTESIAN_POINT('Ctrl Pts',(-0.184189124089649,1.75249567403112,
9.83026841293975));
#26411=CARTESIAN_POINT('Ctrl Pts',(-0.202436830859749,1.76216757989087,
9.82922695531996));
#26412=CARTESIAN_POINT('Ctrl Pts',(-0.21992337534878,1.77328205247676,9.82818549770017));
#26413=CARTESIAN_POINT('Ctrl Pts',(-0.236418268011613,1.78568917843894,
9.82714404008038));
#26414=CARTESIAN_POINT('Ctrl Pts',(-0.252918200583262,1.798100095319,9.82610226424988));
#26415=CARTESIAN_POINT('Ctrl Pts',(-0.268425312378988,1.81180398102266,
9.82506048841938));
#26416=CARTESIAN_POINT('Ctrl Pts',(-0.28274208275248,1.82661052573153,9.82401871258888));
#26417=CARTESIAN_POINT('Ctrl Pts',(-0.297089799150026,1.84144907512279,
9.82297468493629));
#26418=CARTESIAN_POINT('Ctrl Pts',(-0.310241568742107,1.85739447375073,
9.82193065728369));
#26419=CARTESIAN_POINT('Ctrl Pts',(-0.322039591148359,1.87422269438006,
9.8208866296311));
#26420=CARTESIAN_POINT('Ctrl Pts',(-0.326212397027945,1.88017461543658,
9.82051737073523));
#26421=CARTESIAN_POINT('Ctrl Pts',(-0.330216261237806,1.88623671948787,
9.82014811183935));
#26422=CARTESIAN_POINT('Ctrl Pts',(-0.334045571701636,1.89239834772689,
9.81977885294348));
#26423=CARTESIAN_POINT('Ctrl Pts',(-0.345174432997193,1.91030546355741,
9.81870570124343));
#26424=CARTESIAN_POINT('Ctrl Pts',(-0.354888865172677,1.92915663330112,
9.81763254954337));
#26425=CARTESIAN_POINT('Ctrl Pts',(-0.363036937996751,1.94870865308967,
9.81655939784331));
#26426=CARTESIAN_POINT('Ctrl Pts',(-0.371166121038456,1.96821534517844,
9.81548873404469));
#26427=CARTESIAN_POINT('Ctrl Pts',(-0.37773584337263,1.98841906398911,9.81441807024606));
#26428=CARTESIAN_POINT('Ctrl Pts',(-0.38264005286215,2.00905232303324,9.81334740644744));
#26429=CARTESIAN_POINT('Ctrl Pts',(-0.38753456325213,2.02964477549401,9.81227886011032));
#26430=CARTESIAN_POINT('Ctrl Pts',(-0.390769912254042,2.05066443284332,
9.81121031377319));
#26431=CARTESIAN_POINT('Ctrl Pts',(-0.392289769156809,2.07182861354322,
9.81014176743606));
#26432=CARTESIAN_POINT('Ctrl Pts',(-0.392965586731042,2.08123945033659,
9.80966662902521));
#26433=CARTESIAN_POINT('Ctrl Pts',(-0.393302885292492,2.09067869849534,
9.80919149061435));
#26434=CARTESIAN_POINT('Ctrl Pts',(-0.393299981400419,2.10012095631365,
9.80871635220349));
#26435=CARTESIAN_POINT('',(-0.393383546135126,2.10030552476621,9.68371639062669));
#26436=CARTESIAN_POINT('Ctrl Pts',(-0.392686993440875,2.10012251542529,
9.80871626412467));
#26437=CARTESIAN_POINT('Ctrl Pts',(-0.392846725206061,2.15837609996444,
9.80578034589002));
#26438=CARTESIAN_POINT('Ctrl Pts',(-0.353358128587013,2.34784367211105,
9.79622097981441));
#26439=CARTESIAN_POINT('Ctrl Pts',(-0.0599518019945944,2.5611732916345,
9.78003816589791));
#26440=CARTESIAN_POINT('Ctrl Pts',(0.355309766950069,2.40004998415162,9.76016782237512));
#26441=CARTESIAN_POINT('Ctrl Pts',(0.444622995774978,1.96367166432625,9.74029747885231));
#26442=CARTESIAN_POINT('Ctrl Pts',(0.126055155931373,1.65235603305462,9.72042713532955));
#26443=CARTESIAN_POINT('Ctrl Pts',(-0.286080276586348,1.7466434788202,9.7015668080763));
#26444=CARTESIAN_POINT('Ctrl Pts',(-0.392665020011803,1.98959023483791,
9.68932992866398));
#26445=CARTESIAN_POINT('Ctrl Pts',(-0.393615372483065,2.10030360545593,
9.68371649709261));
#26446=CARTESIAN_POINT('',(-0.393409004503689,2.09971354421981,9.55871630428717));
#26447=CARTESIAN_POINT('Ctrl Pts',(-0.393299880791846,2.10030621743879,
9.68371635220349));
#26448=CARTESIAN_POINT('Ctrl Pts',(-0.39328438428292,2.12020964010897,9.68270638423031));
#26449=CARTESIAN_POINT('Ctrl Pts',(-0.391757774685968,2.14005558435781,
9.68169641625714));
#26450=CARTESIAN_POINT('Ctrl Pts',(-0.388747481156827,2.15966813131164,
9.68068644828397));
#26451=CARTESIAN_POINT('Ctrl Pts',(-0.38563586367384,2.17994082013638,9.67964248563642));
#26452=CARTESIAN_POINT('Ctrl Pts',(-0.380924912859241,2.20002985697604,
9.67859852298887));
#26453=CARTESIAN_POINT('Ctrl Pts',(-0.374653403290349,2.21966502163522,
9.67755456034132));
#26454=CARTESIAN_POINT('Ctrl Pts',(-0.368393430839102,2.23926406529322,
9.67651251817555));
#26455=CARTESIAN_POINT('Ctrl Pts',(-0.360578762777487,2.25841018303383,
9.67547047600978));
#26456=CARTESIAN_POINT('Ctrl Pts',(-0.35129889117364,2.27684450531518,9.67442843384401));
#26457=CARTESIAN_POINT('Ctrl Pts',(-0.342028986006111,2.295259029424,9.67338751081515));
#26458=CARTESIAN_POINT('Ctrl Pts',(-0.331297304606908,2.31296260882839,
9.6723465877863));
#26459=CARTESIAN_POINT('Ctrl Pts',(-0.319240858292976,2.32971757528836,
9.67130566475744));
#26460=CARTESIAN_POINT('Ctrl Pts',(-0.30717822010245,2.34648114666242,9.67026420713765));
#26461=CARTESIAN_POINT('Ctrl Pts',(-0.29378987444691,2.36229452516412,9.66922274951785));
#26462=CARTESIAN_POINT('Ctrl Pts',(-0.279255674830849,2.37694973925745,
9.66818129189805));
#26463=CARTESIAN_POINT('Ctrl Pts',(-0.264717034383171,2.39160943115759,
9.66713951606755));
#26464=CARTESIAN_POINT('Ctrl Pts',(-0.249032386357423,2.40510975766971,
9.66609774023705));
#26465=CARTESIAN_POINT('Ctrl Pts',(-0.232417124113025,2.41728090144071,
9.66505596440655));
#26466=CARTESIAN_POINT('Ctrl Pts',(-0.215765947602234,2.42947835341517,
9.66401193675395));
#26467=CARTESIAN_POINT('Ctrl Pts',(-0.198180767506498,2.44034049969521,
9.66296790910135));
#26468=CARTESIAN_POINT('Ctrl Pts',(-0.179904982235449,2.44974145788977,
9.66192388144875));
#26469=CARTESIAN_POINT('Ctrl Pts',(-0.173441076539635,2.45306645357771,
9.66155462255288));
#26470=CARTESIAN_POINT('Ctrl Pts',(-0.166890975759392,2.45620909799058,
9.66118536365702));
#26471=CARTESIAN_POINT('Ctrl Pts',(-0.1602660026435,2.45916528005456,9.66081610476116));
#26472=CARTESIAN_POINT('Ctrl Pts',(-0.141535988142762,2.46752294912835,
9.6597721421136));
#26473=CARTESIAN_POINT('Ctrl Pts',(-0.122094643488743,2.47443645596392,
9.65872817946605));
#26474=CARTESIAN_POINT('Ctrl Pts',(-0.102190164039155,2.47979212784581,
9.65768421681849));
#26475=CARTESIAN_POINT('Ctrl Pts',(-0.0823223010243468,2.48513794739217,
9.65664217465272));
#26476=CARTESIAN_POINT('Ctrl Pts',(-0.0619936814047709,2.48893137405054,
9.65560013248695));
#26477=CARTESIAN_POINT('Ctrl Pts',(-0.04147041099965,2.4911075235936,9.65455809032118));
#26478=CARTESIAN_POINT('Ctrl Pts',(-0.0209691822645188,2.49328133598625,
9.65351716729233));
#26479=CARTESIAN_POINT('Ctrl Pts',(-0.000274442679066934,2.49384121353664,
9.65247624426348));
#26480=CARTESIAN_POINT('Ctrl Pts',(0.0203398053437122,2.49277370370046,
9.65143532123462));
#26481=CARTESIAN_POINT('Ctrl Pts',(0.0409646403069961,2.49170564561906,
9.65039386361483));
#26482=CARTESIAN_POINT('Ctrl Pts',(0.0615081654954153,2.4890085523944,9.64935240599504));
#26483=CARTESIAN_POINT('Ctrl Pts',(0.0816981567661531,2.48472106932297,
9.64831094837525));
#26484=CARTESIAN_POINT('Ctrl Pts',(0.101894316959437,2.48043227623855,9.64726917254476));
#26485=CARTESIAN_POINT('Ctrl Pts',(0.121736016585802,2.47455231403098,9.64622739671426));
#26486=CARTESIAN_POINT('Ctrl Pts',(0.140963873856919,2.46717036409173,9.64518562088376));
#26487=CARTESIAN_POINT('Ctrl Pts',(0.16023329257786,2.45977245790016,9.64414159323117));
#26488=CARTESIAN_POINT('Ctrl Pts',(0.178885555380011,2.45086639967178,9.64309756557857));
#26489=CARTESIAN_POINT('Ctrl Pts',(0.196683062138064,2.44058870073447,9.64205353792598));
#26490=CARTESIAN_POINT('Ctrl Pts',(0.202977806993071,2.43695361333788,9.64168427903011));
#26491=CARTESIAN_POINT('Ctrl Pts',(0.209165886587755,2.43314734153095,9.64131502013425));
#26492=CARTESIAN_POINT('Ctrl Pts',(0.21523771504915,2.42917718028506,9.64094576123838));
#26493=CARTESIAN_POINT('Ctrl Pts',(0.232403888124444,2.4179528060266,9.63990179859083));
#26494=CARTESIAN_POINT('Ctrl Pts',(0.248740839597912,2.40534858152543,9.63885783594327));
#26495=CARTESIAN_POINT('Ctrl Pts',(0.2640186387834,2.39151166078728,9.63781387329572));
#26496=CARTESIAN_POINT('Ctrl Pts',(0.279268332811009,2.37770019455585,9.63677183112995));
#26497=CARTESIAN_POINT('Ctrl Pts',(0.293462162979261,2.36266097760134,9.63572978896418));
#26498=CARTESIAN_POINT('Ctrl Pts',(0.306401525579946,2.34658263345638,9.63468774679841));
#26499=CARTESIAN_POINT('Ctrl Pts',(0.319326991508474,2.33052155720044,9.63364682376956));
#26500=CARTESIAN_POINT('Ctrl Pts',(0.331000183044926,2.3134241214648,9.6326059007407));
#26501=CARTESIAN_POINT('Ctrl Pts',(0.34126146659212,2.29551343027883,9.63156497771185));
#26502=CARTESIAN_POINT('Ctrl Pts',(0.351528020067099,2.27759354062869,9.63052352009206));
#26503=CARTESIAN_POINT('Ctrl Pts',(0.360380837176447,2.25886019153521,9.62948206247227));
#26504=CARTESIAN_POINT('Ctrl Pts',(0.367705051730088,2.23956319332895,9.62844060485247));
#26505=CARTESIAN_POINT('Ctrl Pts',(0.375031504150583,2.22026029904846,9.62739882902198));
#26506=CARTESIAN_POINT('Ctrl Pts',(0.380828197173872,2.20039411296208,9.62635705319148));
#26507=CARTESIAN_POINT('Ctrl Pts',(0.385029708061865,2.1802310034201,9.62531527736098));
#26508=CARTESIAN_POINT('Ctrl Pts',(0.389240300610986,2.16002431085928,9.62427124970838));
#26509=CARTESIAN_POINT('Ctrl Pts',(0.391848734274883,2.13952014409667,9.62322722205578));
#26510=CARTESIAN_POINT('Ctrl Pts',(0.392841172981202,2.1189921776201,9.62218319440319));
#26511=CARTESIAN_POINT('Ctrl Pts',(0.393192185542986,2.11173170495285,9.62181393550732));
#26512=CARTESIAN_POINT('Ctrl Pts',(0.393341523354874,2.10446825313182,9.62144467661145));
#26513=CARTESIAN_POINT('Ctrl Pts',(0.393290131153164,2.09721383103047,9.62107541771558));
#26514=CARTESIAN_POINT('Ctrl Pts',(0.393144835969863,2.07670424876133,9.62003145506803));
#26515=CARTESIAN_POINT('Ctrl Pts',(0.391390465360976,2.05614495299302,9.61898749242048));
#26516=CARTESIAN_POINT('Ctrl Pts',(0.388026283414218,2.03580893068542,9.61794352977292));
#26517=CARTESIAN_POINT('Ctrl Pts',(0.384668290242663,2.0155103186822,9.61690148760715));
#26518=CARTESIAN_POINT('Ctrl Pts',(0.379706424095702,1.99543489226606,9.61585944544138));
#26519=CARTESIAN_POINT('Ctrl Pts',(0.373191775240968,1.97585174631718,9.61481740327561));
#26520=CARTESIAN_POINT('Ctrl Pts',(0.36668412301676,1.95628963235939,9.61377648024676));
#26521=CARTESIAN_POINT('Ctrl Pts',(0.358627202431044,1.93721945301948,9.6127355572179));
#26522=CARTESIAN_POINT('Ctrl Pts',(0.349122190795714,1.91889620132642,9.61169463418905));
#26523=CARTESIAN_POINT('Ctrl Pts',(0.339612297634139,1.90056353928885,9.61065317656926));
#26524=CARTESIAN_POINT('Ctrl Pts',(0.328653152168805,1.88297923180463,9.60961171894947));
#26525=CARTESIAN_POINT('Ctrl Pts',(0.316392620254153,1.86637508726869,9.60857026132967));
#26526=CARTESIAN_POINT('Ctrl Pts',(0.304128342212484,1.84976586944272,9.60752848549918));
#26527=CARTESIAN_POINT('Ctrl Pts',(0.29056235193232,1.83413798067474,9.60648670966868));
#26528=CARTESIAN_POINT('Ctrl Pts',(0.275883202181507,1.8196906195753,9.60544493383818));
#26529=CARTESIAN_POINT('Ctrl Pts',(0.261172323115398,1.805212030177,9.60440090618558));
#26530=CARTESIAN_POINT('Ctrl Pts',(0.245344044860583,1.79191953649461,9.60335687853298));
#26531=CARTESIAN_POINT('Ctrl Pts',(0.228620988110442,1.77997291709075,9.60231285088039));
#26532=CARTESIAN_POINT('Ctrl Pts',(0.22270626213964,1.77574755440096,9.60194359198452));
#26533=CARTESIAN_POINT('Ctrl Pts',(0.216679861056863,1.77169015078198,9.60157433308866));
#26534=CARTESIAN_POINT('Ctrl Pts',(0.210552393540732,1.76780641250279,9.60120507419279));
#26535=CARTESIAN_POINT('Ctrl Pts',(0.193228918649381,1.75682637182742,9.60016111154524));
#26536=CARTESIAN_POINT('Ctrl Pts',(0.174992622155822,1.74717235976401,9.59911714889769));
#26537=CARTESIAN_POINT('Ctrl Pts',(0.156072638020975,1.73899276785475,9.59807318625014));
#26538=CARTESIAN_POINT('Ctrl Pts',(0.137187459235691,1.73082822318621,9.59703114408437));
#26539=CARTESIAN_POINT('Ctrl Pts',(0.117621733466298,1.72413305802274,9.5959891019186));
#26540=CARTESIAN_POINT('Ctrl Pts',(0.0976293765910314,1.71900998067345,
9.59494705975283));
#26541=CARTESIAN_POINT('Ctrl Pts',(0.0776584911929713,1.71389240542875,
9.59390613672398));
#26542=CARTESIAN_POINT('Ctrl Pts',(0.0572625862718146,1.71034377585844,
9.59286521369513));
#26543=CARTESIAN_POINT('Ctrl Pts',(0.0367108336389134,1.70841705260119,
9.59182429066628));
#26544=CARTESIAN_POINT('Ctrl Pts',(0.0161485261615035,1.7064893398291,9.59078283304649));
#26545=CARTESIAN_POINT('Ctrl Pts',(-0.00456905786697798,1.7061852821836,
9.5897413754267));
#26546=CARTESIAN_POINT('Ctrl Pts',(-0.0251669673389064,1.70750603347954,
9.58869991780691));
#26547=CARTESIAN_POINT('Ctrl Pts',(-0.0457711703701748,1.70882718832258,
9.58765814197641));
#26548=CARTESIAN_POINT('Ctrl Pts',(-0.0662548947145264,1.71177405727269,
9.58661636614591));
#26549=CARTESIAN_POINT('Ctrl Pts',(-0.0863485835935361,1.7162959315939,
9.58557459031542));
#26550=CARTESIAN_POINT('Ctrl Pts',(-0.106485705437037,1.72082758004908,
9.58453056266282));
#26551=CARTESIAN_POINT('Ctrl Pts',(-0.126230405137249,1.72694081279087,
9.58348653501023));
#26552=CARTESIAN_POINT('Ctrl Pts',(-0.145327829414169,1.73453493737737,
9.58244250735763));
#26553=CARTESIAN_POINT('Ctrl Pts',(-0.152082338056697,1.73722087970174,
9.58207324846176));
#26554=CARTESIAN_POINT('Ctrl Pts',(-0.158756075461235,1.7400916397396,9.58170398956589));
#26555=CARTESIAN_POINT('Ctrl Pts',(-0.165338501025232,1.74314138643052,
9.58133473067002));
#26556=CARTESIAN_POINT('Ctrl Pts',(-0.183948225790025,1.75176357987102,
9.58029076802246));
#26557=CARTESIAN_POINT('Ctrl Pts',(-0.201937128783059,1.76187109330564,
9.5792468053749));
#26558=CARTESIAN_POINT('Ctrl Pts',(-0.219056405385582,1.77335159382059,
9.57820284272735));
#26559=CARTESIAN_POINT('Ctrl Pts',(-0.236144189234087,1.78481097471775,
9.57716080056158));
#26560=CARTESIAN_POINT('Ctrl Pts',(-0.252364884865585,1.79763797338003,
9.57611875839581));
#26561=CARTESIAN_POINT('Ctrl Pts',(-0.267494684041996,1.81167469065434,
9.57507671623003));
#26562=CARTESIAN_POINT('Ctrl Pts',(-0.282608234051773,1.8256963327148,9.57403579320118));
#26563=CARTESIAN_POINT('Ctrl Pts',(-0.296632657194975,1.84092463744261,
9.57299487017232));
#26564=CARTESIAN_POINT('Ctrl Pts',(-0.309377715653273,1.85716194891006,
9.57195394714347));
#26565=CARTESIAN_POINT('Ctrl Pts',(-0.322129319641413,1.87340759943747,
9.57091248952367));
#26566=CARTESIAN_POINT('Ctrl Pts',(-0.333599779331321,1.89066272312678,
9.56987103190388));
#26567=CARTESIAN_POINT('Ctrl Pts',(-0.343639288572217,1.90869676074467,
9.56882957428409));
#26568=CARTESIAN_POINT('Ctrl Pts',(-0.353681865320874,1.92673630854728,
9.56778779845359));
#26569=CARTESIAN_POINT('Ctrl Pts',(-0.362292295250751,1.94555458413378,
9.56674602262309));
#26570=CARTESIAN_POINT('Ctrl Pts',(-0.369367299220206,1.96489748978361,
9.56570424679258));
#26571=CARTESIAN_POINT('Ctrl Pts',(-0.376457595971295,1.98428220556294,
9.56466021913999));
#26572=CARTESIAN_POINT('Ctrl Pts',(-0.382005643140109,2.00419310592989,
9.56361619148739));
#26573=CARTESIAN_POINT('Ctrl Pts',(-0.385958148049284,2.02436139904541,
9.56257216383479));
#26574=CARTESIAN_POINT('Ctrl Pts',(-0.387356097227164,2.03149465995919,
9.56220290493893));
#26575=CARTESIAN_POINT('Ctrl Pts',(-0.388554925431945,2.03866005213765,
9.56183364604307));
#26576=CARTESIAN_POINT('Ctrl Pts',(-0.389553829705013,2.04584555639509,
9.56146438714721));
#26577=CARTESIAN_POINT('Ctrl Pts',(-0.392031787472687,2.06367046371548,
9.56054837549931));
#26578=CARTESIAN_POINT('Ctrl Pts',(-0.39328671362501,2.08166924724648,9.5596323638514));
#26579=CARTESIAN_POINT('Ctrl Pts',(-0.393299895050531,2.09971267920167,
9.55871635220349));
#26580=CARTESIAN_POINT('',(-0.393077129544589,2.09984967721303,9.43371639324307));
#26581=CARTESIAN_POINT('Ctrl Pts',(-0.393666275384297,2.09971558385956,
9.55871619130454));
#26582=CARTESIAN_POINT('Ctrl Pts',(-0.392741356830577,2.21224405877622,
9.5530088087445));
#26583=CARTESIAN_POINT('Ctrl Pts',(-0.283104739668165,2.45693363482398,
9.54067797834354));
#26584=CARTESIAN_POINT('Ctrl Pts',(0.132384636875694,2.54581311263665,9.52172370010165));
#26585=CARTESIAN_POINT('Ctrl Pts',(0.446509843093515,2.2300153202515,9.50185335657885));
#26586=CARTESIAN_POINT('Ctrl Pts',(0.351023055099136,1.79494617152333,9.48198301305608));
#26587=CARTESIAN_POINT('Ctrl Pts',(-0.0664795984751189,1.63972238109351,
9.46211266953325));
#26588=CARTESIAN_POINT('Ctrl Pts',(-0.355148157932989,1.85592482976135,
9.44602381903774));
#26589=CARTESIAN_POINT('Ctrl Pts',(-0.392897886971203,2.0434661290281,9.43655841638312));
#26590=CARTESIAN_POINT('Ctrl Pts',(-0.392706122236906,2.09984846278313,
9.43371646156944));
#26591=CARTESIAN_POINT('',(-0.39329984275683,2.10035169226946,9.30871635220092));
#26592=CARTESIAN_POINT('Ctrl Pts',(-0.393299971550761,2.09985040664878,
9.43371635220349));
#26593=CARTESIAN_POINT('Ctrl Pts',(-0.393308015136027,2.12099801668889,
9.43265201369966));
#26594=CARTESIAN_POINT('Ctrl Pts',(-0.391606066910142,2.14213467488965,
9.43158767519583));
#26595=CARTESIAN_POINT('Ctrl Pts',(-0.388225481374075,2.1629751189905,9.430523336692));
#26596=CARTESIAN_POINT('Ctrl Pts',(-0.384842081218753,2.18383291449827,
9.42945811203764));
#26597=CARTESIAN_POINT('Ctrl Pts',(-0.379777418637733,2.20439333155889,
9.42839288738329));
#26598=CARTESIAN_POINT('Ctrl Pts',(-0.373113810665123,2.22438237130297,
9.42732766272893));
#26599=CARTESIAN_POINT('Ctrl Pts',(-0.366430817956512,2.24442956006482,
9.42625933928804));
#26600=CARTESIAN_POINT('Ctrl Pts',(-0.358139858177786,2.26390141332144,
9.42519101584714));
#26601=CARTESIAN_POINT('Ctrl Pts',(-0.348371642207012,2.28254338910514,
9.42412269240625));
#26602=CARTESIAN_POINT('Ctrl Pts',(-0.343035769838522,2.29272653859486,
9.42353912243339));
#26603=CARTESIAN_POINT('Ctrl Pts',(-0.337259910800024,2.30266250215418,
9.42295555246054));
#26604=CARTESIAN_POINT('Ctrl Pts',(-0.331070784138775,2.31231350849566,
9.42237198248769));
#26605=CARTESIAN_POINT('Ctrl Pts',(-0.319998903548804,2.32957843061383,
9.42132801984014));
#26606=CARTESIAN_POINT('Ctrl Pts',(-0.307539881826998,2.3460263860022,9.42028405719258));
#26607=CARTESIAN_POINT('Ctrl Pts',(-0.29383883054216,2.36142614954441,9.41924009454503));
#26608=CARTESIAN_POINT('Ctrl Pts',(-0.280162983817534,2.37679758356217,
9.41819805237926));
#26609=CARTESIAN_POINT('Ctrl Pts',(-0.265250081977773,2.39112407022735,
9.41715601021349));
#26610=CARTESIAN_POINT('Ctrl Pts',(-0.249286981977645,2.4042053428467,9.41611396804772));
#26611=CARTESIAN_POINT('Ctrl Pts',(-0.233341026096144,2.41727256638475,
9.41507304501887));
#26612=CARTESIAN_POINT('Ctrl Pts',(-0.216347659082994,2.42909674445078,
9.41403212199002));
#26613=CARTESIAN_POINT('Ctrl Pts',(-0.198528562223755,2.43951627351479,
9.41299119896117));
#26614=CARTESIAN_POINT('Ctrl Pts',(-0.180700313940784,2.44994115377736,
9.41194974134137));
#26615=CARTESIAN_POINT('Ctrl Pts',(-0.162046115631449,2.45895955854018,
9.41090828372158));
#26616=CARTESIAN_POINT('Ctrl Pts',(-0.142814750372396,2.46645441336689,
9.40986682610179));
#26617=CARTESIAN_POINT('Ctrl Pts',(-0.123577509092841,2.4739515581985,9.40882505027129));
#26618=CARTESIAN_POINT('Ctrl Pts',(-0.10376344790945,2.47992399313295,9.4077832744408));
#26619=CARTESIAN_POINT('Ctrl Pts',(-0.083638345225797,2.48430393857973,
9.4067414986103));
#26620=CARTESIAN_POINT('Ctrl Pts',(-0.0634697416759932,2.48869335137798,
9.4056974709577));
#26621=CARTESIAN_POINT('Ctrl Pts',(-0.042989484103173,2.49148330309068,
9.40465344330511));
#26622=CARTESIAN_POINT('Ctrl Pts',(-0.0224711137025956,2.49265753405349,
9.40360941565251));
#26623=CARTESIAN_POINT('Ctrl Pts',(-0.0152140350416648,2.4930728441535,
9.40324015675664));
#26624=CARTESIAN_POINT('Ctrl Pts',(-0.00795219096330203,2.49328651380395,
9.40287089786078));
#26625=CARTESIAN_POINT('Ctrl Pts',(-0.000697598238044414,2.49329938133272,
9.40250163896491));
#26626=CARTESIAN_POINT('Ctrl Pts',(0.0198124664162429,2.49333576019738,
9.40145767631736));
#26627=CARTESIAN_POINT('Ctrl Pts',(0.0403864953755422,2.49176356710999,
9.40041371366981));
#26628=CARTESIAN_POINT('Ctrl Pts',(0.0607515189078829,2.48857964814229,
9.39936975102225));
#26629=CARTESIAN_POINT('Ctrl Pts',(0.0810790787849739,2.48540158633661,
9.39832770885648));
#26630=CARTESIAN_POINT('Ctrl Pts',(0.101197668504876,2.48061773755848,9.39728566669072));
#26631=CARTESIAN_POINT('Ctrl Pts',(0.12083775120033,2.47427680650135,9.39624362452495));
#26632=CARTESIAN_POINT('Ctrl Pts',(0.140456740755505,2.46794268550456,9.39520270149609));
#26633=CARTESIAN_POINT('Ctrl Pts',(0.159597537992918,2.46005499950062,9.39416177846724));
#26634=CARTESIAN_POINT('Ctrl Pts',(0.178004263685736,2.45071266317272,9.39312085543838));
#26635=CARTESIAN_POINT('Ctrl Pts',(0.196420442593136,2.44136552886436,9.39207939781859));
#26636=CARTESIAN_POINT('Ctrl Pts',(0.214101133391507,2.4305625703843,9.3910379401988));
#26637=CARTESIAN_POINT('Ctrl Pts',(0.230813227024003,2.41844959448988,9.38999648257901));
#26638=CARTESIAN_POINT('Ctrl Pts',(0.247530426929695,2.40633291755323,9.38895470674851));
#26639=CARTESIAN_POINT('Ctrl Pts',(0.263277866491292,2.39290588709676,9.38791293091801));
#26640=CARTESIAN_POINT('Ctrl Pts',(0.27785468476336,2.37835528404371,9.38687115508751));
#26641=CARTESIAN_POINT('Ctrl Pts',(0.292463011158912,2.36377322953197,9.38582712743492));
#26642=CARTESIAN_POINT('Ctrl Pts',(0.30589518599026,2.34806331355167,9.38478309978232));
#26643=CARTESIAN_POINT('Ctrl Pts',(0.317989465048927,2.33144673278726,9.38373907212972));
#26644=CARTESIAN_POINT('Ctrl Pts',(0.322267053023165,2.32556966597691,9.38336981323386));
#26645=CARTESIAN_POINT('Ctrl Pts',(0.326377677703724,2.3195794406995,9.38300055433799));
#26646=CARTESIAN_POINT('Ctrl Pts',(0.33031553907667,2.31348661467288,9.38263129544212));
#26647=CARTESIAN_POINT('Ctrl Pts',(0.34144859566814,2.29626107762825,9.38158733279456));
#26648=CARTESIAN_POINT('Ctrl Pts',(0.351263761195903,2.27811100918802,9.38054337014701));
#26649=CARTESIAN_POINT('Ctrl Pts',(0.359610620332432,2.25926421991183,9.37949940749946));
#26650=CARTESIAN_POINT('Ctrl Pts',(0.367942124522152,2.24045210133538,9.37845736533369));
#26651=CARTESIAN_POINT('Ctrl Pts',(0.374810334952862,2.22094644710565,9.37741532316792));
#26652=CARTESIAN_POINT('Ctrl Pts',(0.380110298226388,2.20100025337714,9.37637328100215));
#26653=CARTESIAN_POINT('Ctrl Pts',(0.385404569422622,2.18107548154733,9.37533235797329));
#26654=CARTESIAN_POINT('Ctrl Pts',(0.389133721203222,2.16071180957053,9.37429143494444));
#26655=CARTESIAN_POINT('Ctrl Pts',(0.391242410755887,2.1401779295873,9.37325051191559));
#26656=CARTESIAN_POINT('Ctrl Pts',(0.393352183276546,2.1196335039385,9.37220905429579));
#26657=CARTESIAN_POINT('Ctrl Pts',(0.393839739765151,2.09891942593101,9.371167596676));
#26658=CARTESIAN_POINT('Ctrl Pts',(0.392701491009382,2.07831062566582,9.37012613905621));
#26659=CARTESIAN_POINT('Ctrl Pts',(0.391562894468995,2.05769552851368,9.36908436322571));
#26660=CARTESIAN_POINT('Ctrl Pts',(0.388797580431339,2.03718650518495,9.36804258739521));
#26661=CARTESIAN_POINT('Ctrl Pts',(0.384453867981806,2.01705355104751,9.36700081156471));
#26662=CARTESIAN_POINT('Ctrl Pts',(0.380100766499244,1.99687707907284,9.36595678391212));
#26663=CARTESIAN_POINT('Ctrl Pts',(0.374162666806837,1.97707900459952,9.36491275625952));
#26664=CARTESIAN_POINT('Ctrl Pts',(0.366737999974684,1.95791506281604,9.36386872860693));
#26665=CARTESIAN_POINT('Ctrl Pts',(0.364111992636864,1.95113702780348,9.36349946971106));
#26666=CARTESIAN_POINT('Ctrl Pts',(0.361300459386208,1.94443812379475,9.3631302108152));
#26667=CARTESIAN_POINT('Ctrl Pts',(0.358309137688568,1.93782894262886,9.36276095191933));
#26668=CARTESIAN_POINT('Ctrl Pts',(0.349852122423335,1.91914357486826,9.36171698927178));
#26669=CARTESIAN_POINT('Ctrl Pts',(0.33990434636196,1.9010658479604,9.36067302662422));
#26670=CARTESIAN_POINT('Ctrl Pts',(0.328575934167167,1.88384555177796,9.35962906397667));
#26671=CARTESIAN_POINT('Ctrl Pts',(0.31726836180732,1.86665693418596,9.3585870218109));
#26672=CARTESIAN_POINT('Ctrl Pts',(0.304585544901078,1.85032325680539,9.35754497964513));
#26673=CARTESIAN_POINT('Ctrl Pts',(0.290683393974063,1.83506971772234,9.35650293747936));
#26674=CARTESIAN_POINT('Ctrl Pts',(0.276796173738736,1.81983256070063,9.35546201445051));
#26675=CARTESIAN_POINT('Ctrl Pts',(0.26169269098198,1.8056737995261,9.35442109142165));
#26676=CARTESIAN_POINT('Ctrl Pts',(0.245568908802071,1.79278541533684,9.3533801683928));
#26677=CARTESIAN_POINT('Ctrl Pts',(0.229436845867876,1.77989041200937,9.35233871077301));
#26678=CARTESIAN_POINT('Ctrl Pts',(0.212284001343244,1.76826756107926,9.35129725315322));
#26679=CARTESIAN_POINT('Ctrl Pts',(0.194339598474054,1.75806870505181,9.35025579553342));
#26680=CARTESIAN_POINT('Ctrl Pts',(0.176389712807485,1.74786673282922,9.34921401970293));
#26681=CARTESIAN_POINT('Ctrl Pts',(0.157648444336629,1.73908995348095,9.34817224387243));
#26682=CARTESIAN_POINT('Ctrl Pts',(0.138368965994907,1.73184389282602,9.34713046804193));
#26683=CARTESIAN_POINT('Ctrl Pts',(0.119047814623232,1.72458216964655,9.34608644038933));
#26684=CARTESIAN_POINT('Ctrl Pts',(0.0991868384755821,1.71885797474502,
9.34504241273674));
#26685=CARTESIAN_POINT('Ctrl Pts',(0.0790543467939964,1.71472697959372,
9.34399838508414));
#26686=CARTESIAN_POINT('Ctrl Pts',(0.0719337483779574,1.71326590075678,
9.34362912618827));
#26687=CARTESIAN_POINT('Ctrl Pts',(0.0647792561978769,1.71200365047125,
9.34325986729241));
#26688=CARTESIAN_POINT('Ctrl Pts',(0.0576028818555596,1.71094113812697,
9.34289060839654));
#26689=CARTESIAN_POINT('Ctrl Pts',(0.0373139549208018,1.70793722078765,
9.34184664574899));
#26690=CARTESIAN_POINT('Ctrl Pts',(0.0167289675391714,1.70651568878983,
9.34080268310143));
#26691=CARTESIAN_POINT('Ctrl Pts',(-0.00388244002228689,1.7067191631169,
9.33975872045388));
#26692=CARTESIAN_POINT('Ctrl Pts',(-0.0244559306785246,1.70692226313101,
9.33871667828811));
#26693=CARTESIAN_POINT('Ctrl Pts',(-0.0450550170198653,1.70874448796688,
9.33767463612234));
#26694=CARTESIAN_POINT('Ctrl Pts',(-0.0654059512788471,1.71217664905616,
9.33663259395657));
#26695=CARTESIAN_POINT('Ctrl Pts',(-0.0857350289541158,1.71560512405834,
9.33559167092772));
#26696=CARTESIAN_POINT('Ctrl Pts',(-0.105815756972389,1.72064000952241,
9.33455074789886));
#26697=CARTESIAN_POINT('Ctrl Pts',(-0.125380635789518,1.72722045902569,
9.33350982487001));
#26698=CARTESIAN_POINT('Ctrl Pts',(-0.144955562618521,1.73380428807634,
9.33246836725022));
#26699=CARTESIAN_POINT('Ctrl Pts',(-0.164013408453982,1.74193504764372,
9.33142690963042));
#26700=CARTESIAN_POINT('Ctrl Pts',(-0.182302418713991,1.75150219781033,
9.33038545201063));
#26701=CARTESIAN_POINT('Ctrl Pts',(-0.200597017063961,1.76107227115841,
9.32934367618013));
#26702=CARTESIAN_POINT('Ctrl Pts',(-0.218121677539342,1.77207923599203,
9.32830190034963));
#26703=CARTESIAN_POINT('Ctrl Pts',(-0.234650625058717,1.78436734300844,
9.32726012451913));
#26704=CARTESIAN_POINT('Ctrl Pts',(-0.251215300273235,1.796682011047,9.32621609686654));
#26705=CARTESIAN_POINT('Ctrl Pts',(-0.26677941108841,1.81028286526066,9.32517206921394));
#26706=CARTESIAN_POINT('Ctrl Pts',(-0.281150907292824,1.82497444240867,
9.32412804156134));
#26707=CARTESIAN_POINT('Ctrl Pts',(-0.286233917122273,1.83017066067233,
9.32375878266548));
#26708=CARTESIAN_POINT('Ctrl Pts',(-0.29116809565268,1.83550300690712,9.32338952376961));
#26709=CARTESIAN_POINT('Ctrl Pts',(-0.295946176155712,1.84096187381234,
9.32302026487375));
#26710=CARTESIAN_POINT('Ctrl Pts',(-0.309342113939787,1.85626648020972,
9.32198500203293));
#26711=CARTESIAN_POINT('Ctrl Pts',(-0.321591288173481,1.87266297689702,
9.32094973919211));
#26712=CARTESIAN_POINT('Ctrl Pts',(-0.332512749399159,1.88995200194476,
9.3199144763513));
#26713=CARTESIAN_POINT('Ctrl Pts',(-0.343414206542394,1.90720935988541,
9.31888110972956));
#26714=CARTESIAN_POINT('Ctrl Pts',(-0.352992325725242,1.92535541064501,
9.31784774310783));
#26715=CARTESIAN_POINT('Ctrl Pts',(-0.36110725838568,1.94415893371393,9.3168143764861));
#26716=CARTESIAN_POINT('Ctrl Pts',(-0.369213280638338,1.96294181002394,
9.31578214452788));
#26717=CARTESIAN_POINT('Ctrl Pts',(-0.375858982692616,1.98238005234684,
9.31474991256966));
#26718=CARTESIAN_POINT('Ctrl Pts',(-0.380951273679245,2.00221954652303,
9.31371768061144));
#26719=CARTESIAN_POINT('Ctrl Pts',(-0.386045781822523,2.0220676787104,9.31268499922486));
#26720=CARTESIAN_POINT('Ctrl Pts',(-0.389585330442199,2.04231668851366,
9.31165231783829));
#26721=CARTESIAN_POINT('Ctrl Pts',(-0.391527158554774,2.0626988724832,9.31061963645172));
#26722=CARTESIAN_POINT('Ctrl Pts',(-0.392720121168889,2.07522067259115,
9.30998520836897));
#26723=CARTESIAN_POINT('Ctrl Pts',(-0.393311073280722,2.08779251965456,
9.30935078028623));
#26724=CARTESIAN_POINT('Ctrl Pts',(-0.393299842756876,2.10035169221859,
9.30871635220349));
#26725=CARTESIAN_POINT('',(-0.393299999141086,2.09997400728266,9.18371635220034));
#26726=CARTESIAN_POINT('Ctrl Pts',(-0.39329984275683,2.10035169226946,9.30871635220092));
#26727=CARTESIAN_POINT('Ctrl Pts',(-0.393276918768292,2.1259877436425,9.30742134404343));
#26728=CARTESIAN_POINT('Ctrl Pts',(-0.390743538263717,2.15151131211032,
9.30612633588594));
#26729=CARTESIAN_POINT('Ctrl Pts',(-0.385788147102442,2.17650095133568,
9.30483132772845));
#26730=CARTESIAN_POINT('Ctrl Pts',(-0.3836434948974,2.18731625998109,9.30427085893595));
#26731=CARTESIAN_POINT('Ctrl Pts',(-0.381045787453246,2.19803185263539,
9.30371039014345));
#26732=CARTESIAN_POINT('Ctrl Pts',(-0.378004906977851,2.20861482541838,
9.30314992135095));
#26733=CARTESIAN_POINT('Ctrl Pts',(-0.372340781384306,2.22832730260418,
9.3021059587034));
#26734=CARTESIAN_POINT('Ctrl Pts',(-0.36511365658114,2.24765425595428,9.30106199605585));
#26735=CARTESIAN_POINT('Ctrl Pts',(-0.35639635214647,2.26633258903982,9.30001803340831));
#26736=CARTESIAN_POINT('Ctrl Pts',(-0.347695084132652,2.28497656131894,
9.29897599124254));
#26737=CARTESIAN_POINT('Ctrl Pts',(-0.337509331717907,2.30297359744135,
9.29793394907677));
#26738=CARTESIAN_POINT('Ctrl Pts',(-0.325960777005166,2.32007830845903,
9.29689190691101));
#26739=CARTESIAN_POINT('Ctrl Pts',(-0.314424625258767,2.33716464928578,
9.29585098388216));
#26740=CARTESIAN_POINT('Ctrl Pts',(-0.301528962527767,2.35335994465526,
9.29481006085331));
#26741=CARTESIAN_POINT('Ctrl Pts',(-0.287439908603183,2.36844587711901,
9.29376913782447));
#26742=CARTESIAN_POINT('Ctrl Pts',(-0.273343618907707,2.38353955732448,
9.29272768020468));
#26743=CARTESIAN_POINT('Ctrl Pts',(-0.258053204014208,2.3975221876711,9.29168622258489));
#26744=CARTESIAN_POINT('Ctrl Pts',(-0.241773502075295,2.4102103539443,9.29064476496511));
#26745=CARTESIAN_POINT('Ctrl Pts',(-0.225488825977706,2.42290239700545,
9.28960298913462));
#26746=CARTESIAN_POINT('Ctrl Pts',(-0.208214863174154,2.43429876522881,
9.28856121330412));
#26747=CARTESIAN_POINT('Ctrl Pts',(-0.190186851712651,2.44425840793745,
9.28751943747363));
#26748=CARTESIAN_POINT('Ctrl Pts',(-0.172119872295267,2.45423957863982,
9.28647540982104));
#26749=CARTESIAN_POINT('Ctrl Pts',(-0.153296260927022,2.46277751960126,
9.28543138216845));
#26750=CARTESIAN_POINT('Ctrl Pts',(-0.133973446854709,2.46977831945352,
9.28438735451586));
#26751=CARTESIAN_POINT('Ctrl Pts',(-0.127139220795381,2.47225441059674,
9.28401809561996));
#26752=CARTESIAN_POINT('Ctrl Pts',(-0.120242686105858,2.47453867052581,
9.28364883672406));
#26753=CARTESIAN_POINT('Ctrl Pts',(-0.113295596369067,2.47662846127633,
9.28327957782816));
#26754=CARTESIAN_POINT('Ctrl Pts',(-0.093654899083327,2.48253668314717,
9.28223561518061));
#26755=CARTESIAN_POINT('Ctrl Pts',(-0.0734922774274372,2.48692201627976,
9.28119165253306));
#26756=CARTESIAN_POINT('Ctrl Pts',(-0.053068366142764,2.48970326982839,
9.2801476898855));
#26757=CARTESIAN_POINT('Ctrl Pts',(-0.0326820268436989,2.49247940696142,
9.27910564771974));
#26758=CARTESIAN_POINT('Ctrl Pts',(-0.0120360648190486,2.49365716480032,
9.27806360555397));
#26759=CARTESIAN_POINT('Ctrl Pts',(0.00859732378919101,2.49320602236444,
9.2770215633882));
#26760=CARTESIAN_POINT('Ctrl Pts',(0.0292085524622095,2.49275536444845,
9.27598064035934));
#26761=CARTESIAN_POINT('Ctrl Pts',(0.0498065020218985,2.49067926634919,
9.27493971733049));
#26762=CARTESIAN_POINT('Ctrl Pts',(0.0701176836042718,2.48699922538162,
9.27389879430164));
#26763=CARTESIAN_POINT('Ctrl Pts',(0.0904392964801287,2.48331729444092,
9.27285733668184));
#26764=CARTESIAN_POINT('Ctrl Pts',(0.110473120288156,2.47802989028964,9.27181587906205));
#26765=CARTESIAN_POINT('Ctrl Pts',(0.129954054479622,2.47120995908557,9.27077442144226));
#26766=CARTESIAN_POINT('Ctrl Pts',(0.149440940945777,2.46438794409518,9.26973264561176));
#26767=CARTESIAN_POINT('Ctrl Pts',(0.168373919579263,2.45603274692879,9.26869086978126));
#26768=CARTESIAN_POINT('Ctrl Pts',(0.186507053839617,2.4462658066689,9.26764909395076));
#26769=CARTESIAN_POINT('Ctrl Pts',(0.20467938328117,2.436477754946,9.26660506629817));
#26770=CARTESIAN_POINT('Ctrl Pts',(0.222047797862864,2.4252722671955,9.26556103864557));
#26771=CARTESIAN_POINT('Ctrl Pts',(0.238393984122121,2.41281495861672,9.26451701099297));
#26772=CARTESIAN_POINT('Ctrl Pts',(0.24417541594022,2.40840897185975,9.26414775209711));
#26773=CARTESIAN_POINT('Ctrl Pts',(0.249829281426239,2.40384675318856,9.26377849320124));
#26774=CARTESIAN_POINT('Ctrl Pts',(0.255347000105666,2.39913675724831,9.26340923430538));
#26775=CARTESIAN_POINT('Ctrl Pts',(0.270946603163401,2.38582073456935,9.26236527165782));
#26776=CARTESIAN_POINT('Ctrl Pts',(0.285548261195769,2.37124150134435,9.26132130901027));
#26777=CARTESIAN_POINT('Ctrl Pts',(0.298942621191147,2.35557425385857,9.26027734636271));
#26778=CARTESIAN_POINT('Ctrl Pts',(0.31231234081799,2.33993582796278,9.25923530419694));
#26779=CARTESIAN_POINT('Ctrl Pts',(0.324478652988779,2.32321387503814,9.25819326203117));
#26780=CARTESIAN_POINT('Ctrl Pts',(0.335268550426577,2.30562074091604,9.2571512198654));
#26781=CARTESIAN_POINT('Ctrl Pts',(0.346046859684032,2.2880465015436,9.25611029683655));
#26782=CARTESIAN_POINT('Ctrl Pts',(0.355451281508906,2.26960354734637,9.25506937380769));
#26783=CARTESIAN_POINT('Ctrl Pts',(0.363351846764805,2.25053346954284,9.25402845077883));
#26784=CARTESIAN_POINT('Ctrl Pts',(0.371256469545107,2.23145359784438,9.25298699315904));
#26785=CARTESIAN_POINT('Ctrl Pts',(0.377655396282505,2.21174663268889,9.25194553553925));
#26786=CARTESIAN_POINT('Ctrl Pts',(0.38246645769543,2.19167496243746,9.25090407791946));
#26787=CARTESIAN_POINT('Ctrl Pts',(0.387278989097361,2.17159715941572,9.24986230208896));
#26788=CARTESIAN_POINT('Ctrl Pts',(0.390502553156715,2.15115515280235,9.24882052625846));
#26789=CARTESIAN_POINT('Ctrl Pts',(0.392106128135219,2.13062146761354,9.24777875042796));
#26790=CARTESIAN_POINT('Ctrl Pts',(0.393713169277429,2.11004339839823,9.24673472277536));
#26791=CARTESIAN_POINT('Ctrl Pts',(0.39369323118985,2.0893739914575,9.24569069512276));
#26792=CARTESIAN_POINT('Ctrl Pts',(0.392067389075343,2.06888645915934,9.24464666747017));
#26793=CARTESIAN_POINT('Ctrl Pts',(0.391492350030588,2.06164028753111,9.24427740857431));
#26794=CARTESIAN_POINT('Ctrl Pts',(0.390716894434591,2.05441680480078,9.24390814967844));
#26795=CARTESIAN_POINT('Ctrl Pts',(0.389743486338488,2.04722780223716,9.24353889078258));
#26796=CARTESIAN_POINT('Ctrl Pts',(0.386991483056925,2.02690317300357,9.24249492813503));
#26797=CARTESIAN_POINT('Ctrl Pts',(0.382637144057309,2.00673383512157,9.24145096548748));
#26798=CARTESIAN_POINT('Ctrl Pts',(0.376714450945086,1.98699065326646,9.24040700283993));
#26799=CARTESIAN_POINT('Ctrl Pts',(0.370802653265048,1.96728379112182,9.23936496067416));
#26800=CARTESIAN_POINT('Ctrl Pts',(0.363328380459119,1.94800224275369,9.23832291850839));
#26801=CARTESIAN_POINT('Ctrl Pts',(0.354376524739197,1.92940642241348,9.23728087634262));
#26802=CARTESIAN_POINT('Ctrl Pts',(0.345434283171689,1.91083057369218,9.23623995331377));
#26803=CARTESIAN_POINT('Ctrl Pts',(0.335017900533861,1.89293966309146,9.23519903028492));
#26804=CARTESIAN_POINT('Ctrl Pts',(0.323260156405853,1.87597374868006,9.23415810725606));
#26805=CARTESIAN_POINT('Ctrl Pts',(0.311496373806907,1.85899912101721,9.23311664963627));
#26806=CARTESIAN_POINT('Ctrl Pts',(0.298390259327344,1.84295105252664,9.23207519201648));
#26807=CARTESIAN_POINT('Ctrl Pts',(0.284117954082259,1.82804066817241,9.23103373439669));
#26808=CARTESIAN_POINT('Ctrl Pts',(0.269841288025699,1.81312572804571,9.2299919585662));
#26809=CARTESIAN_POINT('Ctrl Pts',(0.254398256335101,1.79934967012524,9.2289501827357));
#26810=CARTESIAN_POINT('Ctrl Pts',(0.238001210296019,1.78688610075944,9.2279084069052));
#26811=CARTESIAN_POINT('Ctrl Pts',(0.221568721669827,1.77439559110562,9.22686437925261));
#26812=CARTESIAN_POINT('Ctrl Pts',(0.20417872139403,1.76322363195713,9.22582035160001));
#26813=CARTESIAN_POINT('Ctrl Pts',(0.186072339707431,1.75350039769748,9.22477632394741));
#26814=CARTESIAN_POINT('Ctrl Pts',(0.179668349838829,1.75006141718958,9.22440706505155));
#26815=CARTESIAN_POINT('Ctrl Pts',(0.173174948101331,1.74680323241671,9.22403780615568));
#26816=CARTESIAN_POINT('Ctrl Pts',(0.166603382640256,1.7437301543874,9.22366854725981));
#26817=CARTESIAN_POINT('Ctrl Pts',(0.148024361378827,1.73504199897257,9.22262458461226));
#26818=CARTESIAN_POINT('Ctrl Pts',(0.128708538589659,1.72778517813287,9.2215806219647));
#26819=CARTESIAN_POINT('Ctrl Pts',(0.108902056998447,1.72207774346897,9.22053665931715));
#26820=CARTESIAN_POINT('Ctrl Pts',(0.089132011564391,1.71638080824614,9.21949461715138));
#26821=CARTESIAN_POINT('Ctrl Pts',(0.0688737815508266,1.71222786011648,
9.21845257498561));
#26822=CARTESIAN_POINT('Ctrl Pts',(0.0483922816111024,1.70968848712795,
9.21741053281984));
#26823=CARTESIAN_POINT('Ctrl Pts',(0.0279327784805518,1.70715184138611,
9.21636960979098));
#26824=CARTESIAN_POINT('Ctrl Pts',(0.00725120438777207,1.7062254492305,
9.21532868676212));
#26825=CARTESIAN_POINT('Ctrl Pts',(-0.0133787195590345,1.70692761498299,
9.21428776373327));
#26826=CARTESIAN_POINT('Ctrl Pts',(-0.0340192384970955,1.70763014134951,
9.21324630611348));
#26827=CARTESIAN_POINT('Ctrl Pts',(-0.0546073183950077,1.7099628876167,
9.21220484849368));
#26828=CARTESIAN_POINT('Ctrl Pts',(-0.0748700932346642,1.71389203693911,
9.21116339087389));
#26829=CARTESIAN_POINT('Ctrl Pts',(-0.0951390592354162,1.71782238678793,
9.21012161504339));
#26830=CARTESIAN_POINT('Ctrl Pts',(-0.115081807478783,1.72334993526144,
9.20907983921289));
#26831=CARTESIAN_POINT('Ctrl Pts',(-0.134437417050862,1.73039010985,9.20803806338239));
#26832=CARTESIAN_POINT('Ctrl Pts',(-0.153834864212262,1.7374455019357,9.20699403572979));
#26833=CARTESIAN_POINT('Ctrl Pts',(-0.172641968858013,1.74601974217327,
9.2059500080772));
#26834=CARTESIAN_POINT('Ctrl Pts',(-0.190618749880555,1.75598054968654,
9.2049059804246));
#26835=CARTESIAN_POINT('Ctrl Pts',(-0.196976901693017,1.75950355674018,
9.20453672152873));
#26836=CARTESIAN_POINT('Ctrl Pts',(-0.203231437474636,1.76319961089218,
9.20416746263287));
#26837=CARTESIAN_POINT('Ctrl Pts',(-0.209372643627946,1.76706158812741,
9.203798203737));
#26838=CARTESIAN_POINT('Ctrl Pts',(-0.226734960167222,1.77798010633889,
9.20275424108945));
#26839=CARTESIAN_POINT('Ctrl Pts',(-0.243292628948694,1.79029294773496,
9.2017102784419));
#26840=CARTESIAN_POINT('Ctrl Pts',(-0.258813148567935,1.80385705456933,
9.20066631579434));
#26841=CARTESIAN_POINT('Ctrl Pts',(-0.274305116518906,1.81739620876756,
9.19962427362858));
#26842=CARTESIAN_POINT('Ctrl Pts',(-0.288763135611631,1.83218162541249,
9.19858223146281));
#26843=CARTESIAN_POINT('Ctrl Pts',(-0.301985291880888,1.84802822878819,
9.19754018929704));
#26844=CARTESIAN_POINT('Ctrl Pts',(-0.315193247762026,1.86385781316081,
9.19649926626819));
#26845=CARTESIAN_POINT('Ctrl Pts',(-0.327167484621689,1.88074577813618,
9.19545834323933));
#26846=CARTESIAN_POINT('Ctrl Pts',(-0.337744441676624,1.89847188256587,
9.19441742021048));
#26847=CARTESIAN_POINT('Ctrl Pts',(-0.348326830781034,1.9162070906608,9.19337596259069));
#26848=CARTESIAN_POINT('Ctrl Pts',(-0.357510115604936,1.93478067456031,
9.1923345049709));
#26849=CARTESIAN_POINT('Ctrl Pts',(-0.365175022651471,1.95394489796143,
9.19129304735111));
#26850=CARTESIAN_POINT('Ctrl Pts',(-0.37284227166127,1.97311497686828,9.19025127152062));
#26851=CARTESIAN_POINT('Ctrl Pts',(-0.378989979904125,1.99287535851908,
9.18920949569012));
#26852=CARTESIAN_POINT('Ctrl Pts',(-0.383548016255117,2.01296087531021,
9.18816771985962));
#26853=CARTESIAN_POINT('Ctrl Pts',(-0.388115904905117,2.03308980740168,
9.18712369220703));
#26854=CARTESIAN_POINT('Ctrl Pts',(-0.391087155764448,2.05354454888473,
9.18607966455443));
#26855=CARTESIAN_POINT('Ctrl Pts',(-0.3924430868525,2.07405171331897,9.18503563690184));
#26856=CARTESIAN_POINT('Ctrl Pts',(-0.392922661905138,2.08130482857657,
9.18466637800597));
#26857=CARTESIAN_POINT('Ctrl Pts',(-0.393200646629442,2.08856449514136,
9.1842971191101));
#26858=CARTESIAN_POINT('Ctrl Pts',(-0.393277772879087,2.09581868928856,
9.18392786021423));
#26859=CARTESIAN_POINT('Ctrl Pts',(-0.393292498608396,2.09720373393763,
9.18385735754398));
#26860=CARTESIAN_POINT('Ctrl Pts',(-0.393299907597943,2.0985888565162,9.18378685487374));
#26861=CARTESIAN_POINT('Ctrl Pts',(-0.393299999141082,2.09997400722057,
9.1837163522035));
#26862=CARTESIAN_POINT('',(-0.393244728382793,2.09966251899669,9.05871635508085));
#26863=CARTESIAN_POINT('Ctrl Pts',(-0.393299999141086,2.09997400728267,
9.18371635220034));
#26864=CARTESIAN_POINT('Ctrl Pts',(-0.393301352116386,2.12044609480224,
9.18267434512414));
#26865=CARTESIAN_POINT('Ctrl Pts',(-0.391699967753018,2.14098035704797,
9.18163233804793));
#26866=CARTESIAN_POINT('Ctrl Pts',(-0.388492761615384,2.16130468312007,
9.18059033097173));
#26867=CARTESIAN_POINT('Ctrl Pts',(-0.385291446452698,2.18159167760493,
9.1795502378472));
#26868=CARTESIAN_POINT('Ctrl Pts',(-0.380490218272511,2.2016687703632,9.17851014472268));
#26869=CARTESIAN_POINT('Ctrl Pts',(-0.374137850478265,2.22126730325815,
9.17747005159816));
#26870=CARTESIAN_POINT('Ctrl Pts',(-0.367792238111552,2.24084499408711,
9.176431064561));
#26871=CARTESIAN_POINT('Ctrl Pts',(-0.359898959910504,2.25994442708309,
9.17539207752384));
#26872=CARTESIAN_POINT('Ctrl Pts',(-0.350556982617022,2.2783106613146,9.17435309048668));
#26873=CARTESIAN_POINT('Ctrl Pts',(-0.341210125737006,2.29668648876459,
9.17331356075636));
#26874=CARTESIAN_POINT('Ctrl Pts',(-0.330413379812743,2.31432768705437,
9.17227403102604));
#26875=CARTESIAN_POINT('Ctrl Pts',(-0.318312550590783,2.33100218643206,
9.17123450129572));
#26876=CARTESIAN_POINT('Ctrl Pts',(-0.306207738221479,2.34768217444087,
9.17019462939049));
#26877=CARTESIAN_POINT('Ctrl Pts',(-0.292798452407534,2.36339425514184,
9.16915475748527));
#26878=CARTESIAN_POINT('Ctrl Pts',(-0.278271375868845,2.37793871873501,
9.16811488558005));
#26879=CARTESIAN_POINT('Ctrl Pts',(-0.263713205734665,2.39251431313873,
9.16707278794439));
#26880=CARTESIAN_POINT('Ctrl Pts',(-0.248033032995366,2.40591682380063,
9.16603069030873));
#26881=CARTESIAN_POINT('Ctrl Pts',(-0.231451767951575,2.41798580017367,
9.16498859267307));
#26882=CARTESIAN_POINT('Ctrl Pts',(-0.226513517414322,2.42158019595113,
9.16467823401253));
#26883=CARTESIAN_POINT('Ctrl Pts',(-0.221495531294459,2.42505660773875,
9.16436787535198));
#26884=CARTESIAN_POINT('Ctrl Pts',(-0.216404085447837,2.42841157379344,
9.16405751669143));
#26885=CARTESIAN_POINT('Ctrl Pts',(-0.199277837781505,2.43969677279108,
9.16301355404388));
#26886=CARTESIAN_POINT('Ctrl Pts',(-0.181215421465795,2.44967232167622,
9.16196959139633));
#26887=CARTESIAN_POINT('Ctrl Pts',(-0.162443305784822,2.45818579313772,
9.16092562874878));
#26888=CARTESIAN_POINT('Ctrl Pts',(-0.14370572343345,2.46668360315109,9.15988358658301));
#26889=CARTESIAN_POINT('Ctrl Pts',(-0.124261671175083,2.4737243199629,9.15884154441724));
#26890=CARTESIAN_POINT('Ctrl Pts',(-0.104363205590169,2.47920075332064,
9.15779950225147));
#26891=CARTESIAN_POINT('Ctrl Pts',(-0.0844861106446941,2.484671305075,9.15675857922261));
#26892=CARTESIAN_POINT('Ctrl Pts',(-0.0641562693648319,2.4885806864732,
9.15571765619376));
#26893=CARTESIAN_POINT('Ctrl Pts',(-0.0436418731385263,2.49087117687156,
9.15467673316491));
#26894=CARTESIAN_POINT('Ctrl Pts',(-0.0231169412529887,2.4931628436061,
9.15363527554512));
#26895=CARTESIAN_POINT('Ctrl Pts',(-0.00240799451223308,2.4938338606837,
9.15259381792533));
#26896=CARTESIAN_POINT('Ctrl Pts',(0.0182100795606655,2.49287820377618,
9.15155236030553));
#26897=CARTESIAN_POINT('Ctrl Pts',(0.0388344533540614,2.4919222548738,9.15051058447504));
#26898=CARTESIAN_POINT('Ctrl Pts',(0.0593671665102165,2.48933871271772,
9.14946880864454));
#26899=CARTESIAN_POINT('Ctrl Pts',(0.0795378062558533,2.4851735029516,9.14842703281404));
#26900=CARTESIAN_POINT('Ctrl Pts',(0.0997520452970297,2.48099928999005,
9.14738300516144));
#26901=CARTESIAN_POINT('Ctrl Pts',(0.119601941168201,2.47523678925586,9.14633897750885));
#26902=CARTESIAN_POINT('Ctrl Pts',(0.138830896837623,2.46798216272431,9.14529494985625));
#26903=CARTESIAN_POINT('Ctrl Pts',(0.1456319264095,2.46541629641195,9.14492569096038));
#26904=CARTESIAN_POINT('Ctrl Pts',(0.152355471420382,2.46266421054394,9.14455643206452));
#26905=CARTESIAN_POINT('Ctrl Pts',(0.15899088962587,2.45973154854137,9.14418717316865));
#26906=CARTESIAN_POINT('Ctrl Pts',(0.177750434311075,2.45144037499663,9.1431432105211));
#26907=CARTESIAN_POINT('Ctrl Pts',(0.195915566738622,2.44165311682019,9.14209924787354));
#26908=CARTESIAN_POINT('Ctrl Pts',(0.21323553138064,2.43047768178323,9.14105528522599));
#26909=CARTESIAN_POINT('Ctrl Pts',(0.230523634081362,2.41932280516324,9.14001324306022));
#26910=CARTESIAN_POINT('Ctrl Pts',(0.246969011655613,2.40678516511853,9.13897120089445));
#26911=CARTESIAN_POINT('Ctrl Pts',(0.262345093838543,2.39301867131438,9.13792915872867));
#26912=CARTESIAN_POINT('Ctrl Pts',(0.277704662350762,2.37926696250831,9.13688823569982));
#26913=CARTESIAN_POINT('Ctrl Pts',(0.291996650647147,2.3642894867558,9.13584731267097));
#26914=CARTESIAN_POINT('Ctrl Pts',(0.305027349332828,2.34828049895026,9.13480638964211));
#26915=CARTESIAN_POINT('Ctrl Pts',(0.318064740245736,2.33226328934582,9.13376493202232));
#26916=CARTESIAN_POINT('Ctrl Pts',(0.329839070476426,2.31521406981387,9.13272347440253));
#26917=CARTESIAN_POINT('Ctrl Pts',(0.340196473078747,2.29736070962778,9.13168201678273));
#26918=CARTESIAN_POINT('Ctrl Pts',(0.35055704031911,2.27950189446181,9.13064024095223));
#26919=CARTESIAN_POINT('Ctrl Pts',(0.359499480451559,2.26083910356379,9.12959846512173));
#26920=CARTESIAN_POINT('Ctrl Pts',(0.366916029259334,2.2416245652158,9.12855668929124));
#26921=CARTESIAN_POINT('Ctrl Pts',(0.37434860910566,2.22236849420713,9.12751266163864));
#26922=CARTESIAN_POINT('Ctrl Pts',(0.380248502614248,2.20255900058928,9.12646863398604));
#26923=CARTESIAN_POINT('Ctrl Pts',(0.384557663885936,2.18246388995549,9.12542460633344));
#26924=CARTESIAN_POINT('Ctrl Pts',(0.386081757744297,2.17535651272613,9.12505534743758));
#26925=CARTESIAN_POINT('Ctrl Pts',(0.387407331073193,2.16821348189271,9.12468608854171));
#26926=CARTESIAN_POINT('Ctrl Pts',(0.388533368122952,2.16104680053069,9.12431682964585));
#26927=CARTESIAN_POINT('Ctrl Pts',(0.391716881459736,2.14078527742953,9.1232728669983));
#26928=CARTESIAN_POINT('Ctrl Pts',(0.393320693956306,2.12021368915352,9.12222890435075));
#26929=CARTESIAN_POINT('Ctrl Pts',(0.393299797900577,2.09960128786642,9.12118494170319));
#26930=CARTESIAN_POINT('Ctrl Pts',(0.393278940285393,2.0790268053126,9.12014289953742));
#26931=CARTESIAN_POINT('Ctrl Pts',(0.391639248087145,2.05841238630684,9.11910085737166));
#26932=CARTESIAN_POINT('Ctrl Pts',(0.388387484729823,2.03803184926721,9.11805881520589));
#26933=CARTESIAN_POINT('Ctrl Pts',(0.385139213715263,2.0176732006042,9.11701789217703));
#26934=CARTESIAN_POINT('Ctrl Pts',(0.380282395444754,1.9975486627047,9.11597696914818));
#26935=CARTESIAN_POINT('Ctrl Pts',(0.37387550451514,1.97792626357996,9.11493604611933));
#26936=CARTESIAN_POINT('Ctrl Pts',(0.367465323173333,1.95829378690246,9.11389458849954));
#26937=CARTESIAN_POINT('Ctrl Pts',(0.359503691837624,1.93916466863988,9.11285313087975));
#26938=CARTESIAN_POINT('Ctrl Pts',(0.350098916114789,1.92079163263048,9.11181167325996));
#26939=CARTESIAN_POINT('Ctrl Pts',(0.340691266822953,1.90241298285757,9.11076989742946));
#26940=CARTESIAN_POINT('Ctrl Pts',(0.329839962513473,1.884791513157,9.10972812159896));
#26941=CARTESIAN_POINT('Ctrl Pts',(0.317698746524207,1.86815436933824,9.10868634576847));
#26942=CARTESIAN_POINT('Ctrl Pts',(0.305531287021062,1.85148126395558,9.10764231811587));
#26943=CARTESIAN_POINT('Ctrl Pts',(0.292068829070921,1.83579729102943,9.10659829046327));
#26944=CARTESIAN_POINT('Ctrl Pts',(0.277505127117448,1.82129622459764,9.10555426281068));
#26945=CARTESIAN_POINT('Ctrl Pts',(0.272354136633885,1.81616738747709,9.10518500391481));
#26946=CARTESIAN_POINT('Ctrl Pts',(0.267065705212036,1.81118617003201,9.10481574501894));
#26947=CARTESIAN_POINT('Ctrl Pts',(0.261649375409,1.80635992380453,9.10444648612307));
#26948=CARTESIAN_POINT('Ctrl Pts',(0.246336417307073,1.79271524023496,9.10340252347552));
#26949=CARTESIAN_POINT('Ctrl Pts',(0.229907630246419,1.78023095353374,9.10235856082796));
#26950=CARTESIAN_POINT('Ctrl Pts',(0.21256504277933,1.76909065805236,9.10131459818041));
#26951=CARTESIAN_POINT('Ctrl Pts',(0.195254358870659,1.75797085634495,9.10027255601464));
#26952=CARTESIAN_POINT('Ctrl Pts',(0.177033791267862,1.74819058141618,9.09923051384887));
#26953=CARTESIAN_POINT('Ctrl Pts',(0.158137232563017,1.73989236931535,9.0981884716831));
#26954=CARTESIAN_POINT('Ctrl Pts',(0.139260968465368,1.73160306936396,9.09714754865424));
#26955=CARTESIAN_POINT('Ctrl Pts',(0.119710813195054,1.72479299313183,9.09610662562539));
#26956=CARTESIAN_POINT('Ctrl Pts',(0.0997437828586238,1.71955806253641,
9.09506570259653));
#26957=CARTESIAN_POINT('Ctrl Pts',(0.0797664979758132,1.71432044341707,
9.09402424497674));
#26958=CARTESIAN_POINT('Ctrl Pts',(0.0593726179459746,1.71065978823548,
9.09298278735695));
#26959=CARTESIAN_POINT('Ctrl Pts',(0.0388332652790696,1.70862183567837,
9.09194132973715));
#26960=CARTESIAN_POINT('Ctrl Pts',(0.0182876369444851,1.70658326043792,
9.09089955390665));
#26961=CARTESIAN_POINT('Ctrl Pts',(-0.00240281737467288,1.70616841143858,
9.08985777807616));
#26962=CARTESIAN_POINT('Ctrl Pts',(-0.0229638853681445,1.70737097666016,
9.08881600224566));
#26963=CARTESIAN_POINT('Ctrl Pts',(-0.0435693965766733,1.70857614125375,
9.08777197459306));
#26964=CARTESIAN_POINT('Ctrl Pts',(-0.0640442335644598,1.71140559899892,
9.08672794694046));
#26965=CARTESIAN_POINT('Ctrl Pts',(-0.084120584869788,1.71580133107835,
9.08568391928786));
#26966=CARTESIAN_POINT('Ctrl Pts',(-0.0912213271705936,1.71735604389667,
9.085314660392));
#26967=CARTESIAN_POINT('Ctrl Pts',(-0.098272347468519,1.71910622871434,
9.08494540149614));
#26968=CARTESIAN_POINT('Ctrl Pts',(-0.10526229889673,1.7210478415011,9.08457614260027));
#26969=CARTESIAN_POINT('Ctrl Pts',(-0.125024174049869,1.72653713708229,
9.08353217995272));
#26970=CARTESIAN_POINT('Ctrl Pts',(-0.144414385117009,1.73359278542209,
9.08248821730516));
#26971=CARTESIAN_POINT('Ctrl Pts',(-0.163169200974503,1.74214430023634,
9.08144425465761));
#26972=CARTESIAN_POINT('Ctrl Pts',(-0.181889515327279,1.7506800836176,9.08040221249184));
#26973=CARTESIAN_POINT('Ctrl Pts',(-0.199976068065358,1.76070602354879,
9.07936017032607));
#26974=CARTESIAN_POINT('Ctrl Pts',(-0.217182402040207,1.77210261628972,
9.0783181281603));
#26975=CARTESIAN_POINT('Ctrl Pts',(-0.234370256682658,1.78348696926908,
9.07727720513144));
#26976=CARTESIAN_POINT('Ctrl Pts',(-0.25067914300557,1.79623867253913,9.07623628210259));
#26977=CARTESIAN_POINT('Ctrl Pts',(-0.265889280680861,1.8101935466229,9.07519535907374));
#26978=CARTESIAN_POINT('Ctrl Pts',(-0.281107229886447,1.82415558756629,
9.07415390145395));
#26979=CARTESIAN_POINT('Ctrl Pts',(-0.295224750059093,1.83932154824162,
9.07311244383415));
#26980=CARTESIAN_POINT('Ctrl Pts',(-0.308056619778545,1.8554882231658,9.07207098621436));
#26981=CARTESIAN_POINT('Ctrl Pts',(-0.320892410193626,1.87165983771399,
9.07102921038386));
#26982=CARTESIAN_POINT('Ctrl Pts',(-0.332441339435636,1.88883217689623,
9.06998743455336));
#26983=CARTESIAN_POINT('Ctrl Pts',(-0.342560278685943,1.90677126128184,
9.06894565872286));
#26984=CARTESIAN_POINT('Ctrl Pts',(-0.352701090253059,1.92474912140544,
9.06790163107027));
#26985=CARTESIAN_POINT('Ctrl Pts',(-0.361405430739534,1.94349636753665,
9.06685760341767));
#26986=CARTESIAN_POINT('Ctrl Pts',(-0.368577112222484,1.96275641236934,
9.06581357576507));
#26987=CARTESIAN_POINT('Ctrl Pts',(-0.37111364195833,1.96956843777063,9.06544431686921));
#26988=CARTESIAN_POINT('Ctrl Pts',(-0.373458899918739,1.97644446854687,
9.06507505797335));
#26989=CARTESIAN_POINT('Ctrl Pts',(-0.375610144132728,1.98337277494259,
9.06470579907749));
#26990=CARTESIAN_POINT('Ctrl Pts',(-0.382959707516277,2.00704281048059,
9.0634442539482));
#26991=CARTESIAN_POINT('Ctrl Pts',(-0.388076627771857,2.03143715382748,
9.06218270881891));
#26992=CARTESIAN_POINT('Ctrl Pts',(-0.390850208804052,2.05617073719729,
9.06092116368962));
#26993=CARTESIAN_POINT('Ctrl Pts',(-0.392466008626093,2.07057973377733,
9.06018622774517));
#26994=CARTESIAN_POINT('Ctrl Pts',(-0.393287360126491,2.08510347310958,
9.05945129180072));
#26995=CARTESIAN_POINT('Ctrl Pts',(-0.393299855154148,2.09966245633422,
9.05871635585627));
#26996=CARTESIAN_POINT('',(-0.393095239940488,2.10019047587301,8.93371634952743));
#26997=CARTESIAN_POINT('Ctrl Pts',(-0.393040168128258,2.09966275151986,
9.0587163522035));
#26998=CARTESIAN_POINT('Ctrl Pts',(-0.392294723781914,2.19126251015094,
9.0540893866539));
#26999=CARTESIAN_POINT('Ctrl Pts',(-0.314706016092101,2.41512451888509,
9.04283897326335));
#27000=CARTESIAN_POINT('Ctrl Pts',(0.0583154564568577,2.56138306321075,
9.02496511203192));
#27001=CARTESIAN_POINT('Ctrl Pts',(0.419506350600682,2.30072230888762,9.0050947685091));
#27002=CARTESIAN_POINT('Ctrl Pts',(0.395857278700936,1.85592616203501,8.98522442498634));
#27003=CARTESIAN_POINT('Ctrl Pts',(0.00906304469525043,1.63503453386264,
8.96535408146352));
#27004=CARTESIAN_POINT('Ctrl Pts',(-0.332338020341264,1.81273119149951,
8.94818472386927));
#27005=CARTESIAN_POINT('Ctrl Pts',(-0.392402917414063,2.02238938101501,
8.93763881411591));
#27006=CARTESIAN_POINT('Ctrl Pts',(-0.392742359999847,2.10019025177715,
8.93371635220349));
#27007=CARTESIAN_POINT('',(-0.393444746249714,2.10025436408896,8.8087163522035));
#27008=CARTESIAN_POINT('Ctrl Pts',(-0.393299953813117,2.10019060587623,
8.93371634797498));
#27009=CARTESIAN_POINT('Ctrl Pts',(-0.393288928936479,2.12293955548056,
8.9325710447093));
#27010=CARTESIAN_POINT('Ctrl Pts',(-0.391299996201274,2.14562110664529,
8.93142574144361));
#27011=CARTESIAN_POINT('Ctrl Pts',(-0.387392643545173,2.16791045373933,
8.93028043817793));
#27012=CARTESIAN_POINT('Ctrl Pts',(-0.383457008456061,2.19036113691475,
8.92912684490985));
#27013=CARTESIAN_POINT('Ctrl Pts',(-0.377575283507818,2.21241347444076,
8.92797325164176));
#27014=CARTESIAN_POINT('Ctrl Pts',(-0.369857635818388,2.23375432414256,
8.92681965837368));
#27015=CARTESIAN_POINT('Ctrl Pts',(-0.3671676293004,2.24119273376002,8.92641757038844));
#27016=CARTESIAN_POINT('Ctrl Pts',(-0.364255000440692,2.24854490221534,
8.9260154824032));
#27017=CARTESIAN_POINT('Ctrl Pts',(-0.361125734524206,2.25579824730835,
8.92561339441796));
#27018=CARTESIAN_POINT('Ctrl Pts',(-0.353001053233094,2.27463049702693,
8.9245694317704));
#27019=CARTESIAN_POINT('Ctrl Pts',(-0.343375080858931,2.29288160972106,
8.92352546912285));
#27020=CARTESIAN_POINT('Ctrl Pts',(-0.332353499814773,2.31029988388221,
8.9224815064753));
#27021=CARTESIAN_POINT('Ctrl Pts',(-0.321352194156588,2.32768611525112,
8.92143946430953));
#27022=CARTESIAN_POINT('Ctrl Pts',(-0.308960714688259,2.34424190269951,
8.92039742214376));
#27023=CARTESIAN_POINT('Ctrl Pts',(-0.295330958138818,2.35973932156069,
8.91935537997799));
#27024=CARTESIAN_POINT('Ctrl Pts',(-0.281715839733789,2.37522009643748,
8.91831445694914));
#27025=CARTESIAN_POINT('Ctrl Pts',(-0.266865546132116,2.3896441904931,8.91727353392028));
#27026=CARTESIAN_POINT('Ctrl Pts',(-0.250972608780928,2.40281618127454,
8.91623261089143));
#27027=CARTESIAN_POINT('Ctrl Pts',(-0.235071509231343,2.41599493684714,
8.91519115327164));
#27028=CARTESIAN_POINT('Ctrl Pts',(-0.21812725238961,2.42791982255356,8.91414969565184));
#27029=CARTESIAN_POINT('Ctrl Pts',(-0.200366335677794,2.43843495907937,
8.91310823803205));
#27030=CARTESIAN_POINT('Ctrl Pts',(-0.182599992231609,2.44895330843781,
8.91206646220155));
#27031=CARTESIAN_POINT('Ctrl Pts',(-0.164017143206278,2.4580607077223,8.91102468637106));
#27032=CARTESIAN_POINT('Ctrl Pts',(-0.144869052442489,2.46564716277364,
8.90998291054056));
#27033=CARTESIAN_POINT('Ctrl Pts',(-0.125679572645992,2.47325001611974,
8.90893888288796));
#27034=CARTESIAN_POINT('Ctrl Pts',(-0.105923115829145,2.47932514532429,
8.90789485523536));
#27035=CARTESIAN_POINT('Ctrl Pts',(-0.0858669629241464,2.4838121346156,
8.90685082758277));
#27036=CARTESIAN_POINT('Ctrl Pts',(-0.0787733645327732,2.48539912391358,
8.9064815686869));
#27037=CARTESIAN_POINT('Ctrl Pts',(-0.0716423554947472,2.48678791628016,
8.90611230979103));
#27038=CARTESIAN_POINT('Ctrl Pts',(-0.0644859294174,2.4879773896855,8.90574305089517));
#27039=CARTESIAN_POINT('Ctrl Pts',(-0.0442533998876345,2.49134024923835,
8.90469908824761));
#27040=CARTESIAN_POINT('Ctrl Pts',(-0.0236968247830544,2.49312621639706,
8.90365512560006));
#27041=CARTESIAN_POINT('Ctrl Pts',(-0.00308504703835625,2.49328790025218,
8.90261116295251));
#27042=CARTESIAN_POINT('Ctrl Pts',(0.0174888131201405,2.49344928667243,
8.90156912078674));
#27043=CARTESIAN_POINT('Ctrl Pts',(0.03811694736396,2.49199225576357,8.90052707862097));
#27044=CARTESIAN_POINT('Ctrl Pts',(0.0585254881084704,2.48892114527455,
8.89948503645519));
#27045=CARTESIAN_POINT('Ctrl Pts',(0.0789121104008293,2.48585333310995,
8.89844411342634));
#27046=CARTESIAN_POINT('Ctrl Pts',(0.0990788791916744,2.48117496310345,
8.89740319039749));
#27047=CARTESIAN_POINT('Ctrl Pts',(0.118757259032441,2.47494213343808,8.89636226736863));
#27048=CARTESIAN_POINT('Ctrl Pts',(0.13844574517621,2.46870610275385,8.89532080974884));
#27049=CARTESIAN_POINT('Ctrl Pts',(0.157644634977628,2.46091422432674,8.89427935212905));
#27050=CARTESIAN_POINT('Ctrl Pts',(0.176100255171075,2.45167256095505,8.89323789450926));
#27051=CARTESIAN_POINT('Ctrl Pts',(0.194561514361092,2.44242807385229,8.89219611867876));
#27052=CARTESIAN_POINT('Ctrl Pts',(0.212278410690057,2.43173328147029,8.89115434284826));
#27053=CARTESIAN_POINT('Ctrl Pts',(0.229022445442515,2.41973990911916,8.89011256701776));
#27054=CARTESIAN_POINT('Ctrl Pts',(0.24580267280606,2.40772061282153,8.88906853936516));
#27055=CARTESIAN_POINT('Ctrl Pts',(0.261605277264181,2.39439760741178,8.88802451171256));
#27056=CARTESIAN_POINT('Ctrl Pts',(0.276234776156258,2.37996292333433,8.88698048405997));
#27057=CARTESIAN_POINT('Ctrl Pts',(0.281409038154505,2.37485756478243,8.8866112251641));
#27058=CARTESIAN_POINT('Ctrl Pts',(0.286436903683232,2.36961346310885,8.88624196626824));
#27059=CARTESIAN_POINT('Ctrl Pts',(0.291310936963311,2.36424009537835,8.88587270737237));
#27060=CARTESIAN_POINT('Ctrl Pts',(0.305090723298343,2.34904859893771,8.88482874472482));
#27061=CARTESIAN_POINT('Ctrl Pts',(0.317720041999881,2.33273103883036,8.88378478207726));
#27062=CARTESIAN_POINT('Ctrl Pts',(0.329013516404515,2.31548780945366,8.88274081942971));
#27063=CARTESIAN_POINT('Ctrl Pts',(0.34028621524604,2.29827630085546,8.88169877726394));
#27064=CARTESIAN_POINT('Ctrl Pts',(0.350227499363535,2.28014307909137,8.88065673509817));
#27065=CARTESIAN_POINT('Ctrl Pts',(0.35869276654196,2.26132076503189,8.8796146929324));
#27066=CARTESIAN_POINT('Ctrl Pts',(0.36714894215642,2.24251866584202,8.87857376990355));
#27067=CARTESIAN_POINT('Ctrl Pts',(0.374131921228497,2.22302959935182,8.8775328468747));
#27068=CARTESIAN_POINT('Ctrl Pts',(0.37954350902445,2.20310972193449,8.87649192384585));
#27069=CARTESIAN_POINT('Ctrl Pts',(0.384957876070851,2.18317961418729,8.87545046622605));
#27070=CARTESIAN_POINT('Ctrl Pts',(0.388799031131988,2.16281895931506,8.87440900860626));
#27071=CARTESIAN_POINT('Ctrl Pts',(0.391018835785393,2.14229846405055,8.87336755098647));
#27072=CARTESIAN_POINT('Ctrl Pts',(0.393239318685896,2.12177169888011,8.87232577515597));
#27073=CARTESIAN_POINT('Ctrl Pts',(0.393837421874313,2.1010857308776,8.87128399932548));
#27074=CARTESIAN_POINT('Ctrl Pts',(0.392817028224559,2.08051481750595,8.87024222349498));
#27075=CARTESIAN_POINT('Ctrl Pts',(0.391794428970775,2.05989943963825,8.86919819584238));
#27076=CARTESIAN_POINT('Ctrl Pts',(0.389146442810179,2.03940034331423,8.86815416818979));
#27077=CARTESIAN_POINT('Ctrl Pts',(0.384928714082289,2.0192858434043,8.86711014053719));
#27078=CARTESIAN_POINT('Ctrl Pts',(0.383436958716179,2.01217160844204,8.86674088164133));
#27079=CARTESIAN_POINT('Ctrl Pts',(0.38174929859508,2.00510536209381,8.86637162274546));
#27080=CARTESIAN_POINT('Ctrl Pts',(0.379869677083126,1.9980984866022,8.86600236384959));
#27081=CARTESIAN_POINT('Ctrl Pts',(0.374555642209548,1.97828876401688,8.86495840120204));
#27082=CARTESIAN_POINT('Ctrl Pts',(0.367672023925872,1.95883681660674,8.86391443855449));
#27083=CARTESIAN_POINT('Ctrl Pts',(0.359286969691899,1.94000698949763,8.86287047590693));
#27084=CARTESIAN_POINT('Ctrl Pts',(0.350917340668729,1.92121180188451,8.86182843374116));
#27085=CARTESIAN_POINT('Ctrl Pts',(0.341051999865725,1.90303715161852,8.86078639157539));
#27086=CARTESIAN_POINT('Ctrl Pts',(0.329808263283925,1.88573054471147,8.85974434940962));
#27087=CARTESIAN_POINT('Ctrl Pts',(0.31857660229858,1.86844252482837,8.85870342638077));
#27088=CARTESIAN_POINT('Ctrl Pts',(0.30596985900002,1.85202132716239,8.85766250335192));
#27089=CARTESIAN_POINT('Ctrl Pts',(0.292150259669528,1.83668817767706,8.85662158032306));
#27090=CARTESIAN_POINT('Ctrl Pts',(0.278323562953001,1.82134715348578,8.85558012270327));
#27091=CARTESIAN_POINT('Ctrl Pts',(0.263283246431304,1.80709585116084,8.85453866508348));
#27092=CARTESIAN_POINT('Ctrl Pts',(0.247230866974281,1.79412128479552,8.85349720746368));
#27093=CARTESIAN_POINT('Ctrl Pts',(0.231173582815509,1.78114275413453,8.85245543163319));
#27094=CARTESIAN_POINT('Ctrl Pts',(0.214104214612402,1.76944217001355,8.85141365580269));
#27095=CARTESIAN_POINT('Ctrl Pts',(0.196255464820033,1.7591647281629,8.85037187997219));
#27096=CARTESIAN_POINT('Ctrl Pts',(0.178368134549949,1.74886507138846,8.84932785231959));
#27097=CARTESIAN_POINT('Ctrl Pts',(0.159698724582217,1.73999501432749,8.84828382466699));
#27098=CARTESIAN_POINT('Ctrl Pts',(0.140502960150279,1.73265301391054,8.8472397970144));
#27099=CARTESIAN_POINT('Ctrl Pts',(0.133713669884053,1.7300562446002,8.84687053811853));
#27100=CARTESIAN_POINT('Ctrl Pts',(0.126858682520048,1.72765017261927,8.84650127922266));
#27101=CARTESIAN_POINT('Ctrl Pts',(0.119949703065909,1.72543764373018,8.8461320203268));
#27102=CARTESIAN_POINT('Ctrl Pts',(0.100416750539694,1.71918241862199,8.84508805767924));
#27103=CARTESIAN_POINT('Ctrl Pts',(0.0803349779260562,1.71444059751436,
8.84404409503169));
#27104=CARTESIAN_POINT('Ctrl Pts',(0.0599635407910791,1.71129797559596,
8.84300013238414));
#27105=CARTESIAN_POINT('Ctrl Pts',(0.0396295791098609,1.70816113486923,
8.84195809021837));
#27106=CARTESIAN_POINT('Ctrl Pts',(0.0190077205282317,1.70661782346517,
8.8409160480526));
#27107=CARTESIAN_POINT('Ctrl Pts',(-0.00163042219651427,1.70670337946601,
8.83987400588683));
#27108=CARTESIAN_POINT('Ctrl Pts',(-0.022246399880189,1.70678884358104,
8.83883308285797));
#27109=CARTESIAN_POINT('Ctrl Pts',(-0.0428778948260887,1.70849972805363,
8.83779215982912));
#27110=CARTESIAN_POINT('Ctrl Pts',(-0.0632510802658689,1.71181938373329,
8.83675123680026));
#27111=CARTESIAN_POINT('Ctrl Pts',(-0.0836347288427016,1.71514074430159,
8.83570977918047));
#27112=CARTESIAN_POINT('Ctrl Pts',(-0.103759074092783,1.72007242426745,
8.83466832156068));
#27113=CARTESIAN_POINT('Ctrl Pts',(-0.12335776484255,1.72654618511381,8.83362686394089));
#27114=CARTESIAN_POINT('Ctrl Pts',(-0.142962443846772,1.73302192397633,
8.83258508811039));
#27115=CARTESIAN_POINT('Ctrl Pts',(-0.162040461899702,1.74104041677721,
8.83154331227989));
#27116=CARTESIAN_POINT('Ctrl Pts',(-0.180343769788057,1.75048460019817,
8.83050153644939));
#27117=CARTESIAN_POINT('Ctrl Pts',(-0.198686640691771,1.75994919743591,
8.8294575087968));
#27118=CARTESIAN_POINT('Ctrl Pts',(-0.216250832431912,1.77084524944222,
8.8284134811442));
#27119=CARTESIAN_POINT('Ctrl Pts',(-0.232815131968949,1.78301103437772,
8.8273694534916));
#27120=CARTESIAN_POINT('Ctrl Pts',(-0.238673707594395,1.78731391304327,
8.82700019459574));
#27121=CARTESIAN_POINT('Ctrl Pts',(-0.244407504517051,1.79177525891498,
8.82663093569987));
#27122=CARTESIAN_POINT('Ctrl Pts',(-0.250007793836785,1.79638677067548,
8.82626167680401));
#27123=CARTESIAN_POINT('Ctrl Pts',(-0.265626250513275,1.80924765919971,
8.82523186321079));
#27124=CARTESIAN_POINT('Ctrl Pts',(-0.280302271003942,1.82336043277438,
8.82420204961756));
#27125=CARTESIAN_POINT('Ctrl Pts',(-0.293826368015407,1.8385598434462,8.82317223602434));
#27126=CARTESIAN_POINT('Ctrl Pts',(-0.307325503409736,1.85373120035077,
8.82214432317263));
#27127=CARTESIAN_POINT('Ctrl Pts',(-0.319676387843176,1.86998469896286,
8.82111641032092));
#27128=CARTESIAN_POINT('Ctrl Pts',(-0.330704857821977,1.88711696400853,
8.82008849746921));
#27129=CARTESIAN_POINT('Ctrl Pts',(-0.341729443646336,1.90424319518336,
8.81906094664163));
#27130=CARTESIAN_POINT('Ctrl Pts',(-0.35143208895433,1.92224697056919,8.81803339581405));
#27131=CARTESIAN_POINT('Ctrl Pts',(-0.359680771461609,1.94089427213082,
8.81700584498647));
#27132=CARTESIAN_POINT('Ctrl Pts',(-0.367927090802008,1.9595362314229,8.81597858854216));
#27133=CARTESIAN_POINT('Ctrl Pts',(-0.374719976175961,1.97882065423493,
8.81495133209784));
#27134=CARTESIAN_POINT('Ctrl Pts',(-0.379975191608948,1.99849264183448,
8.81392407565353));
#27135=CARTESIAN_POINT('Ctrl Pts',(-0.385240027035102,2.01820064021013,
8.81289493875349));
#27136=CARTESIAN_POINT('Ctrl Pts',(-0.388961406089882,2.03829687848715,
8.81186580185344));
#27137=CARTESIAN_POINT('Ctrl Pts',(-0.391105947897405,2.05851473129806,
8.8108366649534));
#27138=CARTESIAN_POINT('Ctrl Pts',(-0.392578735219475,2.07239956077302,
8.81012989403676));
#27139=CARTESIAN_POINT('Ctrl Pts',(-0.393308912464174,2.0863415328013,8.80942312312013));
#27140=CARTESIAN_POINT('Ctrl Pts',(-0.393299917806418,2.10025427045661,
8.8087163522035));
#27141=CARTESIAN_POINT('',(-0.393343477685089,2.09967036236989,8.6837163522035));
#27142=CARTESIAN_POINT('Ctrl Pts',(-0.393737740759854,2.10025455351144,
8.8087163522035));
#27143=CARTESIAN_POINT('Ctrl Pts',(-0.393852405531071,2.11552756370832,
8.80794134589607));
#27144=CARTESIAN_POINT('Ctrl Pts',(-0.386105851649887,2.26121113565208,
8.80054289174776));
#27145=CARTESIAN_POINT('Ctrl Pts',(-0.204430308564429,2.51771194909898,
8.78652098975839));
#27146=CARTESIAN_POINT('Ctrl Pts',(0.240557865830071,2.49800368926257,8.76665064623566));
#27147=CARTESIAN_POINT('Ctrl Pts',(0.464866947321644,2.11318122783806,8.74678030271284));
#27148=CARTESIAN_POINT('Ctrl Pts',(0.26272389056588,1.71626678433389,8.72690995919007));
#27149=CARTESIAN_POINT('Ctrl Pts',(-0.180432569156138,1.67137532564354,
8.70703961566727));
#27150=CARTESIAN_POINT('Ctrl Pts',(-0.381603726014139,1.92375997419914,
8.69264174667176));
#27151=CARTESIAN_POINT('Ctrl Pts',(-0.393739127627545,2.07695764050864,
8.68486732551716));
#27152=CARTESIAN_POINT('Ctrl Pts',(-0.393535259525408,2.09967020164901,
8.6837163522035));
#27153=CARTESIAN_POINT('',(-0.39305712210104,2.09992355731599,8.55871635455519));
#27154=CARTESIAN_POINT('Ctrl Pts',(-0.393299861890554,2.09967039892168,
8.6837163522035));
#27155=CARTESIAN_POINT('Ctrl Pts',(-0.393316836847012,2.1199259395421,8.68268926714426));
#27156=CARTESIAN_POINT('Ctrl Pts',(-0.391764737712971,2.14023690090369,
8.68166218208501));
#27157=CARTESIAN_POINT('Ctrl Pts',(-0.388644317798756,2.16033642550516,
8.68063509702577));
#27158=CARTESIAN_POINT('Ctrl Pts',(-0.38552796621335,2.18040974482746,8.67960935105544));
#27159=CARTESIAN_POINT('Ctrl Pts',(-0.380847424894488,2.20027142239561,
8.67858360508512));
#27160=CARTESIAN_POINT('Ctrl Pts',(-0.374655259657195,2.2196592094709,8.6775578591148));
#27161=CARTESIAN_POINT('Ctrl Pts',(-0.368461202685,2.23905291960412,8.67653179977437));
#27162=CARTESIAN_POINT('Ctrl Pts',(-0.360754805832814,2.2579717188872,8.67550574043395));
#27163=CARTESIAN_POINT('Ctrl Pts',(-0.351638689139405,2.27616788101218,
8.67447968109352));
#27164=CARTESIAN_POINT('Ctrl Pts',(-0.342520791281123,2.29436759841907,
8.6734534212751));
#27165=CARTESIAN_POINT('Ctrl Pts',(-0.331992997204494,2.31184373491231,
8.67242716145667));
#27166=CARTESIAN_POINT('Ctrl Pts',(-0.320203617888944,2.32837366987206,
8.67140090163825));
#27167=CARTESIAN_POINT('Ctrl Pts',(-0.308389629667196,2.34493810907567,
8.67037249962633));
#27168=CARTESIAN_POINT('Ctrl Pts',(-0.295309292191493,2.36055182540162,
8.66934409761441));
#27169=CARTESIAN_POINT('Ctrl Pts',(-0.281151028374483,2.37502543381289,
8.6683156956025));
#27170=CARTESIAN_POINT('Ctrl Pts',(-0.276485001215232,2.37979538659893,
8.66797677327556));
#27171=CARTESIAN_POINT('Ctrl Pts',(-0.271702180537641,2.38444182541632,
8.66763785094863));
#27172=CARTESIAN_POINT('Ctrl Pts',(-0.266810082825443,2.38895894120563,
8.66729892862169));
#27173=CARTESIAN_POINT('Ctrl Pts',(-0.251741239984959,2.40287274913135,
8.66625496597414));
#27174=CARTESIAN_POINT('Ctrl Pts',(-0.235536187121755,2.41564610892519,
8.66521100332659));
#27175=CARTESIAN_POINT('Ctrl Pts',(-0.218393668755151,2.42709187615663,
8.66416704067903));
#27176=CARTESIAN_POINT('Ctrl Pts',(-0.201282685898296,2.4385165876659,8.66312499851326));
#27177=CARTESIAN_POINT('Ctrl Pts',(-0.183238232722274,2.44861810096978,
8.6620829563475));
#27178=CARTESIAN_POINT('Ctrl Pts',(-0.164491640124325,2.4572497590331,8.66104091418173));
#27179=CARTESIAN_POINT('Ctrl Pts',(-0.145765181072325,2.46587214683127,
8.65999999115287));
#27180=CARTESIAN_POINT('Ctrl Pts',(-0.126338732492407,2.47302748085229,
8.65895906812402));
#27181=CARTESIAN_POINT('Ctrl Pts',(-0.106467570926185,2.47861530125059,
8.65791814509517));
#27182=CARTESIAN_POINT('Ctrl Pts',(-0.0865862040492851,2.48420599140782,
8.65687668747538));
#27183=CARTESIAN_POINT('Ctrl Pts',(-0.066260371850469,2.48822734496792,
8.65583522985559));
#27184=CARTESIAN_POINT('Ctrl Pts',(-0.0457603440453731,2.49062882754969,
8.6547937722358));
#27185=CARTESIAN_POINT('Ctrl Pts',(-0.0252540525880575,2.4930310438891,
8.6537519964053));
#27186=CARTESIAN_POINT('Ctrl Pts',(-0.00457419394235422,2.49381235433887,
8.6527102205748));
#27187=CARTESIAN_POINT('Ctrl Pts',(0.0160049507945768,2.49297421232196,
8.6516684447443));
#27188=CARTESIAN_POINT('Ctrl Pts',(0.0366285778198562,2.49213425864206,
8.6506244170917));
#27189=CARTESIAN_POINT('Ctrl Pts',(0.0571503251020473,2.48966795182948,
8.64958038943911));
#27190=CARTESIAN_POINT('Ctrl Pts',(0.077301395414331,2.48562855738002,8.64853636178651));
#27191=CARTESIAN_POINT('Ctrl Pts',(0.0844285648485482,2.48419987651063,
8.64816710289064));
#27192=CARTESIAN_POINT('Ctrl Pts',(0.0915094828228455,2.48257487350149,
8.64779784399478));
#27193=CARTESIAN_POINT('Ctrl Pts',(0.0985327326118787,2.48075739074119,
8.64742858509891));
#27194=CARTESIAN_POINT('Ctrl Pts',(0.118388748340246,2.4756190335193,8.64638462245135));
#27195=CARTESIAN_POINT('Ctrl Pts',(0.137900905875624,2.4689079853868,8.6453406598038));
#27196=CARTESIAN_POINT('Ctrl Pts',(0.156804266830728,2.4606900496322,8.64429669715625));
#27197=CARTESIAN_POINT('Ctrl Pts',(0.175672853016393,2.45248723165595,8.64325465499048));
#27198=CARTESIAN_POINT('Ctrl Pts',(0.193934174810419,2.44278326402489,8.64221261282471));
#27199=CARTESIAN_POINT('Ctrl Pts',(0.211339696757282,2.43169326579619,8.64117057065894));
#27200=CARTESIAN_POINT('Ctrl Pts',(0.228726525447013,2.42061517805136,8.64012964763008));
#27201=CARTESIAN_POINT('Ctrl Pts',(0.245258746033701,2.40815438386103,8.63908872460123));
#27202=CARTESIAN_POINT('Ctrl Pts',(0.260713704275977,2.39447114358235,8.63804780157238));
#27203=CARTESIAN_POINT('Ctrl Pts',(0.276176599782002,2.3807808759481,8.63700634395259));
#27204=CARTESIAN_POINT('Ctrl Pts',(0.290560566088892,2.36586738365716,8.63596488633279));
#27205=CARTESIAN_POINT('Ctrl Pts',(0.303676811103612,2.34993055915182,8.634923428713));
#27206=CARTESIAN_POINT('Ctrl Pts',(0.31679706370301,2.3339888652518,8.6338816528825));
#27207=CARTESIAN_POINT('Ctrl Pts',(0.328648384664318,2.3170238073062,8.632839877052));
#27208=CARTESIAN_POINT('Ctrl Pts',(0.339083522737738,2.29926679253645,8.6317981012215));
#27209=CARTESIAN_POINT('Ctrl Pts',(0.349541216598902,2.28147139557633,8.63075407356891));
#27210=CARTESIAN_POINT('Ctrl Pts',(0.358576294281472,2.26288128659123,8.62971004591631));
#27211=CARTESIAN_POINT('Ctrl Pts',(0.366088037572277,2.24375130867745,8.62866601826371));
#27212=CARTESIAN_POINT('Ctrl Pts',(0.368744842712165,2.23698528624035,8.62829675936785));
#27213=CARTESIAN_POINT('Ctrl Pts',(0.371211539930955,2.23015188013729,8.62792750047198));
#27214=CARTESIAN_POINT('Ctrl Pts',(0.37348517989806,2.22326276970973,8.62755824157611));
#27215=CARTESIAN_POINT('Ctrl Pts',(0.379913177235985,2.20378599056715,8.62651427892856));
#27216=CARTESIAN_POINT('Ctrl Pts',(0.384832691245211,2.18374700754316,8.625470316281));
#27217=CARTESIAN_POINT('Ctrl Pts',(0.388155634572719,2.16340420608642,8.62442635363345));
#27218=CARTESIAN_POINT('Ctrl Pts',(0.391472464987909,2.14309882740503,8.62338431146768));
#27219=CARTESIAN_POINT('Ctrl Pts',(0.393198378708398,2.12249144806461,8.62234226930191));
#27220=CARTESIAN_POINT('Ctrl Pts',(0.393295633165775,2.10185335715177,8.62130022713614));
#27221=CARTESIAN_POINT('Ctrl Pts',(0.393392783173393,2.08123743122437,8.62025930410728));
#27222=CARTESIAN_POINT('Ctrl Pts',(0.39186471403716,2.06059159110837,8.61921838107843));
#27223=CARTESIAN_POINT('Ctrl Pts',(0.388725648770774,2.04018980030345,8.61817745804958));
#27224=CARTESIAN_POINT('Ctrl Pts',(0.385584971362279,2.01977753167049,8.61713600042979));
#27225=CARTESIAN_POINT('Ctrl Pts',(0.380831740890856,1.9996102924168,8.61609454280999));
#27226=CARTESIAN_POINT('Ctrl Pts',(0.374531833929707,1.97995502770524,8.6150530851902));
#27227=CARTESIAN_POINT('Ctrl Pts',(0.368230002072328,1.96029375745341,8.6140113093597));
#27228=CARTESIAN_POINT('Ctrl Pts',(0.360380811778884,1.94114546219344,8.6129695335292));
#27229=CARTESIAN_POINT('Ctrl Pts',(0.351099124622182,1.92275921832282,8.61192775769871));
#27230=CARTESIAN_POINT('Ctrl Pts',(0.341797374888068,1.90433323216885,8.61088373004611));
#27231=CARTESIAN_POINT('Ctrl Pts',(0.331057329212009,1.88667321519026,8.60983970239351));
#27232=CARTESIAN_POINT('Ctrl Pts',(0.31903874364352,1.87000180423672,8.60879567474092));
#27233=CARTESIAN_POINT('Ctrl Pts',(0.314787927464619,1.86410534470722,8.60842641584505));
#27234=CARTESIAN_POINT('Ctrl Pts',(0.310377545040194,1.85833225532561,8.60805715694919));
#27235=CARTESIAN_POINT('Ctrl Pts',(0.305815820043715,1.85269133818042,8.60768789805332));
#27236=CARTESIAN_POINT('Ctrl Pts',(0.292918986526465,1.83674343045642,8.60664393540577));
#27237=CARTESIAN_POINT('Ctrl Pts',(0.278732872637427,1.82175955140427,8.60559997275822));
#27238=CARTESIAN_POINT('Ctrl Pts',(0.263427050212234,1.80795363515962,8.60455601011067));
#27239=CARTESIAN_POINT('Ctrl Pts',(0.248149384496693,1.79417311638558,8.6035139679449));
#27240=CARTESIAN_POINT('Ctrl Pts',(0.231756599267029,1.78156679043929,8.60247192577913));
#27241=CARTESIAN_POINT('Ctrl Pts',(0.214456368510273,1.77031324563249,8.60142988361336));
#27242=CARTESIAN_POINT('Ctrl Pts',(0.197174717929564,1.75907178695601,8.6003889605845));
#27243=CARTESIAN_POINT('Ctrl Pts',(0.17898815447507,1.74918064854344,8.59934803755565));
#27244=CARTESIAN_POINT('Ctrl Pts',(0.160134730736778,1.74077617282277,8.5983071145268));
#27245=CARTESIAN_POINT('Ctrl Pts',(0.141271624371436,1.73236738078241,8.59726565690701));
#27246=CARTESIAN_POINT('Ctrl Pts',(0.121741638985336,1.72544709105953,8.59622419928722));
#27247=CARTESIAN_POINT('Ctrl Pts',(0.101804887030289,1.72010441569196,8.59518274166742));
#27248=CARTESIAN_POINT('Ctrl Pts',(0.0818620435283626,1.71476010790414,
8.59414096583693));
#27249=CARTESIAN_POINT('Ctrl Pts',(0.0615129055036579,1.71099452942582,
8.59309919000643));
#27250=CARTESIAN_POINT('Ctrl Pts',(0.041029077495528,1.70884593214455,8.59205741417593));
#27251=CARTESIAN_POINT('Ctrl Pts',(0.0205009732283072,1.7066926906215,8.59101338652333));
#27252=CARTESIAN_POINT('Ctrl Pts',(-0.000161666023785048,1.70616342703306,
8.58996935887074));
#27253=CARTESIAN_POINT('Ctrl Pts',(-0.020685164375156,1.70724433298198,
8.58892533121814));
#27254=CARTESIAN_POINT('Ctrl Pts',(-0.0279440567250865,1.70762663524786,
8.58855607232227));
#27255=CARTESIAN_POINT('Ctrl Pts',(-0.0351855933376826,1.70820988616013,
8.58818681342641));
#27256=CARTESIAN_POINT('Ctrl Pts',(-0.0423979216362757,1.70899193583645,
8.58781755453054));
#27257=CARTESIAN_POINT('Ctrl Pts',(-0.0627884970019345,1.71120293375621,
8.58677359188299));
#27258=CARTESIAN_POINT('Ctrl Pts',(-0.0830664105610273,1.71501982783529,
8.58572962923543));
#27259=CARTESIAN_POINT('Ctrl Pts',(-0.102959990363347,1.72041584545139,
8.58468566658788));
#27260=CARTESIAN_POINT('Ctrl Pts',(-0.122816973781957,1.72580193651164,
8.58364362442211));
#27261=CARTESIAN_POINT('Ctrl Pts',(-0.14229030918972,1.73276125181886,8.58260158225634));
#27262=CARTESIAN_POINT('Ctrl Pts',(-0.161117418655004,1.74121584844652,
8.58155954009058));
#27263=CARTESIAN_POINT('Ctrl Pts',(-0.179924308100493,1.74966136497023,
8.58051861706172));
#27264=CARTESIAN_POINT('Ctrl Pts',(-0.198085669780768,1.75959870119769,
8.57947769403287));
#27265=CARTESIAN_POINT('Ctrl Pts',(-0.215358002372933,1.77090150286891,
8.57843677100402));
#27266=CARTESIAN_POINT('Ctrl Pts',(-0.232639205584959,1.7822101093645,8.57739531338423));
#27267=CARTESIAN_POINT('Ctrl Pts',(-0.249029843061413,1.79488519288077,
8.57635385576444));
#27268=CARTESIAN_POINT('Ctrl Pts',(-0.264314184235297,1.80875628416732,
8.57531239814465));
#27269=CARTESIAN_POINT('Ctrl Pts',(-0.279603195441744,1.82263161367698,
8.57427062231415));
#27270=CARTESIAN_POINT('Ctrl Pts',(-0.293784717345044,1.8377031575969,8.57322884648365));
#27271=CARTESIAN_POINT('Ctrl Pts',(-0.306679562628534,1.85376325240539,
8.57218707065316));
#27272=CARTESIAN_POINT('Ctrl Pts',(-0.319602280412728,1.86985806147326,
8.57114304300056));
#27273=CARTESIAN_POINT('Ctrl Pts',(-0.331232354691389,1.8869450785646,8.57009901534796));
#27274=CARTESIAN_POINT('Ctrl Pts',(-0.341433250110269,1.90478671735986,
8.56905498769537));
#27275=CARTESIAN_POINT('Ctrl Pts',(-0.345041173109191,1.9110970711381,8.56868572879949));
#27276=CARTESIAN_POINT('Ctrl Pts',(-0.348470739914145,1.91750160903484,
8.56831646990362));
#27277=CARTESIAN_POINT('Ctrl Pts',(-0.351717342170775,1.92398920142126,
8.56794721100774));
#27278=CARTESIAN_POINT('Ctrl Pts',(-0.361527929255108,1.94359341685747,
8.56683138397743));
#27279=CARTESIAN_POINT('Ctrl Pts',(-0.36971644841328,1.96406147404622,8.56571555694711));
#27280=CARTESIAN_POINT('Ctrl Pts',(-0.376146989037825,1.98511600356108,
8.56459972991679));
#27281=CARTESIAN_POINT('Ctrl Pts',(-0.382546775609156,2.00606983981251,
8.56348923932797));
#27282=CARTESIAN_POINT('Ctrl Pts',(-0.387205093490701,2.02760403730076,
8.56237874873916));
#27283=CARTESIAN_POINT('Ctrl Pts',(-0.390034423487106,2.04942294497422,
8.56126825815034));
#27284=CARTESIAN_POINT('Ctrl Pts',(-0.392201685815372,2.06613619394294,
8.5604176241055));
#27285=CARTESIAN_POINT('Ctrl Pts',(-0.393296703097738,2.08301597580068,
8.55956699006066));
#27286=CARTESIAN_POINT('Ctrl Pts',(-0.393299992556388,2.09992348107888,
8.55871635601582));
#27287=CARTESIAN_POINT('',(-0.393299833419068,2.10036198416185,8.43371635078876));
#27288=CARTESIAN_POINT('Ctrl Pts',(-0.392666085555113,2.09992368006247,
8.55871635220349));
#27289=CARTESIAN_POINT('Ctrl Pts',(-0.392544325623193,2.17030148723538,
8.55516985729731));
#27290=CARTESIAN_POINT('Ctrl Pts',(-0.340838535780804,2.37228409448114,
8.54499991455022));
#27291=CARTESIAN_POINT('Ctrl Pts',(-0.0172983767692793,2.56473195461531,
8.52820652396216));
#27292=CARTESIAN_POINT('Ctrl Pts',(0.381391024272932,2.36611258911132,8.50833618043939));
#27293=CARTESIAN_POINT('Ctrl Pts',(0.430206082244237,1.92337115105522,8.48846583691659));
#27294=CARTESIAN_POINT('Ctrl Pts',(0.0843656270259472,1.64266263605957,
8.46859549339382));
#27295=CARTESIAN_POINT('Ctrl Pts',(-0.304352146860463,1.77017617472703,
8.45034566515609));
#27296=CARTESIAN_POINT('Ctrl Pts',(-0.392351384769331,2.00145617334239,
8.43871928475933));
#27297=CARTESIAN_POINT('Ctrl Pts',(-0.393254489865089,2.10036191446037,
8.43371635220349));
#27298=CARTESIAN_POINT('',(-0.393299984454947,2.09988942089621,8.30871635220045));
#27299=CARTESIAN_POINT('Ctrl Pts',(-0.393299833419068,2.10036198416185,
8.43371635078876));
#27300=CARTESIAN_POINT('Ctrl Pts',(-0.393274985171444,2.12735988263749,
8.43235086541525));
#27301=CARTESIAN_POINT('Ctrl Pts',(-0.390466436935829,2.1542324317043,8.43098538004175));
#27302=CARTESIAN_POINT('Ctrl Pts',(-0.384972992563196,2.18050270179899,
8.42961989466824));
#27303=CARTESIAN_POINT('Ctrl Pts',(-0.383946991062761,2.18540915660324,
8.42936486522824));
#27304=CARTESIAN_POINT('Ctrl Pts',(-0.382827463398736,2.19029467012745,
8.42910983578824));
#27305=CARTESIAN_POINT('Ctrl Pts',(-0.381615229822244,2.19515622085663,
8.42885480634824));
#27306=CARTESIAN_POINT('Ctrl Pts',(-0.376652953412313,2.2150569718067,8.42781084370069));
#27307=CARTESIAN_POINT('Ctrl Pts',(-0.370115001986025,2.23462780852539,
8.42676688105314));
#27308=CARTESIAN_POINT('Ctrl Pts',(-0.362064829497629,2.25360322015131,
8.42572291840558));
#27309=CARTESIAN_POINT('Ctrl Pts',(-0.354029466168979,2.27254372446283,
8.42468087623981));
#27310=CARTESIAN_POINT('Ctrl Pts',(-0.344487633092111,2.29089028498473,
8.42363883407404));
#27311=CARTESIAN_POINT('Ctrl Pts',(-0.333552243348001,2.30839335631808,
8.42259679190827));
#27312=CARTESIAN_POINT('Ctrl Pts',(-0.322628598040686,2.32587762962779,
8.42155586887942));
#27313=CARTESIAN_POINT('Ctrl Pts',(-0.310314730644007,2.34251957600188,
8.42051494585056));
#27314=CARTESIAN_POINT('Ctrl Pts',(-0.296768923016812,2.3580951303908,8.4194740228217));
#27315=CARTESIAN_POINT('Ctrl Pts',(-0.283216158615866,2.3736786839785,8.41843256520191));
#27316=CARTESIAN_POINT('Ctrl Pts',(-0.268430660682067,2.38819418568803,
8.41739110758212));
#27317=CARTESIAN_POINT('Ctrl Pts',(-0.252610641546382,2.40145108023944,
8.41634964996232));
#27318=CARTESIAN_POINT('Ctrl Pts',(-0.236785788705156,2.41471202535008,
8.41530787413182));
#27319=CARTESIAN_POINT('Ctrl Pts',(-0.219926372111198,2.42671315328611,
8.41426609830132));
#27320=CARTESIAN_POINT('Ctrl Pts',(-0.202262485595872,2.4373051688317,8.41322432247082));
#27321=CARTESIAN_POINT('Ctrl Pts',(-0.184560418189,2.44792007925925,8.41218029481822));
#27322=CARTESIAN_POINT('Ctrl Pts',(-0.166051068783666,2.45711946866287,
8.41113626716562));
#27323=CARTESIAN_POINT('Ctrl Pts',(-0.146988378343778,2.4648003654492,8.41009223951302));
#27324=CARTESIAN_POINT('Ctrl Pts',(-0.140246154604264,2.46751699796321,
8.40972298061715));
#27325=CARTESIAN_POINT('Ctrl Pts',(-0.133434865917593,2.47004412688048,
8.40935372172129));
#27326=CARTESIAN_POINT('Ctrl Pts',(-0.126566165042659,2.47237869953368,
8.40898446282542));
#27327=CARTESIAN_POINT('Ctrl Pts',(-0.107147087449817,2.47897896475473,
8.40794050017787));
#27328=CARTESIAN_POINT('Ctrl Pts',(-0.0871524662926278,2.48407578567592,
8.40689653753031));
#27329=CARTESIAN_POINT('Ctrl Pts',(-0.0668398966291456,2.48757878969134,
8.40585257488276));
#27330=CARTESIAN_POINT('Ctrl Pts',(-0.0465646941263617,2.4910753495534,
8.40481053271699));
#27331=CARTESIAN_POINT('Ctrl Pts',(-0.0259734109011967,2.49298373017354,
8.40376849055122));
#27332=CARTESIAN_POINT('Ctrl Pts',(-0.00533699108396289,2.49326378745846,
8.40272644838545));
#27333=CARTESIAN_POINT('Ctrl Pts',(0.0152772655425789,2.49354354396624,
8.4016855253566));
#27334=CARTESIAN_POINT('Ctrl Pts',(0.0359358309370009,2.49219841006009,
8.40064460232775));
#27335=CARTESIAN_POINT('Ctrl Pts',(0.0563646263637204,2.48924018150093,
8.3996036792989));
#27336=CARTESIAN_POINT('Ctrl Pts',(0.0768039134873284,2.48628043367269,
8.39856222167911));
#27337=CARTESIAN_POINT('Ctrl Pts',(0.0970124644043837,2.48170602563857,
8.39752076405932));
#27338=CARTESIAN_POINT('Ctrl Pts',(0.116722760907488,2.47558046685915,8.39647930643953));
#27339=CARTESIAN_POINT('Ctrl Pts',(0.136439079765469,2.46945303645447,8.39543753060903));
#27340=CARTESIAN_POINT('Ctrl Pts',(0.155656149839517,2.46177376452319,8.39439575477853));
#27341=CARTESIAN_POINT('Ctrl Pts',(0.174123887090683,2.45265530188051,8.39335397894804));
#27342=CARTESIAN_POINT('Ctrl Pts',(0.192631542775007,2.44351712947389,8.39230995129544));
#27343=CARTESIAN_POINT('Ctrl Pts',(0.210385999370801,2.43293393280199,8.39126592364285));
#27344=CARTESIAN_POINT('Ctrl Pts',(0.22716321368654,2.42106348958984,8.39022189599025));
#27345=CARTESIAN_POINT('Ctrl Pts',(0.233097094478416,2.41686506942055,8.38985263709439));
#27346=CARTESIAN_POINT('Ctrl Pts',(0.238909023357031,2.4125059964861,8.38948337819852));
#27347=CARTESIAN_POINT('Ctrl Pts',(0.24459012573609,2.40799441617082,8.38911411930265));
#27348=CARTESIAN_POINT('Ctrl Pts',(0.260651644489097,2.39523935086752,8.3880701566551));
#27349=CARTESIAN_POINT('Ctrl Pts',(0.275760592487338,2.38118651666554,8.38702619400755));
#27350=CARTESIAN_POINT('Ctrl Pts',(0.289701541966313,2.36600358377725,8.38598223136));
#27351=CARTESIAN_POINT('Ctrl Pts',(0.303616845566501,2.35084858153006,8.38494018919423));
#27352=CARTESIAN_POINT('Ctrl Pts',(0.316367879830953,2.33456810283204,8.38389814702846));
#27353=CARTESIAN_POINT('Ctrl Pts',(0.327774223933871,2.31736823163597,8.38285610486268));
#27354=CARTESIAN_POINT('Ctrl Pts',(0.339168317802411,2.30018683283136,8.38181518183383));
#27355=CARTESIAN_POINT('Ctrl Pts',(0.349220159854912,2.28208859588042,8.38077425880498));
#27356=CARTESIAN_POINT('Ctrl Pts',(0.357791304406505,2.26331035634978,8.37973333577612));
#27357=CARTESIAN_POINT('Ctrl Pts',(0.366366850874548,2.24452247280473,8.37869187815633));
#27358=CARTESIAN_POINT('Ctrl Pts',(0.373459860454248,2.22505455164884,8.37765042053654));
#27359=CARTESIAN_POINT('Ctrl Pts',(0.378978920597747,2.2051659057992,8.37660896291674));
#27360=CARTESIAN_POINT('Ctrl Pts',(0.384499667054731,2.18527118310118,8.37556718708624));
#27361=CARTESIAN_POINT('Ctrl Pts',(0.38844534498379,2.16495619786109,8.37452541125574));
#27362=CARTESIAN_POINT('Ctrl Pts',(0.390775298198262,2.1444922051382,8.37348363542524));
#27363=CARTESIAN_POINT('Ctrl Pts',(0.39311028765948,2.12398397903066,8.37243960777265));
#27364=CARTESIAN_POINT('Ctrl Pts',(0.393822554570108,2.10332683845759,8.37139558012005));
#27365=CARTESIAN_POINT('Ctrl Pts',(0.392923482638502,2.0827945708792,8.37035155246745));
#27366=CARTESIAN_POINT('Ctrl Pts',(0.392605492681104,2.07553257696858,8.36998229357158));
#27367=CARTESIAN_POINT('Ctrl Pts',(0.392086408228187,2.06828615816552,8.36961303467572));
#27368=CARTESIAN_POINT('Ctrl Pts',(0.391368274090816,2.06106718562477,8.36924377577985));
#27369=CARTESIAN_POINT('Ctrl Pts',(0.389337977126443,2.04065782576755,8.36819981313229));
#27370=CARTESIAN_POINT('Ctrl Pts',(0.385700849074887,2.02034689870207,8.36715585048474));
#27371=CARTESIAN_POINT('Ctrl Pts',(0.380481255111292,2.00040630286541,8.36611188783718));
#27372=CARTESIAN_POINT('Ctrl Pts',(0.375271263153236,1.98050238990351,8.36506984567141));
#27373=CARTESIAN_POINT('Ctrl Pts',(0.368484710415906,1.96096817470571,8.36402780350564));
#27374=CARTESIAN_POINT('Ctrl Pts',(0.360197210923611,1.94206691530002,8.36298576133987));
#27375=CARTESIAN_POINT('Ctrl Pts',(0.351918612075579,1.92318595555,8.36194483831102));
#27376=CARTESIAN_POINT('Ctrl Pts',(0.342142534137718,1.90493728410428,8.36090391528217));
#27377=CARTESIAN_POINT('Ctrl Pts',(0.330993169544062,1.88756551194503,8.35986299225331));
#27378=CARTESIAN_POINT('Ctrl Pts',(0.319838078927337,1.87018481809637,8.35882153463352));
#27379=CARTESIAN_POINT('Ctrl Pts',(0.307308676506359,1.85368255116109,8.35778007701373));
#27380=CARTESIAN_POINT('Ctrl Pts',(0.293573513960775,1.83827594321362,8.35673861939394));
#27381=CARTESIAN_POINT('Ctrl Pts',(0.279834154724232,1.82286462787575,8.35569684356344));
#27382=CARTESIAN_POINT('Ctrl Pts',(0.264888818163925,1.8085501626491,8.35465506773294));
#27383=CARTESIAN_POINT('Ctrl Pts',(0.248943572461899,1.79551356724821,8.35361329190245));
#27384=CARTESIAN_POINT('Ctrl Pts',(0.232963860749445,1.78244879295053,8.35256926424985));
#27385=CARTESIAN_POINT('Ctrl Pts',(0.215980530050778,1.77066782273632,8.35152523659725));
#27386=CARTESIAN_POINT('Ctrl Pts',(0.19822994797147,1.76030929107903,8.35048120894466));
#27387=CARTESIAN_POINT('Ctrl Pts',(0.191951799760306,1.75664561420895,8.35011195004879));
#27388=CARTESIAN_POINT('Ctrl Pts',(0.185577891294464,1.75315945227831,8.34974269115293));
#27389=CARTESIAN_POINT('Ctrl Pts',(0.179119310946591,1.74985551204393,8.34937343225707));
#27390=CARTESIAN_POINT('Ctrl Pts',(0.160859719329671,1.74051466681835,8.34832946960951));
#27391=CARTESIAN_POINT('Ctrl Pts',(0.141813085065345,1.73257815738893,8.34728550696196));
#27392=CARTESIAN_POINT('Ctrl Pts',(0.122221214537222,1.72617268061704,8.34624154431441));
#27393=CARTESIAN_POINT('Ctrl Pts',(0.102665385366083,1.71977898740991,8.34519950214864));
#27394=CARTESIAN_POINT('Ctrl Pts',(0.0825669838577476,1.71491101881307,
8.34415745998287));
#27395=CARTESIAN_POINT('Ctrl Pts',(0.0621882933132476,1.71164770352837,
8.3431154178171));
#27396=CARTESIAN_POINT('Ctrl Pts',(0.0418314891622494,1.70838789299303,
8.34207449478825));
#27397=CARTESIAN_POINT('Ctrl Pts',(0.0211957118491833,1.7067294587717,8.34103357175939));
#27398=CARTESIAN_POINT('Ctrl Pts',(0.000553862276033012,1.70670038998674,
8.33999264873054));
#27399=CARTESIAN_POINT('Ctrl Pts',(-0.0200985884130663,1.70667130627282,
8.33895119111075));
#27400=CARTESIAN_POINT('Ctrl Pts',(-0.0407563818375821,1.7082732768905,
8.33790973349095));
#27401=CARTESIAN_POINT('Ctrl Pts',(-0.0611456253101985,1.71148217221674,
8.33686827587116));
#27402=CARTESIAN_POINT('Ctrl Pts',(-0.0815410985855914,1.7146920480004,
8.33582650004067));
#27403=CARTESIAN_POINT('Ctrl Pts',(-0.101667137965019,1.71950967589419,
8.33478472421017));
#27404=CARTESIAN_POINT('Ctrl Pts',(-0.121259990401106,1.72585977932342,
8.33374294837967));
#27405=CARTESIAN_POINT('Ctrl Pts',(-0.140895193232352,1.73222360864531,
8.33269892072707));
#27406=CARTESIAN_POINT('Ctrl Pts',(-0.159994227695969,1.74012624512724,
8.33165489307448));
#27407=CARTESIAN_POINT('Ctrl Pts',(-0.178312577388737,1.74944399199987,
8.33061086542188));
#27408=CARTESIAN_POINT('Ctrl Pts',(-0.184791537562655,1.75273955693399,
8.33024160652601));
#27409=CARTESIAN_POINT('Ctrl Pts',(-0.191173076753329,1.75621173084899,
8.32987234763015));
#27410=CARTESIAN_POINT('Ctrl Pts',(-0.197447235098884,1.75985373829512,
8.32950308873428));
#27411=CARTESIAN_POINT('Ctrl Pts',(-0.215185431878719,1.77015036155437,
8.32845912608673));
#27412=CARTESIAN_POINT('Ctrl Pts',(-0.232168878383375,1.78186893670427,
8.32741516343918));
#27413=CARTESIAN_POINT('Ctrl Pts',(-0.24816015145877,1.79487473190842,8.32637120079163));
#27414=CARTESIAN_POINT('Ctrl Pts',(-0.264122006864192,1.80785660155083,
8.32532915862586));
#27415=CARTESIAN_POINT('Ctrl Pts',(-0.279094709909914,1.82212057802843,
8.32428711646009));
#27416=CARTESIAN_POINT('Ctrl Pts',(-0.29286991724023,1.83748885437814,8.32324507429432));
#27417=CARTESIAN_POINT('Ctrl Pts',(-0.306630330214274,1.85284062544048,
8.32220415126547));
#27418=CARTESIAN_POINT('Ctrl Pts',(-0.319195290525201,1.86929381606614,
8.32116322823662));
#27419=CARTESIAN_POINT('Ctrl Pts',(-0.330393538228543,1.88663411730826,
8.32012230520777));
#27420=CARTESIAN_POINT('Ctrl Pts',(-0.341597537060042,1.90398332407716,
8.31908084758798));
#27421=CARTESIAN_POINT('Ctrl Pts',(-0.351433008325731,1.92221994229463,
8.31803938996819));
#27422=CARTESIAN_POINT('Ctrl Pts',(-0.359771977584116,1.94110061628435,
8.3169979323484));
#27423=CARTESIAN_POINT('Ctrl Pts',(-0.36811349476116,1.9599870591431,8.3159561565179));
#27424=CARTESIAN_POINT('Ctrl Pts',(-0.374957335741952,1.97951726242553,
8.31491438068741));
#27425=CARTESIAN_POINT('Ctrl Pts',(-0.38022402012802,1.99942870927702,8.31387260485691));
#27426=CARTESIAN_POINT('Ctrl Pts',(-0.385502088571906,2.01938319517272,
8.31282857720431));
#27427=CARTESIAN_POINT('Ctrl Pts',(-0.389196062778896,2.03971984522538,
8.31178454955172));
#27428=CARTESIAN_POINT('Ctrl Pts',(-0.391277588060175,2.06016610636892,
8.31074052189913));
#27429=CARTESIAN_POINT('Ctrl Pts',(-0.392013796268067,2.06739768093108,
8.31037126300325));
#27430=CARTESIAN_POINT('Ctrl Pts',(-0.392548772744236,2.07464294381873,
8.31000200410737));
#27431=CARTESIAN_POINT('Ctrl Pts',(-0.392882822954939,2.08188985292832,
8.30963274521149));
#27432=CARTESIAN_POINT('Ctrl Pts',(-0.393159161391042,2.08788475868127,
8.30932728087549));
#27433=CARTESIAN_POINT('Ctrl Pts',(-0.393298296559854,2.09388603750217,
8.30902181653949));
#27434=CARTESIAN_POINT('Ctrl Pts',(-0.393299984454931,2.09988942083648,
8.30871635220349));
#27435=CARTESIAN_POINT('',(-0.393299884528478,2.09969862003011,8.1837163522079));
#27436=CARTESIAN_POINT('Ctrl Pts',(-0.393299984454947,2.09988942089621,
8.30871635220045));
#27437=CARTESIAN_POINT('Ctrl Pts',(-0.393305711143422,2.12025770397181,
8.30767997259272));
#27438=CARTESIAN_POINT('Ctrl Pts',(-0.39172488296096,2.14069019931158,8.306643592985));
#27439=CARTESIAN_POINT('Ctrl Pts',(-0.388553715200407,2.16091716017643,
8.30560721337727));
#27440=CARTESIAN_POINT('Ctrl Pts',(-0.385388227722587,2.18110788995381,
8.30457269016115));
#27441=CARTESIAN_POINT('Ctrl Pts',(-0.380638108234441,2.20109307632513,
8.30353816694502));
#27442=CARTESIAN_POINT('Ctrl Pts',(-0.374351441161159,2.22060633690052,
8.30250364372889));
#27443=CARTESIAN_POINT('Ctrl Pts',(-0.367899197786451,2.24063353172393,
8.30144187355888));
#27444=CARTESIAN_POINT('Ctrl Pts',(-0.359828357115801,2.26016275633634,
8.30038010338886));
#27445=CARTESIAN_POINT('Ctrl Pts',(-0.350246196936911,2.27892034968452,
8.29931833321885));
#27446=CARTESIAN_POINT('Ctrl Pts',(-0.340913850098907,2.29718891999679,
8.2982842441091));
#27447=CARTESIAN_POINT('Ctrl Pts',(-0.33014852181264,2.31472498149889,8.29725015499935));
#27448=CARTESIAN_POINT('Ctrl Pts',(-0.318096431087108,2.33129969850747,
8.29621606588961));
#27449=CARTESIAN_POINT('Ctrl Pts',(-0.305560414972645,2.34853993708881,
8.29514045518945));
#27450=CARTESIAN_POINT('Ctrl Pts',(-0.291632488933008,2.36473918448366,
8.2940648444893));
#27451=CARTESIAN_POINT('Ctrl Pts',(-0.276523297341258,2.37967795055656,
8.29298923378915));
#27452=CARTESIAN_POINT('Ctrl Pts',(-0.261414105749512,2.39461671662945,
8.291913623089));
#27453=CARTESIAN_POINT('Ctrl Pts',(-0.245124381763525,2.40829447491523,
8.29083801238885));
#27454=CARTESIAN_POINT('Ctrl Pts',(-0.227901906916449,2.42053956202604,
8.2897624016887));
#27455=CARTESIAN_POINT('Ctrl Pts',(-0.211186174694493,2.43242435785221,
8.28871843904114));
#27456=CARTESIAN_POINT('Ctrl Pts',(-0.193488468378395,2.44303348834778,
8.28767447639359));
#27457=CARTESIAN_POINT('Ctrl Pts',(-0.175029715533555,2.45220659942744,
8.28663051374603));
#27458=CARTESIAN_POINT('Ctrl Pts',(-0.15660491955362,2.46136283558081,8.28558847158026));
#27459=CARTESIAN_POINT('Ctrl Pts',(-0.137422481037262,2.46908791901188,
8.28454642941449));
#27460=CARTESIAN_POINT('Ctrl Pts',(-0.117730501263245,2.47526579789838,
8.28350438724872));
#27461=CARTESIAN_POINT('Ctrl Pts',(-0.0980596703661509,2.48143704184,8.28246346421987));
#27462=CARTESIAN_POINT('Ctrl Pts',(-0.0778810744356029,2.48606413332962,
8.28142254119101));
#27463=CARTESIAN_POINT('Ctrl Pts',(-0.0574606918412579,2.48907988754641,
8.28038161816215));
#27464=CARTESIAN_POINT('Ctrl Pts',(-0.037029821870632,2.49209719057596,
8.27934016054236));
#27465=CARTESIAN_POINT('Ctrl Pts',(-0.0163576426898396,2.49350137964718,
8.27829870292257));
#27466=CARTESIAN_POINT('Ctrl Pts',(0.00428134411018631,2.49327669660509,
8.27725724530278));
#27467=CARTESIAN_POINT('Ctrl Pts',(0.0249266370204593,2.49305194491253,
8.27621546947228));
#27468=CARTESIAN_POINT('Ctrl Pts',(0.0455379826392764,2.49119737450204,
8.27517369364178));
#27469=CARTESIAN_POINT('Ctrl Pts',(0.0658435110427064,2.48774930309875,
8.27413191781128));
#27470=CARTESIAN_POINT('Ctrl Pts',(0.0861929303065745,2.48429377861088,
8.27308789015868));
#27471=CARTESIAN_POINT('Ctrl Pts',(0.10623449853258,2.47923805671871,8.27204386250608));
#27472=CARTESIAN_POINT('Ctrl Pts',(0.125708373296824,2.4726691493578,8.27099983485349));
#27473=CARTESIAN_POINT('Ctrl Pts',(0.132596027542103,2.47034581292789,8.27063057595762));
#27474=CARTESIAN_POINT('Ctrl Pts',(0.139412842493954,2.46783362900765,8.27026131706176));
#27475=CARTESIAN_POINT('Ctrl Pts',(0.146147982674934,2.46513786048566,8.2698920581659));
#27476=CARTESIAN_POINT('Ctrl Pts',(0.165189459681377,2.45751642827389,8.26884809551835));
#27477=CARTESIAN_POINT('Ctrl Pts',(0.183689894758163,2.44837879396887,8.26780413287079));
#27478=CARTESIAN_POINT('Ctrl Pts',(0.201394867236247,2.43782391485935,8.26676017022324));
#27479=CARTESIAN_POINT('Ctrl Pts',(0.219067269509644,2.4272884525873,8.26571812805747));
#27480=CARTESIAN_POINT('Ctrl Pts',(0.235946458544924,2.41534124207763,8.2646760858917));
#27481=CARTESIAN_POINT('Ctrl Pts',(0.251800554186977,2.40212807037932,8.26363404372593));
#27482=CARTESIAN_POINT('Ctrl Pts',(0.267637622779372,2.38892908941984,8.26259312069708));
#27483=CARTESIAN_POINT('Ctrl Pts',(0.282451202730362,2.37446729290567,8.26155219766822));
#27484=CARTESIAN_POINT('Ctrl Pts',(0.296040824942273,2.35892995185474,8.26051127463937));
#27485=CARTESIAN_POINT('Ctrl Pts',(0.309637426429964,2.3433846312304,8.25946981701958));
#27486=CARTESIAN_POINT('Ctrl Pts',(0.322008317855323,2.32676320576889,8.25842835939978));
#27487=CARTESIAN_POINT('Ctrl Pts',(0.332991656808402,2.30928795114864,8.25738690177999));
#27488=CARTESIAN_POINT('Ctrl Pts',(0.343978351650364,2.29180735707624,8.2563451259495));
#27489=CARTESIAN_POINT('Ctrl Pts',(0.35357628945113,2.27347305617333,8.255303350119));
#27490=CARTESIAN_POINT('Ctrl Pts',(0.361668838702044,2.25453330098045,8.2542615742885));
#27491=CARTESIAN_POINT('Ctrl Pts',(0.369778880181808,2.23555260707692,8.2532175466359));
#27492=CARTESIAN_POINT('Ctrl Pts',(0.376376801704175,2.21596454406923,8.2521735189833));
#27493=CARTESIAN_POINT('Ctrl Pts',(0.381395107063358,2.19603469325264,8.25112949133071));
#27494=CARTESIAN_POINT('Ctrl Pts',(0.383170015890168,2.18898576625448,8.25076023243484));
#27495=CARTESIAN_POINT('Ctrl Pts',(0.384747791776386,2.18189417564379,8.25039097353898));
#27496=CARTESIAN_POINT('Ctrl Pts',(0.386126994413248,2.1747718809807,8.25002171464312));
#27497=CARTESIAN_POINT('Ctrl Pts',(0.390026253313782,2.15463584722102,8.24897775199557));
#27498=CARTESIAN_POINT('Ctrl Pts',(0.392357786575117,2.1341339836137,8.24793378934802));
#27499=CARTESIAN_POINT('Ctrl Pts',(0.393067076752167,2.11353377898098,8.24688982670046));
#27500=CARTESIAN_POINT('Ctrl Pts',(0.393775062113507,2.09297147064448,8.24584778453469));
#27501=CARTESIAN_POINT('Ctrl Pts',(0.392866643621935,2.07231190537088,8.24480574236892));
#27502=CARTESIAN_POINT('Ctrl Pts',(0.390338880720678,2.05182896931009,8.24376370020315));
#27503=CARTESIAN_POINT('Ctrl Pts',(0.387813832597066,2.03136803160085,8.2427227771743));
#27504=CARTESIAN_POINT('Ctrl Pts',(0.383672953650289,2.01108407658885,8.24168185414545));
#27505=CARTESIAN_POINT('Ctrl Pts',(0.377965187160364,1.99124703546647,8.24064093111659));
#27506=CARTESIAN_POINT('Ctrl Pts',(0.372254489310332,1.97139980655679,8.2395994734968));
#27507=CARTESIAN_POINT('Ctrl Pts',(0.364975484242306,1.95200066162075,8.23855801587701));
#27508=CARTESIAN_POINT('Ctrl Pts',(0.356227457105592,1.93330600249534,8.23751655825721));
#27509=CARTESIAN_POINT('Ctrl Pts',(0.347476757065207,1.91460563133655,8.23647478242671));
#27510=CARTESIAN_POINT('Ctrl Pts',(0.337256485756988,1.89661082502997,8.23543300659622));
#27511=CARTESIAN_POINT('Ctrl Pts',(0.325712243618799,1.87955403302213,8.23439123076572));
#27512=CARTESIAN_POINT('Ctrl Pts',(0.314143048339255,1.8624603723713,8.23334720311312));
#27513=CARTESIAN_POINT('Ctrl Pts',(0.30124462838715,1.84630934938367,8.23230317546053));
#27514=CARTESIAN_POINT('Ctrl Pts',(0.287203752354838,1.83130148003143,8.23125914780793));
#27515=CARTESIAN_POINT('Ctrl Pts',(0.282237678546511,1.82599339336095,8.23088988891206));
#27516=CARTESIAN_POINT('Ctrl Pts',(0.277129020786189,1.82082796501212,8.23052063001619));
#27517=CARTESIAN_POINT('Ctrl Pts',(0.271887055220996,1.81581287994834,8.23015137112032));
#27518=CARTESIAN_POINT('Ctrl Pts',(0.257067056810563,1.80163431434178,8.22910740847277));
#27519=CARTESIAN_POINT('Ctrl Pts',(0.241090823898778,1.78857589021517,8.22806344582521));
#27520=CARTESIAN_POINT('Ctrl Pts',(0.224153754598498,1.77682824334513,8.22701948317766));
#27521=CARTESIAN_POINT('Ctrl Pts',(0.207247842862268,1.76510220753738,8.22597744101189));
#27522=CARTESIAN_POINT('Ctrl Pts',(0.189385167139861,1.75468262609251,8.22493539884612));
#27523=CARTESIAN_POINT('Ctrl Pts',(0.170794424033357,1.74572023100505,8.22389335668035));
#27524=CARTESIAN_POINT('Ctrl Pts',(0.152223647092894,1.73676746138912,8.2228524336515));
#27525=CARTESIAN_POINT('Ctrl Pts',(0.132927001952251,1.72926911519165,8.22181151062265));
#27526=CARTESIAN_POINT('Ctrl Pts',(0.11315794547275,1.72333015865829,8.22077058759379));
#27527=CARTESIAN_POINT('Ctrl Pts',(0.0933787361210852,1.71738815203165,
8.219729129974));
#27528=CARTESIAN_POINT('Ctrl Pts',(0.0731273307625204,1.71300736214477,
8.21868767235421));
#27529=CARTESIAN_POINT('Ctrl Pts',(0.0526730614975844,1.71024310321372,
8.21764621473442));
#27530=CARTESIAN_POINT('Ctrl Pts',(0.0322125425616538,1.70747799968105,
8.21660443890393));
#27531=CARTESIAN_POINT('Ctrl Pts',(0.0115497697054225,1.7063304729854,8.21556266307343));
#27532=CARTESIAN_POINT('Ctrl Pts',(-0.00904099326675641,1.70680392875723,
8.21452088724293));
#27533=CARTESIAN_POINT('Ctrl Pts',(-0.0296762636403592,1.70727840791445,
8.21347685959033));
#27534=CARTESIAN_POINT('Ctrl Pts',(-0.0502384807222144,1.70938078977478,
8.21243283193774));
#27535=CARTESIAN_POINT('Ctrl Pts',(-0.0704579458790627,1.71306257888064,
8.21138880428514));
#27536=CARTESIAN_POINT('Ctrl Pts',(-0.0776093056732729,1.71436477942739,
8.21101954538928));
#27537=CARTESIAN_POINT('Ctrl Pts',(-0.0847178990659698,1.71586409064105,
8.21065028649341));
#27538=CARTESIAN_POINT('Ctrl Pts',(-0.0917722430562946,1.71755687298055,
8.21028102759754));
#27539=CARTESIAN_POINT('Ctrl Pts',(-0.111716167796723,1.72234267923373,
8.20923706494999));
#27540=CARTESIAN_POINT('Ctrl Pts',(-0.131344148152779,1.72870702098008,
8.20819310230244));
#27541=CARTESIAN_POINT('Ctrl Pts',(-0.150390121621155,1.73658879857829,
8.20714913965488));
#27542=CARTESIAN_POINT('Ctrl Pts',(-0.169401057969011,1.74445607679729,
8.20610709748911));
#27543=CARTESIAN_POINT('Ctrl Pts',(-0.187831417730646,1.75383502665889,
8.20506505532335));
#27544=CARTESIAN_POINT('Ctrl Pts',(-0.205430665143305,1.76461494991759,
8.20402301315758));
#27545=CARTESIAN_POINT('Ctrl Pts',(-0.223011011240724,1.77538329570806,
8.20298209012872));
#27546=CARTESIAN_POINT('Ctrl Pts',(-0.239761377659703,1.78754927015365,
8.20194116709987));
#27547=CARTESIAN_POINT('Ctrl Pts',(-0.255456306122845,1.80095658231275,
8.20090024407101));
#27548=CARTESIAN_POINT('Ctrl Pts',(-0.271159295092185,1.81437078011793,
8.19985878645122));
#27549=CARTESIAN_POINT('Ctrl Pts',(-0.285805193304681,1.82902712361073,
8.19881732883143));
#27550=CARTESIAN_POINT('Ctrl Pts',(-0.299201697244564,1.84472909612341,
8.19777587121164));
#27551=CARTESIAN_POINT('Ctrl Pts',(-0.312602294400451,1.86043586627325,
8.19673409538114));
#27552=CARTESIAN_POINT('Ctrl Pts',(-0.324752287691612,1.87718831871015,
8.19569231955064));
#27553=CARTESIAN_POINT('Ctrl Pts',(-0.335500349650052,1.89475769104619,
8.19465054372014));
#27554=CARTESIAN_POINT('Ctrl Pts',(-0.346271643788316,1.91236503997922,
8.19360651606754));
#27555=CARTESIAN_POINT('Ctrl Pts',(-0.355634623120393,1.93079217754411,
8.19256248841494));
#27556=CARTESIAN_POINT('Ctrl Pts',(-0.363484070751981,1.94978608483376,
8.19151846076234));
#27557=CARTESIAN_POINT('Ctrl Pts',(-0.366260317490647,1.95650398087466,
8.19114920186648));
#27558=CARTESIAN_POINT('Ctrl Pts',(-0.368847679825564,1.96329261772501,
8.19077994297061));
#27559=CARTESIAN_POINT('Ctrl Pts',(-0.371243001992155,1.97014037012276,
8.19041068407475));
#27560=CARTESIAN_POINT('Ctrl Pts',(-0.379130780091446,1.99268996789535,
8.18919471727395));
#27561=CARTESIAN_POINT('Ctrl Pts',(-0.384971037397137,2.01599100857184,
8.18797875047315));
#27562=CARTESIAN_POINT('Ctrl Pts',(-0.388648914697292,2.03969319188833,
8.18676278367236));
#27563=CARTESIAN_POINT('Ctrl Pts',(-0.391720380442988,2.05948733895021,
8.18574730651754));
#27564=CARTESIAN_POINT('Ctrl Pts',(-0.393284453216479,2.07956080785454,
8.18473182936272));
#27565=CARTESIAN_POINT('Ctrl Pts',(-0.393299884528477,2.09969862003011,
8.1837163522079));
#27566=CARTESIAN_POINT('',(-0.393134897346159,2.1002525601452,8.058716300174));
#27567=CARTESIAN_POINT('Ctrl Pts',(-0.393299884528545,2.09969862011757,
8.18371635220349));
#27568=CARTESIAN_POINT('Ctrl Pts',(-0.393315697990375,2.12033514257448,
8.18267572688992));
#27569=CARTESIAN_POINT('Ctrl Pts',(-0.391702978785827,2.14098969196552,
8.18163510157636));
#27570=CARTESIAN_POINT('Ctrl Pts',(-0.388479577251369,2.1613881752343,8.18059447626279));
#27571=CARTESIAN_POINT('Ctrl Pts',(-0.385253698249265,2.18180233653196,
8.17955305113713));
#27572=CARTESIAN_POINT('Ctrl Pts',(-0.380414773381228,2.2019593117515,8.17851162601146));
#27573=CARTESIAN_POINT('Ctrl Pts',(-0.374032193501926,2.2215927967609,8.17747020088579));
#27574=CARTESIAN_POINT('Ctrl Pts',(-0.367646440359054,2.24123604306181,
8.17642825798887));
#27575=CARTESIAN_POINT('Ctrl Pts',(-0.359715774467009,2.2603545976506,8.17538631509195));
#27576=CARTESIAN_POINT('Ctrl Pts',(-0.35035827337408,2.27870078421298,8.17434437219502));
#27577=CARTESIAN_POINT('Ctrl Pts',(-0.34097968932248,2.29708830573105,8.17330008174411));
#27578=CARTESIAN_POINT('Ctrl Pts',(-0.330168246545375,2.3146993652735,8.17225579129319));
#27579=CARTESIAN_POINT('Ctrl Pts',(-0.318086425579717,2.33131345802162,
8.17121150084228));
#27580=CARTESIAN_POINT('Ctrl Pts',(-0.31549811678757,2.33487272300789,8.17098778074551));
#27581=CARTESIAN_POINT('Ctrl Pts',(-0.312851648599206,2.33838635565434,
8.17076406064873));
#27582=CARTESIAN_POINT('Ctrl Pts',(-0.310148846771198,2.34185239888514,
8.17054034055196));
#27583=CARTESIAN_POINT('Ctrl Pts',(-0.297536550456057,2.35802626846555,
8.1694963779044));
#27584=CARTESIAN_POINT('Ctrl Pts',(-0.283618098539485,2.37325909994786,
8.16845241525685));
#27585=CARTESIAN_POINT('Ctrl Pts',(-0.268559246455048,2.38733398884138,
8.1674084526093));
#27586=CARTESIAN_POINT('Ctrl Pts',(-0.253528096751699,2.40138298546013,
8.16636641044353));
#27587=CARTESIAN_POINT('Ctrl Pts',(-0.237361201966722,2.41427772758481,
8.16532436827776));
#27588=CARTESIAN_POINT('Ctrl Pts',(-0.22026303984912,2.42583597603154,8.16428232611199));
#27589=CARTESIAN_POINT('Ctrl Pts',(-0.203183240889036,2.43738181110101,
8.16324140308313));
#27590=CARTESIAN_POINT('Ctrl Pts',(-0.185174750446051,2.44759356811661,
8.16220048005428));
#27591=CARTESIAN_POINT('Ctrl Pts',(-0.16647316848108,2.4563307089992,8.16115955702543));
#27592=CARTESIAN_POINT('Ctrl Pts',(-0.14776198187103,2.46507233704962,8.16011809940564));
#27593=CARTESIAN_POINT('Ctrl Pts',(-0.128357652416436,2.47233750996205,
8.15907664178584));
#27594=CARTESIAN_POINT('Ctrl Pts',(-0.108518673153725,2.4780325218509,8.15803518416605));
#27595=CARTESIAN_POINT('Ctrl Pts',(-0.0886736322179369,2.48372927381417,
8.15699340833556));
#27596=CARTESIAN_POINT('Ctrl Pts',(-0.0683943936949748,2.48785474161243,
8.15595163250506));
#27597=CARTESIAN_POINT('Ctrl Pts',(-0.0479518418811187,2.49036586794981,
8.15490985667456));
#27598=CARTESIAN_POINT('Ctrl Pts',(-0.0274651030276245,2.49288242214376,
8.15386582902196));
#27599=CARTESIAN_POINT('Ctrl Pts',(-0.00681508191190315,2.49377763649144,
8.15282180136937));
#27600=CARTESIAN_POINT('Ctrl Pts',(0.0137243439128156,2.49306046911915,
8.15177777371677));
#27601=CARTESIAN_POINT('Ctrl Pts',(0.0209888696012749,2.49280681642002,
8.1514085148209));
#27602=CARTESIAN_POINT('Ctrl Pts',(0.028239602034006,2.49235193915431,8.15103925592504));
#27603=CARTESIAN_POINT('Ctrl Pts',(0.0354646524095694,2.49169777690136,
8.15066999702917));
#27604=CARTESIAN_POINT('Ctrl Pts',(0.0558911954210694,2.48984834019135,
8.14962603438162));
#27605=CARTESIAN_POINT('Ctrl Pts',(0.0762335423787659,2.48639126353976,
8.14858207173407));
#27606=CARTESIAN_POINT('Ctrl Pts',(0.0962195896921495,2.48134850276286,
8.14753810908651));
#27607=CARTESIAN_POINT('Ctrl Pts',(0.116168870517875,2.4763150186878,8.14649606692074));
#27608=CARTESIAN_POINT('Ctrl Pts',(0.135762432833069,2.4697017609996,8.14545402475497));
#27609=CARTESIAN_POINT('Ctrl Pts',(0.154736359168832,2.46158200888758,8.1444119825892));
#27610=CARTESIAN_POINT('Ctrl Pts',(0.173689907805802,2.45347097726176,8.14337105956035));
#27611=CARTESIAN_POINT('Ctrl Pts',(0.192024457209319,2.44385692465364,8.14233013653149));
#27612=CARTESIAN_POINT('Ctrl Pts',(0.209494305930319,2.43286187192704,8.14128921350264));
#27613=CARTESIAN_POINT('Ctrl Pts',(0.226973126710294,2.42186117242793,8.14024775588285));
#27614=CARTESIAN_POINT('Ctrl Pts',(0.243585728321268,2.40947843417078,8.13920629826305));
#27615=CARTESIAN_POINT('Ctrl Pts',(0.259113394225609,2.39588027803976,8.13816484064326));
#27616=CARTESIAN_POINT('Ctrl Pts',(0.274645804508845,2.3822779670792,8.13712306481276));
#27617=CARTESIAN_POINT('Ctrl Pts',(0.289092089932649,2.36746001050347,8.13608128898226));
#27618=CARTESIAN_POINT('Ctrl Pts',(0.302269412587609,2.35163086498667,8.13503951315176));
#27619=CARTESIAN_POINT('Ctrl Pts',(0.315475218324509,2.33576750441264,8.13399548549917));
#27620=CARTESIAN_POINT('Ctrl Pts',(0.327406160128445,2.31888919263453,8.13295145784657));
#27621=CARTESIAN_POINT('Ctrl Pts',(0.337921515284175,2.30123105999832,8.13190743019397));
#27622=CARTESIAN_POINT('Ctrl Pts',(0.341640658570052,2.29498560994338,8.13153817129811));
#27623=CARTESIAN_POINT('Ctrl Pts',(0.345183142098988,2.28864283101102,8.13116891240224));
#27624=CARTESIAN_POINT('Ctrl Pts',(0.348544161080997,2.28221376944771,8.13079965350638));
#27625=CARTESIAN_POINT('Ctrl Pts',(0.358046378398528,2.26403763285064,8.12975569085883));
#27626=CARTESIAN_POINT('Ctrl Pts',(0.366151286424129,2.24506204525451,8.12871172821127));
#27627=CARTESIAN_POINT('Ctrl Pts',(0.37273005141108,2.22552768131011,8.12766776556372));
#27628=CARTESIAN_POINT('Ctrl Pts',(0.379296714050938,2.20602925293313,8.12662572339795));
#27629=CARTESIAN_POINT('Ctrl Pts',(0.384342517894813,2.18597475904724,8.12558368123218));
#27630=CARTESIAN_POINT('Ctrl Pts',(0.38778621410251,2.16562577353481,8.12454163906641));
#27631=CARTESIAN_POINT('Ctrl Pts',(0.391226211834579,2.14529864251315,8.12350071603756));
#27632=CARTESIAN_POINT('Ctrl Pts',(0.393067367144397,2.12467836471419,8.1224597930087));
#27633=CARTESIAN_POINT('Ctrl Pts',(0.393279274725038,2.1040375824138,8.12141886997985));
#27634=CARTESIAN_POINT('Ctrl Pts',(0.393491291135889,2.08338619954558,8.12037741236005));
#27635=CARTESIAN_POINT('Ctrl Pts',(0.392072364526663,2.0627150267122,8.11933595474027));
#27636=CARTESIAN_POINT('Ctrl Pts',(0.389044197506231,2.04229815958973,8.11829449712047));
#27637=CARTESIAN_POINT('Ctrl Pts',(0.386015105248758,2.02187505422425,8.11725272128998));
#27638=CARTESIAN_POINT('Ctrl Pts',(0.381375937381233,2.00170713115017,8.11621094545948));
#27639=CARTESIAN_POINT('Ctrl Pts',(0.375199631271861,1.9820587998473,8.11516916962898));
#27640=CARTESIAN_POINT('Ctrl Pts',(0.369009974936675,1.96236799823044,8.11412514197638));
#27641=CARTESIAN_POINT('Ctrl Pts',(0.361276822574777,1.94319971360829,8.11308111432379));
#27642=CARTESIAN_POINT('Ctrl Pts',(0.352121700242478,1.9247995484642,8.11203708667119));
#27643=CARTESIAN_POINT('Ctrl Pts',(0.34888365347663,1.91829165123757,8.11166782777532));
#27644=CARTESIAN_POINT('Ctrl Pts',(0.345468141729564,1.91187960681759,8.11129856887946));
#27645=CARTESIAN_POINT('Ctrl Pts',(0.341881851963449,1.90557343469052,8.11092930998359));
#27646=CARTESIAN_POINT('Ctrl Pts',(0.331742752808256,1.88774472907665,8.10988534733604));
#27647=CARTESIAN_POINT('Ctrl Pts',(0.32017507217187,1.87065814886244,8.10884138468849));
#27648=CARTESIAN_POINT('Ctrl Pts',(0.307311433574845,1.85455230130601,8.10779742204093));
#27649=CARTESIAN_POINT('Ctrl Pts',(0.294471459027154,1.83847608219167,8.10675537987516));
#27650=CARTESIAN_POINT('Ctrl Pts',(0.280340666297115,1.82337762007559,8.10571333770939));
#27651=CARTESIAN_POINT('Ctrl Pts',(0.265095009923085,1.80946682510619,8.10467129554362));
#27652=CARTESIAN_POINT('Ctrl Pts',(0.249865727144491,1.79557097011204,8.10363037251477));
#27653=CARTESIAN_POINT('Ctrl Pts',(0.233524479014521,1.78286076480544,8.10258944948591));
#27654=CARTESIAN_POINT('Ctrl Pts',(0.216284049098182,1.77150936070309,8.10154852645706));
#27655=CARTESIAN_POINT('Ctrl Pts',(0.199034764946384,1.76015212681544,8.10050706883727));
#27656=CARTESIAN_POINT('Ctrl Pts',(0.180885982111509,1.75015550635439,8.09946561121748));
#27657=CARTESIAN_POINT('Ctrl Pts',(0.162079913159837,1.74164962431986,8.09842415359768));
#27658=CARTESIAN_POINT('Ctrl Pts',(0.143268098134222,1.73314114336754,8.09738237776718));
#27659=CARTESIAN_POINT('Ctrl Pts',(0.123799281928152,1.72612457760075,8.09634060193669));
#27660=CARTESIAN_POINT('Ctrl Pts',(0.103935267081649,1.7206817296034,8.09529882610619));
#27661=CARTESIAN_POINT('Ctrl Pts',(0.0840283157162946,1.7152271167666,8.09425479845359));
#27662=CARTESIAN_POINT('Ctrl Pts',(0.0637251837069782,1.71135315091492,
8.093210770801));
#27663=CARTESIAN_POINT('Ctrl Pts',(0.0432981622691779,1.70909059982636,
8.0921667431484));
#27664=CARTESIAN_POINT('Ctrl Pts',(0.036073392538989,1.7082903651633,8.09179748425253));
#27665=CARTESIAN_POINT('Ctrl Pts',(0.0288331525638997,1.70769123309004,
8.09142822535667));
#27666=CARTESIAN_POINT('Ctrl Pts',(0.0215894866807903,1.70729300481802,
8.0910589664608));
#27667=CARTESIAN_POINT('Ctrl Pts',(0.00111031421407299,1.70616714042898,
8.09001500381325));
#27668=CARTESIAN_POINT('Ctrl Pts',(-0.0195181828979126,1.70664417881538,
8.0889710411657));
#27669=CARTESIAN_POINT('Ctrl Pts',(-0.0400235878923866,1.70874177016679,
8.08792707851814));
#27670=CARTESIAN_POINT('Ctrl Pts',(-0.0604912709847918,1.71083550277287,
8.08688503635237));
#27671=CARTESIAN_POINT('Ctrl Pts',(-0.0808355816926341,1.71454385594809,
8.08584299418661));
#27672=CARTESIAN_POINT('Ctrl Pts',(-0.100784776433899,1.7198325121224,8.08480095202084));
#27673=CARTESIAN_POINT('Ctrl Pts',(-0.120712546053408,1.72511548836305,
8.08376002899198));
#27674=CARTESIAN_POINT('Ctrl Pts',(-0.140245327123944,1.7319752385794,8.08271910596313));
#27675=CARTESIAN_POINT('Ctrl Pts',(-0.159122347161594,1.74032658058485,
8.08167818293428));
#27676=CARTESIAN_POINT('Ctrl Pts',(-0.178009061944737,1.7486822116219,8.08063672531449));
#27677=CARTESIAN_POINT('Ctrl Pts',(-0.196238663487924,1.75853068188917,
8.0795952676947));
#27678=CARTESIAN_POINT('Ctrl Pts',(-0.213570626322764,1.76973877373797,
8.07855381007491));
#27679=CARTESIAN_POINT('Ctrl Pts',(-0.230907884827876,1.78095029014746,
8.07751203424441));
#27680=CARTESIAN_POINT('Ctrl Pts',(-0.247346360943412,1.7935218255598,8.07647025841391));
#27681=CARTESIAN_POINT('Ctrl Pts',(-0.262675555146807,1.80727753292869,
8.07542848258342));
#27682=CARTESIAN_POINT('Ctrl Pts',(-0.278037883751325,1.82106297357119,
8.07438445493082));
#27683=CARTESIAN_POINT('Ctrl Pts',(-0.292285635811347,1.83603716276604,
8.07334042727823));
#27684=CARTESIAN_POINT('Ctrl Pts',(-0.305245545073329,1.85198780833821,
8.07229639962563));
#27685=CARTESIAN_POINT('Ctrl Pts',(-0.309829295104064,1.85762934260004,
8.07192714072976));
#27686=CARTESIAN_POINT('Ctrl Pts',(-0.314252328799765,1.86339274498632,
8.07155788183389));
#27687=CARTESIAN_POINT('Ctrl Pts',(-0.318508293488239,1.86926778079512,
8.07118862293802));
#27688=CARTESIAN_POINT('Ctrl Pts',(-0.330631578193252,1.88600305398831,
8.07013677428508));
#27689=CARTESIAN_POINT('Ctrl Pts',(-0.341468108319497,1.90374564296446,
8.06908492563215));
#27690=CARTESIAN_POINT('Ctrl Pts',(-0.350853335476031,1.92227316751446,
8.06803307697922));
#27691=CARTESIAN_POINT('Ctrl Pts',(-0.360219866270163,1.94076378328137,
8.06698332371974));
#27692=CARTESIAN_POINT('Ctrl Pts',(-0.368140456170937,1.96003562340037,
8.06593357046027));
#27693=CARTESIAN_POINT('Ctrl Pts',(-0.374494500045934,1.97983861087959,
8.06488381720079));
#27694=CARTESIAN_POINT('Ctrl Pts',(-0.380843023719858,1.99962439412244,
8.06383497593519));
#27695=CARTESIAN_POINT('Ctrl Pts',(-0.38562743929961,2.01993973991456,8.06278613466959));
#27696=CARTESIAN_POINT('Ctrl Pts',(-0.38877563735936,2.04051560039957,8.06173729340398));
#27697=CARTESIAN_POINT('Ctrl Pts',(-0.39179818600039,2.06027024669775,8.06073031300382));
#27698=CARTESIAN_POINT('Ctrl Pts',(-0.393312707412277,2.08026435563854,
8.05972333260365));
#27699=CARTESIAN_POINT('Ctrl Pts',(-0.393299919501896,2.10025163426288,
8.05871635220349));
#27700=CARTESIAN_POINT('',(-0.393495572071111,2.10018686531557,7.93371641359789));
#27701=CARTESIAN_POINT('Ctrl Pts',(-0.39282171143197,2.10025431732318,8.05871620143025));
#27702=CARTESIAN_POINT('Ctrl Pts',(-0.393106694558029,2.14914144428112,
8.05625022742525));
#27703=CARTESIAN_POINT('Ctrl Pts',(-0.361959072798305,2.32898542981025,
8.04716080557931));
#27704=CARTESIAN_POINT('Ctrl Pts',(-0.0924540126689525,2.55577108181745,
8.03144793589244));
#27705=CARTESIAN_POINT('Ctrl Pts',(0.333173458296833,2.42445411103268,8.01157759236963));
#27706=CARTESIAN_POINT('Ctrl Pts',(0.453159638745708,1.9954946638146,7.99170724884688));
#27707=CARTESIAN_POINT('Ctrl Pts',(0.157433542759797,1.66240463542945,7.97183690532405));
#27708=CARTESIAN_POINT('Ctrl Pts',(-0.270752563968054,1.72889110048612,
7.95250666287296));
#27709=CARTESIAN_POINT('Ctrl Pts',(-0.39313119258737,1.9803820937068,7.93979986826274));
#27710=CARTESIAN_POINT('Ctrl Pts',(-0.39383935274689,2.1001849047854,7.93371652149347));
#27711=CARTESIAN_POINT('',(-0.393299840076811,2.09964532330949,7.8087163522035));
#27712=CARTESIAN_POINT('Ctrl Pts',(-0.39329995507651,2.10018798089025,7.93371635220349));
#27713=CARTESIAN_POINT('Ctrl Pts',(-0.393294878776239,2.11080878742979,
7.93317630756182));
#27714=CARTESIAN_POINT('Ctrl Pts',(-0.392859630695457,2.12141894325366,
7.93263626292015));
#27715=CARTESIAN_POINT('Ctrl Pts',(-0.391996546742083,2.13199370785455,
7.93209621827848));
#27716=CARTESIAN_POINT('Ctrl Pts',(-0.390328115394942,2.15243583133485,
7.93105225563092));
#27717=CARTESIAN_POINT('Ctrl Pts',(-0.387051361388753,2.17280800210539,
7.93000829298337));
#27718=CARTESIAN_POINT('Ctrl Pts',(-0.382185829458229,2.19283793277171,
7.92896433033582));
#27719=CARTESIAN_POINT('Ctrl Pts',(-0.377329248197983,2.21283101622223,
7.92792228817005));
#27720=CARTESIAN_POINT('Ctrl Pts',(-0.370889804441221,2.2324823883258,7.92688024600428));
#27721=CARTESIAN_POINT('Ctrl Pts',(-0.362938436792736,2.25152749287982,
7.92583820383852));
#27722=CARTESIAN_POINT('Ctrl Pts',(-0.354995608788193,2.27055214329075,
7.92479728080966));
#27723=CARTESIAN_POINT('Ctrl Pts',(-0.345544335837312,2.28897113210632,
7.92375635778081));
#27724=CARTESIAN_POINT('Ctrl Pts',(-0.334704457659796,2.30653768668856,
7.92271543475196));
#27725=CARTESIAN_POINT('Ctrl Pts',(-0.32385901240337,2.32411326299539,7.92167397713217));
#27726=CARTESIAN_POINT('Ctrl Pts',(-0.311623909871164,2.34083489584196,
7.92063251951238));
#27727=CARTESIAN_POINT('Ctrl Pts',(-0.298163827078626,2.35648240138814,
7.91959106189259));
#27728=CARTESIAN_POINT('Ctrl Pts',(-0.284699631643985,2.37213468792944,
7.91854928606209));
#27729=CARTESIAN_POINT('Ctrl Pts',(-0.270010217683464,2.38671166008147,
7.9175075102316));
#27730=CARTESIAN_POINT('Ctrl Pts',(-0.254298414321334,2.40002867608556,
7.9164657344011));
#27731=CARTESIAN_POINT('Ctrl Pts',(-0.23855264953969,2.41337447712195,7.9154217067485));
#27732=CARTESIAN_POINT('Ctrl Pts',(-0.221780680970103,2.4254544544029,7.91437767909591));
#27733=CARTESIAN_POINT('Ctrl Pts',(-0.204216383250429,2.43612580801259,
7.91333365144331));
#27734=CARTESIAN_POINT('Ctrl Pts',(-0.198004121375393,2.43990012590691,
7.91296439254744));
#27735=CARTESIAN_POINT('Ctrl Pts',(-0.191692969636716,2.44349865308767,
7.91259513365157));
#27736=CARTESIAN_POINT('Ctrl Pts',(-0.185293931287982,2.44691648710871,
7.9122258747557));
#27737=CARTESIAN_POINT('Ctrl Pts',(-0.16720267582725,2.45657933096543,7.91118191210815));
#27738=CARTESIAN_POINT('Ctrl Pts',(-0.148299623741452,2.46485200166864,
7.9101379494606));
#27739=CARTESIAN_POINT('Ctrl Pts',(-0.128824299065037,2.47160353869467,
7.90909398681304));
#27740=CARTESIAN_POINT('Ctrl Pts',(-0.109384801346949,2.47834265554083,
7.90805194464727));
#27741=CARTESIAN_POINT('Ctrl Pts',(-0.0893757885776367,2.4835658987333,
7.9070099024815));
#27742=CARTESIAN_POINT('Ctrl Pts',(-0.0690581046975076,2.48718970566841,
7.90596786031573));
#27743=CARTESIAN_POINT('Ctrl Pts',(-0.048762241690685,2.4908096206918,7.90492693728688));
#27744=CARTESIAN_POINT('Ctrl Pts',(-0.028159081291911,2.49283335263135,
7.90388601425803));
#27745=CARTESIAN_POINT('Ctrl Pts',(-0.00752098575915269,2.49322808238122,
7.90284509122917));
#27746=CARTESIAN_POINT('Ctrl Pts',(0.0131277089615774,2.49362301485399,
7.90180363360938));
#27747=CARTESIAN_POINT('Ctrl Pts',(0.0338106393244828,2.49238724358352,
7.90076217598959));
#27748=CARTESIAN_POINT('Ctrl Pts',(0.0542535281705359,2.48954004246168,
7.8997207183698));
#27749=CARTESIAN_POINT('Ctrl Pts',(0.0747026632103695,2.48669197139578,
7.8986789425393));
#27750=CARTESIAN_POINT('Ctrl Pts',(0.0949108875852173,2.48223162754792,
7.8976371667088));
#27751=CARTESIAN_POINT('Ctrl Pts',(0.114613156128634,2.47622960335709,7.8965953908783));
#27752=CARTESIAN_POINT('Ctrl Pts',(0.134358011572604,2.47021460565477,7.8955513632257));
#27753=CARTESIAN_POINT('Ctrl Pts',(0.153594042391942,2.4626515441632,7.89450733557311));
#27754=CARTESIAN_POINT('Ctrl Pts',(0.172074579293369,2.4536597646906,7.89346330792051));
#27755=CARTESIAN_POINT('Ctrl Pts',(0.178610902957094,2.45047949015316,7.89309404902464));
#27756=CARTESIAN_POINT('Ctrl Pts',(0.185052949511451,2.44712090855824,7.89272479012878));
#27757=CARTESIAN_POINT('Ctrl Pts',(0.191390640631951,2.44359061785574,7.89235553123291));
#27758=CARTESIAN_POINT('Ctrl Pts',(0.209308456223094,2.43360983832772,7.89131156858535));
#27759=CARTESIAN_POINT('Ctrl Pts',(0.226496829517949,2.4221939598158,7.8902676059378));
#27760=CARTESIAN_POINT('Ctrl Pts',(0.242715987875687,2.4094734871189,7.88922364329025));
#27761=CARTESIAN_POINT('Ctrl Pts',(0.258905309343913,2.39677641510223,7.88818160112448));
#27762=CARTESIAN_POINT('Ctrl Pts',(0.274128345891043,2.38277991483484,7.88713955895871));
#27763=CARTESIAN_POINT('Ctrl Pts',(0.288173637045684,2.36765807462481,7.88609751679294));
#27764=CARTESIAN_POINT('Ctrl Pts',(0.30220384377827,2.35255247503362,7.88505659376408));
#27765=CARTESIAN_POINT('Ctrl Pts',(0.315058296826067,2.33632445154883,7.88401567073523));
#27766=CARTESIAN_POINT('Ctrl Pts',(0.326561966685752,2.3191852456584,7.88297474770638));
#27767=CARTESIAN_POINT('Ctrl Pts',(0.338071544530455,2.30203723751854,7.88193329008658));
#27768=CARTESIAN_POINT('Ctrl Pts',(0.348228529842791,2.28397771403659,7.88089183246679));
#27769=CARTESIAN_POINT('Ctrl Pts',(0.3569006572741,2.26524772566458,7.879850374847));
#27770=CARTESIAN_POINT('Ctrl Pts',(0.365575434418412,2.24651201446456,7.8788085990165));
#27771=CARTESIAN_POINT('Ctrl Pts',(0.37276417444497,2.22710611287623,7.877766823186));
#27772=CARTESIAN_POINT('Ctrl Pts',(0.378382759002726,2.20729108858375,7.87672504735551));
#27773=CARTESIAN_POINT('Ctrl Pts',(0.384013488258505,2.1874332336666,7.87568101970291));
#27774=CARTESIAN_POINT('Ctrl Pts',(0.388067141799957,2.16716521270317,7.87463699205031));
#27775=CARTESIAN_POINT('Ctrl Pts',(0.390510541173974,2.14675903369415,7.87359296439771));
#27776=CARTESIAN_POINT('Ctrl Pts',(0.391374739505084,2.13954163565784,7.87322370550185));
#27777=CARTESIAN_POINT('Ctrl Pts',(0.392037980166997,2.13230698667105,7.87285444660598));
#27778=CARTESIAN_POINT('Ctrl Pts',(0.392500355254997,2.12506713235895,7.87248518771012));
#27779=CARTESIAN_POINT('Ctrl Pts',(0.393807574461998,2.10459873590271,7.87144122506257));
#27780=CARTESIAN_POINT('Ctrl Pts',(0.393513276453599,2.08396682257882,7.87039726241501));
#27781=CARTESIAN_POINT('Ctrl Pts',(0.391597398738457,2.06344364212242,7.86935329976746));
#27782=CARTESIAN_POINT('Ctrl Pts',(0.389685045486819,2.04295821626795,7.86831125760169));
#27783=CARTESIAN_POINT('Ctrl Pts',(0.386157042209058,2.02258185608459,7.86726921543592));
#27784=CARTESIAN_POINT('Ctrl Pts',(0.381045298097555,2.00258659846948,7.86622717327015));
#27785=CARTESIAN_POINT('Ctrl Pts',(0.375939043918924,1.98261281544694,7.8651862502413));
#27786=CARTESIAN_POINT('Ctrl Pts',(0.369252578920146,1.96302003883919,7.86414532721244));
#27787=CARTESIAN_POINT('Ctrl Pts',(0.361068772093729,1.94406978542076,7.86310440418359));
#27788=CARTESIAN_POINT('Ctrl Pts',(0.352880762277423,1.92510979964608,7.8620629465638));
#27789=CARTESIAN_POINT('Ctrl Pts',(0.34319415126381,1.90679367816525,7.86102148894401));
#27790=CARTESIAN_POINT('Ctrl Pts',(0.332140020965691,1.88936311701672,7.85998003132421));
#27791=CARTESIAN_POINT('Ctrl Pts',(0.321082513148847,1.87192723007186,7.85893825549372));
#27792=CARTESIAN_POINT('Ctrl Pts',(0.308657078511336,1.85537804357542,7.85789647966322));
#27793=CARTESIAN_POINT('Ctrl Pts',(0.295037692652914,1.83992760639767,7.85685470383272));
#27794=CARTESIAN_POINT('Ctrl Pts',(0.281388868182896,1.82444377274935,7.85581067618012));
#27795=CARTESIAN_POINT('Ctrl Pts',(0.266541469177281,1.81006394230613,7.85476664852753));
#27796=CARTESIAN_POINT('Ctrl Pts',(0.25070624473702,1.79696325495105,7.85372262087493));
#27797=CARTESIAN_POINT('Ctrl Pts',(0.245105533416708,1.79232971355413,7.85335336197906));
#27798=CARTESIAN_POINT('Ctrl Pts',(0.23938153517094,1.78785580271229,7.8529841030832));
#27799=CARTESIAN_POINT('Ctrl Pts',(0.233544428029886,1.78354796550473,7.85261484418733));
#27800=CARTESIAN_POINT('Ctrl Pts',(0.217041855192152,1.77136891934832,7.85157088153978));
#27801=CARTESIAN_POINT('Ctrl Pts',(0.199534864238156,1.76044794290577,7.85052691889222));
#27802=CARTESIAN_POINT('Ctrl Pts',(0.181241507430582,1.75094927877987,7.84948295624467));
#27803=CARTESIAN_POINT('Ctrl Pts',(0.162981803224076,1.74146808847018,7.8484409140789));
#27804=CARTESIAN_POINT('Ctrl Pts',(0.143939222834498,1.73340440484813,7.84739887191313));
#27805=CARTESIAN_POINT('Ctrl Pts',(0.124359772778037,1.72687865658127,7.84635682974736));
#27806=CARTESIAN_POINT('Ctrl Pts',(0.104801350743349,1.72035991686554,7.84531590671851));
#27807=CARTESIAN_POINT('Ctrl Pts',(0.0847078890543636,1.71537609235677,
7.84427498368965));
#27808=CARTESIAN_POINT('Ctrl Pts',(0.064344134180387,1.71199906907769,7.8432340606608));
#27809=CARTESIAN_POINT('Ctrl Pts',(0.0439699210126507,1.70862031144748,
7.84219260304101));
#27810=CARTESIAN_POINT('Ctrl Pts',(0.023325860565065,1.70685013991164,7.84115114542122));
#27811=CARTESIAN_POINT('Ctrl Pts',(0.00268613220208843,1.70670917288374,
7.84010968780142));
#27812=CARTESIAN_POINT('Ctrl Pts',(-0.0179599024977188,1.70656816278427,
7.83906791197093));
#27813=CARTESIAN_POINT('Ctrl Pts',(-0.0386008670895658,1.70805731702189,
7.83802613614043));
#27814=CARTESIAN_POINT('Ctrl Pts',(-0.0589642909510291,1.71114513968237,
7.83698436030993));
#27815=CARTESIAN_POINT('Ctrl Pts',(-0.0793717308152733,1.7142396367416,
7.83594033265733));
#27816=CARTESIAN_POINT('Ctrl Pts',(-0.0994997150711637,1.71893953361309,
7.83489630500474));
#27817=CARTESIAN_POINT('Ctrl Pts',(-0.119086900672914,1.72516243506271,
7.83385227735214));
#27818=CARTESIAN_POINT('Ctrl Pts',(-0.126014631476254,1.72736339373718,
7.83348301845627));
#27819=CARTESIAN_POINT('Ctrl Pts',(-0.132874879491201,1.72975442516975,
7.83311375956041));
#27820=CARTESIAN_POINT('Ctrl Pts',(-0.139656717709764,1.73233045924562,
7.83274450066454));
#27821=CARTESIAN_POINT('Ctrl Pts',(-0.158830218636052,1.73961338021013,
7.83170053801699));
#27822=CARTESIAN_POINT('Ctrl Pts',(-0.177489621696974,1.74842184977827,
7.83065657536943));
#27823=CARTESIAN_POINT('Ctrl Pts',(-0.195378793141691,1.75866143319206,
7.82961261272188));
#27824=CARTESIAN_POINT('Ctrl Pts',(-0.213235055527869,1.76888217978879,
7.82857057055611));
#27825=CARTESIAN_POINT('Ctrl Pts',(-0.230323237935067,1.7805285046799,7.82752852839034));
#27826=CARTESIAN_POINT('Ctrl Pts',(-0.246408914011127,1.79345875139574,
7.82648648622457));
#27827=CARTESIAN_POINT('Ctrl Pts',(-0.262477314323779,1.80637511122974,
7.82544556319571));
#27828=CARTESIAN_POINT('Ctrl Pts',(-0.277544757081132,1.82057221932032,
7.82440464016686));
#27829=CARTESIAN_POINT('Ctrl Pts',(-0.291407487180691,1.83586638529896,
7.823363717138));
#27830=CARTESIAN_POINT('Ctrl Pts',(-0.30527733681712,1.85116840596264,7.82232225951821));
#27831=CARTESIAN_POINT('Ctrl Pts',(-0.317940731673067,1.86756807576885,
7.82128080189842));
#27832=CARTESIAN_POINT('Ctrl Pts',(-0.329231917173156,1.88484602091877,
7.82023934427863));
#27833=CARTESIAN_POINT('Ctrl Pts',(-0.340526552622667,1.90212924523418,
7.81919756844813));
#27834=CARTESIAN_POINT('Ctrl Pts',(-0.350447772169409,1.92029064392291,
7.81815579261763));
#27835=CARTESIAN_POINT('Ctrl Pts',(-0.35887456487084,1.93908406949974,7.81711401678713));
#27836=CARTESIAN_POINT('Ctrl Pts',(-0.367319572275924,1.95791811749243,
7.81606998913453));
#27837=CARTESIAN_POINT('Ctrl Pts',(-0.37426345640492,1.97738622613225,7.81502596148194));
#27838=CARTESIAN_POINT('Ctrl Pts',(-0.379634026933072,1.99722405147808,
7.81398193382934));
#27839=CARTESIAN_POINT('Ctrl Pts',(-0.381533527332743,2.0042404302735,7.81361267493348));
#27840=CARTESIAN_POINT('Ctrl Pts',(-0.383236681501575,2.01130295815055,
7.81324341603761));
#27841=CARTESIAN_POINT('Ctrl Pts',(-0.384741837496011,2.01839970294053,
7.81287415714175));
#27842=CARTESIAN_POINT('Ctrl Pts',(-0.390391121414536,2.04503582993608,
7.81148822216234));
#27843=CARTESIAN_POINT('Ctrl Pts',(-0.393275160366044,2.07227807150579,
7.81010228718292));
#27844=CARTESIAN_POINT('Ctrl Pts',(-0.393299840076811,2.09964532330949,
7.8087163522035));
#27845=CARTESIAN_POINT('',(-0.392652606621955,2.10000006244036,7.6837163522035));
#27846=CARTESIAN_POINT('Ctrl Pts',(-0.39339560660603,2.09964617938564,7.80871630448812));
#27847=CARTESIAN_POINT('Ctrl Pts',(-0.392436633507189,2.20309412285361,
7.80347880753172));
#27848=CARTESIAN_POINT('Ctrl Pts',(-0.297548046247412,2.43892015636596,
7.79161786273442));
#27849=CARTESIAN_POINT('Ctrl Pts',(0.100487270537579,2.55406754116476,7.77313347009617));
#27850=CARTESIAN_POINT('Ctrl Pts',(0.436183693642714,2.26130346828162,7.75326312657338));
#27851=CARTESIAN_POINT('Ctrl Pts',(0.371740958878468,1.82056542273442,7.73339278305059));
#27852=CARTESIAN_POINT('Ctrl Pts',(-0.0337234976950709,1.63617056024581,
7.7135224395278));
#27853=CARTESIAN_POINT('Ctrl Pts',(-0.345833540474424,1.83709412712005,
7.69696362924544));
#27854=CARTESIAN_POINT('Ctrl Pts',(-0.392652513771598,2.03427171757279,
7.687028266804));
#27855=CARTESIAN_POINT('Ctrl Pts',(-0.392652606621955,2.10000006244036,
7.6837163522035));
#27856=CARTESIAN_POINT('',(-0.393299840100549,2.10035465036696,7.5587163522035));
#27857=CARTESIAN_POINT('Ctrl Pts',(-0.392652606621955,2.10000006244036,
7.6837163522035));
#27858=CARTESIAN_POINT('Ctrl Pts',(-0.392652699461621,2.16572083882566,
7.68040481896307));
#27859=CARTESIAN_POINT('Ctrl Pts',(-0.345841471197197,2.36289061215051,
7.67046983788174));
#27860=CARTESIAN_POINT('Ctrl Pts',(-0.0337501714246444,2.56382749962499,
7.65391140895943));
#27861=CARTESIAN_POINT('Ctrl Pts',(0.371724888611281,2.37945595478788,7.63404106543665));
#27862=CARTESIAN_POINT('Ctrl Pts',(0.436192969120214,1.93872161592588,7.61417072191384));
#27863=CARTESIAN_POINT('Ctrl Pts',(0.100513382771949,1.64593823838246,7.59430037839108));
#27864=CARTESIAN_POINT('Ctrl Pts',(-0.297536766592373,1.76106510782775,
7.57581560443067));
#27865=CARTESIAN_POINT('Ctrl Pts',(-0.392436806074336,1.99689847231397,
7.56395427831121));
#27866=CARTESIAN_POINT('Ctrl Pts',(-0.393395836408773,2.10035379224535,
7.55871640003268));
#27867=CARTESIAN_POINT('',(-0.393495500114951,2.09981301717212,7.43371629079915));
#27868=CARTESIAN_POINT('Ctrl Pts',(-0.393299840100549,2.10035465036696,
7.5587163522035));
#27869=CARTESIAN_POINT('Ctrl Pts',(-0.393275169063348,2.12771431467307,
7.55733079858416));
#27870=CARTESIAN_POINT('Ctrl Pts',(-0.390392727573699,2.15494904886535,
7.55594524496482));
#27871=CARTESIAN_POINT('Ctrl Pts',(-0.384746529508904,2.18157817128898,
7.55455969134548));
#27872=CARTESIAN_POINT('Ctrl Pts',(-0.380492331188422,2.20164221555212,
7.55351572869793));
#27873=CARTESIAN_POINT('Ctrl Pts',(-0.37465175991358,2.22143236931363,7.55247176605038));
#27874=CARTESIAN_POINT('Ctrl Pts',(-0.36727882436407,2.2406810405625,7.55142780340283));
#27875=CARTESIAN_POINT('Ctrl Pts',(-0.359919452123981,2.25989430180644,
7.55038576123706));
#27876=CARTESIAN_POINT('Ctrl Pts',(-0.351033515787082,2.27856735717682,
7.54934371907129));
#27877=CARTESIAN_POINT('Ctrl Pts',(-0.340725017678054,2.29644681806609,
7.54830167690552));
#27878=CARTESIAN_POINT('Ctrl Pts',(-0.330427590734058,2.31430707669522,
7.54726075387667));
#27879=CARTESIAN_POINT('Ctrl Pts',(-0.318710975674559,2.33137478424272,
7.54621983084782));
#27880=CARTESIAN_POINT('Ctrl Pts',(-0.305725417742669,2.34742040931595,
7.54517890781897));
#27881=CARTESIAN_POINT('Ctrl Pts',(-0.292733190766667,2.36347427500402,
7.54413745019918));
#27882=CARTESIAN_POINT('Ctrl Pts',(-0.27847116931383,2.37850442746855,7.54309599257939));
#27883=CARTESIAN_POINT('Ctrl Pts',(-0.263130691087117,2.39231340955901,
7.5420545349596));
#27884=CARTESIAN_POINT('Ctrl Pts',(-0.247785525675512,2.40612661089553,
7.54101275912911));
#27885=CARTESIAN_POINT('Ctrl Pts',(-0.2313618181023,2.41871743410824,7.53997098329861));
#27886=CARTESIAN_POINT('Ctrl Pts',(-0.214084229156525,2.42992852684552,
7.53892920746812));
#27887=CARTESIAN_POINT('Ctrl Pts',(-0.19676929431017,2.44116385261416,7.53788517981552));
#27888=CARTESIAN_POINT('Ctrl Pts',(-0.17859744075984,2.45101314291104,7.53684115216293));
#27889=CARTESIAN_POINT('Ctrl Pts',(-0.159818802426733,2.45936449517292,
7.53579712451033));
#27890=CARTESIAN_POINT('Ctrl Pts',(-0.153177044193876,2.46231825900057,
7.53542786561446));
#27891=CARTESIAN_POINT('Ctrl Pts',(-0.146459551390773,2.46508508472355,
7.53505860671858));
#27892=CARTESIAN_POINT('Ctrl Pts',(-0.139677861325145,2.46766150880346,
7.5346893478227));
#27893=CARTESIAN_POINT('Ctrl Pts',(-0.120504779254941,2.47494553238072,
7.53364538517515));
#27894=CARTESIAN_POINT('Ctrl Pts',(-0.100703256878215,2.4807474432975,7.5326014225276));
#27895=CARTESIAN_POINT('Ctrl Pts',(-0.080527526223084,2.48496780062804,
7.53155745988004));
#27896=CARTESIAN_POINT('Ctrl Pts',(-0.0603889109985461,2.4891803941565,
7.53051541771427));
#27897=CARTESIAN_POINT('Ctrl Pts',(-0.0398781538156886,2.4918170020599,
7.5294733755485));
#27898=CARTESIAN_POINT('Ctrl Pts',(-0.0192646066900649,2.49282790752323,
7.52843133338273));
#27899=CARTESIAN_POINT('Ctrl Pts',(0.00132680180977449,2.49383772728997,
7.52739041035388));
#27900=CARTESIAN_POINT('Ctrl Pts',(0.0220200513400488,2.49322524605851,
7.52634948732502));
#27901=CARTESIAN_POINT('Ctrl Pts',(0.0425408173313714,2.49099254322912,
7.52530856429617));
#27902=CARTESIAN_POINT('Ctrl Pts',(0.0630721222532712,2.48875869374176,
7.52426710667638));
#27903=CARTESIAN_POINT('Ctrl Pts',(0.0834300334619058,2.48490302385815,
7.52322564905659));
#27904=CARTESIAN_POINT('Ctrl Pts',(0.103344950893888,2.47947952662132,7.52218419143679));
#27905=CARTESIAN_POINT('Ctrl Pts',(0.123265953201359,2.47405437226964,7.5211424156063));
#27906=CARTESIAN_POINT('Ctrl Pts',(0.142742992456503,2.46706066499246,7.5201006397758));
#27907=CARTESIAN_POINT('Ctrl Pts',(0.161522151040302,2.45860212593251,7.5190588639453));
#27908=CARTESIAN_POINT('Ctrl Pts',(0.180341901201536,2.45012530354843,7.5180148362927));
#27909=CARTESIAN_POINT('Ctrl Pts',(0.19846011349999,2.4401776825305,7.5169708086401));
#27910=CARTESIAN_POINT('Ctrl Pts',(0.215647296245783,2.42890900507874,7.51592678098751));
#27911=CARTESIAN_POINT('Ctrl Pts',(0.221726177497598,2.4249234215711,7.51555752209164));
#27912=CARTESIAN_POINT('Ctrl Pts',(0.227688874335315,2.42077296610703,7.51518826319577));
#27913=CARTESIAN_POINT('Ctrl Pts',(0.233526229200695,2.41646546458548,7.51481900429991));
#27914=CARTESIAN_POINT('Ctrl Pts',(0.250029502400629,2.40428736747496,7.51377504165236));
#27915=CARTESIAN_POINT('Ctrl Pts',(0.265626774832429,2.39077857213967,7.5127310790048));
#27916=CARTESIAN_POINT('Ctrl Pts',(0.280096814394786,2.37609901225085,7.51168711635725));
#27917=CARTESIAN_POINT('Ctrl Pts',(0.294540234760133,2.36144645699424,7.51064507419148));
#27918=CARTESIAN_POINT('Ctrl Pts',(0.307859985361099,2.34562788862102,7.50960303202571));
#27919=CARTESIAN_POINT('Ctrl Pts',(0.319868458296564,2.32884287051813,7.50856098985994));
#27920=CARTESIAN_POINT('Ctrl Pts',(0.331864034320745,2.312075879261,7.50752006683109));
#27921=CARTESIAN_POINT('Ctrl Pts',(0.342550679009269,2.29434507739864,7.50647914380223));
#27922=CARTESIAN_POINT('Ctrl Pts',(0.351781643912968,2.27588224755754,7.50543822077338));
#27923=CARTESIAN_POINT('Ctrl Pts',(0.361017349599651,2.25740993568823,7.50439676315359));
#27924=CARTESIAN_POINT('Ctrl Pts',(0.368795538509466,2.23820549567262,7.50335530553379));
#27925=CARTESIAN_POINT('Ctrl Pts',(0.375015669574018,2.21852483948081,7.502313847914));
#27926=CARTESIAN_POINT('Ctrl Pts',(0.381237701159786,2.19883816999052,7.5012720720835));
#27927=CARTESIAN_POINT('Ctrl Pts',(0.38590054013969,2.17867570654299,7.50023029625301));
#27928=CARTESIAN_POINT('Ctrl Pts',(0.388953946912425,2.15830709374721,7.49918852042251));
#27929=CARTESIAN_POINT('Ctrl Pts',(0.39201395369319,2.13789445373265,7.49814449276991));
#27930=CARTESIAN_POINT('Ctrl Pts',(0.393457531527764,2.11727550943757,7.49710046511731));
#27931=CARTESIAN_POINT('Ctrl Pts',(0.393286358340577,2.09672427974226,7.49605643746472));
#27932=CARTESIAN_POINT('Ctrl Pts',(0.393225816627965,2.08945557917951,7.49568717856885));
#27933=CARTESIAN_POINT('Ctrl Pts',(0.392963754899772,2.08219532038326,7.49531791967299));
#27934=CARTESIAN_POINT('Ctrl Pts',(0.392501796160234,2.07495543949297,7.49494866077712));
#27935=CARTESIAN_POINT('Ctrl Pts',(0.391195754046726,2.05448696789535,7.49390469812957));
#27936=CARTESIAN_POINT('Ctrl Pts',(0.388280402454325,2.03405994697172,7.49286073548201));
#27937=CARTESIAN_POINT('Ctrl Pts',(0.38377045954345,2.01394696761991,7.49181677283446));
#27938=CARTESIAN_POINT('Ctrl Pts',(0.379268813158532,1.99387098826091,7.49077473066869));
#27939=CARTESIAN_POINT('Ctrl Pts',(0.373178499321527,1.97410862658987,7.48973268850292));
#27940=CARTESIAN_POINT('Ctrl Pts',(0.365565758954518,1.9549256539563,7.48869064633715));
#27941=CARTESIAN_POINT('Ctrl Pts',(0.357961194551069,1.93576328353398,7.4876497233083));
#27942=CARTESIAN_POINT('Ctrl Pts',(0.348837692751426,1.91717975791872,7.48660880027944));
#27943=CARTESIAN_POINT('Ctrl Pts',(0.338310702950755,1.8994239339578,7.48556787725059));
#27944=CARTESIAN_POINT('Ctrl Pts',(0.327778306762491,1.88165899106846,7.4845264196308));
#27945=CARTESIAN_POINT('Ctrl Pts',(0.31584134395354,1.86472324018675,7.48348496201101));
#27946=CARTESIAN_POINT('Ctrl Pts',(0.302660565193323,1.84883974781654,7.48244350439121));
#27947=CARTESIAN_POINT('Ctrl Pts',(0.289475759130561,1.83295140234695,7.48140172856072));
#27948=CARTESIAN_POINT('Ctrl Pts',(0.275046877859373,1.81811649807065,7.48035995273022));
#27949=CARTESIAN_POINT('Ctrl Pts',(0.259573447790861,1.80452324084293,7.47931817689972));
#27950=CARTESIAN_POINT('Ctrl Pts',(0.244066571552117,1.79090060148124,7.47827414924712));
#27951=CARTESIAN_POINT('Ctrl Pts',(0.227511228784971,1.77852540828395,7.47723012159453));
#27952=CARTESIAN_POINT('Ctrl Pts',(0.210138727760929,1.76754458179326,7.47618609394193));
#27953=CARTESIAN_POINT('Ctrl Pts',(0.203994301863178,1.76366080739747,7.47581683504606));
#27954=CARTESIAN_POINT('Ctrl Pts',(0.197747887528184,1.75995104431961,7.4754475761502));
#27955=CARTESIAN_POINT('Ctrl Pts',(0.191410399437225,1.75642038915663,7.47507831725433));
#27956=CARTESIAN_POINT('Ctrl Pts',(0.173493157847841,1.74643857923194,7.47403435460678));
#27957=CARTESIAN_POINT('Ctrl Pts',(0.154739620427987,1.73783234352959,7.47299039195922));
#27958=CARTESIAN_POINT('Ctrl Pts',(0.135386953691321,1.73073686513519,7.47194642931167));
#27959=CARTESIAN_POINT('Ctrl Pts',(0.116069888270487,1.72365443963789,7.4709043871459));
#27960=CARTESIAN_POINT('Ctrl Pts',(0.0961565438196057,1.71807756109961,
7.46986234498013));
#27961=CARTESIAN_POINT('Ctrl Pts',(0.0759062430558385,1.71409439980074,
7.46882030281436));
#27962=CARTESIAN_POINT('Ctrl Pts',(0.0556776907969656,1.71011551635454,
7.46777937978551));
#27963=CARTESIAN_POINT('Ctrl Pts',(0.0351136133577157,1.70772712181982,
7.46673845675665));
#27964=CARTESIAN_POINT('Ctrl Pts',(0.014485748874539,1.70696685498607,7.4656975337278));
#27965=CARTESIAN_POINT('Ctrl Pts',(-0.00615270954220543,1.70620619769908,
7.46465607610801));
#27966=CARTESIAN_POINT('Ctrl Pts',(-0.0268542857634539,1.70707538179094,
7.46361461848822));
#27967=CARTESIAN_POINT('Ctrl Pts',(-0.0473444042369372,1.70955999514977,
7.46257316086843));
#27968=CARTESIAN_POINT('Ctrl Pts',(-0.0678407833349112,1.7120453676663,
7.46153138503793));
#27969=CARTESIAN_POINT('Ctrl Pts',(-0.0881248506056897,1.71614702764487,
7.46048960920743));
#27970=CARTESIAN_POINT('Ctrl Pts',(-0.107930351944881,1.72179908893677,
7.45944783337693));
#27971=CARTESIAN_POINT('Ctrl Pts',(-0.127778663324661,1.72746336728742,
7.45840380572433));
#27972=CARTESIAN_POINT('Ctrl Pts',(-0.147145653511074,1.73468448021601,
7.45735977807174));
#27973=CARTESIAN_POINT('Ctrl Pts',(-0.165782577734869,1.7433474703306,7.45631575041914));
#27974=CARTESIAN_POINT('Ctrl Pts',(-0.172374213544621,1.74641145638179,
7.45594649152327));
#27975=CARTESIAN_POINT('Ctrl Pts',(-0.178874745706579,1.74965539160765,
7.45557723262741));
#27976=CARTESIAN_POINT('Ctrl Pts',(-0.185273980596595,1.75307285762873,
7.45520797373154));
#27977=CARTESIAN_POINT('Ctrl Pts',(-0.203365791715768,1.76273466108216,
7.45416401108399));
#27978=CARTESIAN_POINT('Ctrl Pts',(-0.220753697443928,1.77384426022481,
7.45312004843643));
#27979=CARTESIAN_POINT('Ctrl Pts',(-0.237195650903155,1.78627541825252,
7.45207608578888));
#27980=CARTESIAN_POINT('Ctrl Pts',(-0.253607357617271,1.79868370782551,
7.45103404362311));
#27981=CARTESIAN_POINT('Ctrl Pts',(-0.269075950105387,1.8124083392554,7.44999200145734));
#27982=CARTESIAN_POINT('Ctrl Pts',(-0.283386917144658,1.82727899752449,
7.44894995929157));
#27983=CARTESIAN_POINT('Ctrl Pts',(-0.29768251443015,1.84213368494022,7.44790903626272));
#27984=CARTESIAN_POINT('Ctrl Pts',(-0.310822426004836,1.85813144832107,
7.44686811323387));
#27985=CARTESIAN_POINT('Ctrl Pts',(-0.322627907737369,1.87506417993346,
7.44582719020501));
#27986=CARTESIAN_POINT('Ctrl Pts',(-0.334439452457633,1.89200560775548,
7.44478573258522));
#27987=CARTESIAN_POINT('Ctrl Pts',(-0.3449147641733,1.90988236874536,7.44374427496543));
#27988=CARTESIAN_POINT('Ctrl Pts',(-0.353917328138373,1.92845579332605,
7.44270281734564));
#27989=CARTESIAN_POINT('Ctrl Pts',(-0.362922642779217,1.94703489289769,
7.44166104151514));
#27990=CARTESIAN_POINT('Ctrl Pts',(-0.370454025755053,1.96631040249137,
7.44061926568465));
#27991=CARTESIAN_POINT('Ctrl Pts',(-0.376422747161753,1.98602278552623,
7.43957748985415));
#27992=CARTESIAN_POINT('Ctrl Pts',(-0.38240437009522,2.00577777732435,7.43853346220155));
#27993=CARTESIAN_POINT('Ctrl Pts',(-0.386816430782504,2.02597080833257,
7.43748943454896));
#27994=CARTESIAN_POINT('Ctrl Pts',(-0.389620937418854,2.0463305009819,7.43644540689636));
#27995=CARTESIAN_POINT('Ctrl Pts',(-0.390612854655356,2.05353145740219,
7.43607614800049));
#27996=CARTESIAN_POINT('Ctrl Pts',(-0.391404151353232,2.06075322198397,
7.43570688910462));
#27997=CARTESIAN_POINT('Ctrl Pts',(-0.391994706207888,2.0679837493608,7.43533763020876));
#27998=CARTESIAN_POINT('Ctrl Pts',(-0.392859008198951,2.07856593179309,
7.434797204207));
#27999=CARTESIAN_POINT('Ctrl Pts',(-0.393294871948269,2.08918358074563,
7.43425677820525));
#28000=CARTESIAN_POINT('Ctrl Pts',(-0.393299955020244,2.09981190142455,
7.4337163522035));
#28001=CARTESIAN_POINT('',(-0.393134823968354,2.09974753055899,7.30871640423617));
#28002=CARTESIAN_POINT('Ctrl Pts',(-0.393839208888362,2.09981497831685,
7.433716182869));
#28003=CARTESIAN_POINT('Ctrl Pts',(-0.393130725605086,2.21961039447394,
7.42763321747465));
#28004=CARTESIAN_POINT('Ctrl Pts',(-0.270765457358387,2.47109464075752,
7.41492680423937));
#28005=CARTESIAN_POINT('Ctrl Pts',(0.157408377376609,2.537604417495,7.39559694316317));
#28006=CARTESIAN_POINT('Ctrl Pts',(0.453153628130196,2.20453139620186,7.3757265996404));
#28007=CARTESIAN_POINT('Ctrl Pts',(0.333192116370157,1.77556504955804,7.35585625611758));
#28008=CARTESIAN_POINT('Ctrl Pts',(-0.0924278021488653,1.64422360211459,
7.33598591259482));
#28009=CARTESIAN_POINT('Ctrl Pts',(-0.361952445184268,1.87099925901134,
7.32027266154399));
#28010=CARTESIAN_POINT('Ctrl Pts',(-0.393106482257739,2.05085104044711,
7.3111828583341));
#28011=CARTESIAN_POINT('Ctrl Pts',(-0.39282156461649,2.09974577364633,7.30871650296516));
#28012=CARTESIAN_POINT('',(-0.393299884474588,2.10030145028756,7.18371635219909));
#28013=CARTESIAN_POINT('Ctrl Pts',(-0.393299919559953,2.09974845649634,
7.3087163522035));
#28014=CARTESIAN_POINT('Ctrl Pts',(-0.393313234865234,2.12056755307232,
7.30766746530676));
#28015=CARTESIAN_POINT('Ctrl Pts',(-0.391669130710796,2.14139400732832,
7.30661857841001));
#28016=CARTESIAN_POINT('Ctrl Pts',(-0.388390445533041,2.16194959094817,
7.30556969151327));
#28017=CARTESIAN_POINT('Ctrl Pts',(-0.385111255528112,2.1825083395615,7.30452064311685));
#28018=CARTESIAN_POINT('Ctrl Pts',(-0.380197122193991,2.2027954253499,7.30347159472042));
#28019=CARTESIAN_POINT('Ctrl Pts',(-0.37372220884026,2.22254224014419,7.302422546324));
#28020=CARTESIAN_POINT('Ctrl Pts',(-0.367229923374881,2.24234203539592,
7.30137068334383));
#28021=CARTESIAN_POINT('Ctrl Pts',(-0.359168748379053,2.26159798513236,
7.30031882036367));
#28022=CARTESIAN_POINT('Ctrl Pts',(-0.349661914960496,2.28005953245013,
7.2992669573835));
#28023=CARTESIAN_POINT('Ctrl Pts',(-0.340558352447886,2.29773795834521,
7.29825971343874));
#28024=CARTESIAN_POINT('Ctrl Pts',(-0.330129824766302,2.3146876375657,7.29725246949399));
#28025=CARTESIAN_POINT('Ctrl Pts',(-0.318521561851313,2.33071390212946,
7.29624522554923));
#28026=CARTESIAN_POINT('Ctrl Pts',(-0.306490124035975,2.34732439819791,
7.29520126290168));
#28027=CARTESIAN_POINT('Ctrl Pts',(-0.293120015089348,2.36304071600702,
7.29415730025412));
#28028=CARTESIAN_POINT('Ctrl Pts',(-0.278569202794085,2.3776402154852,7.29311333760657));
#28029=CARTESIAN_POINT('Ctrl Pts',(-0.264045158285981,2.3922128576109,7.2920712954408));
#28030=CARTESIAN_POINT('Ctrl Pts',(-0.248345193240788,2.405672202284,7.29102925327503));
#28031=CARTESIAN_POINT('Ctrl Pts',(-0.231667201436317,2.41782888128467,
7.28998721110927));
#28032=CARTESIAN_POINT('Ctrl Pts',(-0.215007121533044,2.42997250420307,
7.28894628808041));
#28033=CARTESIAN_POINT('Ctrl Pts',(-0.197371674674546,2.44081578431017,
7.28790536505156));
#28034=CARTESIAN_POINT('Ctrl Pts',(-0.178991334536187,2.45020992584585,
7.28686444202271));
#28035=CARTESIAN_POINT('Ctrl Pts',(-0.16060155473418,2.45960889196778,7.28582298440292));
#28036=CARTESIAN_POINT('Ctrl Pts',(-0.141466765217106,2.46755688348555,
7.28478152678312));
#28037=CARTESIAN_POINT('Ctrl Pts',(-0.121841977349854,2.47395109647583,
7.28374006916333));
#28038=CARTESIAN_POINT('Ctrl Pts',(-0.102211193254336,2.48034726317695,
7.28269829333283));
#28039=CARTESIAN_POINT('Ctrl Pts',(-0.0820908229596269,2.4851885128946,
7.28165651750234));
#28040=CARTESIAN_POINT('Ctrl Pts',(-0.0617500554875966,2.48842221955918,
7.28061474167184));
#28041=CARTESIAN_POINT('Ctrl Pts',(-0.0413653209850891,2.49166291595409,
7.27957071401924));
#28042=CARTESIAN_POINT('Ctrl Pts',(-0.020759972403847,2.49328907420375,
7.27852668636665));
#28043=CARTESIAN_POINT('Ctrl Pts',(-0.000208032736881453,2.49329994498141,
7.27748265871405));
#28044=CARTESIAN_POINT('Ctrl Pts',(0.00706091893365014,2.49330378983298,
7.27711339981818));
#28045=CARTESIAN_POINT('Ctrl Pts',(0.01432321417879,2.49310604779979,7.27674414092231));
#28046=CARTESIAN_POINT('Ctrl Pts',(0.0215669029512129,2.49270823609531,
7.27637488202644));
#28047=CARTESIAN_POINT('Ctrl Pts',(0.0420461401300037,2.49158354941917,
7.27533091937888));
#28048=CARTESIAN_POINT('Ctrl Pts',(0.0624981830902488,2.48884924923919,
7.27428695673133));
#28049=CARTESIAN_POINT('Ctrl Pts',(0.082650321258473,2.48451763860176,7.27324299408378));
#28050=CARTESIAN_POINT('Ctrl Pts',(0.102765387397025,2.48019399642885,7.27220095191801));
#28051=CARTESIAN_POINT('Ctrl Pts',(0.122580920138787,2.47427897118711,7.27115890975224));
#28052=CARTESIAN_POINT('Ctrl Pts',(0.141830571816359,2.46683644706905,7.27011686758647));
#28053=CARTESIAN_POINT('Ctrl Pts',(0.161059549670436,2.45940191610497,7.26907594455761));
#28054=CARTESIAN_POINT('Ctrl Pts',(0.17972315976357,2.45044338008214,7.26803502152876));
#28055=CARTESIAN_POINT('Ctrl Pts',(0.197571532391663,2.44007407955975,7.2669940984999));
#28056=CARTESIAN_POINT('Ctrl Pts',(0.215429071478752,2.42969945363487,7.26595264088011));
#28057=CARTESIAN_POINT('Ctrl Pts',(0.232469892360094,2.41791297143194,7.26491118326032));
#28058=CARTESIAN_POINT('Ctrl Pts',(0.248469513396737,2.40487340145114,7.26386972564053));
#28059=CARTESIAN_POINT('Ctrl Pts',(0.264474023015123,2.39182984731324,7.26282794981003));
#28060=CARTESIAN_POINT('Ctrl Pts',(0.279436152449859,2.3775329356746,7.26178617397953));
#28061=CARTESIAN_POINT('Ctrl Pts',(0.293165935877912,2.36218051804211,7.26074439814903));
#28062=CARTESIAN_POINT('Ctrl Pts',(0.306925396544414,2.34679491581051,7.25970037049644));
#28063=CARTESIAN_POINT('Ctrl Pts',(0.319446747018133,2.33034983864067,7.25865634284384));
#28064=CARTESIAN_POINT('Ctrl Pts',(0.330581023654338,2.31307528434722,7.25761231519124));
#28065=CARTESIAN_POINT('Ctrl Pts',(0.334519071355225,2.30696550092421,7.25724305629538));
#28066=CARTESIAN_POINT('Ctrl Pts',(0.338284017950784,2.30075219171968,7.25687379739951));
#28067=CARTESIAN_POINT('Ctrl Pts',(0.341870670364721,2.29444622584246,7.25650453850364));
#28068=CARTESIAN_POINT('Ctrl Pts',(0.352010794791812,2.2766181033348,7.25546057585609));
#28069=CARTESIAN_POINT('Ctrl Pts',(0.360782806643879,2.2579415333395,7.25441661320854));
#28070=CARTESIAN_POINT('Ctrl Pts',(0.368049427381595,2.23865247565074,7.25337265056098));
#28071=CARTESIAN_POINT('Ctrl Pts',(0.375302680387439,2.21939890226213,7.25233060839521));
#28072=CARTESIAN_POINT('Ctrl Pts',(0.381055727176377,2.19953573750688,7.25128856622944));
#28073=CARTESIAN_POINT('Ctrl Pts',(0.385218103916303,2.17932151294024,7.25024652406368));
#28074=CARTESIAN_POINT('Ctrl Pts',(0.389376010329001,2.15912899813322,7.24920560103482));
#28075=CARTESIAN_POINT('Ctrl Pts',(0.39194646221738,2.13858688318684,7.24816467800597));
#28076=CARTESIAN_POINT('Ctrl Pts',(0.392889415285432,2.11796656218288,7.24712375497712));
#28077=CARTESIAN_POINT('Ctrl Pts',(0.393832852629604,2.09733565111948,7.24608229735732));
#28078=CARTESIAN_POINT('Ctrl Pts',(0.393147071614843,2.07662718803238,7.24504083973753));
#28079=CARTESIAN_POINT('Ctrl Pts',(0.390844051671458,2.05611586536072,7.24399938211774));
#28080=CARTESIAN_POINT('Ctrl Pts',(0.388540328055078,2.03559827558577,7.24295760628724));
#28081=CARTESIAN_POINT('Ctrl Pts',(0.384618499783456,2.01527867267053,7.24191583045675));
#28082=CARTESIAN_POINT('Ctrl Pts',(0.379142092013518,1.99542388387584,7.24087405462625));
#28083=CARTESIAN_POINT('Ctrl Pts',(0.37365384686391,1.97552617850462,7.23983002697365));
#28084=CARTESIAN_POINT('Ctrl Pts',(0.366604564798395,1.95609598542352,7.23878599932106));
#28085=CARTESIAN_POINT('Ctrl Pts',(0.358106995384997,1.937383057905,7.23774197166846));
#28086=CARTESIAN_POINT('Ctrl Pts',(0.355101516467524,1.93076454072614,7.23737271277259));
#28087=CARTESIAN_POINT('Ctrl Pts',(0.35191528846334,1.92423552967978,7.23700345387673));
#28088=CARTESIAN_POINT('Ctrl Pts',(0.348554639207707,1.91780627484245,7.23663419498086));
#28089=CARTESIAN_POINT('Ctrl Pts',(0.33905346717452,1.89962959182434,7.23559023233331));
#28090=CARTESIAN_POINT('Ctrl Pts',(0.328098321245705,1.88214396239898,7.23454626968575));
#28091=CARTESIAN_POINT('Ctrl Pts',(0.315813289287133,1.86559254212026,7.2335023070382));
#28092=CARTESIAN_POINT('Ctrl Pts',(0.303550856968644,1.84907156996267,7.23246026487243));
#28093=CARTESIAN_POINT('Ctrl Pts',(0.289963780582512,1.83348201523114,7.23141822270666));
#28094=CARTESIAN_POINT('Ctrl Pts',(0.275220468382341,1.81903988933764,7.23037618054089));
#28095=CARTESIAN_POINT('Ctrl Pts',(0.260492990267855,1.80461327406046,7.22933525751203));
#28096=CARTESIAN_POINT('Ctrl Pts',(0.244612244279319,1.79133217409741,7.22829433448318));
#28097=CARTESIAN_POINT('Ctrl Pts',(0.227784746718862,1.7793771699298,7.22725341145432));
#28098=CARTESIAN_POINT('Ctrl Pts',(0.210948606994239,1.76741602598364,7.22621195383453));
#28099=CARTESIAN_POINT('Ctrl Pts',(0.193165334803768,1.7567827776921,7.22517049621474));
#28100=CARTESIAN_POINT('Ctrl Pts',(0.174672381150562,1.7476160485164,7.22412903859495));
#28101=CARTESIAN_POINT('Ctrl Pts',(0.156173777093783,1.7384465185053,7.22308726276445));
#28102=CARTESIAN_POINT('Ctrl Pts',(0.1369657346463,1.73074469372405,7.22204548693395));
#28103=CARTESIAN_POINT('Ctrl Pts',(0.117306994261685,1.72460159950089,7.22100371110345));
#28104=CARTESIAN_POINT('Ctrl Pts',(0.0976057610636193,1.71844522684016,
7.21995968345085));
#28105=CARTESIAN_POINT('Ctrl Pts',(0.0774526030808848,1.71385447481779,
7.21891565579826));
#28106=CARTESIAN_POINT('Ctrl Pts',(0.057118550715062,1.7108697375374,7.21787162814566));
#28107=CARTESIAN_POINT('Ctrl Pts',(0.049926662927011,1.70981407508453,7.21750236924979));
#28108=CARTESIAN_POINT('Ctrl Pts',(0.0427121907511549,1.70895884098676,
7.21713311035393));
#28109=CARTESIAN_POINT('Ctrl Pts',(0.0354871780069168,1.70830426323854,
7.21676385145806));
#28110=CARTESIAN_POINT('Ctrl Pts',(0.0150607413861408,1.70645365184715,
7.21571988881051));
#28111=CARTESIAN_POINT('Ctrl Pts',(-0.00557170734229821,1.70619964753602,
7.21467592616295));
#28112=CARTESIAN_POINT('Ctrl Pts',(-0.026138547631234,1.70756953950065,
7.2136319635154));
#28113=CARTESIAN_POINT('Ctrl Pts',(-0.046667553001253,1.70893691140141,
7.21258992134963));
#28114=CARTESIAN_POINT('Ctrl Pts',(-0.0671304596915965,1.71192226083354,
7.21154787918387));
#28115=CARTESIAN_POINT('Ctrl Pts',(-0.0872544790089182,1.71650091800256,
7.2105058370181));
#28116=CARTESIAN_POINT('Ctrl Pts',(-0.10735688544565,1.7210746577657,7.20946491398924));
#28117=CARTESIAN_POINT('Ctrl Pts',(-0.127120406834966,1.72723817394359,
7.20842399096039));
#28118=CARTESIAN_POINT('Ctrl Pts',(-0.146281416869147,1.73491557540926,
7.20738306793154));
#28119=CARTESIAN_POINT('Ctrl Pts',(-0.165452267498667,1.74259691978821,
7.20634161031175));
#28120=CARTESIAN_POINT('Ctrl Pts',(-0.184019299603978,1.75179344401367,
7.20530015269196));
#28121=CARTESIAN_POINT('Ctrl Pts',(-0.201737419578486,1.76238053441513,
7.20425869507217));
#28122=CARTESIAN_POINT('Ctrl Pts',(-0.2194609532111,1.77297085963427,7.20321691924167));
#28123=CARTESIAN_POINT('Ctrl Pts',(-0.236334445827727,1.78495218871504,
7.20217514341117));
#28124=CARTESIAN_POINT('Ctrl Pts',(-0.252141300819966,1.79815624170638,
7.20113336758068));
#28125=CARTESIAN_POINT('Ctrl Pts',(-0.26798232268797,1.8113888355579,7.20008933992808));
#28126=CARTESIAN_POINT('Ctrl Pts',(-0.282751577743477,1.82584891460032,
7.19904531227548));
#28127=CARTESIAN_POINT('Ctrl Pts',(-0.296268388247341,1.84133045767752,
7.19800128462289));
#28128=CARTESIAN_POINT('Ctrl Pts',(-0.301049106947568,1.84680607653571,
7.19763202572702));
#28129=CARTESIAN_POINT('Ctrl Pts',(-0.305673527235467,1.85240918024165,
7.19726276683115));
#28130=CARTESIAN_POINT('Ctrl Pts',(-0.310134937872157,1.85812976555385,
7.19689350793528));
#28131=CARTESIAN_POINT('Ctrl Pts',(-0.323402210825469,1.87514155240117,
7.1957954116243));
#28132=CARTESIAN_POINT('Ctrl Pts',(-0.335308646127504,1.89330340472553,
7.19469731531332));
#28133=CARTESIAN_POINT('Ctrl Pts',(-0.345656671368315,1.91236643280432,
7.19359921900234));
#28134=CARTESIAN_POINT('Ctrl Pts',(-0.355476559111868,1.93045653129457,
7.1925571667987));
#28135=CARTESIAN_POINT('Ctrl Pts',(-0.363892952591292,1.94935726435661,
7.19151511459507));
#28136=CARTESIAN_POINT('Ctrl Pts',(-0.37078024567161,1.96882492836022,7.19047306239144));
#28137=CARTESIAN_POINT('Ctrl Pts',(-0.377659400926478,1.98826958993752,
7.18943224144642));
#28138=CARTESIAN_POINT('Ctrl Pts',(-0.383012770788352,2.00827917357428,
7.1883914205014));
#28139=CARTESIAN_POINT('Ctrl Pts',(-0.386762892875489,2.02859023389911,
7.18735059955638));
#28140=CARTESIAN_POINT('Ctrl Pts',(-0.390512479918614,2.04889839636864,
7.18630992710919));
#28141=CARTESIAN_POINT('Ctrl Pts',(-0.392659131186697,2.06950723080602,
7.18526925466201));
#28142=CARTESIAN_POINT('Ctrl Pts',(-0.393176466959007,2.0901432343219,7.18422858221483));
#28143=CARTESIAN_POINT('Ctrl Pts',(-0.393261346342918,2.09352898755716,
7.18405783887772));
#28144=CARTESIAN_POINT('Ctrl Pts',(-0.393302479711247,2.09691546388672,
7.18388709554061));
#28145=CARTESIAN_POINT('Ctrl Pts',(-0.393299884474655,2.10030145020012,
7.1837163522035));
#28146=CARTESIAN_POINT('',(-0.393299984492277,2.10011044625411,7.0587163522066));
#28147=CARTESIAN_POINT('Ctrl Pts',(-0.393299884474588,2.10030145028756,
7.18371635219909));
#28148=CARTESIAN_POINT('Ctrl Pts',(-0.39328140121979,2.12441641144914,7.18250031983454));
#28149=CARTESIAN_POINT('Ctrl Pts',(-0.391040925770389,2.1484385973344,7.18128428747));
#28150=CARTESIAN_POINT('Ctrl Pts',(-0.386653358989397,2.17200048598598,
7.18006825510545));
#28151=CARTESIAN_POINT('Ctrl Pts',(-0.382991028073696,2.19166774976753,
7.17905322487446));
#28152=CARTESIAN_POINT('Ctrl Pts',(-0.377833722194587,2.21101458890354,
7.17803819464347));
#28153=CARTESIAN_POINT('Ctrl Pts',(-0.371250469312817,2.22983828031445,
7.17702316441248));
#28154=CARTESIAN_POINT('Ctrl Pts',(-0.364479567424196,2.24919852213014,
7.17597920176493));
#28155=CARTESIAN_POINT('Ctrl Pts',(-0.356169995743994,2.26808538203898,
7.17493523911737));
#28156=CARTESIAN_POINT('Ctrl Pts',(-0.346409350110455,2.28624030754929,
7.17389127646981));
#28157=CARTESIAN_POINT('Ctrl Pts',(-0.336666660236327,2.30436183511781,
7.17284923430404));
#28158=CARTESIAN_POINT('Ctrl Pts',(-0.325478487175651,2.32175343208349,
7.17180719213827));
#28159=CARTESIAN_POINT('Ctrl Pts',(-0.312980208580934,2.33817699098913,
7.17076514997249));
#28160=CARTESIAN_POINT('Ctrl Pts',(-0.30049535294108,2.35458291125051,7.16972422694364));
#28161=CARTESIAN_POINT('Ctrl Pts',(-0.286703605366512,2.37002225735787,
7.16868330391478));
#28162=CARTESIAN_POINT('Ctrl Pts',(-0.271783177515999,2.38428646541703,
7.16764238088593));
#28163=CARTESIAN_POINT('Ctrl Pts',(-0.256855086922622,2.39855799920167,
7.16660092326613));
#28164=CARTESIAN_POINT('Ctrl Pts',(-0.240797678718658,2.41165266914036,
7.16555946564634));
#28165=CARTESIAN_POINT('Ctrl Pts',(-0.223825845084588,2.42339895032633,
7.16451800802655));
#28166=CARTESIAN_POINT('Ctrl Pts',(-0.20684882581543,2.4351488205133,7.16347623219605));
#28167=CARTESIAN_POINT('Ctrl Pts',(-0.188957449992455,2.44554909314379,
7.16243445636555));
#28168=CARTESIAN_POINT('Ctrl Pts',(-0.170394562886644,2.45447225975902,
7.16139268053505));
#28169=CARTESIAN_POINT('Ctrl Pts',(-0.151791551679105,2.46341471400139,
7.16034865288245));
#28170=CARTESIAN_POINT('Ctrl Pts',(-0.132514818220812,2.47087342219975,
7.15930462522985));
#28171=CARTESIAN_POINT('Ctrl Pts',(-0.112826694998145,2.47676919578941,
7.15826059757725));
#28172=CARTESIAN_POINT('Ctrl Pts',(-0.105863263881689,2.47885445362762,
7.1578913386814));
#28173=CARTESIAN_POINT('Ctrl Pts',(-0.0988484829767498,2.48074466075623,
7.15752207978556));
#28174=CARTESIAN_POINT('Ctrl Pts',(-0.0917942363465021,2.48243784877227,
7.15715282088971));
#28175=CARTESIAN_POINT('Ctrl Pts',(-0.0718505868599785,2.48722480194768,
7.15610885824215));
#28176=CARTESIAN_POINT('Ctrl Pts',(-0.0514720555961654,2.49046176383376,
7.1550648955946));
#28177=CARTESIAN_POINT('Ctrl Pts',(-0.0309234553292937,2.49208242744415,
7.15402093294705));
#28178=CARTESIAN_POINT('Ctrl Pts',(-0.0104126564268489,2.49370010966919,
7.15297889078128));
#28179=CARTESIAN_POINT('Ctrl Pts',(0.0102668699228779,2.49370727912618,
7.15193684861551));
#28180=CARTESIAN_POINT('Ctrl Pts',(0.0308416363372745,2.49208887190029,
7.15089480644974));
#28181=CARTESIAN_POINT('Ctrl Pts',(0.0513943057757651,2.49047220281833,
7.14985388342088));
#28182=CARTESIAN_POINT('Ctrl Pts',(0.0718417065779379,2.48723345154411,
7.14881296039203));
#28183=CARTESIAN_POINT('Ctrl Pts',(0.0919120052963912,2.48240956222667,
7.14777203736317));
#28184=CARTESIAN_POINT('Ctrl Pts',(0.111992611597167,2.47758319548541,7.14673057974338));
#28185=CARTESIAN_POINT('Ctrl Pts',(0.131695009733336,2.47117022061305,7.14568912212359));
#28186=CARTESIAN_POINT('Ctrl Pts',(0.15075865347209,2.46325847327114,7.1446476645038));
#28187=CARTESIAN_POINT('Ctrl Pts',(0.169828121985114,2.4553443085455,7.1436058886733));
#28188=CARTESIAN_POINT('Ctrl Pts',(0.188257782432902,2.44593077491543,7.1425641128428));
#28189=CARTESIAN_POINT('Ctrl Pts',(0.205808966887233,2.43515303840009,7.1415223370123));
#28190=CARTESIAN_POINT('Ctrl Pts',(0.223398088625048,2.42435200556269,7.1404783093597));
#28191=CARTESIAN_POINT('Ctrl Pts',(0.240104348151232,2.41218131645107,7.13943428170711));
#28192=CARTESIAN_POINT('Ctrl Pts',(0.255719156987838,2.39881867871575,7.13839025405451));
#28193=CARTESIAN_POINT('Ctrl Pts',(0.261241910198285,2.39409248890293,7.13802099515864));
#28194=CARTESIAN_POINT('Ctrl Pts',(0.266628457848157,2.3892175387951,7.13765173626277));
#28195=CARTESIAN_POINT('Ctrl Pts',(0.271870711810878,2.38420275519327,7.13728247736691));
#28196=CARTESIAN_POINT('Ctrl Pts',(0.286691525574139,2.37002504187486,7.13623851471935));
#28197=CARTESIAN_POINT('Ctrl Pts',(0.300444488273553,2.35464263388032,7.1351945520718));
#28198=CARTESIAN_POINT('Ctrl Pts',(0.312930499868253,2.33824229736175,7.13415058942425));
#28199=CARTESIAN_POINT('Ctrl Pts',(0.325393542099181,2.32187213102944,7.13310854725848));
#28200=CARTESIAN_POINT('Ctrl Pts',(0.336593771575419,2.30448829597703,7.13206650509271));
#28201=CARTESIAN_POINT('Ctrl Pts',(0.346370478625851,2.28631259092315,7.13102446292694));
#28202=CARTESIAN_POINT('Ctrl Pts',(0.356136685646498,2.26815640629097,7.12998353989809));
#28203=CARTESIAN_POINT('Ctrl Pts',(0.364482033102595,2.24921067101315,7.12894261686923));
#28204=CARTESIAN_POINT('Ctrl Pts',(0.371290435939313,2.22972394605467,7.12790169384038));
#28205=CARTESIAN_POINT('Ctrl Pts',(0.37810233539428,2.21022721322214,7.12686023622059));
#28206=CARTESIAN_POINT('Ctrl Pts',(0.383375455412086,2.19018962493644,7.1258187786008));
#28207=CARTESIAN_POINT('Ctrl Pts',(0.38704261140603,2.16987780016573,7.12477732098101));
#28208=CARTESIAN_POINT('Ctrl Pts',(0.390710887876003,2.14955976924703,7.12373554515051));
#28209=CARTESIAN_POINT('Ctrl Pts',(0.392772128459542,2.1289680649251,7.12269376932001));
#28210=CARTESIAN_POINT('Ctrl Pts',(0.393210787903623,2.10837653127566,7.12165199348952));
#28211=CARTESIAN_POINT('Ctrl Pts',(0.393650395520046,2.08774048855896,7.12060796583692));
#28212=CARTESIAN_POINT('Ctrl Pts',(0.39246046235079,2.06710535250755,7.11956393818433));
#28213=CARTESIAN_POINT('Ctrl Pts',(0.389677495458099,2.04674270441054,7.11851991053173));
#28214=CARTESIAN_POINT('Ctrl Pts',(0.388693196546589,2.03954070268713,7.11815065163586));
#28215=CARTESIAN_POINT('Ctrl Pts',(0.387510086784553,2.03237269840211,7.11778139273999));
#28216=CARTESIAN_POINT('Ctrl Pts',(0.38613129373705,2.02525032443581,7.11741213384412));
#28217=CARTESIAN_POINT('Ctrl Pts',(0.382233192820861,2.00511406647181,7.11636817119657));
#28218=CARTESIAN_POINT('Ctrl Pts',(0.37674411597597,1.98522355380588,7.11532420854901));
#28219=CARTESIAN_POINT('Ctrl Pts',(0.369713323077346,1.96584729320992,7.11428024590146));
#28220=CARTESIAN_POINT('Ctrl Pts',(0.362695464079869,1.94650667733323,7.11323820373569));
#28221=CARTESIAN_POINT('Ctrl Pts',(0.354141710911723,1.92767913983654,7.11219616156992));
#28222=CARTESIAN_POINT('Ctrl Pts',(0.344151560857891,1.9096198719428,7.11115411940415));
#28223=CARTESIAN_POINT('Ctrl Pts',(0.334172140068277,1.89157999941907,7.1101131963753));
#28224=CARTESIAN_POINT('Ctrl Pts',(0.32275971400379,1.87430741302607,7.10907227334644));
#28225=CARTESIAN_POINT('Ctrl Pts',(0.310060438236427,1.85803426969789,7.10803135031759));
#28226=CARTESIAN_POINT('Ctrl Pts',(0.297354640452012,1.84175276890742,7.1069898926978));
#28227=CARTESIAN_POINT('Ctrl Pts',(0.283361112605571,1.82647232658918,7.105948435078));
#28228=CARTESIAN_POINT('Ctrl Pts',(0.26826766446845,1.81239375841153,7.10490697745821));
#28229=CARTESIAN_POINT('Ctrl Pts',(0.253169604624906,1.79831088861753,7.10386520162771));
#28230=CARTESIAN_POINT('Ctrl Pts',(0.23697151772135,1.7854310990117,7.10282342579721));
#28231=CARTESIAN_POINT('Ctrl Pts',(0.219895241833309,1.77391569706735,7.10178164996671));
#28232=CARTESIAN_POINT('Ctrl Pts',(0.202782055187426,1.76237540432038,7.10073762231412));
#28233=CARTESIAN_POINT('Ctrl Pts',(0.184787531010729,1.75220574943624,7.09969359466152));
#28234=CARTESIAN_POINT('Ctrl Pts',(0.166159781646032,1.74352304848231,7.09864956700892));
#28235=CARTESIAN_POINT('Ctrl Pts',(0.15957139086373,1.74045209096563,7.09828030811306));
#28236=CARTESIAN_POINT('Ctrl Pts',(0.15290396583066,1.73756670059935,7.0979110492172));
#28237=CARTESIAN_POINT('Ctrl Pts',(0.146168980688353,1.73487054475908,7.09754179032133));
#28238=CARTESIAN_POINT('Ctrl Pts',(0.127127942004791,1.72724801752751,7.09649782767378));
#28239=CARTESIAN_POINT('Ctrl Pts',(0.107432306350444,1.72109623771241,7.09545386502623));
#28240=CARTESIAN_POINT('Ctrl Pts',(0.0873345042869595,1.71651913429618,
7.09440990237867));
#28241=CARTESIAN_POINT('Ctrl Pts',(0.0672736742960345,1.7119504509549,7.0933678602129));
#28242=CARTESIAN_POINT('Ctrl Pts',(0.0468128425269421,1.70895091352938,
7.09232581804714));
#28243=CARTESIAN_POINT('Ctrl Pts',(0.0262204380071245,1.70757500254098,
7.09128377588137));
#28244=CARTESIAN_POINT('Ctrl Pts',(0.00565014940626087,1.70620056925936,
7.09024285285251));
#28245=CARTESIAN_POINT('Ctrl Pts',(-0.0150507029261533,1.70644637831647,
7.08920192982366));
#28246=CARTESIAN_POINT('Ctrl Pts',(-0.0356078006313174,1.70831521023379,
7.08816100679481));
#28247=CARTESIAN_POINT('Ctrl Pts',(-0.0561754559260802,1.71018500193448,
7.08711954917501));
#28248=CARTESIAN_POINT('Ctrl Pts',(-0.0765984748844406,1.71367943116632,
7.08607809155522));
#28249=CARTESIAN_POINT('Ctrl Pts',(-0.0966063432742216,1.71874928926075,
7.08503663393543));
#28250=CARTESIAN_POINT('Ctrl Pts',(-0.116620324940065,1.72382069641786,
7.08399485810493));
#28251=CARTESIAN_POINT('Ctrl Pts',(-0.136218199767095,1.73046827506646,
7.08295308227444));
#28252=CARTESIAN_POINT('Ctrl Pts',(-0.155144252585005,1.73859281843073,
7.08191130644394));
#28253=CARTESIAN_POINT('Ctrl Pts',(-0.174111214495567,1.74673492317986,
7.08086727879134));
#28254=CARTESIAN_POINT('Ctrl Pts',(-0.192402803480825,1.7563600233457,7.07982325113874));
#28255=CARTESIAN_POINT('Ctrl Pts',(-0.209786911214481,1.7673224656171,7.07877922348615));
#28256=CARTESIAN_POINT('Ctrl Pts',(-0.215935442253274,1.7711997377555,7.07840996459028));
#28257=CARTESIAN_POINT('Ctrl Pts',(-0.221970727777545,1.7752439141585,7.07804070569442));
#28258=CARTESIAN_POINT('Ctrl Pts',(-0.227883473032081,1.77944733237916,
7.07767144679855));
#28259=CARTESIAN_POINT('Ctrl Pts',(-0.244480686196773,1.79124642488616,
7.07663492850733));
#28260=CARTESIAN_POINT('Ctrl Pts',(-0.26021196929393,1.80437570726496,7.07559841021611));
#28261=CARTESIAN_POINT('Ctrl Pts',(-0.27485505209332,1.81868240307656,7.07456189192489));
#28262=CARTESIAN_POINT('Ctrl Pts',(-0.289471198982429,1.83296278176081,
7.07352728030619));
#28263=CARTESIAN_POINT('Ctrl Pts',(-0.303002545897912,1.84841580435665,
7.0724926686875));
#28264=CARTESIAN_POINT('Ctrl Pts',(-0.315259522961878,1.86484829751446,
7.07145805706881));
#28265=CARTESIAN_POINT('Ctrl Pts',(-0.327838702548867,1.88171275613384,
7.07039624833029));
#28266=CARTESIAN_POINT('Ctrl Pts',(-0.339074904738169,1.89960839978937,
7.06933443959177));
#28267=CARTESIAN_POINT('Ctrl Pts',(-0.348806813328766,1.91828952431015,
7.06827263085326));
#28268=CARTESIAN_POINT('Ctrl Pts',(-0.358284341061996,1.93648234579891,
7.06723857656956));
#28269=CARTESIAN_POINT('Ctrl Pts',(-0.366335033678184,1.9554193233398,7.06620452228586));
#28270=CARTESIAN_POINT('Ctrl Pts',(-0.372856655426999,1.9748488733419,7.06517046800216));
#28271=CARTESIAN_POINT('Ctrl Pts',(-0.379640841809533,1.99506066936748,
7.06409478203623));
#28272=CARTESIAN_POINT('Ctrl Pts',(-0.384769773501248,2.01580476897136,
7.0630190960703));
#28273=CARTESIAN_POINT('Ctrl Pts',(-0.388186045340862,2.03678224772564,
7.06194341010438));
#28274=CARTESIAN_POINT('Ctrl Pts',(-0.391602317180476,2.05775972647993,
7.06086772413845));
#28275=CARTESIAN_POINT('Ctrl Pts',(-0.393305921228637,2.07896968111761,
7.05979203817253));
#28276=CARTESIAN_POINT('Ctrl Pts',(-0.393299984492276,2.10011044625411,
7.0587163522066));
#28277=CARTESIAN_POINT('',(-0.393299833421324,2.09963801828994,6.93371635362524));
#28278=CARTESIAN_POINT('Ctrl Pts',(-0.393299984492259,2.10011044631513,
7.0587163522035));
#28279=CARTESIAN_POINT('Ctrl Pts',(-0.393298300731149,2.10610632963539,
7.05841126922758));
#28280=CARTESIAN_POINT('Ctrl Pts',(-0.393159512893997,2.11210011602306,
7.05810618625166));
#28281=CARTESIAN_POINT('Ctrl Pts',(-0.392883863779012,2.11808755323626,
7.05780110327574));
#28282=CARTESIAN_POINT('Ctrl Pts',(-0.391940620784181,2.13857594917634,
7.05675714062819));
#28283=CARTESIAN_POINT('Ctrl Pts',(-0.389387586552351,2.15905140948699,
7.05571317798064));
#28284=CARTESIAN_POINT('Ctrl Pts',(-0.38523464805053,2.17924112531624,7.05466921533309));
#28285=CARTESIAN_POINT('Ctrl Pts',(-0.381089349326588,2.19939369998765,
7.05362717316732));
#28286=CARTESIAN_POINT('Ctrl Pts',(-0.375350076778481,2.2192608490551,7.05258513100155));
#28287=CARTESIAN_POINT('Ctrl Pts',(-0.368078352856691,2.2385756694312,7.05154308883578));
#28288=CARTESIAN_POINT('Ctrl Pts',(-0.36081443865216,2.25786974599363,7.05050216580693));
#28289=CARTESIAN_POINT('Ctrl Pts',(-0.352021571301162,2.27661197620053,
7.04946124277807));
#28290=CARTESIAN_POINT('Ctrl Pts',(-0.341810773641972,2.29455149709595,
7.04842031974922));
#28291=CARTESIAN_POINT('Ctrl Pts',(-0.331594731983229,2.31250023126175,
7.04737886212943));
#28292=CARTESIAN_POINT('Ctrl Pts',(-0.31995965516463,2.32964478510415,7.04633740450964));
#28293=CARTESIAN_POINT('Ctrl Pts',(-0.307062317059976,2.34575927946216,
7.04529594688985));
#28294=CARTESIAN_POINT('Ctrl Pts',(-0.294161038256251,2.36187869750073,
7.04425417105935));
#28295=CARTESIAN_POINT('Ctrl Pts',(-0.279997217999062,2.3769668781514,7.04321239522885));
#28296=CARTESIAN_POINT('Ctrl Pts',(-0.264767017367462,2.39083211052829,
7.04217061939835));
#28297=CARTESIAN_POINT('Ctrl Pts',(-0.24950389631158,2.4047273129196,7.04112659174576));
#28298=CARTESIAN_POINT('Ctrl Pts',(-0.233170375035,2.41739383823302,7.04008256409316));
#28299=CARTESIAN_POINT('Ctrl Pts',(-0.21599512284965,2.4286806914091,7.03903853644056));
#28300=CARTESIAN_POINT('Ctrl Pts',(-0.209920461280633,2.43267270343221,
7.0386692775447));
#28301=CARTESIAN_POINT('Ctrl Pts',(-0.203740744708566,2.43649253814428,
7.03830001864883));
#28302=CARTESIAN_POINT('Ctrl Pts',(-0.197466795816991,2.44013490639711,
7.03793075975296));
#28303=CARTESIAN_POINT('Ctrl Pts',(-0.179729191202037,2.45043254972306,
7.03688679710541));
#28304=CARTESIAN_POINT('Ctrl Pts',(-0.16113105401224,2.45936964946468,7.03584283445785));
#28305=CARTESIAN_POINT('Ctrl Pts',(-0.141907118808706,2.46680684239994,
7.0347988718103));
#28306=CARTESIAN_POINT('Ctrl Pts',(-0.122718548105475,2.47423035381738,
7.03375682964453));
#28307=CARTESIAN_POINT('Ctrl Pts',(-0.102907121528119,2.48015911746761,
7.03271478747876));
#28308=CARTESIAN_POINT('Ctrl Pts',(-0.0827305591853479,2.48450038306467,
7.03167274531299));
#28309=CARTESIAN_POINT('Ctrl Pts',(-0.0625756661535695,2.48883698621068,
7.03063182228414));
#28310=CARTESIAN_POINT('Ctrl Pts',(-0.0420571254533872,2.49158929377269,
7.02959089925528));
#28311=CARTESIAN_POINT('Ctrl Pts',(-0.0214459658181039,2.49271485909006,
7.02854997622643));
#28312=CARTESIAN_POINT('Ctrl Pts',(-0.000824220828423809,2.49384100246845,
7.02750851860664));
#28313=CARTESIAN_POINT('Ctrl Pts',(0.0198895043193526,2.4933386783378,7.02646706098685));
#28314=CARTESIAN_POINT('Ctrl Pts',(0.0404204218518309,2.49121743250694,
7.02542560336705));
#28315=CARTESIAN_POINT('Ctrl Pts',(0.0609576124746873,2.48909553854299,
7.02438382753656));
#28316=CARTESIAN_POINT('Ctrl Pts',(0.0813111567395613,2.48535384968859,
7.02334205170606));
#28317=CARTESIAN_POINT('Ctrl Pts',(0.101213675164648,2.48005352512464,7.02230027587556));
#28318=CARTESIAN_POINT('Ctrl Pts',(0.12115921333496,2.47474174378886,7.02125624822296));
#28319=CARTESIAN_POINT('Ctrl Pts',(0.140651084799832,2.46786484567961,7.02021222057036));
#28320=CARTESIAN_POINT('Ctrl Pts',(0.159438547379486,2.45953336369455,7.01916819291777));
#28321=CARTESIAN_POINT('Ctrl Pts',(0.166083426632471,2.45658662772346,7.0187989340219));
#28322=CARTESIAN_POINT('Ctrl Pts',(0.17264040429098,2.45345835693534,7.01842967512604));
#28323=CARTESIAN_POINT('Ctrl Pts',(0.179099174630351,2.45015478812481,7.01806041623017));
#28324=CARTESIAN_POINT('Ctrl Pts',(0.197359303388023,2.44081499298261,7.01701645358262));
#28325=CARTESIAN_POINT('Ctrl Pts',(0.214941284571895,2.43001515981853,7.01597249093506));
#28326=CARTESIAN_POINT('Ctrl Pts',(0.231600873030352,2.41787721782408,7.01492852828751));
#28327=CARTESIAN_POINT('Ctrl Pts',(0.24822981438067,2.40576160488187,7.01388648612174));
#28328=CARTESIAN_POINT('Ctrl Pts',(0.263939108184732,2.39231314959407,7.01284444395597));
#28329=CARTESIAN_POINT('Ctrl Pts',(0.278511259789918,2.37769834023673,7.0118024017902));
#28330=CARTESIAN_POINT('Ctrl Pts',(0.293067761133201,2.36309922695504,7.01076147876135));
#28331=CARTESIAN_POINT('Ctrl Pts',(0.306489007437223,2.34733674437685,7.00972055573249));
#28332=CARTESIAN_POINT('Ctrl Pts',(0.318592596039228,2.33061580116936,7.00867963270364));
#28333=CARTESIAN_POINT('Ctrl Pts',(0.330702400728881,2.31388627052123,7.00763817508385));
#28334=CARTESIAN_POINT('Ctrl Pts',(0.341492751301786,2.29619788242215,7.00659671746406));
#28335=CARTESIAN_POINT('Ctrl Pts',(0.350822926458063,2.27778685067068,7.00555525984426));
#28336=CARTESIAN_POINT('Ctrl Pts',(0.36015595238961,2.25937019354637,7.00451348401377));
#28337=CARTESIAN_POINT('Ctrl Pts',(0.368027614683983,2.24023112532588,7.00347170818327));
#28338=CARTESIAN_POINT('Ctrl Pts',(0.374344599730752,2.22062757003448,7.00242993235277));
#28339=CARTESIAN_POINT('Ctrl Pts',(0.380675239084051,2.20098164121345,7.00138590470017));
#28340=CARTESIAN_POINT('Ctrl Pts',(0.385444322246868,2.18086993749164,7.00034187704758));
#28341=CARTESIAN_POINT('Ctrl Pts',(0.388609055986058,2.16056312083789,6.99929784939498));
#28342=CARTESIAN_POINT('Ctrl Pts',(0.389728380827061,2.1533808659642,6.99892859049911));
#28343=CARTESIAN_POINT('Ctrl Pts',(0.390647485222271,2.1461742522484,6.99855933160325));
#28344=CARTESIAN_POINT('Ctrl Pts',(0.391366034505286,2.13895532101789,6.99819007270738));
#28345=CARTESIAN_POINT('Ctrl Pts',(0.39339750516257,2.11854607795223,6.99714611005983));
#28346=CARTESIAN_POINT('Ctrl Pts',(0.393834256174918,2.09791668854596,6.99610214741227));
#28347=CARTESIAN_POINT('Ctrl Pts',(0.392646593475837,2.07733852097014,6.99505818476472));
#28348=CARTESIAN_POINT('Ctrl Pts',(0.391461115610268,2.05679820915098,6.99401614259895));
#28349=CARTESIAN_POINT('Ctrl Pts',(0.388657138203044,2.03630966180985,6.99297410043318));
#28350=CARTESIAN_POINT('Ctrl Pts',(0.384256913792191,2.01614587545684,6.99193205826741));
#28351=CARTESIAN_POINT('Ctrl Pts',(0.37986141515323,1.9960037446936,6.99089113523856));
#28352=CARTESIAN_POINT('Ctrl Pts',(0.373873200714846,1.97618640387247,6.9898502122097));
#28353=CARTESIAN_POINT('Ctrl Pts',(0.36636582349603,1.95695814118212,6.98880928918085));
#28354=CARTESIAN_POINT('Ctrl Pts',(0.358854590683942,1.9377200033572,6.98776783156106));
#28355=CARTESIAN_POINT('Ctrl Pts',(0.34982288900492,1.919072239314,6.98672637394127));
#28356=CARTESIAN_POINT('Ctrl Pts',(0.339393156267765,1.90126103683826,6.98568491632147));
#28357=CARTESIAN_POINT('Ctrl Pts',(0.328960236792561,1.88344439226366,6.98464314049098));
#28358=CARTESIAN_POINT('Ctrl Pts',(0.317128838591403,1.86646543422052,6.98360136466048));
#28359=CARTESIAN_POINT('Ctrl Pts',(0.304065316459306,1.85054224139846,6.98255958882998));
#28360=CARTESIAN_POINT('Ctrl Pts',(0.29097355722767,1.83458463023378,6.98151556117738));
#28361=CARTESIAN_POINT('Ctrl Pts',(0.276644867538597,1.81968787110294,6.98047153352479));
#28362=CARTESIAN_POINT('Ctrl Pts',(0.261283660071214,1.80603445953685,6.97942750587219));
#28363=CARTESIAN_POINT('Ctrl Pts',(0.255850602340914,1.80120542683147,6.97905824697632));
#28364=CARTESIAN_POINT('Ctrl Pts',(0.25028868031497,1.79653155718037,6.97868898808046));
#28365=CARTESIAN_POINT('Ctrl Pts',(0.2446078373961,1.79201965016514,6.97831972918459));
#28366=CARTESIAN_POINT('Ctrl Pts',(0.228547052184692,1.77926366122119,6.97727576653704));
#28367=CARTESIAN_POINT('Ctrl Pts',(0.211437913429965,1.76772937191523,6.97623180388948));
#28368=CARTESIAN_POINT('Ctrl Pts',(0.193492518414073,1.75758864604429,6.97518784124193));
#28369=CARTESIAN_POINT('Ctrl Pts',(0.175580135886038,1.74746657513132,6.97414579907616));
#28370=CARTESIAN_POINT('Ctrl Pts',(0.156835154811601,1.73873338865849,6.97310375691039));
#28371=CARTESIAN_POINT('Ctrl Pts',(0.137499161245205,1.73151815423706,6.97206171474462));
#28372=CARTESIAN_POINT('Ctrl Pts',(0.118183934232137,1.72431066886404,6.97102079171577));
#28373=CARTESIAN_POINT('Ctrl Pts',(0.0982796305767786,1.71861818211602,
6.96997986868691));
#28374=CARTESIAN_POINT('Ctrl Pts',(0.0780482840982825,1.71452191326962,
6.96893894565806));
#28375=CARTESIAN_POINT('Ctrl Pts',(0.0578065473275278,1.7104235406863,6.96789748803827));
#28376=CARTESIAN_POINT('Ctrl Pts',(0.0372381501319202,1.70792318554478,
6.96685603041847));
#28377=CARTESIAN_POINT('Ctrl Pts',(0.016616369407768,1.70705116584,6.96581457279868));
#28378=CARTESIAN_POINT('Ctrl Pts',(-0.00401171216942507,1.70617887969518,
6.96477279696818));
#28379=CARTESIAN_POINT('Ctrl Pts',(-0.0246924737159749,1.70693591435756,
6.96373102113769));
#28380=CARTESIAN_POINT('Ctrl Pts',(-0.0451524999086895,1.70930044567213,
6.96268924530719));
#28381=CARTESIAN_POINT('Ctrl Pts',(-0.0656567509123161,1.7116700879748,
6.96164521765459));
#28382=CARTESIAN_POINT('Ctrl Pts',(-0.0859385913385113,1.71565402192686,
6.960601190002));
#28383=CARTESIAN_POINT('Ctrl Pts',(-0.105733923400703,1.72117916181618,
6.9595571623494));
#28384=CARTESIAN_POINT('Ctrl Pts',(-0.112735272878758,1.72313333137286,
6.95918790345353));
#28385=CARTESIAN_POINT('Ctrl Pts',(-0.119675915054347,1.72527984490144,
6.95881864455767));
#28386=CARTESIAN_POINT('Ctrl Pts',(-0.126544750173951,1.72761402254729,
6.9584493856618));
#28387=CARTESIAN_POINT('Ctrl Pts',(-0.145964207301035,1.73421317101005,
6.95740542301425));
#28388=CARTESIAN_POINT('Ctrl Pts',(-0.164923930214275,1.7423551219909,6.9563614603667));
#28389=CARTESIAN_POINT('Ctrl Pts',(-0.183164600664807,1.75195457327627,
6.95531749771915));
#28390=CARTESIAN_POINT('Ctrl Pts',(-0.201371715436502,1.7615363653366,6.95427545555338));
#28391=CARTESIAN_POINT('Ctrl Pts',(-0.218861731941079,1.7725700494049,6.95323341338761));
#28392=CARTESIAN_POINT('Ctrl Pts',(-0.23539535292366,1.78492236223123,6.95219137122184));
#28393=CARTESIAN_POINT('Ctrl Pts',(-0.251911217057038,1.79726140886763,
6.95115044819299));
#28394=CARTESIAN_POINT('Ctrl Pts',(-0.267472121051817,1.81091585782192,
6.95010952516414));
#28395=CARTESIAN_POINT('Ctrl Pts',(-0.281867930645074,1.82570935182937,
6.94906860213528));
#28396=CARTESIAN_POINT('Ctrl Pts',(-0.296271133550944,1.84051044338978,
6.94802714451549));
#28397=CARTESIAN_POINT('Ctrl Pts',(-0.309507521970585,1.85645123259965,
6.9469856868957));
#28398=CARTESIAN_POINT('Ctrl Pts',(-0.321403674269256,1.87331835503018,
6.94594422927591));
#28399=CARTESIAN_POINT('Ctrl Pts',(-0.333303461361082,1.89019063110196,
6.94490245344542));
#28400=CARTESIAN_POINT('Ctrl Pts',(-0.343861802965516,1.90798918222806,
6.94386067761492));
#28401=CARTESIAN_POINT('Ctrl Pts',(-0.352949044568082,1.92647230209999,
6.94281890178442));
#28402=CARTESIAN_POINT('Ctrl Pts',(-0.362055928449588,1.94499537365495,
6.94177487413183));
#28403=CARTESIAN_POINT('Ctrl Pts',(-0.369685092145126,1.9642052836525,6.94073084647923));
#28404=CARTESIAN_POINT('Ctrl Pts',(-0.375755026526189,1.98384041132862,
6.93968681882663));
#28405=CARTESIAN_POINT('Ctrl Pts',(-0.377901882753596,1.99078509861535,
6.93931755993076));
#28406=CARTESIAN_POINT('Ctrl Pts',(-0.379854150765881,1.99778286138267,
6.93894830103489));
#28407=CARTESIAN_POINT('Ctrl Pts',(-0.381609756971484,2.0048218334692,6.93857904213902));
#28408=CARTESIAN_POINT('Ctrl Pts',(-0.388101192253086,2.03084875887132,
6.93721369026395));
#28409=CARTESIAN_POINT('Ctrl Pts',(-0.391931856124105,2.05756443576007,
6.93584833838888));
#28410=CARTESIAN_POINT('Ctrl Pts',(-0.392994316331167,2.08449653808342,
6.93448298651381));
#28411=CARTESIAN_POINT('Ctrl Pts',(-0.393193170304858,2.08953724975551,
6.93422744221762));
#28412=CARTESIAN_POINT('Ctrl Pts',(-0.393295183208218,2.09458547560849,
6.93397189792143));
#28413=CARTESIAN_POINT('Ctrl Pts',(-0.393299833421324,2.09963801828994,
6.93371635362524));
#28414=CARTESIAN_POINT('',(-0.393057143940665,2.10007656503152,6.80871634984815));
#28415=CARTESIAN_POINT('Ctrl Pts',(-0.393254262534486,2.09963808833903,
6.9337163522035));
#28416=CARTESIAN_POINT('Ctrl Pts',(-0.392351278880494,2.19853643597861,
6.92871380100774));
#28417=CARTESIAN_POINT('Ctrl Pts',(-0.30436299103977,2.42980898719343,6.91708780197104));
#28418=CARTESIAN_POINT('Ctrl Pts',(0.0843393264457993,2.55734221486119,
6.89883835509345));
#28419=CARTESIAN_POINT('Ctrl Pts',(0.430195924005982,2.27665358883452,6.87896801157065));
#28420=CARTESIAN_POINT('Ctrl Pts',(0.381406327177297,1.83390934426664,6.85909766804786));
#28421=CARTESIAN_POINT('Ctrl Pts',(-0.0172716510538061,1.63526705136245,
6.83922732452507));
#28422=CARTESIAN_POINT('Ctrl Pts',(-0.340830224277894,1.8277006749777,6.82243355257695));
#28423=CARTESIAN_POINT('Ctrl Pts',(-0.392544160566776,2.02969108662713,
6.81226322846976));
#28424=CARTESIAN_POINT('Ctrl Pts',(-0.392666129258272,2.10007644209519,
6.8087163522035));
#28425=CARTESIAN_POINT('',(-0.393343588509023,2.1003295827536,6.6837163522035));
#28426=CARTESIAN_POINT('Ctrl Pts',(-0.393299992532543,2.10007664138394,
6.80871634838531));
#28427=CARTESIAN_POINT('Ctrl Pts',(-0.393295695528997,2.12212754098503,
6.80760694442949));
#28428=CARTESIAN_POINT('Ctrl Pts',(-0.39143267046183,2.1441308409618,6.80649754047367));
#28429=CARTESIAN_POINT('Ctrl Pts',(-0.38776007247249,2.16578005925909,6.80538813651785));
#28430=CARTESIAN_POINT('Ctrl Pts',(-0.384068304695278,2.18754227955757,
6.80427294182791));
#28431=CARTESIAN_POINT('Ctrl Pts',(-0.378548221487941,2.20894615427118,
6.80315774713797));
#28432=CARTESIAN_POINT('Ctrl Pts',(-0.371299894246872,2.22969687171348,
6.80204255244803));
#28433=CARTESIAN_POINT('Ctrl Pts',(-0.365762413285198,2.24554972975315,
6.80119058079185));
#28434=CARTESIAN_POINT('Ctrl Pts',(-0.359217317625601,2.26102165989602,
6.80033860913567));
#28435=CARTESIAN_POINT('Ctrl Pts',(-0.351727463573401,2.27599057181628,
6.79948663747949));
#28436=CARTESIAN_POINT('Ctrl Pts',(-0.342549778131173,2.29433271360692,
6.79844267483194));
#28437=CARTESIAN_POINT('Ctrl Pts',(-0.33190610509672,2.3120096670508,6.79739871218439));
#28438=CARTESIAN_POINT('Ctrl Pts',(-0.319916205420557,2.32877611656227,
6.79635474953683));
#28439=CARTESIAN_POINT('Ctrl Pts',(-0.307948362456833,2.34551172238317,
6.79531270737106));
#28440=CARTESIAN_POINT('Ctrl Pts',(-0.294639583445627,2.36133952269403,
6.79427066520529));
#28441=CARTESIAN_POINT('Ctrl Pts',(-0.280154423622598,2.37604055666639,
6.79322862303952));
#28442=CARTESIAN_POINT('Ctrl Pts',(-0.265684820633667,2.39072580195921,
6.79218770001067));
#28443=CARTESIAN_POINT('Ctrl Pts',(-0.250041838204806,2.40428614156079,
6.79114677698182));
#28444=CARTESIAN_POINT('Ctrl Pts',(-0.233428761290965,2.41653736493843,
6.79010585395297));
#28445=CARTESIAN_POINT('Ctrl Pts',(-0.216807152333808,2.42879488022509,
6.78906439633318));
#28446=CARTESIAN_POINT('Ctrl Pts',(-0.19921503617343,2.43974148645848,6.78802293871339));
#28447=CARTESIAN_POINT('Ctrl Pts',(-0.180887370870302,2.44923437554117,
6.7869814810936));
#28448=CARTESIAN_POINT('Ctrl Pts',(-0.162554105666405,2.45873016511533,
6.7859397052631));
#28449=CARTESIAN_POINT('Ctrl Pts',(-0.143485513341916,2.46677104730492,
6.7848979294326));
#28450=CARTESIAN_POINT('Ctrl Pts',(-0.123938681256822,2.47326142753882,
6.7838561536021));
#28451=CARTESIAN_POINT('Ctrl Pts',(-0.104349598250602,2.47976583687688,
6.78281212594951));
#28452=CARTESIAN_POINT('Ctrl Pts',(-0.084280926772598,2.48471287699348,
6.78176809829691));
#28453=CARTESIAN_POINT('Ctrl Pts',(-0.064002939122556,2.48805735888355,
6.78072407064432));
#28454=CARTESIAN_POINT('Ctrl Pts',(-0.0568308806894853,2.48924025828944,
6.78035481174844));
#28455=CARTESIAN_POINT('Ctrl Pts',(-0.0496326908711968,2.49022316086833,
6.77998555285257));
#28456=CARTESIAN_POINT('Ctrl Pts',(-0.0424204075583441,2.49100562530811,
6.7796162939567));
#28457=CARTESIAN_POINT('Ctrl Pts',(-0.0220299593758823,2.49321779584022,
6.77857233130915));
#28458=CARTESIAN_POINT('Ctrl Pts',(-0.00140524789277181,2.4938372592859,
6.77752836866159));
#28459=CARTESIAN_POINT('Ctrl Pts',(0.0191826323878835,2.49283191903748,
6.77648440601404));
#28460=CARTESIAN_POINT('Ctrl Pts',(0.0397326390442958,2.49182842822079,
6.77544236384827));
#28461=CARTESIAN_POINT('Ctrl Pts',(0.0602452194858398,2.48920604284114,
6.7744003216825));
#28462=CARTESIAN_POINT('Ctrl Pts',(0.0804471908052092,2.48498459643413,
6.77335827951673));
#28463=CARTESIAN_POINT('Ctrl Pts',(0.100627465524746,2.48076768379425,6.77231735648788));
#28464=CARTESIAN_POINT('Ctrl Pts',(0.120497070890807,2.47495524093621,6.77127643345902));
#28465=CARTESIAN_POINT('Ctrl Pts',(0.139791077570064,2.467618477,6.77023551043017));
#28466=CARTESIAN_POINT('Ctrl Pts',(0.159094993148286,2.46027794509306,6.76919405281038));
#28467=CARTESIAN_POINT('Ctrl Pts',(0.177822026008554,2.45141177459615,6.76815259519059));
#28468=CARTESIAN_POINT('Ctrl Pts',(0.195724913502099,2.44114021784978,6.76711113757079));
#28469=CARTESIAN_POINT('Ctrl Pts',(0.213633271108271,2.43086552269503,6.7660693617403));
#28470=CARTESIAN_POINT('Ctrl Pts',(0.230716362393179,2.41918498367593,6.7650275859098));
#28471=CARTESIAN_POINT('Ctrl Pts',(0.24675464369661,2.40626301737911,6.7639858100793));
#28472=CARTESIAN_POINT('Ctrl Pts',(0.262827592109034,2.39331311995891,6.7629417824267));
#28473=CARTESIAN_POINT('Ctrl Pts',(0.277850686501704,2.37911694386544,6.76189775477411));
#28474=CARTESIAN_POINT('Ctrl Pts',(0.291639627870715,2.36387727726243,6.76085372712151));
#28475=CARTESIAN_POINT('Ctrl Pts',(0.296516595690895,2.35848720694273,6.76048446822564));
#28476=CARTESIAN_POINT('Ctrl Pts',(0.301239547989098,2.35296690299031,6.76011520932978));
#28477=CARTESIAN_POINT('Ctrl Pts',(0.305801597374482,2.34732624818894,6.75974595043391));
#28478=CARTESIAN_POINT('Ctrl Pts',(0.318699347998627,2.33137908215912,6.75870198778636));
#28479=CARTESIAN_POINT('Ctrl Pts',(0.330384732945562,2.31437278222749,6.7576580251388));
#28480=CARTESIAN_POINT('Ctrl Pts',(0.340684016460012,2.29651791503238,6.75661406249125));
#28481=CARTESIAN_POINT('Ctrl Pts',(0.350964353332628,2.27869589378945,6.75557202032548));
#28482=CARTESIAN_POINT('Ctrl Pts',(0.359863235185042,2.26002900429957,6.75452997815971));
#28483=CARTESIAN_POINT('Ctrl Pts',(0.367249459565265,2.24075767989357,6.75348793599394));
#28484=CARTESIAN_POINT('Ctrl Pts',(0.374627751256537,2.22150705258724,6.75244701296508));
#28485=CARTESIAN_POINT('Ctrl Pts',(0.380496321638926,2.20165395229917,6.75140608993623));
#28486=CARTESIAN_POINT('Ctrl Pts',(0.384771633597181,2.18145968315036,6.75036516690738));
#28487=CARTESIAN_POINT('Ctrl Pts',(0.389049141244229,2.16125504275124,6.74932370928758));
#28488=CARTESIAN_POINT('Ctrl Pts',(0.391731587610378,2.14070959993482,6.74828225166779));
#28489=CARTESIAN_POINT('Ctrl Pts',(0.392786235277038,2.12009635232801,6.747240794048));
#28490=CARTESIAN_POINT('Ctrl Pts',(0.393841205184539,2.09947680647539,6.7461990182175));
#28491=CARTESIAN_POINT('Ctrl Pts',(0.393267384828812,2.07879015063581,6.745157242387));
#28492=CARTESIAN_POINT('Ctrl Pts',(0.391084175669496,2.05830998271875,6.7441154665565));
#28493=CARTESIAN_POINT('Ctrl Pts',(0.388896247454038,2.03778554645398,6.74307143890391));
#28494=CARTESIAN_POINT('Ctrl Pts',(0.385092120865691,2.01746921308134,6.74202741125131));
#28495=CARTESIAN_POINT('Ctrl Pts',(0.379742539442433,1.99762571740026,6.74098338359871));
#28496=CARTESIAN_POINT('Ctrl Pts',(0.377850462614033,1.99060733308155,6.74061412470285));
#28497=CARTESIAN_POINT('Ctrl Pts',(0.375765511630558,1.98364794995271,6.74024486580698));
#28498=CARTESIAN_POINT('Ctrl Pts',(0.373492267844443,1.9767587087847,6.73987560691112));
#28499=CARTESIAN_POINT('Ctrl Pts',(0.367065390582806,1.9572815600147,6.73883164426357));
#28500=CARTESIAN_POINT('Ctrl Pts',(0.35909169912626,1.93825046169438,6.73778768161601));
#28501=CARTESIAN_POINT('Ctrl Pts',(0.349654195370835,1.91992547748342,6.73674371896846));
#28502=CARTESIAN_POINT('Ctrl Pts',(0.340234052920517,1.90163420405555,6.73570167680269));
#28503=CARTESIAN_POINT('Ctrl Pts',(0.329355723557583,1.88404714029489,6.73465963463692));
#28504=CARTESIAN_POINT('Ctrl Pts',(0.317150345673459,1.8674047544785,6.73361759247115));
#28505=CARTESIAN_POINT('Ctrl Pts',(0.304958076173439,1.85078024232304,6.7325766694423));
#28506=CARTESIAN_POINT('Ctrl Pts',(0.291441997180033,1.8350990013637,6.73153574641345));
#28507=CARTESIAN_POINT('Ctrl Pts',(0.27677659772676,1.82057271974483,6.73049482338459));
#28508=CARTESIAN_POINT('Ctrl Pts',(0.262103666506556,1.80603897780633,6.7294533657648));
#28509=CARTESIAN_POINT('Ctrl Pts',(0.24628074701975,1.792661909445,6.72841190814501));
#28510=CARTESIAN_POINT('Ctrl Pts',(0.229519659202689,1.78061681941674,6.72737045052522));
#28511=CARTESIAN_POINT('Ctrl Pts',(0.212753450142578,1.76856804908835,6.72632867469472));
#28512=CARTESIAN_POINT('Ctrl Pts',(0.195049120204018,1.75785246692723,6.72528689886422));
#28513=CARTESIAN_POINT('Ctrl Pts',(0.176647217768549,1.74860186333074,6.72424512303372));
#28514=CARTESIAN_POINT('Ctrl Pts',(0.158205539203375,1.73933126434465,6.72320109538113));
#28515=CARTESIAN_POINT('Ctrl Pts',(0.139063959893764,1.73153224374321,6.72215706772853));
#28516=CARTESIAN_POINT('Ctrl Pts',(0.119483368354343,1.72528862482345,6.72111304007593));
#28517=CARTESIAN_POINT('Ctrl Pts',(0.112557969784387,1.72308033865134,6.72074378118007));
#28518=CARTESIAN_POINT('Ctrl Pts',(0.105577774206092,1.72106616293227,6.7203745222842));
#28519=CARTESIAN_POINT('Ctrl Pts',(0.0985546289480032,1.71924827628372,
6.72000526338833));
#28520=CARTESIAN_POINT('Ctrl Pts',(0.0786989087478119,1.71410877719563,
6.71896130074078));
#28521=CARTESIAN_POINT('Ctrl Pts',(0.0583809172791021,1.71051132234542,
6.71791733809322));
#28522=CARTESIAN_POINT('Ctrl Pts',(0.03786425114929,1.70852689941082,6.71687337544567));
#28523=CARTESIAN_POINT('Ctrl Pts',(0.0173853276376203,1.70654612703605,
6.7158313332799));
#28524=CARTESIAN_POINT('Ctrl Pts',(-0.003290826700979,1.70617262574247,
6.71478929111413));
#28525=CARTESIAN_POINT('Ctrl Pts',(-0.0238910342529198,1.70742630184598,
6.71374724894836));
#28526=CARTESIAN_POINT('Ctrl Pts',(-0.0444691175055708,1.70867863152104,
6.71270632591951));
#28527=CARTESIAN_POINT('Ctrl Pts',(-0.0649706834463184,1.71155465366243,
6.71166540289066));
#28528=CARTESIAN_POINT('Ctrl Pts',(-0.0851232868265916,1.71602224538414,
6.7106244798618));
#28529=CARTESIAN_POINT('Ctrl Pts',(-0.105286240058719,1.72049213154452,
6.70958302224201));
#28530=CARTESIAN_POINT('Ctrl Pts',(-0.125099150865311,1.72655507673637,
6.70854156462222));
#28531=CARTESIAN_POINT('Ctrl Pts',(-0.144299957910001,1.73412787459664,
6.70750010700243));
#28532=CARTESIAN_POINT('Ctrl Pts',(-0.163506631638328,1.7417029862768,6.70645833117193));
#28533=CARTESIAN_POINT('Ctrl Pts',(-0.182100158667977,1.75078856563216,
6.70541655534143));
#28534=CARTESIAN_POINT('Ctrl Pts',(-0.199839514087861,1.76125369580005,
6.70437477951094));
#28535=CARTESIAN_POINT('Ctrl Pts',(-0.217617213527045,1.77174144658427,
6.70333075185834));
#28536=CARTESIAN_POINT('Ctrl Pts',(-0.234536452432076,1.78361427841506,
6.70228672420575));
#28537=CARTESIAN_POINT('Ctrl Pts',(-0.250385527007085,1.79669820662353,
6.70124269655315));
#28538=CARTESIAN_POINT('Ctrl Pts',(-0.255991136938539,1.80132582052999,
6.70087343765728));
#28539=CARTESIAN_POINT('Ctrl Pts',(-0.26146319793638,1.80610458423775,6.70050417876141));
#28540=CARTESIAN_POINT('Ctrl Pts',(-0.266793465007023,1.81102571562586,
6.70013491986554));
#28541=CARTESIAN_POINT('Ctrl Pts',(-0.281638481231432,1.82473127190113,
6.69910651843133));
#28542=CARTESIAN_POINT('Ctrl Pts',(-0.295475092709904,1.8396306599348,6.69807811699712));
#28543=CARTESIAN_POINT('Ctrl Pts',(-0.308103769275524,1.85554763785511,
6.69704971556291));
#28544=CARTESIAN_POINT('Ctrl Pts',(-0.320708900013305,1.87143493899814,
6.69602323155552));
#28545=CARTESIAN_POINT('Ctrl Pts',(-0.332110047029178,1.88833551806399,
6.69499674754813));
#28546=CARTESIAN_POINT('Ctrl Pts',(-0.342145090725859,1.90603704762972,
6.69397026354073));
#28547=CARTESIAN_POINT('Ctrl Pts',(-0.352174893520385,1.92372933239421,
6.6929443156249));
#28548=CARTESIAN_POINT('Ctrl Pts',(-0.360839597491012,1.94222110075685,
6.69191836770907));
#28549=CARTESIAN_POINT('Ctrl Pts',(-0.368020943743174,1.96127193879253,
6.69089241979324));
#28550=CARTESIAN_POINT('Ctrl Pts',(-0.375200246816398,1.98031735663683,
6.68986676377187));
#28551=CARTESIAN_POINT('Ctrl Pts',(-0.380896771828865,1.99992081446266,
6.6888411077505));
#28552=CARTESIAN_POINT('Ctrl Pts',(-0.385041122121011,2.01982379233343,
6.68781545172912));
#28553=CARTESIAN_POINT('Ctrl Pts',(-0.389191248184781,2.03975450797894,
6.68678836630277));
#28554=CARTESIAN_POINT('Ctrl Pts',(-0.391784765705901,2.05998482575166,
6.68576128087642));
#28555=CARTESIAN_POINT('Ctrl Pts',(-0.392803692771429,2.08024781163697,
6.68473419545006));
#28556=CARTESIAN_POINT('Ctrl Pts',(-0.393140278870883,2.08694136175765,
6.68439491436787));
#28557=CARTESIAN_POINT('Ctrl Pts',(-0.393305468394936,2.09363846652409,
6.68405563328569));
#28558=CARTESIAN_POINT('Ctrl Pts',(-0.393299861936612,2.10032954611508,
6.6837163522035));
#28559=CARTESIAN_POINT('',(-0.393444654250221,2.09974553930462,6.5587163522035));
#28560=CARTESIAN_POINT('Ctrl Pts',(-0.393535481127247,2.1003297435405,6.6837163522035));
#28561=CARTESIAN_POINT('Ctrl Pts',(-0.393739262162669,2.123034746097,6.68256576024992));
#28562=CARTESIAN_POINT('Ctrl Pts',(-0.38160853246158,2.27622476562375,6.67479172045541));
#28563=CARTESIAN_POINT('Ctrl Pts',(-0.180457218096371,2.52861429737727,
6.66039423281995));
#28564=CARTESIAN_POINT('Ctrl Pts',(0.262701822499401,2.48374832369023,6.64052388929717));
#28565=CARTESIAN_POINT('Ctrl Pts',(0.464867704575669,2.08684550563379,6.62065354577438));
#28566=CARTESIAN_POINT('Ctrl Pts',(0.240580753727069,1.70201014533589,6.60078320225161));
#28567=CARTESIAN_POINT('Ctrl Pts',(-0.204406286553996,1.68227629526599,
6.58091285872879));
#28568=CARTESIAN_POINT('Ctrl Pts',(-0.386101521636573,1.9387736364229,6.56689057537943));
#28569=CARTESIAN_POINT('Ctrl Pts',(-0.393852311160616,2.08446480552085,
6.559491739871));
#28570=CARTESIAN_POINT('Ctrl Pts',(-0.39373755682333,2.09974534986961,6.5587163522035));
#28571=CARTESIAN_POINT('',(-0.393095185008428,2.09980963099506,6.43371635487844));
#28572=CARTESIAN_POINT('Ctrl Pts',(-0.393299917743934,2.09974563291309,
6.5587163522035));
#28573=CARTESIAN_POINT('Ctrl Pts',(-0.393313019800725,2.12000390579344,
6.55768722808122));
#28574=CARTESIAN_POINT('Ctrl Pts',(-0.39175662785168,2.14032428942168,6.55665810395893));
#28575=CARTESIAN_POINT('Ctrl Pts',(-0.388628280275941,2.16043963740597,
6.55562897983665));
#28576=CARTESIAN_POINT('Ctrl Pts',(-0.385504851375482,2.18052335819331,
6.55460147379779));
#28577=CARTESIAN_POINT('Ctrl Pts',(-0.380814432876337,2.20040193311181,
6.55357396775894));
#28578=CARTESIAN_POINT('Ctrl Pts',(-0.374606423218514,2.21981200976293,
6.55254646172009));
#28579=CARTESIAN_POINT('Ctrl Pts',(-0.368398006858026,2.23922335801804,
6.55151888836667));
#28580=CARTESIAN_POINT('Ctrl Pts',(-0.360671990179837,2.25816541306581,
6.55049131501326));
#28581=CARTESIAN_POINT('Ctrl Pts',(-0.351528071102636,2.27638850650442,
6.54946374165984));
#28582=CARTESIAN_POINT('Ctrl Pts',(-0.342384631981106,2.29461064343008,
6.54843622224278));
#28583=CARTESIAN_POINT('Ctrl Pts',(-0.331823796686522,2.31211322546783,
6.54740870282572));
#28584=CARTESIAN_POINT('Ctrl Pts',(-0.319991410043564,2.3286709152873,6.54638118340866));
#28585=CARTESIAN_POINT('Ctrl Pts',(-0.308133033489064,2.3452649741764,6.54535140703875));
#28586=CARTESIAN_POINT('Ctrl Pts',(-0.294998004680345,2.36090940404951,
6.54432163066884));
#28587=CARTESIAN_POINT('Ctrl Pts',(-0.280773126646011,2.37541122227212,
6.54329185429893));
#28588=CARTESIAN_POINT('Ctrl Pts',(-0.271013005399951,2.38536136060015,
6.54258529342703));
#28589=CARTESIAN_POINT('Ctrl Pts',(-0.26074065664211,2.3947743075843,6.54187873255513));
#28590=CARTESIAN_POINT('Ctrl Pts',(-0.250025253535614,2.40359885143797,
6.54117217168322));
#28591=CARTESIAN_POINT('Ctrl Pts',(-0.234192957916791,2.41663735177286,
6.54012820903567));
#28592=CARTESIAN_POINT('Ctrl Pts',(-0.217290831138302,2.42847291551465,
6.53908424638812));
#28593=CARTESIAN_POINT('Ctrl Pts',(-0.19952789267338,2.4389299485813,6.53804028374056));
#28594=CARTESIAN_POINT('Ctrl Pts',(-0.181797631047831,2.44936774480881,
6.53699824157479));
#28595=CARTESIAN_POINT('Ctrl Pts',(-0.163210297763946,2.4584316238263,6.53595619940902));
#28596=CARTESIAN_POINT('Ctrl Pts',(-0.144005154564302,2.46598825863532,
6.53491415724325));
#28597=CARTESIAN_POINT('Ctrl Pts',(-0.124820637386743,2.47353677773726,
6.5338732342144));
#28598=CARTESIAN_POINT('Ctrl Pts',(-0.10502029815858,2.47958097130056,6.53283231118554));
#28599=CARTESIAN_POINT('Ctrl Pts',(-0.0848646908004932,2.48403499092574,
6.53179138815669));
#28600=CARTESIAN_POINT('Ctrl Pts',(-0.0646987320477896,2.48849129801932,
6.5307499305369));
#28601=CARTESIAN_POINT('Ctrl Pts',(-0.0441778556250099,2.49135562514288,
6.52970847291711));
#28602=CARTESIAN_POINT('Ctrl Pts',(-0.0235747584700142,2.4925928180228,
6.52866701529732));
#28603=CARTESIAN_POINT('Ctrl Pts',(-0.00296536617062622,2.49383038891907,
6.52762523946682));
#28604=CARTESIAN_POINT('Ctrl Pts',(0.0177255608677979,2.49343982789248,
6.52658346363632));
#28605=CARTESIAN_POINT('Ctrl Pts',(0.0382242636162741,2.49143811218505,
6.52554168780582));
#28606=CARTESIAN_POINT('Ctrl Pts',(0.0587672747759153,2.48943206972369,
6.52449766015323));
#28607=CARTESIAN_POINT('Ctrl Pts',(0.0791165070566686,2.48580804897436,
6.52345363250063));
#28608=CARTESIAN_POINT('Ctrl Pts',(0.0990066094176043,2.48063444575029,
6.52240960484803));
#28609=CARTESIAN_POINT('Ctrl Pts',(0.106041477908135,2.47880461010425,6.52204034595217));
#28610=CARTESIAN_POINT('Ctrl Pts',(0.113019055950688,2.47678138525304,6.5216710870563));
#28611=CARTESIAN_POINT('Ctrl Pts',(0.119928162630974,2.47456925368743,6.52130182816043));
#28612=CARTESIAN_POINT('Ctrl Pts',(0.139461474848773,2.46831515188565,6.52025786551288));
#28613=CARTESIAN_POINT('Ctrl Pts',(0.1585624553786,2.46051034557662,6.51921390286533));
#28614=CARTESIAN_POINT('Ctrl Pts',(0.176970315554775,2.45123552982642,6.51816994021777));
#28615=CARTESIAN_POINT('Ctrl Pts',(0.195344312488598,2.4419777760992,6.517127898052));
#28616=CARTESIAN_POINT('Ctrl Pts',(0.213027043608052,2.43125565496542,6.51608585588624));
#28617=CARTESIAN_POINT('Ctrl Pts',(0.229776888481254,2.41919816966874,6.51504381372047));
#28618=CARTESIAN_POINT('Ctrl Pts',(0.246508744284196,2.40715363392185,6.51400289069161));
#28619=CARTESIAN_POINT('Ctrl Pts',(0.262309091843415,2.39377698537339,6.51296196766276));
#28620=CARTESIAN_POINT('Ctrl Pts',(0.276964705742394,2.37924083113511,6.51192104463391));
#28621=CARTESIAN_POINT('Ctrl Pts',(0.291627846382698,2.36469721150688,6.51087958701412));
#28622=CARTESIAN_POINT('Ctrl Pts',(0.305144545108561,2.34899340322404,6.50983812939432));
#28623=CARTESIAN_POINT('Ctrl Pts',(0.31733762779751,2.33233966511091,6.50879667177453));
#28624=CARTESIAN_POINT('Ctrl Pts',(0.329534436004794,2.31568083855474,6.50775489594403));
#28625=CARTESIAN_POINT('Ctrl Pts',(0.340406417968111,2.29807211890184,6.50671312011354));
#28626=CARTESIAN_POINT('Ctrl Pts',(0.349819657747619,2.27975287773312,6.50567134428304));
#28627=CARTESIAN_POINT('Ctrl Pts',(0.359253244458523,2.26139403910891,6.50462731663044));
#28628=CARTESIAN_POINT('Ctrl Pts',(0.367221510047495,2.24232229235326,6.50358328897785));
#28629=CARTESIAN_POINT('Ctrl Pts',(0.373638323625835,2.22279777326188,6.50253926132525));
#28630=CARTESIAN_POINT('Ctrl Pts',(0.375907866478482,2.21589220678185,6.50217000242938));
#28631=CARTESIAN_POINT('Ctrl Pts',(0.377983791870252,2.20893012606515,6.50180074353352));
#28632=CARTESIAN_POINT('Ctrl Pts',(0.379863816328703,2.20192335867795,6.50143148463765));
#28633=CARTESIAN_POINT('Ctrl Pts',(0.385178990405976,2.18211394172355,6.5003875219901));
#28634=CARTESIAN_POINT('Ctrl Pts',(0.388956275414707,2.1618286126238,6.49934355934255));
#28635=CARTESIAN_POINT('Ctrl Pts',(0.391122351594362,2.1413303288554,6.49829959669499));
#28636=CARTESIAN_POINT('Ctrl Pts',(0.393284443043476,2.12086975388883,6.49725755452922));
#28637=CARTESIAN_POINT('Ctrl Pts',(0.393841073482857,2.10019771905904,6.49621551236345));
#28638=CARTESIAN_POINT('Ctrl Pts',(0.39276991764392,2.07958721493799,6.49517347019768));
#28639=CARTESIAN_POINT('Ctrl Pts',(0.391699912209527,2.05899884617456,6.49413254716883));
#28640=CARTESIAN_POINT('Ctrl Pts',(0.389005600237303,2.03847260949129,6.49309162413998));
#28641=CARTESIAN_POINT('Ctrl Pts',(0.38471669010653,2.01828122398447,6.49205070111112));
#28642=CARTESIAN_POINT('Ctrl Pts',(0.380425577303298,1.99807946870831,6.49100924349133));
#28643=CARTESIAN_POINT('Ctrl Pts',(0.374538367383634,1.97821363123813,6.48996778587154));
#28644=CARTESIAN_POINT('Ctrl Pts',(0.367135942177745,1.95894649964903,6.48892632825175));
#28645=CARTESIAN_POINT('Ctrl Pts',(0.359731255208238,1.93967348111127,6.48788455242125));
#28646=CARTESIAN_POINT('Ctrl Pts',(0.350810728731795,1.92100020590288,6.48684277659075));
#28647=CARTESIAN_POINT('Ctrl Pts',(0.340503139541513,1.9031688491057,6.48580100076025));
#28648=CARTESIAN_POINT('Ctrl Pts',(0.330173270263286,1.88529894942616,6.48475697310766));
#28649=CARTESIAN_POINT('Ctrl Pts',(0.318450770263997,1.86827520792864,6.48371294545506));
#28650=CARTESIAN_POINT('Ctrl Pts',(0.305507742171899,1.85231086121303,6.48266891780246));
#28651=CARTESIAN_POINT('Ctrl Pts',(0.300929962789732,1.84666448103643,6.48229965890659));
#28652=CARTESIAN_POINT('Ctrl Pts',(0.296199856595505,1.84115030571008,6.48193040001073));
#28653=CARTESIAN_POINT('Ctrl Pts',(0.291326132333721,1.83577665769377,6.48156114111486));
#28654=CARTESIAN_POINT('Ctrl Pts',(0.277547219650182,1.82058436883381,6.48051717846731));
#28655=CARTESIAN_POINT('Ctrl Pts',(0.262535664373227,1.80642754479418,6.47947321581975));
#28656=CARTESIAN_POINT('Ctrl Pts',(0.246472876546173,1.79351017777575,6.4784292531722));
#28657=CARTESIAN_POINT('Ctrl Pts',(0.230439637948193,1.78061657364587,6.47738721100643));
#28658=CARTESIAN_POINT('Ctrl Pts',(0.213359535057764,1.76895840283298,6.47634516884066));
#28659=CARTESIAN_POINT('Ctrl Pts',(0.195450018164215,1.75870221155184,6.47530312667489));
#28660=CARTESIAN_POINT('Ctrl Pts',(0.177559735810453,1.748457035259,6.47426220364604));
#28661=CARTESIAN_POINT('Ctrl Pts',(0.158842428743844,1.73961123820303,6.47322128061718));
#28662=CARTESIAN_POINT('Ctrl Pts',(0.139543485745911,1.73228746882125,6.47218035758833));
#28663=CARTESIAN_POINT('Ctrl Pts',(0.12023463131385,1.7249599381424,6.47113889996854));
#28664=CARTESIAN_POINT('Ctrl Pts',(0.100344226378691,1.71915627287421,6.47009744234875));
#28665=CARTESIAN_POINT('Ctrl Pts',(0.0801370106551709,1.71495071805903,
6.46905598472895));
#28666=CARTESIAN_POINT('Ctrl Pts',(0.0599236207462894,1.71074387826352,
6.46801420889846));
#28667=CARTESIAN_POINT('Ctrl Pts',(0.0393939544522009,1.70813623536647,
6.46697243306796));
#28668=CARTESIAN_POINT('Ctrl Pts',(0.0188213461226517,1.70715060528221,
6.46593065723746));
#28669=CARTESIAN_POINT('Ctrl Pts',(-0.00179573036665489,1.70616284473616,
6.46488662958486));
#28670=CARTESIAN_POINT('Ctrl Pts',(-0.0224551980791312,1.70680407374761,
6.46384260193227));
#28671=CARTESIAN_POINT('Ctrl Pts',(-0.0428846016013375,1.7090450141698,
6.46279857427967));
#28672=CARTESIAN_POINT('Ctrl Pts',(-0.0501102138435607,1.70983760542343,
6.4624293153838));
#28673=CARTESIAN_POINT('Ctrl Pts',(-0.057307123136383,1.71082984066219,
6.46206005648794));
#28674=CARTESIAN_POINT('Ctrl Pts',(-0.0644636176058504,1.71201890251564,
6.46169079759207));
#28675=CARTESIAN_POINT('Ctrl Pts',(-0.0846963404926527,1.71538059853578,
6.46064683494451));
#28676=CARTESIAN_POINT('Ctrl Pts',(-0.10472567772742,1.72033923833506,6.45960287229696));
#28677=CARTESIAN_POINT('Ctrl Pts',(-0.124281908480982,1.7268527137653,6.45855890964941));
#28678=CARTESIAN_POINT('Ctrl Pts',(-0.143802163440763,1.7333542069556,6.45751686748364));
#28679=CARTESIAN_POINT('Ctrl Pts',(-0.16285033050509,1.74140468476381,6.45647482531786));
#28680=CARTESIAN_POINT('Ctrl Pts',(-0.181168664863993,1.75091146556869,
6.45543278315209));
#28681=CARTESIAN_POINT('Ctrl Pts',(-0.199467325619588,1.76040803624034,
6.45439186012324));
#28682=CARTESIAN_POINT('Ctrl Pts',(-0.217037046678252,1.77135749336402,
6.45335093709438));
#28683=CARTESIAN_POINT('Ctrl Pts',(-0.233641869656607,1.78361990147393,
6.45231001406553));
#28684=CARTESIAN_POINT('Ctrl Pts',(-0.250255220439252,1.79588860723704,
6.45126855644573));
#28685=CARTESIAN_POINT('Ctrl Pts',(-0.265902081696018,1.80947118695674,
6.45022709882594));
#28686=CARTESIAN_POINT('Ctrl Pts',(-0.280376718474852,1.82418523292385,
6.44918564120615));
#28687=CARTESIAN_POINT('Ctrl Pts',(-0.294855777886267,1.83890377467348,
6.44814386537565));
#28688=CARTESIAN_POINT('Ctrl Pts',(-0.308161410034871,1.85475392144732,
6.44710208954515));
#28689=CARTESIAN_POINT('Ctrl Pts',(-0.320126470069047,1.87151819949692,
6.44606031371465));
#28690=CARTESIAN_POINT('Ctrl Pts',(-0.33211739285201,1.88831871391394,6.44501628606205));
#28691=CARTESIAN_POINT('Ctrl Pts',(-0.342761579184032,1.90603667311185,
6.44397225840945));
#28692=CARTESIAN_POINT('Ctrl Pts',(-0.35193616161686,1.92442714291101,6.44292823075685));
#28693=CARTESIAN_POINT('Ctrl Pts',(-0.355181091165119,1.93093161102109,
6.44255897186099));
#28694=CARTESIAN_POINT('Ctrl Pts',(-0.358242619051046,1.93752001607389,
6.44218971296513));
#28695=CARTESIAN_POINT('Ctrl Pts',(-0.36111677432116,1.94418098542257,6.44182045406927));
#28696=CARTESIAN_POINT('Ctrl Pts',(-0.370099885543174,1.96499970357876,
6.44066634323688));
#28697=CARTESIAN_POINT('Ctrl Pts',(-0.377294905324939,1.98663448604179,
6.43951223240448));
#28698=CARTESIAN_POINT('Ctrl Pts',(-0.382575171450579,2.00877978190357,
6.43835812157209));
#28699=CARTESIAN_POINT('Ctrl Pts',(-0.387818378277732,2.03076965205197,
6.43721211081208));
#28700=CARTESIAN_POINT('Ctrl Pts',(-0.391173400330171,2.05326247125569,
6.43606610005207));
#28701=CARTESIAN_POINT('Ctrl Pts',(-0.392563289122906,2.07593853634947,
6.43492008929206));
#28702=CARTESIAN_POINT('Ctrl Pts',(-0.393049920625344,2.08387793961947,
6.43451884500484));
#28703=CARTESIAN_POINT('Ctrl Pts',(-0.393296093584315,2.09183965120009,
6.43411760071762));
#28704=CARTESIAN_POINT('Ctrl Pts',(-0.393299953864913,2.09980950103034,
6.4337163564304));
#28705=CARTESIAN_POINT('',(-0.39324503037053,2.10033752756207,6.30871634932427));
#28706=CARTESIAN_POINT('Ctrl Pts',(-0.392742250083973,2.0998098549993,6.4337163522035));
#28707=CARTESIAN_POINT('Ctrl Pts',(-0.392403036532226,2.17760321604289,
6.42979427165116));
#28708=CARTESIAN_POINT('Ctrl Pts',(-0.332346957112888,2.38725364339046,
6.41924874325792));
#28709=CARTESIAN_POINT('Ctrl Pts',(0.0090363055646272,2.56496598656384,
6.40207976702369));
#28710=CARTESIAN_POINT('Ctrl Pts',(0.395843241910259,2.34409660242095,6.38220942350092));
#28711=CARTESIAN_POINT('Ctrl Pts',(0.419517892994406,1.89930181630866,6.36233907997812));
#28712=CARTESIAN_POINT('Ctrl Pts',(0.0583419894601582,1.63862029114263,
6.34246873645533));
#28713=CARTESIAN_POINT('Ctrl Pts',(-0.314695852507185,1.78486050374472,
6.32459449386379));
#28714=CARTESIAN_POINT('Ctrl Pts',(-0.392294735639502,2.00873010655664,
6.31334369911318));
#28715=CARTESIAN_POINT('Ctrl Pts',(-0.393040371861386,2.10033729489334,
6.3087163522035));
#28716=CARTESIAN_POINT('',(-0.393299999150334,2.10002585241028,6.18371635220694));
#28717=CARTESIAN_POINT('Ctrl Pts',(-0.393299855114474,2.10033758989031,
6.30871634855296));
#28718=CARTESIAN_POINT('Ctrl Pts',(-0.393278402612745,2.12533023944529,
6.30745471991717));
#28719=CARTESIAN_POINT('Ctrl Pts',(-0.39087066562027,2.15021782623328,6.30619309128138));
#28720=CARTESIAN_POINT('Ctrl Pts',(-0.386159708715007,2.17460274368373,
6.30493146264559));
#28721=CARTESIAN_POINT('Ctrl Pts',(-0.383417172994628,2.18879869335834,
6.30419699156698));
#28722=CARTESIAN_POINT('Ctrl Pts',(-0.379894970891419,2.20282469293395,
6.30346252048836));
#28723=CARTESIAN_POINT('Ctrl Pts',(-0.375616850480374,2.21660562437209,
6.30272804940975));
#28724=CARTESIAN_POINT('Ctrl Pts',(-0.369536014841058,2.23619356743597,
6.3016840867622));
#28725=CARTESIAN_POINT('Ctrl Pts',(-0.361900706051859,2.25536293149472,
6.30064012411464));
#28726=CARTESIAN_POINT('Ctrl Pts',(-0.352789306017484,2.27385222333839,
6.29959616146709));
#28727=CARTESIAN_POINT('Ctrl Pts',(-0.343694667385279,2.29230750213739,
6.29855411930131));
#28728=CARTESIAN_POINT('Ctrl Pts',(-0.333129595748178,2.31008451321221,
6.29751207713554));
#28729=CARTESIAN_POINT('Ctrl Pts',(-0.321220949080374,2.32694050293393,
6.29647003496977));
#28730=CARTESIAN_POINT('Ctrl Pts',(-0.309325092112015,2.34377838958748,
6.29542911194092));
#28731=CARTESIAN_POINT('Ctrl Pts',(-0.296088923552708,2.3596966040367,6.29438818891206));
#28732=CARTESIAN_POINT('Ctrl Pts',(-0.281683155049516,2.37448040032277,
6.29334726588321));
#28733=CARTESIAN_POINT('Ctrl Pts',(-0.267269988119078,2.38927178918131,
6.29230580826341));
#28734=CARTESIAN_POINT('Ctrl Pts',(-0.251686523175508,2.40292705773903,
6.29126435064362));
#28735=CARTESIAN_POINT('Ctrl Pts',(-0.235141441433974,2.41526717640813,
6.29022289302383));
#28736=CARTESIAN_POINT('Ctrl Pts',(-0.218591304448665,2.42761106552146,
6.28918111719333));
#28737=CARTESIAN_POINT('Ctrl Pts',(-0.201079576677824,2.43863859426122,
6.28813934136283));
#28738=CARTESIAN_POINT('Ctrl Pts',(-0.182844434120438,2.44821373165224,
6.28709756553233));
#28739=CARTESIAN_POINT('Ctrl Pts',(-0.164569875888608,2.45780956592002,
6.28605353787973));
#28740=CARTESIAN_POINT('Ctrl Pts',(-0.145569458073787,2.46594645129903,
6.28500951022713));
#28741=CARTESIAN_POINT('Ctrl Pts',(-0.126102543342242,2.47253595606682,
6.28396548257454));
#28742=CARTESIAN_POINT('Ctrl Pts',(-0.119217350769364,2.47486657752953,
6.28359622367868));
#28743=CARTESIAN_POINT('Ctrl Pts',(-0.112273931165657,2.47700408971494,
6.28322696478282));
#28744=CARTESIAN_POINT('Ctrl Pts',(-0.105284091406899,2.4789461044748,6.28285770588696));
#28745=CARTESIAN_POINT('Ctrl Pts',(-0.0855225319634753,2.48443653650778,
6.28181374323941));
#28746=CARTESIAN_POINT('Ctrl Pts',(-0.0652714568383826,2.48839335530575,
6.28076978059186));
#28747=CARTESIAN_POINT('Ctrl Pts',(-0.0447931637457112,2.49074091477813,
6.2797258179443));
#28748=CARTESIAN_POINT('Ctrl Pts',(-0.0243525426798438,2.49308415566189,
6.27868377577853));
#28749=CARTESIAN_POINT('Ctrl Pts',(-0.00368624930583731,2.49382387157334,
6.27764173361276));
#28750=CARTESIAN_POINT('Ctrl Pts',(0.0169329342651354,2.49293532004284,
6.27659969144699));
#28751=CARTESIAN_POINT('Ctrl Pts',(0.0375299731568701,2.49204772280274,
6.27555876841814));
#28752=CARTESIAN_POINT('Ctrl Pts',(0.0580792700751206,2.48953533239789,
6.27451784538928));
#28753=CARTESIAN_POINT('Ctrl Pts',(0.0783078534736942,2.48542544036991,
6.27347692236043));
#28754=CARTESIAN_POINT('Ctrl Pts',(0.0985468257454806,2.48131343760851,
6.27243546474064));
#28755=CARTESIAN_POINT('Ctrl Pts',(0.118464031187259,2.47560242487698,6.27139400712085));
#28756=CARTESIAN_POINT('Ctrl Pts',(0.137795975603788,2.4683709531266,6.27035254950106));
#28757=CARTESIAN_POINT('Ctrl Pts',(0.157133826772139,2.46113727184634,6.26931077367056));
#28758=CARTESIAN_POINT('Ctrl Pts',(0.175885385036822,2.45238249816158,6.26826899784006));
#28759=CARTESIAN_POINT('Ctrl Pts',(0.193807344146551,2.44223325869188,6.26722722200956));
#28760=CARTESIAN_POINT('Ctrl Pts',(0.211768041977596,2.43206208141075,6.26618319435697));
#28761=CARTESIAN_POINT('Ctrl Pts',(0.228894950369111,2.42049083300115,6.26513916670437));
#28762=CARTESIAN_POINT('Ctrl Pts',(0.244973316647901,2.40768972054738,6.26409513905177));
#28763=CARTESIAN_POINT('Ctrl Pts',(0.250660024049458,2.4031621348663,6.26372588015591));
#28764=CARTESIAN_POINT('Ctrl Pts',(0.256215881057035,2.39848105731411,6.26335662126004));
#28765=CARTESIAN_POINT('Ctrl Pts',(0.261632488397629,2.39365512257556,6.26298736236417));
#28766=CARTESIAN_POINT('Ctrl Pts',(0.276946231149214,2.38001131964224,6.26194339971662));
#28767=CARTESIAN_POINT('Ctrl Pts',(0.291235468117868,2.36512575060456,6.26089943706907));
#28768=CARTESIAN_POINT('Ctrl Pts',(0.304294608224188,2.34917801148113,6.25985547442151));
#28769=CARTESIAN_POINT('Ctrl Pts',(0.31732972463508,2.33325960994227,6.25881343225574));
#28770=CARTESIAN_POINT('Ctrl Pts',(0.329138729037153,2.31628344204484,6.25777139008998));
#28771=CARTESIAN_POINT('Ctrl Pts',(0.339553155633321,2.29846547432602,6.25672934792421));
#28772=CARTESIAN_POINT('Ctrl Pts',(0.349956397298931,2.28066664282463,6.25568842489535));
#28773=CARTESIAN_POINT('Ctrl Pts',(0.358967640187817,2.2620284237311,6.2546475018665));
#28774=CARTESIAN_POINT('Ctrl Pts',(0.366462067086566,2.24279510981347,6.25360657883765));
#28775=CARTESIAN_POINT('Ctrl Pts',(0.37396034292764,2.2235519181671,6.25256512121786));
#28776=CARTESIAN_POINT('Ctrl Pts',(0.379939964357503,2.20371370084333,6.25152366359807));
#28777=CARTESIAN_POINT('Ctrl Pts',(0.384324344253478,2.18354452952847,6.25048220597828));
#28778=CARTESIAN_POINT('Ctrl Pts',(0.388710063768655,2.16336919565248,6.24944043014778));
#28779=CARTESIAN_POINT('Ctrl Pts',(0.391499450613506,2.14286343254415,6.24839865431728));
#28780=CARTESIAN_POINT('Ctrl Pts',(0.392667268646851,2.12230036173298,6.24735687848678));
#28781=CARTESIAN_POINT('Ctrl Pts',(0.393837610945376,2.10169284337762,6.24631285083419));
#28782=CARTESIAN_POINT('Ctrl Pts',(0.393379403082437,2.08102850631199,6.24526882318159));
#28783=CARTESIAN_POINT('Ctrl Pts',(0.391319508719631,2.06058005459889,6.24422479552899));
#28784=CARTESIAN_POINT('Ctrl Pts',(0.390590951084092,2.05334770526121,6.24385553663313));
#28785=CARTESIAN_POINT('Ctrl Pts',(0.389662503052564,2.04614228935432,6.24348627773726));
#28786=CARTESIAN_POINT('Ctrl Pts',(0.388536878144342,2.03897554324823,6.24311701884139));
#28787=CARTESIAN_POINT('Ctrl Pts',(0.385354530007331,2.01871383710388,6.24207305619384));
#28788=CARTESIAN_POINT('Ctrl Pts',(0.38057349920476,1.99864136333538,6.24102909354628));
#28789=CARTESIAN_POINT('Ctrl Pts',(0.374233503118566,1.97902820517325,6.23998513089873));
#28790=CARTESIAN_POINT('Ctrl Pts',(0.367905170138346,1.95945112752899,6.23894308873296));
#28791=CARTESIAN_POINT('Ctrl Pts',(0.360023731680361,1.940332398772,6.23790104656719));
#28792=CARTESIAN_POINT('Ctrl Pts',(0.350679582695893,1.9219305745496,6.23685900440142));
#28793=CARTESIAN_POINT('Ctrl Pts',(0.341345469180641,1.90354851359733,6.23581808137257));
#28794=CARTESIAN_POINT('Ctrl Pts',(0.330552069459546,1.88588249446903,6.23477715834371));
#28795=CARTESIAN_POINT('Ctrl Pts',(0.318437223452953,1.86916970580192,6.23373623531486));
#28796=CARTESIAN_POINT('Ctrl Pts',(0.306316155577203,1.85244833388214,6.23269477769507));
#28797=CARTESIAN_POINT('Ctrl Pts',(0.292872704385196,1.83668177563127,6.23165332007528));
#28798=CARTESIAN_POINT('Ctrl Pts',(0.278287448085478,1.82207737364858,6.23061186245548));
#28799=CARTESIAN_POINT('Ctrl Pts',(0.263697735354096,1.80746850938438,6.22957008662498));
#28800=CARTESIAN_POINT('Ctrl Pts',(0.247966068089686,1.79402300289681,6.22852831079448));
#28801=CARTESIAN_POINT('Ctrl Pts',(0.231308430985115,1.78190991880412,6.22748653496399));
#28802=CARTESIAN_POINT('Ctrl Pts',(0.214614788019932,1.76977065200527,6.22644250731139));
#28803=CARTESIAN_POINT('Ctrl Pts',(0.19699180723741,1.75896994234586,6.22539847965879));
#28804=CARTESIAN_POINT('Ctrl Pts',(0.178683324881579,1.74963282201487,6.22435445200619));
#28805=CARTESIAN_POINT('Ctrl Pts',(0.172207854655414,1.74633040494248,6.22398519311033));
#28806=CARTESIAN_POINT('Ctrl Pts',(0.165646826256953,1.7432106388467,6.22361593421446));
#28807=CARTESIAN_POINT('Ctrl Pts',(0.159011576713248,1.74027759526106,6.2232466753186));
#28808=CARTESIAN_POINT('Ctrl Pts',(0.140252508865768,1.73198534291091,6.22220271267104));
#28809=CARTESIAN_POINT('Ctrl Pts',(0.120787155174758,1.72513972647364,6.22115875002349));
#28810=CARTESIAN_POINT('Ctrl Pts',(0.100864106192603,1.7198535517962,6.22011478737594));
#28811=CARTESIAN_POINT('Ctrl Pts',(0.0809777078058816,1.71457710160669,
6.21907274521017));
#28812=CARTESIAN_POINT('Ctrl Pts',(0.0606359733120824,1.71085464284479,
6.2180307030444));
#28813=CARTESIAN_POINT('Ctrl Pts',(0.0401052333492136,1.70875013066072,
6.21698866087863));
#28814=CARTESIAN_POINT('Ctrl Pts',(0.0195965430785354,1.70664787868967,
6.21594773784977));
#28815=CARTESIAN_POINT('Ctrl Pts',(-0.00110002439711979,1.70616022706547,
6.21490681482092));
#28816=CARTESIAN_POINT('Ctrl Pts',(-0.0217104213853552,1.70729967201023,
6.21386589179207));
#28817=CARTESIAN_POINT('Ctrl Pts',(-0.0423314033363119,1.70843970214422,
6.21282443417228));
#28818=CARTESIAN_POINT('Ctrl Pts',(-0.0628653908421377,1.71120847373835,
6.21178297655248));
#28819=CARTESIAN_POINT('Ctrl Pts',(-0.0830402962858998,1.71556639169715,
6.21074151893269));
#28820=CARTESIAN_POINT('Ctrl Pts',(-0.103221366042826,1.71992564118988,
6.20969974310219));
#28821=CARTESIAN_POINT('Ctrl Pts',(-0.123042424374501,1.72587481308499,
6.2086579672717));
#28822=CARTESIAN_POINT('Ctrl Pts',(-0.142244402306054,1.73332382131833,
6.2076161914412));
#28823=CARTESIAN_POINT('Ctrl Pts',(-0.161487885748656,1.740788930752,6.2065721637886));
#28824=CARTESIAN_POINT('Ctrl Pts',(-0.180108953734982,1.74976002922748,
6.205528136136));
#28825=CARTESIAN_POINT('Ctrl Pts',(-0.197870483997161,1.76009977704813,
6.20448410848341));
#28826=CARTESIAN_POINT('Ctrl Pts',(-0.204152504437129,1.76375681032143,
6.20411484958754));
#28827=CARTESIAN_POINT('Ctrl Pts',(-0.210327262850315,1.76758465471179,
6.20374559069167));
#28828=CARTESIAN_POINT('Ctrl Pts',(-0.216385198880832,1.77157598183857,
6.20337633179581));
#28829=CARTESIAN_POINT('Ctrl Pts',(-0.2334803086943,1.78283925289159,6.2023343066997));
#28830=CARTESIAN_POINT('Ctrl Pts',(-0.249745511449496,1.79547506393309,
6.20129228160359));
#28831=CARTESIAN_POINT('Ctrl Pts',(-0.264951878099973,1.80933629003383,
6.20025025650748));
#28832=CARTESIAN_POINT('Ctrl Pts',(-0.280130271322575,1.82317201720919,
6.19921014830674));
#28833=CARTESIAN_POINT('Ctrl Pts',(-0.294253114086703,1.83822823763965,
6.198170040106));
#28834=CARTESIAN_POINT('Ctrl Pts',(-0.307122888588786,1.85431642035968,
6.19712993190526));
#28835=CARTESIAN_POINT('Ctrl Pts',(-0.319978940282616,1.87038744854088,
6.19609093275313));
#28836=CARTESIAN_POINT('Ctrl Pts',(-0.331584094239873,1.88748769870106,
6.19505193360099));
#28837=CARTESIAN_POINT('Ctrl Pts',(-0.341779899852588,1.90539427023658,
6.19401293444885));
#28838=CARTESIAN_POINT('Ctrl Pts',(-0.351980988928091,1.923310120951,6.19297339688773));
#28839=CARTESIAN_POINT('Ctrl Pts',(-0.360770892043115,1.9420324931187,6.19193385932661));
#28840=CARTESIAN_POINT('Ctrl Pts',(-0.368036025297585,1.96131195407262,
6.19089432176548));
#28841=CARTESIAN_POINT('Ctrl Pts',(-0.375303531796892,1.9805977128988,6.18985444462667));
#28842=CARTESIAN_POINT('Ctrl Pts',(-0.381045052205479,2.00044021872025,
6.18881456748786));
#28843=CARTESIAN_POINT('Ctrl Pts',(-0.385196512858386,2.02057370409153,
6.18777469034905));
#28844=CARTESIAN_POINT('Ctrl Pts',(-0.389356845623493,2.04075021685875,
6.18673259088238));
#28845=CARTESIAN_POINT('Ctrl Pts',(-0.391920246540558,2.06121821665557,
6.18569049141572));
#28846=CARTESIAN_POINT('Ctrl Pts',(-0.392874256139133,2.0817049497644,6.18464839194905));
#28847=CARTESIAN_POINT('Ctrl Pts',(-0.39315867392223,2.08781263591602,6.18433771203501));
#28848=CARTESIAN_POINT('Ctrl Pts',(-0.393300400369471,2.09392199268277,
6.18402703212098));
#28849=CARTESIAN_POINT('Ctrl Pts',(-0.393299999150334,2.10002585241028,
6.18371635220694));
#28850=CARTESIAN_POINT('',(-0.393299842784111,2.09964833823957,6.05871635220607));
#28851=CARTESIAN_POINT('Ctrl Pts',(-0.39329999915033,2.10002585247783,6.1837163522035));
#28852=CARTESIAN_POINT('Ctrl Pts',(-0.393299908593832,2.10140351038807,
6.18364623089334));
#28853=CARTESIAN_POINT('Ctrl Pts',(-0.393292579542064,2.10278114062278,
6.18357610958318));
#28854=CARTESIAN_POINT('Ctrl Pts',(-0.393278012686526,2.10415869418649,
6.18350598827302));
#28855=CARTESIAN_POINT('Ctrl Pts',(-0.393061142051354,2.12466764449294,
6.18246202562547));
#28856=CARTESIAN_POINT('Ctrl Pts',(-0.39123503229439,2.14522069248777,6.18141806297791));
#28857=CARTESIAN_POINT('Ctrl Pts',(-0.3877999002043,2.16554485030523,6.18037410033036));
#28858=CARTESIAN_POINT('Ctrl Pts',(-0.384371087409844,2.18583161964435,
6.17933205816459));
#28859=CARTESIAN_POINT('Ctrl Pts',(-0.379339190301892,2.20588960740347,
6.17829001599882));
#28860=CARTESIAN_POINT('Ctrl Pts',(-0.372756237950457,2.22544989864094,
6.17724797383305));
#28861=CARTESIAN_POINT('Ctrl Pts',(-0.366180355586435,2.2449891824329,6.17620705080419));
#28862=CARTESIAN_POINT('Ctrl Pts',(-0.358056931096819,2.26403112781519,
6.17516612777534));
#28863=CARTESIAN_POINT('Ctrl Pts',(-0.348488031076856,2.28232109641009,
6.17412520474649));
#28864=CARTESIAN_POINT('Ctrl Pts',(-0.338914216719235,2.30062045825617,
6.17308374712669));
#28865=CARTESIAN_POINT('Ctrl Pts',(-0.32789377056395,2.31816641236441,6.1720422895069));
#28866=CARTESIAN_POINT('Ctrl Pts',(-0.315575366552483,2.33472766778815,
6.17100083188711));
#28867=CARTESIAN_POINT('Ctrl Pts',(-0.303253198731549,2.35129398339745,
6.16995905605661));
#28868=CARTESIAN_POINT('Ctrl Pts',(-0.289632751336844,2.36687443308267,
6.16891728022611));
#28869=CARTESIAN_POINT('Ctrl Pts',(-0.274903271170681,2.38127047747615,
6.16787550439561));
#28870=CARTESIAN_POINT('Ctrl Pts',(-0.260141952898891,2.39569763924626,
6.16683147674301));
#28871=CARTESIAN_POINT('Ctrl Pts',(-0.244267381595321,2.40893481291498,
6.16578744909042));
#28872=CARTESIAN_POINT('Ctrl Pts',(-0.227502734208435,2.42082299781606,
6.16474342143782));
#28873=CARTESIAN_POINT('Ctrl Pts',(-0.221573298174556,2.42502769298818,
6.16437416254195));
#28874=CARTESIAN_POINT('Ctrl Pts',(-0.215532773868685,2.42906404037763,
6.16400490364609));
#28875=CARTESIAN_POINT('Ctrl Pts',(-0.209391789819131,2.43292637077339,
6.16363564475022));
#28876=CARTESIAN_POINT('Ctrl Pts',(-0.192030101207922,2.4438458874345,6.16259168210267));
#28877=CARTESIAN_POINT('Ctrl Pts',(-0.173760224257052,2.45343619790509,
6.16154771945511));
#28878=CARTESIAN_POINT('Ctrl Pts',(-0.154811809403332,2.46154971120064,
6.16050375680756));
#28879=CARTESIAN_POINT('Ctrl Pts',(-0.13589825220054,2.46964829881421,6.15946171464179));
#28880=CARTESIAN_POINT('Ctrl Pts',(-0.116309280141604,2.47627514083168,
6.15841967247602));
#28881=CARTESIAN_POINT('Ctrl Pts',(-0.0962991659999387,2.48132841570976,
6.15737763031025));
#28882=CARTESIAN_POINT('Ctrl Pts',(-0.0763105424065161,2.48637626345001,
6.1563367072814));
#28883=CARTESIAN_POINT('Ctrl Pts',(-0.0559023773375834,2.48985369179578,
6.15529578425255));
#28884=CARTESIAN_POINT('Ctrl Pts',(-0.0353440257925067,2.49170867981292,
6.15425486122369));
#28885=CARTESIAN_POINT('Ctrl Pts',(-0.0147751160138901,2.49356462050355,
6.1532134036039));
#28886=CARTESIAN_POINT('Ctrl Pts',(0.00594340298049596,2.49379637405595,
6.15217194598411));
#28887=CARTESIAN_POINT('Ctrl Pts',(0.0265365777307039,2.49240374621344,
6.15113048836432));
#28888=CARTESIAN_POINT('Ctrl Pts',(0.0471360445935823,2.49101069286241,
6.15008871253382));
#28889=CARTESIAN_POINT('Ctrl Pts',(0.0676093599278807,2.4879923557627,6.14904693670333));
#28890=CARTESIAN_POINT('Ctrl Pts',(0.087687145564979,2.48340038406693,6.14800516087283));
#28891=CARTESIAN_POINT('Ctrl Pts',(0.107808329791356,2.47879848672013,6.14696113322023));
#28892=CARTESIAN_POINT('Ctrl Pts',(0.12753157469738,2.4726163842311,6.14591710556764));
#28893=CARTESIAN_POINT('Ctrl Pts',(0.146602379961316,2.46495565784034,6.14487307791504));
#28894=CARTESIAN_POINT('Ctrl Pts',(0.153347473807763,2.46224615933084,6.14450381901917));
#28895=CARTESIAN_POINT('Ctrl Pts',(0.160011151913248,2.45935212611668,6.14413456012331));
#28896=CARTESIAN_POINT('Ctrl Pts',(0.166582894089214,2.45627942600838,6.14376530122744));
#28897=CARTESIAN_POINT('Ctrl Pts',(0.185162414956153,2.44759233904554,6.14272133857989));
#28898=CARTESIAN_POINT('Ctrl Pts',(0.20311593421766,2.437422107738,6.14167737593233));
#28899=CARTESIAN_POINT('Ctrl Pts',(0.220195040800469,2.42588193261806,6.14063341328478));
#28900=CARTESIAN_POINT('Ctrl Pts',(0.237242728526341,2.41436298689377,6.13959137111901));
#28901=CARTESIAN_POINT('Ctrl Pts',(0.253418560469922,2.40147945778163,6.13854932895324));
#28902=CARTESIAN_POINT('Ctrl Pts',(0.268499280807892,2.38739002454094,6.13750728678747));
#28903=CARTESIAN_POINT('Ctrl Pts',(0.283563804689129,2.37331572313022,6.13646636375861));
#28904=CARTESIAN_POINT('Ctrl Pts',(0.297534997207425,2.35803856734134,6.13542544072976));
#28905=CARTESIAN_POINT('Ctrl Pts',(0.310223311501841,2.3417568758088,6.13438451770091));
#28906=CARTESIAN_POINT('Ctrl Pts',(0.322918142183783,2.32546682242384,6.13334306008111));
#28907=CARTESIAN_POINT('Ctrl Pts',(0.334328313411587,2.30817177308647,6.13230160246132));
#28908=CARTESIAN_POINT('Ctrl Pts',(0.344304824574808,2.29010280843404,6.13126014484153));
#28909=CARTESIAN_POINT('Ctrl Pts',(0.354284383997128,2.27202832292518,6.13021836901103));
#28910=CARTESIAN_POINT('Ctrl Pts',(0.362829087642008,2.25318011242003,6.12917659318053));
#28911=CARTESIAN_POINT('Ctrl Pts',(0.369836543771707,2.23381263352538,6.12813481735003));
#28912=CARTESIAN_POINT('Ctrl Pts',(0.376859146676849,2.2144032913856,6.12709078969743));
#28913=CARTESIAN_POINT('Ctrl Pts',(0.382337673061383,2.19447315015525,6.12604676204484));
#28914=CARTESIAN_POINT('Ctrl Pts',(0.386219768628404,2.17429118602245,6.12500273439224));
#28915=CARTESIAN_POINT('Ctrl Pts',(0.387592814944907,2.16715308984889,6.12463347549637));
#28916=CARTESIAN_POINT('Ctrl Pts',(0.388766629366076,2.15998355751807,6.12426421660051));
#28917=CARTESIAN_POINT('Ctrl Pts',(0.38974045088391,2.15279461094474,6.12389495770464));
#28918=CARTESIAN_POINT('Ctrl Pts',(0.392493622984526,2.13247014000626,6.12285099505709));
#28919=CARTESIAN_POINT('Ctrl Pts',(0.393660874785178,2.11186916959329,6.12180703240953));
#28920=CARTESIAN_POINT('Ctrl Pts',(0.393202917917753,2.09126184567742,6.12076306976198));
#28921=CARTESIAN_POINT('Ctrl Pts',(0.392745803511332,2.07069243115447,6.11972102759621));
#28922=CARTESIAN_POINT('Ctrl Pts',(0.390669371671991,2.050117414939,6.11867898543044));
#28923=CARTESIAN_POINT('Ctrl Pts',(0.386986190350865,2.02981041047474,6.11763694326467));
#28924=CARTESIAN_POINT('Ctrl Pts',(0.383306964708616,2.00952521541426,6.11659602023582));
#28925=CARTESIAN_POINT('Ctrl Pts',(0.378024517546849,1.98950818613007,6.11555509720697));
#28926=CARTESIAN_POINT('Ctrl Pts',(0.371202993583489,1.97002605047681,6.11451417417811));
#28927=CARTESIAN_POINT('Ctrl Pts',(0.364377966263212,1.95053390930645,6.11347271655832));
#28928=CARTESIAN_POINT('Ctrl Pts',(0.35601251097747,1.93157791033799,6.11243125893853));
#28929=CARTESIAN_POINT('Ctrl Pts',(0.346220267740802,1.91340842407684,6.11138980131874));
#28930=CARTESIAN_POINT('Ctrl Pts',(0.336425032546919,1.89523338624552,6.11034802548825));
#28931=CARTESIAN_POINT('Ctrl Pts',(0.325202522164563,1.87784596952126,6.10930624965775));
#28932=CARTESIAN_POINT('Ctrl Pts',(0.312711261766873,1.86147000866941,6.10826447382725));
#28933=CARTESIAN_POINT('Ctrl Pts',(0.300193001226371,1.84505865080657,6.10722044617466));
#28934=CARTESIAN_POINT('Ctrl Pts',(0.286401006965626,1.82966366217002,6.10617641852206));
#28935=CARTESIAN_POINT('Ctrl Pts',(0.271533098652582,1.81547466486071,6.10513239086946));
#28936=CARTESIAN_POINT('Ctrl Pts',(0.266274514367124,1.81045620249827,6.1047631319736));
#28937=CARTESIAN_POINT('Ctrl Pts',(0.260881650172954,1.80558824092061,6.10439387307773));
#28938=CARTESIAN_POINT('Ctrl Pts',(0.255364202363869,1.80087792767657,6.10402461418186));
#28939=CARTESIAN_POINT('Ctrl Pts',(0.239765365106384,1.78756100792163,6.10298065153431));
#28940=CARTESIAN_POINT('Ctrl Pts',(0.223075554826068,1.77542788418826,6.10193668888676));
#28941=CARTESIAN_POINT('Ctrl Pts',(0.205500647589076,1.76465782573546,6.1008927262392));
#28942=CARTESIAN_POINT('Ctrl Pts',(0.187958071287748,1.75390757996572,6.09985068407343));
#28943=CARTESIAN_POINT('Ctrl Pts',(0.169534219197412,1.74451585298908,6.09880864190766));
#28944=CARTESIAN_POINT('Ctrl Pts',(0.150465953659464,1.73662018934819,6.09776659974189));
#28945=CARTESIAN_POINT('Ctrl Pts',(0.131418167139149,1.728733005526,6.09672567671304));
#28946=CARTESIAN_POINT('Ctrl Pts',(0.111728006427996,1.72233900204228,6.09568475368418));
#28947=CARTESIAN_POINT('Ctrl Pts',(0.0916544637766103,1.7175286294769,6.09464383065533));
#28948=CARTESIAN_POINT('Ctrl Pts',(0.0715706118769009,1.71271578642953,
6.09360237303554));
#28949=CARTESIAN_POINT('Ctrl Pts',(0.0511036964483818,1.70948838625732,
6.09256091541575));
#28950=CARTESIAN_POINT('Ctrl Pts',(0.030525748887928,1.70788640847985,6.09151945779596));
#28951=CARTESIAN_POINT('Ctrl Pts',(0.00994151386737211,1.70628394122833,
6.09047768196546));
#28952=CARTESIAN_POINT('Ctrl Pts',(-0.0107530850732378,1.70630790604642,
6.08943590613496));
#28953=CARTESIAN_POINT('Ctrl Pts',(-0.0312840311149845,1.70794617793319,
6.08839413030446));
#28954=CARTESIAN_POINT('Ctrl Pts',(-0.051859355262508,1.70958799098181,
6.08735010265186));
#28955=CARTESIAN_POINT('Ctrl Pts',(-0.0722695930447734,1.71285096117465,
6.08630607499927));
#28956=CARTESIAN_POINT('Ctrl Pts',(-0.0922482234436121,1.71767140406256,
6.08526204734667));
#28957=CARTESIAN_POINT('Ctrl Pts',(-0.0993144031407224,1.71937633152683,
6.0848927884508));
#28958=CARTESIAN_POINT('Ctrl Pts',(-0.106326727224237,1.72127563273673,
6.08452352955494));
#28959=CARTESIAN_POINT('Ctrl Pts',(-0.11327393712809,1.72336502397215,6.08415427065907));
#28960=CARTESIAN_POINT('Ctrl Pts',(-0.13291497414987,1.729272116341,6.08311030801152));
#28961=CARTESIAN_POINT('Ctrl Pts',(-0.152151217691466,1.73673732853695,
6.08206634536396));
#28962=CARTESIAN_POINT('Ctrl Pts',(-0.170720490515658,1.7456845979666,6.08102238271641));
#28963=CARTESIAN_POINT('Ctrl Pts',(-0.189255603161535,1.75461540793,6.07998034055064));
#28964=CARTESIAN_POINT('Ctrl Pts',(-0.207125499390956,1.76502260112509,
6.07893829838487));
#28965=CARTESIAN_POINT('Ctrl Pts',(-0.224086311424601,1.77678147480054,
6.0778962562191));
#28966=CARTESIAN_POINT('Ctrl Pts',(-0.241028907812571,1.78852771963039,
6.07685533319025));
#28967=CARTESIAN_POINT('Ctrl Pts',(-0.257063740193955,1.80162236967847,
6.07581441016139));
#28968=CARTESIAN_POINT('Ctrl Pts',(-0.271974558916785,1.81589662215662,
6.07477348713254));
#28969=CARTESIAN_POINT('Ctrl Pts',(-0.286893035447487,1.8301782055188,6.07373202951275));
#28970=CARTESIAN_POINT('Ctrl Pts',(-0.300685802432052,1.84564010442998,
6.07269057189296));
#28971=CARTESIAN_POINT('Ctrl Pts',(-0.313171988864168,1.86207523165744,
6.07164911427316));
#28972=CARTESIAN_POINT('Ctrl Pts',(-0.325661990370595,1.87851538053279,
6.07060733844267));
#28973=CARTESIAN_POINT('Ctrl Pts',(-0.336844200656697,1.89592874243516,
6.06956556261217));
#28974=CARTESIAN_POINT('Ctrl Pts',(-0.346580484385113,1.91407835563501,
6.06852378678167));
#28975=CARTESIAN_POINT('Ctrl Pts',(-0.35633781331175,1.93226719963566,6.06747975912907));
#28976=CARTESIAN_POINT('Ctrl Pts',(-0.364642680053273,1.95119479771925,
6.06643573147648));
#28977=CARTESIAN_POINT('Ctrl Pts',(-0.371404358991896,1.97060258069877,
6.06539170382388));
#28978=CARTESIAN_POINT('Ctrl Pts',(-0.373795876202062,1.97746685914618,
6.06502244492801));
#28979=CARTESIAN_POINT('Ctrl Pts',(-0.375994807470021,1.98439107285004,
6.06465318603215));
#28980=CARTESIAN_POINT('Ctrl Pts',(-0.377998660159086,1.99136343655134,
6.06428392713628));
#28981=CARTESIAN_POINT('Ctrl Pts',(-0.385025732525039,2.01581398850962,
6.06298901708767));
#28982=CARTESIAN_POINT('Ctrl Pts',(-0.389684076670332,2.04097403727138,
6.06169410703905));
#28983=CARTESIAN_POINT('Ctrl Pts',(-0.391864857411872,2.06643180782983,
6.06039919699043));
#28984=CARTESIAN_POINT('Ctrl Pts',(-0.39280956022492,2.07745998090674,6.05983824872898));
#28985=CARTESIAN_POINT('Ctrl Pts',(-0.393289913826653,2.08854375466981,
6.05927730046753));
#28986=CARTESIAN_POINT('Ctrl Pts',(-0.393299842784111,2.09964833823957,
6.05871635220607));
#28987=CARTESIAN_POINT('',(-0.393077172497714,2.10015043742846,5.93371631113999));
#28988=CARTESIAN_POINT('Ctrl Pts',(-0.393299842784156,2.0996483382905,6.0587163522035));
#28989=CARTESIAN_POINT('Ctrl Pts',(-0.393318117775776,2.12008716099077,
6.05768388466541));
#28990=CARTESIAN_POINT('Ctrl Pts',(-0.391738844875401,2.14055949436901,
6.05665141712732));
#28991=CARTESIAN_POINT('Ctrl Pts',(-0.388572825286167,2.16079514330213,
6.05561894958924));
#28992=CARTESIAN_POINT('Ctrl Pts',(-0.385406021092393,2.18103580704376,
6.05458622618453));
#28993=CARTESIAN_POINT('Ctrl Pts',(-0.380651767631321,2.20103892416321,
6.05355350277983));
#28994=CARTESIAN_POINT('Ctrl Pts',(-0.374372619051574,2.22054058281121,
6.05252077937513));
#28995=CARTESIAN_POINT('Ctrl Pts',(-0.368092998734516,2.24004370657184,
6.0514879783844));
#28996=CARTESIAN_POINT('Ctrl Pts',(-0.360288510019637,2.25904459142575,
6.05045517739367));
#28997=CARTESIAN_POINT('Ctrl Pts',(-0.351070906641866,2.27729666807264,
6.04942237640295));
#28998=CARTESIAN_POINT('Ctrl Pts',(-0.341832636631956,2.29558966739089,
6.04838725978664));
#28999=CARTESIAN_POINT('Ctrl Pts',(-0.331175306035825,2.3131298581053,6.04735214317034));
#29000=CARTESIAN_POINT('Ctrl Pts',(-0.319255925186921,2.3296966352236,6.04631702655404));
#29001=CARTESIAN_POINT('Ctrl Pts',(-0.311949868724265,2.33985134129138,
6.04568254557386));
#29002=CARTESIAN_POINT('Ctrl Pts',(-0.304170494125852,2.34964090855378,
6.04504806459368));
#29003=CARTESIAN_POINT('Ctrl Pts',(-0.2959610723649,2.35902110656203,6.0444135836135));
#29004=CARTESIAN_POINT('Ctrl Pts',(-0.282453449687211,2.37445510167483,
6.04336962096594));
#29005=CARTESIAN_POINT('Ctrl Pts',(-0.267695034824309,2.38887563042575,
6.04232565831839));
#29006=CARTESIAN_POINT('Ctrl Pts',(-0.251863595678851,2.40207551898775,
6.04128169567084));
#29007=CARTESIAN_POINT('Ctrl Pts',(-0.236061280171633,2.41525112493237,
6.04023965350507));
#29008=CARTESIAN_POINT('Ctrl Pts',(-0.219190379233024,2.42721003637822,
6.0391976113393));
#29009=CARTESIAN_POINT('Ctrl Pts',(-0.201465358703167,2.43778188116387,
6.03815556917353));
#29010=CARTESIAN_POINT('Ctrl Pts',(-0.183759374566912,2.4483423719543,6.03711464614467));
#29011=CARTESIAN_POINT('Ctrl Pts',(-0.165201705818374,2.45751835364565,
6.03607372311582));
#29012=CARTESIAN_POINT('Ctrl Pts',(-0.14603553004465,2.4651828500417,6.03503280008697));
#29013=CARTESIAN_POINT('Ctrl Pts',(-0.126859511022575,2.47285128272334,
6.03399134246717));
#29014=CARTESIAN_POINT('Ctrl Pts',(-0.107075037835066,2.47900639114825,
6.03294988484738));
#29015=CARTESIAN_POINT('Ctrl Pts',(-0.086945493420707,2.48356925212252,
6.03190842722759));
#29016=CARTESIAN_POINT('Ctrl Pts',(-0.0668097985529559,2.48813350724974,
6.03086665139709));
#29017=CARTESIAN_POINT('Ctrl Pts',(-0.0463295475315251,2.49110441918453,
6.02982487556659));
#29018=CARTESIAN_POINT('Ctrl Pts',(-0.0257776276362968,2.49245433353888,
6.02878309973609));
#29019=CARTESIAN_POINT('Ctrl Pts',(-0.00518128429983682,2.49380716576374,
6.0277390720835));
#29020=CARTESIAN_POINT('Ctrl Pts',(0.015486300775959,2.49353201500072,6.0266950444309));
#29021=CARTESIAN_POINT('Ctrl Pts',(0.0359521962755143,2.49165332831851,
6.0256510167783));
#29022=CARTESIAN_POINT('Ctrl Pts',(0.0431907152518356,2.49098886146437,
6.02528175788244));
#29023=CARTESIAN_POINT('Ctrl Pts',(0.0504040724291839,2.49012427348697,
6.02491249898657));
#29024=CARTESIAN_POINT('Ctrl Pts',(0.0575805078623604,2.48906217384155,
6.0245432400907));
#29025=CARTESIAN_POINT('Ctrl Pts',(0.0778696075120675,2.48605942327764,
6.02349927744315));
#29026=CARTESIAN_POINT('Ctrl Pts',(0.0979836429094615,2.48145637659588,
6.02245531479559));
#29027=CARTESIAN_POINT('Ctrl Pts',(0.117652189613658,2.47529035729567,6.02141135214804));
#29028=CARTESIAN_POINT('Ctrl Pts',(0.137284553906781,2.46913568105239,6.02036930998227));
#29029=CARTESIAN_POINT('Ctrl Pts',(0.156472344283298,2.46142390032958,6.0193272678165));
#29030=CARTESIAN_POINT('Ctrl Pts',(0.174956214545047,2.45224311631609,6.01828522565073));
#29031=CARTESIAN_POINT('Ctrl Pts',(0.193420233420518,2.44307219232039,6.01724430262188));
#29032=CARTESIAN_POINT('Ctrl Pts',(0.211181164526297,2.43243569686198,6.01620337959302));
#29033=CARTESIAN_POINT('Ctrl Pts',(0.228000607581332,2.4204693635007,6.01516245656417));
#29034=CARTESIAN_POINT('Ctrl Pts',(0.244828688663949,2.40849688454248,6.01412099894438));
#29035=CARTESIAN_POINT('Ctrl Pts',(0.260713706850183,2.39519361666377,6.01307954132459));
#29036=CARTESIAN_POINT('Ctrl Pts',(0.275446728161847,2.38073829440412,6.0120380837048));
#29037=CARTESIAN_POINT('Ctrl Pts',(0.290184251053825,2.36627855541332,6.0109963078743));
#29038=CARTESIAN_POINT('Ctrl Pts',(0.303768576933495,2.35066660197949,6.0099545320438));
#29039=CARTESIAN_POINT('Ctrl Pts',(0.31602873468093,2.33411691279352,6.0089127562133));
#29040=CARTESIAN_POINT('Ctrl Pts',(0.328315393037552,2.31753145107883,6.00786872856071));
#29041=CARTESIAN_POINT('Ctrl Pts',(0.339271778590694,2.30000483142703,6.00682470090811));
#29042=CARTESIAN_POINT('Ctrl Pts',(0.34877070422074,2.28177977301496,6.00578067325552));
#29043=CARTESIAN_POINT('Ctrl Pts',(0.352130349706522,2.27533380874416,6.00541141435965));
#29044=CARTESIAN_POINT('Ctrl Pts',(0.355308109232392,2.26880067178446,6.00504215546378));
#29045=CARTESIAN_POINT('Ctrl Pts',(0.358299811004213,2.26219166265362,6.00467289656791));
#29046=CARTESIAN_POINT('Ctrl Pts',(0.366757900808832,2.2435067812678,6.00362893392036));
#29047=CARTESIAN_POINT('Ctrl Pts',(0.373775667542263,2.22410282783564,6.00258497127281));
#29048=CARTESIAN_POINT('Ctrl Pts',(0.37923810783494,2.20422738395342,6.00154100862525));
#29049=CARTESIAN_POINT('Ctrl Pts',(0.384690499380086,2.18438850309194,6.00049896645949));
#29050=CARTESIAN_POINT('Ctrl Pts',(0.38859299370584,2.16408053914949,5.99945692429372));
#29051=CARTESIAN_POINT('Ctrl Pts',(0.390879279086038,2.14356924581834,5.99841488212795));
#29052=CARTESIAN_POINT('Ctrl Pts',(0.393163109031653,2.12307998129402,5.99737395909909));
#29053=CARTESIAN_POINT('Ctrl Pts',(0.393834066137538,2.10238854524085,5.99633303607024));
#29054=CARTESIAN_POINT('Ctrl Pts',(0.392877227231284,2.08176886391203,5.99529211304139));
#29055=CARTESIAN_POINT('Ctrl Pts',(0.391919896917505,2.06113859285228,5.9942506554216));
#29056=CARTESIAN_POINT('Ctrl Pts',(0.389333118466535,2.04058088587227,5.9932091978018));
#29057=CARTESIAN_POINT('Ctrl Pts',(0.38515407534178,2.0203681706375,5.99216774018201));
#29058=CARTESIAN_POINT('Ctrl Pts',(0.380973755337161,2.00014927953703,5.99112596435151));
#29059=CARTESIAN_POINT('Ctrl Pts',(0.375200386419442,1.98027630263458,5.99008418852102));
#29060=CARTESIAN_POINT('Ctrl Pts',(0.367921756355568,1.9610090966997,5.98904241269052));
#29061=CARTESIAN_POINT('Ctrl Pts',(0.36062739336764,1.94170024426196,5.98799838503792));
#29062=CARTESIAN_POINT('Ctrl Pts',(0.35182158723032,1.92300044321811,5.98695435738532));
#29063=CARTESIAN_POINT('Ctrl Pts',(0.341639571887238,1.90514802305159,5.98591032973273));
#29064=CARTESIAN_POINT('Ctrl Pts',(0.338038326523736,1.89883385604381,5.98554107083686));
#29065=CARTESIAN_POINT('Ctrl Pts',(0.334265326646065,1.89262543385607,5.98517181194099));
#29066=CARTESIAN_POINT('Ctrl Pts',(0.330327815664333,1.88653238138202,5.98480255304513));
#29067=CARTESIAN_POINT('Ctrl Pts',(0.319195749693074,1.86930620412889,5.98375859039757));
#29068=CARTESIAN_POINT('Ctrl Pts',(0.306679402167288,1.85290182961062,5.98271462775002));
#29069=CARTESIAN_POINT('Ctrl Pts',(0.29292469072401,1.83754997511099,5.98167066510247));
#29070=CARTESIAN_POINT('Ctrl Pts',(0.279195282554585,1.82222636200197,5.9806286229367));
#29071=CARTESIAN_POINT('Ctrl Pts',(0.264232473562321,1.80795200707744,5.97958658077093));
#29072=CARTESIAN_POINT('Ctrl Pts',(0.248223818474283,1.79492652369954,5.97854453860516));
#29073=CARTESIAN_POINT('Ctrl Pts',(0.232232356430318,1.78191502948616,5.9775036155763));
#29074=CARTESIAN_POINT('Ctrl Pts',(0.215197827734225,1.77015022853234,5.97646269254745));
#29075=CARTESIAN_POINT('Ctrl Pts',(0.197342476301318,1.75979294973904,5.97542176951859));
#29076=CARTESIAN_POINT('Ctrl Pts',(0.179477954825285,1.74943035171729,5.9743803118988));
#29077=CARTESIAN_POINT('Ctrl Pts',(0.160792396807795,1.74047710311107,5.97333885427901));
#29078=CARTESIAN_POINT('Ctrl Pts',(0.141534992388243,1.73304940941639,5.97229739665922));
#29079=CARTESIAN_POINT('Ctrl Pts',(0.122271703992083,1.72561944623746,5.97125562082872));
#29080=CARTESIAN_POINT('Ctrl Pts',(0.102436920285775,1.71971619671289,5.97021384499822));
#29081=CARTESIAN_POINT('Ctrl Pts',(0.0822966545981881,1.7154065124811,5.96917206916772));
#29082=CARTESIAN_POINT('Ctrl Pts',(0.0621128552692868,1.71108751276906,
5.96812804151513));
#29083=CARTESIAN_POINT('Ctrl Pts',(0.0416229857702449,1.70836905204285,
5.96708401386253));
#29084=CARTESIAN_POINT('Ctrl Pts',(0.0211006423750957,1.70726643523712,
5.96603998620993));
#29085=CARTESIAN_POINT('Ctrl Pts',(0.0138421585180325,1.70687645412576,
5.96567072731406));
#29086=CARTESIAN_POINT('Ctrl Pts',(0.00657961297702736,1.70668812886686,
5.9653014684182));
#29087=CARTESIAN_POINT('Ctrl Pts',(-0.000674980476240858,1.70670057920033,
5.96493220952233));
#29088=CARTESIAN_POINT('Ctrl Pts',(-0.0211850471886834,1.70673577857736,
5.96388824687478));
#29089=CARTESIAN_POINT('Ctrl Pts',(-0.041753464065631,1.70837976333955,
5.96284428422722));
#29090=CARTESIAN_POINT('Ctrl Pts',(-0.0621072520305343,1.71163473475964,
5.96180032157967));
#29091=CARTESIAN_POINT('Ctrl Pts',(-0.0824235970092251,1.71488371830906,
5.9607582794139));
#29092=CARTESIAN_POINT('Ctrl Pts',(-0.102525369071605,1.71973774976776,
5.95971623724813));
#29093=CARTESIAN_POINT('Ctrl Pts',(-0.122143202966196,1.72614718408288,
5.95867419508236));
#29094=CARTESIAN_POINT('Ctrl Pts',(-0.141739967615372,1.73254973476624,
5.95763327205351));
#29095=CARTESIAN_POINT('Ctrl Pts',(-0.160853121076448,1.74050417215389,
5.95659234902466));
#29096=CARTESIAN_POINT('Ctrl Pts',(-0.17922713088291,1.74991068917278,5.95555142599581));
#29097=CARTESIAN_POINT('Ctrl Pts',(-0.197610577101928,1.75932203713364,
5.95450996837601));
#29098=CARTESIAN_POINT('Ctrl Pts',(-0.215253459013915,1.77018663362267,
5.95346851075622));
#29099=CARTESIAN_POINT('Ctrl Pts',(-0.231923177832209,1.78235785924376,
5.95242705313643));
#29100=CARTESIAN_POINT('Ctrl Pts',(-0.248597989976352,1.7945328037049,5.95138527730593));
#29101=CARTESIAN_POINT('Ctrl Pts',(-0.26429847468269,1.80801470934215,5.95034350147543));
#29102=CARTESIAN_POINT('Ctrl Pts',(-0.278824424075222,1.82261609538562,
5.94930172564494));
#29103=CARTESIAN_POINT('Ctrl Pts',(-0.293381771636991,1.83724904265635,
5.94825769799234));
#29104=CARTESIAN_POINT('Ctrl Pts',(-0.306759038676237,1.85300573987908,
5.94721367033974));
#29105=CARTESIAN_POINT('Ctrl Pts',(-0.318795253923177,1.86966442724569,
5.94616964268715));
#29106=CARTESIAN_POINT('Ctrl Pts',(-0.323052305488274,1.87555638660928,
5.94580038379128));
#29107=CARTESIAN_POINT('Ctrl Pts',(-0.327141999865019,1.88156092106608,
5.94543112489541));
#29108=CARTESIAN_POINT('Ctrl Pts',(-0.331058573920149,1.88766745272107,
5.94506186599955));
#29109=CARTESIAN_POINT('Ctrl Pts',(-0.342388352507316,1.9053322920967,5.94399368205291));
#29110=CARTESIAN_POINT('Ctrl Pts',(-0.352331112848581,1.92395378138503,
5.94292549810627));
#29111=CARTESIAN_POINT('Ctrl Pts',(-0.360732399787938,1.94329318539631,
5.94185731415963));
#29112=CARTESIAN_POINT('Ctrl Pts',(-0.369114934475254,1.96258942252364,
5.94079151447326));
#29113=CARTESIAN_POINT('Ctrl Pts',(-0.37596250182271,1.9825997914935,5.93972571478688));
#29114=CARTESIAN_POINT('Ctrl Pts',(-0.381166155586733,2.00306057646535,
5.9386599151005));
#29115=CARTESIAN_POINT('Ctrl Pts',(-0.386360756782567,2.02348576670712,
5.93759596953909));
#29116=CARTESIAN_POINT('Ctrl Pts',(-0.389916919389646,2.04435916204525,
5.93653202397768));
#29117=CARTESIAN_POINT('Ctrl Pts',(-0.39177519953194,2.06540111227642,5.93546807841626));
#29118=CARTESIAN_POINT('Ctrl Pts',(-0.392795050595118,2.07694923940009,
5.93488416967867));
#29119=CARTESIAN_POINT('Ctrl Pts',(-0.393304387679479,2.0885478865703,5.93430026094109));
#29120=CARTESIAN_POINT('Ctrl Pts',(-0.393299971507302,2.10014970756677,
5.9337163522035));
#29121=CARTESIAN_POINT('',(-0.393409105398565,2.10028637322991,5.80871640015418));
#29122=CARTESIAN_POINT('Ctrl Pts',(-0.392706208187778,2.10015165266115,
5.93371624276851));
#29123=CARTESIAN_POINT('Ctrl Pts',(-0.392898096062828,2.15652638923434,
5.93087466933792));
#29124=CARTESIAN_POINT('Ctrl Pts',(-0.355155351020755,2.3440598714961,5.92140964806639));
#29125=CARTESIAN_POINT('Ctrl Pts',(-0.0665060678930708,2.56027379505342,
5.90532117895399));
#29126=CARTESIAN_POINT('Ctrl Pts',(0.351005511560806,2.40507401451683,5.88545083543116));
#29127=CARTESIAN_POINT('Ctrl Pts',(0.44651731924308,1.97001035773783,5.8655804919084));
#29128=CARTESIAN_POINT('Ctrl Pts',(0.132410274363759,1.65419450124252,5.84571014838559));
#29129=CARTESIAN_POINT('Ctrl Pts',(-0.283092572096759,1.74305187273891,
5.82675548880205));
#29130=CARTESIAN_POINT('Ctrl Pts',(-0.392741683210659,1.98774849000428,
5.81442427705941));
#29131=CARTESIAN_POINT('Ctrl Pts',(-0.393666477116067,2.10028433320096,
5.80871651315772));
#29132=CARTESIAN_POINT('',(-0.393383440529804,2.09969440306954,5.68371631382268));
#29133=CARTESIAN_POINT('Ctrl Pts',(-0.393299895110372,2.10028723887339,
5.8087163522035));
#29134=CARTESIAN_POINT('Ctrl Pts',(-0.393286722953847,2.11832312558545,
5.80780072191567));
#29135=CARTESIAN_POINT('Ctrl Pts',(-0.392032844841001,2.13631441240402,
5.80688509162785));
#29136=CARTESIAN_POINT('Ctrl Pts',(-0.389556943360793,2.15413204115306,
5.80596946134003));
#29137=CARTESIAN_POINT('Ctrl Pts',(-0.386734025968569,2.17444694240656,
5.80492549869248));
#29138=CARTESIAN_POINT('Ctrl Pts',(-0.382309324566935,2.19460096126699,
5.80388153604494));
#29139=CARTESIAN_POINT('Ctrl Pts',(-0.376317765844307,2.21432335330084,
5.80283757339739));
#29140=CARTESIAN_POINT('Ctrl Pts',(-0.370337229239578,2.23400946386934,
5.80179553123162));
#29141=CARTESIAN_POINT('Ctrl Pts',(-0.362795711325402,2.25326481037358,
5.80075348906585));
#29142=CARTESIAN_POINT('Ctrl Pts',(-0.353779012615713,2.2718292764131,5.79971144690009));
#29143=CARTESIAN_POINT('Ctrl Pts',(-0.34477199769879,2.29037380450774,5.79867052387123));
#29144=CARTESIAN_POINT('Ctrl Pts',(-0.33429324105237,2.30822825405188,5.79762960084238));
#29145=CARTESIAN_POINT('Ctrl Pts',(-0.32247635922602,2.32515303182576,5.79658867781353));
#29146=CARTESIAN_POINT('Ctrl Pts',(-0.31065340855715,2.34208650172438,5.79554722019374));
#29147=CARTESIAN_POINT('Ctrl Pts',(-0.297491367778473,2.35808873349275,
5.79450576257394));
#29148=CARTESIAN_POINT('Ctrl Pts',(-0.283167113736886,2.3729492181669,5.79346430495415));
#29149=CARTESIAN_POINT('Ctrl Pts',(-0.268838483011204,2.38781424336698,
5.79242252912365));
#29150=CARTESIAN_POINT('Ctrl Pts',(-0.2533474683363,2.40153632279997,5.79138075329315));
#29151=CARTESIAN_POINT('Ctrl Pts',(-0.236907025572907,2.41394259225884,
5.79033897746265));
#29152=CARTESIAN_POINT('Ctrl Pts',(-0.220431046419399,2.42637567815067,
5.78929494981006));
#29153=CARTESIAN_POINT('Ctrl Pts',(-0.203002163053162,2.43748687994941,
5.78825092215746));
#29154=CARTESIAN_POINT('Ctrl Pts',(-0.184861958539821,2.44714686558404,
5.78720689450486));
#29155=CARTESIAN_POINT('Ctrl Pts',(-0.178446005980517,2.45056347588244,
5.78683763560898));
#29156=CARTESIAN_POINT('Ctrl Pts',(-0.171941273055359,2.45379897950855,
5.7864683767131));
#29157=CARTESIAN_POINT('Ctrl Pts',(-0.165359022886146,2.45684910473496,
5.78609911781722));
#29158=CARTESIAN_POINT('Ctrl Pts',(-0.146749793995061,2.46547236836449,
5.78505515516966));
#29159=CARTESIAN_POINT('Ctrl Pts',(-0.127408763273877,2.47266173477362,
5.78401119252211));
#29160=CARTESIAN_POINT('Ctrl Pts',(-0.107582483937317,2.47830001209341,
5.78296722987455));
#29161=CARTESIAN_POINT('Ctrl Pts',(-0.087792677178002,2.48392791719451,
5.78192518770878));
#29162=CARTESIAN_POINT('Ctrl Pts',(-0.0675200771685368,2.48801014089082,
5.78088314554301));
#29163=CARTESIAN_POINT('Ctrl Pts',(-0.0470298398041594,2.49047802008307,
5.77984110337724));
#29164=CARTESIAN_POINT('Ctrl Pts',(-0.0265616086328142,2.49294324881184,
5.77880018034838));
#29165=CARTESIAN_POINT('Ctrl Pts',(-0.00587692747130106,2.4937974587555,
5.77775925731953));
#29166=CARTESIAN_POINT('Ctrl Pts',(0.014750420358856,2.49302330096222,5.77671833429068));
#29167=CARTESIAN_POINT('Ctrl Pts',(0.0353883618572411,2.49224874558166,
5.77567687667089));
#29168=CARTESIAN_POINT('Ctrl Pts',(0.055968175334715,2.48984416323488,5.7746354190511));
#29169=CARTESIAN_POINT('Ctrl Pts',(0.0762171144521648,2.48584432283576,
5.77359396143131));
#29170=CARTESIAN_POINT('Ctrl Pts',(0.0964722405032938,2.48184326031102,
5.77255218560081));
#29171=CARTESIAN_POINT('Ctrl Pts',(0.116395576724372,2.47624614735455,5.77151040977031));
#29172=CARTESIAN_POINT('Ctrl Pts',(0.135726498939805,2.46913846654818,5.77046863393982));
#29173=CARTESIAN_POINT('Ctrl Pts',(0.155099205382283,2.46201542232845,5.76942460628722));
#29174=CARTESIAN_POINT('Ctrl Pts',(0.173876272279996,2.45337559944097,5.76838057863463));
#29175=CARTESIAN_POINT('Ctrl Pts',(0.191818181633477,2.44335211546578,5.76733655098203));
#29176=CARTESIAN_POINT('Ctrl Pts',(0.198163999793638,2.43980694056914,5.76696729208617));
#29177=CARTESIAN_POINT('Ctrl Pts',(0.204405598637342,2.43608908123724,5.7665980331903));
#29178=CARTESIAN_POINT('Ctrl Pts',(0.210533289488355,2.43220569534132,5.76622877429444));
#29179=CARTESIAN_POINT('Ctrl Pts',(0.227857395788466,2.42122665091808,5.76518481164689));
#29180=CARTESIAN_POINT('Ctrl Pts',(0.244371993186064,2.40885609993933,5.76414084899933));
#29181=CARTESIAN_POINT('Ctrl Pts',(0.259845080949438,2.39523791068625,5.76309688635178));
#29182=CARTESIAN_POINT('Ctrl Pts',(0.275289704300553,2.38164477355973,5.76205484418601));
#29183=CARTESIAN_POINT('Ctrl Pts',(0.289696035761867,2.36680898995127,5.76101280202024));
#29184=CARTESIAN_POINT('Ctrl Pts',(0.302862808493005,2.35091633910873,5.75997075985447));
#29185=CARTESIAN_POINT('Ctrl Pts',(0.316015440317073,2.33504075672354,5.75892983682562));
#29186=CARTESIAN_POINT('Ctrl Pts',(0.327930666993002,2.31811110573357,5.75788891379676));
#29187=CARTESIAN_POINT('Ctrl Pts',(0.338445697352575,2.30034819675637,5.75684799076791));
#29188=CARTESIAN_POINT('Ctrl Pts',(0.348966127957685,2.28257616521208,5.75580653314812));
#29189=CARTESIAN_POINT('Ctrl Pts',(0.358084536956932,2.26397064569898,5.75476507552832));
#29190=CARTESIAN_POINT('Ctrl Pts',(0.365682516154062,2.24477978926367,5.75372361790853));
#29191=CARTESIAN_POINT('Ctrl Pts',(0.373282816865082,2.22558306918508,5.75268184207803));
#29192=CARTESIAN_POINT('Ctrl Pts',(0.379361525966739,2.20580135299859,5.75164006624753));
#29193=CARTESIAN_POINT('Ctrl Pts',(0.38384943816891,2.18570005144346,5.75059829041703));
#29194=CARTESIAN_POINT('Ctrl Pts',(0.388347051095149,2.16555530046887,5.74955426276444));
#29195=CARTESIAN_POINT('Ctrl Pts',(0.391246898912448,2.14509031418877,5.74851023511184));
#29196=CARTESIAN_POINT('Ctrl Pts',(0.392531253844577,2.1245785425769,5.74746620745924));
#29197=CARTESIAN_POINT('Ctrl Pts',(0.392985513349061,2.11732379782107,5.74709694856338));
#29198=CARTESIAN_POINT('Ctrl Pts',(0.393238160889453,2.11006320532748,5.74672768966751));
#29199=CARTESIAN_POINT('Ctrl Pts',(0.393289970276536,2.10280878619362,5.74635843077165));
#29200=CARTESIAN_POINT('Ctrl Pts',(0.39343644491943,2.08229921231399,5.74531446812409));
#29201=CARTESIAN_POINT('Ctrl Pts',(0.391974714140571,2.06171704037194,5.74427050547654));
#29202=CARTESIAN_POINT('Ctrl Pts',(0.388900158778556,2.04133521923663,5.74322654282899));
#29203=CARTESIAN_POINT('Ctrl Pts',(0.385831259392432,2.02099089265757,5.74218450066321));
#29204=CARTESIAN_POINT('Ctrl Pts',(0.381155474434773,2.00084691349555,5.74114245849745));
#29205=CARTESIAN_POINT('Ctrl Pts',(0.374920061046105,1.98117307617722,5.74010041633167));
#29206=CARTESIAN_POINT('Ctrl Pts',(0.36869134439346,1.9615203682511,5.73905949330282));
#29207=CARTESIAN_POINT('Ctrl Pts',(0.360906518220287,1.94233750634693,5.73801857027397));
#29208=CARTESIAN_POINT('Ctrl Pts',(0.3516631222465,1.92388089697071,5.73697764724511));
#29209=CARTESIAN_POINT('Ctrl Pts',(0.342414979105453,1.90541480876094,5.73593618962532));
#29210=CARTESIAN_POINT('Ctrl Pts',(0.331707084728963,1.88767638332203,5.73489473200553));
#29211=CARTESIAN_POINT('Ctrl Pts',(0.31968399246388,1.87089950903074,5.73385327438574));
#29212=CARTESIAN_POINT('Ctrl Pts',(0.307657226619948,1.85411750867295,5.73281149855524));
#29213=CARTESIAN_POINT('Ctrl Pts',(0.29431492054294,1.83829822082006,5.73176972272474));
#29214=CARTESIAN_POINT('Ctrl Pts',(0.27984277426044,1.82364350614791,5.73072794689424));
#29215=CARTESIAN_POINT('Ctrl Pts',(0.265339346105336,1.80895711497744,5.72968391924164));
#29216=CARTESIAN_POINT('Ctrl Pts',(0.24970175924849,1.79544080416041,5.72863989158905));
#29217=CARTESIAN_POINT('Ctrl Pts',(0.233150338958184,1.78325750294019,5.72759586393645));
#29218=CARTESIAN_POINT('Ctrl Pts',(0.227296318553429,1.7789484289943,5.72722660504058));
#29219=CARTESIAN_POINT('Ctrl Pts',(0.221328245067012,1.77480570851145,5.72685734614472));
#29220=CARTESIAN_POINT('Ctrl Pts',(0.215256644930681,1.77083519809496,5.72648808724885));
#29221=CARTESIAN_POINT('Ctrl Pts',(0.198091117372228,1.75960983666715,5.7254441246013));
#29222=CARTESIAN_POINT('Ctrl Pts',(0.17999399740984,1.74969738450892,5.72440016195374));
#29223=CARTESIAN_POINT('Ctrl Pts',(0.161192284904169,1.74124947764864,5.72335619930619));
#29224=CARTESIAN_POINT('Ctrl Pts',(0.142425160174654,1.73281711162335,5.72231415714042));
#29225=CARTESIAN_POINT('Ctrl Pts',(0.122956654946036,1.72584429543379,5.72127211497465));
#29226=CARTESIAN_POINT('Ctrl Pts',(0.103039198346786,1.72043733902812,5.72023007280888));
#29227=CARTESIAN_POINT('Ctrl Pts',(0.0831431327830263,1.7150361896087,5.71918914978003));
#29228=CARTESIAN_POINT('Ctrl Pts',(0.0627997719662527,1.71119778107657,
5.71814822675118));
#29229=CARTESIAN_POINT('Ctrl Pts',(0.0422775070903213,1.70897889776353,
5.71710730372232));
#29230=CARTESIAN_POINT('Ctrl Pts',(0.0217447025140247,1.70675887488984,
5.71606584610253));
#29231=CARTESIAN_POINT('Ctrl Pts',(0.00103354010403899,1.70616013399676,
5.71502438848274));
#29232=CARTESIAN_POINT('Ctrl Pts',(-0.0195810732662579,1.70718774004654,
5.71398293086295));
#29233=CARTESIAN_POINT('Ctrl Pts',(-0.040201985299664,1.70821566007478,
5.71294115503245));
#29234=CARTESIAN_POINT('Ctrl Pts',(-0.0607255571206432,1.71087084355894,
5.71189937920196));
#29235=CARTESIAN_POINT('Ctrl Pts',(-0.0808815378784357,1.71510642142221,
5.71085760337146));
#29236=CARTESIAN_POINT('Ctrl Pts',(-0.101081086246029,1.71935115458314,
5.70981357571886));
#29237=CARTESIAN_POINT('Ctrl Pts',(-0.120910750701084,1.72518289432425,
5.70876954806626));
#29238=CARTESIAN_POINT('Ctrl Pts',(-0.140114271369878,1.73250458375853,
5.70772552041367));
#29239=CARTESIAN_POINT('Ctrl Pts',(-0.14690630491541,1.73509416934054,5.7073562615178));
#29240=CARTESIAN_POINT('Ctrl Pts',(-0.153620204484674,1.73786970293102,
5.70698700262194));
#29241=CARTESIAN_POINT('Ctrl Pts',(-0.160245347593037,1.74082550400288,
5.70661774372607));
#29242=CARTESIAN_POINT('Ctrl Pts',(-0.17897584269351,1.74918209594194,5.70557378107852));
#29243=CARTESIAN_POINT('Ctrl Pts',(-0.197106707974342,1.7590326889642,5.70452981843097));
#29244=CARTESIAN_POINT('Ctrl Pts',(-0.214387566021736,1.77026850084459,
5.70348585578341));
#29245=CARTESIAN_POINT('Ctrl Pts',(-0.231636634068633,1.78148364323829,
5.70244381361764));
#29246=CARTESIAN_POINT('Ctrl Pts',(-0.248038156418609,1.79407859961191,
5.70140177145187));
#29247=CARTESIAN_POINT('Ctrl Pts',(-0.263366101315495,1.80789867053045,
5.7003597292861));
#29248=CARTESIAN_POINT('Ctrl Pts',(-0.27867758424036,1.82170389890995,5.69931880625725));
#29249=CARTESIAN_POINT('Ctrl Pts',(-0.292917215649837,1.83673116102595,
5.6982778832284));
#29250=CARTESIAN_POINT('Ctrl Pts',(-0.305891965258325,1.85278552714212,
5.69723696019954));
#29251=CARTESIAN_POINT('Ctrl Pts',(-0.318873378360047,1.86884813836229,
5.69619550257975));
#29252=CARTESIAN_POINT('Ctrl Pts',(-0.330588136862522,1.88593834527322,
5.69515404495996));
#29253=CARTESIAN_POINT('Ctrl Pts',(-0.340883169996976,1.90382774300933,
5.69411258734017));
#29254=CARTESIAN_POINT('Ctrl Pts',(-0.351181348712877,1.92172260673636,
5.69307081150967));
#29255=CARTESIAN_POINT('Ctrl Pts',(-0.360058603164078,1.94041649218144,
5.69202903567917));
#29256=CARTESIAN_POINT('Ctrl Pts',(-0.367408050040885,1.95965679651243,
5.69098725984867));
#29257=CARTESIAN_POINT('Ctrl Pts',(-0.374773382913896,1.97893868919784,
5.68994323219608));
#29258=CARTESIAN_POINT('Ctrl Pts',(-0.380604107394695,1.99876865220429,
5.68889920454348));
#29259=CARTESIAN_POINT('Ctrl Pts',(-0.384843112551628,2.01887867899513,
5.68785517689088));
#29260=CARTESIAN_POINT('Ctrl Pts',(-0.386342393111804,2.0259913318738,5.68748591799502));
#29261=CARTESIAN_POINT('Ctrl Pts',(-0.387643029924026,2.03313894532313,
5.68711665909915));
#29262=CARTESIAN_POINT('Ctrl Pts',(-0.388744049134309,2.04030951279591,
5.68674740020328));
#29263=CARTESIAN_POINT('Ctrl Pts',(-0.391756607633146,2.05992929216021,
5.68573705087002));
#29264=CARTESIAN_POINT('Ctrl Pts',(-0.393284374731537,2.07978273465513,
5.68472670153676));
#29265=CARTESIAN_POINT('Ctrl Pts',(-0.393299880736251,2.09969371116471,
5.6837163522035));
#29266=CARTESIAN_POINT('',(-0.393067535617534,2.0998785711675,5.55871638557015));
#29267=CARTESIAN_POINT('Ctrl Pts',(-0.393615161326375,2.0996963218002,5.68371620738833));
#29268=CARTESIAN_POINT('Ctrl Pts',(-0.392664726535533,2.2104023257077,5.67810315715238));
#29269=CARTESIAN_POINT('Ctrl Pts',(-0.28609226402674,2.45334197563328,5.66586665907551));
#29270=CARTESIAN_POINT('Ctrl Pts',(0.126029412727711,2.54765121535297,5.6470067131577));
#29271=CARTESIAN_POINT('Ctrl Pts',(0.444615155104554,2.23635390471428,5.62713636963491));
#29272=CARTESIAN_POINT('Ctrl Pts',(0.355327021560618,1.79997044940816,5.60726602611212));
#29273=CARTESIAN_POINT('Ctrl Pts',(-0.0599252808592673,1.63882326143504,
5.58739568258933));
#29274=CARTESIAN_POINT('Ctrl Pts',(-0.35335079016512,1.85214103468178,5.57121248728709));
#29275=CARTESIAN_POINT('Ctrl Pts',(-0.392846519052558,2.04161642652764,
5.56165273982576));
#29276=CARTESIAN_POINT('Ctrl Pts',(-0.392686924180345,2.09987760405252,
5.55871644020536));
#29277=CARTESIAN_POINT('',(-0.39329983717694,2.10035787790198,5.43371635219978));
#29278=CARTESIAN_POINT('Ctrl Pts',(-0.393299981436727,2.09987916180092,
5.5587163522035));
#29279=CARTESIAN_POINT('Ctrl Pts',(-0.393306508722677,2.12112394583906,
5.55764730633775));
#29280=CARTESIAN_POINT('Ctrl Pts',(-0.391587338751787,2.14235300093295,
5.556578260472));
#29281=CARTESIAN_POINT('Ctrl Pts',(-0.388176079816389,2.16327891480091,
5.55550921460626));
#29282=CARTESIAN_POINT('Ctrl Pts',(-0.384761280410992,2.1842265472108,5.55443905920151));
#29283=CARTESIAN_POINT('Ctrl Pts',(-0.379651056279692,2.20486974989942,
5.55336890379676));
#29284=CARTESIAN_POINT('Ctrl Pts',(-0.372929877145995,2.22493276884738,
5.55229874839202));
#29285=CARTESIAN_POINT('Ctrl Pts',(-0.366188560547455,2.24505589902444,
5.55122538667237));
#29286=CARTESIAN_POINT('Ctrl Pts',(-0.357826919027129,2.26459474733118,
5.55015202495272));
#29287=CARTESIAN_POINT('Ctrl Pts',(-0.347977653231523,2.28329332462335,
5.54907866323307));
#29288=CARTESIAN_POINT('Ctrl Pts',(-0.34362308470784,2.29156036074603,5.54860410733663));
#29289=CARTESIAN_POINT('Ctrl Pts',(-0.338978322112813,2.29966349503001,
5.54812955144019));
#29290=CARTESIAN_POINT('Ctrl Pts',(-0.334057509852243,2.30758244172212,
5.54765499554374));
#29291=CARTESIAN_POINT('Ctrl Pts',(-0.323232348402992,2.3250031178038,5.54661103289619));
#29292=CARTESIAN_POINT('Ctrl Pts',(-0.311008564576172,2.34162664233014,
5.54556707024864));
#29293=CARTESIAN_POINT('Ctrl Pts',(-0.297527966009004,2.35721974932447,
5.54452310760108));
#29294=CARTESIAN_POINT('Ctrl Pts',(-0.284072166455519,2.37278417111824,
5.54348106543531));
#29295=CARTESIAN_POINT('Ctrl Pts',(-0.269364572260165,2.38732134878226,
5.54243902326954));
#29296=CARTESIAN_POINT('Ctrl Pts',(-0.253589172615231,2.40062837778946,
5.54139698110377));
#29297=CARTESIAN_POINT('Ctrl Pts',(-0.237830715501688,2.41392111525656,
5.54035605807492));
#29298=CARTESIAN_POINT('Ctrl Pts',(-0.22100727053391,2.4259858327749,5.53931513504607));
#29299=CARTESIAN_POINT('Ctrl Pts',(-0.203338197706689,2.43665778968174,
5.53827421201721));
#29300=CARTESIAN_POINT('Ctrl Pts',(-0.185660050504178,2.4473352274275,5.53723275439742));
#29301=CARTESIAN_POINT('Ctrl Pts',(-0.167136029301738,2.45661808138098,
5.53619129677763));
#29302=CARTESIAN_POINT('Ctrl Pts',(-0.148013226583032,2.46438574993608,
5.53514983915784));
#29303=CARTESIAN_POINT('Ctrl Pts',(-0.128884581014407,2.47215579185257,
5.53410806332734));
#29304=CARTESIAN_POINT('Ctrl Pts',(-0.109157484439478,2.47840948359018,
5.53306628749684));
#29305=CARTESIAN_POINT('Ctrl Pts',(-0.0890967241835292,2.483075271637,5.53202451166634));
#29306=CARTESIAN_POINT('Ctrl Pts',(-0.0689926021390549,2.48775114489057,
5.53098048401375));
#29307=CARTESIAN_POINT('Ctrl Pts',(-0.048554104779658,2.49083215227422,
5.52993645636115));
#29308=CARTESIAN_POINT('Ctrl Pts',(-0.0280545143236507,2.49229814456108,
5.52889242870856));
#29309=CARTESIAN_POINT('Ctrl Pts',(-0.0208040778829734,2.49281664681707,
5.52852316981269));
#29310=CARTESIAN_POINT('Ctrl Pts',(-0.0135460081095542,2.49313359681599,
5.52815391091683));
#29311=CARTESIAN_POINT('Ctrl Pts',(-0.00629233248348705,2.49324966185862,
5.52778465202096));
#29312=CARTESIAN_POINT('Ctrl Pts',(0.0142151393631943,2.4935777990289,5.52674068937341));
#29313=CARTESIAN_POINT('Ctrl Pts',(0.0348094514741135,2.49229843692212,
5.52569672672586));
#29314=CARTESIAN_POINT('Ctrl Pts',(0.055217706603292,2.48940453885063,5.5246527640783));
#29315=CARTESIAN_POINT('Ctrl Pts',(0.0755884185480483,2.48651596441648,
5.52361072191253));
#29316=CARTESIAN_POINT('Ctrl Pts',(0.0957730242944711,2.48201879282628,
5.52256867974676));
#29317=CARTESIAN_POINT('Ctrl Pts',(0.115501321409074,2.47595788960036,5.52152663758099));
#29318=CARTESIAN_POINT('Ctrl Pts',(0.135208430642493,2.4699034956893,5.52048571455214));
#29319=CARTESIAN_POINT('Ctrl Pts',(0.15445949588466,2.46228889153527,5.51944479152329));
#29320=CARTESIAN_POINT('Ctrl Pts',(0.172997256708,2.45320934185198,5.51840386849443));
#29321=CARTESIAN_POINT('Ctrl Pts',(0.191544538042147,2.44412512914861,5.51736241087464));
#29322=CARTESIAN_POINT('Ctrl Pts',(0.209377115234713,2.43357477703596,5.51632095325485));
#29323=CARTESIAN_POINT('Ctrl Pts',(0.226259828669919,2.42170076146982,5.51527949563506));
#29324=CARTESIAN_POINT('Ctrl Pts',(0.243147700510096,2.40982311787426,5.51423771980456));
#29325=CARTESIAN_POINT('Ctrl Pts',(0.259084550313592,2.39662145820717,5.51319594397406));
#29326=CARTESIAN_POINT('Ctrl Pts',(0.273866880442892,2.38227968718361,5.51215416814356));
#29327=CARTESIAN_POINT('Ctrl Pts',(0.288681162914224,2.36790691609653,5.51111014049097));
#29328=CARTESIAN_POINT('Ctrl Pts',(0.30233545700679,2.35238966654509,5.51006611283837));
#29329=CARTESIAN_POINT('Ctrl Pts',(0.314664888287206,2.33594681197083,5.50902208518577));
#29330=CARTESIAN_POINT('Ctrl Pts',(0.319025646519955,2.33013118983679,5.5086528262899));
#29331=CARTESIAN_POINT('Ctrl Pts',(0.323221068067221,2.32420004558132,5.50828356739404));
#29332=CARTESIAN_POINT('Ctrl Pts',(0.327245203315154,2.31816385334703,5.50791430849817));
#29333=CARTESIAN_POINT('Ctrl Pts',(0.338622171980128,2.30109843042402,5.50687034585062));
#29334=CARTESIAN_POINT('Ctrl Pts',(0.348694534675806,2.28308982224769,5.50582638320307));
#29335=CARTESIAN_POINT('Ctrl Pts',(0.357308650619032,2.26436367662232,5.50478242055551));
#29336=CARTESIAN_POINT('Ctrl Pts',(0.365906919967752,2.2456719797597,5.50374037838974));
#29337=CARTESIAN_POINT('Ctrl Pts',(0.37305190937884,2.22626600161468,5.50269833622397));
#29338=CARTESIAN_POINT('Ctrl Pts',(0.378635077125592,2.20639721974796,5.50165629405821));
#29339=CARTESIAN_POINT('Ctrl Pts',(0.3842122486379,2.18654977664083,5.50061537102935));
#29340=CARTESIAN_POINT('Ctrl Pts',(0.388230702590658,2.16624121349099,5.4995744480005));
#29341=CARTESIAN_POINT('Ctrl Pts',(0.390631279542963,2.14573940798291,5.49853352497165));
#29342=CARTESIAN_POINT('Ctrl Pts',(0.393033089369024,2.12522707328187,5.49749206735186));
#29343=CARTESIAN_POINT('Ctrl Pts',(0.39381526066371,2.10452202686571,5.49645060973206));
#29344=CARTESIAN_POINT('Ctrl Pts',(0.392970293612514,2.08389911995901,5.49540915211227));
#29345=CARTESIAN_POINT('Ctrl Pts',(0.392125068387046,2.06326991185515,5.49436737628178));
#29346=CARTESIAN_POINT('Ctrl Pts',(0.389651781330608,2.04272362628423,5.49332560045128));
#29347=CARTESIAN_POINT('Ctrl Pts',(0.385594905872169,2.02253091864858,5.49228382462078));
#29348=CARTESIAN_POINT('Ctrl Pts',(0.381529261385364,2.00229456401714,5.49123979696818));
#29349=CARTESIAN_POINT('Ctrl Pts',(0.375873396245463,1.98241402151128,5.49019576931559));
#29350=CARTESIAN_POINT('Ctrl Pts',(0.368722093651012,1.96314640065525,5.48915174166299));
#29351=CARTESIAN_POINT('Ctrl Pts',(0.366192771660865,1.95633169571369,5.48878248276712));
#29352=CARTESIAN_POINT('Ctrl Pts',(0.363476816867384,1.94959347460586,5.48841322387126));
#29353=CARTESIAN_POINT('Ctrl Pts',(0.360579815483704,1.94294240971625,5.48804396497539));
#29354=CARTESIAN_POINT('Ctrl Pts',(0.352389461051284,1.92413862898428,5.48700000232784));
#29355=CARTESIAN_POINT('Ctrl Pts',(0.342699852786798,1.90592122108955,5.48595603968028));
#29356=CARTESIAN_POINT('Ctrl Pts',(0.331617550872154,1.88854151718705,5.48491207703273));
#29357=CARTESIAN_POINT('Ctrl Pts',(0.320555636046073,1.87119378512266,5.48387003486696));
#29358=CARTESIAN_POINT('Ctrl Pts',(0.308106454039638,1.85468134348551,5.48282799270119));
#29359=CARTESIAN_POINT('Ctrl Pts',(0.294422696090562,1.8392315854503,5.48178595053542));
#29360=CARTESIAN_POINT('Ctrl Pts',(0.280753634282543,1.8237984202125,5.48074502750656));
#29361=CARTESIAN_POINT('Ctrl Pts',(0.26585309250733,1.80942623999562,5.47970410447771));
#29362=CARTESIAN_POINT('Ctrl Pts',(0.24991428304389,1.79630979414762,5.47866318144886));
#29363=CARTESIAN_POINT('Ctrl Pts',(0.233967287823335,1.78318661203491,5.47762172382906));
#29364=CARTESIAN_POINT('Ctrl Pts',(0.216981517540274,1.77132093266452,5.47658026620927));
#29365=CARTESIAN_POINT('Ctrl Pts',(0.199184012240271,1.7608678439489,5.47553880858948));
#29366=CARTESIAN_POINT('Ctrl Pts',(0.181381069026487,1.75041156135896,5.47449703275898));
#29367=CARTESIAN_POINT('Ctrl Pts',(0.162766549276754,1.74136906977133,5.47345525692848));
#29368=CARTESIAN_POINT('Ctrl Pts',(0.14359209916996,1.73384948579039,5.47241348109798));
#29369=CARTESIAN_POINT('Ctrl Pts',(0.12437620305414,1.72631364805803,5.47136945344538));
#29370=CARTESIAN_POINT('Ctrl Pts',(0.104598664971117,1.72030750385541,5.47032542579279));
#29371=CARTESIAN_POINT('Ctrl Pts',(0.0845269750702698,1.71589053580331,
5.46928139814019));
#29372=CARTESIAN_POINT('Ctrl Pts',(0.0774278814471054,1.71432831209981,
5.46891213924432));
#29373=CARTESIAN_POINT('Ctrl Pts',(0.0702920690920527,1.71296441468007,
5.46854288034846));
#29374=CARTESIAN_POINT('Ctrl Pts',(0.0631315354551739,1.71179992371063,
5.46817362145259));
#29375=CARTESIAN_POINT('Ctrl Pts',(0.042887393101039,1.70850769408768,5.46712965880504));
#29376=CARTESIAN_POINT('Ctrl Pts',(0.0223247103380108,1.70679347814184,
5.46608569615748));
#29377=CARTESIAN_POINT('Ctrl Pts',(0.00171249385301841,1.70670372825972,
5.46504173350993));
#29378=CARTESIAN_POINT('Ctrl Pts',(-0.0188618042386542,1.70661414348218,
5.46399969134416));
#29379=CARTESIAN_POINT('Ctrl Pts',(-0.039484727974799,1.70814315558904,
5.46295764917839));
#29380=CARTESIAN_POINT('Ctrl Pts',(-0.0598824265768568,1.71128547108801,
5.46191560701263));
#29381=CARTESIAN_POINT('Ctrl Pts',(-0.0802582183710648,1.7144244117895,
5.46087468398377));
#29382=CARTESIAN_POINT('Ctrl Pts',(-0.10040853732107,1.71917313325891,5.45983376095492));
#29383=CARTESIAN_POINT('Ctrl Pts',(-0.12006504539051,1.72547460049367,5.45879283792607));
#29384=CARTESIAN_POINT('Ctrl Pts',(-0.139731648530185,1.73177930399777,
5.45775138030628));
#29385=CARTESIAN_POINT('Ctrl Pts',(-0.158903228560105,1.73963813712911,
5.45670992268648));
#29386=CARTESIAN_POINT('Ctrl Pts',(-0.177326483907724,1.74894415244163,
5.45566846506669));
#29387=CARTESIAN_POINT('Ctrl Pts',(-0.195755368363045,1.75825301114754,
5.45462668923619));
#29388=CARTESIAN_POINT('Ctrl Pts',(-0.213434833073728,1.76900956855079,
5.4535849134057));
#29389=CARTESIAN_POINT('Ctrl Pts',(-0.230136910221563,1.78106130282816,
5.4525431375752));
#29390=CARTESIAN_POINT('Ctrl Pts',(-0.246875089288167,1.79313908720265,
5.4514991099226));
#29391=CARTESIAN_POINT('Ctrl Pts',(-0.26263110159182,1.80651716094648,5.45045508227001));
#29392=CARTESIAN_POINT('Ctrl Pts',(-0.277210135828873,1.8210028125702,5.44941105461741));
#29393=CARTESIAN_POINT('Ctrl Pts',(-0.282366549140134,1.82612619767517,
5.44904179572154));
#29394=CARTESIAN_POINT('Ctrl Pts',(-0.287376082674135,1.83138781414826,
5.44867253682567));
#29395=CARTESIAN_POINT('Ctrl Pts',(-0.292231333771012,1.83677815903232,
5.44830327792981));
#29396=CARTESIAN_POINT('Ctrl Pts',(-0.30582172046043,1.85186633262047,5.44726968129738));
#29397=CARTESIAN_POINT('Ctrl Pts',(-0.318285162804529,1.86805964649283,
5.44623608466495));
#29398=CARTESIAN_POINT('Ctrl Pts',(-0.329438218792112,1.88516203780737,
5.44520248803252));
#29399=CARTESIAN_POINT('Ctrl Pts',(-0.340571639718522,1.9022343201993,5.44417071105679));
#29400=CARTESIAN_POINT('Ctrl Pts',(-0.350398789634137,1.92021191835659,
5.44313893408107));
#29401=CARTESIAN_POINT('Ctrl Pts',(-0.358776823701344,1.93886626431819,
5.44210715710534));
#29402=CARTESIAN_POINT('Ctrl Pts',(-0.367145819706796,1.95750048633074,
5.44107649319074));
#29403=CARTESIAN_POINT('Ctrl Pts',(-0.374068469320275,1.97680933592006,
5.44004582927614));
#29404=CARTESIAN_POINT('Ctrl Pts',(-0.379448363355163,1.99654068651355,
5.43901516536154));
#29405=CARTESIAN_POINT('Ctrl Pts',(-0.384831406635258,2.01628358730874,
5.43798389812402));
#29406=CARTESIAN_POINT('Ctrl Pts',(-0.388669681058896,2.03644876007996,
5.43695263088649));
#29407=CARTESIAN_POINT('Ctrl Pts',(-0.390916911969147,2.05676971042768,
5.43592136364897));
#29408=CARTESIAN_POINT('Ctrl Pts',(-0.392518556268971,2.07125283903853,
5.43518635983381));
#29409=CARTESIAN_POINT('Ctrl Pts',(-0.393313070471383,2.08581477928863,
5.43445135601866));
#29410=CARTESIAN_POINT('Ctrl Pts',(-0.393299837177007,2.10035787782838,
5.4337163522035));
#29411=CARTESIAN_POINT('',(-0.393299995348526,2.09993951157533,5.3087163521999));
#29412=CARTESIAN_POINT('Ctrl Pts',(-0.39329983717694,2.10035787790198,5.43371635219978));
#29413=CARTESIAN_POINT('Ctrl Pts',(-0.393276057989764,2.12649067457004,
5.43239560853574));
#29414=CARTESIAN_POINT('Ctrl Pts',(-0.390643793227004,2.15250592406765,
5.43107486487169));
#29415=CARTESIAN_POINT('Ctrl Pts',(-0.385495397888704,2.17796273601298,
5.42975412120765));
#29416=CARTESIAN_POINT('Ctrl Pts',(-0.38377869031185,2.18645118708899,5.42931372560744));
#29417=CARTESIAN_POINT('Ctrl Pts',(-0.381782613840906,2.19487774264244,
5.42887333000723));
#29418=CARTESIAN_POINT('Ctrl Pts',(-0.379511737965943,2.20322659902404,
5.42843293440702));
#29419=CARTESIAN_POINT('Ctrl Pts',(-0.374128601555078,2.22301765553767,
5.42738897175947));
#29420=CARTESIAN_POINT('Ctrl Pts',(-0.36717713989106,2.24244546136991,5.42634500911192));
#29421=CARTESIAN_POINT('Ctrl Pts',(-0.358726422556043,2.26124591083232,
5.42530104646436));
#29422=CARTESIAN_POINT('Ctrl Pts',(-0.350291251226182,2.28001177484207,
5.4242590042986));
#29423=CARTESIAN_POINT('Ctrl Pts',(-0.34036254283658,2.29815188540302,5.42321696213283));
#29424=CARTESIAN_POINT('Ctrl Pts',(-0.329058476444429,2.3154191474314,5.42217491996706));
#29425=CARTESIAN_POINT('Ctrl Pts',(-0.317766550442001,2.33266786469162,
5.42113399693821));
#29426=CARTESIAN_POINT('Ctrl Pts',(-0.305102575620766,2.3490449661173,5.42009307390936));
#29427=CARTESIAN_POINT('Ctrl Pts',(-0.291229549329997,2.36432979324519,
5.4190521508805));
#29428=CARTESIAN_POINT('Ctrl Pts',(-0.277349398214499,2.37962247026193,
5.41801069326071));
#29429=CARTESIAN_POINT('Ctrl Pts',(-0.26225943770187,2.39382119663989,5.41696923564092));
#29430=CARTESIAN_POINT('Ctrl Pts',(-0.246161876094521,2.40673966283744,
5.41592777802113));
#29431=CARTESIAN_POINT('Ctrl Pts',(-0.230059395980306,2.41966207618961,
5.41488600219063));
#29432=CARTESIAN_POINT('Ctrl Pts',(-0.212949297887291,2.43130301871467,
5.41384422636013));
#29433=CARTESIAN_POINT('Ctrl Pts',(-0.195064789571651,2.4415181076742,5.41280245052964));
#29434=CARTESIAN_POINT('Ctrl Pts',(-0.177141623485433,2.45175527678033,
5.41175842287704));
#29435=CARTESIAN_POINT('Ctrl Pts',(-0.158441371620449,2.46056012550098,
5.41071439522444));
#29436=CARTESIAN_POINT('Ctrl Pts',(-0.139220101257428,2.46783508995999,
5.40967036757185));
#29437=CARTESIAN_POINT('Ctrl Pts',(-0.132421789877577,2.47040814953075,
5.40930110867597));
#29438=CARTESIAN_POINT('Ctrl Pts',(-0.125558447314126,2.47279028365725,
5.4089318497801));
#29439=CARTESIAN_POINT('Ctrl Pts',(-0.118641788434857,2.47497868744367,
5.40856259088423));
#29440=CARTESIAN_POINT('Ctrl Pts',(-0.099087124765188,2.48116570646021,
5.40751862823667));
#29441=CARTESIAN_POINT('Ctrl Pts',(-0.0789889259748524,2.48583741536663,
5.40647466558912));
#29442=CARTESIAN_POINT('Ctrl Pts',(-0.0586066454681531,2.48890892392303,
5.40543070294157));
#29443=CARTESIAN_POINT('Ctrl Pts',(-0.038261860362759,2.49197478210847,
5.4043886607758));
#29444=CARTESIAN_POINT('Ctrl Pts',(-0.0176347413639124,2.49344611594472,
5.40334661861003));
#29445=CARTESIAN_POINT('Ctrl Pts',(0.00300297709885603,2.49328853546543,
5.40230457644426));
#29446=CARTESIAN_POINT('Ctrl Pts',(0.0236185309762048,2.4931311242251,5.4012636534154));
#29447=CARTESIAN_POINT('Ctrl Pts',(0.0442439294710951,2.4913482483719,5.40022273038655));
#29448=CARTESIAN_POINT('Ctrl Pts',(0.0646054055865343,2.48795751258224,
5.3991818073577));
#29449=CARTESIAN_POINT('Ctrl Pts',(0.0849773388254204,2.48456503539906,
5.39814034973791));
#29450=CARTESIAN_POINT('Ctrl Pts',(0.10508435046725,2.47956315356667,5.39709889211811));
#29451=CARTESIAN_POINT('Ctrl Pts',(0.124660329105881,2.47302103472487,5.39605743449832));
#29452=CARTESIAN_POINT('Ctrl Pts',(0.144242289059426,2.46647691698055,5.39501565866782));
#29453=CARTESIAN_POINT('Ctrl Pts',(0.163292207216022,2.45839189268546,5.39397388283733));
#29454=CARTESIAN_POINT('Ctrl Pts',(0.181562444411897,2.44888389011128,5.39293210700683));
#29455=CARTESIAN_POINT('Ctrl Pts',(0.199872173140076,2.43935533577377,5.39188807935423));
#29456=CARTESIAN_POINT('Ctrl Pts',(0.217398231816419,2.42839805289518,5.39084405170164));
#29457=CARTESIAN_POINT('Ctrl Pts',(0.233919973141138,2.41617453434084,5.38980002404904));
#29458=CARTESIAN_POINT('Ctrl Pts',(0.239763496484775,2.41185123605105,5.38943076515317));
#29459=CARTESIAN_POINT('Ctrl Pts',(0.245481688851205,2.40736990698496,5.38906150625731));
#29460=CARTESIAN_POINT('Ctrl Pts',(0.251065850364198,2.40273887887237,5.38869224736144));
#29461=CARTESIAN_POINT('Ctrl Pts',(0.266853299502816,2.3896461127307,5.38764828471389));
#29462=CARTESIAN_POINT('Ctrl Pts',(0.281660874152024,2.37527606778538,5.38660432206633));
#29463=CARTESIAN_POINT('Ctrl Pts',(0.295276750262427,2.35980094448339,5.38556035941878));
#29464=CARTESIAN_POINT('Ctrl Pts',(0.308867578501532,2.34435428933824,5.38451831725301));
#29465=CARTESIAN_POINT('Ctrl Pts',(0.321270534556845,2.32780709795903,5.38347627508724));
#29466=CARTESIAN_POINT('Ctrl Pts',(0.332309607972287,2.31036923360916,5.38243423292147));
#29467=CARTESIAN_POINT('Ctrl Pts',(0.343336825596299,2.29295009725166,5.38139330989262));
#29468=CARTESIAN_POINT('Ctrl Pts',(0.353002652540214,2.27464278999824,5.38035238686376));
#29469=CARTESIAN_POINT('Ctrl Pts',(0.361173696109049,2.25568702977104,5.37931146383491));
#29470=CARTESIAN_POINT('Ctrl Pts',(0.369348936112899,2.23672153435943,5.37827000621512));
#29471=CARTESIAN_POINT('Ctrl Pts',(0.376027553024985,2.21710758995318,5.37722854859533));
#29472=CARTESIAN_POINT('Ctrl Pts',(0.381123653322771,2.19710638948032,5.37618709097553));
#29473=CARTESIAN_POINT('Ctrl Pts',(0.386221310701368,2.17709907776875,5.37514531514504));
#29474=CARTESIAN_POINT('Ctrl Pts',(0.389735342425015,2.15670499576757,5.37410353931454));
#29475=CARTESIAN_POINT('Ctrl Pts',(0.391630853142078,2.13619619962383,5.37306176348404));
#29476=CARTESIAN_POINT('Ctrl Pts',(0.393530461048571,2.11564307325181,5.37201773583144));
#29477=CARTESIAN_POINT('Ctrl Pts',(0.393804553658141,2.09497547411574,5.37097370817884));
#29478=CARTESIAN_POINT('Ctrl Pts',(0.392470317511078,2.07446688673988,5.36992968052625));
#29479=CARTESIAN_POINT('Ctrl Pts',(0.391998415674701,2.06721326820657,5.36956042163038));
#29480=CARTESIAN_POINT('Ctrl Pts',(0.391325794809628,2.05997948528822,5.36919116273452));
#29481=CARTESIAN_POINT('Ctrl Pts',(0.39045475098324,2.05277736311242,5.36882190383865));
#29482=CARTESIAN_POINT('Ctrl Pts',(0.387992150273246,2.03241564232837,5.3677779411911));
#29483=CARTESIAN_POINT('Ctrl Pts',(0.383925166909935,2.01218640346367,5.36673397854354));
#29484=CARTESIAN_POINT('Ctrl Pts',(0.378283925926897,1.99236096718507,5.36569001589599));
#29485=CARTESIAN_POINT('Ctrl Pts',(0.372653062614526,1.97257200193281,5.36464797373022));
#29486=CARTESIAN_POINT('Ctrl Pts',(0.365453832055553,1.95318608073188,5.36360593156445));
#29487=CARTESIAN_POINT('Ctrl Pts',(0.356767413399143,1.93446479910157,5.36256388939868));
#29488=CARTESIAN_POINT('Ctrl Pts',(0.348090323819911,1.91576362383363,5.36152296636983));
#29489=CARTESIAN_POINT('Ctrl Pts',(0.337929498875328,1.89772634727018,5.36048204334097));
#29490=CARTESIAN_POINT('Ctrl Pts',(0.326414289810293,1.88059489202017,5.35944112031212));
#29491=CARTESIAN_POINT('Ctrl Pts',(0.314893166834003,1.86345463850124,5.35839966269233));
#29492=CARTESIAN_POINT('Ctrl Pts',(0.3020166672111,1.84722175531644,5.35735820507254));
#29493=CARTESIAN_POINT('Ctrl Pts',(0.287957910916233,1.83210985172881,5.35631674745275));
#29494=CARTESIAN_POINT('Ctrl Pts',(0.273894859058409,1.81699333079581,5.35527497162225));
#29495=CARTESIAN_POINT('Ctrl Pts',(0.258649358634886,1.80299898492108,5.35423319579175));
#29496=CARTESIAN_POINT('Ctrl Pts',(0.242431269840718,1.79030342364918,5.35319141996125));
#29497=CARTESIAN_POINT('Ctrl Pts',(0.226178125279587,1.7775804206335,5.35214739230865));
#29498=CARTESIAN_POINT('Ctrl Pts',(0.208948809167448,1.76616221380773,5.35110336465606));
#29499=CARTESIAN_POINT('Ctrl Pts',(0.190982575573689,1.75618239453565,5.35005933700346));
#29500=CARTESIAN_POINT('Ctrl Pts',(0.184628154248526,1.75265266327212,5.34969007810759));
#29501=CARTESIAN_POINT('Ctrl Pts',(0.178181758226575,1.74930243753846,5.34932081921173));
#29502=CARTESIAN_POINT('Ctrl Pts',(0.171654573189592,1.74613618791532,5.34895156031586));
#29503=CARTESIAN_POINT('Ctrl Pts',(0.153201023529593,1.73718461931027,5.34790759766831));
#29504=CARTESIAN_POINT('Ctrl Pts',(0.13399038571981,1.72965375922237,5.34686363502075));
#29505=CARTESIAN_POINT('Ctrl Pts',(0.114267098259657,1.72366514876334,5.3458196723732));
#29506=CARTESIAN_POINT('Ctrl Pts',(0.0945800939120914,1.71768755499856,
5.34477763020743));
#29507=CARTESIAN_POINT('Ctrl Pts',(0.0743829906899506,1.7132468475229,5.34373558804166));
#29508=CARTESIAN_POINT('Ctrl Pts',(0.0539396865298279,1.71041637583561,
5.34269354587589));
#29509=CARTESIAN_POINT('Ctrl Pts',(0.033518338157218,1.70758894403044,5.34165262284704));
#29510=CARTESIAN_POINT('Ctrl Pts',(0.0128520349393816,1.70636844385046,
5.34061169981818));
#29511=CARTESIAN_POINT('Ctrl Pts',(-0.00778579009651449,1.70677707153248,
5.33957077678933));
#29512=CARTESIAN_POINT('Ctrl Pts',(-0.0284342141814631,1.70718590907503,
5.33852931916954));
#29513=CARTESIAN_POINT('Ctrl Pts',(-0.0490533949124762,1.70922554752625,
5.33748786154975));
#29514=CARTESIAN_POINT('Ctrl Pts',(-0.069370012826302,1.71286605506559,
5.33644640392995));
#29515=CARTESIAN_POINT('Ctrl Pts',(-0.0896928383526334,1.7165076749387,
5.33540462809946));
#29516=CARTESIAN_POINT('Ctrl Pts',(-0.10971219977222,1.72175097237232,5.33436285226896));
#29517=CARTESIAN_POINT('Ctrl Pts',(-0.129165999502396,1.72851509509464,
5.33332107643846));
#29518=CARTESIAN_POINT('Ctrl Pts',(-0.148661849062148,1.73529383862171,
5.33227704878586));
#29519=CARTESIAN_POINT('Ctrl Pts',(-0.1675890219227,1.7435996744204,5.33123302113327));
#29520=CARTESIAN_POINT('Ctrl Pts',(-0.185705679522728,1.75330374880452,
5.33018899348067));
#29521=CARTESIAN_POINT('Ctrl Pts',(-0.19211330384717,1.75673595271556,5.3298197345848));
#29522=CARTESIAN_POINT('Ctrl Pts',(-0.19841978427341,1.76034266018519,5.32945047568894));
#29523=CARTESIAN_POINT('Ctrl Pts',(-0.204615306845539,1.764116886098,5.32908121679307));
#29524=CARTESIAN_POINT('Ctrl Pts',(-0.222131185866424,1.77478731522107,
5.32803725414552));
#29525=CARTESIAN_POINT('Ctrl Pts',(-0.238862333224376,1.78686337280658,
5.32699329149796));
#29526=CARTESIAN_POINT('Ctrl Pts',(-0.254574236000076,1.80020532298759,
5.32594932885041));
#29527=CARTESIAN_POINT('Ctrl Pts',(-0.270257235037567,1.81352272921356,
5.32490728668464));
#29528=CARTESIAN_POINT('Ctrl Pts',(-0.284924118303874,1.82810098002436,
5.32386524451887));
#29529=CARTESIAN_POINT('Ctrl Pts',(-0.298370359505342,1.84375789071924,
5.3228232023531));
#29530=CARTESIAN_POINT('Ctrl Pts',(-0.311802159654996,1.859397986138,5.32178227932425));
#29531=CARTESIAN_POINT('Ctrl Pts',(-0.324015421406848,1.87611390510052,
5.3207413562954));
#29532=CARTESIAN_POINT('Ctrl Pts',(-0.334843467529343,1.89368775544596,
5.31970043326654));
#29533=CARTESIAN_POINT('Ctrl Pts',(-0.345677074654112,1.9112706312629,5.31865897564675));
#29534=CARTESIAN_POINT('Ctrl Pts',(-0.355123645220509,1.92971170074283,
5.31761751802696));
#29535=CARTESIAN_POINT('Ctrl Pts',(-0.36306039367513,1.94876494935214,5.31657606040717));
#29536=CARTESIAN_POINT('Ctrl Pts',(-0.370999567152417,1.96782401955956,
5.31553428457667));
#29537=CARTESIAN_POINT('Ctrl Pts',(-0.377427750855548,1.98749494871666,
5.31449250874617));
#29538=CARTESIAN_POINT('Ctrl Pts',(-0.382271048664976,2.00751359368761,
5.31345073291567));
#29539=CARTESIAN_POINT('Ctrl Pts',(-0.387124815372529,2.02757550941396,
5.31240670526308));
#29540=CARTESIAN_POINT('Ctrl Pts',(-0.390386740583849,2.04798591422924,
5.31136267761048));
#29541=CARTESIAN_POINT('Ctrl Pts',(-0.392034255202344,2.06847171511256,
5.31031864995788));
#29542=CARTESIAN_POINT('Ctrl Pts',(-0.392616959527691,2.07571727436218,
5.30994939106201));
#29543=CARTESIAN_POINT('Ctrl Pts',(-0.39299818711695,2.08297225194062,5.30958013216615));
#29544=CARTESIAN_POINT('Ctrl Pts',(-0.393178498708552,2.09022461492885,
5.30921087327028));
#29545=CARTESIAN_POINT('Ctrl Pts',(-0.393258991358046,2.09346213231099,
5.30904603291468));
#29546=CARTESIAN_POINT('Ctrl Pts',(-0.393299497219904,2.09670064799264,
5.30888119255909));
#29547=CARTESIAN_POINT('Ctrl Pts',(-0.393299995348515,2.09993951150465,
5.3087163522035));
#29548=CARTESIAN_POINT('',(-0.393222743871143,2.09967523239219,5.18371635531477));
#29549=CARTESIAN_POINT('Ctrl Pts',(-0.393299995348526,2.09993951157533,
5.3087163521999));
#29550=CARTESIAN_POINT('Ctrl Pts',(-0.393303136849036,2.12036576904277,
5.30767676793465));
#29551=CARTESIAN_POINT('Ctrl Pts',(-0.391710695555704,2.14085529073421,
5.30663718366939));
#29552=CARTESIAN_POINT('Ctrl Pts',(-0.38851918392407,2.16113700780194,5.30559759940414));
#29553=CARTESIAN_POINT('Ctrl Pts',(-0.3853334959826,2.18138171593791,5.30455991211354));
#29554=CARTESIAN_POINT('Ctrl Pts',(-0.380554582847914,2.20141863733601,
5.30352222482293));
#29555=CARTESIAN_POINT('Ctrl Pts',(-0.374230820545827,2.22098009321205,
5.30248453753233));
#29556=CARTESIAN_POINT('Ctrl Pts',(-0.367913650014553,2.24052115859463,
5.30144793190743));
#29557=CARTESIAN_POINT('Ctrl Pts',(-0.360055026981877,2.25958703034488,
5.30041132628253));
#29558=CARTESIAN_POINT('Ctrl Pts',(-0.350753523762467,2.27792373525815,
5.29937472065763));
#29559=CARTESIAN_POINT('Ctrl Pts',(-0.341446999305944,2.29627033888791,
5.29833755544117));
#29560=CARTESIAN_POINT('Ctrl Pts',(-0.330696363142974,2.31388632122879,
5.29730039022472));
#29561=CARTESIAN_POINT('Ctrl Pts',(-0.318646999340026,2.33054062507853,
5.29626322500827));
#29562=CARTESIAN_POINT('Ctrl Pts',(-0.306593243899986,2.34720099892994,
5.29522568177574));
#29563=CARTESIAN_POINT('Ctrl Pts',(-0.293240286425889,2.36289841977707,
5.29418813854321));
#29564=CARTESIAN_POINT('Ctrl Pts',(-0.27877432215448,2.37743425763108,5.29315059531067));
#29565=CARTESIAN_POINT('Ctrl Pts',(-0.264277792181525,2.39200080882526,
5.29211085981248));
#29566=CARTESIAN_POINT('Ctrl Pts',(-0.248664130199837,2.40540040086757,
5.29107112431428));
#29567=CARTESIAN_POINT('Ctrl Pts',(-0.232153588232405,2.41747378076121,
5.29003138881609));
#29568=CARTESIAN_POINT('Ctrl Pts',(-0.228496742279588,2.42014785957025,
5.28980110245989));
#29569=CARTESIAN_POINT('Ctrl Pts',(-0.224796006455495,2.42275705217892,
5.28957081610369));
#29570=CARTESIAN_POINT('Ctrl Pts',(-0.221053944425669,2.42529992876398,
5.28934052974749));
#29571=CARTESIAN_POINT('Ctrl Pts',(-0.204089965106973,2.43682761201864,
5.28829656709993));
#29572=CARTESIAN_POINT('Ctrl Pts',(-0.186171281688737,2.44705909496488,
5.28725260445238));
#29573=CARTESIAN_POINT('Ctrl Pts',(-0.167522172214379,2.45583874411955,
5.28620864180483));
#29574=CARTESIAN_POINT('Ctrl Pts',(-0.148907369786457,2.46460224216353,
5.28516659963906));
#29575=CARTESIAN_POINT('Ctrl Pts',(-0.129565441336004,2.47191884419368,
5.28412455747329));
#29576=CARTESIAN_POINT('Ctrl Pts',(-0.109746893124813,2.47767778522101,
5.28308251530752));
#29577=CARTESIAN_POINT('Ctrl Pts',(-0.0899496297230533,2.48343054123616,
5.28204159227866));
#29578=CARTESIAN_POINT('Ctrl Pts',(-0.0696774576688189,2.48762872531793,
5.28100066924981));
#29579=CARTESIAN_POINT('Ctrl Pts',(-0.0491977201192234,2.49021080755801,
5.27995974622096));
#29580=CARTESIAN_POINT('Ctrl Pts',(-0.0287074647101889,2.49279421588822,
5.27891828860117));
#29581=CARTESIAN_POINT('Ctrl Pts',(-0.00801015882493114,2.49375975621462,
5.27787683098138));
#29582=CARTESIAN_POINT('Ctrl Pts',(0.0126194235258416,2.49309749445891,
5.27683537336158));
#29583=CARTESIAN_POINT('Ctrl Pts',(0.0332553091133903,2.49243503035337,
5.27579359753109));
#29584=CARTESIAN_POINT('Ctrl Pts',(0.0538226963536793,2.49014383378103,
5.27475182170059));
#29585=CARTESIAN_POINT('Ctrl Pts',(0.0740505465286713,2.48626597903363,
5.27371004587009));
#29586=CARTESIAN_POINT('Ctrl Pts',(0.0943221196608452,2.48237974221518,
5.2726660182175));
#29587=CARTESIAN_POINT('Ctrl Pts',(0.114251980371752,2.47690019544089,5.2716219905649));
#29588=CARTESIAN_POINT('Ctrl Pts',(0.133582189659656,2.4699198407841,5.2705779629123));
#29589=CARTESIAN_POINT('Ctrl Pts',(0.140419031309186,2.46745098083875,5.27020870401643));
#29590=CARTESIAN_POINT('Ctrl Pts',(0.147181045268516,2.46479481793859,5.26983944512057));
#29591=CARTESIAN_POINT('Ctrl Pts',(0.153857510090674,2.4619568435445,5.2694701862247));
#29592=CARTESIAN_POINT('Ctrl Pts',(0.17273310109213,2.4539333692415,5.26842622357715));
#29593=CARTESIAN_POINT('Ctrl Pts',(0.191035622246087,2.44440550599042,5.26738226092959));
#29594=CARTESIAN_POINT('Ctrl Pts',(0.208512808376046,2.43347758356917,5.26633829828204));
#29595=CARTESIAN_POINT('Ctrl Pts',(0.225957843338845,2.42256976423877,5.26529625611627));
#29596=CARTESIAN_POINT('Ctrl Pts',(0.242579908681752,2.41026733337383,5.2642542139505));
#29597=CARTESIAN_POINT('Ctrl Pts',(0.258150267652994,2.39672096203451,5.26321217178473));
#29598=CARTESIAN_POINT('Ctrl Pts',(0.273703904303309,2.3831891392852,5.26217124875588));
#29599=CARTESIAN_POINT('Ctrl Pts',(0.28820750567303,2.36841648696108,5.26113032572702));
#29600=CARTESIAN_POINT('Ctrl Pts',(0.30146461863205,2.3525944847241,5.26008940269817));
#29601=CARTESIAN_POINT('Ctrl Pts',(0.314728540098761,2.33676435671915,5.25904794507838));
#29602=CARTESIAN_POINT('Ctrl Pts',(0.326744209344882,2.31988435578319,5.25800648745858));
#29603=CARTESIAN_POINT('Ctrl Pts',(0.337354533482663,2.30218013932801,5.25696502983879));
#29604=CARTESIAN_POINT('Ctrl Pts',(0.347968099537041,2.28447051346287,5.25592325400829));
#29605=CARTESIAN_POINT('Ctrl Pts',(0.357175118778837,2.26593681992092,5.25488147817779));
#29606=CARTESIAN_POINT('Ctrl Pts',(0.364864249870397,2.24682972848341,5.2538397023473));
#29607=CARTESIAN_POINT('Ctrl Pts',(0.3725700011933,2.22768133663417,5.2527956746947));
#29608=CARTESIAN_POINT('Ctrl Pts',(0.378751093870111,2.20795777523849,5.2517516470421));
#29609=CARTESIAN_POINT('Ctrl Pts',(0.383345678257984,2.18792599707098,5.25070761938951));
#29610=CARTESIAN_POINT('Ctrl Pts',(0.384970722531286,2.18084101970479,5.25033836049364));
#29611=CARTESIAN_POINT('Ctrl Pts',(0.386397773545883,2.17371756832646,5.24996910159778));
#29612=CARTESIAN_POINT('Ctrl Pts',(0.387625644907437,2.16656763034759,5.24959984270191));
#29613=CARTESIAN_POINT('Ctrl Pts',(0.391097062527484,2.14635344386255,5.24855588005436));
#29614=CARTESIAN_POINT('Ctrl Pts',(0.392993349921659,2.12580675184556,5.24751191740681));
#29615=CARTESIAN_POINT('Ctrl Pts',(0.393265673737016,2.1051961389676,5.24646795475925));
#29616=CARTESIAN_POINT('Ctrl Pts',(0.393537496583371,2.08462344153295,5.24542591259349));
#29617=CARTESIAN_POINT('Ctrl Pts',(0.392191216756465,2.0639877832668,5.24438387042772));
#29618=CARTESIAN_POINT('Ctrl Pts',(0.389229701844604,2.04356305109274,5.24334182826195));
#29619=CARTESIAN_POINT('Ctrl Pts',(0.386271367553231,2.02316025476014,5.24230090523309));
#29620=CARTESIAN_POINT('Ctrl Pts',(0.381701318468743,2.00296866342249,5.24125998220424));
#29621=CARTESIAN_POINT('Ctrl Pts',(0.375574210490237,1.98325710978978,5.24021905917539));
#29622=CARTESIAN_POINT('Ctrl Pts',(0.369443955788769,1.96353543281689,5.23917760155559));
#29623=CARTESIAN_POINT('Ctrl Pts',(0.361755247648095,1.9442949934727,5.2381361439358));
#29624=CARTESIAN_POINT('Ctrl Pts',(0.35261278564167,1.92579003070426,5.23709468631601));
#29625=CARTESIAN_POINT('Ctrl Pts',(0.343467530214528,1.90727941386296,5.23605291048551));
#29626=CARTESIAN_POINT('Ctrl Pts',(0.332867994725971,1.88950536404161,5.23501113465502));
#29627=CARTESIAN_POINT('Ctrl Pts',(0.32096467573827,1.87269719111232,5.23396935882452));
#29628=CARTESIAN_POINT('Ctrl Pts',(0.309035627456456,1.85585268693583,5.23292533117192));
#29629=CARTESIAN_POINT('Ctrl Pts',(0.295797641047986,1.83997879337889,5.23188130351933));
#29630=CARTESIAN_POINT('Ctrl Pts',(0.281441694856146,1.82527202108904,5.23083727586673));
#29631=CARTESIAN_POINT('Ctrl Pts',(0.276364184862279,1.82007042850285,5.23046801697086));
#29632=CARTESIAN_POINT('Ctrl Pts',(0.271147147901713,1.81501448551558,5.230098758075));
#29633=CARTESIAN_POINT('Ctrl Pts',(0.265800020988035,1.81011167867132,5.22972949917913));
#29634=CARTESIAN_POINT('Ctrl Pts',(0.250682712151121,1.79625054419126,5.22868553653158));
#29635=CARTESIAN_POINT('Ctrl Pts',(0.234433180257581,1.78353381615442,5.22764157388402));
#29636=CARTESIAN_POINT('Ctrl Pts',(0.217250821731293,1.7721479442537,5.22659761123647));
#29637=CARTESIAN_POINT('Ctrl Pts',(0.20010007200502,1.76078301789123,5.2255555690707));
#29638=CARTESIAN_POINT('Ctrl Pts',(0.182020475470047,1.75074453939185,5.22451352690493));
#29639=CARTESIAN_POINT('Ctrl Pts',(0.16324387343287,1.74217835757653,5.22347148473916));
#29640=CARTESIAN_POINT('Ctrl Pts',(0.144487437171302,1.7336213757059,5.2224305617103));
#29641=CARTESIAN_POINT('Ctrl Pts',(0.125036135511626,1.72653388157008,5.22138963868145));
#29642=CARTESIAN_POINT('Ctrl Pts',(0.105145594035449,1.72101544351394,5.22034871565259));
#29643=CARTESIAN_POINT('Ctrl Pts',(0.085244837295583,1.71549417133185,5.2193072580328));
#29644=CARTESIAN_POINT('Ctrl Pts',(0.0649050947640875,1.71154377732843,
5.21826580041301));
#29645=CARTESIAN_POINT('Ctrl Pts',(0.0443968108705369,1.70921385236356,
5.21722434279322));
#29646=CARTESIAN_POINT('Ctrl Pts',(0.0238822608021649,1.70688321550505,
5.21618256696272));
#29647=CARTESIAN_POINT('Ctrl Pts',(0.00319980139753719,1.70617408039698,
5.21514079113222));
#29648=CARTESIAN_POINT('Ctrl Pts',(-0.0173762929887746,1.70708403641241,
5.21409901530172));
#29649=CARTESIAN_POINT('Ctrl Pts',(-0.0379968630700355,1.7079959593184,
5.21305498764912));
#29650=CARTESIAN_POINT('Ctrl Pts',(-0.0585098782231471,1.71053386990322,
5.21201095999652));
#29651=CARTESIAN_POINT('Ctrl Pts',(-0.0786467287493022,1.71464356492069,
5.21096693234393));
#29652=CARTESIAN_POINT('Ctrl Pts',(-0.0857688688315183,1.7160971101795,
5.21059767344806));
#29653=CARTESIAN_POINT('Ctrl Pts',(-0.0928440725913599,1.71774681496967,
5.21022841455219));
#29654=CARTESIAN_POINT('Ctrl Pts',(-0.0998609367825471,1.7195887970828,
5.20985915565633));
#29655=CARTESIAN_POINT('Ctrl Pts',(-0.119698899254308,1.72479641847012,
5.20881519300878));
#29656=CARTESIAN_POINT('Ctrl Pts',(-0.139187517097244,1.73157552116103,
5.20777123036122));
#29657=CARTESIAN_POINT('Ctrl Pts',(-0.158062083184193,1.73985937765996,
5.20672726771367));
#29658=CARTESIAN_POINT('Ctrl Pts',(-0.176901927472966,1.74812799511222,
5.2056852255479));
#29659=CARTESIAN_POINT('Ctrl Pts',(-0.195129272209971,1.75789563378735,
5.20464318338213));
#29660=CARTESIAN_POINT('Ctrl Pts',(-0.212495985206887,1.76904630796597,
5.20360114121636));
#29661=CARTESIAN_POINT('Ctrl Pts',(-0.229844046626877,1.78018500649571,
5.20256021818751));
#29662=CARTESIAN_POINT('Ctrl Pts',(-0.246332679644588,1.79270342055612,
5.20151929515866));
#29663=CARTESIAN_POINT('Ctrl Pts',(-0.261739790666748,1.80644051372554,
5.2004783721298));
#29664=CARTESIAN_POINT('Ctrl Pts',(-0.277154814379576,1.82018466190798,
5.19943691451001));
#29665=CARTESIAN_POINT('Ctrl Pts',(-0.291486646535155,1.83514826194588,
5.19839545689022));
#29666=CARTESIAN_POINT('Ctrl Pts',(-0.304547193794242,1.85113076374921,
5.19735399927043));
#29667=CARTESIAN_POINT('Ctrl Pts',(-0.31761173161991,1.86711814890362,5.19631222343993));
#29668=CARTESIAN_POINT('Ctrl Pts',(-0.329403774099449,1.88412446343047,
5.19527044760943));
#29669=CARTESIAN_POINT('Ctrl Pts',(-0.339776878467228,1.90191778762578,
5.19422867177894));
#29670=CARTESIAN_POINT('Ctrl Pts',(-0.35017240453549,1.91974957249511,5.19318464412634));
#29671=CARTESIAN_POINT('Ctrl Pts',(-0.359142549625092,1.93837109976543,
5.19214061647374));
#29672=CARTESIAN_POINT('Ctrl Pts',(-0.366587485512455,1.95752717639614,
5.19109658882115));
#29673=CARTESIAN_POINT('Ctrl Pts',(-0.369220661749444,1.96430242960733,
5.19072732992528));
#29674=CARTESIAN_POINT('Ctrl Pts',(-0.37166349606096,1.97114440261701,5.19035807102941));
#29675=CARTESIAN_POINT('Ctrl Pts',(-0.373913079894079,1.97804140586197,
5.18998881213354));
#29676=CARTESIAN_POINT('Ctrl Pts',(-0.381478973819856,2.00123769407711,
5.18874690525452));
#29677=CARTESIAN_POINT('Ctrl Pts',(-0.386891989129394,2.02516888945576,
5.1875049983755));
#29678=CARTESIAN_POINT('Ctrl Pts',(-0.390039890821214,2.04946512522846,
5.18626309149648));
#29679=CARTESIAN_POINT('Ctrl Pts',(-0.392191654911472,2.06607293982444,
5.18541417978088));
#29680=CARTESIAN_POINT('Ctrl Pts',(-0.393285969585091,2.08285087349683,
5.18456526806529));
#29681=CARTESIAN_POINT('Ctrl Pts',(-0.393299865841963,2.09967514819741,
5.1837163563497));
#29682=CARTESIAN_POINT('',(-0.393112574114025,2.1002161969804,5.05871634925479));
#29683=CARTESIAN_POINT('Ctrl Pts',(-0.392990894347882,2.09967548550446,
5.1837163522035));
#29684=CARTESIAN_POINT('Ctrl Pts',(-0.392294416640166,2.1894360675245,5.17918372433925));
#29685=CARTESIAN_POINT('Ctrl Pts',(-0.317199300604699,2.41141571974295,
5.16802764863407));
#29686=CARTESIAN_POINT('Ctrl Pts',(0.0517462396427426,2.56216593358049,
5.15024812508798));
#29687=CARTESIAN_POINT('Ctrl Pts',(0.416608566264656,2.30666960587948,5.13037778156518));
#29688=CARTESIAN_POINT('Ctrl Pts',(0.399289249473655,1.86158205031028,5.11050743804239));
#29689=CARTESIAN_POINT('Ctrl Pts',(0.015676404613339,1.63521050590846,5.0906370945196));
#29690=CARTESIAN_POINT('Ctrl Pts',(-0.330107445811104,1.80898222584714,
5.07337339923997));
#29691=CARTESIAN_POINT('Ctrl Pts',(-0.39237518151986,2.02055869281699,5.06273315180127));
#29692=CARTESIAN_POINT('Ctrl Pts',(-0.392771469173745,2.100215950882,5.0587163522035));
#29693=CARTESIAN_POINT('',(-0.393299933199252,2.10022922797308,4.93371635220805));
#29694=CARTESIAN_POINT('Ctrl Pts',(-0.393299940503932,2.1002163321604,5.05871634763509));
#29695=CARTESIAN_POINT('Ctrl Pts',(-0.393287312904279,2.12317377955501,
5.05756024661416));
#29696=CARTESIAN_POINT('Ctrl Pts',(-0.391260460548536,2.14605889974054,
5.05640414559323));
#29697=CARTESIAN_POINT('Ctrl Pts',(-0.387281563959997,2.16854108415176,
5.0552480445723));
#29698=CARTESIAN_POINT('Ctrl Pts',(-0.383271022275013,2.19120207464103,
5.05408274880919));
#29699=CARTESIAN_POINT('Ctrl Pts',(-0.377277462436426,2.2134532889445,5.05291745304608));
#29700=CARTESIAN_POINT('Ctrl Pts',(-0.369413741228829,2.23497547107278,
5.05175215728296));
#29701=CARTESIAN_POINT('Ctrl Pts',(-0.367488799900917,2.24024383407191,
5.05146690734665));
#29702=CARTESIAN_POINT('Ctrl Pts',(-0.365452017723983,2.2454686187123,5.05118165741033));
#29703=CARTESIAN_POINT('Ctrl Pts',(-0.363305472136611,2.25064535809508,
5.05089640747402));
#29704=CARTESIAN_POINT('Ctrl Pts',(-0.355449507492256,2.26959127836966,
5.04985244482647));
#29705=CARTESIAN_POINT('Ctrl Pts',(-0.346084136819551,2.28797747675009,
5.04880848217892));
#29706=CARTESIAN_POINT('Ctrl Pts',(-0.335311451306619,2.30555077383131,
5.04776451953136));
#29707=CARTESIAN_POINT('Ctrl Pts',(-0.32455858330951,2.32309174293891,5.04672247736559));
#29708=CARTESIAN_POINT('Ctrl Pts',(-0.312403868846199,2.33982212780493,
5.04568043519982));
#29709=CARTESIAN_POINT('Ctrl Pts',(-0.298995946977492,2.35551186604742,
5.04463839303406));
#29710=CARTESIAN_POINT('Ctrl Pts',(-0.285602425006236,2.37118475375752,
5.0435974700052));
#29711=CARTESIAN_POINT('Ctrl Pts',(-0.270958821209181,2.3858186383141,5.04255654697635));
#29712=CARTESIAN_POINT('Ctrl Pts',(-0.255254867607614,2.3992153782188,5.0415156239475));
#29713=CARTESIAN_POINT('Ctrl Pts',(-0.239542848864775,2.41261899833995,
5.04047416632771));
#29714=CARTESIAN_POINT('Ctrl Pts',(-0.222769941696439,2.42478371470128,
5.03943270870791));
#29715=CARTESIAN_POINT('Ctrl Pts',(-0.205160403175313,2.43555044176538,
5.03839125108812));
#29716=CARTESIAN_POINT('Ctrl Pts',(-0.187545484172456,2.44632045853399,
5.03734947525763));
#29717=CARTESIAN_POINT('Ctrl Pts',(-0.169094071009059,2.45569128303871,
5.03630769942713));
#29718=CARTESIAN_POINT('Ctrl Pts',(-0.150055837400931,2.46354935794457,
5.03526592359663));
#29719=CARTESIAN_POINT('Ctrl Pts',(-0.130976452218827,2.47142441825765,
5.03422189594403));
#29720=CARTESIAN_POINT('Ctrl Pts',(-0.111308415039399,2.47777997443441,
5.03317786829144));
#29721=CARTESIAN_POINT('Ctrl Pts',(-0.091318120317115,2.48255181466273,
5.03213384063884));
#29722=CARTESIAN_POINT('Ctrl Pts',(-0.0842478151016081,2.4842395520034,
5.03176458174297));
#29723=CARTESIAN_POINT('Ctrl Pts',(-0.0771372836124449,2.48572964464515,
5.0313953228471));
#29724=CARTESIAN_POINT('Ctrl Pts',(-0.0699985022821658,2.48702080005893,
5.03102606395123));
#29725=CARTESIAN_POINT('Ctrl Pts',(-0.049815857689946,2.49067113330545,
5.02998210130367));
#29726=CARTESIAN_POINT('Ctrl Pts',(-0.0292867685314287,2.49274934336349,
5.02893813865612));
#29727=CARTESIAN_POINT('Ctrl Pts',(-0.00867937638820636,2.4932042197453,
5.02789417600856));
#29728=CARTESIAN_POINT('Ctrl Pts',(0.0118901062365955,2.49365825933299,
5.02685213384279));
#29729=CARTESIAN_POINT('Ctrl Pts',(0.0325368799399694,2.49249481741639,
5.02581009167702));
#29730=CARTESIAN_POINT('Ctrl Pts',(0.0529870431427076,2.48971433545482,
5.02476804951125));
#29731=CARTESIAN_POINT('Ctrl Pts',(0.0734152431914291,2.48693683968719,
5.02372712648239));
#29732=CARTESIAN_POINT('Ctrl Pts',(0.0936465226658073,2.48254582155789,
5.02268620345354));
#29733=CARTESIAN_POINT('Ctrl Pts',(0.113411575275055,2.47659355357418,5.02164528042468));
#29734=CARTESIAN_POINT('Ctrl Pts',(0.133186778700184,2.47063822866078,5.02060382280489));
#29735=CARTESIAN_POINT('Ctrl Pts',(0.152494567736001,2.46312024877389,5.01956236518509));
#29736=CARTESIAN_POINT('Ctrl Pts',(0.171079786008797,2.45414205739955,5.0185209075653));
#29737=CARTESIAN_POINT('Ctrl Pts',(0.189670682876021,2.44516112279632,5.0174791317348));
#29738=CARTESIAN_POINT('Ctrl Pts',(0.207537923239685,2.43471944087176,5.0164373559043));
#29739=CARTESIAN_POINT('Ctrl Pts',(0.224450873165666,2.42296547111908,5.0153955800738));
#29740=CARTESIAN_POINT('Ctrl Pts',(0.241400380816714,2.41118609489405,5.0143515524212));
#29741=CARTESIAN_POINT('Ctrl Pts',(0.257390910146576,2.39808923448553,5.0133075247686));
#29742=CARTESIAN_POINT('Ctrl Pts',(0.27222426658229,2.38386412010632,5.01226349711601));
#29743=CARTESIAN_POINT('Ctrl Pts',(0.27747063032145,2.37883288360985,5.01189423822015));
#29744=CARTESIAN_POINT('Ctrl Pts',(0.282572586067836,2.37366083549554,5.0115249793243));
#29745=CARTESIAN_POINT('Ctrl Pts',(0.287522563980542,2.36835734609296,5.01115572042844));
#29746=CARTESIAN_POINT('Ctrl Pts',(0.301517059726161,2.35336340850572,5.01011175778089));
#29747=CARTESIAN_POINT('Ctrl Pts',(0.314377222850617,2.33722715543588,5.00906779513334));
#29748=CARTESIAN_POINT('Ctrl Pts',(0.325914844775779,2.32014632396381,5.00802383248578));
#29749=CARTESIAN_POINT('Ctrl Pts',(0.33743124200216,2.3030969145218,5.00698179032001));
#29750=CARTESIAN_POINT('Ctrl Pts',(0.347629470877126,2.28510694539278,5.00593974815425));
#29751=CARTESIAN_POINT('Ctrl Pts',(0.356361634713657,2.26640695689847,5.00489770598848));
#29752=CARTESIAN_POINT('Ctrl Pts',(0.365084420343407,2.24772705189804,5.00385678295962));
#29753=CARTESIAN_POINT('Ctrl Pts',(0.372343930817319,2.22833929243338,5.00281585993077));
#29754=CARTESIAN_POINT('Ctrl Pts',(0.378038337434165,2.20849841210825,5.00177493690192));
#29755=CARTESIAN_POINT('Ctrl Pts',(0.383735668549835,2.18864734202411,5.00073347928213));
#29756=CARTESIAN_POINT('Ctrl Pts',(0.38786607153086,2.16834338895473,4.99969202166234));
#29757=CARTESIAN_POINT('Ctrl Pts',(0.390377561939004,2.14785654745758,4.99865056404255));
#29758=CARTESIAN_POINT('Ctrl Pts',(0.392889819716959,2.1273634463372,4.99760878821205));
#29759=CARTESIAN_POINT('Ctrl Pts',(0.393782126652338,2.10668807964256,4.99656701238155));
#29760=CARTESIAN_POINT('Ctrl Pts',(0.393054463829288,2.08610473232102,4.99552523655106));
#29761=CARTESIAN_POINT('Ctrl Pts',(0.392325228146534,2.06547689362714,4.99448120889846));
#29762=CARTESIAN_POINT('Ctrl Pts',(0.389969115880667,2.04494220308168,4.99343718124586));
#29763=CARTESIAN_POINT('Ctrl Pts',(0.386037948879175,2.0247697399635,4.99239315359327));
#29764=CARTESIAN_POINT('Ctrl Pts',(0.384647546639489,2.01763500417414,4.99202389469739));
#29765=CARTESIAN_POINT('Ctrl Pts',(0.383060576814579,2.0105454653376,4.99165463580152));
#29766=CARTESIAN_POINT('Ctrl Pts',(0.381280820453666,2.00351256064037,4.99128537690565));
#29767=CARTESIAN_POINT('Ctrl Pts',(0.376249122684712,1.98362924871547,4.9902414142581));
#29768=CARTESIAN_POINT('Ctrl Pts',(0.369642910861621,1.96408134795691,4.98919745161055));
#29769=CARTESIAN_POINT('Ctrl Pts',(0.361526565157871,1.94513414616142,4.988153488963));
#29770=CARTESIAN_POINT('Ctrl Pts',(0.35342515034663,1.92622179978531,4.98711144679724));
#29771=CARTESIAN_POINT('Ctrl Pts',(0.343819347764002,1.90790865100664,4.98606940463148));
#29772=CARTESIAN_POINT('Ctrl Pts',(0.332822940691177,1.8904438496496,4.98502736246571));
#29773=CARTESIAN_POINT('Ctrl Pts',(0.3218383435868,1.87299780521486,4.98398643943686));
#29774=CARTESIAN_POINT('Ctrl Pts',(0.309466472493654,1.85639893431858,4.98294551640801));
#29775=CARTESIAN_POINT('Ctrl Pts',(0.295866390270717,1.84087074825837,4.98190459337916));
#29776=CARTESIAN_POINT('Ctrl Pts',(0.282259323400011,1.82533458732652,4.98086313575938));
#29777=CARTESIAN_POINT('Ctrl Pts',(0.267423257894862,1.81087077388217,4.97982167813959));
#29778=CARTESIAN_POINT('Ctrl Pts',(0.251557069897546,1.79766917030418,4.9787802205198));
#29779=CARTESIAN_POINT('Ctrl Pts',(0.235686034088089,1.78446353306076,4.97773844468931));
#29780=CARTESIAN_POINT('Ctrl Pts',(0.218784837458711,1.77252131584131,4.97669666885882));
#29781=CARTESIAN_POINT('Ctrl Pts',(0.201084093464547,1.76199100994864,4.97565489302832));
#29782=CARTESIAN_POINT('Ctrl Pts',(0.183345088910557,1.75143794256081,4.97461086537573));
#29783=CARTESIAN_POINT('Ctrl Pts',(0.164803747297285,1.7423032049081,4.97356683772314));
#29784=CARTESIAN_POINT('Ctrl Pts',(0.145714367402498,1.73468888172889,4.97252281007055));
#29785=CARTESIAN_POINT('Ctrl Pts',(0.138962703952014,1.73199579542684,4.97215355117465));
#29786=CARTESIAN_POINT('Ctrl Pts',(0.132142637323045,1.72949245259711,4.97178429227876));
#29787=CARTESIAN_POINT('Ctrl Pts',(0.125265830857022,1.72718186522153,4.97141503338286));
#29788=CARTESIAN_POINT('Ctrl Pts',(0.105823837272394,1.72064941078139,4.97037107073529));
#29789=CARTESIAN_POINT('Ctrl Pts',(0.0858115504945747,1.71562240007358,
4.96932710808772));
#29790=CARTESIAN_POINT('Ctrl Pts',(0.065486879404064,1.71219030617335,4.96828314544015));
#29791=CARTESIAN_POINT('Ctrl Pts',(0.0451995977361308,1.70876452597968,
4.96724110327437));
#29792=CARTESIAN_POINT('Ctrl Pts',(0.0246017798531759,1.7069280184457,4.96619906110858));
#29793=CARTESIAN_POINT('Ctrl Pts',(0.0039645083343114,1.70671998185305,
4.9651570189428));
#29794=CARTESIAN_POINT('Ctrl Pts',(-0.0166505990791454,1.70651216868843,
4.96411609591393));
#29795=CARTESIAN_POINT('Ctrl Pts',(-0.0373043442899069,1.70792939067573,
4.96307517288506));
#29796=CARTESIAN_POINT('Ctrl Pts',(-0.0577226913974393,1.7109588956192,
4.96203424985619));
#29797=CARTESIAN_POINT('Ctrl Pts',(-0.0781515248358711,1.71398995643744,
4.96099279223638));
#29798=CARTESIAN_POINT('Ctrl Pts',(-0.098343988474489,1.71863486238312,
4.95995133461658));
#29799=CARTESIAN_POINT('Ctrl Pts',(-0.118032787376494,1.72482917077132,
4.95890987699677));
#29800=CARTESIAN_POINT('Ctrl Pts',(-0.137727602064921,1.73102537179078,
4.95786810116626));
#29801=CARTESIAN_POINT('Ctrl Pts',(-0.156917755242051,1.73877166255961,
4.95682632533574));
#29802=CARTESIAN_POINT('Ctrl Pts',(-0.175353557531653,1.747954520181,4.95578454950523));
#29803=CARTESIAN_POINT('Ctrl Pts',(-0.193829209226259,1.75715722675752,
4.95474052185262));
#29804=CARTESIAN_POINT('Ctrl Pts',(-0.211546623432728,1.76780232021209,
4.95369649420001));
#29805=CARTESIAN_POINT('Ctrl Pts',(-0.22828230895195,1.77973124189274,4.95265246654739));
#29806=CARTESIAN_POINT('Ctrl Pts',(-0.234201501551311,1.78395034512872,
4.95228320765162));
#29807=CARTESIAN_POINT('Ctrl Pts',(-0.239998182318464,1.78832967455179,
4.95191394875585));
#29808=CARTESIAN_POINT('Ctrl Pts',(-0.245663505147719,1.79286105385585,
4.95154468986007));
#29809=CARTESIAN_POINT('Ctrl Pts',(-0.261477141913282,1.8055095098258,4.95051397612562));
#29810=CARTESIAN_POINT('Ctrl Pts',(-0.276364208224235,1.81942499701367,
4.94948326239116));
#29811=CARTESIAN_POINT('Ctrl Pts',(-0.290112689812862,1.83444488856445,
4.9484525486567));
#29812=CARTESIAN_POINT('Ctrl Pts',(-0.303835828818759,1.84943709394192,
4.94742373483737));
#29813=CARTESIAN_POINT('Ctrl Pts',(-0.31642399524006,1.86552915697693,4.94639492101804));
#29814=CARTESIAN_POINT('Ctrl Pts',(-0.327699970669064,1.88251984177058,
4.94536610719871));
#29815=CARTESIAN_POINT('Ctrl Pts',(-0.338972373206054,1.89950514291628,
4.94433761936808));
#29816=CARTESIAN_POINT('Ctrl Pts',(-0.348932950714574,1.91738790085643,
4.94330913153746));
#29817=CARTESIAN_POINT('Ctrl Pts',(-0.357446176121318,1.93593561880698,
4.94228064370684));
#29818=CARTESIAN_POINT('Ctrl Pts',(-0.365956920978892,1.95447793239853,
4.94125245555284));
#29819=CARTESIAN_POINT('Ctrl Pts',(-0.373020843267589,1.97368413017175,
4.94022426739884));
#29820=CARTESIAN_POINT('Ctrl Pts',(-0.378549904924822,1.9933001430113,4.93919607924483));
#29821=CARTESIAN_POINT('Ctrl Pts',(-0.384089670934554,2.01295413276793,
4.93816590050199));
#29822=CARTESIAN_POINT('Ctrl Pts',(-0.388088463864271,2.0330187842476,4.93713572175915));
#29823=CARTESIAN_POINT('Ctrl Pts',(-0.390508923268107,2.05322745625922,
4.93610554301631));
#29824=CARTESIAN_POINT('Ctrl Pts',(-0.392380099961015,2.06885010872049,
4.93530914608023));
#29825=CARTESIAN_POINT('Ctrl Pts',(-0.393309066605004,2.08455850583689,
4.93451274914414));
#29826=CARTESIAN_POINT('Ctrl Pts',(-0.393299933199252,2.10022922797308,
4.93371635220805));
#29827=CARTESIAN_POINT('',(-0.393315750863,2.09965835142492,4.80871634439493));
#29828=CARTESIAN_POINT('Ctrl Pts',(-0.3932999331992,2.10022922806266,4.9337163522035));
#29829=CARTESIAN_POINT('Ctrl Pts',(-0.39329212701003,2.11362276131211,4.93303568358143));
#29830=CARTESIAN_POINT('Ctrl Pts',(-0.39260021454605,2.12699611331515,4.93235501495935));
#29831=CARTESIAN_POINT('Ctrl Pts',(-0.391230019245934,2.14029841238592,
4.93167434633727));
#29832=CARTESIAN_POINT('Ctrl Pts',(-0.389128508074786,2.16070056242748,
4.93063038368973));
#29833=CARTESIAN_POINT('Ctrl Pts',(-0.385420519122019,2.1809986726012,4.9295864210422));
#29834=CARTESIAN_POINT('Ctrl Pts',(-0.380131366312023,2.20092093115779,
4.92854245839467));
#29835=CARTESIAN_POINT('Ctrl Pts',(-0.374851943468561,2.22080654057301,
4.92750041622893));
#29836=CARTESIAN_POINT('Ctrl Pts',(-0.367997259653949,2.24031695244025,
4.92645837406319));
#29837=CARTESIAN_POINT('Ctrl Pts',(-0.359643847175506,2.25918917421986,
4.92541633189744));
#29838=CARTESIAN_POINT('Ctrl Pts',(-0.351299406130838,2.27804112752976,
4.92437540886862));
#29839=CARTESIAN_POINT('Ctrl Pts',(-0.341459701736896,2.29625557033757,
4.9233344858398));
#29840=CARTESIAN_POINT('Ctrl Pts',(-0.330249779338624,2.31358832656957,
4.92229356281097));
#29841=CARTESIAN_POINT('Ctrl Pts',(-0.319034099816375,2.33092998445343,
4.92125210519121));
#29842=CARTESIAN_POINT('Ctrl Pts',(-0.306447182478844,2.34738842456622,
4.92021064757146));
#29843=CARTESIAN_POINT('Ctrl Pts',(-0.292658336096874,2.36274700438446,
4.9191691899517));
#29844=CARTESIAN_POINT('Ctrl Pts',(-0.278865276621196,2.37811027691841,
4.91812741412124));
#29845=CARTESIAN_POINT('Ctrl Pts',(-0.263870075060144,2.39237249728365,
4.91708563829077));
#29846=CARTESIAN_POINT('Ctrl Pts',(-0.247879430081077,2.40535336602481,
4.91604386246031));
#29847=CARTESIAN_POINT('Ctrl Pts',(-0.231854220960001,2.41836229320834,
4.91499983480774));
#29848=CARTESIAN_POINT('Ctrl Pts',(-0.214829879308957,2.43008392159923,
4.91395580715518));
#29849=CARTESIAN_POINT('Ctrl Pts',(-0.197043255114176,2.44038044246697,
4.91291177950261));
#29850=CARTESIAN_POINT('Ctrl Pts',(-0.190752359276096,2.44402218693541,
4.91254252060658));
#29851=CARTESIAN_POINT('Ctrl Pts',(-0.184366323275313,2.4474860833518,4.91217326171054));
#29852=CARTESIAN_POINT('Ctrl Pts',(-0.177896251843067,2.45076746368526,
4.91180400281451));
#29853=CARTESIAN_POINT('Ctrl Pts',(-0.159604172828913,2.46004452792847,
4.91076004016685));
#29854=CARTESIAN_POINT('Ctrl Pts',(-0.14052995694789,2.46791451822913,4.90971607751919));
#29855=CARTESIAN_POINT('Ctrl Pts',(-0.120915851270176,2.47425158237689,
4.90867211487152));
#29856=CARTESIAN_POINT('Ctrl Pts',(-0.101337827853386,2.4805769888123,4.90763007270564));
#29857=CARTESIAN_POINT('Ctrl Pts',(-0.0812225600257416,2.48537478640656,
4.90658803053976));
#29858=CARTESIAN_POINT('Ctrl Pts',(-0.0608326049441621,2.48856696228026,
4.90554598837388));
#29859=CARTESIAN_POINT('Ctrl Pts',(-0.0404645483540277,2.49175570980721,
4.90450506534491));
#29860=CARTESIAN_POINT('Ctrl Pts',(-0.0198231089396549,2.49334211718406,
4.90346414231595));
#29861=CARTESIAN_POINT('Ctrl Pts',(0.000818716379649284,2.49329914785503,
4.90242321928698));
#29862=CARTESIAN_POINT('Ctrl Pts',(0.0214711428024116,2.49325615645806,
4.90138176166708));
#29863=CARTESIAN_POINT('Ctrl Pts',(0.0421232197158089,2.49158210201624,
4.90034030404717));
#29864=CARTESIAN_POINT('Ctrl Pts',(0.0625011403103141,2.48830206986303,
4.89929884642727));
#29865=CARTESIAN_POINT('Ctrl Pts',(0.0828852872479474,2.485021035517,4.89825707059666));
#29866=CARTESIAN_POINT('Ctrl Pts',(0.10299439104046,2.48013319914792,4.89721529476605));
#29867=CARTESIAN_POINT('Ctrl Pts',(0.122564962954127,2.47371475734316,4.89617351893544));
#29868=CARTESIAN_POINT('Ctrl Pts',(0.142177837103041,2.46728244193079,4.89512949128274));
#29869=CARTESIAN_POINT('Ctrl Pts',(0.161249175870259,2.45931319990156,4.89408546363003));
#29870=CARTESIAN_POINT('Ctrl Pts',(0.179534896030575,2.44993158060868,4.89304143597733));
#29871=CARTESIAN_POINT('Ctrl Pts',(0.186002315554453,2.44661342484296,4.89267217708212));
#29872=CARTESIAN_POINT('Ctrl Pts',(0.19237169834148,2.44311900116171,4.8923029181869));
#29873=CARTESIAN_POINT('Ctrl Pts',(0.198633108236113,2.43945511973229,4.89193365929169));
#29874=CARTESIAN_POINT('Ctrl Pts',(0.216335262835472,2.42909665469184,4.89088969664426));
#29875=CARTESIAN_POINT('Ctrl Pts',(0.233277709289957,2.41731888042127,4.88984573399683));
#29876=CARTESIAN_POINT('Ctrl Pts',(0.249223496091635,2.40425735651889,4.88880177134941));
#29877=CARTESIAN_POINT('Ctrl Pts',(0.265139948900249,2.39121986069718,4.88775972918376));
#29878=CARTESIAN_POINT('Ctrl Pts',(0.280062780951827,2.37690371788836,4.88671768701811));
#29879=CARTESIAN_POINT('Ctrl Pts',(0.293784270687491,2.36148746106959,4.88567564485247));
#29880=CARTESIAN_POINT('Ctrl Pts',(0.307491023758754,2.34608776106844,4.88463472182374));
#29881=CARTESIAN_POINT('Ctrl Pts',(0.319998487605928,2.32959082021855,4.88359379879501));
#29882=CARTESIAN_POINT('Ctrl Pts',(0.331136151243724,2.31221154384127,4.88255287576628));
#29883=CARTESIAN_POINT('Ctrl Pts',(0.342279534895317,2.29482334192054,4.88151141814661));
#29884=CARTESIAN_POINT('Ctrl Pts',(0.352051302340476,2.27655250997617,4.88046996052694));
#29885=CARTESIAN_POINT('Ctrl Pts',(0.360324329203391,2.25764284882013,4.87942850290727));
#29886=CARTESIAN_POINT('Ctrl Pts',(0.368599883836701,2.23872740993818,4.87838672707689));
#29887=CARTESIAN_POINT('Ctrl Pts',(0.375375524736701,2.21917344128914,4.87734495124651));
#29888=CARTESIAN_POINT('Ctrl Pts',(0.380572688145833,2.19924373550736,4.87630317541613));
#29889=CARTESIAN_POINT('Ctrl Pts',(0.385781085341637,2.17927095121417,4.87525914776365));
#29890=CARTESIAN_POINT('Ctrl Pts',(0.389404064233882,2.15892153341763,4.87421512011117));
#29891=CARTESIAN_POINT('Ctrl Pts',(0.391414221488676,2.1384681324789,4.87317109245868));
#29892=CARTESIAN_POINT('Ctrl Pts',(0.392125187762522,2.13123403265003,4.87280183356209));
#29893=CARTESIAN_POINT('Ctrl Pts',(0.392634875758463,2.12398694685707,4.87243257466551));
#29894=CARTESIAN_POINT('Ctrl Pts',(0.392943632966605,2.11673891606425,4.87206331576891));
#29895=CARTESIAN_POINT('Ctrl Pts',(0.393816546240716,2.09624740324003,4.87101935312151));
#29896=CARTESIAN_POINT('Ctrl Pts',(0.393084835156576,2.07562636889449,4.86997539047411));
#29897=CARTESIAN_POINT('Ctrl Pts',(0.390734214518835,2.05514842695792,4.8689314278267));
#29898=CARTESIAN_POINT('Ctrl Pts',(0.388387918101057,2.03470815640222,4.86788938566109));
#29899=CARTESIAN_POINT('Ctrl Pts',(0.384428647533905,2.01441118525129,4.86684734349547));
#29900=CARTESIAN_POINT('Ctrl Pts',(0.378894073107929,1.99452881263737,4.86580530132985));
#29901=CARTESIAN_POINT('Ctrl Pts',(0.373365442727952,1.97466779337933,4.86476437830115));
#29902=CARTESIAN_POINT('Ctrl Pts',(0.36626503567026,1.955221201676,4.86372345527245));
#29903=CARTESIAN_POINT('Ctrl Pts',(0.357681247499471,1.93644873835026,4.86268253224375));
#29904=CARTESIAN_POINT('Ctrl Pts',(0.349093050918806,1.91766663397664,4.86164107462411));
#29905=CARTESIAN_POINT('Ctrl Pts',(0.339020242575313,1.89956002548728,4.86059961700448));
#29906=CARTESIAN_POINT('Ctrl Pts',(0.32759899983515,1.88236777511818,4.85955815938484));
#29907=CARTESIAN_POINT('Ctrl Pts',(0.316174267407413,1.86517027176709,4.8585163835545));
#29908=CARTESIAN_POINT('Ctrl Pts',(0.303400717313503,1.84888827503743,4.85747460772415));
#29909=CARTESIAN_POINT('Ctrl Pts',(0.289456782323964,1.83373009714454,4.85643283189381));
#29910=CARTESIAN_POINT('Ctrl Pts',(0.275482707202496,1.81853915450612,4.85538880424137));
#29911=CARTESIAN_POINT('Ctrl Pts',(0.260333736313617,1.80447738144244,4.85434477658892));
#29912=CARTESIAN_POINT('Ctrl Pts',(0.244224285042832,1.79171540973426,4.85330074893648));
#29913=CARTESIAN_POINT('Ctrl Pts',(0.238526583272011,1.78720166760992,4.85293149003969));
#29914=CARTESIAN_POINT('Ctrl Pts',(0.232709007101227,1.78285013432857,4.8525622311429));
#29915=CARTESIAN_POINT('Ctrl Pts',(0.2267818688915,1.77866703570583,4.85219297224612));
#29916=CARTESIAN_POINT('Ctrl Pts',(0.210024761733678,1.7668406484355,4.85114900959779));
#29917=CARTESIAN_POINT('Ctrl Pts',(0.192290138401755,1.75629334571834,4.85010504694946));
#29918=CARTESIAN_POINT('Ctrl Pts',(0.173799484735446,1.74718470964867,4.84906108430113));
#29919=CARTESIAN_POINT('Ctrl Pts',(0.155342846618986,1.73809282989653,4.84801904213458));
#29920=CARTESIAN_POINT('Ctrl Pts',(0.136133565155466,1.73043473824831,4.84697699996803));
#29921=CARTESIAN_POINT('Ctrl Pts',(0.116420145122099,1.72432561997156,4.84593495780148));
#29922=CARTESIAN_POINT('Ctrl Pts',(0.0967278969921625,1.71822306279188,
4.84489403477185));
#29923=CARTESIAN_POINT('Ctrl Pts',(0.0765332758542779,1.71366642071083,
4.84385311174222));
#29924=CARTESIAN_POINT('Ctrl Pts',(0.0561024929268396,1.71072194990291,
4.84281218871259));
#29925=CARTESIAN_POINT('Ctrl Pts',(0.0356612172819931,1.70777596689155,
4.84177073109203));
#29926=CARTESIAN_POINT('Ctrl Pts',(0.0149842634987702,1.70644393016169,
4.84072927347147));
#29927=CARTESIAN_POINT('Ctrl Pts',(-0.005653813508861,1.70674063978996,
4.83968781585091));
#29928=CARTESIAN_POINT('Ctrl Pts',(-0.0262981963486536,1.70703744007596,
4.83864604001965));
#29929=CARTESIAN_POINT('Ctrl Pts',(-0.0469029442032106,1.70896393068438,
4.83760426418839));
#29930=CARTESIAN_POINT('Ctrl Pts',(-0.0671963155490089,1.71248284531309,
4.83656248835713));
#29931=CARTESIAN_POINT('Ctrl Pts',(-0.087533551477086,1.71600936615556,
4.83551846070379));
#29932=CARTESIAN_POINT('Ctrl Pts',(-0.107557353716536,1.72113500029117,
4.83447443305045));
#29933=CARTESIAN_POINT('Ctrl Pts',(-0.127008185088199,1.72777182949083,
4.83343040539711));
#29934=CARTESIAN_POINT('Ctrl Pts',(-0.133887689096931,1.73011918895388,
4.83306114650585));
#29935=CARTESIAN_POINT('Ctrl Pts',(-0.140695695187009,1.73265514753066,
4.83269188761459));
#29936=CARTESIAN_POINT('Ctrl Pts',(-0.147421386314326,1.73537440455014,
4.83232262872333));
#29937=CARTESIAN_POINT('Ctrl Pts',(-0.166436149329981,1.7430622431418,4.83127866607684));
#29938=CARTESIAN_POINT('Ctrl Pts',(-0.184904582322735,1.75226438641009,
4.83023470343036));
#29939=CARTESIAN_POINT('Ctrl Pts',(-0.202572611524001,1.76288098976719,
4.82919074078387));
#29940=CARTESIAN_POINT('Ctrl Pts',(-0.220208138481783,1.77347806273847,
4.82814869861916));
#29941=CARTESIAN_POINT('Ctrl Pts',(-0.237045530177403,1.78548410711521,
4.82710665645445));
#29942=CARTESIAN_POINT('Ctrl Pts',(-0.252853416649968,1.79875252749867,
4.82606461428974));
#29943=CARTESIAN_POINT('Ctrl Pts',(-0.268644325700925,1.81200669780719,
4.82502369126194));
#29944=CARTESIAN_POINT('Ctrl Pts',(-0.283407345248792,1.82652010410806,
4.82398276823414));
#29945=CARTESIAN_POINT('Ctrl Pts',(-0.296942660973606,1.84210477690753,
4.82294184520633));
#29946=CARTESIAN_POINT('Ctrl Pts',(-0.310484928084148,1.85769745358917,
4.82190038758757));
#29947=CARTESIAN_POINT('Ctrl Pts',(-0.322797737103604,1.87436195095103,
4.8208589299688));
#29948=CARTESIAN_POINT('Ctrl Pts',(-0.333720022327178,1.89187542985522,
4.81981747235003));
#29949=CARTESIAN_POINT('Ctrl Pts',(-0.344645644785207,1.90939425989098,
4.81877569652054));
#29950=CARTESIAN_POINT('Ctrl Pts',(-0.354179539312652,1.92776194493778,
4.81773392069106));
#29951=CARTESIAN_POINT('Ctrl Pts',(-0.362205941487288,1.94672982693522,
4.81669214486157));
#29952=CARTESIAN_POINT('Ctrl Pts',(-0.370249692912656,1.96573870844072,
4.81564811720995));
#29953=CARTESIAN_POINT('Ctrl Pts',(-0.376779213936063,1.9853496782075,4.81460408955833));
#29954=CARTESIAN_POINT('Ctrl Pts',(-0.38172793561452,2.00529692100319,4.81356006190671));
#29955=CARTESIAN_POINT('Ctrl Pts',(-0.383478233636536,2.01235199944131,
4.81319080300465));
#29956=CARTESIAN_POINT('Ctrl Pts',(-0.385031251020226,2.01944905325987,
4.8128215441026));
#29957=CARTESIAN_POINT('Ctrl Pts',(-0.38638558920318,2.02657611794442,4.81245228520054));
#29958=CARTESIAN_POINT('Ctrl Pts',(-0.39095304099983,2.05061186086891,4.81120697420153));
#29959=CARTESIAN_POINT('Ctrl Pts',(-0.393278498021054,2.07508656686066,
4.80996166320251));
#29960=CARTESIAN_POINT('Ctrl Pts',(-0.393299851487826,2.09965821109775,
4.8087163522035));
#29961=CARTESIAN_POINT('',(-0.39305280653286,2.09995383756141,4.68371636473574));
#29962=CARTESIAN_POINT('Ctrl Pts',(-0.393479809868051,2.09965979940225,
4.80871626382152));
#29963=CARTESIAN_POINT('Ctrl Pts',(-0.392508166945697,2.20582651071962,
4.80333815644026));
#29964=CARTESIAN_POINT('Ctrl Pts',(-0.293340422281615,2.44434164323185,
4.79133660121808));
#29965=CARTESIAN_POINT('Ctrl Pts',(0.110092729177043,2.55183472037241,4.77271159815497));
#29966=CARTESIAN_POINT('Ctrl Pts',(0.4395059068619,2.25201835981764,4.75284125463216));
#29967=CARTESIAN_POINT('Ctrl Pts',(0.36573224633123,1.81274585059014,4.7329709111094));
#29968=CARTESIAN_POINT('Ctrl Pts',(-0.0435509564148769,1.63698991534316,
4.71310056758659));
#29969=CARTESIAN_POINT('Ctrl Pts',(-0.348716460461016,1.84272401725045,
4.69668239214361));
#29970=CARTESIAN_POINT('Ctrl Pts',(-0.392722693669812,2.03701811531716,
4.68688766454154));
#29971=CARTESIAN_POINT('Ctrl Pts',(-0.392657437396775,2.09995348595077,
4.68371638478041));
#29972=CARTESIAN_POINT('',(-0.393299834232345,2.10036109944607,4.55871635220349));
#29973=CARTESIAN_POINT('Ctrl Pts',(-0.39329999731665,2.09995405739372,4.6837163522035));
#29974=CARTESIAN_POINT('Ctrl Pts',(-0.393302510661517,2.12147000107707,
4.68263394642612));
#29975=CARTESIAN_POINT('Ctrl Pts',(-0.391535126025817,2.14295809897274,
4.68155154064874));
#29976=CARTESIAN_POINT('Ctrl Pts',(-0.388037245285784,2.16412477111866,
4.68046913487136));
#29977=CARTESIAN_POINT('Ctrl Pts',(-0.38453365162738,2.18532601376001,4.6793849612533));
#29978=CARTESIAN_POINT('Ctrl Pts',(-0.379294099505847,2.20620415606676,
4.67830078763524));
#29979=CARTESIAN_POINT('Ctrl Pts',(-0.372408589511198,2.2264781896545,4.67721661401719));
#29980=CARTESIAN_POINT('Ctrl Pts',(-0.365500533233302,2.24681860962527,
4.67612889032288));
#29981=CARTESIAN_POINT('Ctrl Pts',(-0.356936024386469,2.26655037781274,
4.67504116662858));
#29982=CARTESIAN_POINT('Ctrl Pts',(-0.346852916917358,2.28541290145489,
4.67395344293428));
#29983=CARTESIAN_POINT('Ctrl Pts',(-0.34501882570705,2.28884394579536,4.67375558880319));
#29984=CARTESIAN_POINT('Ctrl Pts',(-0.343134606349185,2.29224630457451,
4.6735577346721));
#29985=CARTESIAN_POINT('Ctrl Pts',(-0.341201241198039,2.29561851396255,
4.67335988054101));
#29986=CARTESIAN_POINT('Ctrl Pts',(-0.330999981106641,2.31341173063956,
4.67231591766096));
#29987=CARTESIAN_POINT('Ctrl Pts',(-0.319372737625787,2.33045784032205,
4.67127195478091));
#29988=CARTESIAN_POINT('Ctrl Pts',(-0.306452966299499,2.346518699993,4.67022799190086));
#29989=CARTESIAN_POINT('Ctrl Pts',(-0.293556962264146,2.36255001400754,
4.66918594950135));
#29990=CARTESIAN_POINT('Ctrl Pts',(-0.279373559743091,2.37759907158861,
4.66814390710184));
#29991=CARTESIAN_POINT('Ctrl Pts',(-0.264079444876189,2.39145657788749,
4.66710186470234));
#29992=CARTESIAN_POINT('Ctrl Pts',(-0.248801755638117,2.4052992014516,4.6660609414393));
#29993=CARTESIAN_POINT('Ctrl Pts',(-0.232416245287508,2.41795230129518,
4.66502001817626));
#29994=CARTESIAN_POINT('Ctrl Pts',(-0.215136300475679,2.42924346951403,
4.66397909491322));
#29995=CARTESIAN_POINT('Ctrl Pts',(-0.197847481170762,2.44054043655894,
4.66293763706131));
#29996=CARTESIAN_POINT('Ctrl Pts',(-0.17966391683757,2.45047365866721,4.66189617920939));
#29997=CARTESIAN_POINT('Ctrl Pts',(-0.160828272786028,2.45891385689698,
4.66085472135748));
#29998=CARTESIAN_POINT('Ctrl Pts',(-0.141986873641556,2.46735663396743,
4.65981294529575));
#29999=CARTESIAN_POINT('Ctrl Pts',(-0.122493683820887,2.47430521140443,
4.65877116923402));
#30000=CARTESIAN_POINT('Ctrl Pts',(-0.102610789848103,2.47967870075466,
4.6577293931723));
#30001=CARTESIAN_POINT('Ctrl Pts',(-0.0826849186502222,2.48506380499665,
4.65668536529329));
#30002=CARTESIAN_POINT('Ctrl Pts',(-0.0623683854883882,2.48886688856434,
4.65564133741428));
#30003=CARTESIAN_POINT('Ctrl Pts',(-0.0419335873946778,2.49105813410312,
4.65459730953527));
#30004=CARTESIAN_POINT('Ctrl Pts',(-0.0347060959408396,2.49183314584202,
4.65422805202959));
#30005=CARTESIAN_POINT('Ctrl Pts',(-0.0274638362901075,2.49240700373886,
4.65385879452391));
#30006=CARTESIAN_POINT('Ctrl Pts',(-0.0202188518732227,2.49277994860854,
4.65348953701823));
#30007=CARTESIAN_POINT('Ctrl Pts',(0.000264115230046272,2.4938343356241,
4.6524455748913));
#30008=CARTESIAN_POINT('Ctrl Pts',(0.0208908123270126,2.49328531004609,
4.65140161276437));
#30009=CARTESIAN_POINT('Ctrl Pts',(0.0413887629450701,2.491116172386,4.65035765063744));
#30010=CARTESIAN_POINT('Ctrl Pts',(0.0618490053731108,2.4889510250885,4.64931560899139));
#30011=CARTESIAN_POINT('Ctrl Pts',(0.0821802417579286,2.48517169904134,
4.64827356734533));
#30012=CARTESIAN_POINT('Ctrl Pts',(0.102110850141772,2.47981345985013,4.64723152569928));
#30013=CARTESIAN_POINT('Ctrl Pts',(0.122020053404073,2.47446097531322,4.64619060318756));
#30014=CARTESIAN_POINT('Ctrl Pts',(0.141528768394392,2.46753310618056,4.64514968067584));
#30015=CARTESIAN_POINT('Ctrl Pts',(0.160376521685547,2.45911594407941,4.64410875816412));
#30016=CARTESIAN_POINT('Ctrl Pts',(0.179233954872339,2.45069445906245,4.64306730105174));
#30017=CARTESIAN_POINT('Ctrl Pts',(0.19742906979512,2.44078243833551,4.64202584393937));
#30018=CARTESIAN_POINT('Ctrl Pts',(0.214721807551827,2.42951393803855,4.64098438682699));
#30019=CARTESIAN_POINT('Ctrl Pts',(0.232019829078899,2.41824199466805,4.63994261149894));
#30020=CARTESIAN_POINT('Ctrl Pts',(0.24841432836989,2.4056131782879,4.63890083617089));
#30021=CARTESIAN_POINT('Ctrl Pts',(0.263695421065623,2.39180406938393,4.63785906084284));
#30022=CARTESIAN_POINT('Ctrl Pts',(0.279009544424255,2.377965111566,4.6368150336778));
#30023=CARTESIAN_POINT('Ctrl Pts',(0.293204950586356,2.36294130310269,4.63577100651276));
#30024=CARTESIAN_POINT('Ctrl Pts',(0.306109115434745,2.34694553943685,4.63472697934773));
#30025=CARTESIAN_POINT('Ctrl Pts',(0.31067318928691,2.34128799804999,4.63435771739697));
#30026=CARTESIAN_POINT('Ctrl Pts',(0.315076119829795,2.33550914814184,4.6339884554462));
#30027=CARTESIAN_POINT('Ctrl Pts',(0.319311589995046,2.32961924678658,4.63361919349544));
#30028=CARTESIAN_POINT('Ctrl Pts',(0.331285944740875,2.31296754921957,4.63257523062472));
#30029=CARTESIAN_POINT('Ctrl Pts',(0.341989923292617,2.2953270437564,4.63153126775399));
#30030=CARTESIAN_POINT('Ctrl Pts',(0.351261987899915,2.27691779406436,4.63048730488327));
#30031=CARTESIAN_POINT('Ctrl Pts',(0.360516995491423,2.2585424102777,4.6294452625008));
#30032=CARTESIAN_POINT('Ctrl Pts',(0.368344937507908,2.23940171233885,4.62840322011833));
#30033=CARTESIAN_POINT('Ctrl Pts',(0.374628431954159,2.21974317505214,4.62736117773587));
#30034=CARTESIAN_POINT('Ctrl Pts',(0.38090517798497,2.20010575085429,4.62632025449737));
#30035=CARTESIAN_POINT('Ctrl Pts',(0.385640518980635,2.17995227989731,4.62527933125887));
#30036=CARTESIAN_POINT('Ctrl Pts',(0.388765843277035,2.15954837614155,4.62423840802036));
#30037=CARTESIAN_POINT('Ctrl Pts',(0.391892772620308,2.1391339937222,4.62319695020355));
#30038=CARTESIAN_POINT('Ctrl Pts',(0.393407906080117,2.11846964641939,4.62215549238674));
#30039=CARTESIAN_POINT('Ctrl Pts',(0.393294012163239,2.09782974735531,4.62111403456992));
#30040=CARTESIAN_POINT('Ctrl Pts',(0.39318008344758,2.07718354204287,4.62007225854944));
#30041=CARTESIAN_POINT('Ctrl Pts',(0.39143617673339,2.05656253478705,4.61903048252895));
#30042=CARTESIAN_POINT('Ctrl Pts',(0.388097149784235,2.03623878663833,4.61798870650847));
#30043=CARTESIAN_POINT('Ctrl Pts',(0.384750905496115,2.01587110851189,4.61694467867907));
#30044=CARTESIAN_POINT('Ctrl Pts',(0.379802833779225,1.99580268733233,4.61590065084966));
#30045=CARTESIAN_POINT('Ctrl Pts',(0.373338550443823,1.97629382896353,4.61485662302026));
#30046=CARTESIAN_POINT('Ctrl Pts',(0.371052226060063,1.96939382531678,4.61448736533772));
#30047=CARTESIAN_POINT('Ctrl Pts',(0.368576677877943,1.96256364576548,4.61411810765519));
#30048=CARTESIAN_POINT('Ctrl Pts',(0.3659171104889,1.95581415377557,4.61374884997265));
#30049=CARTESIAN_POINT('Ctrl Pts',(0.358397990258774,1.93673201208086,4.61270488585942));
#30050=CARTESIAN_POINT('Ctrl Pts',(0.349359781576677,1.91818276843518,4.61166092174618));
#30051=CARTESIAN_POINT('Ctrl Pts',(0.338900075299647,1.90042137148008,4.61061695763295));
#30052=CARTESIAN_POINT('Ctrl Pts',(0.328459610650787,1.88269264831016,4.60957491399135));
#30053=CARTESIAN_POINT('Ctrl Pts',(0.316603156946611,1.8657495520126,4.60853287034976));
#30054=CARTESIAN_POINT('Ctrl Pts',(0.303475255083612,1.84982474232663,4.60749082670817));
#30055=CARTESIAN_POINT('Ctrl Pts',(0.290361452296511,1.83391703553363,4.60644990219837));
#30056=CARTESIAN_POINT('Ctrl Pts',(0.275979355542149,1.81902602751197,4.60540897768858));
#30057=CARTESIAN_POINT('Ctrl Pts',(0.260515157659317,1.8053531900228,4.60436805317878));
#30058=CARTESIAN_POINT('Ctrl Pts',(0.245043017923279,1.79167333065839,4.60332659408777));
#30059=CARTESIAN_POINT('Ctrl Pts',(0.228488207378558,1.7792133910942,4.60228513499677));
#30060=CARTESIAN_POINT('Ctrl Pts',(0.211072130331362,1.76813640483268,4.60124367590576));
#30061=CARTESIAN_POINT('Ctrl Pts',(0.193650731983767,1.75705603411373,4.6002018986078));
#30062=CARTESIAN_POINT('Ctrl Pts',(0.175368182998202,1.74735982189582,4.59916012130985));
#30063=CARTESIAN_POINT('Ctrl Pts',(0.156472106851897,1.73916573087174,4.5981183440119));
#30064=CARTESIAN_POINT('Ctrl Pts',(0.137535186968691,1.73095392837701,4.59707431491957));
#30065=CARTESIAN_POINT('Ctrl Pts',(0.11798278903514,1.72425096803732,4.59603028582725));
#30066=CARTESIAN_POINT('Ctrl Pts',(0.0980801287989144,1.71912577097579,
4.59498625673493));
#30067=CARTESIAN_POINT('Ctrl Pts',(0.0910409962331123,1.71731310165853,
4.5946170066399));
#30068=CARTESIAN_POINT('Ctrl Pts',(0.0839581446602437,1.71569732406559,
4.59424775654488));
#30069=CARTESIAN_POINT('Ctrl Pts',(0.0768435248601465,1.71427994259169,
4.59387850644986));
#30070=CARTESIAN_POINT('Ctrl Pts',(0.056728784763575,1.71027266451274,4.59283454768598));
#30071=CARTESIAN_POINT('Ctrl Pts',(0.0362398046289374,1.70783111395,4.5917905889221));
#30072=CARTESIAN_POINT('Ctrl Pts',(0.0156437749488127,1.70701124404717,
4.59074663015821));
#30073=CARTESIAN_POINT('Ctrl Pts',(-0.00491436603069629,1.70619288238675,
4.58970459187326));
#30074=CARTESIAN_POINT('Ctrl Pts',(-0.0255784411254026,1.70699036808954,
4.58866255358831));
#30075=CARTESIAN_POINT('Ctrl Pts',(-0.0460745855597139,1.7094081125196,
4.58762051530336));
#30076=CARTESIAN_POINT('Ctrl Pts',(-0.0665487176794167,1.71182326035638,
4.58657959613984));
#30077=CARTESIAN_POINT('Ctrl Pts',(-0.0868545467815963,1.71585515534059,
4.58553867697633));
#30078=CARTESIAN_POINT('Ctrl Pts',(-0.106721884374345,1.72145630450952,
4.58449775781281));
#30079=CARTESIAN_POINT('Ctrl Pts',(-0.126599426632449,1.72706033065442,
4.58345630399125));
#30080=CARTESIAN_POINT('Ctrl Pts',(-0.146037314875636,1.73423503711632,
4.5824148501697));
#30081=CARTESIAN_POINT('Ctrl Pts',(-0.164778619486665,1.74288251714587,
4.58137339634815));
#30082=CARTESIAN_POINT('Ctrl Pts',(-0.183525651014859,1.75153263964898,
4.58033162428195));
#30083=CARTESIAN_POINT('Ctrl Pts',(-0.201575022785195,1.76165609079279,
4.57928985221576));
#30084=CARTESIAN_POINT('Ctrl Pts',(-0.218693508662671,1.77310852065432,
4.57824808014956));
#30085=CARTESIAN_POINT('Ctrl Pts',(-0.235848998422755,1.78458570646524,
4.57720405615457));
#30086=CARTESIAN_POINT('Ctrl Pts',(-0.252069007019751,1.79739714983084,
4.57616003215958));
#30087=CARTESIAN_POINT('Ctrl Pts',(-0.267152020423162,1.8113571619045,4.57511600816459));
#30088=CARTESIAN_POINT('Ctrl Pts',(-0.272487033362416,1.81629495802344,
4.57474672641875));
#30089=CARTESIAN_POINT('Ctrl Pts',(-0.277680138024386,1.82137611966157,
4.57437744467291));
#30090=CARTESIAN_POINT('Ctrl Pts',(-0.282723598343368,1.82659141026702,
4.57400816292707));
#30091=CARTESIAN_POINT('Ctrl Pts',(-0.296797343894201,1.84114464719416,
4.57297768444626));
#30092=CARTESIAN_POINT('Ctrl Pts',(-0.309791624911384,1.85683650285156,
4.57194720596545));
#30093=CARTESIAN_POINT('Ctrl Pts',(-0.321516802775297,1.87347884087099,
4.57091672748464));
#30094=CARTESIAN_POINT('Ctrl Pts',(-0.333223256999998,1.89009460316284,
4.56988789454878));
#30095=CARTESIAN_POINT('Ctrl Pts',(-0.34366413939655,1.90765726636389,4.56885906161293));
#30096=CARTESIAN_POINT('Ctrl Pts',(-0.352689122616453,1.92594462723594,
4.56783022867707));
#30097=CARTESIAN_POINT('Ctrl Pts',(-0.361704682477759,1.94421289351744,
4.56680246998828));
#30098=CARTESIAN_POINT('Ctrl Pts',(-0.369306917863024,1.96320369221295,
4.56577471129948));
#30099=CARTESIAN_POINT('Ctrl Pts',(-0.375391091138084,1.98266961734419,
4.56474695261069));
#30100=CARTESIAN_POINT('Ctrl Pts',(-0.381481113779663,2.00215425715129,
4.56371820582754));
#30101=CARTESIAN_POINT('Ctrl Pts',(-0.386049919062549,2.02211421592566,
4.56268945904439));
#30102=CARTESIAN_POINT('Ctrl Pts',(-0.389042356387749,2.04228574754649,
4.56166071226124));
#30103=CARTESIAN_POINT('Ctrl Pts',(-0.391897225723248,2.06152995580087,
4.56067925890865));
#30104=CARTESIAN_POINT('Ctrl Pts',(-0.393317641356229,2.08096605758746,
4.55969780555607));
#30105=CARTESIAN_POINT('Ctrl Pts',(-0.393299834232345,2.10036109944607,
4.55871635220349));
#30106=CARTESIAN_POINT('',(-0.393445918996423,2.09985495139376,4.4337163522035));
#30107=CARTESIAN_POINT('Ctrl Pts',(-0.393310908181485,2.10036110961337,
4.55871635220349));
#30108=CARTESIAN_POINT('Ctrl Pts',(-0.39358942096467,2.13052187855199,4.55719017460375));
#30109=CARTESIAN_POINT('Ctrl Pts',(-0.376632741138322,2.29126728843717,
4.54904054916312));
#30110=CARTESIAN_POINT('Ctrl Pts',(-0.155906186004341,2.5381425209697,4.53426747588148));
#30111=CARTESIAN_POINT('Ctrl Pts',(0.284004796300236,2.46826155993621,4.5143971323587));
#30112=CARTESIAN_POINT('Ctrl Pts',(0.463374845213788,2.06055343100496,4.49452678883592));
#30113=CARTESIAN_POINT('Ctrl Pts',(0.217671564353364,1.6890269994191,4.47465644531311));
#30114=CARTESIAN_POINT('Ctrl Pts',(-0.227735017592104,1.69452228360619,
4.45478610179035));
#30115=CARTESIAN_POINT('Ctrl Pts',(-0.390128315479153,1.95374788316366,
4.44113940408713));
#30116=CARTESIAN_POINT('Ctrl Pts',(-0.393918994188849,2.09198357827423,
4.43411615422485));
#30117=CARTESIAN_POINT('Ctrl Pts',(-0.393882594814329,2.09985479040793,
4.4337163522035));
#30118=CARTESIAN_POINT('',(0.293078184270657,1.8377213925906,4.35670005929419));
#30119=CARTESIAN_POINT('Ctrl Pts',(-0.393299973272956,2.09985500519842,
4.4337163522035));
#30120=CARTESIAN_POINT('Ctrl Pts',(-0.393307473039213,2.12019820258479,
4.43268152877099));
#30121=CARTESIAN_POINT('Ctrl Pts',(-0.39173231746941,2.14060550769227,4.43164670533848));
#30122=CARTESIAN_POINT('Ctrl Pts',(-0.388570851337203,2.16080775847769,
4.43061188190596));
#30123=CARTESIAN_POINT('Ctrl Pts',(-0.38541493166847,2.18097456651554,4.42957887396352));
#30124=CARTESIAN_POINT('Ctrl Pts',(-0.380678279633258,2.2009362922915,4.42854586602108));
#30125=CARTESIAN_POINT('Ctrl Pts',(-0.374409109528847,2.22042719253481,
4.42751285807864));
#30126=CARTESIAN_POINT('Ctrl Pts',(-0.368103856053702,2.24003027626775,
4.42647390446748));
#30127=CARTESIAN_POINT('Ctrl Pts',(-0.360248522858196,2.25915634225469,
4.42543495085633));
#30128=CARTESIAN_POINT('Ctrl Pts',(-0.350943650004022,2.27754842866625,
4.42439599724517));
#30129=CARTESIAN_POINT('Ctrl Pts',(-0.341695228996082,2.29582893190518,
4.42336334687431));
#30130=CARTESIAN_POINT('Ctrl Pts',(-0.331015194686975,2.3133836840058,4.42233069650344));
#30131=CARTESIAN_POINT('Ctrl Pts',(-0.319048907629175,2.32998409627761,
4.42129804613258));
#30132=CARTESIAN_POINT('Ctrl Pts',(-0.306973058247754,2.34673650053598,
4.42025594090128));
#30133=CARTESIAN_POINT('Ctrl Pts',(-0.29358773345619,2.36251636979888,4.41921383566997));
#30134=CARTESIAN_POINT('Ctrl Pts',(-0.279083872946256,2.37712286419803,
4.41817173043867));
#30135=CARTESIAN_POINT('Ctrl Pts',(-0.264580012436322,2.39172935859718,
4.41712962520737));
#30136=CARTESIAN_POINT('Ctrl Pts',(-0.248958245337701,2.40516202011686,
4.41608751997606));
#30137=CARTESIAN_POINT('Ctrl Pts',(-0.232442705828144,2.41726216053493,
4.41504541474476));
#30138=CARTESIAN_POINT('Ctrl Pts',(-0.215920112107219,2.42936746923394,
4.41400286440353));
#30139=CARTESIAN_POINT('Ctrl Pts',(-0.19839928804482,2.44021524029002,4.4129603140623));
#30140=CARTESIAN_POINT('Ctrl Pts',(-0.180098122380582,2.44964204025687,
4.41191776372107));
#30141=CARTESIAN_POINT('Ctrl Pts',(-0.161830718147231,2.45905144995136,
4.41087713664484));
#30142=CARTESIAN_POINT('Ctrl Pts',(-0.142786450456267,2.46704470382945,
4.4098365095686));
#30143=CARTESIAN_POINT('Ctrl Pts',(-0.123211075344355,2.47350223682394,
4.40879588249237));
#30144=CARTESIAN_POINT('Ctrl Pts',(-0.103656718593553,2.47995283627261,
4.40775637275236));
#30145=CARTESIAN_POINT('Ctrl Pts',(-0.0835730745182236,2.48487073034174,
4.40671686301234));
#30146=CARTESIAN_POINT('Ctrl Pts',(-0.0632245156711306,2.48818494383238,
4.40567735327233));
#30147=CARTESIAN_POINT('Ctrl Pts',(-0.0428651243813793,2.49150092162623,
4.40463729015506));
#30148=CARTESIAN_POINT('Ctrl Pts',(-0.0222412624082241,2.49321137882844,
4.4035972270378));
#30149=CARTESIAN_POINT('Ctrl Pts',(-0.0016265849958498,2.4932966364225,
4.40255716392053));
#30150=CARTESIAN_POINT('Ctrl Pts',(0.0189945776486265,2.493381920838,4.40151677360674));
#30151=CARTESIAN_POINT('Ctrl Pts',(0.0396058124959531,2.49184102187124,
4.40047638329295));
#30152=CARTESIAN_POINT('Ctrl Pts',(0.0599353663630418,2.48870636971746,
4.39943599297916));
#30153=CARTESIAN_POINT('Ctrl Pts',(0.0803095879231295,2.48556483016808,
4.39839331674039));
#30154=CARTESIAN_POINT('Ctrl Pts',(0.100400174222778,2.48082271714529,4.39735064050161));
#30155=CARTESIAN_POINT('Ctrl Pts',(0.11994670300977,2.47456331699338,4.39630796426284));
#30156=CARTESIAN_POINT('Ctrl Pts',(0.12702596232744,2.47229632026311,4.39593033324922));
#30157=CARTESIAN_POINT('Ctrl Pts',(0.134034034163761,2.46983076463011,4.39555270223559));
#30158=CARTESIAN_POINT('Ctrl Pts',(0.1409592423106,2.4671721421993,4.39517507122197));
#30159=CARTESIAN_POINT('Ctrl Pts',(0.160140515404261,2.45980835445211,4.39412911802499));
#30160=CARTESIAN_POINT('Ctrl Pts',(0.17879941889945,2.45091589366128,4.393083164828));
#30161=CARTESIAN_POINT('Ctrl Pts',(0.196679518697313,2.44059074697501,4.39203721163102));
#30162=CARTESIAN_POINT('Ctrl Pts',(0.21452659328169,2.43028467122108,4.39099319034874));
#30163=CARTESIAN_POINT('Ctrl Pts',(0.231597062858027,2.41855147410596,4.38994916906646));
#30164=CARTESIAN_POINT('Ctrl Pts',(0.247656429732667,2.40553425800075,4.38890514778418));
#30165=CARTESIAN_POINT('Ctrl Pts',(0.263698306885079,2.39253121851257,4.38786226351074));
#30166=CARTESIAN_POINT('Ctrl Pts',(0.278730683003493,2.37824737297298,4.38681937923731));
#30167=CARTESIAN_POINT('Ctrl Pts',(0.29254990300435,2.36286773147754,4.38577649496387));
#30168=CARTESIAN_POINT('Ctrl Pts',(0.306375559559247,2.34748092663324,4.38473312494805));
#30169=CARTESIAN_POINT('Ctrl Pts',(0.318986428939915,2.33099783993888,4.38368975493222));
#30170=CARTESIAN_POINT('Ctrl Pts',(0.330216985574048,2.3136390236787,4.3826463849164));
#30171=CARTESIAN_POINT('Ctrl Pts',(0.341450687666683,2.29627534555478,4.3816027226731));
#30172=CARTESIAN_POINT('Ctrl Pts',(0.351302938472491,2.27803608295674,4.38055906042981));
#30173=CARTESIAN_POINT('Ctrl Pts',(0.359653019480331,2.25916845032443,4.37951539818652));
#30174=CARTESIAN_POINT('Ctrl Pts',(0.368020583496849,2.24026131352627,4.37846955077209));
#30175=CARTESIAN_POINT('Ctrl Pts',(0.374879453596798,2.22072387138932,4.37742370335765));
#30176=CARTESIAN_POINT('Ctrl Pts',(0.380157769311558,2.20082142843692,4.37637785594322));
#30177=CARTESIAN_POINT('Ctrl Pts',(0.381963102669721,2.19401422968023,4.37602014652854));
#30178=CARTESIAN_POINT('Ctrl Pts',(0.383583977842243,2.18716442574047,4.37566243711386));
#30179=CARTESIAN_POINT('Ctrl Pts',(0.385018902038723,2.18028284420034,4.37530472769918));
#30180=CARTESIAN_POINT('Ctrl Pts',(0.389170687082921,2.16037179427255,4.37426973741769));
#30181=CARTESIAN_POINT('Ctrl Pts',(0.391786937179193,2.14007437079021,4.37323474713619));
#30182=CARTESIAN_POINT('Ctrl Pts',(0.392808659387981,2.11965317047748,4.3721997568547));
#30183=CARTESIAN_POINT('Ctrl Pts',(0.393828534995012,2.09926887826369,4.37116663715491));
#30184=CARTESIAN_POINT('Ctrl Pts',(0.393259502817064,2.07876199016779,4.37013351745512));
#30185=CARTESIAN_POINT('Ctrl Pts',(0.391094023194851,2.05840246375967,4.36910039775533));
#30186=CARTESIAN_POINT('Ctrl Pts',(0.388928036664634,2.03803817147577,4.3680670362169));
#30187=CARTESIAN_POINT('Ctrl Pts',(0.385164873135253,2.01782206049515,4.36703367467847));
#30188=CARTESIAN_POINT('Ctrl Pts',(0.379849126078133,1.99802190716787,4.36600031314005));
#30189=CARTESIAN_POINT('Ctrl Pts',(0.374537207809709,1.978236015355,4.36496769590396));
#30190=CARTESIAN_POINT('Ctrl Pts',(0.367675141274041,1.95886620608699,4.36393507866787));
#30191=CARTESIAN_POINT('Ctrl Pts',(0.359357831763001,1.94016621524035,4.36290246143178));
#30192=CARTESIAN_POINT('Ctrl Pts',(0.351021974972372,1.92142452413498,4.36186754149906));
#30193=CARTESIAN_POINT('Ctrl Pts',(0.341224718531711,1.90335631496584,4.36083262156635));
#30194=CARTESIAN_POINT('Ctrl Pts',(0.330108221488342,1.88619295590228,4.35979770163363));
#30195=CARTESIAN_POINT('Ctrl Pts',(0.319017208287179,1.86906894271651,4.35876515418715));
#30196=CARTESIAN_POINT('Ctrl Pts',(0.306613508066773,1.85284617978107,4.35773260674067));
#30197=CARTESIAN_POINT('Ctrl Pts',(0.293078184270657,1.8377213925906,4.35670005929419));
#30198=CARTESIAN_POINT('',(0.287740166859834,1.83187598694732,4.3567));
#30199=CARTESIAN_POINT('Ctrl Pts',(0.293078184270657,1.8377213925906,4.3567));
#30200=CARTESIAN_POINT('Ctrl Pts',(0.291298845133716,1.83577292404284,4.3567));
#30201=CARTESIAN_POINT('Ctrl Pts',(0.289519505996775,1.83382445549508,4.3567));
#30202=CARTESIAN_POINT('Ctrl Pts',(0.287740166859834,1.83187598694732,4.3567));
#30203=CARTESIAN_POINT('',(0.386085631082133,2.17498516834622,4.3567));
#30204=CARTESIAN_POINT('Origin',(0.,2.1,4.3567));
#30205=CARTESIAN_POINT('',(-0.393882850542516,2.09986682733705,4.41538364779653));
#30206=CARTESIAN_POINT('Ctrl Pts',(0.386085631082133,2.17498516834622,4.3567));
#30207=CARTESIAN_POINT('Ctrl Pts',(0.36112075890231,2.30352496685583,4.36332344784093));
#30208=CARTESIAN_POINT('Ctrl Pts',(0.173109802419442,2.53147029156881,4.37657034352279));
#30209=CARTESIAN_POINT('Ctrl Pts',(-0.263054777401013,2.47987360215571,
4.39613155945497));
#30210=CARTESIAN_POINT('Ctrl Pts',(-0.393452793012018,2.22418599272304,
4.40906932754621));
#30211=CARTESIAN_POINT('Ctrl Pts',(-0.393882850542516,2.09986682733705,
4.41538364779653));
#30212=CARTESIAN_POINT('',(-0.393255881934822,2.1003613435798,4.54038364779653));
#30213=CARTESIAN_POINT('Ctrl Pts',(-0.393882850542516,2.09986682733705,
4.41538364779653));
#30214=CARTESIAN_POINT('Ctrl Pts',(-0.393903904692916,2.09378058486925,
4.41569277538714));
#30215=CARTESIAN_POINT('Ctrl Pts',(-0.390978467245773,1.95731419778572,
4.42262535081861));
#30216=CARTESIAN_POINT('Ctrl Pts',(-0.233315454838252,1.69771858502018,
4.43618137409123));
#30217=CARTESIAN_POINT('Ctrl Pts',(0.212061907806772,1.6860660404583,4.4560517176139));
#30218=CARTESIAN_POINT('Ctrl Pts',(0.4627766764693,2.05423342872913,4.47592206113677));
#30219=CARTESIAN_POINT('Ctrl Pts',(0.289021540344744,2.46433772613338,4.4957924046595));
#30220=CARTESIAN_POINT('Ctrl Pts',(-0.149905097511465,2.5402365181872,4.51566274818232));
#30221=CARTESIAN_POINT('Ctrl Pts',(-0.375357159811075,2.29490204802152,
4.53052649589464));
#30222=CARTESIAN_POINT('Ctrl Pts',(-0.393547872205643,2.13232530629972,
4.53876679576605));
#30223=CARTESIAN_POINT('Ctrl Pts',(-0.393255881934822,2.1003613435798,4.54038364779653));
#30224=CARTESIAN_POINT('',(-0.393062271237487,2.09992472497766,4.66538365014497));
#30225=CARTESIAN_POINT('Ctrl Pts',(-0.393255881934822,2.1003613435798,4.54038364779653));
#30226=CARTESIAN_POINT('Ctrl Pts',(-0.39235173162358,2.00138466617034,4.54539024360698));
#30227=CARTESIAN_POINT('Ctrl Pts',(-0.304249124076242,1.77003449934502,
4.55702028725837));
#30228=CARTESIAN_POINT('Ctrl Pts',(0.0846189449362708,1.64270878203361,
4.57527377875067));
#30229=CARTESIAN_POINT('Ctrl Pts',(0.430303245215323,1.92360908410859,4.59514412227347));
#30230=CARTESIAN_POINT('Ctrl Pts',(0.381244165381663,2.36632310413653,4.61501446579626));
#30231=CARTESIAN_POINT('Ctrl Pts',(-0.0175551922214225,2.56472241761119,
4.63488480931905));
#30232=CARTESIAN_POINT('Ctrl Pts',(-0.340918328246028,2.37213778114564,
4.65167453665247));
#30233=CARTESIAN_POINT('Ctrl Pts',(-0.392545913529889,2.1702301438735,4.66184081614497));
#30234=CARTESIAN_POINT('Ctrl Pts',(-0.392665676133501,2.09992484756078,
4.66538364779653));
#30235=CARTESIAN_POINT('',(-0.393336985380828,2.09966984214535,4.79038364779653));
#30236=CARTESIAN_POINT('Ctrl Pts',(-0.393299992782359,2.09992465150058,
4.66538365155264));
#30237=CARTESIAN_POINT('Ctrl Pts',(-0.393295769512778,2.07788025900139,
4.66649272362475));
#30238=CARTESIAN_POINT('Ctrl Pts',(-0.391433911723158,2.05588325308345,
4.66760179569686));
#30239=CARTESIAN_POINT('Ctrl Pts',(-0.387763466838727,2.03423995297134,
4.66871086776897));
#30240=CARTESIAN_POINT('Ctrl Pts',(-0.384073922335051,2.01248402923884,
4.66982571103638));
#30241=CARTESIAN_POINT('Ctrl Pts',(-0.378557116761919,1.99108606085747,
4.6709405543038));
#30242=CARTESIAN_POINT('Ctrl Pts',(-0.371313017604665,1.97034070431582,
4.67205539757122));
#30243=CARTESIAN_POINT('Ctrl Pts',(-0.365746300725396,1.95439896692102,
4.67291209716902));
#30244=CARTESIAN_POINT('Ctrl Pts',(-0.359160659068457,1.938842327753,4.67376879676682));
#30245=CARTESIAN_POINT('Ctrl Pts',(-0.351620062476746,1.92379494427273,
4.67462549636463));
#30246=CARTESIAN_POINT('Ctrl Pts',(-0.342431196821245,1.90545841299364,
4.67566945852539));
#30247=CARTESIAN_POINT('Ctrl Pts',(-0.331776750804907,1.88778796277536,
4.67671342068616));
#30248=CARTESIAN_POINT('Ctrl Pts',(-0.319776634642432,1.87102883601475,
4.67775738284692));
#30249=CARTESIAN_POINT('Ctrl Pts',(-0.307798594125831,1.85430053966798,
4.6787994245147));
#30250=CARTESIAN_POINT('Ctrl Pts',(-0.294480172437816,1.83848086511535,
4.67984146618247));
#30251=CARTESIAN_POINT('Ctrl Pts',(-0.27998605802235,1.82378867272846,4.68088350785025));
#30252=CARTESIAN_POINT('Ctrl Pts',(-0.265507510197148,1.80911225966637,
4.68192443037164));
#30253=CARTESIAN_POINT('Ctrl Pts',(-0.24985626990208,1.79556146627513,4.68296535289304));
#30254=CARTESIAN_POINT('Ctrl Pts',(-0.2332357341274,1.78332037904839,4.68400627541443));
#30255=CARTESIAN_POINT('Ctrl Pts',(-0.216606662603788,1.77107300521041,
4.68504773251867));
#30256=CARTESIAN_POINT('Ctrl Pts',(-0.199007883991114,1.76013713059733,
4.68608918962291));
#30257=CARTESIAN_POINT('Ctrl Pts',(-0.180674443153325,1.7506554199773,4.68713064672715));
#30258=CARTESIAN_POINT('Ctrl Pts',(-0.16233540074126,1.74117081232846,4.68817242203676));
#30259=CARTESIAN_POINT('Ctrl Pts',(-0.143261918860075,1.73314155875621,
4.68921419734637));
#30260=CARTESIAN_POINT('Ctrl Pts',(-0.123711142893961,1.72666309702379,
4.69025597265598));
#30261=CARTESIAN_POINT('Ctrl Pts',(-0.104118107463642,1.72017063194326,
4.69129999978754));
#30262=CARTESIAN_POINT('Ctrl Pts',(-0.084046433425361,1.71523582678645,
4.6923440269191));
#30263=CARTESIAN_POINT('Ctrl Pts',(-0.063766420372174,1.71190370572122,
4.69338805405065));
#30264=CARTESIAN_POINT('Ctrl Pts',(-0.0565935827607402,1.7107251678554,
4.69375731599624));
#30265=CARTESIAN_POINT('Ctrl Pts',(-0.0493947352562634,1.70974664603408,
4.69412657794183));
#30266=CARTESIAN_POINT('Ctrl Pts',(-0.0421819163230374,1.70896857423563,
4.69449583988742));
#30267=CARTESIAN_POINT('Ctrl Pts',(-0.0217901178502496,1.70676884019846,
4.69553980276072));
#30268=CARTESIAN_POINT('Ctrl Pts',(-0.00116502768758128,1.70616195661353,
4.69658376563402));
#30269=CARTESIAN_POINT('Ctrl Pts',(0.0194222400179982,1.70717985465014,
4.69762772850732));
#30270=CARTESIAN_POINT('Ctrl Pts',(0.039971635303871,1.70819588015747,4.69866977090236));
#30271=CARTESIAN_POINT('Ctrl Pts',(0.0604826167254509,1.71083077780269,
4.6997118132974));
#30272=CARTESIAN_POINT('Ctrl Pts',(0.0806820134259272,1.71506454734652,
4.70075385569243));
#30273=CARTESIAN_POINT('Ctrl Pts',(0.100859716349234,1.71929376990043,4.70179477895328));
#30274=CARTESIAN_POINT('Ctrl Pts',(0.120725776473047,1.72511833351522,4.70283570221412));
#30275=CARTESIAN_POINT('Ctrl Pts',(0.140015307863677,1.7324668673931,4.70387662547497));
#30276=CARTESIAN_POINT('Ctrl Pts',(0.159314745876898,1.73981917529484,4.70491808332806));
#30277=CARTESIAN_POINT('Ctrl Pts',(0.178036370321091,1.74869677019204,4.70595954118115));
#30278=CARTESIAN_POINT('Ctrl Pts',(0.195932991866882,1.75897924887466,4.70700099903424));
#30279=CARTESIAN_POINT('Ctrl Pts',(0.213835081627622,1.76926486931247,4.70804277509909));
#30280=CARTESIAN_POINT('Ctrl Pts',(0.23091104725502,1.78095583046984,4.70908455116394));
#30281=CARTESIAN_POINT('Ctrl Pts',(0.246941445344783,1.79388758180853,4.71012632722879));
#30282=CARTESIAN_POINT('Ctrl Pts',(0.263006493465729,1.80684728539049,4.71117035511377));
#30283=CARTESIAN_POINT('Ctrl Pts',(0.278020927055499,1.82105262746797,4.71221438299874));
#30284=CARTESIAN_POINT('Ctrl Pts',(0.291800570764912,1.83630070743123,4.71325841088372));
#30285=CARTESIAN_POINT('Ctrl Pts',(0.296674230733087,1.841693731988,4.71362766839255));
#30286=CARTESIAN_POINT('Ctrl Pts',(0.3013937969224,1.84721689521838,4.71399692590138));
#30287=CARTESIAN_POINT('Ctrl Pts',(0.305952388048845,1.85286031025509,4.71436618341021));
#30288=CARTESIAN_POINT('Ctrl Pts',(0.318840410004825,1.86881533997423,4.71541014606209));
#30289=CARTESIAN_POINT('Ctrl Pts',(0.330515420489601,1.88582876395813,4.71645410871397));
#30290=CARTESIAN_POINT('Ctrl Pts',(0.340803812214894,1.90368990963327,4.71749807136584));
#30291=CARTESIAN_POINT('Ctrl Pts',(0.35107327734531,1.92151819782424,4.71854011353698));
#30292=CARTESIAN_POINT('Ctrl Pts',(0.359960772381131,1.94019051152622,4.71958215570812));
#30293=CARTESIAN_POINT('Ctrl Pts',(0.367335241547277,1.95946633742265,4.72062419787925));
#30294=CARTESIAN_POINT('Ctrl Pts',(0.374701790656649,1.97872146140387,4.72166512091449));
#30295=CARTESIAN_POINT('Ctrl Pts',(0.380558251252852,1.99857813743754,4.72270604394973));
#30296=CARTESIAN_POINT('Ctrl Pts',(0.384821245619206,2.01877501049503,4.72374696698497));
#30297=CARTESIAN_POINT('Ctrl Pts',(0.389086429354271,2.03898225616813,4.7247884246126));
#30298=CARTESIAN_POINT('Ctrl Pts',(0.391756344222165,2.05952933132301,4.72582988224022));
#30299=CARTESIAN_POINT('Ctrl Pts',(0.392798419325999,2.08014321841293,4.72687133986785));
#30300=CARTESIAN_POINT('Ctrl Pts',(0.393840812830054,2.10076340396077,4.72791311570703));
#30301=CARTESIAN_POINT('Ctrl Pts',(0.39325437542767,2.12144970603567,4.72895489154621));
#30302=CARTESIAN_POINT('Ctrl Pts',(0.391058675456665,2.1419285386113,4.72999666738539));
#30303=CARTESIAN_POINT('Ctrl Pts',(0.388858229427969,2.16245163667043,4.73104069504781));
#30304=CARTESIAN_POINT('Ctrl Pts',(0.385041712244149,2.18276564610716,4.73208472271024));
#30305=CARTESIAN_POINT('Ctrl Pts',(0.379680028905663,2.20260587532006,4.73312875037266));
#30306=CARTESIAN_POINT('Ctrl Pts',(0.377783672024161,2.20962310345966,4.73349800922611));
#30307=CARTESIAN_POINT('Ctrl Pts',(0.375694477057357,2.21658121279524,4.73386726807955));
#30308=CARTESIAN_POINT('Ctrl Pts',(0.373417032150404,2.2234690653564,4.734236526933));
#30309=CARTESIAN_POINT('Ctrl Pts',(0.36697827720004,2.24294228933658,4.73528048951727));
#30310=CARTESIAN_POINT('Ctrl Pts',(0.358992980580432,2.26196851967134,4.73632445210155));
#30311=CARTESIAN_POINT('Ctrl Pts',(0.349544302746481,2.28028774339227,4.73736841468582));
#30312=CARTESIAN_POINT('Ctrl Pts',(0.340113006788501,2.29857326689818,4.73841045678677));
#30313=CARTESIAN_POINT('Ctrl Pts',(0.329223953843854,2.31615369166456,4.73945249888773));
#30314=CARTESIAN_POINT('Ctrl Pts',(0.317008428904983,2.33278862945426,4.74049454098868));
#30315=CARTESIAN_POINT('Ctrl Pts',(0.304806023264139,2.34940570156012,4.74153546395141));
#30316=CARTESIAN_POINT('Ctrl Pts',(0.291280383801512,2.36507869541469,4.74257638691414));
#30317=CARTESIAN_POINT('Ctrl Pts',(0.276606128593381,2.37959602934338,4.74361730987687));
#30318=CARTESIAN_POINT('Ctrl Pts',(0.261924337086183,2.39412081898062,4.74465876742938));
#30319=CARTESIAN_POINT('Ctrl Pts',(0.246093263074994,2.40748823405086,4.74570022498188));
#30320=CARTESIAN_POINT('Ctrl Pts',(0.229324833344335,2.41952309902665,4.74674168253438));
#30321=CARTESIAN_POINT('Ctrl Pts',(0.212551280139252,2.43156164116982,4.74778345829683));
#30322=CARTESIAN_POINT('Ctrl Pts',(0.194840419405803,2.44226642341539,4.74882523405928));
#30323=CARTESIAN_POINT('Ctrl Pts',(0.176432879831052,2.45150580210648,4.74986700982173));
#30324=CARTESIAN_POINT('Ctrl Pts',(0.157985551941207,2.46076515192457,4.75091103740617));
#30325=CARTESIAN_POINT('Ctrl Pts',(0.138839220988392,2.46855249695004,4.7519550649906));
#30326=CARTESIAN_POINT('Ctrl Pts',(0.11925482653518,2.47478417302237,4.75299909257504));
#30327=CARTESIAN_POINT('Ctrl Pts',(0.112328075011662,2.47698823768372,4.75336835186862));
#30328=CARTESIAN_POINT('Ctrl Pts',(0.105346644754062,2.47899815808783,4.75373761116221));
#30329=CARTESIAN_POINT('Ctrl Pts',(0.0983223844569184,2.48081176283658,
4.75410687045579));
#30330=CARTESIAN_POINT('Ctrl Pts',(0.0784635325716178,2.48593915085474,
4.75515083313775));
#30331=CARTESIAN_POINT('Ctrl Pts',(0.0581433500240972,2.48952421285417,
4.7561947958197));
#30332=CARTESIAN_POINT('Ctrl Pts',(0.0376254766890382,2.4914961219526,4.75723875850166));
#30333=CARTESIAN_POINT('Ctrl Pts',(0.0171453481802259,2.49346440351297,
4.75828080070242));
#30334=CARTESIAN_POINT('Ctrl Pts',(-0.00353103079621325,2.4938252938848,
4.75932284290317));
#30335=CARTESIAN_POINT('Ctrl Pts',(-0.0241304705196809,2.49255905338242,
4.76036488510393));
#30336=CARTESIAN_POINT('Ctrl Pts',(-0.0447077867783312,2.49129417280184,
4.76140580816822));
#30337=CARTESIAN_POINT('Ctrl Pts',(-0.0652075953844509,2.48840564662385,
4.76244673123252));
#30338=CARTESIAN_POINT('Ctrl Pts',(-0.085357470718213,2.48392576390832,
4.76348765429682));
#30339=CARTESIAN_POINT('Ctrl Pts',(-0.105517694507556,2.47944358044073,
4.76452911195233));
#30340=CARTESIAN_POINT('Ctrl Pts',(-0.125326904251082,2.47336855164252,
4.76557056960783));
#30341=CARTESIAN_POINT('Ctrl Pts',(-0.144523089397569,2.46578404370746,
4.76661202726333));
#30342=CARTESIAN_POINT('Ctrl Pts',(-0.163725139818961,2.4581972183732,4.76765380312974));
#30343=CARTESIAN_POINT('Ctrl Pts',(-0.182313122331425,2.44910029953093,
4.76869557899614));
#30344=CARTESIAN_POINT('Ctrl Pts',(-0.200046091905373,2.43862435103428,
4.76973735486255));
#30345=CARTESIAN_POINT('Ctrl Pts',(-0.217817391689976,2.42812575854047,
4.77078138255081));
#30346=CARTESIAN_POINT('Ctrl Pts',(-0.234729386239739,2.41624260877569,
4.77182541023907));
#30347=CARTESIAN_POINT('Ctrl Pts',(-0.250570477902909,2.40314901550806,
4.77286943792733));
#30348=CARTESIAN_POINT('Ctrl Pts',(-0.256173260973188,2.39851798601535,
4.77323869661108));
#30349=CARTESIAN_POINT('Ctrl Pts',(-0.261642403097666,2.3937358883794,4.77360795529483));
#30350=CARTESIAN_POINT('Ctrl Pts',(-0.26696966465499,2.38881150973256,4.77397721397858));
#30351=CARTESIAN_POINT('Ctrl Pts',(-0.281806371321473,2.37509685339147,
4.77500561904484));
#30352=CARTESIAN_POINT('Ctrl Pts',(-0.29563393681208,2.36018897340975,4.7760340241111));
#30353=CARTESIAN_POINT('Ctrl Pts',(-0.308252937633149,2.344264234878,4.77706242917736));
#30354=CARTESIAN_POINT('Ctrl Pts',(-0.320848406880124,2.32836919237132,
4.77808891650145));
#30355=CARTESIAN_POINT('Ctrl Pts',(-0.332239266041854,2.31146160149699,
4.77911540382553));
#30356=CARTESIAN_POINT('Ctrl Pts',(-0.342263524440448,2.29375388986444,
4.78014189114962));
#30357=CARTESIAN_POINT('Ctrl Pts',(-0.352282526817308,2.27605546292045,
4.78116784025538));
#30358=CARTESIAN_POINT('Ctrl Pts',(-0.360935939505943,2.25755838482288,
4.78219378936113));
#30359=CARTESIAN_POINT('Ctrl Pts',(-0.368105650349287,2.23850314141177,
4.78321973846688));
#30360=CARTESIAN_POINT('Ctrl Pts',(-0.375273320297017,2.21945332217515,
4.78424539553086));
#30361=CARTESIAN_POINT('Ctrl Pts',(-0.380957869115705,2.19984636711062,
4.78527105259485));
#30362=CARTESIAN_POINT('Ctrl Pts',(-0.385090057524706,2.1799408380968,4.78629670965883));
#30363=CARTESIAN_POINT('Ctrl Pts',(-0.389227985100154,2.16000766243841,
4.78732379125046));
#30364=CARTESIAN_POINT('Ctrl Pts',(-0.391809133214506,2.13977583627541,
4.78835087284208));
#30365=CARTESIAN_POINT('Ctrl Pts',(-0.392815682131082,2.11951230052794,
4.78937795443371));
#30366=CARTESIAN_POINT('Ctrl Pts',(-0.393144211553025,2.11289844642109,
4.78971318555465));
#30367=CARTESIAN_POINT('Ctrl Pts',(-0.393305410862432,2.10628122371761,
4.79004841667559));
#30368=CARTESIAN_POINT('Ctrl Pts',(-0.393299861449716,2.09966987330631,
4.79038364779653));
#30369=CARTESIAN_POINT('',(-0.393440202014609,2.10025343067764,4.91538364779653));
#30370=CARTESIAN_POINT('Ctrl Pts',(-0.393533145238993,2.09966967749336,
4.79038364779653));
#30371=CARTESIAN_POINT('Ctrl Pts',(-0.39373784894553,2.07688450824866,4.79153828436481));
#30372=CARTESIAN_POINT('Ctrl Pts',(-0.381557546592789,1.92361338030581,
4.79931636877403));
#30373=CARTESIAN_POINT('Ctrl Pts',(-0.180195773708327,1.67127570200156,
4.81371790102414));
#30374=CARTESIAN_POINT('Ctrl Pts',(0.262935837116425,1.71641195809303,4.83358824454696));
#30375=CARTESIAN_POINT('Ctrl Pts',(0.464859613354694,2.11343802147946,4.85345858806974));
#30376=CARTESIAN_POINT('Ctrl Pts',(0.240337979009523,2.49813652976592,4.87332893159252));
#30377=CARTESIAN_POINT('Ctrl Pts',(-0.204661031884562,2.51759897328978,
4.89319927511531));
#30378=CARTESIAN_POINT('Ctrl Pts',(-0.386147435745799,2.26106486793884,
4.90721751384998));
#30379=CARTESIAN_POINT('Ctrl Pts',(-0.393853325308977,2.11545426420355,
4.91461230474372));
#30380=CARTESIAN_POINT('Ctrl Pts',(-0.393739520313072,2.10025362348061,
4.91538364779653));
#30381=CARTESIAN_POINT('',(-0.39310121130446,2.10019150475592,5.0403836450683));
#30382=CARTESIAN_POINT('Ctrl Pts',(-0.393299918406659,2.10025334031532,
4.91538364779653));
#30383=CARTESIAN_POINT('Ctrl Pts',(-0.393312967850958,2.07999464058418,
4.91641281199908));
#30384=CARTESIAN_POINT('Ctrl Pts',(-0.391756457283335,2.05967378052778,
4.91744197620162));
#30385=CARTESIAN_POINT('Ctrl Pts',(-0.388627900065919,2.03955791788535,
4.91847114040417));
#30386=CARTESIAN_POINT('Ctrl Pts',(-0.385504269603249,2.0194737330787,4.9194986839109));
#30387=CARTESIAN_POINT('Ctrl Pts',(-0.380813566429206,1.99959465497,4.92052622741762));
#30388=CARTESIAN_POINT('Ctrl Pts',(-0.374605164255451,1.98018405401139,
4.92155377092434));
#30389=CARTESIAN_POINT('Ctrl Pts',(-0.368396369260136,1.96077222489417,
4.92258137944639));
#30390=CARTESIAN_POINT('Ctrl Pts',(-0.360669872719226,1.94182966575812,
4.92360898796843));
#30391=CARTESIAN_POINT('Ctrl Pts',(-0.351525349917601,1.92360607049757,
4.92463659649047));
#30392=CARTESIAN_POINT('Ctrl Pts',(-0.342381329015625,1.90538347544406,
4.92566414861194));
#30393=CARTESIAN_POINT('Ctrl Pts',(-0.331819794710035,1.88788043413982,
4.9266917007334));
#30394=CARTESIAN_POINT('Ctrl Pts',(-0.319986573370135,1.87132231664887,
4.92771925285487));
#30395=CARTESIAN_POINT('Ctrl Pts',(-0.308127343858601,1.85472780616322,
4.92874906342745));
#30396=CARTESIAN_POINT('Ctrl Pts',(-0.294991322080486,1.83908295917413,
4.92977887400003));
#30397=CARTESIAN_POINT('Ctrl Pts',(-0.280765301029734,1.82458079998358,
4.93080868457261));
#30398=CARTESIAN_POINT('Ctrl Pts',(-0.270951327909145,1.81457633000714,
4.93151911043537));
#30399=CARTESIAN_POINT('Ctrl Pts',(-0.260619465562916,1.80511495377878,
4.93222953629813));
#30400=CARTESIAN_POINT('Ctrl Pts',(-0.249840037995042,1.79624871125436,
4.93293996216089));
#30401=CARTESIAN_POINT('Ctrl Pts',(-0.233999792961889,1.78321986967388,
4.93398392480855));
#30402=CARTESIAN_POINT('Ctrl Pts',(-0.217090450655174,1.77139461696758,
4.93502788745621));
#30403=CARTESIAN_POINT('Ctrl Pts',(-0.199321137606527,1.76094841970101,
4.93607185010387));
#30404=CARTESIAN_POINT('Ctrl Pts',(-0.181584513123947,1.75052143933994,
4.93711389226974));
#30405=CARTESIAN_POINT('Ctrl Pts',(-0.162991655113017,1.74146889867327,
4.93815593443562));
#30406=CARTESIAN_POINT('Ctrl Pts',(-0.143781906589812,1.73392397874567,
4.9391979766015));
#30407=CARTESIAN_POINT('Ctrl Pts',(-0.124592789034708,1.72638716194354,
4.94023889963046));
#30408=CARTESIAN_POINT('Ctrl Pts',(-0.104788767051975,1.72035504599876,
4.94127982265942));
#30409=CARTESIAN_POINT('Ctrl Pts',(-0.0846304468739844,1.71591332037949,
4.94232074568838));
#30410=CARTESIAN_POINT('Ctrl Pts',(-0.0644617739081169,1.7114693136057,
4.94336220330829));
#30411=CARTESIAN_POINT('Ctrl Pts',(-0.0439391543082961,1.70861750297522,
4.94440366092819));
#30412=CARTESIAN_POINT('Ctrl Pts',(-0.023335306402776,1.70739287643359,
4.94544511854809));
#30413=CARTESIAN_POINT('Ctrl Pts',(-0.00272516312345551,1.70616787571517,
4.9464868943787));
#30414=CARTESIAN_POINT('Ctrl Pts',(0.0179655218600142,1.70657105634623,
4.94752867020931));
#30415=CARTESIAN_POINT('Ctrl Pts',(0.0384629999241706,1.70858527411857,
4.94857044603992));
#30416=CARTESIAN_POINT('Ctrl Pts',(0.0590047837522991,1.71060384566834,
4.94961447369263));
#30417=CARTESIAN_POINT('Ctrl Pts',(0.0793518019106534,1.71424027701707,
4.95065850134533));
#30418=CARTESIAN_POINT('Ctrl Pts',(0.0992387451231446,1.71942601052307,
4.95170252899804));
#30419=CARTESIAN_POINT('Ctrl Pts',(0.106272496251066,1.72126013648739,4.95207178789325));
#30420=CARTESIAN_POINT('Ctrl Pts',(0.113248838991173,1.72328761667799,4.95244104678847));
#30421=CARTESIAN_POINT('Ctrl Pts',(0.120156595165249,1.72550396178558,4.95281030568368));
#30422=CARTESIAN_POINT('Ctrl Pts',(0.139686089288282,1.73176997605455,4.95385426833121));
#30423=CARTESIAN_POINT('Ctrl Pts',(0.158782306008209,1.73958643085733,4.95489823097873));
#30424=CARTESIAN_POINT('Ctrl Pts',(0.177184505924877,1.74887247208435,4.95594219362625));
#30425=CARTESIAN_POINT('Ctrl Pts',(0.19555285301185,1.7581414306379,4.956984235792));
#30426=CARTESIAN_POINT('Ctrl Pts',(0.213229041275652,1.76887433471324,4.95802627795774));
#30427=CARTESIAN_POINT('Ctrl Pts',(0.22997152901017,1.78094203372314,4.95906832012348));
#30428=CARTESIAN_POINT('Ctrl Pts',(0.246696035575856,1.79299677221387,4.9601092431523));
#30429=CARTESIAN_POINT('Ctrl Pts',(0.262488221597581,1.8063830551189,4.96115016618113));
#30430=CARTESIAN_POINT('Ctrl Pts',(0.277134966973898,1.82092814530953,4.96219108920995));
#30431=CARTESIAN_POINT('Ctrl Pts',(0.291789234536915,1.83548070547942,4.96323254682972));
#30432=CARTESIAN_POINT('Ctrl Pts',(0.305296352784089,1.85119275485768,4.96427400444948));
#30433=CARTESIAN_POINT('Ctrl Pts',(0.317479275865602,1.86785392659825,4.96531546206924));
#30434=CARTESIAN_POINT('Ctrl Pts',(0.329665921361247,1.88452018905314,4.96635723789971));
#30435=CARTESIAN_POINT('Ctrl Pts',(0.340527161506805,1.90213553639867,4.96739901373018));
#30436=CARTESIAN_POINT('Ctrl Pts',(0.349929226383304,1.92046051542131,4.96844078956065));
#30437=CARTESIAN_POINT('Ctrl Pts',(0.359351614036396,1.93882510430195,4.96948481721322));
#30438=CARTESIAN_POINT('Ctrl Pts',(0.367308246027899,1.95790170746229,4.97052884486579));
#30439=CARTESIAN_POINT('Ctrl Pts',(0.373713150145471,1.97743013662262,4.97157287251835));
#30440=CARTESIAN_POINT('Ctrl Pts',(0.375978480779071,1.98433708604621,4.97194213141439));
#30441=CARTESIAN_POINT('Ctrl Pts',(0.37805015951883,1.99130043160611,4.97231139031043));
#30442=CARTESIAN_POINT('Ctrl Pts',(0.379925910106522,1.99830834434561,4.97268064920647));
#30443=CARTESIAN_POINT('Ctrl Pts',(0.385229001164475,2.01812099941161,4.97372461185401));
#30444=CARTESIAN_POINT('Ctrl Pts',(0.38899391317474,2.03840862855515,4.97476857450155));
#30445=CARTESIAN_POINT('Ctrl Pts',(0.391147486771727,2.05890822962974,4.97581253714909));
#30446=CARTESIAN_POINT('Ctrl Pts',(0.39329709863802,2.0793701194792,4.97685457931485));
#30447=CARTESIAN_POINT('Ctrl Pts',(0.39384112082101,2.10004248996021,4.97789662148061));
#30448=CARTESIAN_POINT('Ctrl Pts',(0.392757394556891,2.12065233693515,4.97893866364636));
#30449=CARTESIAN_POINT('Ctrl Pts',(0.391674832197754,2.14124004925822,4.97997958667521));
#30450=CARTESIAN_POINT('Ctrl Pts',(0.388968001498133,2.16176463882623,4.98102050970405));
#30451=CARTESIAN_POINT('Ctrl Pts',(0.384666777166834,2.18195340471317,4.98206143273289));
#30452=CARTESIAN_POINT('Ctrl Pts',(0.380363343838828,2.20215253902407,4.98310289035267));
#30453=CARTESIAN_POINT('Ctrl Pts',(0.374464018572094,2.22201478211032,4.98414434797245));
#30454=CARTESIAN_POINT('Ctrl Pts',(0.36704984345978,2.24127739527664,4.98518580559222));
#30455=CARTESIAN_POINT('Ctrl Pts',(0.359633402993741,2.26054589401105,4.98622758142271));
#30456=CARTESIAN_POINT('Ctrl Pts',(0.350701489094281,2.27921372499669,4.98726935725319));
#30457=CARTESIAN_POINT('Ctrl Pts',(0.34038302623639,2.29703879173949,4.98831113308368));
#30458=CARTESIAN_POINT('Ctrl Pts',(0.330042259786875,2.31490238776855,4.98935516073626));
#30459=CARTESIAN_POINT('Ctrl Pts',(0.318309378958636,2.33191897638875,4.99039918838884));
#30460=CARTESIAN_POINT('Ctrl Pts',(0.305356616403787,2.34787542600756,4.99144321604143));
#30461=CARTESIAN_POINT('Ctrl Pts',(0.300775394068722,2.3535190130858,4.99181247493737));
#30462=CARTESIAN_POINT('Ctrl Pts',(0.296041925583385,2.35903030243214,4.99218173383332));
#30463=CARTESIAN_POINT('Ctrl Pts',(0.291164924766646,2.36440097689992,4.99255099272926));
#30464=CARTESIAN_POINT('Ctrl Pts',(0.277376748663788,2.37958485898965,4.99359495537683));
#30465=CARTESIAN_POINT('Ctrl Pts',(0.262356561740721,2.39373252464626,4.9946389180244));
#30466=CARTESIAN_POINT('Ctrl Pts',(0.246285898424623,2.40664009235124,4.99568288067196));
#30467=CARTESIAN_POINT('Ctrl Pts',(0.230244798825399,2.41952391519456,4.99672492283775));
#30468=CARTESIAN_POINT('Ctrl Pts',(0.213157588635871,2.43117166645398,4.99776696500354));
#30469=CARTESIAN_POINT('Ctrl Pts',(0.195241819683713,2.44141693257159,4.99880900716932));
#30470=CARTESIAN_POINT('Ctrl Pts',(0.177345291985949,2.45165119543434,4.99984993019819));
#30471=CARTESIAN_POINT('Ctrl Pts',(0.15862259322943,2.46048557490693,5.00089085322706));
#30472=CARTESIAN_POINT('Ctrl Pts',(0.13931918695498,2.46779757224077,5.00193177625593));
#30473=CARTESIAN_POINT('Ctrl Pts',(0.120005866954183,2.47511332482586,5.00297323387574));
#30474=CARTESIAN_POINT('Ctrl Pts',(0.100111925984529,2.48090485758819,5.00401469149554));
#30475=CARTESIAN_POINT('Ctrl Pts',(0.0799021489945708,2.48509808696753,
5.00505614911535));
#30476=CARTESIAN_POINT('Ctrl Pts',(0.0596861970366758,2.48929259756125,
5.00609792494586));
#30477=CARTESIAN_POINT('Ctrl Pts',(0.0391549441241704,2.49188771865266,
5.00713970077638));
#30478=CARTESIAN_POINT('Ctrl Pts',(0.0185817384717031,2.49286080104201,
5.00818147660689));
#30479=CARTESIAN_POINT('Ctrl Pts',(-0.00203593663165084,2.49383598677102,
5.0092255042595));
#30480=CARTESIAN_POINT('Ctrl Pts',(-0.0226950094075678,2.4931821573905,
5.01026953191211));
#30481=CARTESIAN_POINT('Ctrl Pts',(-0.0431230423504149,2.490928757216,5.01131355956473));
#30482=CARTESIAN_POINT('Ctrl Pts',(-0.050348169834772,2.4901317591115,5.0116828184605));
#30483=CARTESIAN_POINT('Ctrl Pts',(-0.0575444726095197,2.48913513456542,
5.01205207735628));
#30484=CARTESIAN_POINT('Ctrl Pts',(-0.0647002405212437,2.48794170809091,
5.01242133625205));
#30485=CARTESIAN_POINT('Ctrl Pts',(-0.0849309093009322,2.48456767248543,
5.0134652988996));
#30486=CARTESIAN_POINT('Ctrl Pts',(-0.104957218468869,2.47959681744548,
5.01450926154715));
#30487=CARTESIAN_POINT('Ctrl Pts',(-0.124509472928379,2.47307141561784,
5.01555322419469));
#30488=CARTESIAN_POINT('Ctrl Pts',(-0.144025758908919,2.46655801797001,
5.01659526636046));
#30489=CARTESIAN_POINT('Ctrl Pts',(-0.163069012335207,2.45849592392518,
5.01763730852622));
#30490=CARTESIAN_POINT('Ctrl Pts',(-0.181381544972989,2.44897797228939,
5.01867935069199));
#30491=CARTESIAN_POINT('Ctrl Pts',(-0.199674410238418,2.43947024278411,
5.01972027372083));
#30492=CARTESIAN_POINT('Ctrl Pts',(-0.217237449807466,2.42851007168722,
5.02076119674968));
#30493=CARTESIAN_POINT('Ctrl Pts',(-0.233834790689169,2.41623753835266,
5.02180211977853));
#30494=CARTESIAN_POINT('Ctrl Pts',(-0.25044065553257,2.40395870216485,5.02284357739832));
#30495=CARTESIAN_POINT('Ctrl Pts',(-0.266079229680419,2.39036658173983,
5.02388503501811));
#30496=CARTESIAN_POINT('Ctrl Pts',(-0.280544889471852,2.37564371023338,
5.02492649263789));
#30497=CARTESIAN_POINT('Ctrl Pts',(-0.295014969153004,2.36091634024783,
5.02596826846839));
#30498=CARTESIAN_POINT('Ctrl Pts',(-0.308310931608444,2.34505808113766,
5.02701004429888));
#30499=CARTESIAN_POINT('Ctrl Pts',(-0.320265764657819,2.3282865085548,5.02805182012937));
#30500=CARTESIAN_POINT('Ctrl Pts',(-0.332246438350117,2.31147868383721,
5.02909584778196));
#30501=CARTESIAN_POINT('Ctrl Pts',(-0.342879816280033,2.29375423590212,
5.03013987543456));
#30502=CARTESIAN_POINT('Ctrl Pts',(-0.35204318041083,2.27535817382212,5.03118390308715));
#30503=CARTESIAN_POINT('Ctrl Pts',(-0.355284142193057,2.2688517277949,5.03155316198304));
#30504=CARTESIAN_POINT('Ctrl Pts',(-0.358341651152754,2.2622614566997,5.03192242087894));
#30505=CARTESIAN_POINT('Ctrl Pts',(-0.361211743273508,2.2555987356032,5.03229167977484));
#30506=CARTESIAN_POINT('Ctrl Pts',(-0.37018587552907,2.23476590592863,5.03344626925451));
#30507=CARTESIAN_POINT('Ctrl Pts',(-0.377369900235882,2.21311751646781,
5.03460085873419));
#30508=CARTESIAN_POINT('Ctrl Pts',(-0.38263725037188,2.19095946695011,5.03575544821386));
#30509=CARTESIAN_POINT('Ctrl Pts',(-0.38786747216244,2.16895760445159,5.03690189925658));
#30510=CARTESIAN_POINT('Ctrl Pts',(-0.391207731046514,2.14645366367599,
5.03804835029929));
#30511=CARTESIAN_POINT('Ctrl Pts',(-0.392581187677273,2.12376764779909,
5.039194801342));
#30512=CARTESIAN_POINT('Ctrl Pts',(-0.393055934862718,2.11592602983656,
5.03959108207893));
#30513=CARTESIAN_POINT('Ctrl Pts',(-0.393296118158558,2.10806280903969,
5.03998736281586));
#30514=CARTESIAN_POINT('Ctrl Pts',(-0.393299953314656,2.10019163165046,
5.04038364355279));
#30515=CARTESIAN_POINT('',(-0.39324855931036,2.09966296070036,5.1653836507501));
#30516=CARTESIAN_POINT('Ctrl Pts',(-0.392743434489697,2.10019127631944,
5.04038364779653));
#30517=CARTESIAN_POINT('Ctrl Pts',(-0.392401791420311,2.02231826806415,
5.04430977296356));
#30518=CARTESIAN_POINT('Ctrl Pts',(-0.332252156026397,1.8125855117155,5.05485934597154));
#30519=CARTESIAN_POINT('Ctrl Pts',(0.00931989327823174,1.63503959300418,
5.07203236682041));
#30520=CARTESIAN_POINT('Ctrl Pts',(0.395992061663179,1.85614486352699,5.09190271034321));
#30521=CARTESIAN_POINT('Ctrl Pts',(0.419395422923265,2.30095402388483,5.111773053866));
#30522=CARTESIAN_POINT('Ctrl Pts',(0.0580605791824544,2.56141522474824,
5.13164339738879));
#30523=CARTESIAN_POINT('Ctrl Pts',(-0.314803622727929,2.41498065574447,
5.14951359536563));
#30524=CARTESIAN_POINT('Ctrl Pts',(-0.392294629728231,2.19119159158929,
5.16076034550154));
#30525=CARTESIAN_POINT('Ctrl Pts',(-0.393038228349958,2.09966319944716,
5.16538364779653));
#30526=CARTESIAN_POINT('',(-0.393299999049727,2.09997265983606,5.29038364779291));
#30527=CARTESIAN_POINT('Ctrl Pts',(-0.393299855536788,2.09966290247398,
5.16538365147043));
#30528=CARTESIAN_POINT('Ctrl Pts',(-0.393278448914784,2.0746872776426,5.16664439623088));
#30529=CARTESIAN_POINT('Ctrl Pts',(-0.390874000548172,2.04981650347134,
5.16790514099134));
#30530=CARTESIAN_POINT('Ctrl Pts',(-0.386169426696434,2.02544757626376,
5.16916588575179));
#30531=CARTESIAN_POINT('Ctrl Pts',(-0.383410295784998,2.01115572700049,
5.16990528531265));
#30532=CARTESIAN_POINT('Ctrl Pts',(-0.379860949704092,1.99703607904903,
5.17064468487351));
#30533=CARTESIAN_POINT('Ctrl Pts',(-0.375545661273262,1.98316530353175,
5.17138408443437));
#30534=CARTESIAN_POINT('Ctrl Pts',(-0.369452879814242,1.9635810728949,5.17242804708192));
#30535=CARTESIAN_POINT('Ctrl Pts',(-0.361805880791454,1.94441636927946,
5.17347200972948));
#30536=CARTESIAN_POINT('Ctrl Pts',(-0.35268320558326,1.92593263804057,5.17451597237703));
#30537=CARTESIAN_POINT('Ctrl Pts',(-0.343577312519135,1.90748290961703,
5.1755580145428));
#30538=CARTESIAN_POINT('Ctrl Pts',(-0.33300140040825,1.88971234562842,5.17660005670857));
#30539=CARTESIAN_POINT('Ctrl Pts',(-0.321082475259915,1.87286362228616,
5.17764209887434));
#30540=CARTESIAN_POINT('Ctrl Pts',(-0.309176350849944,1.85603299420807,
5.17868302190319));
#30541=CARTESIAN_POINT('Ctrl Pts',(-0.295930476018805,1.84012285563736,
5.17972394493204));
#30542=CARTESIAN_POINT('Ctrl Pts',(-0.281515693358266,1.82534784837359,
5.1807648679609));
#30543=CARTESIAN_POINT('Ctrl Pts',(-0.267093507641053,1.81056525305118,
5.18180632558069));
#30544=CARTESIAN_POINT('Ctrl Pts',(-0.251501717063482,1.79691949159882,
5.18284778320048));
#30545=CARTESIAN_POINT('Ctrl Pts',(-0.234949111994465,1.78458946629351,
5.18388924082027));
#30546=CARTESIAN_POINT('Ctrl Pts',(-0.218391449382962,1.77225567362793,
5.18493101665077));
#30547=CARTESIAN_POINT('Ctrl Pts',(-0.20087299903073,1.76123882757827,5.18597279248126));
#30548=CARTESIAN_POINT('Ctrl Pts',(-0.182632019859586,1.75167481382764,
5.18701456831176));
#30549=CARTESIAN_POINT('Ctrl Pts',(-0.164351612398027,1.74209012724426,
5.18805859596436));
#30550=CARTESIAN_POINT('Ctrl Pts',(-0.145346235321096,1.73396483198983,
5.18910262361695));
#30551=CARTESIAN_POINT('Ctrl Pts',(-0.125875305182518,1.72738720158158,
5.19014665126955));
#30552=CARTESIAN_POINT('Ctrl Pts',(-0.118988692412658,1.72506077992414,
5.19051591016542));
#30553=CARTESIAN_POINT('Ctrl Pts',(-0.112043970402749,1.72292750302154,
5.19088516906128));
#30554=CARTESIAN_POINT('Ctrl Pts',(-0.105052947482939,1.72098975182042,
5.19125442795715));
#30555=CARTESIAN_POINT('Ctrl Pts',(-0.0852880430265416,1.71551137365034,
5.1922983906047));
#30556=CARTESIAN_POINT('Ctrl Pts',(-0.0650345583509261,1.71156690699225,
5.19334235325226));
#30557=CARTESIAN_POINT('Ctrl Pts',(-0.0445548372589666,1.70923183794374,
5.19438631589981));
#30558=CARTESIAN_POINT('Ctrl Pts',(-0.0241127908207696,1.70690106450636,
5.19542835806558));
#30559=CARTESIAN_POINT('Ctrl Pts',(-0.00344605012792134,1.70617395338364,
5.19647040023135));
#30560=CARTESIAN_POINT('Ctrl Pts',(0.0171725876683758,1.70707508066709,
5.19751244239712));
#30561=CARTESIAN_POINT('Ctrl Pts',(0.0377690813715958,1.707975240154,5.19855336542598));
#30562=CARTESIAN_POINT('Ctrl Pts',(0.0583168421269406,1.71050016338497,
5.19959428845483));
#30563=CARTESIAN_POINT('Ctrl Pts',(0.0785429150844682,1.71462239233444,
5.20063521148369));
#30564=CARTESIAN_POINT('Ctrl Pts',(0.098779375625906,1.71874673835325,5.20167666910348));
#30565=CARTESIAN_POINT('Ctrl Pts',(0.11869309413943,1.72446989779485,5.20271812672327));
#30566=CARTESIAN_POINT('Ctrl Pts',(0.138020624388094,1.7317131590139,5.20375958434306));
#30567=CARTESIAN_POINT('Ctrl Pts',(0.157354060039858,1.73895863336503,5.20480136017356));
#30568=CARTESIAN_POINT('Ctrl Pts',(0.176100275162223,1.74772484224979,5.20584313600406));
#30569=CARTESIAN_POINT('Ctrl Pts',(0.194016040780442,1.75788501067641,5.20688491183456));
#30570=CARTESIAN_POINT('Ctrl Pts',(0.211970531732606,1.76806714053764,5.20792893948716));
#30571=CARTESIAN_POINT('Ctrl Pts',(0.229090379478053,1.7796488327275,5.20897296713976));
#30572=CARTESIAN_POINT('Ctrl Pts',(0.245160935195129,1.79245974921281,5.21001699479235));
#30573=CARTESIAN_POINT('Ctrl Pts',(0.25084488010337,1.79699080245132,5.21038625368822));
#30574=CARTESIAN_POINT('Ctrl Pts',(0.256397881025208,1.80167526772497,5.21075551258409));
#30575=CARTESIAN_POINT('Ctrl Pts',(0.26181154395561,1.8065045052278,5.21112477147995));
#30576=CARTESIAN_POINT('Ctrl Pts',(0.277116962319406,1.8201576456817,5.2121687341275));
#30577=CARTESIAN_POINT('Ctrl Pts',(0.291397117720928,1.83505192714911,5.21321269677506));
#30578=CARTESIAN_POINT('Ctrl Pts',(0.304446528657043,1.85100762825204,5.21425665942261));
#30579=CARTESIAN_POINT('Ctrl Pts',(0.317471933795589,1.86693397712346,5.21529870158838));
#30580=CARTESIAN_POINT('Ctrl Pts',(0.329270582007397,1.88391734433447,5.21634074375415));
#30581=CARTESIAN_POINT('Ctrl Pts',(0.33967413924762,1.90174166063848,5.21738278591992));
#30582=CARTESIAN_POINT('Ctrl Pts',(0.350066523230802,1.91954683390678,5.21842370894877));
#30583=CARTESIAN_POINT('Ctrl Pts',(0.359066396742351,1.93819054561226,5.21946463197762));
#30584=CARTESIAN_POINT('Ctrl Pts',(0.366549091589525,1.95742842690461,5.22050555500647));
#30585=CARTESIAN_POINT('Ctrl Pts',(0.37403562935375,1.9766761882714,5.22154701262627));
#30586=CARTESIAN_POINT('Ctrl Pts',(0.380003150075041,1.9965180489571,5.22258847024606));
#30587=CARTESIAN_POINT('Ctrl Pts',(0.38437522770585,2.01668989061299,5.22362992786585));
#30588=CARTESIAN_POINT('Ctrl Pts',(0.388748641196982,2.03686789564592,5.22467170369634));
#30589=CARTESIAN_POINT('Ctrl Pts',(0.391525520781456,2.05737535622491,5.22571347952684));
#30590=CARTESIAN_POINT('Ctrl Pts',(0.392680796903289,2.07793913547937,5.22675525535734));
#30591=CARTESIAN_POINT('Ctrl Pts',(0.393838570180677,2.09854736380935,5.22779928300993));
#30592=CARTESIAN_POINT('Ctrl Pts',(0.393367758945009,2.11921141756431,5.22884331066253));
#30593=CARTESIAN_POINT('Ctrl Pts',(0.391295393178771,2.1396586091167,5.22988733831512));
#30594=CARTESIAN_POINT('Ctrl Pts',(0.39056242457131,2.14689051275205,5.23025659721099));
#30595=CARTESIAN_POINT('Ctrl Pts',(0.389629582032103,2.15409536104576,5.23062585610686));
#30596=CARTESIAN_POINT('Ctrl Pts',(0.38849958623811,2.16126141928504,5.23099511500273));
#30597=CARTESIAN_POINT('Ctrl Pts',(0.385304880805083,2.1815211807037,5.23203907765028));
#30598=CARTESIAN_POINT('Ctrl Pts',(0.380511608419225,2.2015907347236,5.23308304029783));
#30599=CARTESIAN_POINT('Ctrl Pts',(0.374159651182492,2.22120002238859,5.23412700294539));
#30600=CARTESIAN_POINT('Ctrl Pts',(0.367819379055558,2.24077323665591,5.23516904511116));
#30601=CARTESIAN_POINT('Ctrl Pts',(0.359926281292902,2.25988715486123,5.23621108727693));
#30602=CARTESIAN_POINT('Ctrl Pts',(0.35057091052557,2.27828327653842,5.2372531294427));
#30603=CARTESIAN_POINT('Ctrl Pts',(0.341225587279472,2.29665964106992,5.23829405247155));
#30604=CARTESIAN_POINT('Ctrl Pts',(0.330421414822523,2.31431907387229,5.23933497550041));
#30605=CARTESIAN_POINT('Ctrl Pts',(0.318296377713979,2.33102447042285,5.24037589852926));
#30606=CARTESIAN_POINT('Ctrl Pts',(0.306165113502394,2.34773844642969,5.24141735614905));
#30607=CARTESIAN_POINT('Ctrl Pts',(0.292712048574248,2.36349680240577,5.24245881376884));
#30608=CARTESIAN_POINT('Ctrl Pts',(0.27811788756555,2.3780923059275,5.24350027138864));
#30609=CARTESIAN_POINT('Ctrl Pts',(0.263519267404413,2.39269226901187,5.24454204721914));
#30610=CARTESIAN_POINT('Ctrl Pts',(0.24777940247025,2.40612817804252,5.24558382304964));
#30611=CARTESIAN_POINT('Ctrl Pts',(0.231114380530547,2.41823110016462,5.24662559888013));
#30612=CARTESIAN_POINT('Ctrl Pts',(0.214413336767746,2.43036018302753,5.24766962653273));
#30613=CARTESIAN_POINT('Ctrl Pts',(0.196783771764517,2.44115014218432,5.24871365418533));
#30614=CARTESIAN_POINT('Ctrl Pts',(0.178469597978355,2.45047609418824,5.24975768183793));
#30615=CARTESIAN_POINT('Ctrl Pts',(0.17199211476789,2.45377456116974,5.25012694073379));
#30616=CARTESIAN_POINT('Ctrl Pts',(0.165429184802336,2.45689032502551,5.25049619962966));
#30617=CARTESIAN_POINT('Ctrl Pts',(0.158792147589922,2.4598193211374,5.25086545852552));
#30618=CARTESIAN_POINT('Ctrl Pts',(0.140028025675,2.46810013053666,5.25190942117308));
#30619=CARTESIAN_POINT('Ctrl Pts',(0.120558500370676,2.47493387351884,5.25295338382063));
#30620=CARTESIAN_POINT('Ctrl Pts',(0.100632230984904,2.48020789587672,5.25399734646818));
#30621=CARTESIAN_POINT('Ctrl Pts',(0.0807426181188446,2.48547221610216,
5.25503938863395));
#30622=CARTESIAN_POINT('Ctrl Pts',(0.0603986170307354,2.48918226747339,
5.25608143079972));
#30623=CARTESIAN_POINT('Ctrl Pts',(0.0398665973161565,2.49127425729075,
5.25712347296549));
#30624=CARTESIAN_POINT('Ctrl Pts',(0.0193566286682032,2.49336400034392,
5.25816439599434));
#30625=CARTESIAN_POINT('Ctrl Pts',(-0.00134023238324855,2.49383902876169,
5.2592053190232));
#30626=CARTESIAN_POINT('Ctrl Pts',(-0.0219499305751598,2.49268701346969,
5.26024624205205));
#30627=CARTESIAN_POINT('Ctrl Pts',(-0.0425702133709115,2.49153440653266,
5.26128769967184));
#30628=CARTESIAN_POINT('Ctrl Pts',(-0.0631025083463235,2.48875311149752,
5.26232915729163));
#30629=CARTESIAN_POINT('Ctrl Pts',(-0.0832747520846534,2.48438288940227,
5.26337061491142));
#30630=CARTESIAN_POINT('Ctrl Pts',(-0.10345315932288,2.48001133201365,5.26441239074192));
#30631=CARTESIAN_POINT('Ctrl Pts',(-0.123270585487693,2.47405007209419,
5.26545416657242));
#30632=CARTESIAN_POINT('Ctrl Pts',(-0.142468016597115,2.46658935370096,
5.26649594240292));
#30633=CARTESIAN_POINT('Ctrl Pts',(-0.161706943389524,2.45911250879561,
5.26753997005552));
#30634=CARTESIAN_POINT('Ctrl Pts',(-0.180322536318393,2.45013005474816,
5.26858399770811));
#30635=CARTESIAN_POINT('Ctrl Pts',(-0.198077756925285,2.43977947585375,
5.26962802536071));
#30636=CARTESIAN_POINT('Ctrl Pts',(-0.204357545722892,2.43611861177163,
5.26999728425658));
#30637=CARTESIAN_POINT('Ctrl Pts',(-0.210529968333663,2.43228700202477,
5.27036654315244));
#30638=CARTESIAN_POINT('Ctrl Pts',(-0.216585468873167,2.42829198082346,
5.27073580204831));
#30639=CARTESIAN_POINT('Ctrl Pts',(-0.233671942193388,2.41701944889573,
5.27177771959605));
#30640=CARTESIAN_POINT('Ctrl Pts',(-0.249927900178604,2.40437512782881,
5.27281963714379));
#30641=CARTESIAN_POINT('Ctrl Pts',(-0.265124530554396,2.39050623624685,
5.27386155469154));
#30642=CARTESIAN_POINT('Ctrl Pts',(-0.280293205464843,2.37666285764431,
5.27490155554531));
#30643=CARTESIAN_POINT('Ctrl Pts',(-0.294405840299752,2.36159982764347,
5.27594155639907));
#30644=CARTESIAN_POINT('Ctrl Pts',(-0.307265055974466,2.34550575426455,
5.27698155725284));
#30645=CARTESIAN_POINT('Ctrl Pts',(-0.320110565501371,2.32942883494497,
5.27802044960934));
#30646=CARTESIAN_POINT('Ctrl Pts',(-0.331704826296372,2.31232361015645,
5.27905934196584));
#30647=CARTESIAN_POINT('Ctrl Pts',(-0.34188954617818,2.29441303509302,5.28009823432234));
#30648=CARTESIAN_POINT('Ctrl Pts',(-0.352079545237533,2.27649317620963,
5.28113766518135));
#30649=CARTESIAN_POINT('Ctrl Pts',(-0.360858165496563,2.25776776814142,
5.28217709604036));
#30650=CARTESIAN_POINT('Ctrl Pts',(-0.368111998054116,2.2384862696754,5.28321652689937));
#30651=CARTESIAN_POINT('Ctrl Pts',(-0.375368208515285,2.21919845047554,
5.28425629849776));
#30652=CARTESIAN_POINT('Ctrl Pts',(-0.381098411966207,2.19935488235279,
5.28529607009615));
#30653=CARTESIAN_POINT('Ctrl Pts',(-0.385238720190411,2.17922132582868,
5.28633584169454));
#30654=CARTESIAN_POINT('Ctrl Pts',(-0.389387870101292,2.15904477381032,
5.28737783373985));
#30655=CARTESIAN_POINT('Ctrl Pts',(-0.391940259039512,2.13857773128581,
5.28841982578517));
#30656=CARTESIAN_POINT('Ctrl Pts',(-0.392883617329559,2.11809290562736,
5.28946181783049));
#30657=CARTESIAN_POINT('Ctrl Pts',(-0.393161807532951,2.11205206422437,
5.28976909448463));
#30658=CARTESIAN_POINT('Ctrl Pts',(-0.393300418711213,2.10600967052975,
5.29007637113877));
#30659=CARTESIAN_POINT('Ctrl Pts',(-0.393299999049727,2.09997265983607,
5.29038364779291));
#30660=CARTESIAN_POINT('',(-0.393299842496665,2.10035198309414,5.41538364779399));
#30661=CARTESIAN_POINT('Ctrl Pts',(-0.393299999049722,2.09997265976493,
5.29038364779653));
#30662=CARTESIAN_POINT('Ctrl Pts',(-0.393299897757734,2.09851553480785,
5.29045781372138));
#30663=CARTESIAN_POINT('Ctrl Pts',(-0.393291698817535,2.09705844255106,
5.29053197964624));
#30664=CARTESIAN_POINT('Ctrl Pts',(-0.393275403094208,2.09560144102145,
5.2906061455711));
#30665=CARTESIAN_POINT('Ctrl Pts',(-0.3930460238139,2.07509262680193,5.29165010821865));
#30666=CARTESIAN_POINT('Ctrl Pts',(-0.391207378815338,2.05454069639888,
5.29269407086621));
#30667=CARTESIAN_POINT('Ctrl Pts',(-0.387759851386128,2.03421863749505,
5.29373803351376));
#30668=CARTESIAN_POINT('Ctrl Pts',(-0.384318666055116,2.01393396320839,
5.29478007567953));
#30669=CARTESIAN_POINT('Ctrl Pts',(-0.379274536245748,1.99387904820193,
5.2958221178453));
#30670=CARTESIAN_POINT('Ctrl Pts',(-0.372679655033211,1.97432277563406,
5.29686416001107));
#30671=CARTESIAN_POINT('Ctrl Pts',(-0.366091856619499,1.95478750619573,
5.29790508303992));
#30672=CARTESIAN_POINT('Ctrl Pts',(-0.357956819701436,1.93575051894137,
5.29894600606878));
#30673=CARTESIAN_POINT('Ctrl Pts',(-0.348376766162668,1.91746638994957,
5.29998692909763));
#30674=CARTESIAN_POINT('Ctrl Pts',(-0.338791792558084,1.89917287070565,
5.30102838671742));
#30675=CARTESIAN_POINT('Ctrl Pts',(-0.327760646938449,1.8816336413797,5.30206984433721));
#30676=CARTESIAN_POINT('Ctrl Pts',(-0.31543214428506,1.86507990219709,5.30311130195701));
#30677=CARTESIAN_POINT('Ctrl Pts',(-0.303099874736633,1.84852110512548,
5.3041530777875));
#30678=CARTESIAN_POINT('Ctrl Pts',(-0.289469927148838,1.8329489656328,5.305194853618));
#30679=CARTESIAN_POINT('Ctrl Pts',(-0.27473166938063,1.81856190762562,5.3062366294485));
#30680=CARTESIAN_POINT('Ctrl Pts',(-0.259961554533801,1.80414375166606,
5.3072806571011));
#30681=CARTESIAN_POINT('Ctrl Pts',(-0.24407891265205,1.79091626257462,5.3083246847537));
#30682=CARTESIAN_POINT('Ctrl Pts',(-0.227307017618983,1.77903830486931,
5.30936871240629));
#30683=CARTESIAN_POINT('Ctrl Pts',(-0.221375018187665,1.7748372269223,5.30973797130216));
#30684=CARTESIAN_POINT('Ctrl Pts',(-0.215332033182601,1.77080456448087,
5.31010723019802));
#30685=CARTESIAN_POINT('Ctrl Pts',(-0.209188694587853,1.76694598027252,
5.31047648909389));
#30686=CARTESIAN_POINT('Ctrl Pts',(-0.191820349245343,1.75603705477052,
5.31152045174144));
#30687=CARTESIAN_POINT('Ctrl Pts',(-0.173544626432881,1.74645788912813,
5.312564414389));
#30688=CARTESIAN_POINT('Ctrl Pts',(-0.154591266562296,1.73835593423552,
5.31360837703655));
#30689=CARTESIAN_POINT('Ctrl Pts',(-0.135672773439533,1.73026888376197,
5.31465041920232));
#30690=CARTESIAN_POINT('Ctrl Pts',(-0.116079763223746,1.7236539905554,5.31569246136809));
#30691=CARTESIAN_POINT('Ctrl Pts',(-0.0960665707433878,1.71861292105578,
5.31673450353386));
#30692=CARTESIAN_POINT('Ctrl Pts',(-0.0760748721173508,1.71357726558561,
5.31777542656271));
#30693=CARTESIAN_POINT('Ctrl Pts',(-0.0556645899138119,1.71011228510182,
5.31881634959157));
#30694=CARTESIAN_POINT('Ctrl Pts',(-0.0351051108103078,1.70826983624567,
5.31985727262042));
#30695=CARTESIAN_POINT('Ctrl Pts',(-0.0145350728941838,1.7064264411558,
5.32089873024021));
#30696=CARTESIAN_POINT('Ctrl Pts',(0.00618358359623564,1.70620732415075,
5.32194018786001));
#30697=CARTESIAN_POINT('Ctrl Pts',(0.0267759051336634,1.70761251178934,
5.3229816454798));
#30698=CARTESIAN_POINT('Ctrl Pts',(0.047374518523068,1.709018128774,5.3240234213103));
#30699=CARTESIAN_POINT('Ctrl Pts',(0.0678459891248714,1.71204895226355,
5.32506519714079));
#30700=CARTESIAN_POINT('Ctrl Pts',(0.0879209703220723,1.71665316881755,
5.32610697297129));
#30701=CARTESIAN_POINT('Ctrl Pts',(0.108039344046691,1.72126733749012,5.32715100062389));
#30702=CARTESIAN_POINT('Ctrl Pts',(0.127758814736537,1.72746146830245,5.32819502827648));
#30703=CARTESIAN_POINT('Ctrl Pts',(0.146824944072981,1.73513382480974,5.32923905592908));
#30704=CARTESIAN_POINT('Ctrl Pts',(0.153568384105152,1.73784743673901,5.32960831482495));
#30705=CARTESIAN_POINT('Ctrl Pts',(0.160230295861298,1.74074553368207,5.32997757372081));
#30706=CARTESIAN_POINT('Ctrl Pts',(0.166800162733676,1.74382224141306,5.33034683261668));
#30707=CARTESIAN_POINT('Ctrl Pts',(0.185374381773336,1.75252065866055,5.33139079526423));
#30708=CARTESIAN_POINT('Ctrl Pts',(0.203321694734255,1.76270183817006,5.33243475791179));
#30709=CARTESIAN_POINT('Ctrl Pts',(0.220393759631902,1.77425242792107,5.33347872055934));
#30710=CARTESIAN_POINT('Ctrl Pts',(0.237434418626551,1.78578176911759,5.33452076272511));
#30711=CARTESIAN_POINT('Ctrl Pts',(0.253602389723254,1.79867516169156,5.33556280489088));
#30712=CARTESIAN_POINT('Ctrl Pts',(0.268674513920839,1.81277379024643,5.33660484705665));
#30713=CARTESIAN_POINT('Ctrl Pts',(0.283730450893813,1.82685727709572,5.3376457700855));
#30714=CARTESIAN_POINT('Ctrl Pts',(0.297692323070091,1.84214295126189,5.33868669311436));
#30715=CARTESIAN_POINT('Ctrl Pts',(0.310370704581198,1.85843237854015,5.33972761614321));
#30716=CARTESIAN_POINT('Ctrl Pts',(0.323055597378609,1.8747301716437,5.340769073763));
#30717=CARTESIAN_POINT('Ctrl Pts',(0.334455218000237,1.8920321769816,5.34181053138279));
#30718=CARTESIAN_POINT('Ctrl Pts',(0.344420706802546,1.91010722308199,5.34285198900258));
#30719=CARTESIAN_POINT('Ctrl Pts',(0.354389240496144,1.92818779189697,5.34389376483308));
#30720=CARTESIAN_POINT('Ctrl Pts',(0.362922446773869,1.94704121042643,5.34493554066358));
#30721=CARTESIAN_POINT('Ctrl Pts',(0.36991808911354,1.9664129596608,5.34597731649408));
#30722=CARTESIAN_POINT('Ctrl Pts',(0.37692885269288,1.98582658137074,5.34702134414668));
#30723=CARTESIAN_POINT('Ctrl Pts',(0.382395222396415,2.0057600603213,5.34806537179927));
#30724=CARTESIAN_POINT('Ctrl Pts',(0.386265007989182,2.02594438844276,5.34910939945187));
#30725=CARTESIAN_POINT('Ctrl Pts',(0.387633700429152,2.03308332072814,5.34947865834774));
#30726=CARTESIAN_POINT('Ctrl Pts',(0.388803141837507,2.04025356765072,5.3498479172436));
#30727=CARTESIAN_POINT('Ctrl Pts',(0.389772578538716,2.04744310683383,5.35021717613947));
#30728=CARTESIAN_POINT('Ctrl Pts',(0.39251335395823,2.06776925318883,5.35126113878702));
#30729=CARTESIAN_POINT('Ctrl Pts',(0.393668040731998,2.0883709316927,5.35230510143458));
#30730=CARTESIAN_POINT('Ctrl Pts',(0.393197515264884,2.10897797246158,5.35334906408213));
#30731=CARTESIAN_POINT('Ctrl Pts',(0.39272785538007,2.12954710435845,5.3543911062479));
#30732=CARTESIAN_POINT('Ctrl Pts',(0.390638874946974,2.15012085030323,5.35543314841367));
#30733=CARTESIAN_POINT('Ctrl Pts',(0.386943308794926,2.17042560456847,5.35647519057944));
#30734=CARTESIAN_POINT('Ctrl Pts',(0.38325171162287,2.19070855184661,5.35751611360829));
#30735=CARTESIAN_POINT('Ctrl Pts',(0.377957056787415,2.2107223555719,5.35855703663715));
#30736=CARTESIAN_POINT('Ctrl Pts',(0.371123651675472,2.23020032706204,5.359597959666));
#30737=CARTESIAN_POINT('Ctrl Pts',(0.364286737104763,2.24968830193069,5.36063941728579));
#30738=CARTESIAN_POINT('Ctrl Pts',(0.355909721855467,2.26863919516935,5.36168087490559));
#30739=CARTESIAN_POINT('Ctrl Pts',(0.346106398625333,2.28680270562977,5.36272233252538));
#30740=CARTESIAN_POINT('Ctrl Pts',(0.336300080052563,2.3049717658345,5.36376410835588));
#30741=CARTESIAN_POINT('Ctrl Pts',(0.325066966937527,2.32235233456427,5.36480588418637));
#30742=CARTESIAN_POINT('Ctrl Pts',(0.312565720943722,2.338720673782,5.36584766001687));
#30743=CARTESIAN_POINT('Ctrl Pts',(0.300037453223013,2.35512439353639,5.36689168766947));
#30744=CARTESIAN_POINT('Ctrl Pts',(0.286236071916274,2.37051096738615,5.36793571532207));
#30745=CARTESIAN_POINT('Ctrl Pts',(0.271359512307732,2.38469089391849,5.36897974297466));
#30746=CARTESIAN_POINT('Ctrl Pts',(0.266097868172478,2.38970614806599,5.36934900187053));
#30747=CARTESIAN_POINT('Ctrl Pts',(0.260702035945947,2.39457081955757,5.36971826076639));
#30748=CARTESIAN_POINT('Ctrl Pts',(0.255181716279521,2.39927776675964,5.37008751966226));
#30749=CARTESIAN_POINT('Ctrl Pts',(0.239574759754362,2.41258517009638,5.37113148230981));
#30750=CARTESIAN_POINT('Ctrl Pts',(0.222877552422454,2.42470811223257,5.37217544495737));
#30751=CARTESIAN_POINT('Ctrl Pts',(0.205296079650398,2.43546744950915,5.37321940760492));
#30752=CARTESIAN_POINT('Ctrl Pts',(0.187746949892017,2.44620699382543,5.37426144977069));
#30753=CARTESIAN_POINT('Ctrl Pts',(0.169317373087481,2.45558748209929,5.37530349193646));
#30754=CARTESIAN_POINT('Ctrl Pts',(0.150244295424405,2.46347151427921,5.37634553410223));
#30755=CARTESIAN_POINT('Ctrl Pts',(0.131191701947108,2.47134707913243,5.37738645713108));
#30756=CARTESIAN_POINT('Ctrl Pts',(0.111497645109286,2.47772907213223,5.37842738015994));
#30757=CARTESIAN_POINT('Ctrl Pts',(0.091421172280401,2.48252720067843,5.37946830318879));
#30758=CARTESIAN_POINT('Ctrl Pts',(0.0713343886983286,2.4873277934184,5.38050976080858));
#30759=CARTESIAN_POINT('Ctrl Pts',(0.0508655086416936,2.49054270994249,
5.38155121842837));
#30760=CARTESIAN_POINT('Ctrl Pts',(0.0302865878408223,2.49213213665416,
5.38259267604817));
#30761=CARTESIAN_POINT('Ctrl Pts',(0.00970137928248253,2.49372204900499,
5.38363445187866));
#30762=CARTESIAN_POINT('Ctrl Pts',(-0.0109932011925229,2.49368546227628,
5.38467622770916));
#30763=CARTESIAN_POINT('Ctrl Pts',(-0.0315231442114445,2.49203466859326,
5.38571800353966));
#30764=CARTESIAN_POINT('Ctrl Pts',(-0.0520974631680873,2.49038030668223,
5.38676203119226));
#30765=CARTESIAN_POINT('Ctrl Pts',(-0.0725057070245646,2.48710488861692,
5.38780605884485));
#30766=CARTESIAN_POINT('Ctrl Pts',(-0.0924813936542848,2.48227226138939,
5.38885008649745));
#30767=CARTESIAN_POINT('Ctrl Pts',(-0.099546532178845,2.4805630244839,5.38921934539332));
#30768=CARTESIAN_POINT('Ctrl Pts',(-0.106557696548657,2.47865944671621,
5.38958860428918));
#30769=CARTESIAN_POINT('Ctrl Pts',(-0.113503630812447,2.47656581867237,
5.38995786318505));
#30770=CARTESIAN_POINT('Ctrl Pts',(-0.133141061365718,2.47064674806877,
5.3910018258326));
#30771=CARTESIAN_POINT('Ctrl Pts',(-0.152372748195794,2.46316980481688,
5.39204578848016));
#30772=CARTESIAN_POINT('Ctrl Pts',(-0.170936560505818,2.45421121140139,
5.39308975112771));
#30773=CARTESIAN_POINT('Ctrl Pts',(-0.189466222682733,2.44526909828384,
5.39413179329348));
#30774=CARTESIAN_POINT('Ctrl Pts',(-0.20732976810087,2.43485100793367,5.39517383545925));
#30775=CARTESIAN_POINT('Ctrl Pts',(-0.224283405084158,2.42308179181727,
5.39621587762502));
#30776=CARTESIAN_POINT('Ctrl Pts',(-0.241218834127655,2.41132521565409,
5.39725680065387));
#30777=CARTESIAN_POINT('Ctrl Pts',(-0.257245676922874,2.39822078818098,
5.39829772368273));
#30778=CARTESIAN_POINT('Ctrl Pts',(-0.272147786813168,2.38393744404832,
5.39933864671158));
#30779=CARTESIAN_POINT('Ctrl Pts',(-0.287057550038711,2.36964676436238,
5.40038010433137));
#30780=CARTESIAN_POINT('Ctrl Pts',(-0.300840884037119,2.35417645593242,
5.40142156195116));
#30781=CARTESIAN_POINT('Ctrl Pts',(-0.31331704414102,2.3377337162683,5.40246301957095));
#30782=CARTESIAN_POINT('Ctrl Pts',(-0.325797016255748,2.32128595263036,
5.40350479540145));
#30783=CARTESIAN_POINT('Ctrl Pts',(-0.336968603817644,2.30386577378592,
5.40454657123195));
#30784=CARTESIAN_POINT('Ctrl Pts',(-0.346693816041194,2.28571022567106,
5.40558834706245));
#30785=CARTESIAN_POINT('Ctrl Pts',(-0.356440049531657,2.26751543392694,
5.40663237471505));
#30786=CARTESIAN_POINT('Ctrl Pts',(-0.364733370531078,2.24858277411358,
5.40767640236764));
#30787=CARTESIAN_POINT('Ctrl Pts',(-0.371483211143384,2.22917087070466,
5.40872043002024));
#30788=CARTESIAN_POINT('Ctrl Pts',(-0.373870541292716,2.22230513491535,
5.40908968891611));
#30789=CARTESIAN_POINT('Ctrl Pts',(-0.376065248980338,2.2153795813415,5.40945894781197));
#30790=CARTESIAN_POINT('Ctrl Pts',(-0.378064848758017,2.20840599676022,
5.40982820670784));
#30791=CARTESIAN_POINT('Ctrl Pts',(-0.385082654093672,2.18393146959264,
5.4111241595673));
#30792=CARTESIAN_POINT('Ctrl Pts',(-0.389727460306299,2.15874785035819,
5.41242011242676));
#30793=CARTESIAN_POINT('Ctrl Pts',(-0.391890476555899,2.13326776795625,
5.41371606528622));
#30794=CARTESIAN_POINT('Ctrl Pts',(-0.392818238713173,2.12233883655264,
5.41427192612214));
#30795=CARTESIAN_POINT('Ctrl Pts',(-0.393289994800293,2.11135562928169,
5.41482778695806));
#30796=CARTESIAN_POINT('Ctrl Pts',(-0.393299842496665,2.10035198309414,
5.41538364779398));
#30797=CARTESIAN_POINT('',(-0.393082160614917,2.09985082257753,5.54038368632201));
#30798=CARTESIAN_POINT('Ctrl Pts',(-0.39329984249671,2.10035198304379,5.41538364779653));
#30799=CARTESIAN_POINT('Ctrl Pts',(-0.39331813262776,2.07991490293939,5.41641604853325));
#30800=CARTESIAN_POINT('Ctrl Pts',(-0.391739146712473,2.05944415779562,
5.41744844926996));
#30801=CARTESIAN_POINT('Ctrl Pts',(-0.38857361574904,2.03920990916509,5.41848085000668));
#30802=CARTESIAN_POINT('Ctrl Pts',(-0.385407316009461,2.01897074647499,
5.41951350147071));
#30803=CARTESIAN_POINT('Ctrl Pts',(-0.380653784186541,1.99896894018719,
5.42054615293473));
#30804=CARTESIAN_POINT('Ctrl Pts',(-0.374375506108631,1.97946838412306,
5.42157880439876));
#30805=CARTESIAN_POINT('Ctrl Pts',(-0.368096782342726,1.95996644373609,
5.42261152916957));
#30806=CARTESIAN_POINT('Ctrl Pts',(-0.36029335144596,1.94096653004302,5.42364425394037));
#30807=CARTESIAN_POINT('Ctrl Pts',(-0.351076903972026,1.92271520793532,
5.42467697871118));
#30808=CARTESIAN_POINT('Ctrl Pts',(-0.341839789496302,1.90442295898376,
5.4257120192685));
#30809=CARTESIAN_POINT('Ctrl Pts',(-0.331183711860069,1.88688330180213,
5.42674705982581));
#30810=CARTESIAN_POINT('Ctrl Pts',(-0.319265627307391,1.87031685037857,
5.42778210038312));
#30811=CARTESIAN_POINT('Ctrl Pts',(-0.311909905459202,1.86009220327655,
5.42842091699896));
#30812=CARTESIAN_POINT('Ctrl Pts',(-0.304074315194476,1.85023768421479,
5.4290597336148));
#30813=CARTESIAN_POINT('Ctrl Pts',(-0.295803036849655,1.84079843096439,
5.42969855023063));
#30814=CARTESIAN_POINT('Ctrl Pts',(-0.282286003282509,1.82537267720357,
5.43074251287818));
#30815=CARTESIAN_POINT('Ctrl Pts',(-0.267518795889601,1.81096115249115,
5.43178647552574));
#30816=CARTESIAN_POINT('Ctrl Pts',(-0.251679308898635,1.79777092219261,
5.43283043817329));
#30817=CARTESIAN_POINT('Ctrl Pts',(-0.235868960350793,1.78460495674403,
5.43387248033906));
#30818=CARTESIAN_POINT('Ctrl Pts',(-0.218990768648704,1.7726563373126,5.43491452250483));
#30819=CARTESIAN_POINT('Ctrl Pts',(-0.2012593035049,1.76209530522243,5.4359565646706));
#30820=CARTESIAN_POINT('Ctrl Pts',(-0.183546881676084,1.75154561551481,
5.43699748769945));
#30821=CARTESIAN_POINT('Ctrl Pts',(-0.164983619824173,1.74238095410268,
5.43803841072831));
#30822=CARTESIAN_POINT('Ctrl Pts',(-0.145812772935528,1.73472814884137,
5.43907933375716));
#30823=CARTESIAN_POINT('Ctrl Pts',(-0.126632080399596,1.72707141329874,
5.44012079137695));
#30824=CARTESIAN_POINT('Ctrl Pts',(-0.106843856808282,1.72092837283578,
5.44116224899674));
#30825=CARTESIAN_POINT('Ctrl Pts',(-0.086711533187502,1.71637778999089,
5.44220370661654));
#30826=CARTESIAN_POINT('Ctrl Pts',(-0.0665730582641609,1.71182581674456,
5.44324548244703));
#30827=CARTESIAN_POINT('Ctrl Pts',(-0.0460909990527346,1.70886739654375,
5.44428725827753));
#30828=CARTESIAN_POINT('Ctrl Pts',(-0.0255382596491352,1.70753001733369,
5.44532903410803));
#30829=CARTESIAN_POINT('Ctrl Pts',(-0.00494109503290615,1.70618974734812,
5.44637306176062));
#30830=CARTESIAN_POINT('Ctrl Pts',(0.0157263183806198,1.70647750349892,
5.44741708941322));
#30831=CARTESIAN_POINT('Ctrl Pts',(0.036191064237229,1.70836867225747,5.44846111706582));
#30832=CARTESIAN_POINT('Ctrl Pts',(0.0434291765998863,1.7090375538584,5.44883037596169));
#30833=CARTESIAN_POINT('Ctrl Pts',(0.0506420051116785,1.70990654119884,
5.44919963485755));
#30834=CARTESIAN_POINT('Ctrl Pts',(0.0578177914211348,1.7109730176515,5.44956889375342));
#30835=CARTESIAN_POINT('Ctrl Pts',(0.0781050558790529,1.7139881422525,5.45061285640097));
#30836=CARTESIAN_POINT('Ctrl Pts',(0.0982162800750279,1.71860345589965,
5.45165681904853));
#30837=CARTESIAN_POINT('Ctrl Pts',(0.117881062382578,1.72478147016498,5.45270078169608));
#30838=CARTESIAN_POINT('Ctrl Pts',(0.137509669204067,1.73094811930735,5.45374282386185));
#30839=CARTESIAN_POINT('Ctrl Pts',(0.156692752492609,1.738671601488,5.45478486602762));
#30840=CARTESIAN_POINT('Ctrl Pts',(0.175171019832387,1.74786365735573,5.45582690819339));
#30841=CARTESIAN_POINT('Ctrl Pts',(0.193629441803336,1.75704584109987,5.45686783122224));
#30842=CARTESIAN_POINT('Ctrl Pts',(0.211383882263559,1.76769316721141,5.4579087542511));
#30843=CARTESIAN_POINT('Ctrl Pts',(0.228196023762074,1.77966975675222,5.45894967727995));
#30844=CARTESIAN_POINT('Ctrl Pts',(0.245016799538276,1.79165249715727,5.45999113489974));
#30845=CARTESIAN_POINT('Ctrl Pts',(0.260893700927387,1.80496545104851,5.46103259251953));
#30846=CARTESIAN_POINT('Ctrl Pts',(0.275617903002686,1.81942975648797,5.46207405013933));
#30847=CARTESIAN_POINT('Ctrl Pts',(0.290346603963644,1.83389848140333,5.46311582596982));
#30848=CARTESIAN_POINT('Ctrl Pts',(0.303921405375651,1.84951871719701,5.46415760180032));
#30849=CARTESIAN_POINT('Ctrl Pts',(0.316171466964028,1.86607588094039,5.46519937763082));
#30850=CARTESIAN_POINT('Ctrl Pts',(0.328448007338517,1.88266883336893,5.46624340528342));
#30851=CARTESIAN_POINT('Ctrl Pts',(0.339393701132029,1.90020213220819,5.46728743293601));
#30852=CARTESIAN_POINT('Ctrl Pts',(0.348881509286305,1.91843298075336,5.46833146058861));
#30853=CARTESIAN_POINT('Ctrl Pts',(0.352237222666619,1.92488099291831,5.46870071948448));
#30854=CARTESIAN_POINT('Ctrl Pts',(0.355410996953054,1.93141606682124,5.46906997838034));
#30855=CARTESIAN_POINT('Ctrl Pts',(0.358398667244586,1.93802689940208,5.46943923727621));
#30856=CARTESIAN_POINT('Ctrl Pts',(0.36684535931479,1.95671693601564,5.47048319992376));
#30857=CARTESIAN_POINT('Ctrl Pts',(0.373851290009961,1.97612516606932,5.47152716257132));
#30858=CARTESIAN_POINT('Ctrl Pts',(0.379301606985278,1.99600393787077,5.47257112521887));
#30859=CARTESIAN_POINT('Ctrl Pts',(0.384741897515215,2.01584614052945,5.47361316738464));
#30860=CARTESIAN_POINT('Ctrl Pts',(0.388632005013936,2.0361564808786,5.47465520955041));
#30861=CARTESIAN_POINT('Ctrl Pts',(0.390905779854375,2.056669164831,5.47569725171618));
#30862=CARTESIAN_POINT('Ctrl Pts',(0.393177112696356,2.07715981848309,5.47673817474503));
#30863=CARTESIAN_POINT('Ctrl Pts',(0.393835449691452,2.09785165991352,5.47777909777389));
#30864=CARTESIAN_POINT('Ctrl Pts',(0.392866034741345,2.11847075381819,5.47882002080274));
#30865=CARTESIAN_POINT('Ctrl Pts',(0.391896121924987,2.13910043715209,5.47986147842253));
#30866=CARTESIAN_POINT('Ctrl Pts',(0.389296805532323,2.15965656259733,5.48090293604233));
#30867=CARTESIAN_POINT('Ctrl Pts',(0.38510543517715,2.17986672521781,5.48194439366212));
#30868=CARTESIAN_POINT('Ctrl Pts',(0.380912784175606,2.20008306292406,5.48298616949262));
#30869=CARTESIAN_POINT('Ctrl Pts',(0.375127295534998,2.2199525148746,5.48402794532312));
#30870=CARTESIAN_POINT('Ctrl Pts',(0.367836915496096,2.23921527789118,5.48506972115361));
#30871=CARTESIAN_POINT('Ctrl Pts',(0.3605307771353,2.25851967780714,5.48611374880621));
#30872=CARTESIAN_POINT('Ctrl Pts',(0.351713567374897,2.27721410459293,5.48715777645881));
#30873=CARTESIAN_POINT('Ctrl Pts',(0.34152066549373,2.29506031129043,5.4882018041114));
#30874=CARTESIAN_POINT('Ctrl Pts',(0.337915569704419,2.30137228067564,5.48857106300727));
#30875=CARTESIAN_POINT('Ctrl Pts',(0.334138783928079,2.30757840050508,5.48894032190313));
#30876=CARTESIAN_POINT('Ctrl Pts',(0.330197557443822,2.31366905030475,5.489309580799));
#30877=CARTESIAN_POINT('Ctrl Pts',(0.319054987065194,2.33088843475665,5.49035354344655));
#30878=CARTESIAN_POINT('Ctrl Pts',(0.306528636618086,2.34728517233454,5.49139750609411));
#30879=CARTESIAN_POINT('Ctrl Pts',(0.292764564429977,2.3626286347947,5.49244146874166));
#30880=CARTESIAN_POINT('Ctrl Pts',(0.279025812735833,2.37794387130229,5.49348351090743));
#30881=CARTESIAN_POINT('Ctrl Pts',(0.264054300404986,2.39220909755274,5.4945255530732));
#30882=CARTESIAN_POINT('Ctrl Pts',(0.248037703876494,2.40522481461322,5.49556759523897));
#30883=CARTESIAN_POINT('Ctrl Pts',(0.232038308921056,2.41822655299806,5.49660851826782));
#30884=CARTESIAN_POINT('Ctrl Pts',(0.214996607882537,2.42998096217478,5.49764944129667));
#30885=CARTESIAN_POINT('Ctrl Pts',(0.19713494272663,2.44032734882194,5.49869036432552));
#30886=CARTESIAN_POINT('Ctrl Pts',(0.179264104285027,2.45067904910361,5.49973182194532));
#30887=CARTESIAN_POINT('Ctrl Pts',(0.1605730890359,2.45962089947064,5.50077327956511));
#30888=CARTESIAN_POINT('Ctrl Pts',(0.141311157947594,2.46703684643304,5.5018147371849));
#30889=CARTESIAN_POINT('Ctrl Pts',(0.122043341499598,2.47445505929055,5.5028565130154));
#30890=CARTESIAN_POINT('Ctrl Pts',(0.102204961011002,2.48034621021496,5.50389828884589));
#30891=CARTESIAN_POINT('Ctrl Pts',(0.0820620705349193,2.48464360982541,
5.50494006467639));
#30892=CARTESIAN_POINT('Ctrl Pts',(0.0618756407439544,2.48895029836264,
5.50598409232899));
#30893=CARTESIAN_POINT('Ctrl Pts',(0.0413841170300968,2.4916562615354,5.50702811998158));
#30894=CARTESIAN_POINT('Ctrl Pts',(0.0208611049511767,2.49274636128195,
5.50807214763418));
#30895=CARTESIAN_POINT('Ctrl Pts',(0.0136023845893694,2.49313191527356,
5.50844140653005));
#30896=CARTESIAN_POINT('Ctrl Pts',(0.00633972553699942,2.49331581097294,
5.50881066542592));
#30897=CARTESIAN_POINT('Ctrl Pts',(-0.000914858973369157,2.49329893596736,
5.50917992432179));
#30898=CARTESIAN_POINT('Ctrl Pts',(-0.0214249004024134,2.4932512272305,
5.51022388696934));
#30899=CARTESIAN_POINT('Ctrl Pts',(-0.0419923107651998,2.49159469781914,
5.5112678496169));
#30900=CARTESIAN_POINT('Ctrl Pts',(-0.0623441096933663,2.4883273129546,
5.51231181226445));
#30901=CARTESIAN_POINT('Ctrl Pts',(-0.0826584692943649,2.4850659387966,
5.51335385443022));
#30902=CARTESIAN_POINT('Ctrl Pts',(-0.10275727707859,2.48019964789877,5.51439589659599));
#30903=CARTESIAN_POINT('Ctrl Pts',(-0.122371198123852,2.47377824959424,
5.51543793876176));
#30904=CARTESIAN_POINT('Ctrl Pts',(-0.141964054126048,2.46736374777061,
5.51647886179061));
#30905=CARTESIAN_POINT('Ctrl Pts',(-0.161072352513457,2.45939765449231,
5.51751978481946));
#30906=CARTESIAN_POINT('Ctrl Pts',(-0.179440621740774,2.44997993266655,
5.51856070784832));
#30907=CARTESIAN_POINT('Ctrl Pts',(-0.197818324432443,2.44055737414431,
5.51960216546811));
#30908=CARTESIAN_POINT('Ctrl Pts',(-0.215454576598941,2.42968201904437,
5.5206436230879));
#30909=CARTESIAN_POINT('Ctrl Pts',(-0.232116868922016,2.4175006286007,5.52168508070769));
#30910=CARTESIAN_POINT('Ctrl Pts',(-0.248784252301796,2.4053155162112,5.52272685653819));
#30911=CARTESIAN_POINT('Ctrl Pts',(-0.264476511291741,2.39182403714412,
5.52376863236869));
#30912=CARTESIAN_POINT('Ctrl Pts',(-0.27899355240014,2.37721379424399,5.52481040819919));
#30913=CARTESIAN_POINT('Ctrl Pts',(-0.293541972422333,2.36257197097228,
5.52585443585178));
#30914=CARTESIAN_POINT('Ctrl Pts',(-0.306909626751238,2.34680711770463,
5.52689846350438));
#30915=CARTESIAN_POINT('Ctrl Pts',(-0.318935679401313,2.33014109238644,
5.52794249115697));
#30916=CARTESIAN_POINT('Ctrl Pts',(-0.323189136589131,2.32424653768552,
5.52831175005284));
#30917=CARTESIAN_POINT('Ctrl Pts',(-0.327275167958654,2.31823950998575,
5.52868100894871));
#30918=CARTESIAN_POINT('Ctrl Pts',(-0.331188016829293,2.31213059069517,
5.52905026784458));
#30919=CARTESIAN_POINT('Ctrl Pts',(-0.342509195383825,2.29445544699543,
5.53011865715149));
#30920=CARTESIAN_POINT('Ctrl Pts',(-0.35244220085537,2.27582419445772,5.53118704645841));
#30921=CARTESIAN_POINT('Ctrl Pts',(-0.360832686475196,2.25647575649631,
5.53225543576533));
#30922=CARTESIAN_POINT('Ctrl Pts',(-0.36920441509842,2.23717057212016,5.53332143667954));
#30923=CARTESIAN_POINT('Ctrl Pts',(-0.376040145698522,2.21715198672075,
5.53438743759376));
#30924=CARTESIAN_POINT('Ctrl Pts',(-0.381231056446065,2.1966838745656,5.53545343850798));
#30925=CARTESIAN_POINT('Ctrl Pts',(-0.386412884918501,2.17625157443546,
5.53651757429408));
#30926=CARTESIAN_POINT('Ctrl Pts',(-0.389955404934743,2.15537196405331,
5.53758171008019));
#30927=CARTESIAN_POINT('Ctrl Pts',(-0.391799306690207,2.1343248201317,5.53864584586629));
#30928=CARTESIAN_POINT('Ctrl Pts',(-0.392803043265827,2.12286770854543,
5.53922511317637));
#30929=CARTESIAN_POINT('Ctrl Pts',(-0.393304317595768,2.11136119740429,
5.53980438048645));
#30930=CARTESIAN_POINT('Ctrl Pts',(-0.393299971966862,2.0998515046609,5.54038364779653));
#30931=CARTESIAN_POINT('',(-0.393402607802015,2.09971271023449,5.66538360260035));
#30932=CARTESIAN_POINT('Ctrl Pts',(-0.392705315208772,2.09984964247381,
5.54038375297671));
#30933=CARTESIAN_POINT('Ctrl Pts',(-0.392895903822687,2.04339430721444,
5.54322937244026));
#30934=CARTESIAN_POINT('Ctrl Pts',(-0.355079068065668,1.855777880858,5.55269843974473));
#30935=CARTESIAN_POINT('Ctrl Pts',(-0.0662253309296011,1.63968570951168,
5.56879095489017));
#30936=CARTESIAN_POINT('Ctrl Pts',(0.351191528838419,1.79514011323788,5.58866129841293));
#30937=CARTESIAN_POINT('Ctrl Pts',(0.446437971306593,2.2302619601424,5.60853164193575));
#30938=CARTESIAN_POINT('Ctrl Pts',(0.132138352142635,2.54588619218082,5.62840198545851));
#30939=CARTESIAN_POINT('Ctrl Pts',(-0.283221592391678,2.45679442678442,
5.64735260062244));
#30940=CARTESIAN_POINT('Ctrl Pts',(-0.392738243985543,2.21217249115798,
5.65967976794542));
#30941=CARTESIAN_POINT('Ctrl Pts',(-0.393664350931912,2.0997147892973,5.66538348742747));
#30942=CARTESIAN_POINT('',(-0.393379133237835,2.10030487424134,5.79038368413719));
#30943=CARTESIAN_POINT('Ctrl Pts',(-0.393299894476397,2.09971189436798,
5.66538364779653));
#30944=CARTESIAN_POINT('Ctrl Pts',(-0.393286623951248,2.08159598283861,
5.66630332269905));
#30945=CARTESIAN_POINT('Ctrl Pts',(-0.392021608078033,2.06352518737575,
5.66722299760158));
#30946=CARTESIAN_POINT('Ctrl Pts',(-0.389523855042085,2.04563037288014,
5.66814267250411));
#30947=CARTESIAN_POINT('Ctrl Pts',(-0.386688547842559,2.02531719714043,
5.66918663515167));
#30948=CARTESIAN_POINT('Ctrl Pts',(-0.382251555055874,2.00516588071356,
5.67023059779923));
#30949=CARTESIAN_POINT('Ctrl Pts',(-0.376247968494637,1.98544714668041,
5.67127456044679));
#30950=CARTESIAN_POINT('Ctrl Pts',(-0.370255426177802,1.96576468738333,
5.67231660261256));
#30951=CARTESIAN_POINT('Ctrl Pts',(-0.362702165570659,1.94651394413396,
5.67335864477834));
#30952=CARTESIAN_POINT('Ctrl Pts',(-0.353674145819687,1.92795498095349,
5.67440068694411));
#30953=CARTESIAN_POINT('Ctrl Pts',(-0.3446558220201,1.90941594980791,5.67544160997296));
#30954=CARTESIAN_POINT('Ctrl Pts',(-0.334166177652963,1.89156789471963,
5.67648253300182));
#30955=CARTESIAN_POINT('Ctrl Pts',(-0.322338975374128,1.87465032736931,
5.67752345603067));
#30956=CARTESIAN_POINT('Ctrl Pts',(-0.310505698952456,1.85772407159733,
5.67856491365047));
#30957=CARTESIAN_POINT('Ctrl Pts',(-0.297333900644732,1.84172987051153,
5.67960637127026));
#30958=CARTESIAN_POINT('Ctrl Pts',(-0.283000585657215,1.82687812515715,
5.68064782889005));
#30959=CARTESIAN_POINT('Ctrl Pts',(-0.268662891217087,1.81202184194708,
5.68168960472055));
#30960=CARTESIAN_POINT('Ctrl Pts',(-0.253163510141973,1.79830921324518,
5.68273138055105));
#30961=CARTESIAN_POINT('Ctrl Pts',(-0.236715503685208,1.78591297334169,
5.68377315638155));
#30962=CARTESIAN_POINT('Ctrl Pts',(-0.220231944489237,1.77348993868434,
5.68481718403414));
#30963=CARTESIAN_POINT('Ctrl Pts',(-0.202796287492711,1.76238936906338,
5.68586121168674));
#30964=CARTESIAN_POINT('Ctrl Pts',(-0.184650194597699,1.75274044918097,
5.68690523933934));
#30965=CARTESIAN_POINT('Ctrl Pts',(-0.178232159395585,1.74932775269441,
5.68727449823519));
#30966=CARTESIAN_POINT('Ctrl Pts',(-0.171725454303548,1.74609621699476,
5.68764375713103));
#30967=CARTESIAN_POINT('Ctrl Pts',(-0.165141345046674,1.74305010693912,
5.68801301602688));
#30968=CARTESIAN_POINT('Ctrl Pts',(-0.14652686017205,1.73443819493324,5.68905697867443));
#30969=CARTESIAN_POINT('Ctrl Pts',(-0.127181448156699,1.72726062621688,
5.69010094132198));
#30970=CARTESIAN_POINT('Ctrl Pts',(-0.107351733646389,1.72163444226104,
5.69114490396954));
#30971=CARTESIAN_POINT('Ctrl Pts',(-0.0875584980326944,1.71601860827684,
5.6921869461353));
#30972=CARTESIAN_POINT('Ctrl Pts',(-0.0672834119905888,1.71194874987206,
5.69322898830107));
#30973=CARTESIAN_POINT('Ctrl Pts',(-0.0467916732445428,1.70949336841101,
5.69427103046684));
#30974=CARTESIAN_POINT('Ctrl Pts',(-0.0263219423039875,1.70704062399109,
5.6953119534957));
#30975=CARTESIAN_POINT('Ctrl Pts',(-0.0056367439956138,1.7061990300724,
5.69635287652455));
#30976=CARTESIAN_POINT('Ctrl Pts',(0.0149901278286173,1.7069857686194,5.69739379955341));
#30977=CARTESIAN_POINT('Ctrl Pts',(0.0356275930766123,1.70777291121482,
5.6984352571732));
#30978=CARTESIAN_POINT('Ctrl Pts',(0.0562059361390714,1.71019004502023,
5.69947671479299));
#30979=CARTESIAN_POINT('Ctrl Pts',(0.0764524319336417,1.71420223477652,
5.70051817241279));
#30980=CARTESIAN_POINT('Ctrl Pts',(0.0967051139153531,1.7182156504317,5.70155994824329));
#30981=CARTESIAN_POINT('Ctrl Pts',(0.116625032676036,1.72382491385864,5.70260172407379));
#30982=CARTESIAN_POINT('Ctrl Pts',(0.135951616225552,1.73094438353324,5.70364349990428));
#30983=CARTESIAN_POINT('Ctrl Pts',(0.155319974623986,1.7380792421031,5.70468752755688));
#30984=CARTESIAN_POINT('Ctrl Pts',(0.174091768484672,1.74673051577,5.70573155520948));
#30985=CARTESIAN_POINT('Ctrl Pts',(0.1920275610429,1.75676494089339,5.70677558286208));
#30986=CARTESIAN_POINT('Ctrl Pts',(0.198371215772838,1.76031398553079,5.70714484175795));
#30987=CARTESIAN_POINT('Ctrl Pts',(0.204610545883134,1.76403565100655,5.70751410065382));
#30988=CARTESIAN_POINT('Ctrl Pts',(0.210735867065037,1.76792277354153,5.70788335954968));
#30989=CARTESIAN_POINT('Ctrl Pts',(0.228053273875588,1.77891238212885,5.70892732219724));
#30990=CARTESIAN_POINT('Ctrl Pts',(0.244560323235575,1.79129300328244,5.70997128484479));
#30991=CARTESIAN_POINT('Ctrl Pts',(0.260025102203642,1.80492062724754,5.71101524749234));
#30992=CARTESIAN_POINT('Ctrl Pts',(0.275461432044374,1.8185231817299,5.71205728965811));
#30993=CARTESIAN_POINT('Ctrl Pts',(0.289858712281573,1.83336774919484,5.71309933182388));
#30994=CARTESIAN_POINT('Ctrl Pts',(0.30301578942157,1.84926842767369,5.71414137398965));
#30995=CARTESIAN_POINT('Ctrl Pts',(0.316158736067408,1.86515202907364,5.71518229701851));
#30996=CARTESIAN_POINT('Ctrl Pts',(0.328063634904601,1.88208894417223,5.71622322004736));
#30997=CARTESIAN_POINT('Ctrl Pts',(0.338567829470585,1.89985826310443,5.71726414307621));
#30998=CARTESIAN_POINT('Ctrl Pts',(0.349077418717127,1.91763670789571,5.718305600696));
#30999=CARTESIAN_POINT('Ctrl Pts',(0.358184478263024,1.93624778538888,5.71934705831579));
#31000=CARTESIAN_POINT('Ctrl Pts',(0.365770751284716,1.95544327236474,5.72038851593558));
#31001=CARTESIAN_POINT('Ctrl Pts',(0.373359342243549,1.97464462439872,5.72143029176608));
#31002=CARTESIAN_POINT('Ctrl Pts',(0.379425985079017,1.99443004439254,5.72247206759658));
#31003=CARTESIAN_POINT('Ctrl Pts',(0.383901636391456,2.01453407944705,5.72351384342707));
#31004=CARTESIAN_POINT('Ctrl Pts',(0.388386961925772,2.03468156982956,5.72455787107967));
#31005=CARTESIAN_POINT('Ctrl Pts',(0.391274327332497,2.05514832095952,5.72560189873226));
#31006=CARTESIAN_POINT('Ctrl Pts',(0.392546171619527,2.07566087210164,5.72664592638486));
#31007=CARTESIAN_POINT('Ctrl Pts',(0.392996006272832,2.08291589256721,5.72701518528073));
#31008=CARTESIAN_POINT('Ctrl Pts',(0.393244225432926,2.09017663780359,5.7273844441766));
#31009=CARTESIAN_POINT('Ctrl Pts',(0.393291610242275,2.09743108718749,5.72775370307247));
#31010=CARTESIAN_POINT('Ctrl Pts',(0.393425575792125,2.11794074658926,5.72879766572002));
#31011=CARTESIAN_POINT('Ctrl Pts',(0.391951291940804,2.13852202317378,5.72984162836757));
#31012=CARTESIAN_POINT('Ctrl Pts',(0.388864306002967,2.15890196530534,5.73088559101513));
#31013=CARTESIAN_POINT('Ctrl Pts',(0.385782998908404,2.17924441633728,5.7319276331809));
#31014=CARTESIAN_POINT('Ctrl Pts',(0.381094928735773,2.19938553992826,5.73296967534667));
#31015=CARTESIAN_POINT('Ctrl Pts',(0.374847517168071,2.21905557052458,5.73401171751244));
#31016=CARTESIAN_POINT('Ctrl Pts',(0.368606815222249,2.23870447581704,5.73505264054129));
#31017=CARTESIAN_POINT('Ctrl Pts',(0.360810290610757,2.25788258608275,5.73609356357015));
#31018=CARTESIAN_POINT('Ctrl Pts',(0.351555639421154,2.27633355435419,5.737134486599));
#31019=CARTESIAN_POINT('Ctrl Pts',(0.342296235283906,2.29479399856205,5.73817594421879));
#31020=CARTESIAN_POINT('Ctrl Pts',(0.331577523994065,2.31252588981243,5.73921740183859));
#31021=CARTESIAN_POINT('Ctrl Pts',(0.31954420152327,2.3292954279371,5.74025885945838));
#31022=CARTESIAN_POINT('Ctrl Pts',(0.307507202347852,2.34607008988675,5.74130063528888));
#31023=CARTESIAN_POINT('Ctrl Pts',(0.294155250355389,2.36188123714482,5.74234241111938));
#31024=CARTESIAN_POINT('Ctrl Pts',(0.279674168656474,2.37652712233398,5.74338418694988));
#31025=CARTESIAN_POINT('Ctrl Pts',(0.265161785770851,2.39120466493632,5.74442821460247));
#31026=CARTESIAN_POINT('Ctrl Pts',(0.249515958042227,2.40471143566417,5.74547224225507));
#31027=CARTESIAN_POINT('Ctrl Pts',(0.23295711007065,2.4168846396838,5.74651626990767));
#31028=CARTESIAN_POINT('Ctrl Pts',(0.22710046259244,2.42119014238216,5.74688552880353));
#31029=CARTESIAN_POINT('Ctrl Pts',(0.221129863515003,2.4253292220859,5.7472547876994));
#31030=CARTESIAN_POINT('Ctrl Pts',(0.215055842840153,2.42929602861303,5.74762404659526));
#31031=CARTESIAN_POINT('Ctrl Pts',(0.197883471975067,2.44051091846612,5.74866800924282));
#31032=CARTESIAN_POINT('Ctrl Pts',(0.179780309640395,2.45041233110304,5.74971197189037));
#31033=CARTESIAN_POINT('Ctrl Pts',(0.160973448139428,2.45884876897393,5.75075593453792));
#31034=CARTESIAN_POINT('Ctrl Pts',(0.142201183886746,2.46726968710827,5.75179797670369));
#31035=CARTESIAN_POINT('Ctrl Pts',(0.122728429464549,2.47423062789692,5.75284001886946));
#31036=CARTESIAN_POINT('Ctrl Pts',(0.102807678794231,2.47962543537142,5.75388206103523));
#31037=CARTESIAN_POINT('Ctrl Pts',(0.082908322697187,2.48501444890745,5.75492298406409));
#31038=CARTESIAN_POINT('Ctrl Pts',(0.0625626245670739,2.48884044903543,
5.75596390709294));
#31039=CARTESIAN_POINT('Ctrl Pts',(0.0420390101813584,2.49104681512956,
5.75700483012179));
#31040=CARTESIAN_POINT('Ctrl Pts',(0.0215048554022065,2.49325431435581,
5.75804628774159));
#31041=CARTESIAN_POINT('Ctrl Pts',(0.000793331664292161,2.49384042312017,
5.75908774536138));
#31042=CARTESIAN_POINT('Ctrl Pts',(-0.0198206511209501,2.49280024413071,
5.76012920298117));
#31043=CARTESIAN_POINT('Ctrl Pts',(-0.0404409323766265,2.49175974732122,
5.76117097881167));
#31044=CARTESIAN_POINT('Ctrl Pts',(-0.0609628809480463,2.48909204672758,
5.76221275464216));
#31045=CARTESIAN_POINT('Ctrl Pts',(-0.0811162746207978,2.48484417624753,
5.76325453047266));
#31046=CARTESIAN_POINT('Ctrl Pts',(-0.101313230311313,2.48058712389905,
5.76429855812526));
#31047=CARTESIAN_POINT('Ctrl Pts',(-0.121139334221363,2.47474329086276,
5.76534258577786));
#31048=CARTESIAN_POINT('Ctrl Pts',(-0.140338385721195,2.46740989030396,
5.76638661343045));
#31049=CARTESIAN_POINT('Ctrl Pts',(-0.147128838580244,2.46481616265072,
5.76675587232632));
#31050=CARTESIAN_POINT('Ctrl Pts',(-0.153841044065357,2.46203653467856,
5.76712513122218));
#31051=CARTESIAN_POINT('Ctrl Pts',(-0.160464383158511,2.45907669339232,
5.76749439011805));
#31052=CARTESIAN_POINT('Ctrl Pts',(-0.179189777977002,2.45070867902591,
5.7685383527656));
#31053=CARTESIAN_POINT('Ctrl Pts',(-0.197314631875966,2.44084702957649,
5.76958231541316));
#31054=CARTESIAN_POINT('Ctrl Pts',(-0.214588633835922,2.42960067995748,
5.77062627806071));
#31055=CARTESIAN_POINT('Ctrl Pts',(-0.231830858407894,2.41837501921045,
5.77166832022648));
#31056=CARTESIAN_POINT('Ctrl Pts',(-0.248224695873425,2.40577006166971,
5.77271036239225));
#31057=CARTESIAN_POINT('Ctrl Pts',(-0.263544208871659,2.39194064460128,
5.77375240455802));
#31058=CARTESIAN_POINT('Ctrl Pts',(-0.2788472689536,2.37812608010952,5.77479332758687));
#31059=CARTESIAN_POINT('Ctrl Pts',(-0.29307773238465,2.36309013584524,5.77583425061573));
#31060=CARTESIAN_POINT('Ctrl Pts',(-0.306042687805391,2.34702785924031,
5.77687517364458));
#31061=CARTESIAN_POINT('Ctrl Pts',(-0.319014301689326,2.33095733346876,
5.77791663126437));
#31062=CARTESIAN_POINT('Ctrl Pts',(-0.330718634465133,2.31385998474731,
5.77895808888416));
#31063=CARTESIAN_POINT('Ctrl Pts',(-0.341002754699717,2.29596431125897,
5.77999954650396));
#31064=CARTESIAN_POINT('Ctrl Pts',(-0.351290017181381,2.27806316986221,
5.78104132233445));
#31065=CARTESIAN_POINT('Ctrl Pts',(-0.360155868328508,2.25936387353689,
5.78208309816495));
#31066=CARTESIAN_POINT('Ctrl Pts',(-0.367493578917158,2.24011909025775,
5.78312487399545));
#31067=CARTESIAN_POINT('Ctrl Pts',(-0.37484715013376,2.22083270894282,5.78416890164805));
#31068=CARTESIAN_POINT('Ctrl Pts',(-0.380665778968099,2.20099919338717,
5.78521292930064));
#31069=CARTESIAN_POINT('Ctrl Pts',(-0.384892517959947,2.18088658491031,
5.78625695695324));
#31070=CARTESIAN_POINT('Ctrl Pts',(-0.386387460138313,2.17377301892314,
5.78662621584911));
#31071=CARTESIAN_POINT('Ctrl Pts',(-0.387683737282749,2.16662461352731,
5.78699547474497));
#31072=CARTESIAN_POINT('Ctrl Pts',(-0.388780382862406,2.15945337586177,
5.78736473364084));
#31073=CARTESIAN_POINT('Ctrl Pts',(-0.391768962511404,2.13991031168231,
5.78837103835941));
#31074=CARTESIAN_POINT('Ctrl Pts',(-0.393284476002902,2.12013639346441,
5.78937734307797));
#31075=CARTESIAN_POINT('Ctrl Pts',(-0.393299881326936,2.10030552940591,
5.79038364779653));
#31076=CARTESIAN_POINT('',(-0.393073346508676,2.10012267207431,5.91538361492347));
#31077=CARTESIAN_POINT('Ctrl Pts',(-0.393617414534465,2.10030290440287,
5.79038379340017));
#31078=CARTESIAN_POINT('Ctrl Pts',(-0.392667861142396,1.98951876646131,
5.79600088798799));
#31079=CARTESIAN_POINT('Ctrl Pts',(-0.285965102257327,1.74650375455207,
5.80824143041673));
#31080=CARTESIAN_POINT('Ctrl Pts',(0.126302422767384,1.65242571735234,5.82710542068643));
#31081=CARTESIAN_POINT('Ctrl Pts',(0.444698253975958,1.96391729207861,5.84697576420921));
#31082=CARTESIAN_POINT('Ctrl Pts',(0.355143977362131,2.40024622533497,5.866846107732));
#31083=CARTESIAN_POINT('Ctrl Pts',(-0.0602065499947629,2.56114012167909,
5.88671645125477));
#31084=CARTESIAN_POINT('Ctrl Pts',(-0.353428603581954,2.34769677766452,
5.90289560167169));
#31085=CARTESIAN_POINT('Ctrl Pts',(-0.392848721613529,2.15830431178998,
5.91245130424765));
#31086=CARTESIAN_POINT('Ctrl Pts',(-0.392687677656695,2.10012366230725,
5.91538355898269));
#31087=CARTESIAN_POINT('',(-0.393299837367108,2.09964233114976,6.04038364780031));
#31088=CARTESIAN_POINT('Ctrl Pts',(-0.393299981050075,2.10012209017358,
5.91538364779653));
#31089=CARTESIAN_POINT('Ctrl Pts',(-0.393306574629672,2.07888160328984,
5.9164524844718));
#31090=CARTESIAN_POINT('Ctrl Pts',(-0.391588166963785,2.05765663935881,
5.91752132114708));
#31091=CARTESIAN_POINT('Ctrl Pts',(-0.388178268836697,2.03673451491576,
5.91859015782235));
#31092=CARTESIAN_POINT('Ctrl Pts',(-0.384764862865103,2.01579086737831,
5.9196600940357));
#31093=CARTESIAN_POINT('Ctrl Pts',(-0.379656662610636,1.99515134218412,
5.92073003024906));
#31094=CARTESIAN_POINT('Ctrl Pts',(-0.3729380446889,1.97509161427822,5.92179996646242));
#31095=CARTESIAN_POINT('Ctrl Pts',(-0.366199323910776,1.95497186542248,
5.92287310404461));
#31096=CARTESIAN_POINT('Ctrl Pts',(-0.357840831602137,1.93543600556655,
5.92394624162681));
#31097=CARTESIAN_POINT('Ctrl Pts',(-0.347995182185459,1.9167399575038,5.925019379209));
#31098=CARTESIAN_POINT('Ctrl Pts',(-0.343598208863494,1.90839048038156,
5.92549863223945));
#31099=CARTESIAN_POINT('Ctrl Pts',(-0.338905235391115,1.90020814633051,
5.9259778852699));
#31100=CARTESIAN_POINT('Ctrl Pts',(-0.333930840386804,1.89221385070568,
5.92645713830036));
#31101=CARTESIAN_POINT('Ctrl Pts',(-0.323095055845649,1.87479978027621,
5.92750110094791));
#31102=CARTESIAN_POINT('Ctrl Pts',(-0.310861135380553,1.85818371429248,
5.92854506359546));
#31103=CARTESIAN_POINT('Ctrl Pts',(-0.29737102887443,1.84259883219736,5.92958902624301));
#31104=CARTESIAN_POINT('Ctrl Pts',(-0.283905738872863,1.82704262017221,
5.93063106840878));
#31105=CARTESIAN_POINT('Ctrl Pts',(-0.269189280992312,1.81251441557219,
5.93167311057455));
#31106=CARTESIAN_POINT('Ctrl Pts',(-0.253405768145051,1.79921701066913,
5.93271515274032));
#31107=CARTESIAN_POINT('Ctrl Pts',(-0.23763920654264,1.78593388697003,5.93375607576918));
#31108=CARTESIAN_POINT('Ctrl Pts',(-0.220808406270014,1.77387943254175,
5.93479699879803));
#31109=CARTESIAN_POINT('Ctrl Pts',(-0.203132827758717,1.76321825422576,
5.93583792182689));
#31110=CARTESIAN_POINT('Ctrl Pts',(-0.185448171530978,1.75255160060644,
5.93687937944668));
#31111=CARTESIAN_POINT('Ctrl Pts',(-0.166918492036109,1.74328004642999,
5.93792083706647));
#31112=CARTESIAN_POINT('Ctrl Pts',(-0.147790955268361,1.73552404257501,
5.93896229468627));
#31113=CARTESIAN_POINT('Ctrl Pts',(-0.128657574204237,1.72776566892271,
5.94000407051677));
#31114=CARTESIAN_POINT('Ctrl Pts',(-0.108926667087551,1.7215240101706,5.94104584634727));
#31115=CARTESIAN_POINT('Ctrl Pts',(-0.0888630648357885,1.71687045831992,
5.94208762217777));
#31116=CARTESIAN_POINT('Ctrl Pts',(-0.0687560946524599,1.7122068477113,
5.94313164983036));
#31117=CARTESIAN_POINT('Ctrl Pts',(-0.0483157219466113,1.70913830661598,
5.94417567748296));
#31118=CARTESIAN_POINT('Ctrl Pts',(-0.0278152411750107,1.70768481757855,
5.94521970513556));
#31119=CARTESIAN_POINT('Ctrl Pts',(-0.0205644898413008,1.70717073755798,
5.94558896403142));
#31120=CARTESIAN_POINT('Ctrl Pts',(-0.0133062281057095,1.70685821441269,
5.94595822292729));
#31121=CARTESIAN_POINT('Ctrl Pts',(-0.00605248303909771,1.70674657350627,
5.94632748182316));
#31122=CARTESIAN_POINT('Ctrl Pts',(0.0144551851285342,1.70643094418076,
5.94737144447072));
#31123=CARTESIAN_POINT('Ctrl Pts',(0.0350487131087565,1.70772286679837,
5.94841540711827));
#31124=CARTESIAN_POINT('Ctrl Pts',(0.055455199414578,1.71062921160173,5.94945936976582));
#31125=CARTESIAN_POINT('Ctrl Pts',(0.0758241457899177,1.71353020987065,
5.95050141193159));
#31126=CARTESIAN_POINT('Ctrl Pts',(0.096006004896433,1.71803969148774,5.95154345409736));
#31127=CARTESIAN_POINT('Ctrl Pts',(0.115730601714979,1.7241126261409,5.95258549626313));
#31128=CARTESIAN_POINT('Ctrl Pts',(0.135434014626404,1.73017903855765,5.95362641929198));
#31129=CARTESIAN_POINT('Ctrl Pts',(0.154680432038124,1.73780538277979,5.95466734232083));
#31130=CARTESIAN_POINT('Ctrl Pts',(0.173212651673648,1.74689623720472,5.95570826534969));
#31131=CARTESIAN_POINT('Ctrl Pts',(0.191754388974173,1.75599176045555,5.95674972296948));
#31132=CARTESIAN_POINT('Ctrl Pts',(0.209580528047845,1.76655298693527,5.95779118058927));
#31133=CARTESIAN_POINT('Ctrl Pts',(0.226455996220631,1.77843729728757,5.95883263820906));
#31134=CARTESIAN_POINT('Ctrl Pts',(0.24333662058465,1.79032523881479,5.95987441403956));
#31135=CARTESIAN_POINT('Ctrl Pts',(0.259265415553611,1.80353661612611,5.96091618987005));
#31136=CARTESIAN_POINT('Ctrl Pts',(0.274038995693815,1.81788740042471,5.96195796570055));
#31137=CARTESIAN_POINT('Ctrl Pts',(0.288844509262749,1.83226920426924,5.96300199335315));
#31138=CARTESIAN_POINT('Ctrl Pts',(0.302489336635816,1.84779477887269,5.96404602100574));
#31139=CARTESIAN_POINT('Ctrl Pts',(0.314808736904162,1.86424515027511,5.96509004865834));
#31140=CARTESIAN_POINT('Ctrl Pts',(0.319165947299418,1.87006343101273,5.9654593075542));
#31141=CARTESIAN_POINT('Ctrl Pts',(0.323357750581443,1.87599713300921,5.96582856645007));
#31142=CARTESIAN_POINT('Ctrl Pts',(0.327378203525815,1.88203577849516,5.96619782534594));
#31143=CARTESIAN_POINT('Ctrl Pts',(0.338744761643042,1.89910813721073,5.96724178799349));
#31144=CARTESIAN_POINT('Ctrl Pts',(0.348806138772213,1.91712288530741,5.96828575064105));
#31145=CARTESIAN_POINT('Ctrl Pts',(0.357408831784391,1.9358542813153,5.9693297132886));
#31146=CARTESIAN_POINT('Ctrl Pts',(0.365995699215781,1.95455121890181,5.97037175545437));
#31147=CARTESIAN_POINT('Ctrl Pts',(0.373128851330051,1.97396155126283,5.97141379762014));
#31148=CARTESIAN_POINT('Ctrl Pts',(0.378699899800244,1.99383373468335,5.97245583978591));
#31149=CARTESIAN_POINT('Ctrl Pts',(0.384264965051899,2.01368457569106,5.97349676281477));
#31150=CARTESIAN_POINT('Ctrl Pts',(0.388271031790586,2.03399558597284,5.97453768584362));
#31151=CARTESIAN_POINT('Ctrl Pts',(0.39065910396862,2.05449885181191,5.97557860887248));
#31152=CARTESIAN_POINT('Ctrl Pts',(0.393048402598285,2.07501264759393,5.97662006649227));
#31153=CARTESIAN_POINT('Ctrl Pts',(0.393817945460347,2.09571816721585,5.97766152411206));
#31154=CARTESIAN_POINT('Ctrl Pts',(0.392960400377164,2.11634055492995,5.97870298173186));
#31155=CARTESIAN_POINT('Ctrl Pts',(0.392102593276572,2.13696924368257,5.97974475756236));
#31156=CARTESIAN_POINT('Ctrl Pts',(0.389616775223395,2.15751401694081,5.98078653339286));
#31157=CARTESIAN_POINT('Ctrl Pts',(0.385547584714711,2.17770424647761,5.98182830922336));
#31158=CARTESIAN_POINT('Ctrl Pts',(0.381469598558404,2.19793811765371,5.98287233687595));
#31159=CARTESIAN_POINT('Ctrl Pts',(0.375801609059394,2.21781520687339,5.98391636452855));
#31160=CARTESIAN_POINT('Ctrl Pts',(0.368638556213166,2.23707846246976,5.98496039218115));
#31161=CARTESIAN_POINT('Ctrl Pts',(0.366105078313,2.24389162347615,5.98532965107701));
#31162=CARTESIAN_POINT('Ctrl Pts',(0.363385014292737,2.25062818683317,5.98569890997288));
#31163=CARTESIAN_POINT('Ctrl Pts',(0.360483956873705,2.25727748356544,5.98606816886874));
#31164=CARTESIAN_POINT('Ctrl Pts',(0.352282135285122,2.2760762653923,5.98711213151629));
#31165=CARTESIAN_POINT('Ctrl Pts',(0.342581417780033,2.29428776007584,5.98815609416385));
#31166=CARTESIAN_POINT('Ctrl Pts',(0.331488517810789,2.31166070150032,5.9892000568114));
#31167=CARTESIAN_POINT('Ctrl Pts',(0.320416024426366,2.329001683527,5.99024209897717));
#31168=CARTESIAN_POINT('Ctrl Pts',(0.307956773574515,2.34550652916884,5.99128414114294));
#31169=CARTESIAN_POINT('Ctrl Pts',(0.294263595154714,2.36094793842187,5.99232618330871));
#31170=CARTESIAN_POINT('Ctrl Pts',(0.280585122993427,2.37637276384393,5.99336710633756));
#31171=CARTESIAN_POINT('Ctrl Pts',(0.265675818203077,2.39073585334616,5.99440802936641));
#31172=CARTESIAN_POINT('Ctrl Pts',(0.24972901180695,2.4038425754596,5.99544895239527));
#31173=CARTESIAN_POINT('Ctrl Pts',(0.233774015546679,2.41695602884392,5.99649041001506));
#31174=CARTESIAN_POINT('Ctrl Pts',(0.216781011384998,2.42881134615688,5.99753186763485));
#31175=CARTESIAN_POINT('Ctrl Pts',(0.198977133915454,2.43925357798967,5.99857332525464));
#31176=CARTESIAN_POINT('Ctrl Pts',(0.181167816585161,2.44969900037953,5.99961510108513));
#31177=CARTESIAN_POINT('Ctrl Pts',(0.162547785160077,2.45873013703855,6.00065687691563));
#31178=CARTESIAN_POINT('Ctrl Pts',(0.143368752323972,2.46623802486507,6.00169865274613));
#31179=CARTESIAN_POINT('Ctrl Pts',(0.124148263573157,2.4737621411615,6.00274268039872));
#31180=CARTESIAN_POINT('Ctrl Pts',(0.104367065940325,2.47975622165971,6.00378670805132));
#31181=CARTESIAN_POINT('Ctrl Pts',(0.0842926858043522,2.48416094689581,
6.00483073570392));
#31182=CARTESIAN_POINT('Ctrl Pts',(0.0771926406802738,2.48571884047578,
6.00519999459978));
#31183=CARTESIAN_POINT('Ctrl Pts',(0.0700559977930121,2.48707838541361,
6.00556925349565));
#31184=CARTESIAN_POINT('Ctrl Pts',(0.0628947552492071,2.48823850886039,
6.00593851239152));
#31185=CARTESIAN_POINT('Ctrl Pts',(0.0426486086851545,2.49151839069546,
6.00698247503907));
#31186=CARTESIAN_POINT('Ctrl Pts',(0.0220848842232862,2.49322006486484,
6.00802643768662));
#31187=CARTESIAN_POINT('Ctrl Pts',(0.00147261683243485,2.49329724306136,
6.00907040033418));
#31188=CARTESIAN_POINT('Ctrl Pts',(-0.0191017320714582,2.49337427928027,
6.01011244249995));
#31189=CARTESIAN_POINT('Ctrl Pts',(-0.0397237194067034,2.49183268925838,
6.01115448466572));
#31190=CARTESIAN_POINT('Ctrl Pts',(-0.0601194976742482,2.48867793351231,
6.01219652683149));
#31191=CARTESIAN_POINT('Ctrl Pts',(-0.0804933711963228,2.48552656592435,
6.01323744986034));
#31192=CARTESIAN_POINT('Ctrl Pts',(-0.100640790089124,2.48076555538682,
6.0142783728892));
#31193=CARTESIAN_POINT('Ctrl Pts',(-0.120293451152618,2.47445210055465,
6.01531929591805));
#31194=CARTESIAN_POINT('Ctrl Pts',(-0.139956205310639,2.46813540329663,
6.01636075353784));
#31195=CARTESIAN_POINT('Ctrl Pts',(-0.159122988566352,2.46026487862171,
6.01740221115763));
#31196=CARTESIAN_POINT('Ctrl Pts',(-0.177540564623014,2.45094762844809,
6.01844366877743));
#31197=CARTESIAN_POINT('Ctrl Pts',(-0.195963768052096,2.44162753144836,
6.01948544460792));
#31198=CARTESIAN_POINT('Ctrl Pts',(-0.213636668904965,2.43086019310176,
6.02052722043842));
#31199=CARTESIAN_POINT('Ctrl Pts',(-0.230331392430929,2.41879827424381,
6.02156899626892));
#31200=CARTESIAN_POINT('Ctrl Pts',(-0.247062201980651,2.40671028327452,
6.02261302392152));
#31201=CARTESIAN_POINT('Ctrl Pts',(-0.262810051886074,2.3933226022145,6.02365705157412));
#31202=CARTESIAN_POINT('Ctrl Pts',(-0.27738024841712,2.3788280613354,6.02470107922672));
#31203=CARTESIAN_POINT('Ctrl Pts',(-0.28253353594759,2.37370153221734,6.02507033812258));
#31204=CARTESIAN_POINT('Ctrl Pts',(-0.287539859418942,2.36843686134083,
6.02543959701845));
#31205=CARTESIAN_POINT('Ctrl Pts',(-0.292391821968674,2.36304355617623,
6.02580885591431));
#31206=CARTESIAN_POINT('Ctrl Pts',(-0.305973877518868,2.34794612506585,
6.02684251905261));
#31207=CARTESIAN_POINT('Ctrl Pts',(-0.318428148253966,2.33174412380622,
6.0278761821909));
#31208=CARTESIAN_POINT('Ctrl Pts',(-0.329571298961343,2.31463375526914,
6.0289098453292));
#31209=CARTESIAN_POINT('Ctrl Pts',(-0.340694798819114,2.29755356071854,
6.02994168561152));
#31210=CARTESIAN_POINT('Ctrl Pts',(-0.350511304813724,2.27956876371628,
6.03097352589383));
#31211=CARTESIAN_POINT('Ctrl Pts',(-0.358878100659044,2.26090804475649,
6.03200536617615));
#31212=CARTESIAN_POINT('Ctrl Pts',(-0.36723586424299,2.24226747072365,6.03303609254924));
#31213=CARTESIAN_POINT('Ctrl Pts',(-0.37414669104312,2.22295309431302,6.03406681892232));
#31214=CARTESIAN_POINT('Ctrl Pts',(-0.379514314441636,2.20321712616565,
6.03509754529541));
#31215=CARTESIAN_POINT('Ctrl Pts',(-0.384885045315495,2.18346973228479,
6.03612886838636));
#31216=CARTESIAN_POINT('Ctrl Pts',(-0.388710579364642,2.16330098220474,
6.03716019147732));
#31217=CARTESIAN_POINT('Ctrl Pts',(-0.390944793159439,2.14297742083377,
6.03819151456827));
#31218=CARTESIAN_POINT('Ctrl Pts',(-0.392527774070581,2.12857780976183,
6.03892222564436));
#31219=CARTESIAN_POINT('Ctrl Pts',(-0.393312985966233,2.11410079734308,
6.03965293672044));
#31220=CARTESIAN_POINT('Ctrl Pts',(-0.393299837367176,2.09964233122461,
6.04038364779653));
#31221=CARTESIAN_POINT('',(-0.393299995571548,2.10005902050583,6.16538364780005));
#31222=CARTESIAN_POINT('Ctrl Pts',(-0.393299837367108,2.09964233114976,
6.04038364780031));
#31223=CARTESIAN_POINT('Ctrl Pts',(-0.393276092566639,2.07353207257771,
6.04170322450934));
#31224=CARTESIAN_POINT('Ctrl Pts',(-0.390648350684809,2.04753914190753,
6.04302280121837));
#31225=CARTESIAN_POINT('Ctrl Pts',(-0.385508793148372,2.02210352764544,
6.0443423779274));
#31226=CARTESIAN_POINT('Ctrl Pts',(-0.383773218647329,2.01351418834557,
6.0447879850973));
#31227=CARTESIAN_POINT('Ctrl Pts',(-0.381751609043668,2.00498820323357,
6.0452335922672));
#31228=CARTESIAN_POINT('Ctrl Pts',(-0.379448708082446,1.99654195084691,
6.0456791994371));
#31229=CARTESIAN_POINT('Ctrl Pts',(-0.374053501840455,1.97675418126185,
6.04672316208466));
#31230=CARTESIAN_POINT('Ctrl Pts',(-0.367090192188503,1.95733061883335,
6.04776712473221));
#31231=CARTESIAN_POINT('Ctrl Pts',(-0.358628009777519,1.93853532707426,
6.04881108737976));
#31232=CARTESIAN_POINT('Ctrl Pts',(-0.350181394462932,1.91977461127967,
6.04985312954553));
#31233=CARTESIAN_POINT('Ctrl Pts',(-0.340241624021866,1.9016405597459,6.0508951717113));
#31234=CARTESIAN_POINT('Ctrl Pts',(-0.328927028196155,1.88438019543176,
6.05193721387707));
#31235=CARTESIAN_POINT('Ctrl Pts',(-0.317624584068612,1.86713836847774,
6.05297813690593));
#31236=CARTESIAN_POINT('Ctrl Pts',(-0.304950622987712,1.85076899402723,
6.05401905993478));
#31237=CARTESIAN_POINT('Ctrl Pts',(-0.291068276854987,1.83549263108815,
6.05505998296363));
#31238=CARTESIAN_POINT('Ctrl Pts',(-0.277178801111106,1.82020842260722,
6.05610144058343));
#31239=CARTESIAN_POINT('Ctrl Pts',(-0.262080183410367,1.80601890244067,
6.05714289820322));
#31240=CARTESIAN_POINT('Ctrl Pts',(-0.245974745650272,1.79311025676591,
6.05818435582301));
#31241=CARTESIAN_POINT('Ctrl Pts',(-0.229864386976807,1.78019766693714,
6.05922613165351));
#31242=CARTESIAN_POINT('Ctrl Pts',(-0.2127471920983,1.76856716225692,6.06026790748401));
#31243=CARTESIAN_POINT('Ctrl Pts',(-0.194856456788532,1.75836298320027,
6.06130968331451));
#31244=CARTESIAN_POINT('Ctrl Pts',(-0.176927050248394,1.74813674757903,
6.0623537109671));
#31245=CARTESIAN_POINT('Ctrl Pts',(-0.158221431665553,1.73934330603197,
6.0633977386197));
#31246=CARTESIAN_POINT('Ctrl Pts',(-0.138995727778631,1.7320800662382,6.0644417662723));
#31247=CARTESIAN_POINT('Ctrl Pts',(-0.132195848319658,1.72951115352792,
6.06481102516816));
#31248=CARTESIAN_POINT('Ctrl Pts',(-0.125331054137186,1.72713320588977,
6.06518028406403));
#31249=CARTESIAN_POINT('Ctrl Pts',(-0.118413061807564,1.72494902107399,
6.06554954295989));
#31250=CARTESIAN_POINT('Ctrl Pts',(-0.098854628228644,1.7187739298614,6.06659350560744));
#31251=CARTESIAN_POINT('Ctrl Pts',(-0.0787535838382332,1.71411447998649,
6.067637468255));
#31252=CARTESIAN_POINT('Ctrl Pts',(-0.058369433768079,1.71105540342924,
6.06868143090255));
#31253=CARTESIAN_POINT('Ctrl Pts',(-0.0380227825384923,1.70800195437295,
6.06972347306832));
#31254=CARTESIAN_POINT('Ctrl Pts',(-0.0173947699898787,1.70654320156851,
6.07076551523409));
#31255=CARTESIAN_POINT('Ctrl Pts',(0.00324284852386898,1.7067133692414,
6.07180755739986));
#31256=CARTESIAN_POINT('Ctrl Pts',(0.0238583025595397,1.70688335415688,
6.07284848042871));
#31257=CARTESIAN_POINT('Ctrl Pts',(0.0444826098181244,1.70867880938727,
6.07388940345757));
#31258=CARTESIAN_POINT('Ctrl Pts',(0.0648420140908806,1.71208196328523,
6.07493032648642));
#31259=CARTESIAN_POINT('Ctrl Pts',(0.0852118744230393,1.71548686495434,
6.07597178410621));
#31260=CARTESIAN_POINT('Ctrl Pts',(0.105315831609809,1.72050100939405,6.077013241726));
#31261=CARTESIAN_POINT('Ctrl Pts',(0.124887816480819,1.7270550666725,6.0780546993458));
#31262=CARTESIAN_POINT('Ctrl Pts',(0.144465781446479,1.73361112650118,6.07909647517629));
#31263=CARTESIAN_POINT('Ctrl Pts',(0.163510764894453,1.74170776809457,6.08013825100679));
#31264=CARTESIAN_POINT('Ctrl Pts',(0.181775199633076,1.75122691216443,6.08118002683729));
#31265=CARTESIAN_POINT('Ctrl Pts',(0.200079113361855,1.76076663208022,6.08222405448989));
#31266=CARTESIAN_POINT('Ctrl Pts',(0.217598485783747,1.77173460230041,6.08326808214248));
#31267=CARTESIAN_POINT('Ctrl Pts',(0.234112768746594,1.78396819541413,6.08431210979508));
#31268=CARTESIAN_POINT('Ctrl Pts',(0.239953654165408,1.78829505694353,6.08468136869095));
#31269=CARTESIAN_POINT('Ctrl Pts',(0.245669112245223,1.79277987277877,6.08505062758681));
#31270=CARTESIAN_POINT('Ctrl Pts',(0.251250448193061,1.79741430588545,6.08541988648268));
#31271=CARTESIAN_POINT('Ctrl Pts',(0.267029908940553,1.81051669857012,6.08646384913023));
#31272=CARTESIAN_POINT('Ctrl Pts',(0.281828716351315,1.82489577218219,6.08750781177779));
#31273=CARTESIAN_POINT('Ctrl Pts',(0.295435151442728,1.84037919711238,6.08855177442534));
#31274=CARTESIAN_POINT('Ctrl Pts',(0.309016556030614,1.85583413861398,6.08959381659111));
#31275=CARTESIAN_POINT('Ctrl Pts',(0.321409417423752,1.87238889164568,6.09063585875688));
#31276=CARTESIAN_POINT('Ctrl Pts',(0.332437853197238,1.88983348563196,6.09167790092265));
#31277=CARTESIAN_POINT('Ctrl Pts',(0.343454444603954,1.90725934439834,6.0927188239515));
#31278=CARTESIAN_POINT('Ctrl Pts',(0.353109103876376,1.9255725435649,6.09375974698036));
#31279=CARTESIAN_POINT('Ctrl Pts',(0.361268584551529,1.94453328389609,6.09480067000921));
#31280=CARTESIAN_POINT('Ctrl Pts',(0.369432255723295,1.96350376196933,6.095842127629));
#31281=CARTESIAN_POINT('Ctrl Pts',(0.376098908583875,1.98312177610599,6.09688358524879));
#31282=CARTESIAN_POINT('Ctrl Pts',(0.3811828089318,2.003126081039,6.09792504286859));
#31283=CARTESIAN_POINT('Ctrl Pts',(0.38626826263292,2.02313649815927,6.09896681869908));
#31284=CARTESIAN_POINT('Ctrl Pts',(0.389769855077223,2.04353271962256,6.10000859452958));
#31285=CARTESIAN_POINT('Ctrl Pts',(0.391652856850279,2.06404266804928,6.10105037036008));
#31286=CARTESIAN_POINT('Ctrl Pts',(0.3935399287744,2.08459694919495,6.10209439801268));
#31287=CARTESIAN_POINT('Ctrl Pts',(0.393801415885455,2.10526471165969,6.10313842566527));
#31288=CARTESIAN_POINT('Ctrl Pts',(0.392454671522441,2.12577248145237,6.10418245331787));
#31289=CARTESIAN_POINT('Ctrl Pts',(0.391978345694036,2.13302581081726,6.10455171221374));
#31290=CARTESIAN_POINT('Ctrl Pts',(0.391301312972275,2.14025918214962,6.1049209711096));
#31291=CARTESIAN_POINT('Ctrl Pts',(0.390425876636419,2.14746077172448,6.10529023000547));
#31292=CARTESIAN_POINT('Ctrl Pts',(0.387950857496259,2.16782098674792,6.10633419265302));
#31293=CARTESIAN_POINT('Ctrl Pts',(0.383871536803702,2.18804774134201,6.10737815530058));
#31294=CARTESIAN_POINT('Ctrl Pts',(0.378218205068872,2.20786973326416,6.10842211794813));
#31295=CARTESIAN_POINT('Ctrl Pts',(0.372575273246948,2.22765526049623,6.1094641601139));
#31296=CARTESIAN_POINT('Ctrl Pts',(0.365364220292138,2.24703678718359,6.11050620227967));
#31297=CARTESIAN_POINT('Ctrl Pts',(0.356666384889145,2.26575276736787,6.11154824444544));
#31298=CARTESIAN_POINT('Ctrl Pts',(0.347977890824735,2.28444864688345,6.11258916747429));
#31299=CARTESIAN_POINT('Ctrl Pts',(0.33780606659172,2.30247972286781,6.11363009050315));
#31300=CARTESIAN_POINT('Ctrl Pts',(0.326280410962804,2.31960415165006,6.114671013532));
#31301=CARTESIAN_POINT('Ctrl Pts',(0.314748836057552,2.33673737509262,6.11571247115179));
#31302=CARTESIAN_POINT('Ctrl Pts',(0.30186243817519,2.35296240170731,6.11675392877158));
#31303=CARTESIAN_POINT('Ctrl Pts',(0.28779446754134,2.36806572785904,6.11779538639138));
#31304=CARTESIAN_POINT('Ctrl Pts',(0.27372219852915,2.38317366873536,6.11883716222187));
#31305=CARTESIAN_POINT('Ctrl Pts',(0.258468165600901,2.39715871357079,6.11987893805237));
#31306=CARTESIAN_POINT('Ctrl Pts',(0.242242336629156,2.4098443808502,6.12092071388287));
#31307=CARTESIAN_POINT('Ctrl Pts',(0.225981435159879,2.42255746848731,6.12196474153547));
#31308=CARTESIAN_POINT('Ctrl Pts',(0.208745158133959,2.43396516479699,6.12300876918806));
#31309=CARTESIAN_POINT('Ctrl Pts',(0.190772841055458,2.4439340243646,6.12405279684066));
#31310=CARTESIAN_POINT('Ctrl Pts',(0.184416268081496,2.44745987932431,6.12442205573653));
#31311=CARTESIAN_POINT('Ctrl Pts',(0.177967829910699,2.45080617269093,6.12479131463239));
#31312=CARTESIAN_POINT('Ctrl Pts',(0.171438714949408,2.45396844070693,6.12516057352826));
#31313=CARTESIAN_POINT('Ctrl Pts',(0.152979709039263,2.46290875257812,6.12620453617581));
#31314=CARTESIAN_POINT('Ctrl Pts',(0.133764481629443,2.47042789443814,6.12724849882337));
#31315=CARTESIAN_POINT('Ctrl Pts',(0.114037545303458,2.4764044742842,6.12829246147092));
#31316=CARTESIAN_POINT('Ctrl Pts',(0.0943468988025437,2.48237005956761,
6.12933450363669));
#31317=CARTESIAN_POINT('Ctrl Pts',(0.0741470908896119,2.48679844773158,
6.13037654580246));
#31318=CARTESIAN_POINT('Ctrl Pts',(0.0537020641890218,2.48961645024542,
6.13141858796823));
#31319=CARTESIAN_POINT('Ctrl Pts',(0.0332789951259194,2.49243142626882,
6.13245951099708));
#31320=CARTESIAN_POINT('Ctrl Pts',(0.0126119513524283,2.49363932156465,
6.13350043402594));
#31321=CARTESIAN_POINT('Ctrl Pts',(-0.00802562061735804,2.49321810667072,
6.13454135705479));
#31322=CARTESIAN_POINT('Ctrl Pts',(-0.0286737915062241,2.4927966754518,
6.13558281467458));
#31323=CARTESIAN_POINT('Ctrl Pts',(-0.0492917243991184,2.49074446146345,
6.13662427229437));
#31324=CARTESIAN_POINT('Ctrl Pts',(-0.0696061181394477,2.48709156322188,
6.13766572991417));
#31325=CARTESIAN_POINT('Ctrl Pts',(-0.0899267188126951,2.48343754886064,
6.13870750574466));
#31326=CARTESIAN_POINT('Ctrl Pts',(-0.109942878550889,2.47818204232365,
6.13974928157516));
#31327=CARTESIAN_POINT('Ctrl Pts',(-0.129392549133005,2.47140605572454,
6.14079105740566));
#31328=CARTESIAN_POINT('Ctrl Pts',(-0.148884260619454,2.46461542267663,
6.14183508505826));
#31329=CARTESIAN_POINT('Ctrl Pts',(-0.167806364118297,2.45629804448474,
6.14287911271085));
#31330=CARTESIAN_POINT('Ctrl Pts',(-0.185917099702794,2.44658292231168,
6.14392314036345));
#31331=CARTESIAN_POINT('Ctrl Pts',(-0.192322629487972,2.44314681094249,
6.14429239925932));
#31332=CARTESIAN_POINT('Ctrl Pts',(-0.198626908961687,2.43953625773621,
6.14466165815518));
#31333=CARTESIAN_POINT('Ctrl Pts',(-0.20482012843017,2.43575825379259,6.14503091705105));
#31334=CARTESIAN_POINT('Ctrl Pts',(-0.222329496154477,2.42507714348327,
6.1460748796986));
#31335=CARTESIAN_POINT('Ctrl Pts',(-0.239053275050047,2.41299088359138,
6.14711884234616));
#31336=CARTESIAN_POINT('Ctrl Pts',(-0.25475703746797,2.39963935299046,6.14816280499371));
#31337=CARTESIAN_POINT('Ctrl Pts',(-0.270431911122744,2.3863123839688,6.14920484715948));
#31338=CARTESIAN_POINT('Ctrl Pts',(-0.285089900189208,2.37172519033955,
6.15024688932525));
#31339=CARTESIAN_POINT('Ctrl Pts',(-0.298526589528653,2.3560600815129,6.15128893149102));
#31340=CARTESIAN_POINT('Ctrl Pts',(-0.311948848074838,2.34041179676703,
6.15232985451987));
#31341=CARTESIAN_POINT('Ctrl Pts',(-0.324151912290571,2.32368843188051,
6.15337077754873));
#31342=CARTESIAN_POINT('Ctrl Pts',(-0.334969237870668,2.30610798063235,
6.15441170057758));
#31343=CARTESIAN_POINT('Ctrl Pts',(-0.345792118947249,2.28851850052263,
6.15545315819737));
#31344=CARTESIAN_POINT('Ctrl Pts',(-0.35522744029955,2.27007167288185,6.15649461581716));
#31345=CARTESIAN_POINT('Ctrl Pts',(-0.363152566444587,2.25101358708643,
6.15753607343695));
#31346=CARTESIAN_POINT('Ctrl Pts',(-0.371080114061167,2.23194967821494,
6.15857784926745));
#31347=CARTESIAN_POINT('Ctrl Pts',(-0.377496299003602,2.2122748320806,6.15961962509795));
#31348=CARTESIAN_POINT('Ctrl Pts',(-0.382327386270553,2.19225323684038,
6.16066140092845));
#31349=CARTESIAN_POINT('Ctrl Pts',(-0.387168916042263,2.1721883644677,6.16170542858104));
#31350=CARTESIAN_POINT('Ctrl Pts',(-0.39041839206562,2.1517759739565,6.16274945623364));
#31351=CARTESIAN_POINT('Ctrl Pts',(-0.39205341181135,2.1312891720421,6.16379348388624));
#31352=CARTESIAN_POINT('Ctrl Pts',(-0.392631696863979,2.12404325874091,
6.1641627427821));
#31353=CARTESIAN_POINT('Ctrl Pts',(-0.393008499473629,2.11678804999605,
6.16453200167797));
#31354=CARTESIAN_POINT('Ctrl Pts',(-0.393184387717665,2.10953557838228,
6.16490126057383));
#31355=CARTESIAN_POINT('Ctrl Pts',(-0.393260979184605,2.10637745122671,
6.16506205631473));
#31356=CARTESIAN_POINT('Ctrl Pts',(-0.393299521459542,2.10321839755623,
6.16522285205563));
#31357=CARTESIAN_POINT('Ctrl Pts',(-0.393299995571538,2.10005902057492,
6.16538364779653));
#31358=CARTESIAN_POINT('',(-0.393227355315136,2.10032536725365,6.2903836446444));
#31359=CARTESIAN_POINT('Ctrl Pts',(-0.393299995571548,2.10005902050583,
6.16538364780004));
#31360=CARTESIAN_POINT('Ctrl Pts',(-0.393303061112308,2.07963091419915,
6.16642333141745));
#31361=CARTESIAN_POINT('Ctrl Pts',(-0.391710255539657,2.05913958273797,
6.16746301503486));
#31362=CARTESIAN_POINT('Ctrl Pts',(-0.388518105140135,2.0388561370347,6.16850269865227));
#31363=CARTESIAN_POINT('Ctrl Pts',(-0.385331781825707,2.01860971758312,
6.16954048438763));
#31364=CARTESIAN_POINT('Ctrl Pts',(-0.380551962062052,1.9985711652666,6.170578270123));
#31365=CARTESIAN_POINT('Ctrl Pts',(-0.374227035493721,1.97900819901505,
6.17161605585837));
#31366=CARTESIAN_POINT('Ctrl Pts',(-0.367908708593547,1.95946564550412,
6.17265275872876));
#31367=CARTESIAN_POINT('Ctrl Pts',(-0.360048675288858,1.94039840477248,
6.17368946159915));
#31368=CARTESIAN_POINT('Ctrl Pts',(-0.350745521553215,1.92206049030538,
6.17472616446954));
#31369=CARTESIAN_POINT('Ctrl Pts',(-0.341437353842434,1.90371269253958,
6.17576342607544));
#31370=CARTESIAN_POINT('Ctrl Pts',(-0.330684836323542,1.88609567427874,
6.17680068768135));
#31371=CARTESIAN_POINT('Ctrl Pts',(-0.318633368128757,1.86944053540372,
6.17783794928726));
#31372=CARTESIAN_POINT('Ctrl Pts',(-0.306577526772869,1.85277935281649,
6.17887558728814));
#31373=CARTESIAN_POINT('Ctrl Pts',(-0.293222264163319,1.83708132115032,
6.17991322528903));
#31374=CARTESIAN_POINT('Ctrl Pts',(-0.278753793705845,1.82254511628988,
6.18095086328991));
#31375=CARTESIAN_POINT('Ctrl Pts',(-0.264254735541846,1.80797818052601,
6.18199069495507));
#31376=CARTESIAN_POINT('Ctrl Pts',(-0.248638340683192,1.79457845148889,
6.18303052662022));
#31377=CARTESIAN_POINT('Ctrl Pts',(-0.232124886913118,1.78250523330995,
6.18407035828537));
#31378=CARTESIAN_POINT('Ctrl Pts',(-0.228412750717217,1.77979123835607,
6.18430410688912));
#31379=CARTESIAN_POINT('Ctrl Pts',(-0.224655394221444,1.77714409837398,
6.18453785549287));
#31380=CARTESIAN_POINT('Ctrl Pts',(-0.22085549849512,1.774565307958,6.18477160409662));
#31381=CARTESIAN_POINT('Ctrl Pts',(-0.203884491442143,1.76304797340731,
6.18581556674418));
#31382=CARTESIAN_POINT('Ctrl Pts',(-0.185959571037253,1.75282742121085,
6.18685952939173));
#31383=CARTESIAN_POINT('Ctrl Pts',(-0.167305110205114,1.74405914803263,
6.18790349203929));
#31384=CARTESIAN_POINT('Ctrl Pts',(-0.148684966263819,1.73530700503777,
6.18894553420505));
#31385=CARTESIAN_POINT('Ctrl Pts',(-0.129338578916634,1.72800220127159,
6.18998757637082));
#31386=CARTESIAN_POINT('Ctrl Pts',(-0.109516521935822,1.72225534891533,
6.19102961853659));
#31387=CARTESIAN_POINT('Ctrl Pts',(-0.0897157535328079,1.71651466858821,
6.19207054156545));
#31388=CARTESIAN_POINT('Ctrl Pts',(-0.0694410247200447,1.71232884955851,
6.1931114645943));
#31389=CARTESIAN_POINT('Ctrl Pts',(-0.0489597161328431,1.70975925866692,
6.19415238762315));
#31390=CARTESIAN_POINT('Ctrl Pts',(-0.028467888879353,1.70718834810042,
6.19519384524295));
#31391=CARTESIAN_POINT('Ctrl Pts',(-0.00776999794767176,1.70623543151968,
6.19623530286274));
#31392=CARTESIAN_POINT('Ctrl Pts',(0.0128591766436706,1.70691027541279,
6.19727676048253));
#31393=CARTESIAN_POINT('Ctrl Pts',(0.0334946543472138,1.70758532550014,
6.19831853631303));
#31394=CARTESIAN_POINT('Ctrl Pts',(0.0540606403303332,1.70988906597326,
6.19936031214353));
#31395=CARTESIAN_POINT('Ctrl Pts',(0.0742861215870826,1.71377925723811,
6.20040208797403));
#31396=CARTESIAN_POINT('Ctrl Pts',(0.0945553206805387,1.71767785723965,
6.20144611562662));
#31397=CARTESIAN_POINT('Ctrl Pts',(0.114481835635049,1.72316955848568,6.20249014327922));
#31398=CARTESIAN_POINT('Ctrl Pts',(0.133807783915114,1.73016170159957,6.20353417093182));
#31399=CARTESIAN_POINT('Ctrl Pts',(0.140643118502037,1.73263473096767,6.20390342982768));
#31400=CARTESIAN_POINT('Ctrl Pts',(0.147403511174077,1.73529501761734,6.20427268872355));
#31401=CARTESIAN_POINT('Ctrl Pts',(0.154078243835575,1.73813706354955,6.20464194761942));
#31402=CARTESIAN_POINT('Ctrl Pts',(0.172948937701002,1.7461720488378,6.20568591026697));
#31403=CARTESIAN_POINT('Ctrl Pts',(0.191245644278404,1.75571107327129,6.20672987291453));
#31404=CARTESIAN_POINT('Ctrl Pts',(0.208716162070342,1.76664965323158,6.20777383556208));
#31405=CARTESIAN_POINT('Ctrl Pts',(0.226154540962252,1.77756811049533,6.20881587772785));
#31406=CARTESIAN_POINT('Ctrl Pts',(0.242769099794949,1.78988067709395,6.20985791989362));
#31407=CARTESIAN_POINT('Ctrl Pts',(0.258331193755519,1.80343654248568,6.21089996205939));
#31408=CARTESIAN_POINT('Ctrl Pts',(0.273876574271647,1.81697784909093,6.21194088508825));
#31409=CARTESIAN_POINT('Ctrl Pts',(0.288371162903788,1.83175934460952,6.2129818081171));
#31410=CARTESIAN_POINT('Ctrl Pts',(0.301618623344404,1.8475894295957,6.21402273114595));
#31411=CARTESIAN_POINT('Ctrl Pts',(0.314872887335429,1.86342764450093,6.21506418876575));
#31412=CARTESIAN_POINT('Ctrl Pts',(0.326878259006371,1.88031497081602,6.21610564638554));
#31413=CARTESIAN_POINT('Ctrl Pts',(0.3374777831302,1.8980256553581,6.21714710400533));
#31414=CARTESIAN_POINT('Ctrl Pts',(0.348080545870744,1.91574175128641,6.21818887983583));
#31415=CARTESIAN_POINT('Ctrl Pts',(0.357276259450329,1.93428105686638,6.21923065566632));
#31416=CARTESIAN_POINT('Ctrl Pts',(0.36495373543889,1.95339283445479,6.22027243149682));
#31417=CARTESIAN_POINT('Ctrl Pts',(0.37264780646603,1.97254592258418,6.22131645914942));
#31418=CARTESIAN_POINT('Ctrl Pts',(0.378816868326995,1.99227325024314,6.22236048680201));
#31419=CARTESIAN_POINT('Ctrl Pts',(0.38339923420854,2.01230782698379,6.22340451445461));
#31420=CARTESIAN_POINT('Ctrl Pts',(0.385019956956315,2.01939379416864,6.22377377335048));
#31421=CARTESIAN_POINT('Ctrl Pts',(0.386442663016391,2.0265181145997,6.22414303224634));
#31422=CARTESIAN_POINT('Ctrl Pts',(0.387666173305935,2.03366880014403,6.22451229114221));
#31423=CARTESIAN_POINT('Ctrl Pts',(0.391125261375264,2.05388510013373,6.22555625378976));
#31424=CARTESIAN_POINT('Ctrl Pts',(0.393009016712081,2.07443294490035,6.22660021643731));
#31425=CARTESIAN_POINT('Ctrl Pts',(0.393268769785939,2.09504372003876,6.22764417908486));
#31426=CARTESIAN_POINT('Ctrl Pts',(0.393528045016027,2.11561657943536,6.22868622125063));
#31427=CARTESIAN_POINT('Ctrl Pts',(0.392169179473157,2.13625141274911,6.2297282634164));
#31428=CARTESIAN_POINT('Ctrl Pts',(0.389195207792429,2.15667433485633,6.23077030558217));
#31429=CARTESIAN_POINT('Ctrl Pts',(0.386224430110566,2.17707532306606,6.23181122861102));
#31430=CARTESIAN_POINT('Ctrl Pts',(0.381642066752141,2.19726412331353,6.23285215163988));
#31431=CARTESIAN_POINT('Ctrl Pts',(0.37550293757078,2.21697193627411,6.23389307466873));
#31432=CARTESIAN_POINT('Ctrl Pts',(0.369360655492676,2.23668987065379,6.23493453228852));
#31433=CARTESIAN_POINT('Ctrl Pts',(0.361660213778556,2.25592561697248,6.23597598990831));
#31434=CARTESIAN_POINT('Ctrl Pts',(0.352506467046164,2.27442500018814,6.23701744752811));
#31435=CARTESIAN_POINT('Ctrl Pts',(0.343349923445087,2.29293003577185,6.2380592233586));
#31436=CARTESIAN_POINT('Ctrl Pts',(0.33273954929525,2.31069761748757,6.2391009991891));
#31437=CARTESIAN_POINT('Ctrl Pts',(0.320825980990119,2.32749852729573,6.2401427750196));
#31438=CARTESIAN_POINT('Ctrl Pts',(0.308886661236732,2.34433575265173,6.24118680267219));
#31439=CARTESIAN_POINT('Ctrl Pts',(0.295638995588657,2.36020156922966,6.24223083032479));
#31440=CARTESIAN_POINT('Ctrl Pts',(0.281274082208155,2.37489958289885,6.24327485797739));
#31441=CARTESIAN_POINT('Ctrl Pts',(0.276193400637187,2.38009807767573,6.24364411687325));
#31442=CARTESIAN_POINT('Ctrl Pts',(0.270973280959128,2.38515083778139,6.24401337576912));
#31443=CARTESIAN_POINT('Ctrl Pts',(0.265623164751951,2.39005038242891,6.24438263466499));
#31444=CARTESIAN_POINT('Ctrl Pts',(0.250497404633898,2.40390229408023,6.24542659731255));
#31445=CARTESIAN_POINT('Ctrl Pts',(0.23424011965874,2.41660910894307,6.2464705599601));
#31446=CARTESIAN_POINT('Ctrl Pts',(0.217050819931449,2.42798449897379,6.24751452260765));
#31447=CARTESIAN_POINT('Ctrl Pts',(0.19989314177325,2.43933896274878,6.24855656477342));
#31448=CARTESIAN_POINT('Ctrl Pts',(0.18180742599756,2.4493664123912,6.24959860693919));
#31449=CARTESIAN_POINT('Ctrl Pts',(0.163025602822916,2.45792114051034,6.25064064910496));
#31450=CARTESIAN_POINT('Ctrl Pts',(0.144263951031311,2.46646668098588,6.25168157213382));
#31451=CARTESIAN_POINT('Ctrl Pts',(0.124808330231236,2.47354231019215,6.25272249516267));
#31452=CARTESIAN_POINT('Ctrl Pts',(0.104914426684827,2.47904861571228,6.25376341819153));
#31453=CARTESIAN_POINT('Ctrl Pts',(0.0850103061480592,2.48455774912741,
6.25480487581132));
#31454=CARTESIAN_POINT('Ctrl Pts',(0.0646681580011058,2.4884957369127,6.25584633343111));
#31455=CARTESIAN_POINT('Ctrl Pts',(0.0441584568693738,2.49081315316519,
6.2568877910509));
#31456=CARTESIAN_POINT('Ctrl Pts',(0.0236424891298007,2.49313127748937,
6.2579295668814));
#31457=CARTESIAN_POINT('Ctrl Pts',(0.00295960106099637,2.49382779795452,
6.2589713427119));
#31458=CARTESIAN_POINT('Ctrl Pts',(-0.0176159345037573,2.49290529247079,
6.2600131185424));
#31459=CARTESIAN_POINT('Ctrl Pts',(-0.0382359445555444,2.49198079297053,
6.261057146195));
#31460=CARTESIAN_POINT('Ctrl Pts',(-0.0587474079873671,2.48943037169309,
6.26210117384759));
#31461=CARTESIAN_POINT('Ctrl Pts',(-0.0788817482096687,2.48530839570322,
6.26314520150019));
#31462=CARTESIAN_POINT('Ctrl Pts',(-0.0860030004303546,2.48385050682544,
6.26351446039606));
#31463=CARTESIAN_POINT('Ctrl Pts',(-0.0930771966970507,2.48219648707988,
6.26388371929192));
#31464=CARTESIAN_POINT('Ctrl Pts',(-0.10009293613341,2.48035022562921,6.26425297818779));
#31465=CARTESIAN_POINT('Ctrl Pts',(-0.119927718716834,2.47513050576955,
6.26529694083534));
#31466=CARTESIAN_POINT('Ctrl Pts',(-0.139412198268763,2.4683395179686,6.2663409034829));
#31467=CARTESIAN_POINT('Ctrl Pts',(-0.158281708409268,2.46004415115794,
6.26738486613045));
#31468=CARTESIAN_POINT('Ctrl Pts',(-0.177116506052565,2.45176404456841,
6.26842690829622));
#31469=CARTESIAN_POINT('Ctrl Pts',(-0.19533788998475,2.44198529060657,6.26946895046199));
#31470=CARTESIAN_POINT('Ctrl Pts',(-0.212697798804906,2.43082402630938,
6.27051099262776));
#31471=CARTESIAN_POINT('Ctrl Pts',(-0.230039063355709,2.4196747490347,6.27155191565661));
#31472=CARTESIAN_POINT('Ctrl Pts',(-0.246520058156968,2.40714628066294,
6.27259283868546));
#31473=CARTESIAN_POINT('Ctrl Pts',(-0.261918787875003,2.3933997930437,6.27363376171432));
#31474=CARTESIAN_POINT('Ctrl Pts',(-0.277325425979278,2.37964624558671,
6.27467521933411));
#31475=CARTESIAN_POINT('Ctrl Pts',(-0.291648128967637,2.36467390715421,
6.2757166769539));
#31476=CARTESIAN_POINT('Ctrl Pts',(-0.304698925854026,2.34868344251961,
6.27675813457369));
#31477=CARTESIAN_POINT('Ctrl Pts',(-0.317753710327837,2.33268809210092,
6.27779991040419));
#31478=CARTESIAN_POINT('Ctrl Pts',(-0.329535378233429,2.3156745886114,6.27884168623469));
#31479=CARTESIAN_POINT('Ctrl Pts',(-0.339897628283363,2.29787494102929,
6.27988346206518));
#31480=CARTESIAN_POINT('Ctrl Pts',(-0.350282276571922,2.28003681910502,
6.28092748971778));
#31481=CARTESIAN_POINT('Ctrl Pts',(-0.359241062472394,2.26140982428574,
6.28197151737038));
#31482=CARTESIAN_POINT('Ctrl Pts',(-0.366674313425443,2.24224921045117,
6.28301554502297));
#31483=CARTESIAN_POINT('Ctrl Pts',(-0.369303356854312,2.23547235249049,
6.28338480391884));
#31484=CARTESIAN_POINT('Ctrl Pts',(-0.371742017699808,2.22862889083584,
6.2837540628147));
#31485=CARTESIAN_POINT('Ctrl Pts',(-0.373987394539171,2.22173051682221,
6.28412332171057));
#31486=CARTESIAN_POINT('Ctrl Pts',(-0.381544018087779,2.19851462958019,
6.28536603091604));
#31487=CARTESIAN_POINT('Ctrl Pts',(-0.386944506159296,2.17456429864603,
6.28660874012152));
#31488=CARTESIAN_POINT('Ctrl Pts',(-0.390076693750689,2.15025000490081,
6.28785144932699));
#31489=CARTESIAN_POINT('Ctrl Pts',(-0.39220411762502,2.13373541007154,6.28869551410774));
#31490=CARTESIAN_POINT('Ctrl Pts',(-0.393286023394877,2.11705335145469,
6.28953957888848));
#31491=CARTESIAN_POINT('Ctrl Pts',(-0.393299865350261,2.10032544656516,
6.29038364366923));
#31492=CARTESIAN_POINT('',(-0.393115187231275,2.09978487279504,6.41538365076377));
#31493=CARTESIAN_POINT('Ctrl Pts',(-0.392992974431572,2.10032511088776,
6.29038364779653));
#31494=CARTESIAN_POINT('Ctrl Pts',(-0.392294339636222,2.01048562007843,
6.29492032027548));
#31495=CARTESIAN_POINT('Ctrl Pts',(-0.317093268726177,1.7884251043508,6.30608044059534));
#31496=CARTESIAN_POINT('Ctrl Pts',(0.0520281133013657,1.63786569494271,
6.32386400875615));
#31497=CARTESIAN_POINT('Ctrl Pts',(0.416734555740583,1.89358451963055,6.34373435227894));
#31498=CARTESIAN_POINT('Ctrl Pts',(0.399143776574688,2.33866144662726,6.36360469580175));
#31499=CARTESIAN_POINT('Ctrl Pts',(0.0153929209198437,2.56479898716546,
6.38347503932451));
#31500=CARTESIAN_POINT('Ctrl Pts',(-0.330203906139794,2.39085715588212,
6.40073468998947));
#31501=CARTESIAN_POINT('Ctrl Pts',(-0.392376313660633,2.17936284500731,
6.41137089281346));
#31502=CARTESIAN_POINT('Ctrl Pts',(-0.392770159222556,2.09978512047867,
6.41538364779653));
#31503=CARTESIAN_POINT('',(-0.393299932545456,2.09976965300128,6.54038364779198));
#31504=CARTESIAN_POINT('Ctrl Pts',(-0.393299941092297,2.09978474016666,
6.41538365235266));
#31505=CARTESIAN_POINT('Ctrl Pts',(-0.393287381153227,2.07683655136687,
6.41653927342683));
#31506=CARTESIAN_POINT('Ctrl Pts',(-0.391262216182739,2.05396047902279,
6.41769489450101));
#31507=CARTESIAN_POINT('Ctrl Pts',(-0.38728651038287,2.03148687078042,6.41885051557518));
#31508=CARTESIAN_POINT('Ctrl Pts',(-0.383279315437034,2.00883526276493,
6.42001528962056));
#31509=CARTESIAN_POINT('Ctrl Pts',(-0.377290759060769,1.98659292679144,
6.42118006366594));
#31510=CARTESIAN_POINT('Ctrl Pts',(-0.369433581160785,1.96507884113039,
6.42234483771131));
#31511=CARTESIAN_POINT('Ctrl Pts',(-0.36747533951717,1.95971689323994,6.42263513393091));
#31512=CARTESIAN_POINT('Ctrl Pts',(-0.365401256312991,1.95440007141614,
6.4229254301505));
#31513=CARTESIAN_POINT('Ctrl Pts',(-0.363213523926563,1.94913308501581,
6.4232157263701));
#31514=CARTESIAN_POINT('Ctrl Pts',(-0.355346005371014,1.9301919597239,6.42425968901765));
#31515=CARTESIAN_POINT('Ctrl Pts',(-0.345969422449791,1.91181147682915,
6.42530365166521));
#31516=CARTESIAN_POINT('Ctrl Pts',(-0.335186020749563,1.89424475342273,
6.42634761431276));
#31517=CARTESIAN_POINT('Ctrl Pts',(-0.324422456278741,1.87671034589693,
6.42738965647853));
#31518=CARTESIAN_POINT('Ctrl Pts',(-0.312257539988718,1.85998737746704,
6.4284316986443));
#31519=CARTESIAN_POINT('Ctrl Pts',(-0.298840051230804,1.84430581981521,
6.42947374081007));
#31520=CARTESIAN_POINT('Ctrl Pts',(-0.285436972645028,1.82864110390995,
6.43051466383893));
#31521=CARTESIAN_POINT('Ctrl Pts',(-0.270784446168001,1.81401615340673,
6.43155558686778));
#31522=CARTESIAN_POINT('Ctrl Pts',(-0.255072324634896,1.80062899404694,
6.43259650989664));
#31523=CARTESIAN_POINT('Ctrl Pts',(-0.239352133765684,1.78723495939101,
6.43363796751643));
#31524=CARTESIAN_POINT('Ctrl Pts',(-0.222571810292413,1.77508047531464,
6.43467942513622));
#31525=CARTESIAN_POINT('Ctrl Pts',(-0.204955708274494,1.76432449054824,
6.43572088275601));
#31526=CARTESIAN_POINT('Ctrl Pts',(-0.187334223769412,1.75356521935957,
6.43676265858651));
#31527=CARTESIAN_POINT('Ctrl Pts',(-0.168877098645611,1.74420565036361,
6.43780443441701));
#31528=CARTESIAN_POINT('Ctrl Pts',(-0.149834075832615,1.73635918859486,
6.43884621024751));
#31529=CARTESIAN_POINT('Ctrl Pts',(-0.130749891093668,1.72849576652095,
6.43989023790011));
#31530=CARTESIAN_POINT('Ctrl Pts',(-0.111077981232955,1.72215220732753,
6.4409342655527));
#31531=CARTESIAN_POINT('Ctrl Pts',(-0.0910847798190486,1.71739256033721,
6.4419782932053));
#31532=CARTESIAN_POINT('Ctrl Pts',(-0.0840134465449763,1.71570913558503,
6.44234755210116));
#31533=CARTESIAN_POINT('Ctrl Pts',(-0.0769020075508997,1.71422338002955,
6.44271681099702));
#31534=CARTESIAN_POINT('Ctrl Pts',(-0.069762440055462,1.712936578895,6.44308606989289));
#31535=CARTESIAN_POINT('Ctrl Pts',(-0.0495775728297026,1.70929855599466,
6.44413003254044));
#31536=CARTESIAN_POINT('Ctrl Pts',(-0.0290472199612253,1.70723286729158,
6.44517399518799));
#31537=CARTESIAN_POINT('Ctrl Pts',(-0.00843955421571544,1.70679055972085,
6.44621795783555));
#31538=CARTESIAN_POINT('Ctrl Pts',(0.012130201508055,1.70634906582256,6.44726000000132));
#31539=CARTESIAN_POINT('Ctrl Pts',(0.0327762617722319,1.70752510026857,
6.44830204216709));
#31540=CARTESIAN_POINT('Ctrl Pts',(0.0532247253178052,1.7103180545434,6.44934408433286));
#31541=CARTESIAN_POINT('Ctrl Pts',(0.0736512275347659,1.7131080092292,6.45038500736171));
#31542=CARTESIAN_POINT('Ctrl Pts',(0.0938798251049557,1.71751136587206,
6.45142593039057));
#31543=CARTESIAN_POINT('Ctrl Pts',(0.113641243669386,1.72347568772087,6.45246685341942));
#31544=CARTESIAN_POINT('Ctrl Pts',(0.133412811183346,1.72944307268992,6.45350831103921));
#31545=CARTESIAN_POINT('Ctrl Pts',(0.152716011310585,1.73697282725947,6.454549768659));
#31546=CARTESIAN_POINT('Ctrl Pts',(0.171295750206517,1.74596235233921,6.45559122627879));
#31547=CARTESIAN_POINT('Ctrl Pts',(0.189881166022688,1.75495462411077,6.45663300210929));
#31548=CARTESIAN_POINT('Ctrl Pts',(0.207742034540402,1.76540720156411,6.45767477793979));
#31549=CARTESIAN_POINT('Ctrl Pts',(0.224647812415882,1.77717148456687,6.45871655377029));
#31550=CARTESIAN_POINT('Ctrl Pts',(0.241590132513881,1.7889611963343,6.45976058142289));
#31551=CARTESIAN_POINT('Ctrl Pts',(0.257572670917688,1.80206780714636,6.46080460907548));
#31552=CARTESIAN_POINT('Ctrl Pts',(0.272397348505266,1.81630196594389,6.46184863672808));
#31553=CARTESIAN_POINT('Ctrl Pts',(0.277640642649778,1.82133640133274,6.46221789562395));
#31554=CARTESIAN_POINT('Ctrl Pts',(0.28273944294546,1.82651156023687,6.46258715451981));
#31555=CARTESIAN_POINT('Ctrl Pts',(0.287686185267906,1.83181806771149,6.46295641341568));
#31556=CARTESIAN_POINT('Ctrl Pts',(0.301671533405767,1.84682053794165,6.46400037606323));
#31557=CARTESIAN_POINT('Ctrl Pts',(0.314521852419824,1.86296463159717,6.46504433871078));
#31558=CARTESIAN_POINT('Ctrl Pts',(0.326049054369466,1.8800524968435,6.46608830135834));
#31559=CARTESIAN_POINT('Ctrl Pts',(0.337555050788995,1.8971089271204,6.46713034352411));
#31560=CARTESIAN_POINT('Ctrl Pts',(0.347742305442243,1.91510511294071,6.46817238568987));
#31561=CARTESIAN_POINT('Ctrl Pts',(0.356463062279352,1.93381042382139,6.46921442785564));
#31562=CARTESIAN_POINT('Ctrl Pts',(0.365174453160618,1.95249564549204,6.4702553508845));
#31563=CARTESIAN_POINT('Ctrl Pts',(0.372422137428226,1.97188782902399,6.47129627391335));
#31564=CARTESIAN_POINT('Ctrl Pts',(0.378104441765347,1.99173217875419,6.4723371969422));
#31565=CARTESIAN_POINT('Ctrl Pts',(0.383789664385877,2.01158672002519,6.47337865456199));
#31566=CARTESIAN_POINT('Ctrl Pts',(0.387907682943764,2.03189318850659,6.47442011218178));
#31567=CARTESIAN_POINT('Ctrl Pts',(0.390406677683765,2.05238155798512,6.47546156980157));
#31568=CARTESIAN_POINT('Ctrl Pts',(0.392906435975606,2.07287618755374,6.47650334563207));
#31569=CARTESIAN_POINT('Ctrl Pts',(0.393786132559946,2.09355209463284,6.47754512146257));
#31570=CARTESIAN_POINT('Ctrl Pts',(0.393045915811025,2.11413499431456,6.47858689729306));
#31571=CARTESIAN_POINT('Ctrl Pts',(0.392304099066804,2.13476238440103,6.47963092494566));
#31572=CARTESIAN_POINT('Ctrl Pts',(0.389935462854378,2.15529563410243,6.48067495259825));
#31573=CARTESIAN_POINT('Ctrl Pts',(0.385991993126678,2.17546569579679,6.48171898025085));
#31574=CARTESIAN_POINT('Ctrl Pts',(0.384597239573994,2.18259958223403,6.48208823914672));
#31575=CARTESIAN_POINT('Ctrl Pts',(0.383005946038878,2.18968815183762,6.48245749804259));
#31576=CARTESIAN_POINT('Ctrl Pts',(0.381221900545541,2.19671996972935,6.48282675693847));
#31577=CARTESIAN_POINT('Ctrl Pts',(0.376178076612252,2.21660020905579,6.48387071958602));
#31578=CARTESIAN_POINT('Ctrl Pts',(0.369559943489457,2.2361440769609,6.48491468223358));
#31579=CARTESIAN_POINT('Ctrl Pts',(0.361432043141268,2.25508632496364,6.48595864488113));
#31580=CARTESIAN_POINT('Ctrl Pts',(0.3533190949416,2.27399372666004,6.4870006870469));
#31581=CARTESIAN_POINT('Ctrl Pts',(0.343702124709039,2.29230101332403,6.48804272921268));
#31582=CARTESIAN_POINT('Ctrl Pts',(0.332695067663452,2.30975910457573,6.48908477137845));
#31583=CARTESIAN_POINT('Ctrl Pts',(0.321699832024213,2.32719844611168,6.4901256944073));
#31584=CARTESIAN_POINT('Ctrl Pts',(0.309317839356789,2.34378976814962,6.49116661743616));
#31585=CARTESIAN_POINT('Ctrl Pts',(0.295708288813132,2.35930965644806,6.49220754046502));
#31586=CARTESIAN_POINT('Ctrl Pts',(0.282091748759025,2.37483751535663,6.49324899808481));
#31587=CARTESIAN_POINT('Ctrl Pts',(0.267246864338255,2.38929227739429,6.4942904557046));
#31588=CARTESIAN_POINT('Ctrl Pts',(0.251372627455732,2.40248420151473,6.4953319133244));
#31589=CARTESIAN_POINT('Ctrl Pts',(0.235493540301784,2.41568015634311,6.4963736891549));
#31590=CARTESIAN_POINT('Ctrl Pts',(0.218585063096429,2.4276120630735,6.4974154649854));
#31591=CARTESIAN_POINT('Ctrl Pts',(0.200877899818762,2.43813157108499,6.4984572408159));
#31592=CARTESIAN_POINT('Ctrl Pts',(0.183132462105845,2.44867381725176,6.49950126846849));
#31593=CARTESIAN_POINT('Ctrl Pts',(0.164585552541311,2.45779724459101,6.50054529612109));
#31594=CARTESIAN_POINT('Ctrl Pts',(0.145491532118493,2.46539992348359,6.50158932377369));
#31595=CARTESIAN_POINT('Ctrl Pts',(0.138738227374833,2.46808889135378,6.50195858266955));
#31596=CARTESIAN_POINT('Ctrl Pts',(0.131916635192529,2.47058807406696,6.50232784156541));
#31597=CARTESIAN_POINT('Ctrl Pts',(0.125038420747888,2.47289446675551,6.50269710046126));
#31598=CARTESIAN_POINT('Ctrl Pts',(0.105592446547591,2.47941506204636,6.50374106310882));
#31599=CARTESIAN_POINT('Ctrl Pts',(0.0855770974506221,2.48442986605543,
6.50478502575637));
#31600=CARTESIAN_POINT('Ctrl Pts',(0.0652503368603409,2.4878495630262,6.50582898840393));
#31601=CARTESIAN_POINT('Ctrl Pts',(0.0449609695365006,2.4912629690959,6.5068710305697));
#31602=CARTESIAN_POINT('Ctrl Pts',(0.0243620353742315,2.49308691340133,
6.50791307273547));
#31603=CARTESIAN_POINT('Ctrl Pts',(0.00372464080977932,2.49328236300505,
6.50895511490124));
#31604=CARTESIAN_POINT('Ctrl Pts',(-0.0168905895171121,2.49347760269898,
6.50999603793009));
#31605=CARTESIAN_POINT('Ctrl Pts',(-0.0375434665032679,2.49204778397756,
6.51103696095895));
#31606=CARTESIAN_POINT('Ctrl Pts',(-0.0579599620768663,2.48900582617237,
6.5120778839878));
#31607=CARTESIAN_POINT('Ctrl Pts',(-0.0783869430304766,2.48596230609694,
6.51311934160759));
#31608=CARTESIAN_POINT('Ctrl Pts',(-0.0985765699223359,2.48130508535941,
6.51416079922739));
#31609=CARTESIAN_POINT('Ctrl Pts',(-0.11826158716983,2.4750987696595,6.51520225684718));
#31610=CARTESIAN_POINT('Ctrl Pts',(-0.137952619048288,2.46889055765958,
6.51624403267768));
#31611=CARTESIAN_POINT('Ctrl Pts',(-0.157138044088684,2.4611325639985,6.51728580850818));
#31612=CARTESIAN_POINT('Ctrl Pts',(-0.175568242200381,2.45193846384087,
6.51832758433868));
#31613=CARTESIAN_POINT('Ctrl Pts',(-0.19403827760353,2.4427244904271,6.51937161199128));
#31614=CARTESIAN_POINT('Ctrl Pts',(-0.211749195928382,2.43206859286288,
6.52041563964387));
#31615=CARTESIAN_POINT('Ctrl Pts',(-0.228477602724462,2.42012946608096,
6.52145966729647));
#31616=CARTESIAN_POINT('Ctrl Pts',(-0.234394220936296,2.41590675343341,
6.52182892619233));
#31617=CARTESIAN_POINT('Ctrl Pts',(-0.24018822961454,2.4115238893501,6.52219818508819));
#31618=CARTESIAN_POINT('Ctrl Pts',(-0.245850787641983,2.406989055531,6.52256744398405));
#31619=CARTESIAN_POINT('Ctrl Pts',(-0.261656045743758,2.39433148652912,
6.52359811459743));
#31620=CARTESIAN_POINT('Ctrl Pts',(-0.276534058619568,2.38040754097505,
6.52462878521081));
#31621=CARTESIAN_POINT('Ctrl Pts',(-0.290272920650004,2.36537995692463,
6.52565945582419));
#31622=CARTESIAN_POINT('Ctrl Pts',(-0.30398645661347,2.35038007455716,6.52668822651071));
#31623=CARTESIAN_POINT('Ctrl Pts',(-0.316564456390915,2.33428109815806,
6.52771699719724));
#31624=CARTESIAN_POINT('Ctrl Pts',(-0.327829832865636,2.31728435443743,
6.52874576788376));
#31625=CARTESIAN_POINT('Ctrl Pts',(-0.339091623489328,2.30029302090358,
6.52977421110511));
#31626=CARTESIAN_POINT('Ctrl Pts',(-0.349041161188116,2.28240508741081,
6.53080265432646));
#31627=CARTESIAN_POINT('Ctrl Pts',(-0.35754306959627,2.26385311526998,6.53183109754781));
#31628=CARTESIAN_POINT('Ctrl Pts',(-0.366042502827262,2.24530654420094,
6.53285924135648));
#31629=CARTESIAN_POINT('Ctrl Pts',(-0.373094836165821,2.22609700970157,
6.53388738516516));
#31630=CARTESIAN_POINT('Ctrl Pts',(-0.378612195223621,2.20647861582473,
6.53491552897383));
#31631=CARTESIAN_POINT('Ctrl Pts',(-0.384140211372701,2.1868223279098,6.53594565870046));
#31632=CARTESIAN_POINT('Ctrl Pts',(-0.388127154582712,2.16675634147602,
6.53697578842708));
#31633=CARTESIAN_POINT('Ctrl Pts',(-0.390535836004804,2.14654729633425,
6.53800591815371));
#31634=CARTESIAN_POINT('Ctrl Pts',(-0.392389063178822,2.1309985603021,6.5387984946998));
#31635=CARTESIAN_POINT('Ctrl Pts',(-0.393309066661416,2.11536545937624,
6.53959107124589));
#31636=CARTESIAN_POINT('Ctrl Pts',(-0.393299932545456,2.09976965300128,
6.54038364779198));
#31637=CARTESIAN_POINT('',(-0.39331152360305,2.10034122134638,6.66538365352491));
#31638=CARTESIAN_POINT('Ctrl Pts',(-0.393299932545403,2.09976965291168,
6.54038364779653));
#31639=CARTESIAN_POINT('Ctrl Pts',(-0.393292041506276,2.08629631066401,
6.5410683610333));
#31640=CARTESIAN_POINT('Ctrl Pts',(-0.392591866303222,2.07284347841698,
6.54175307427007));
#31641=CARTESIAN_POINT('Ctrl Pts',(-0.391205367932869,2.05946297864287,
6.54243778750684));
#31642=CARTESIAN_POINT('Ctrl Pts',(-0.389091413606023,2.0390621141358,6.54348175015438));
#31643=CARTESIAN_POINT('Ctrl Pts',(-0.385371045251637,2.01876626928969,
6.54452571280192));
#31644=CARTESIAN_POINT('Ctrl Pts',(-0.380069742571046,1.998847240364,6.54556967544945));
#31645=CARTESIAN_POINT('Ctrl Pts',(-0.374778192207985,1.97896485463841,
6.54661171761521));
#31646=CARTESIAN_POINT('Ctrl Pts',(-0.367911610004776,1.95945862716396,
6.54765375978097));
#31647=CARTESIAN_POINT('Ctrl Pts',(-0.359546688657205,1.94059150375329,
6.54869580194672));
#31648=CARTESIAN_POINT('Ctrl Pts',(-0.351190751103754,1.92174464333676,
6.54973672497556));
#31649=CARTESIAN_POINT('Ctrl Pts',(-0.341339939305365,1.90353620528506,
6.5507776480044));
#31650=CARTESIAN_POINT('Ctrl Pts',(-0.330119447510008,1.88621028935964,
6.55181857103324));
#31651=CARTESIAN_POINT('Ctrl Pts',(-0.318893193162514,1.86887547529539,
6.55286002865302));
#31652=CARTESIAN_POINT('Ctrl Pts',(-0.306296239941186,1.85242471517439,
6.5539014862728));
#31653=CARTESIAN_POINT('Ctrl Pts',(-0.292498028718581,1.83707454821615,
6.55494294389258));
#31654=CARTESIAN_POINT('Ctrl Pts',(-0.278695601540899,1.82171969111268,
6.55598471972306));
#31655=CARTESIAN_POINT('Ctrl Pts',(-0.263691704047982,1.80746661917585,
6.55702649555355));
#31656=CARTESIAN_POINT('Ctrl Pts',(-0.24769314483582,1.79449550575918,6.55806827138403));
#31657=CARTESIAN_POINT('Ctrl Pts',(-0.231660004374866,1.7814963549865,6.55911229903662));
#31658=CARTESIAN_POINT('Ctrl Pts',(-0.214628516710658,1.76978511215146,
6.5601563266892));
#31659=CARTESIAN_POINT('Ctrl Pts',(-0.196835615836783,1.75949944150097,
6.56120035434178));
#31660=CARTESIAN_POINT('Ctrl Pts',(-0.190542500021145,1.75586153461305,
6.56156961323773));
#31661=CARTESIAN_POINT('Ctrl Pts',(-0.184154352532472,1.75240153377129,
6.56193887213368));
#31662=CARTESIAN_POINT('Ctrl Pts',(-0.177682280947023,1.74912410023277,
6.56230813102963));
#31663=CARTESIAN_POINT('Ctrl Pts',(-0.159384547130388,1.73985819430176,
6.56335209367719));
#31664=CARTESIAN_POINT('Ctrl Pts',(-0.140305534785827,1.73199983908709,
6.56439605632475));
#31665=CARTESIAN_POINT('Ctrl Pts',(-0.120687567697363,1.72567473902595,
6.5654400189723));
#31666=CARTESIAN_POINT('Ctrl Pts',(-0.101105689973313,1.71936127466793,
6.56648206113807));
#31667=CARTESIAN_POINT('Ctrl Pts',(-0.0809874996476068,1.71457574653924,
6.56752410330385));
#31668=CARTESIAN_POINT('Ctrl Pts',(-0.0605956014093857,1.71139600736761,
6.56856614546962));
#31669=CARTESIAN_POINT('Ctrl Pts',(-0.0402256037495277,1.7082196831859,
6.56960706849847));
#31670=CARTESIAN_POINT('Ctrl Pts',(-0.0195832006051351,1.70664586559583,
6.57064799152733));
#31671=CARTESIAN_POINT('Ctrl Pts',(0.00105859466534771,1.70670142464365,
6.57168891455618));
#31672=CARTESIAN_POINT('Ctrl Pts',(0.021710991023893,1.70675701222515,6.57273037217598));
#31673=CARTESIAN_POINT('Ctrl Pts',(0.0423620430658482,1.70844366233467,
6.57377182979577));
#31674=CARTESIAN_POINT('Ctrl Pts',(0.0627379593325417,1.71173612264494,
6.57481328741556));
#31675=CARTESIAN_POINT('Ctrl Pts',(0.083120101329971,1.71502958894537,6.57585506324606));
#31676=CARTESIAN_POINT('Ctrl Pts',(0.103226220223315,1.71992968921717,6.57689683907656));
#31677=CARTESIAN_POINT('Ctrl Pts',(0.122792873801231,1.72636006618185,6.57793861490706));
#31678=CARTESIAN_POINT('Ctrl Pts',(0.142401821144877,1.73280434255225,6.57898264255966));
#31679=CARTESIAN_POINT('Ctrl Pts',(0.161468295815427,1.74078521496365,6.58002667021226));
#31680=CARTESIAN_POINT('Ctrl Pts',(0.17974829059745,1.75017798521635,6.58107069786486));
#31681=CARTESIAN_POINT('Ctrl Pts',(0.186213685141952,1.75350008493649,6.58143995676071));
#31682=CARTESIAN_POINT('Ctrl Pts',(0.192580935459323,1.75699839274605,6.58180921565656));
#31683=CARTESIAN_POINT('Ctrl Pts',(0.198840109549427,1.76066609241873,6.58217847455242));
#31684=CARTESIAN_POINT('Ctrl Pts',(0.216535943090567,1.77103535231666,6.58322243719997));
#31685=CARTESIAN_POINT('Ctrl Pts',(0.233471202972059,1.78282345782475,6.58426639984752));
#31686=CARTESIAN_POINT('Ctrl Pts',(0.249409020409639,1.79589470484994,6.58531036249508));
#31687=CARTESIAN_POINT('Ctrl Pts',(0.265317518514646,1.80894190590772,6.58635240466085));
#31688=CARTESIAN_POINT('Ctrl Pts',(0.28023161618312,1.8232671476923,6.58739444682662));
#31689=CARTESIAN_POINT('Ctrl Pts',(0.293943700784461,1.83869177056752,6.58843648899239));
#31690=CARTESIAN_POINT('Ctrl Pts',(0.307641058822351,1.85409982764009,6.58947741202125));
#31691=CARTESIAN_POINT('Ctrl Pts',(0.320138458636934,1.87060439389482,6.5905183350501));
#31692=CARTESIAN_POINT('Ctrl Pts',(0.331265520348259,1.88799046005333,6.59155925807896));
#31693=CARTESIAN_POINT('Ctrl Pts',(0.342398296628475,1.9053854552423,6.59260071569875));
#31694=CARTESIAN_POINT('Ctrl Pts',(0.352158918629106,1.92366224372364,6.59364217331854));
#31695=CARTESIAN_POINT('Ctrl Pts',(0.360420410695364,1.94257694719583,6.59468363093834));
#31696=CARTESIAN_POINT('Ctrl Pts',(0.368684427007619,1.96149742993454,6.59572540676884));
#31697=CARTESIAN_POINT('Ctrl Pts',(0.375448140417293,1.98105552750404,6.59676718259934));
#31698=CARTESIAN_POINT('Ctrl Pts',(0.380633147462184,2.00098839940173,6.59780895842984));
#31699=CARTESIAN_POINT('Ctrl Pts',(0.385829362017467,2.02096435665437,6.59885298608243));
#31700=CARTESIAN_POINT('Ctrl Pts',(0.389439928849869,2.04131598037234,6.59989701373503));
#31701=CARTESIAN_POINT('Ctrl Pts',(0.391437610923698,2.06177060353148,6.60094104138763));
#31702=CARTESIAN_POINT('Ctrl Pts',(0.392144164888067,2.06900513562849,6.60131030028349));
#31703=CARTESIAN_POINT('Ctrl Pts',(0.39264943269245,2.07625253092481,6.60167955917935));
#31704=CARTESIAN_POINT('Ctrl Pts',(0.392953769170832,2.08350074867042,6.6020488180752));
#31705=CARTESIAN_POINT('Ctrl Pts',(0.393814184232686,2.10399279008812,6.60309278072275));
#31706=CARTESIAN_POINT('Ctrl Pts',(0.393069896237303,2.1246133743209,6.60413674337031));
#31707=CARTESIAN_POINT('Ctrl Pts',(0.390706786262966,2.14508987877634,6.60518070601786));
#31708=CARTESIAN_POINT('Ctrl Pts',(0.388348023484066,2.16552871449537,6.60622274818363));
#31709=CARTESIAN_POINT('Ctrl Pts',(0.384376374255578,2.18582326706139,6.6072647903494));
#31710=CARTESIAN_POINT('Ctrl Pts',(0.378829674330109,2.20570226036819,6.60830683251517));
#31711=CARTESIAN_POINT('Ctrl Pts',(0.373288931473224,2.22555990394846,6.60934775554402));
#31712=CARTESIAN_POINT('Ctrl Pts',(0.366176664995522,2.24500216140303,6.61038867857287));
#31713=CARTESIAN_POINT('Ctrl Pts',(0.357581428840274,2.26376938587095,6.61142960160173));
#31714=CARTESIAN_POINT('Ctrl Pts',(0.348981778395756,2.28254624869622,6.61247105922152));
#31715=CARTESIAN_POINT('Ctrl Pts',(0.338897928458248,2.30064671027781,6.6135125168413));
#31716=CARTESIAN_POINT('Ctrl Pts',(0.327466202053937,2.31783199148052,6.6145539744611));
#31717=CARTESIAN_POINT('Ctrl Pts',(0.316030982758827,2.33502252353586,6.61559575029159));
#31718=CARTESIAN_POINT('Ctrl Pts',(0.303247504427968,2.35129672647759,6.61663752612209));
#31719=CARTESIAN_POINT('Ctrl Pts',(0.289294326851198,2.36644639695765,6.61767930195259));
#31720=CARTESIAN_POINT('Ctrl Pts',(0.275310989164459,2.38162881379424,6.61872332960518));
#31721=CARTESIAN_POINT('Ctrl Pts',(0.260153444624358,2.39568134468094,6.61976735725778));
#31722=CARTESIAN_POINT('Ctrl Pts',(0.244036212647197,2.40843348864352,6.62081138491038));
#31723=CARTESIAN_POINT('Ctrl Pts',(0.238335758957439,2.41294375481123,6.62118064380625));
#31724=CARTESIAN_POINT('Ctrl Pts',(0.232515529823981,2.41729173905392,6.62154990270212));
#31725=CARTESIAN_POINT('Ctrl Pts',(0.226585841403053,2.42147122184679,6.621919161598));
#31726=CARTESIAN_POINT('Ctrl Pts',(0.209821524301329,2.43328738652312,6.62296312424555));
#31727=CARTESIAN_POINT('Ctrl Pts',(0.192080471339188,2.44382387068611,6.62400708689311));
#31728=CARTESIAN_POINT('Ctrl Pts',(0.17358426564602,2.45292122735836,6.62505104954066));
#31729=CARTESIAN_POINT('Ctrl Pts',(0.155122085716303,2.46200184846271,6.62609309170643));
#31730=CARTESIAN_POINT('Ctrl Pts',(0.135908137066768,2.46964822268475,6.6271351338722));
#31731=CARTESIAN_POINT('Ctrl Pts',(0.116190994681086,2.47574531634475,6.62817717603797));
#31732=CARTESIAN_POINT('Ctrl Pts',(0.0964950281965777,2.48183586182195,
6.62921809906682));
#31733=CARTESIAN_POINT('Ctrl Pts',(0.0762976316722112,2.4863801860862,6.63025902209567));
#31734=CARTESIAN_POINT('Ctrl Pts',(0.0558650566870586,2.48931219534116,
6.63129994512453));
#31735=CARTESIAN_POINT('Ctrl Pts',(0.0354219880639309,2.49224571039965,
6.63234140274432));
#31736=CARTESIAN_POINT('Ctrl Pts',(0.0147442257137023,2.49356513573576,
6.63338286036411));
#31737=CARTESIAN_POINT('Ctrl Pts',(-0.0058936664742866,2.49325583873032,
6.6344243179839));
#31738=CARTESIAN_POINT('Ctrl Pts',(-0.0265378644380765,2.49294644722117,
6.6354660938144));
#31739=CARTESIAN_POINT('Ctrl Pts',(-0.0471414334543857,2.4910073898688,
6.6365078696449));
#31740=CARTESIAN_POINT('Ctrl Pts',(-0.0674326547797886,2.4874760987072,
6.6375496454754));
#31741=CARTESIAN_POINT('Ctrl Pts',(-0.0877677360405539,2.48393717457962,
6.63859367312799));
#31742=CARTESIAN_POINT('Ctrl Pts',(-0.107788408351039,2.47879932862586,
6.63963770078059));
#31743=CARTESIAN_POINT('Ctrl Pts',(-0.12723518820322,2.47215063735387,6.64068172843319));
#31744=CARTESIAN_POINT('Ctrl Pts',(-0.134113259333297,2.46979908240039,
6.64105098732905));
#31745=CARTESIAN_POINT('Ctrl Pts',(-0.140919717527131,2.46725897197108,
6.64142024622492));
#31746=CARTESIAN_POINT('Ctrl Pts',(-0.14764374897517,2.46453561333367,6.64178950512078));
#31747=CARTESIAN_POINT('Ctrl Pts',(-0.166653819555366,2.4568361788036,6.64283346776834));
#31748=CARTESIAN_POINT('Ctrl Pts',(-0.185116636617798,2.44762277309,6.64387743041589));
#31749=CARTESIAN_POINT('Ctrl Pts',(-0.202778187337366,2.43699539572548,
6.64492139306345));
#31750=CARTESIAN_POINT('Ctrl Pts',(-0.220407247731244,2.42638756856678,
6.64596343522922));
#31751=CARTESIAN_POINT('Ctrl Pts',(-0.2372373136588,2.41437125705591,6.64700547739499));
#31752=CARTESIAN_POINT('Ctrl Pts',(-0.253037104612386,2.40109319768035,
6.64804751956077));
#31753=CARTESIAN_POINT('Ctrl Pts',(-0.268819926838699,2.38782939873197,
6.64908844258962));
#31754=CARTESIAN_POINT('Ctrl Pts',(-0.283574091725867,2.37330699094726,
6.65012936561848));
#31755=CARTESIAN_POINT('Ctrl Pts',(-0.297099899635937,2.35771406565478,
6.65117028864734));
#31756=CARTESIAN_POINT('Ctrl Pts',(-0.31063265404842,2.34211313224227,6.65221174626713));
#31757=CARTESIAN_POINT('Ctrl Pts',(-0.322935296878158,2.32544112821049,
6.65325320388693));
#31758=CARTESIAN_POINT('Ctrl Pts',(-0.333846898362626,2.30792099089235,
6.65429466150672));
#31759=CARTESIAN_POINT('Ctrl Pts',(-0.344761833817051,2.29039550040844,
6.65533643733722));
#31760=CARTESIAN_POINT('Ctrl Pts',(-0.354284523868938,2.27202200390388,
6.65637821316772));
#31761=CARTESIAN_POINT('Ctrl Pts',(-0.362299355777202,2.25304922999945,
6.65741998899822));
#31762=CARTESIAN_POINT('Ctrl Pts',(-0.370331511926516,2.23403544601368,
6.65846401665082));
#31763=CARTESIAN_POINT('Ctrl Pts',(-0.376849070730866,2.2144204974274,6.65950804430342));
#31764=CARTESIAN_POINT('Ctrl Pts',(-0.381785625383631,2.19447024002526,
6.66055207195602));
#31765=CARTESIAN_POINT('Ctrl Pts',(-0.383531620057107,2.18741409548544,
6.66092133085188));
#31766=CARTESIAN_POINT('Ctrl Pts',(-0.385080308534198,2.18031609589856,
6.66129058974773));
#31767=CARTESIAN_POINT('Ctrl Pts',(-0.386430299550126,2.17318820662921,
6.66165984864358));
#31768=CARTESIAN_POINT('Ctrl Pts',(-0.390968303877209,2.14922775654797,
6.6629011150279));
#31769=CARTESIAN_POINT('Ctrl Pts',(-0.393278597173609,2.1248326289864,6.66414238141221));
#31770=CARTESIAN_POINT('Ctrl Pts',(-0.393299851891308,2.10034132429566,
6.66538364779653));
#31771=CARTESIAN_POINT('',(-0.393058384114589,2.10004747884629,6.79038363519587));
#31772=CARTESIAN_POINT('Ctrl Pts',(-0.393482223946032,2.10033971569951,
6.66538373730318));
#31773=CARTESIAN_POINT('Ctrl Pts',(-0.392510478521912,1.99409483509794,
6.67076588892424));
#31774=CARTESIAN_POINT('Ctrl Pts',(-0.29321797659763,1.75550278257759,6.68277148838622));
#31775=CARTESIAN_POINT('Ctrl Pts',(0.110368293424312,1.64823249309944,6.70140053568915));
#31776=CARTESIAN_POINT('Ctrl Pts',(0.439598559880011,1.94824972278144,6.72127087921195));
#31777=CARTESIAN_POINT('Ctrl Pts',(0.365556993585621,2.38747717287657,6.74114122273472));
#31778=CARTESIAN_POINT('Ctrl Pts',(-0.0438333482327071,2.56298345334063,
6.76101156625752));
#31779=CARTESIAN_POINT('Ctrl Pts',(-0.348798170201786,2.35711399190874,
6.77742569677967));
#31780=CARTESIAN_POINT('Ctrl Pts',(-0.392724778002082,2.16290283319788,
6.7872163794609));
#31781=CARTESIAN_POINT('Ctrl Pts',(-0.392657736298662,2.10004784536838,
6.7903836143012));
#31782=CARTESIAN_POINT('',(-0.393299834087712,2.0996387430578,6.91538364779653));
#31783=CARTESIAN_POINT('Ctrl Pts',(-0.393299997160818,2.10004725781296,
6.79038364779653));
#31784=CARTESIAN_POINT('Ctrl Pts',(-0.393302581849858,2.07853635562221,
6.79146580267118));
#31785=CARTESIAN_POINT('Ctrl Pts',(-0.391536095407621,2.05705308860708,
6.79254795754583));
#31786=CARTESIAN_POINT('Ctrl Pts',(-0.388039837948008,2.03589091979069,
6.79363011242049));
#31787=CARTESIAN_POINT('Ctrl Pts',(-0.384537910187648,2.0146944297428,6.7947140223557));
#31788=CARTESIAN_POINT('Ctrl Pts',(-0.379300790769184,1.99382070473038,
6.79579793229092));
#31789=CARTESIAN_POINT('Ctrl Pts',(-0.372418383116233,1.97355065078423,
6.79688184222614));
#31790=CARTESIAN_POINT('Ctrl Pts',(-0.365513477736801,1.95321433657679,
6.79796929532684));
#31791=CARTESIAN_POINT('Ctrl Pts',(-0.356952812209818,1.9334862275484,6.79905674842755));
#31792=CARTESIAN_POINT('Ctrl Pts',(-0.346874149351669,1.91462682364604,
6.80014420152825));
#31793=CARTESIAN_POINT('Ctrl Pts',(-0.344995647239727,1.91111173136057,
6.8003468854532));
#31794=CARTESIAN_POINT('Ctrl Pts',(-0.343064534298844,1.90762673863315,
6.80054956937815));
#31795=CARTESIAN_POINT('Ctrl Pts',(-0.341081867415064,1.90417341926936,
6.80075225330309));
#31796=CARTESIAN_POINT('Ctrl Pts',(-0.330869759228678,1.8863864318366,6.80179621595065));
#31797=CARTESIAN_POINT('Ctrl Pts',(-0.319232124137762,1.86934742047409,
6.8028401785982));
#31798=CARTESIAN_POINT('Ctrl Pts',(-0.306302562791849,1.85329444670388,
6.80388414124575));
#31799=CARTESIAN_POINT('Ctrl Pts',(-0.293396786767268,1.83727100410872,
6.80492618341152));
#31800=CARTESIAN_POINT('Ctrl Pts',(-0.27920421202316,1.82223060239925,6.80596822557729));
#31801=CARTESIAN_POINT('Ctrl Pts',(-0.263901652210097,1.8083824285802,6.80701026774306));
#31802=CARTESIAN_POINT('Ctrl Pts',(-0.248615527105874,1.79454912748228,
6.80805119077191));
#31803=CARTESIAN_POINT('Ctrl Pts',(-0.232222306929764,1.78190602495015,
6.80909211380076));
#31804=CARTESIAN_POINT('Ctrl Pts',(-0.214935483346197,1.77062539867389,
6.81013303682962));
#31805=CARTESIAN_POINT('Ctrl Pts',(-0.197639781700593,1.75933897896198,
6.81117449444941));
#31806=CARTESIAN_POINT('Ctrl Pts',(-0.179450167183249,1.74941684901224,
6.8122159520692));
#31807=CARTESIAN_POINT('Ctrl Pts',(-0.160609383812146,1.74098813970638,
6.81325740968899));
#31808=CARTESIAN_POINT('Ctrl Pts',(-0.141762843760332,1.73255685506237,
6.81429918551949));
#31809=CARTESIAN_POINT('Ctrl Pts',(-0.122265424613192,1.72562016664315,
6.81534096134999));
#31810=CARTESIAN_POINT('Ctrl Pts',(-0.102379262085259,1.72025880300542,
6.81638273718049));
#31811=CARTESIAN_POINT('Ctrl Pts',(-0.082450115165751,1.71488585065851,
6.81742676483308));
#31812=CARTESIAN_POINT('Ctrl Pts',(-0.0621312712786171,1.71109515627656,
6.81847079248568));
#31813=CARTESIAN_POINT('Ctrl Pts',(-0.0416951454928683,1.70891637103769,
6.81951482013828));
#31814=CARTESIAN_POINT('Ctrl Pts',(-0.034467155674026,1.70814576325767,
6.81988407903415));
#31815=CARTESIAN_POINT('Ctrl Pts',(-0.0272245202219977,1.70757631980235,
6.82025333793002));
#31816=CARTESIAN_POINT('Ctrl Pts',(-0.0199792825574456,1.70720779250539,
6.82062259682589));
#31817=CARTESIAN_POINT('Ctrl Pts',(0.000504333623478286,1.70616589822218,
6.82166655947345));
#31818=CARTESIAN_POINT('Ctrl Pts',(0.0211307016035394,1.70672750544539,
6.822710522121));
#31819=CARTESIAN_POINT('Ctrl Pts',(0.0416273345470524,1.70890914736022,
6.82375448476855));
#31820=CARTESIAN_POINT('Ctrl Pts',(0.0620862617256241,1.71108677590967,
6.82479652693432));
#31821=CARTESIAN_POINT('Ctrl Pts',(0.0824151979246268,1.71487850565568,
6.82583856910009));
#31822=CARTESIAN_POINT('Ctrl Pts',(0.102342542541241,1.72024890522055,6.82688061126586));
#31823=CARTESIAN_POINT('Ctrl Pts',(0.122248485502793,1.72561353706064,6.82792153429472));
#31824=CARTESIAN_POINT('Ctrl Pts',(0.1417529787668,1.73255331024823,6.82896245732357));
#31825=CARTESIAN_POINT('Ctrl Pts',(0.160595601271428,1.74098197419591,6.83000338035242));
#31826=CARTESIAN_POINT('Ctrl Pts',(0.179447900855871,1.74941496688571,6.83104483797221));
#31827=CARTESIAN_POINT('Ctrl Pts',(0.197636972370958,1.75933809222245,6.832086295592));
#31828=CARTESIAN_POINT('Ctrl Pts',(0.214922838536312,1.77061714756913,6.83312775321179));
#31829=CARTESIAN_POINT('Ctrl Pts',(0.232213986287385,1.78189964915895,6.83416952904229));
#31830=CARTESIAN_POINT('Ctrl Pts',(0.248600783387758,1.79453847348784,6.83521130487279));
#31831=CARTESIAN_POINT('Ctrl Pts',(0.263873453022812,1.80835691198004,6.83625308070329));
#31832=CARTESIAN_POINT('Ctrl Pts',(0.279179134879864,1.82220521934062,6.83729710835588));
#31833=CARTESIAN_POINT('Ctrl Pts',(0.293365375920581,1.83723769571488,6.83834113600848));
#31834=CARTESIAN_POINT('Ctrl Pts',(0.306259781704422,1.85324134035386,6.83938516366108));
#31835=CARTESIAN_POINT('Ctrl Pts',(0.310820364013487,1.85890161969085,6.83975442255694));
#31836=CARTESIAN_POINT('Ctrl Pts',(0.315219731702494,1.86468310722222,6.84012368145281));
#31837=CARTESIAN_POINT('Ctrl Pts',(0.31945157411294,1.8705755422873,6.84049294034868));
#31838=CARTESIAN_POINT('Ctrl Pts',(0.331415769034932,1.88723453731743,6.84153690299623));
#31839=CARTESIAN_POINT('Ctrl Pts',(0.342108985308859,1.904881564955,6.84258086564378));
#31840=CARTESIAN_POINT('Ctrl Pts',(0.351369819488892,1.92329646310177,6.84362482829134));
#31841=CARTESIAN_POINT('Ctrl Pts',(0.360613617366539,1.94167748505908,6.84466687045711));
#31842=CARTESIAN_POINT('Ctrl Pts',(0.368429883592596,1.96082295041602,6.84570891262288));
#31843=CARTESIAN_POINT('Ctrl Pts',(0.374701387190005,1.98048531287793,6.84675095478865));
#31844=CARTESIAN_POINT('Ctrl Pts',(0.380966155291075,2.00012655827145,6.8477918778175));
#31845=CARTESIAN_POINT('Ctrl Pts',(0.385689204370225,2.02028291004397,6.84883280084636));
#31846=CARTESIAN_POINT('Ctrl Pts',(0.388802084839317,2.04068871250259,6.84987372387521));
#31847=CARTESIAN_POINT('Ctrl Pts',(0.391916564002687,2.06110499484952,6.850915181495));
#31848=CARTESIAN_POINT('Ctrl Pts',(0.393419095618887,2.08177025888781,6.8519566391148));
#31849=CARTESIAN_POINT('Ctrl Pts',(0.393292615629937,2.1024100811112,6.85299809673459));
#31850=CARTESIAN_POINT('Ctrl Pts',(0.393166096995836,2.1230562097001,6.85403987256509));
#31851=CARTESIAN_POINT('Ctrl Pts',(0.3914096165708,2.1436761460759,6.85508164839559));
#31852=CARTESIAN_POINT('Ctrl Pts',(0.388058198109005,2.16399785059197,6.85612342422609));
#31853=CARTESIAN_POINT('Ctrl Pts',(0.384699535480151,2.18436348093351,6.85716745187868));
#31854=CARTESIAN_POINT('Ctrl Pts',(0.379739228801881,2.20442887747746,6.85821147953128));
#31855=CARTESIAN_POINT('Ctrl Pts',(0.373263052691939,2.22393378673749,6.85925550718388));
#31856=CARTESIAN_POINT('Ctrl Pts',(0.370972514089987,2.23083241747718,6.85962476607974));
#31857=CARTESIAN_POINT('Ctrl Pts',(0.368492793081253,2.23766110826359,6.85999402497561));
#31858=CARTESIAN_POINT('Ctrl Pts',(0.365829100939446,2.24440899870104,6.86036328387147));
#31859=CARTESIAN_POINT('Ctrl Pts',(0.358298354539635,2.26348652302173,6.86140724651902));
#31860=CARTESIAN_POINT('Ctrl Pts',(0.349248848926038,2.28203022564207,6.86245120916658));
#31861=CARTESIAN_POINT('Ctrl Pts',(0.338778329731138,2.29978521793311,6.86349517181413));
#31862=CARTESIAN_POINT('Ctrl Pts',(0.328327072184561,2.31750754800262,6.8645372139799));
#31863=CARTESIAN_POINT('Ctrl Pts',(0.316460308263824,2.33444339092523,6.86557925614567));
#31864=CARTESIAN_POINT('Ctrl Pts',(0.303322720079523,2.35036017551432,6.86662129831144));
#31865=CARTESIAN_POINT('Ctrl Pts',(0.290199241458535,2.36625986572681,6.86766222134029));
#31866=CARTESIAN_POINT('Ctrl Pts',(0.275808091807768,2.38114208737248,6.86870314436915));
#31867=CARTESIAN_POINT('Ctrl Pts',(0.260335586191335,2.39480548258541,6.869744067398));
#31868=CARTESIAN_POINT('Ctrl Pts',(0.244855134299287,2.408475894962,6.87078552501779));
#31869=CARTESIAN_POINT('Ctrl Pts',(0.228292757809945,2.42092573126836,6.87182698263758));
#31870=CARTESIAN_POINT('Ctrl Pts',(0.210869959837856,2.43199209333654,6.87286844025738));
#31871=CARTESIAN_POINT('Ctrl Pts',(0.193441838441429,2.44306183666079,6.87391021608787));
#31872=CARTESIAN_POINT('Ctrl Pts',(0.175153412157756,2.45274690060954,6.87495199191837));
#31873=CARTESIAN_POINT('Ctrl Pts',(0.156252375783406,2.46092947380623,6.87599376774887));
#31874=CARTESIAN_POINT('Ctrl Pts',(0.137310484390003,2.46912973382057,6.87703779540146));
#31875=CARTESIAN_POINT('Ctrl Pts',(0.117754036085296,2.4758207808622,6.87808182305406));
#31876=CARTESIAN_POINT('Ctrl Pts',(0.0978482880106924,2.48093385585082,
6.87912585070666));
#31877=CARTESIAN_POINT('Ctrl Pts',(0.0908078858363308,2.48274228345338,
6.87949510960252));
#31878=CARTESIAN_POINT('Ctrl Pts',(0.0837238825718224,2.48435378334066,
6.87986436849839));
#31879=CARTESIAN_POINT('Ctrl Pts',(0.0766082307889138,2.48576685831651,
6.88023362739426));
#31880=CARTESIAN_POINT('Ctrl Pts',(0.0564909776705838,2.48976188053396,
6.88127759004181));
#31881=CARTESIAN_POINT('Ctrl Pts',(0.0360004395909989,2.49219093548006,
6.88232155268936));
#31882=CARTESIAN_POINT('Ctrl Pts',(0.015403842950015,2.49299823361228,6.88336551533691));
#31883=CARTESIAN_POINT('Ctrl Pts',(-0.00515486403204175,2.4938040466326,
6.88440755750268));
#31884=CARTESIAN_POINT('Ctrl Pts',(-0.0258185177163293,2.49299393684622,
6.88544959966845));
#31885=CARTESIAN_POINT('Ctrl Pts',(-0.0463132490443797,2.49056366057655,
6.88649164183422));
#31886=CARTESIAN_POINT('Ctrl Pts',(-0.0667859693529384,2.48813599438542,
6.88753256486308));
#31887=CARTESIAN_POINT('Ctrl Pts',(-0.087089397107138,2.48409167357587,
6.88857348789193));
#31888=CARTESIAN_POINT('Ctrl Pts',(-0.106953371297437,2.47847835653854,
6.88961441092078));
#31889=CARTESIAN_POINT('Ctrl Pts',(-0.126827547107173,2.47286215664788,
6.89065586854057));
#31890=CARTESIAN_POINT('Ctrl Pts',(-0.146261106037048,2.46567553530339,
6.89169732616036));
#31891=CARTESIAN_POINT('Ctrl Pts',(-0.164997176752652,2.45701655656798,
6.89273878378016));
#31892=CARTESIAN_POINT('Ctrl Pts',(-0.183738972154671,2.44835493213706,
6.89378055961065));
#31893=CARTESIAN_POINT('Ctrl Pts',(-0.201782202926135,2.43822039598821,
6.89482233544115));
#31894=CARTESIAN_POINT('Ctrl Pts',(-0.218893729483336,2.42675744091432,
6.89586411127165));
#31895=CARTESIAN_POINT('Ctrl Pts',(-0.236042242993499,2.41526970840292,
6.89690813892425));
#31896=CARTESIAN_POINT('Ctrl Pts',(-0.252254453975106,2.40244828118534,
6.89795216657684));
#31897=CARTESIAN_POINT('Ctrl Pts',(-0.267328960078824,2.38847897168281,
6.89899619422944));
#31898=CARTESIAN_POINT('Ctrl Pts',(-0.272660615294824,2.38353821001801,
6.89936545312531));
#31899=CARTESIAN_POINT('Ctrl Pts',(-0.277850292219873,2.37845418724543,
6.89973471202117));
#31900=CARTESIAN_POINT('Ctrl Pts',(-0.282890261841573,2.37323614284206,
6.90010397091704));
#31901=CARTESIAN_POINT('Ctrl Pts',(-0.296955634656005,2.35867380508913,
6.9011344858656));
#31902=CARTESIAN_POINT('Ctrl Pts',(-0.309940758242874,2.34297343956352,
6.90216500081415));
#31903=CARTESIAN_POINT('Ctrl Pts',(-0.321656101468961,2.3263233138406,6.90319551576271));
#31904=CARTESIAN_POINT('Ctrl Pts',(-0.333352706677958,2.3096998190353,6.90422438246193));
#31905=CARTESIAN_POINT('Ctrl Pts',(-0.343783071916386,2.2921301483415,6.90525324916115));
#31906=CARTESIAN_POINT('Ctrl Pts',(-0.352796999717656,2.27383661004006,
6.90628211586036));
#31907=CARTESIAN_POINT('Ctrl Pts',(-0.361801511979625,2.2555621803373,6.90730990785219));
#31908=CARTESIAN_POINT('Ctrl Pts',(-0.36939216422126,2.23656604732395,6.90833769984402));
#31909=CARTESIAN_POINT('Ctrl Pts',(-0.375464363780332,2.21709569390473,
6.90936549183584));
#31910=CARTESIAN_POINT('Ctrl Pts',(-0.381542362665326,2.19760674509447,
6.91039426543255));
#31911=CARTESIAN_POINT('Ctrl Pts',(-0.386098772648862,2.1776433911913,6.91142303902926));
#31912=CARTESIAN_POINT('Ctrl Pts',(-0.389078598302285,2.15746942093956,
6.91245181262597));
#31913=CARTESIAN_POINT('Ctrl Pts',(-0.391909268944431,2.13830525767334,
6.91342909101616));
#31914=CARTESIAN_POINT('Ctrl Pts',(-0.393317573582477,2.11895170160064,
6.91440636940634));
#31915=CARTESIAN_POINT('Ctrl Pts',(-0.393299834087712,2.0996387430578,6.91538364779653));
#31916=CARTESIAN_POINT('',(-0.393445913694928,2.10014151066963,7.04038364779653));
#31917=CARTESIAN_POINT('Ctrl Pts',(-0.393308615227651,2.09963873499208,
6.91538364779653));
#31918=CARTESIAN_POINT('Ctrl Pts',(-0.393587780238266,2.06939755311191,
6.91691387001097));
#31919=CARTESIAN_POINT('Ctrl Pts',(-0.376576601026969,1.9085705283121,6.92506754006631));
#31920=CARTESIAN_POINT('Ctrl Pts',(-0.155638169461425,1.66176284880085,
6.93984465796265));
#31921=CARTESIAN_POINT('Ctrl Pts',(0.284227889761795,1.73191095212428,6.95971500148539));
#31922=CARTESIAN_POINT('Ctrl Pts',(0.463353554261716,2.13973064607486,6.97958534500821));
#31923=CARTESIAN_POINT('Ctrl Pts',(0.217415412616838,2.51110288109078,6.999455688531));
#31924=CARTESIAN_POINT('Ctrl Pts',(-0.227971771668255,2.50534418930942,
7.01932603205377));
#31925=CARTESIAN_POINT('Ctrl Pts',(-0.390179988506806,2.24608553033568,
7.03296868514229));
#31926=CARTESIAN_POINT('Ctrl Pts',(-0.393924158185101,2.10793299234673,
7.03998789038988));
#31927=CARTESIAN_POINT('Ctrl Pts',(-0.393888044763371,2.10014166969089,
7.04038364779653));
#31928=CARTESIAN_POINT('',(-0.393238618660761,2.1002837677798,7.16538364368174));
#31929=CARTESIAN_POINT('Ctrl Pts',(-0.393299974560873,2.10014145817971,
7.04038364779653));
#31930=CARTESIAN_POINT('Ctrl Pts',(-0.393307289300358,2.07980409162154,
7.04141822341494));
#31931=CARTESIAN_POINT('Ctrl Pts',(-0.391732853256908,2.05940230957188,
7.04245279903335));
#31932=CARTESIAN_POINT('Ctrl Pts',(-0.388572870996293,2.03920514885537,
7.04348737465176));
#31933=CARTESIAN_POINT('Ctrl Pts',(-0.385418453513969,2.01904355565545,
7.04452012836629));
#31934=CARTESIAN_POINT('Ctrl Pts',(-0.380684085738039,1.99908661093811,
7.04555288208082));
#31935=CARTESIAN_POINT('Ctrl Pts',(-0.374417843067382,1.97959996348518,
7.04658563579535));
#31936=CARTESIAN_POINT('Ctrl Pts',(-0.3681070857465,1.95997488518286,7.04762572607068));
#31937=CARTESIAN_POINT('Ctrl Pts',(-0.360242731002926,1.9408275735491,7.04866581634602));
#31938=CARTESIAN_POINT('Ctrl Pts',(-0.350925623435377,1.92241594436298,
7.04970590662135));
#31939=CARTESIAN_POINT('Ctrl Pts',(-0.341677524073189,1.90414068297971,
7.05073829335105));
#31940=CARTESIAN_POINT('Ctrl Pts',(-0.330998514642647,1.8865908935706,7.05177068008075));
#31941=CARTESIAN_POINT('Ctrl Pts',(-0.319033892043583,1.86999507455812,
7.05280306681045));
#31942=CARTESIAN_POINT('Ctrl Pts',(-0.306935351581878,1.8532135015369,7.0538470088586));
#31943=CARTESIAN_POINT('Ctrl Pts',(-0.293522685922765,1.83740802937615,
7.05489095090675));
#31944=CARTESIAN_POINT('Ctrl Pts',(-0.278987967121695,1.82278058473241,
7.0559348929549));
#31945=CARTESIAN_POINT('Ctrl Pts',(-0.264453248320622,1.80815314008867,
7.05697883500306));
#31946=CARTESIAN_POINT('Ctrl Pts',(-0.248797112435385,1.7947041855536,7.05802277705121));
#31947=CARTESIAN_POINT('Ctrl Pts',(-0.232245073167206,1.78259313808684,
7.05906671909936));
#31948=CARTESIAN_POINT('Ctrl Pts',(-0.215692707288845,1.77048185164099,
7.06011068174691));
#31949=CARTESIAN_POINT('Ctrl Pts',(-0.198141089577947,1.75963274225577,
7.06115464439446));
#31950=CARTESIAN_POINT('Ctrl Pts',(-0.17980894382752,1.75020915718156,7.06219860704202));
#31951=CARTESIAN_POINT('Ctrl Pts',(-0.161510522034605,1.74080290780756,
7.06324064920779));
#31952=CARTESIAN_POINT('Ctrl Pts',(-0.142435042141189,1.73281736284896,
7.06428269137356));
#31953=CARTESIAN_POINT('Ctrl Pts',(-0.122829002330193,1.72637194138212,
7.06532473353932));
#31954=CARTESIAN_POINT('Ctrl Pts',(-0.103244019097943,1.71993344219667,
7.06636565656818));
#31955=CARTESIAN_POINT('Ctrl Pts',(-0.0831302935632959,1.71503203887742,
7.06740657959703));
#31956=CARTESIAN_POINT('Ctrl Pts',(-0.0627528646893455,1.71173853143367,
7.06844750262589));
#31957=CARTESIAN_POINT('Ctrl Pts',(-0.0423649704990329,1.70844333253034,
7.06948896024568));
#31958=CARTESIAN_POINT('Ctrl Pts',(-0.021713826188412,1.70675781252406,
7.07053041786547));
#31959=CARTESIAN_POINT('Ctrl Pts',(-0.00107369334917631,1.70670146557279,
7.07157187548526));
#31960=CARTESIAN_POINT('Ctrl Pts',(0.0195727459504677,1.70664510140506,
7.07261365131576));
#31961=CARTESIAN_POINT('Ctrl Pts',(0.0402074318264637,1.70821886708768,
7.07365542714626));
#31962=CARTESIAN_POINT('Ctrl Pts',(0.0605580250734511,1.71139014989426,
7.07469720297676));
#31963=CARTESIAN_POINT('Ctrl Pts',(0.0809526065895549,1.7145682875006,7.07574123062935));
#31964=CARTESIAN_POINT('Ctrl Pts',(0.101061153017379,1.71935066571312,7.07678525828195));
#31965=CARTESIAN_POINT('Ctrl Pts',(0.120622661312042,1.72565381853423,7.07782928593455));
#31966=CARTESIAN_POINT('Ctrl Pts',(0.127541310388466,1.7278831610669,7.07819854483041));
#31967=CARTESIAN_POINT('Ctrl Pts',(0.134391697982113,1.73030229809388,7.07856780372628));
#31968=CARTESIAN_POINT('Ctrl Pts',(0.141162917963318,1.73290611474436,7.07893706262215));
#31969=CARTESIAN_POINT('Ctrl Pts',(0.160306399184353,1.7402675821446,7.0799810252697));
#31970=CARTESIAN_POINT('Ctrl Pts',(0.178929532406589,1.74915247762564,7.08102498791726));
#31971=CARTESIAN_POINT('Ctrl Pts',(0.19677657319603,1.75946531712434,7.08206895056481));
#31972=CARTESIAN_POINT('Ctrl Pts',(0.214590782430805,1.7697591850435,7.08311099273058));
#31973=CARTESIAN_POINT('Ctrl Pts',(0.231631073546616,1.78147547029687,7.08415303489635));
#31974=CARTESIAN_POINT('Ctrl Pts',(0.247663602925591,1.79447155650265,7.08519507706212));
#31975=CARTESIAN_POINT('Ctrl Pts',(0.263678913619891,1.80745368511601,7.08623600009097));
#31976=CARTESIAN_POINT('Ctrl Pts',(0.278688024351192,1.82171244748997,7.08727692311983));
#31977=CARTESIAN_POINT('Ctrl Pts',(0.292487934824368,1.8370633194433,7.08831784614868));
#31978=CARTESIAN_POINT('Ctrl Pts',(0.306294932571885,1.85242207520437,7.08935930376847));
#31979=CARTESIAN_POINT('Ctrl Pts',(0.318890985529203,1.86887352465195,7.09040076138827));
#31980=CARTESIAN_POINT('Ctrl Pts',(0.330111239904106,1.8861976162692,7.09144221900806));
#31981=CARTESIAN_POINT('Ctrl Pts',(0.341334922555885,1.90352700115171,7.09248399483856));
#31982=CARTESIAN_POINT('Ctrl Pts',(0.351181600502437,1.92172892228774,7.09352577066905));
#31983=CARTESIAN_POINT('Ctrl Pts',(0.359531272975277,1.94055673813931,7.09456754649955));
#31984=CARTESIAN_POINT('Ctrl Pts',(0.367898993454642,1.95942525074209,7.09561157415215));
#31985=CARTESIAN_POINT('Ctrl Pts',(0.37476300374778,1.97892166434828,7.09665560180474));
#31986=CARTESIAN_POINT('Ctrl Pts',(0.380052197895641,1.99878134127201,7.09769962945734));
#31987=CARTESIAN_POINT('Ctrl Pts',(0.381922916536285,2.00580544868418,7.09806888835321));
#31988=CARTESIAN_POINT('Ctrl Pts',(0.383597101393925,2.0128748998086,7.09843814724907));
#31989=CARTESIAN_POINT('Ctrl Pts',(0.385073149458468,2.01997775580417,7.09880740614494));
#31990=CARTESIAN_POINT('Ctrl Pts',(0.389246208151508,2.04005883288409,7.09985136879249));
#31991=CARTESIAN_POINT('Ctrl Pts',(0.391856667464328,2.06052705119684,7.10089533144004));
#31992=CARTESIAN_POINT('Ctrl Pts',(0.392846373023673,2.0811156889947,7.1019392940876));
#31993=CARTESIAN_POINT('Ctrl Pts',(0.393834257912996,2.10166645177478,7.10298133625337));
#31994=CARTESIAN_POINT('Ctrl Pts',(0.393207212978599,2.12233647054837,7.10402337841914));
#31995=CARTESIAN_POINT('Ctrl Pts',(0.390958568852128,2.14285192459034,7.10506542058491));
#31996=CARTESIAN_POINT('Ctrl Pts',(0.388712339734123,2.16334534535695,7.10610634361376));
#31997=CARTESIAN_POINT('Ctrl Pts',(0.384848019872022,2.1836838001012,7.10714726664261));
#31998=CARTESIAN_POINT('Ctrl Pts',(0.379410872773451,2.20359671626692,7.10818818967147));
#31999=CARTESIAN_POINT('Ctrl Pts',(0.373970933297836,2.22351985918739,7.10922964729126));
#32000=CARTESIAN_POINT('Ctrl Pts',(0.366956731111274,2.24301631288328,7.11027110491105));
#32001=CARTESIAN_POINT('Ctrl Pts',(0.358464051132569,2.26182834747233,7.11131256253084));
#32002=CARTESIAN_POINT('Ctrl Pts',(0.349968776269881,2.28064612995809,7.11235433836134));
#32003=CARTESIAN_POINT('Ctrl Pts',(0.339994459775168,2.29877842187304,7.11339611419184));
#32004=CARTESIAN_POINT('Ctrl Pts',(0.328683523685281,2.31599081290145,7.11443789002234));
#32005=CARTESIAN_POINT('Ctrl Pts',(0.317348138750357,2.33324040890366,7.11548191767494));
#32006=CARTESIAN_POINT('Ctrl Pts',(0.304670817915465,2.34956555261688,7.11652594532753));
#32007=CARTESIAN_POINT('Ctrl Pts',(0.290835582344614,2.36476320371658,7.11756997298013));
#32008=CARTESIAN_POINT('Ctrl Pts',(0.285942240872061,2.37013841370348,7.117939231876));
#32009=CARTESIAN_POINT('Ctrl Pts',(0.280904386306522,2.37537291993756,7.11830849077186));
#32010=CARTESIAN_POINT('Ctrl Pts',(0.27573118930101,2.38045891186883,7.11867774966773));
#32011=CARTESIAN_POINT('Ctrl Pts',(0.261105612225831,2.39483794419938,7.11972171231529));
#32012=CARTESIAN_POINT('Ctrl Pts',(0.245308656591666,2.4081126815382,7.12076567496284));
#32013=CARTESIAN_POINT('Ctrl Pts',(0.228533106806461,2.42008984534563,7.12180963761039));
#32014=CARTESIAN_POINT('Ctrl Pts',(0.21178841745276,2.43204497586961,7.12285167977616));
#32015=CARTESIAN_POINT('Ctrl Pts',(0.194069264831007,2.4427067999076,7.12389372194193));
#32016=CARTESIAN_POINT('Ctrl Pts',(0.175602272059871,2.45192148562913,7.1249357641077));
#32017=CARTESIAN_POINT('Ctrl Pts',(0.157155112548858,2.46112627492295,7.12597668713655));
#32018=CARTESIAN_POINT('Ctrl Pts',(0.137962349487193,2.46888665864025,7.12701761016541));
#32019=CARTESIAN_POINT('Ctrl Pts',(0.118275987079078,2.47509422933507,7.12805853319426));
#32020=CARTESIAN_POINT('Ctrl Pts',(0.0985795142683154,2.48130498807641,
7.12909999081405));
#32021=CARTESIAN_POINT('Ctrl Pts',(0.0783896325466369,2.48596110395713,
7.13014144843385));
#32022=CARTESIAN_POINT('Ctrl Pts',(0.0579748959208028,2.48900360080978,
7.13118290605364));
#32023=CARTESIAN_POINT('Ctrl Pts',(0.0375539217029225,2.49204702727786,
7.13222468188414));
#32024=CARTESIAN_POINT('Ctrl Pts',(0.0169086882702682,2.49347578062839,
7.13326645771463));
#32025=CARTESIAN_POINT('Ctrl Pts',(-0.00368661236477904,2.49328272132052,
7.13430823354513));
#32026=CARTESIAN_POINT('Ctrl Pts',(-0.0243264302095114,2.49308924471057,
7.13535226119773));
#32027=CARTESIAN_POINT('Ctrl Pts',(-0.0449153661678067,2.49126702164157,
7.13639628885033));
#32028=CARTESIAN_POINT('Ctrl Pts',(-0.0651830863183576,2.48786087100662,
7.13744031650292));
#32029=CARTESIAN_POINT('Ctrl Pts',(-0.0723515132713222,2.48665616017402,
7.13780957539879));
#32030=CARTESIAN_POINT('Ctrl Pts',(-0.0794798615381201,2.48525377466167,
7.13817883429465));
#32031=CARTESIAN_POINT('Ctrl Pts',(-0.0865565996283024,2.48365719732697,
7.13854809319052));
#32032=CARTESIAN_POINT('Ctrl Pts',(-0.106563836597748,2.47914338027336,
7.13959205583807));
#32033=CARTESIAN_POINT('Ctrl Pts',(-0.126276650945867,2.47304687232218,
7.14063601848563));
#32034=CARTESIAN_POINT('Ctrl Pts',(-0.145428172932575,2.46542514488947,
7.14167998113318));
#32035=CARTESIAN_POINT('Ctrl Pts',(-0.164544463630889,2.45781743844567,
7.14272202329895));
#32036=CARTESIAN_POINT('Ctrl Pts',(-0.183100813654346,2.44869029566948,
7.14376406546472));
#32037=CARTESIAN_POINT('Ctrl Pts',(-0.200845203256677,2.43815099338725,
7.14480610763049));
#32038=CARTESIAN_POINT('Ctrl Pts',(-0.218570535663357,2.42762301015008,
7.14584703065934));
#32039=CARTESIAN_POINT('Ctrl Pts',(-0.235484994674274,2.41568622726063,
7.1468879536882));
#32040=CARTESIAN_POINT('Ctrl Pts',(-0.251361014938732,2.40249385145647,
7.14792887671705));
#32041=CARTESIAN_POINT('Ctrl Pts',(-0.267245188713404,2.38929470039194,
7.14897033433685));
#32042=CARTESIAN_POINT('Ctrl Pts',(-0.282089282094752,2.37483912600987,
7.15001179195664));
#32043=CARTESIAN_POINT('Ctrl Pts',(-0.295698333728938,2.35932100846235,
7.15105324957643));
#32044=CARTESIAN_POINT('Ctrl Pts',(-0.309311543521694,2.3437981494534,7.15209502540693));
#32045=CARTESIAN_POINT('Ctrl Pts',(-0.321688502812557,2.32721267754762,
7.15313680123742));
#32046=CARTESIAN_POINT('Ctrl Pts',(-0.332674783457099,2.3097912735358,7.15417857706792));
#32047=CARTESIAN_POINT('Ctrl Pts',(-0.343684811196566,2.29233221276386,
7.15522260472052));
#32048=CARTESIAN_POINT('Ctrl Pts',(-0.353297816467056,2.27403426450518,
7.15626663237312));
#32049=CARTESIAN_POINT('Ctrl Pts',(-0.36140514716012,2.25514899163763,7.15731066002571));
#32050=CARTESIAN_POINT('Ctrl Pts',(-0.36427260375736,2.24846951816788,7.15767991892158));
#32051=CARTESIAN_POINT('Ctrl Pts',(-0.366952156627619,2.24171673869915,
7.15804917781744));
#32052=CARTESIAN_POINT('Ctrl Pts',(-0.369440492015627,2.2349022344487,7.15841843671331));
#32053=CARTESIAN_POINT('Ctrl Pts',(-0.377534369956373,2.21273650634965,
7.15961953542616));
#32054=CARTESIAN_POINT('Ctrl Pts',(-0.383641314242097,2.18980835275673,
7.16082063413901));
#32055=CARTESIAN_POINT('Ctrl Pts',(-0.387644613228899,2.16645708265202,
7.16202173285185));
#32056=CARTESIAN_POINT('Ctrl Pts',(-0.391379729877021,2.14467012194525,
7.16314236956002));
#32057=CARTESIAN_POINT('Ctrl Pts',(-0.393283854254901,2.12251519922877,
7.1642630062682));
#32058=CARTESIAN_POINT('Ctrl Pts',(-0.393299897588104,2.1002838259803,7.16538364297637));
#32059=CARTESIAN_POINT('',(-0.393212132698943,2.09972772529158,7.29038365170245));
#32060=CARTESIAN_POINT('Ctrl Pts',(-0.392881147913482,2.10028342826704,
7.16538364779653));
#32061=CARTESIAN_POINT('Ctrl Pts',(-0.392314472383569,2.01503579577097,
7.16968535860972));
#32062=CARTESIAN_POINT('Ctrl Pts',(-0.323128061668355,1.79769261307425,
7.18061051726384));
#32063=CARTESIAN_POINT('Ctrl Pts',(0.0356248266137504,1.63631269996556,
7.19815912375889));
#32064=CARTESIAN_POINT('Ctrl Pts',(0.409160946250237,1.87895167825091,7.21802946728168));
#32065=CARTESIAN_POINT('Ctrl Pts',(0.407347599935112,2.32437239872943,7.23789981080447));
#32066=CARTESIAN_POINT('Ctrl Pts',(0.0318482860476476,2.56396198891753,
7.25777015432726));
#32067=CARTESIAN_POINT('Ctrl Pts',(-0.324479005289757,2.40017195559432,
7.27526476665795));
#32068=CARTESIAN_POINT('Ctrl Pts',(-0.392323111645839,2.18391812223174,
7.2861359311477));
#32069=CARTESIAN_POINT('Ctrl Pts',(-0.392858015080995,2.09972804792847,
7.29038364779653));
#32070=CARTESIAN_POINT('',(-0.393452426999084,2.09984062647883,7.41538364779653));
#32071=CARTESIAN_POINT('Ctrl Pts',(-0.39329990569911,2.09972764532152,7.29038365267059));
#32072=CARTESIAN_POINT('Ctrl Pts',(-0.393283516148222,2.07605994533971,
7.29157644434568));
#32073=CARTESIAN_POINT('Ctrl Pts',(-0.39112659367968,2.05247744071622,7.29276923602077));
#32074=CARTESIAN_POINT('Ctrl Pts',(-0.386899369366362,2.02933340262959,
7.29396202769585));
#32075=CARTESIAN_POINT('Ctrl Pts',(-0.382707066616411,2.00638055997824,
7.29514496558818));
#32076=CARTESIAN_POINT('Ctrl Pts',(-0.376478845323879,1.98385918914853,
7.2963279034805));
#32077=CARTESIAN_POINT('Ctrl Pts',(-0.368329867046097,1.96209423854746,
7.29751084137283));
#32078=CARTESIAN_POINT('Ctrl Pts',(-0.361138256232981,1.94288630244137,
7.29855480402038));
#32079=CARTESIAN_POINT('Ctrl Pts',(-0.352418668001632,1.92418519980553,
7.29959876666793));
#32080=CARTESIAN_POINT('Ctrl Pts',(-0.342264317354093,1.90624751081306,
7.30064272931548));
#32081=CARTESIAN_POINT('Ctrl Pts',(-0.332128646728762,1.88834282013237,
7.30168477148125));
#32082=CARTESIAN_POINT('Ctrl Pts',(-0.320563759413357,1.87119941782039,
7.30272681364702));
#32083=CARTESIAN_POINT('Ctrl Pts',(-0.307710194871082,1.85505240157862,
7.30376885581279));
#32084=CARTESIAN_POINT('Ctrl Pts',(-0.294870434855203,1.83892272697864,
7.30480977884164));
#32085=CARTESIAN_POINT('Ctrl Pts',(-0.280745178513786,1.82378790479044,
7.30585070187049));
#32086=CARTESIAN_POINT('Ctrl Pts',(-0.265517144667215,1.80985256181078,
7.30689162489935));
#32087=CARTESIAN_POINT('Ctrl Pts',(-0.250281290099351,1.79591006200216,
7.30793308251914));
#32088=CARTESIAN_POINT('Ctrl Pts',(-0.233942058489515,1.78316878069185,
7.30897454013893));
#32089=CARTESIAN_POINT('Ctrl Pts',(-0.2167180324914,1.77179551436177,7.31001599775872));
#32090=CARTESIAN_POINT('Ctrl Pts',(-0.199488743802439,1.76041877300299,
7.31105777358922));
#32091=CARTESIAN_POINT('Ctrl Pts',(-0.181374755953678,1.7504112536381,7.31209954941971));
#32092=CARTESIAN_POINT('Ctrl Pts',(-0.1626216378728,1.74189513701212,7.31314132525021));
#32093=CARTESIAN_POINT('Ctrl Pts',(-0.143827984501629,1.7333606126068,7.31418535290281));
#32094=CARTESIAN_POINT('Ctrl Pts',(-0.124393135300646,1.72632417761872,
7.3152293805554));
#32095=CARTESIAN_POINT('Ctrl Pts',(-0.104581087736443,1.72085927930666,
7.316273408208));
#32096=CARTESIAN_POINT('Ctrl Pts',(-0.0975738262041833,1.71892641640616,
7.31664266710387));
#32097=CARTESIAN_POINT('Ctrl Pts',(-0.0905194818952901,1.71718967793619,
7.31701192599975));
#32098=CARTESIAN_POINT('Ctrl Pts',(-0.0834299789834502,1.715650772595,7.31738118489563));
#32099=CARTESIAN_POINT('Ctrl Pts',(-0.0633866535218433,1.71130000484841,
7.31842514754318));
#32100=CARTESIAN_POINT('Ctrl Pts',(-0.0429423609312796,1.70850834598792,
7.31946911019074));
#32101=CARTESIAN_POINT('Ctrl Pts',(-0.0223632973801085,1.70733631065467,
7.32051307283829));
#32102=CARTESIAN_POINT('Ctrl Pts',(-0.00182209123385836,1.7061664314067,
7.32155511500406));
#32103=CARTESIAN_POINT('Ctrl Pts',(0.0188526708402339,1.70661036229058,
7.32259715716983));
#32104=CARTESIAN_POINT('Ctrl Pts',(0.0393872379346304,1.70867719784316,
7.3236391993356));
#32105=CARTESIAN_POINT('Ctrl Pts',(0.0598997512265555,1.71074181364682,
7.32468012236445));
#32106=CARTESIAN_POINT('Ctrl Pts',(0.0802716371868918,1.71442582936336,
7.3257210453933));
#32107=CARTESIAN_POINT('Ctrl Pts',(0.100231932942214,1.71968637991959,7.32676196842215));
#32108=CARTESIAN_POINT('Ctrl Pts',(0.120202479785208,1.72494963215747,7.32780342604194));
#32109=CARTESIAN_POINT('Ctrl Pts',(0.139760298537318,1.73179086484532,7.32884488366174));
#32110=CARTESIAN_POINT('Ctrl Pts',(0.158646820990185,1.74011657972378,7.32988634128152));
#32111=CARTESIAN_POINT('Ctrl Pts',(0.177539114099043,1.74844483847111,7.33092811711202));
#32112=CARTESIAN_POINT('Ctrl Pts',(0.195759044481055,1.75825815271757,7.33196989294252));
#32113=CARTESIAN_POINT('Ctrl Pts',(0.213070949480534,1.76941618235693,7.33301166877302));
#32114=CARTESIAN_POINT('Ctrl Pts',(0.230420274555529,1.78059833033057,7.33405569642561));
#32115=CARTESIAN_POINT('Ctrl Pts',(0.246857070114484,1.79313055010845,7.33509972407821));
#32116=CARTESIAN_POINT('Ctrl Pts',(0.262176673788396,1.80683062622222,7.3361437517308));
#32117=CARTESIAN_POINT('Ctrl Pts',(0.267595016802297,1.81167616356647,7.33651301062667));
#32118=CARTESIAN_POINT('Ctrl Pts',(0.272873941641249,1.81666745465028,7.33688226952254));
#32119=CARTESIAN_POINT('Ctrl Pts',(0.278005556830508,1.82179539836416,7.33725152841841));
#32120=CARTESIAN_POINT('Ctrl Pts',(0.292513574481946,1.83629303608107,7.33829549106596));
#32121=CARTESIAN_POINT('Ctrl Pts',(0.305927716218984,1.85197178795044,7.33933945371351));
#32122=CARTESIAN_POINT('Ctrl Pts',(0.318053003452094,1.86864058913651,7.34038341636107));
#32123=CARTESIAN_POINT('Ctrl Pts',(0.330155984912766,1.88527872626663,7.34142545852684));
#32124=CARTESIAN_POINT('Ctrl Pts',(0.340974342157243,1.90290274419619,7.34246750069261));
#32125=CARTESIAN_POINT('Ctrl Pts',(0.350352242023501,1.92128739129791,7.34350954285838));
#32126=CARTESIAN_POINT('Ctrl Pts',(0.359720070172624,1.93965229357745,7.34455046588723));
#32127=CARTESIAN_POINT('Ctrl Pts',(0.367650153765075,1.95877556431229,7.34559138891609));
#32128=CARTESIAN_POINT('Ctrl Pts',(0.374031857422495,1.97840616942838,7.34663231194494));
#32129=CARTESIAN_POINT('Ctrl Pts',(0.380416838556585,1.99804685631163,7.34767376956473));
#32130=CARTESIAN_POINT('Ctrl Pts',(0.385251608302461,2.01819470335628,7.34871522718453));
#32131=CARTESIAN_POINT('Ctrl Pts',(0.388474814027385,2.03858168948605,7.34975668480432));
#32132=CARTESIAN_POINT('Ctrl Pts',(0.391699004582178,2.05897490472888,7.35079846063482));
#32133=CARTESIAN_POINT('Ctrl Pts',(0.393310571791438,2.07960667272766,7.35184023646532));
#32134=CARTESIAN_POINT('Ctrl Pts',(0.393299947675492,2.10020287546682,7.35288201229582));
#32135=CARTESIAN_POINT('Ctrl Pts',(0.393289300595279,2.12084359736559,7.35392603994841));
#32136=CARTESIAN_POINT('Ctrl Pts',(0.391649520254463,2.14144786637088,7.35497006760101));
#32137=CARTESIAN_POINT('Ctrl Pts',(0.388423029242925,2.16174496217304,7.35601409525361));
#32138=CARTESIAN_POINT('Ctrl Pts',(0.387281861664202,2.16892377890888,7.35638335414947));
#32139=CARTESIAN_POINT('Ctrl Pts',(0.385942672154399,2.17606426947985,7.35675261304534));
#32140=CARTESIAN_POINT('Ctrl Pts',(0.384408841291466,2.18315487199769,7.3571218719412));
#32141=CARTESIAN_POINT('Ctrl Pts',(0.380072420025781,2.20320130624799,7.35816583458876));
#32142=CARTESIAN_POINT('Ctrl Pts',(0.374150762036044,2.22296734847639,7.35920979723631));
#32143=CARTESIAN_POINT('Ctrl Pts',(0.366698972623503,2.24218563034592,7.36025375988386));
#32144=CARTESIAN_POINT('Ctrl Pts',(0.359260891580563,2.26136855811507,7.36129580204963));
#32145=CARTESIAN_POINT('Ctrl Pts',(0.350298474009957,2.28000502593331,7.3623378442154));
#32146=CARTESIAN_POINT('Ctrl Pts',(0.339916760206563,2.29784207371202,7.36337988638117));
#32147=CARTESIAN_POINT('Ctrl Pts',(0.3295461962007,2.31565996478164,7.36442080941003));
#32148=CARTESIAN_POINT('Ctrl Pts',(0.317759705312583,2.33267949303378,7.36546173243888));
#32149=CARTESIAN_POINT('Ctrl Pts',(0.304708472556916,2.34867174498127,7.36650265546773));
#32150=CARTESIAN_POINT('Ctrl Pts',(0.291650537028262,2.36467221013256,7.36754411308752));
#32151=CARTESIAN_POINT('Ctrl Pts',(0.277327014720529,2.37964376475223,7.36858557070731));
#32152=CARTESIAN_POINT('Ctrl Pts',(0.26193005126473,2.39338973779677,7.36962702832711));
#32153=CARTESIAN_POINT('Ctrl Pts',(0.246528383365344,2.40713991083534,7.3706688041576));
#32154=CARTESIAN_POINT('Ctrl Pts',(0.230053193882422,2.41966329420914,7.3717105799881));
#32155=CARTESIAN_POINT('Ctrl Pts',(0.212729786831095,2.43080345795472,7.3727523558186));
#32156=CARTESIAN_POINT('Ctrl Pts',(0.195368934842308,2.44196770141703,7.3737963834712));
#32157=CARTESIAN_POINT('Ctrl Pts',(0.177156853828494,2.45174240785529,7.37484041112379));
#32158=CARTESIAN_POINT('Ctrl Pts',(0.158344134387518,2.46001670114742,7.37588443877639));
#32159=CARTESIAN_POINT('Ctrl Pts',(0.151690322113735,2.46294321022744,7.37625369767226));
#32160=CARTESIAN_POINT('Ctrl Pts',(0.144961542316253,2.4656824722768,7.37662295656812));
#32161=CARTESIAN_POINT('Ctrl Pts',(0.138169346405668,2.46823107108693,7.37699221546399));
#32162=CARTESIAN_POINT('Ctrl Pts',(0.118966562383692,2.47543642752156,7.37803617811154));
#32163=CARTESIAN_POINT('Ctrl Pts',(0.0991414197118359,2.4811571072681,7.3790801407591));
#32164=CARTESIAN_POINT('Ctrl Pts',(0.0789485559701378,2.48529471253864,
7.38012410340665));
#32165=CARTESIAN_POINT('Ctrl Pts',(0.0587928391771958,2.48942470623842,
7.38116614557242));
#32166=CARTESIAN_POINT('Ctrl Pts',(0.0382714447895694,2.49197720184811,
7.38220818773819));
#32167=CARTESIAN_POINT('Ctrl Pts',(0.0176539263884321,2.49290358726165,
7.38325022990396));
#32168=CARTESIAN_POINT('Ctrl Pts',(-0.00294144912182975,2.49382897775181,
7.38429115293281));
#32169=CARTESIAN_POINT('Ctrl Pts',(-0.0236320136864995,2.49313166334946,
7.38533207596166));
#32170=CARTESIAN_POINT('Ctrl Pts',(-0.0441434535668194,2.49081484811506,
7.38637299899052));
#32171=CARTESIAN_POINT('Ctrl Pts',(-0.0646654275880691,2.48849684302473,
7.38741445661031));
#32172=CARTESIAN_POINT('Ctrl Pts',(-0.0850073602035416,2.484557742049,7.3884559142301));
#32173=CARTESIAN_POINT('Ctrl Pts',(-0.104899874976661,2.47905264308521,
7.38949737184989));
#32174=CARTESIAN_POINT('Ctrl Pts',(-0.124798467780291,2.47354586207368,
7.39053914768039));
#32175=CARTESIAN_POINT('Ctrl Pts',(-0.144246670499333,2.46647236148174,
7.39158092351089));
#32176=CARTESIAN_POINT('Ctrl Pts',(-0.162990992885366,2.45793690259352,
7.39262269934139));
#32177=CARTESIAN_POINT('Ctrl Pts',(-0.181775831549595,2.44938299411722,
7.39366672699398));
#32178=CARTESIAN_POINT('Ctrl Pts',(-0.199853108257183,2.4393611755375,7.39471075464658));
#32179=CARTESIAN_POINT('Ctrl Pts',(-0.216993947160994,2.4280221286674,7.39575478229918));
#32180=CARTESIAN_POINT('Ctrl Pts',(-0.223056437203418,2.42401165641885,
7.39612404119505));
#32181=CARTESIAN_POINT('Ctrl Pts',(-0.229002067865071,2.41983678993309,
7.39649330009091));
#32182=CARTESIAN_POINT('Ctrl Pts',(-0.234821713749347,2.41550539258754,
7.39686255898678));
#32183=CARTESIAN_POINT('Ctrl Pts',(-0.251115636933297,2.40337828777207,
7.39789641503299));
#32184=CARTESIAN_POINT('Ctrl Pts',(-0.266520733870789,2.38994591250046,
7.39893027107921));
#32185=CARTESIAN_POINT('Ctrl Pts',(-0.280818729815168,2.37536472356676,
7.39996412712542));
#32186=CARTESIAN_POINT('Ctrl Pts',(-0.295090416083402,2.36081036541131,
7.40099608077791));
#32187=CARTESIAN_POINT('Ctrl Pts',(-0.308258478460216,2.34511187397496,
7.4020280344304));
#32188=CARTESIAN_POINT('Ctrl Pts',(-0.320138146793209,2.32846543932904,
7.40305998808288));
#32189=CARTESIAN_POINT('Ctrl Pts',(-0.332014905654445,2.31182308159251,
7.40409168899768));
#32190=CARTESIAN_POINT('Ctrl Pts',(-0.342603417874453,2.29423382004764,
7.40512338991247));
#32191=CARTESIAN_POINT('Ctrl Pts',(-0.351759479259452,2.2759265720439,7.40615509082726));
#32192=CARTESIAN_POINT('Ctrl Pts',(-0.360912697844894,2.25762500812575,
7.40718647141666));
#32193=CARTESIAN_POINT('Ctrl Pts',(-0.368634018416044,2.23860657620211,
7.40821785200607));
#32194=CARTESIAN_POINT('Ctrl Pts',(-0.374825953099693,2.21912344388451,
7.40924923259547));
#32195=CARTESIAN_POINT('Ctrl Pts',(-0.381031373848938,2.19959787720449,
7.41028285953711));
#32196=CARTESIAN_POINT('Ctrl Pts',(-0.38570054657744,2.17960631464732,7.41131648647874));
#32197=CARTESIAN_POINT('Ctrl Pts',(-0.388786161499595,2.1594155756213,7.41235011342038));
#32198=CARTESIAN_POINT('Ctrl Pts',(-0.391804761525357,2.13966334895605,
7.41336129154576));
#32199=CARTESIAN_POINT('Ctrl Pts',(-0.393308020622564,2.11972120808856,
7.41437246967114));
#32200=CARTESIAN_POINT('Ctrl Pts',(-0.393299967734249,2.09984068823463,
7.41538364779653));
#32201=CARTESIAN_POINT('',(-0.393299835621208,2.10035958355185,7.54038364779653));
#32202=CARTESIAN_POINT('Ctrl Pts',(-0.393871230970384,2.0998404568363,7.41538364779653));
#32203=CARTESIAN_POINT('Ctrl Pts',(-0.393916702120302,2.09098514042463,
7.41583339936755));
#32204=CARTESIAN_POINT('Ctrl Pts',(-0.38962793339212,1.95176327063558,7.42290659877944));
#32205=CARTESIAN_POINT('Ctrl Pts',(-0.224663887225575,1.69281309173686,
7.4366032460324));
#32206=CARTESIAN_POINT('Ctrl Pts',(0.220755421324649,1.69068095030845,7.45647358955513));
#32207=CARTESIAN_POINT('Ctrl Pts',(0.463661683946385,2.06404331321586,7.47634393307795));
#32208=CARTESIAN_POINT('Ctrl Pts',(0.281221473385678,2.47039104118654,7.49621427660072));
#32209=CARTESIAN_POINT('Ctrl Pts',(-0.159201154159844,2.53695541305568,
7.51608462012352));
#32210=CARTESIAN_POINT('Ctrl Pts',(-0.377322826346887,2.2892653798589,7.53080774385545));
#32211=CARTESIAN_POINT('Ctrl Pts',(-0.39361134344189,2.12952756160154,7.53890741974645));
#32212=CARTESIAN_POINT('Ctrl Pts',(-0.39334115544482,2.10035962132946,7.54038364779653));
#32213=CARTESIAN_POINT('',(-0.393056831489965,2.09997021398409,7.66538365574708));
#32214=CARTESIAN_POINT('Ctrl Pts',(-0.393299835621208,2.10035958355185,
7.54038364779653));
#32215=CARTESIAN_POINT('Ctrl Pts',(-0.393318404588432,2.08004950062605,
7.54141168552471));
#32216=CARTESIAN_POINT('Ctrl Pts',(-0.391759450431452,2.0596927690009,7.5424397232529));
#32217=CARTESIAN_POINT('Ctrl Pts',(-0.38862778303309,2.0395571653975,7.54346776098108));
#32218=CARTESIAN_POINT('Ctrl Pts',(-0.385490760961835,2.01938713298762,
7.54449755649675));
#32219=CARTESIAN_POINT('Ctrl Pts',(-0.380775683903768,1.99943974722539,
7.54552735201241));
#32220=CARTESIAN_POINT('Ctrl Pts',(-0.374539625500721,1.97997933957114,
7.54655714752808));
#32221=CARTESIAN_POINT('Ctrl Pts',(-0.36831701768203,1.96056090616374,7.54758472187285));
#32222=CARTESIAN_POINT('Ctrl Pts',(-0.360580232459262,1.94162807082187,
7.54861229621762));
#32223=CARTESIAN_POINT('Ctrl Pts',(-0.351435703674561,1.92342753277261,
7.54963987056239));
#32224=CARTESIAN_POINT('Ctrl Pts',(-0.342261525120969,1.9051679821969,7.55067077666351));
#32225=CARTESIAN_POINT('Ctrl Pts',(-0.331670832463183,1.88764615303161,
7.55170168276462));
#32226=CARTESIAN_POINT('Ctrl Pts',(-0.319816577306472,1.87108462943705,
7.55273258886574));
#32227=CARTESIAN_POINT('Ctrl Pts',(-0.30796232214976,1.85452310584248,7.55376349496686));
#32228=CARTESIAN_POINT('Ctrl Pts',(-0.29484504310219,1.83892242880877,7.55479440106798));
#32229=CARTESIAN_POINT('Ctrl Pts',(-0.280656185780356,1.82446961078091,
7.5558253071691));
#32230=CARTESIAN_POINT('Ctrl Pts',(-0.266287624919792,1.80983374612109,
7.55686926981665));
#32231=CARTESIAN_POINT('Ctrl Pts',(-0.250728306984616,1.79628125247181,
7.5579132324642));
#32232=CARTESIAN_POINT('Ctrl Pts',(-0.234167562247261,1.78400879317428,
7.55895719511176));
#32233=CARTESIAN_POINT('Ctrl Pts',(-0.217637282784374,1.77175891038806,
7.55999923727753));
#32234=CARTESIAN_POINT('Ctrl Pts',(-0.20010978234379,1.76078486875542,7.5610412794433));
#32235=CARTESIAN_POINT('Ctrl Pts',(-0.181808923387943,1.75124449054314,
7.56208332160907));
#32236=CARTESIAN_POINT('Ctrl Pts',(-0.163527719267103,1.74171435854717,
7.56312424463792));
#32237=CARTESIAN_POINT('Ctrl Pts',(-0.144475441288614,1.73361519728125,
7.56416516766677));
#32238=CARTESIAN_POINT('Ctrl Pts',(-0.124902133699992,1.7270598613756,7.56520609069563));
#32239=CARTESIAN_POINT('Ctrl Pts',(-0.105318773770749,1.72050115882028,
7.56624754831542));
#32240=CARTESIAN_POINT('Ctrl Pts',(-0.0852145422218727,1.71548811454974,
7.56728900593521));
#32241=CARTESIAN_POINT('Ctrl Pts',(-0.0648569061699768,1.71208445284823,
7.568330463555));
#32242=CARTESIAN_POINT('Ctrl Pts',(-0.0444930499727531,1.70867975117968,
7.5693722393855));
#32243=CARTESIAN_POINT('Ctrl Pts',(-0.0238763661954681,1.70688549655674,
7.570414015216));
#32244=CARTESIAN_POINT('Ctrl Pts',(-0.00328087734933675,1.70671368464715,
7.57145579104649));
#32245=CARTESIAN_POINT('Ctrl Pts',(0.0173591291133135,1.70654150136223,
7.57249981869909));
#32246=CARTESIAN_POINT('Ctrl Pts',(0.0379771145355644,1.70799871031615,
7.57354384635169));
#32247=CARTESIAN_POINT('Ctrl Pts',(0.0583019934603891,1.71104528855078,
7.57458787400428));
#32248=CARTESIAN_POINT('Ctrl Pts',(0.0654906367226648,1.71212282333858,
7.57495713290015));
#32249=CARTESIAN_POINT('Ctrl Pts',(0.0726427093484844,1.71339871177181,
7.57532639179602));
#32250=CARTESIAN_POINT('Ctrl Pts',(0.0797466199589037,1.71486967581722,
7.57569565069189));
#32251=CARTESIAN_POINT('Ctrl Pts',(0.0998306786282814,1.71902836105536,
7.57673961333944));
#32252=CARTESIAN_POINT('Ctrl Pts',(0.119648397875006,1.72477470446489,7.577783575987));
#32253=CARTESIAN_POINT('Ctrl Pts',(0.138931931743202,1.73205597118298,7.57882753863455));
#32254=CARTESIAN_POINT('Ctrl Pts',(0.158179991472921,1.73932384322633,7.57986958080032));
#32255=CARTESIAN_POINT('Ctrl Pts',(0.17689511485143,1.74812083239178,7.58091162296609));
#32256=CARTESIAN_POINT('Ctrl Pts',(0.194823421295257,1.75834414315746,7.58195366513186));
#32257=CARTESIAN_POINT('Ctrl Pts',(0.212732473019612,1.76855647424798,7.58299458816071));
#32258=CARTESIAN_POINT('Ctrl Pts',(0.229855735145054,1.7801917483558,7.58403551118957));
#32259=CARTESIAN_POINT('Ctrl Pts',(0.245962964008723,1.79310081405119,7.58507643421842));
#32260=CARTESIAN_POINT('Ctrl Pts',(0.262078465125334,1.80601650950627,7.58611789183821));
#32261=CARTESIAN_POINT('Ctrl Pts',(0.277176306301301,1.82020685590285,7.587159349458));
#32262=CARTESIAN_POINT('Ctrl Pts',(0.291058122234436,1.83548145720694,7.58820080707779));
#32263=CARTESIAN_POINT('Ctrl Pts',(0.304944179667533,1.85076072556764,7.58924258290829));
#32264=CARTESIAN_POINT('Ctrl Pts',(0.317613004528018,1.8671243399691,7.59028435873879));
#32265=CARTESIAN_POINT('Ctrl Pts',(0.328906177307067,1.88434839084938,7.59132613456929));
#32266=CARTESIAN_POINT('Ctrl Pts',(0.340223760535351,1.9016096719065,7.59237016222188));
#32267=CARTESIAN_POINT('Ctrl Pts',(0.350159401208883,1.91973445673872,7.59341418987448));
#32268=CARTESIAN_POINT('Ctrl Pts',(0.358600007891362,1.93847314668974,7.59445821752707));
#32269=CARTESIAN_POINT('Ctrl Pts',(0.361585339837577,1.94510077570331,7.59482747642294));
#32270=CARTESIAN_POINT('Ctrl Pts',(0.364384096141018,1.95180502788328,7.59519673531881));
#32271=CARTESIAN_POINT('Ctrl Pts',(0.366992758407857,1.95857438253204,7.59556599421468));
#32272=CARTESIAN_POINT('Ctrl Pts',(0.374367925254579,1.97771259011604,7.59660995686223));
#32273=CARTESIAN_POINT('Ctrl Pts',(0.380263986342827,1.99748628280016,7.59765391950978));
#32274=CARTESIAN_POINT('Ctrl Pts',(0.384580292233866,2.01764170457499,7.59869788215734));
#32275=CARTESIAN_POINT('Ctrl Pts',(0.388888657815109,2.03776004827958,7.59973992432311));
#32276=CARTESIAN_POINT('Ctrl Pts',(0.391622826265736,2.05825802828576,7.60078196648888));
#32277=CARTESIAN_POINT('Ctrl Pts',(0.392731799753853,2.07886653217998,7.60182400865464));
#32278=CARTESIAN_POINT('Ctrl Pts',(0.393839582221865,2.09945290286478,7.6028649316835));
#32279=CARTESIAN_POINT('Ctrl Pts',(0.39332556661581,2.12014883235194,7.60390585471235));
#32280=CARTESIAN_POINT('Ctrl Pts',(0.391190527073315,2.14067998928346,7.6049467777412));
#32281=CARTESIAN_POINT('Ctrl Pts',(0.389054391030155,2.16122169048208,7.605988235361));
#32282=CARTESIAN_POINT('Ctrl Pts',(0.385295627939723,2.18159771656814,7.60702969298079));
#32283=CARTESIAN_POINT('Ctrl Pts',(0.379966947474016,2.20153821363053,7.60807115060058));
#32284=CARTESIAN_POINT('Ctrl Pts',(0.374636638864115,2.2214848033841,7.60911292643108));
#32285=CARTESIAN_POINT('Ctrl Pts',(0.367735682703048,2.24099489830156,7.61015470226157));
#32286=CARTESIAN_POINT('Ctrl Pts',(0.35936659081686,2.25981409013184,7.61119647809207));
#32287=CARTESIAN_POINT('Ctrl Pts',(0.350979408948642,2.27867396007232,7.61224050574467));
#32288=CARTESIAN_POINT('Ctrl Pts',(0.341118107170815,2.29683929816591,7.61328453339727));
#32289=CARTESIAN_POINT('Ctrl Pts',(0.329931334064598,2.31407990284554,7.61432856104986));
#32290=CARTESIAN_POINT('Ctrl Pts',(0.325974719050399,2.32017767873512,7.61469781994573));
#32291=CARTESIAN_POINT('Ctrl Pts',(0.321852681139374,2.32616005598819,7.6150670788416));
#32292=CARTESIAN_POINT('Ctrl Pts',(0.317573002570163,2.33201783991446,7.61543633773746));
#32293=CARTESIAN_POINT('Ctrl Pts',(0.305473566050664,2.34857886981768,7.61648030038501));
#32294=CARTESIAN_POINT('Ctrl Pts',(0.292039135608204,2.36424024068389,7.61752426303257));
#32295=CARTESIAN_POINT('Ctrl Pts',(0.277428590479045,2.37877996194994,7.61856822568012));
#32296=CARTESIAN_POINT('Ctrl Pts',(0.262844923022031,2.39329293583198,7.61961026784589));
#32297=CARTESIAN_POINT('Ctrl Pts',(0.247089909214749,2.4066878005712,7.62065231001166));
#32298=CARTESIAN_POINT('Ctrl Pts',(0.230362217544916,2.41877600086548,7.62169435217743));
#32299=CARTESIAN_POINT('Ctrl Pts',(0.213652491153156,2.43085121862254,7.62273527520629));
#32300=CARTESIAN_POINT('Ctrl Pts',(0.195972737157262,2.44162210568095,7.62377619823514));
#32301=CARTESIAN_POINT('Ctrl Pts',(0.177554037329464,2.45094081242855,7.62481712126399));
#32302=CARTESIAN_POINT('Ctrl Pts',(0.15912587813748,2.46026430502106,7.62585857888378));
#32303=CARTESIAN_POINT('Ctrl Pts',(0.139958664206744,2.4681337808081,7.62690003650358));
#32304=CARTESIAN_POINT('Ctrl Pts',(0.120307826235156,2.47444748222758,7.62794149412337));
#32305=CARTESIAN_POINT('Ctrl Pts',(0.100650984075859,2.4807631127581,7.62898326995387));
#32306=CARTESIAN_POINT('Ctrl Pts',(0.0805109346906823,2.48552183216438,
7.63002504578437));
#32307=CARTESIAN_POINT('Ctrl Pts',(0.0601570805958678,2.48867211844199,
7.63106682161486));
#32308=CARTESIAN_POINT('Ctrl Pts',(0.0397592311835402,2.49182921413488,
7.63211084926746));
#32309=CARTESIAN_POINT('Ctrl Pts',(0.0191473888405084,2.49337088077645,
7.63315487692006));
#32310=CARTESIAN_POINT('Ctrl Pts',(-0.00140442267107771,2.49329749248751,
7.63419890457266));
#32311=CARTESIAN_POINT('Ctrl Pts',(-0.00867332901469911,2.49327153601166,
7.63456816346852));
#32312=CARTESIAN_POINT('Ctrl Pts',(-0.0159347525216559,2.49304402163531,
7.63493742236439));
#32313=CARTESIAN_POINT('Ctrl Pts',(-0.0231767494653366,2.49261651555203,
7.63530668126026));
#32314=CARTESIAN_POINT('Ctrl Pts',(-0.0436512035339527,2.49140787741892,
7.63635064390782));
#32315=CARTESIAN_POINT('Ctrl Pts',(-0.0640918645087113,2.48858975080059,
7.63739460655537));
#32316=CARTESIAN_POINT('Ctrl Pts',(-0.0842260745481705,2.48417555670059,
7.63843856920292));
#32317=CARTESIAN_POINT('Ctrl Pts',(-0.104323245538683,2.47976948298629,
7.63948061136869));
#32318=CARTESIAN_POINT('Ctrl Pts',(-0.124114361287151,2.4737732676065,7.64052265353446));
#32319=CARTESIAN_POINT('Ctrl Pts',(-0.143333338277454,2.46625188619069,
7.64156469570023));
#32320=CARTESIAN_POINT('Ctrl Pts',(-0.162531674388393,2.45873858262037,
7.64260561872908));
#32321=CARTESIAN_POINT('Ctrl Pts',(-0.181158399364075,2.44970360469781,
7.64364654175794));
#32322=CARTESIAN_POINT('Ctrl Pts',(-0.198964109864743,2.43926121644793,
7.64468746478679));
#32323=CARTESIAN_POINT('Ctrl Pts',(-0.216778964914245,2.42881346525962,
7.64572892240658));
#32324=CARTESIAN_POINT('Ctrl Pts',(-0.233771320284392,2.41695721804542,
7.64677038002637));
#32325=CARTESIAN_POINT('Ctrl Pts',(-0.249717347142957,2.40385216230247,
7.64781183764616));
#32326=CARTESIAN_POINT('Ctrl Pts',(-0.265668246207912,2.39074310239365,
7.64885361347666));
#32327=CARTESIAN_POINT('Ctrl Pts',(-0.280571635326441,2.37638496907464,
7.64989538930716));
#32328=CARTESIAN_POINT('Ctrl Pts',(-0.294238361424916,2.36097639101264,
7.65093716513766));
#32329=CARTESIAN_POINT('Ctrl Pts',(-0.307934628462002,2.34553450695947,
7.65198119279025));
#32330=CARTESIAN_POINT('Ctrl Pts',(-0.320388452069471,2.32903823288433,
7.65302522044285));
#32331=CARTESIAN_POINT('Ctrl Pts',(-0.33145181280105,2.31171817539101,7.65406924809545));
#32332=CARTESIAN_POINT('Ctrl Pts',(-0.335364778476012,2.30559229808265,
7.65443850699131));
#32333=CARTESIAN_POINT('Ctrl Pts',(-0.339104220064762,2.29936360554387,
7.65480776588718));
#32334=CARTESIAN_POINT('Ctrl Pts',(-0.342664989095891,2.29304298808274,
7.65517702478305));
#32335=CARTESIAN_POINT('Ctrl Pts',(-0.353181870689793,2.27437477768831,
7.6562676465143));
#32336=CARTESIAN_POINT('Ctrl Pts',(-0.362194639744218,2.25480029445585,
7.65735826824556));
#32337=CARTESIAN_POINT('Ctrl Pts',(-0.369558942677454,2.23457740481642,
7.65844888997681));
#32338=CARTESIAN_POINT('Ctrl Pts',(-0.376903549625527,2.21440860172638,
7.659536594817));
#32339=CARTESIAN_POINT('Ctrl Pts',(-0.382608177514571,2.19359541255137,
7.66062429965719));
#32340=CARTESIAN_POINT('Ctrl Pts',(-0.386575409562742,2.17241783427719,
7.66171200449738));
#32341=CARTESIAN_POINT('Ctrl Pts',(-0.390531598309264,2.15129920652121,
7.66279668157098));
#32342=CARTESIAN_POINT('Ctrl Pts',(-0.392759846853305,2.1298188234893,7.66388135864457));
#32343=CARTESIAN_POINT('Ctrl Pts',(-0.393213048917556,2.10826971347505,
7.66496603571817));
#32344=CARTESIAN_POINT('Ctrl Pts',(-0.393271211437559,2.10550416882927,
7.66510523974429));
#32345=CARTESIAN_POINT('Ctrl Pts',(-0.393300207467801,2.10273750562405,
7.66524444377041));
#32346=CARTESIAN_POINT('Ctrl Pts',(-0.393299998882636,2.09997035343927,
7.66538364779653));
#32347=CARTESIAN_POINT('',(-0.393299846840641,2.09965290472694,7.79038364779653));
#32348=CARTESIAN_POINT('Ctrl Pts',(-0.392654629287079,2.09996998332331,
7.66538366889741));
#32349=CARTESIAN_POINT('Ctrl Pts',(-0.392697384672877,2.03604211742209,
7.66860490203355));
#32350=CARTESIAN_POINT('Ctrl Pts',(-0.347701914019137,1.84072366953728,
7.67844958301063));
#32351=CARTESIAN_POINT('Ctrl Pts',(-0.0400622663258958,1.63667500034933,
7.69491771182861));
#32352=CARTESIAN_POINT('Ctrl Pts',(0.367885526613611,1.81550873512054,7.71478805535143));
#32353=CARTESIAN_POINT('Ctrl Pts',(0.438348431977121,2.2553244754303,7.73465839887419));
#32354=CARTESIAN_POINT('Ctrl Pts',(0.106686326751942,2.55265115505061,7.754528742397));
#32355=CARTESIAN_POINT('Ctrl Pts',(-0.294846097879019,2.4424188008677,7.77310380060152));
#32356=CARTESIAN_POINT('Ctrl Pts',(-0.392480938382109,2.20485551238996,
7.78505541096512));
#32357=CARTESIAN_POINT('Ctrl Pts',(-0.393450074714008,2.09965423931595,
7.79038357348779));
#32358=CARTESIAN_POINT('',(-0.393472008642783,2.10021399309012,7.91538370816546));
#32359=CARTESIAN_POINT('Ctrl Pts',(-0.393299846840641,2.09965290472694,
7.79038364779653));
#32360=CARTESIAN_POINT('Ctrl Pts',(-0.393277285971461,2.0740887813239,7.79167890834521));
#32361=CARTESIAN_POINT('Ctrl Pts',(-0.390760409603109,2.04863121630469,
7.79297416889389));
#32362=CARTESIAN_POINT('Ctrl Pts',(-0.385821589392683,2.02366788907344,
7.79426942944257));
#32363=CARTESIAN_POINT('Ctrl Pts',(-0.381840966476314,2.00354778179849,
7.79531339209014));
#32364=CARTESIAN_POINT('Ctrl Pts',(-0.376270388510308,1.98367994044972,
7.79635735473771));
#32365=CARTESIAN_POINT('Ctrl Pts',(-0.369160215781451,1.96433266758651,
7.79740131738527));
#32366=CARTESIAN_POINT('Ctrl Pts',(-0.36206312298149,1.94502098611651,7.79844335955106));
#32367=CARTESIAN_POINT('Ctrl Pts',(-0.353432252440912,1.92622867558337,
7.79948540171684));
#32368=CARTESIAN_POINT('Ctrl Pts',(-0.343368146843134,1.90821051714572,
7.80052744388263));
#32369=CARTESIAN_POINT('Ctrl Pts',(-0.333314849936666,1.89021170992718,
7.80156836691149));
#32370=CARTESIAN_POINT('Ctrl Pts',(-0.321831705523261,1.87298605743524,
7.80260928994036));
#32371=CARTESIAN_POINT('Ctrl Pts',(-0.309065819745101,1.85676511544335,
7.80365021296923));
#32372=CARTESIAN_POINT('Ctrl Pts',(-0.296293377740715,1.8405358427984,7.80469167058903));
#32373=CARTESIAN_POINT('Ctrl Pts',(-0.282237320642678,1.82531289965662,
7.80573312820884));
#32374=CARTESIAN_POINT('Ctrl Pts',(-0.26708627994932,1.81129633001496,7.80677458582865));
#32375=CARTESIAN_POINT('Ctrl Pts',(-0.251930609952505,1.7972754777002,7.80781636165916));
#32376=CARTESIAN_POINT('Ctrl Pts',(-0.235679854536496,1.78446220536074,
7.80885813748967));
#32377=CARTESIAN_POINT('Ctrl Pts',(-0.21855651124187,1.77301690962103,7.80989991332018));
#32378=CARTESIAN_POINT('Ctrl Pts',(-0.201396155452133,1.76154687461485,
7.81094394097279));
#32379=CARTESIAN_POINT('Ctrl Pts',(-0.183360088888524,1.75145107926569,
7.8119879686254));
#32380=CARTESIAN_POINT('Ctrl Pts',(-0.164696898682035,1.74284482145079,
7.81303199627801));
#32381=CARTESIAN_POINT('Ctrl Pts',(-0.158095972940099,1.7398009008711,7.81340125517379));
#32382=CARTESIAN_POINT('Ctrl Pts',(-0.15141677440106,1.73694286990731,7.81377051406958));
#32383=CARTESIAN_POINT('Ctrl Pts',(-0.144670792145537,1.73427434886245,
7.81413977296536));
#32384=CARTESIAN_POINT('Ctrl Pts',(-0.125598662601031,1.72672995026606,
7.81518373561291));
#32385=CARTESIAN_POINT('Ctrl Pts',(-0.105877971366907,1.72065897044652,
7.81622769826046));
#32386=CARTESIAN_POINT('Ctrl Pts',(-0.0857615729720408,1.71616430259633,
7.81727166090801));
#32387=CARTESIAN_POINT('Ctrl Pts',(-0.0656821808596817,1.71167790317198,
7.81831370307378));
#32388=CARTESIAN_POINT('Ctrl Pts',(-0.0452092235254467,1.70876227640579,
7.81935574523955));
#32389=CARTESIAN_POINT('Ctrl Pts',(-0.0246113511004285,1.70747080185417,
7.82039778740532));
#32390=CARTESIAN_POINT('Ctrl Pts',(-0.00403560046681622,1.70618071432592,
7.82143871043417));
#32391=CARTESIAN_POINT('Ctrl Pts',(0.0166640701210328,1.70651139080553,
7.82247963346302));
#32392=CARTESIAN_POINT('Ctrl Pts',(0.0372133332101566,1.70846448713892,
7.82352055649188));
#32393=CARTESIAN_POINT('Ctrl Pts',(0.0577731498652244,1.71041858653168,
7.82456201411167));
#32394=CARTESIAN_POINT('Ctrl Pts',(0.0781816706999862,1.71399671682075,
7.82560347173146));
#32395=CARTESIAN_POINT('Ctrl Pts',(0.098168585501751,1.71914856069514,7.82664492935125));
#32396=CARTESIAN_POINT('Ctrl Pts',(0.118161607177343,1.72430197868243,7.82768670518174));
#32397=CARTESIAN_POINT('Ctrl Pts',(0.137732063513107,1.73102984895718,7.82872848101224));
#32398=CARTESIAN_POINT('Ctrl Pts',(0.156624648216409,1.7392319171946,7.82977025684274));
#32399=CARTESIAN_POINT('Ctrl Pts',(0.175558069670281,1.74745171438864,7.83081428449533));
#32400=CARTESIAN_POINT('Ctrl Pts',(0.193810043880642,1.75715172563766,7.83185831214793));
#32401=CARTESIAN_POINT('Ctrl Pts',(0.211149061622278,1.76818534725538,7.83290233980053));
#32402=CARTESIAN_POINT('Ctrl Pts',(0.217281644922087,1.77208779459568,7.8332715986964));
#32403=CARTESIAN_POINT('Ctrl Pts',(0.223300299383926,1.77615668051319,7.83364085759228));
#32404=CARTESIAN_POINT('Ctrl Pts',(0.229195761745247,1.78038430451867,7.83401011648815));
#32405=CARTESIAN_POINT('Ctrl Pts',(0.245863315496847,1.79233657323556,7.83505407913571));
#32406=CARTESIAN_POINT('Ctrl Pts',(0.261643070521576,1.80563175244007,7.83609804178326));
#32407=CARTESIAN_POINT('Ctrl Pts',(0.276311637655667,1.82011293546138,7.83714200443081));
#32408=CARTESIAN_POINT('Ctrl Pts',(0.290953220379886,1.8345674787861,7.83818404659658));
#32409=CARTESIAN_POINT('Ctrl Pts',(0.304487113295279,1.85020322641783,7.83922608876235));
#32410=CARTESIAN_POINT('Ctrl Pts',(0.316723008744935,1.86682318783473,7.84026813092811));
#32411=CARTESIAN_POINT('Ctrl Pts',(0.328945763035101,1.88342529967417,7.84130905395697));
#32412=CARTESIAN_POINT('Ctrl Pts',(0.339872830039004,1.90100895447264,7.84234997698582));
#32413=CARTESIAN_POINT('Ctrl Pts',(0.349354319084676,1.91934438913534,7.84339090001467));
#32414=CARTESIAN_POINT('Ctrl Pts',(0.358840677576003,1.93768924039941,7.84443235763446));
#32415=CARTESIAN_POINT('Ctrl Pts',(0.36687962265116,1.95678599669745,7.84547381525425));
#32416=CARTESIAN_POINT('Ctrl Pts',(0.373367138203819,1.97638013869329,7.84651527287404));
#32417=CARTESIAN_POINT('Ctrl Pts',(0.379856635975311,1.99598026755374,7.84755704870454));
#32418=CARTESIAN_POINT('Ctrl Pts',(0.384793563820189,2.01607737538244,7.84859882453503));
#32419=CARTESIAN_POINT('Ctrl Pts',(0.388124015460432,2.03640252659995,7.84964060036553));
#32420=CARTESIAN_POINT('Ctrl Pts',(0.391461665947473,2.05677161109305,7.85068462801812));
#32421=CARTESIAN_POINT('Ctrl Pts',(0.39318584624889,2.07736898915665,7.85172865567072));
#32422=CARTESIAN_POINT('Ctrl Pts',(0.393294503242237,2.09792064446481,7.85277268332331));
#32423=CARTESIAN_POINT('Ctrl Pts',(0.393332933796537,2.10518949556152,7.85314194221919));
#32424=CARTESIAN_POINT('Ctrl Pts',(0.393169748076574,2.11245264946065,7.85351120111507));
#32425=CARTESIAN_POINT('Ctrl Pts',(0.392806406420191,2.11969814903121,7.85388046001095));
#32426=CARTESIAN_POINT('Ctrl Pts',(0.391779172894343,2.14018250566815,7.8549244226585));
#32427=CARTESIAN_POINT('Ctrl Pts',(0.389142214694143,2.16064732695185,7.85596838530606));
#32428=CARTESIAN_POINT('Ctrl Pts',(0.384906537167002,2.18081984685773,7.85701234795361));
#32429=CARTESIAN_POINT('Ctrl Pts',(0.380678651625093,2.20095525723953,7.85805439011938));
#32430=CARTESIAN_POINT('Ctrl Pts',(0.374857975844893,2.22079870943196,7.85909643228515));
#32431=CARTESIAN_POINT('Ctrl Pts',(0.367507126010841,2.24008355482087,7.86013847445092));
#32432=CARTESIAN_POINT('Ctrl Pts',(0.360164170874032,2.25934768858879,7.86117939747978));
#32433=CARTESIAN_POINT('Ctrl Pts',(0.351294537903702,2.27805371222702,7.86222032050863));
#32434=CARTESIAN_POINT('Ctrl Pts',(0.341010277494635,2.29595122006008,7.86326124353749));
#32435=CARTESIAN_POINT('Ctrl Pts',(0.330720735357464,2.31385791958669,7.86430270115728));
#32436=CARTESIAN_POINT('Ctrl Pts',(0.319015466970043,2.33095462777889,7.86534415877707));
#32437=CARTESIAN_POINT('Ctrl Pts',(0.306052170949453,2.34701611011658,7.86638561639686));
#32438=CARTESIAN_POINT('Ctrl Pts',(0.293084914076774,2.36308249993735,7.86742739222736));
#32439=CARTESIAN_POINT('Ctrl Pts',(0.278859354235047,2.37811248486136,7.86846916805786));
#32440=CARTESIAN_POINT('Ctrl Pts',(0.263572436832274,2.39191515983638,7.86951094388836));
#32441=CARTESIAN_POINT('Ctrl Pts',(0.248252476410633,2.40574766960658,7.87055497154096));
#32442=CARTESIAN_POINT('Ctrl Pts',(0.231867162102429,2.41834712419121,7.87159899919356));
#32443=CARTESIAN_POINT('Ctrl Pts',(0.214645780348323,2.42956346729979,7.87264302684616));
#32444=CARTESIAN_POINT('Ctrl Pts',(0.208554803355672,2.43353054083614,7.87301228574201));
#32445=CARTESIAN_POINT('Ctrl Pts',(0.202359478136538,2.43732500780329,7.87338154463787));
#32446=CARTESIAN_POINT('Ctrl Pts',(0.19607064896799,2.4409416234684,7.87375080353373));
#32447=CARTESIAN_POINT('Ctrl Pts',(0.178290975079414,2.45116645950429,7.87479476618128));
#32448=CARTESIAN_POINT('Ctrl Pts',(0.15965635381351,2.46002723537316,7.87583872882884));
#32449=CARTESIAN_POINT('Ctrl Pts',(0.140402089120858,2.4673855513905,7.87688269147639));
#32450=CARTESIAN_POINT('Ctrl Pts',(0.121183244722872,2.47473033099261,7.87792473364216));
#32451=CARTESIAN_POINT('Ctrl Pts',(0.101347677861961,2.4805778218012,7.87896677580793));
#32452=CARTESIAN_POINT('Ctrl Pts',(0.0811534867391165,2.48483633091236,
7.8800088179737));
#32453=CARTESIAN_POINT('Ctrl Pts',(0.0609809838603006,2.48909026645163,
7.88104974100255));
#32454=CARTESIAN_POINT('Ctrl Pts',(0.0404513316745512,2.49175842883664,
7.8820906640314));
#32455=CARTESIAN_POINT('Ctrl Pts',(0.0198357306604741,2.49279948292884,
7.88313158706026));
#32456=CARTESIAN_POINT('Ctrl Pts',(-0.000790457988976343,2.4938410716793,
7.88417304468005));
#32457=CARTESIAN_POINT('Ctrl Pts',(-0.0215019496218682,2.4932538295059,
7.88521450229984));
#32458=CARTESIAN_POINT('Ctrl Pts',(-0.0420239979101587,2.49104842871395,
7.88625595991963));
#32459=CARTESIAN_POINT('Ctrl Pts',(-0.0625523165788904,2.4888423540759,
7.88729773575013));
#32460=CARTESIAN_POINT('Ctrl Pts',(-0.0828903495874746,2.48501725107508,
7.88833951158063));
#32461=CARTESIAN_POINT('Ctrl Pts',(-0.102770970442034,2.47963537458251,
7.88938128741113));
#32462=CARTESIAN_POINT('Ctrl Pts',(-0.122694563709719,2.47424186504177,
7.89042531506373));
#32463=CARTESIAN_POINT('Ctrl Pts',(-0.142158077408814,2.46728511182687,
7.89146934271632));
#32464=CARTESIAN_POINT('Ctrl Pts',(-0.160911224630327,2.45887667490096,
7.89251337036892));
#32465=CARTESIAN_POINT('Ctrl Pts',(-0.167543966990968,2.45590272097597,
7.89288262926479));
#32466=CARTESIAN_POINT('Ctrl Pts',(-0.174088064238261,2.45274759413915,
7.89325188816065));
#32467=CARTESIAN_POINT('Ctrl Pts',(-0.180533236303805,2.44941757338416,
7.89362114705652));
#32468=CARTESIAN_POINT('Ctrl Pts',(-0.198754920246359,2.44000299374183,
7.89466510970407));
#32469=CARTESIAN_POINT('Ctrl Pts',(-0.2162924764411,2.42913116862194,7.89570907235163));
#32470=CARTESIAN_POINT('Ctrl Pts',(-0.232902161675197,2.41692502754914,
7.89675303499918));
#32471=CARTESIAN_POINT('Ctrl Pts',(-0.249481291603513,2.40474134098812,
7.89779507716495));
#32472=CARTESIAN_POINT('Ctrl Pts',(-0.26513531731884,2.39122859366002,7.89883711933072));
#32473=CARTESIAN_POINT('Ctrl Pts',(-0.279647428566151,2.37655416412764,
7.89987916149648));
#32474=CARTESIAN_POINT('Ctrl Pts',(-0.294143954033967,2.36189549470205,
7.90092008452534));
#32475=CARTESIAN_POINT('Ctrl Pts',(-0.307500464414512,2.34607812008314,
7.90196100755419));
#32476=CARTESIAN_POINT('Ctrl Pts',(-0.319535398663865,2.32930769503164,
7.90300193058304));
#32477=CARTESIAN_POINT('Ctrl Pts',(-0.331576513741777,2.31252865712693,
7.90404338820283));
#32478=CARTESIAN_POINT('Ctrl Pts',(-0.342294254661971,2.29479617933626,
7.90508484582262));
#32479=CARTESIAN_POINT('Ctrl Pts',(-0.351548869738086,2.2763470504031,7.90612630344241));
#32480=CARTESIAN_POINT('Ctrl Pts',(-0.360806312502575,2.25789228445674,
7.90716807927291));
#32481=CARTESIAN_POINT('Ctrl Pts',(-0.368599442165857,2.23872110479362,
7.90820985510341));
#32482=CARTESIAN_POINT('Ctrl Pts',(-0.374836003340324,2.21909181583909,
7.90925163093391));
#32483=CARTESIAN_POINT('Ctrl Pts',(-0.381086044983296,2.19942009773105,
7.9102956585865));
#32484=CARTESIAN_POINT('Ctrl Pts',(-0.385772633972532,2.17928901071487,
7.9113396862391));
#32485=CARTESIAN_POINT('Ctrl Pts',(-0.388854087096225,2.15896938992868,
7.91238371389169));
#32486=CARTESIAN_POINT('Ctrl Pts',(-0.389943956675164,2.15178260640108,
7.91275297278756));
#32487=CARTESIAN_POINT('Ctrl Pts',(-0.390833507624469,2.14457228510115,
7.91312223168343));
#32488=CARTESIAN_POINT('Ctrl Pts',(-0.39152245464766,2.1373504686272,7.9134914905793));
#32489=CARTESIAN_POINT('Ctrl Pts',(-0.392699222580031,2.12501511953074,
7.91412220965171));
#32490=CARTESIAN_POINT('Ctrl Pts',(-0.393293155378434,2.11262329265773,
7.91475292872412));
#32491=CARTESIAN_POINT('Ctrl Pts',(-0.393299941186222,2.10021508815424,
7.91538364779652));
#32492=CARTESIAN_POINT('',(-0.393123696123607,2.1002301365466,8.04038359743823));
#32493=CARTESIAN_POINT('Ctrl Pts',(-0.39380310770544,2.10021188592406,7.91538382432977));
#32494=CARTESIAN_POINT('Ctrl Pts',(-0.393024373222605,1.98216613471237,
7.92137649425388));
#32495=CARTESIAN_POINT('Ctrl Pts',(-0.273797281021035,1.73228844719605,
7.93399261201892));
#32496=CARTESIAN_POINT('Ctrl Pts',(0.151435609798601,1.6602929423249,7.95323217762489));
#32497=CARTESIAN_POINT('Ctrl Pts',(0.451688398629209,1.98930839675799,7.97310252114768));
#32498=CARTESIAN_POINT('Ctrl Pts',(0.337578573540234,2.41986832786486,7.99297286467047));
#32499=CARTESIAN_POINT('Ctrl Pts',(-0.0862136355990253,2.55699261429619,
8.01284320819326));
#32500=CARTESIAN_POINT('Ctrl Pts',(-0.360367354736448,2.33262573473897,
8.02864675384896));
#32501=CARTESIAN_POINT('Ctrl Pts',(-0.393056166243688,2.15092736107523,
8.03782685166375));
#32502=CARTESIAN_POINT('Ctrl Pts',(-0.392788426279983,2.10023184074339,
8.0403835016376));
#32503=CARTESIAN_POINT('',(-0.393299872203804,2.09968294405636,8.16538364780065));
#32504=CARTESIAN_POINT('Ctrl Pts',(-0.393299933191821,2.10022924072298,
8.04038364779653));
#32505=CARTESIAN_POINT('Ctrl Pts',(-0.393312109279616,2.0793391717426,8.04143579816531));
#32506=CARTESIAN_POINT('Ctrl Pts',(-0.391655576185796,2.05844602648898,
8.04248794853408));
#32507=CARTESIAN_POINT('Ctrl Pts',(-0.38835514890639,2.03782952213554,8.04354009890286));
#32508=CARTESIAN_POINT('Ctrl Pts',(-0.385053731339344,2.01720683183473,
8.04459256496758));
#32509=CARTESIAN_POINT('Ctrl Pts',(-0.380107581434242,1.99686164941892,
8.04564503103231));
#32510=CARTESIAN_POINT('Ctrl Pts',(-0.373592758590756,1.97706367205521,
8.04669749709703));
#32511=CARTESIAN_POINT('Ctrl Pts',(-0.367060207838806,1.95721182112673,
8.04775282709566));
#32512=CARTESIAN_POINT('Ctrl Pts',(-0.358950717066223,1.93791081977075,
8.04880815709429));
#32513=CARTESIAN_POINT('Ctrl Pts',(-0.349389250212133,1.91941195544499,
8.04986348709293));
#32514=CARTESIAN_POINT('Ctrl Pts',(-0.341173465465354,1.90351662372658,
8.05077028980823));
#32515=CARTESIAN_POINT('Ctrl Pts',(-0.33188659664511,1.88821339649346,8.05167709252353));
#32516=CARTESIAN_POINT('Ctrl Pts',(-0.321633311049409,1.87364429933533,
8.05258389523884));
#32517=CARTESIAN_POINT('Ctrl Pts',(-0.309829147921141,1.85687152948697,
8.05362785788639));
#32518=CARTESIAN_POINT('Ctrl Pts',(-0.296674263106577,1.84097462839784,
8.05467182053395));
#32519=CARTESIAN_POINT('Ctrl Pts',(-0.282323578400054,1.82617836630502,
8.0557157831815));
#32520=CARTESIAN_POINT('Ctrl Pts',(-0.267999293324419,1.8114093235307,8.05675782534727));
#32521=CARTESIAN_POINT('Ctrl Pts',(-0.252484038663387,1.79773746432086,
8.05779986751304));
#32522=CARTESIAN_POINT('Ctrl Pts',(-0.235973111516883,1.78535483375548,
8.05884190967881));
#32523=CARTESIAN_POINT('Ctrl Pts',(-0.219479916846765,1.77298550194081,
8.05988283270766));
#32524=CARTESIAN_POINT('Ctrl Pts',(-0.201993740875486,1.7619031123392,8.06092375573651));
#32525=CARTESIAN_POINT('Ctrl Pts',(-0.183743009992987,1.75225958492186,
8.06196467876536));
#32526=CARTESIAN_POINT('Ctrl Pts',(-0.165482906010769,1.74261110484018,
8.06300613638516));
#32527=CARTESIAN_POINT('Ctrl Pts',(-0.1464581056945,1.73440332121998,8.06404759400495));
#32528=CARTESIAN_POINT('Ctrl Pts',(-0.12692219704885,1.72774250055064,8.06508905162474));
#32529=CARTESIAN_POINT('Ctrl Pts',(-0.107380319331415,1.72107964471019,
8.06613082745523));
#32530=CARTESIAN_POINT('Ctrl Pts',(-0.0873277298967882,1.71596489578267,
8.06717260328573));
#32531=CARTESIAN_POINT('Ctrl Pts',(-0.0670328762866684,1.71245454009015,
8.06821437911623));
#32532=CARTESIAN_POINT('Ctrl Pts',(-0.0466941548899186,1.70893659668415,
8.06925840676883));
#32533=CARTESIAN_POINT('Ctrl Pts',(-0.0261128571950155,1.70703003800371,
8.07030243442142));
#32534=CARTESIAN_POINT('Ctrl Pts',(-0.00556297059209929,1.70673934425347,
8.07134646207402));
#32535=CARTESIAN_POINT('Ctrl Pts',(0.00170525493651206,1.70663652968435,
8.07171572096989));
#32536=CARTESIAN_POINT('Ctrl Pts',(0.00896956935361507,1.70673537394422,
8.07208497986575));
#32537=CARTESIAN_POINT('Ctrl Pts',(0.0162180030620408,1.70703452266557,
8.07245423876162));
#32538=CARTESIAN_POINT('Ctrl Pts',(0.0367106550456766,1.70788027098645,
8.07349820140917));
#32539=CARTESIAN_POINT('Ctrl Pts',(0.0571980309494468,1.71033585387032,
8.07454216405673));
#32540=CARTESIAN_POINT('Ctrl Pts',(0.0774072779671117,1.7143926824894,8.07558612670428));
#32541=CARTESIAN_POINT('Ctrl Pts',(0.0975793478972116,1.71844204813508,
8.07662816887005));
#32542=CARTESIAN_POINT('Ctrl Pts',(0.117473579597926,1.72408672762005,8.07767021103582));
#32543=CARTESIAN_POINT('Ctrl Pts',(0.136822780278586,1.73126646911782,8.07871225320159));
#32544=CARTESIAN_POINT('Ctrl Pts',(0.156151200221679,1.73843849968602,8.07975317623044));
#32545=CARTESIAN_POINT('Ctrl Pts',(0.174935054830473,1.74714209178445,8.0807940992593));
#32546=CARTESIAN_POINT('Ctrl Pts',(0.192922955740864,1.75726741744006,8.08183502228815));
#32547=CARTESIAN_POINT('Ctrl Pts',(0.210920094768347,1.76739794319902,8.08287647990794));
#32548=CARTESIAN_POINT('Ctrl Pts',(0.228119814359035,1.77895131435342,8.08391793752773));
#32549=CARTESIAN_POINT('Ctrl Pts',(0.244295491977069,1.79177183353937,8.08495939514752));
#32550=CARTESIAN_POINT('Ctrl Pts',(0.260476111969821,1.80459626995287,8.08600117097802));
#32551=CARTESIAN_POINT('Ctrl Pts',(0.275631513432774,1.81868814016664,8.08704294680852));
#32552=CARTESIAN_POINT('Ctrl Pts',(0.289569054313693,1.83385219748442,8.08808472263902));
#32553=CARTESIAN_POINT('Ctrl Pts',(0.303536721505506,1.8490490322562,8.08912875029162));
#32554=CARTESIAN_POINT('Ctrl Pts',(0.316280818502472,1.86532210119047,8.09017277794421));
#32555=CARTESIAN_POINT('Ctrl Pts',(0.327649263943418,1.88244345599974,8.09121680559681));
#32556=CARTESIAN_POINT('Ctrl Pts',(0.331670134081134,1.88849905477333,8.09158606449268));
#32557=CARTESIAN_POINT('Ctrl Pts',(0.335519328709527,1.89466052658222,8.09195532338855));
#32558=CARTESIAN_POINT('Ctrl Pts',(0.339191507245826,1.90091707403118,8.09232458228442));
#32559=CARTESIAN_POINT('Ctrl Pts',(0.349573429712498,1.91860548157514,8.09336854493197));
#32560=CARTESIAN_POINT('Ctrl Pts',(0.358598918418144,1.9371608854335,8.09441250757953));
#32561=CARTESIAN_POINT('Ctrl Pts',(0.366127494848793,1.95634921679383,8.09545647022708));
#32562=CARTESIAN_POINT('Ctrl Pts',(0.373642221651847,1.97550224915096,8.09649851239285));
#32563=CARTESIAN_POINT('Ctrl Pts',(0.379665181161932,1.995285242357,8.09754055455862));
#32564=CARTESIAN_POINT('Ctrl Pts',(0.384102397908064,2.01544092052727,8.09858259672439));
#32565=CARTESIAN_POINT('Ctrl Pts',(0.388534849153124,2.03557495181586,8.09962351975324));
#32566=CARTESIAN_POINT('Ctrl Pts',(0.391384752986762,2.05608016475114,8.1006644427821));
#32567=CARTESIAN_POINT('Ctrl Pts',(0.39260837367134,2.07668573562933,8.10170536581095));
#32568=CARTESIAN_POINT('Ctrl Pts',(0.393832622775608,2.09730188899165,8.10274682343074));
#32569=CARTESIAN_POINT('Ctrl Pts',(0.393428860446642,2.11801776973594,8.10378828105053));
#32570=CARTESIAN_POINT('Ctrl Pts',(0.391405324942168,2.13855854778018,8.10482973867033));
#32571=CARTESIAN_POINT('Ctrl Pts',(0.389381171159378,2.15910560192761,8.10587151450082));
#32572=CARTESIAN_POINT('Ctrl Pts',(0.38573636702999,2.17947671879645,8.10691329033132));
#32573=CARTESIAN_POINT('Ctrl Pts',(0.380530798848308,2.19940423093545,8.10795506616182));
#32574=CARTESIAN_POINT('Ctrl Pts',(0.375313978712872,2.21937481684416,8.10899909381441));
#32575=CARTESIAN_POINT('Ctrl Pts',(0.368529900969318,2.23889918802424,8.11004312146701));
#32576=CARTESIAN_POINT('Ctrl Pts',(0.360287904230309,2.25772607921752,8.11108714911961));
#32577=CARTESIAN_POINT('Ctrl Pts',(0.357372818017805,2.26438490385428,8.11145640801547));
#32578=CARTESIAN_POINT('Ctrl Pts',(0.354275780806462,2.27095669163608,8.11182566691134));
#32579=CARTESIAN_POINT('Ctrl Pts',(0.351002980285546,2.27743110728016,8.1121949258072));
#32580=CARTESIAN_POINT('Ctrl Pts',(0.341750172743193,2.29573546818485,8.11323888845475));
#32581=CARTESIAN_POINT('Ctrl Pts',(0.331034117072615,2.31336863606777,8.11428285110231));
#32582=CARTESIAN_POINT('Ctrl Pts',(0.318975578964254,2.33008578840167,8.11532681374986));
#32583=CARTESIAN_POINT('Ctrl Pts',(0.306939223836122,2.34677218773249,8.11636885591563));
#32584=CARTESIAN_POINT('Ctrl Pts',(0.29356566575696,2.36254529160438,8.1174108980814));
#32585=CARTESIAN_POINT('Ctrl Pts',(0.279020356276489,2.37718681567373,8.11845294024717));
#32586=CARTESIAN_POINT('Ctrl Pts',(0.264490668229895,2.39181261497624,8.11949386327603));
#32587=CARTESIAN_POINT('Ctrl Pts',(0.248792222500366,2.40530870741288,8.12053478630488));
#32588=CARTESIAN_POINT('Ctrl Pts',(0.23212905756193,2.41749171742805,8.12157570933374));
#32589=CARTESIAN_POINT('Ctrl Pts',(0.215457334856286,2.42968098431962,8.12261716695353));
#32590=CARTESIAN_POINT('Ctrl Pts',(0.197820487577217,2.44055537428341,8.12365862457332));
#32591=CARTESIAN_POINT('Ctrl Pts',(0.179454057296113,2.44997304370475,8.12470008219311));
#32592=CARTESIAN_POINT('Ctrl Pts',(0.161082015269849,2.45939359063467,8.12574185802361));
#32593=CARTESIAN_POINT('Ctrl Pts',(0.141980617141569,2.46735622770853,8.12678363385411));
#32594=CARTESIAN_POINT('Ctrl Pts',(0.12240734002988,2.47376641516703,8.12782540968461));
#32595=CARTESIAN_POINT('Ctrl Pts',(0.102791754835532,2.48019045839118,8.12886943733721));
#32596=CARTESIAN_POINT('Ctrl Pts',(0.0827029701123902,2.48505517926245,
8.1299134649898));
#32597=CARTESIAN_POINT('Ctrl Pts',(0.0624114411549417,2.48831649721968,
8.1309574926424));
#32598=CARTESIAN_POINT('Ctrl Pts',(0.0552345933390587,2.4894699826326,8.13132675153827));
#32599=CARTESIAN_POINT('Ctrl Pts',(0.0480324343058591,2.49042336576572,
8.13169601043413));
#32600=CARTESIAN_POINT('Ctrl Pts',(0.0408170036541203,2.49117625466367,
8.13206526933));
#32601=CARTESIAN_POINT('Ctrl Pts',(0.0204176573668355,2.49330480971277,
8.13310923197755));
#32602=CARTESIAN_POINT('Ctrl Pts',(-0.000209420461472831,2.49383971062672,
8.13415319462511));
#32603=CARTESIAN_POINT('Ctrl Pts',(-0.0207930060161651,2.49274997250262,
8.13519715727266));
#32604=CARTESIAN_POINT('Ctrl Pts',(-0.0413387258472349,2.49166223906923,
8.13623919943843));
#32605=CARTESIAN_POINT('Ctrl Pts',(-0.0618403826235695,2.48895577811871,
8.1372812416042));
#32606=CARTESIAN_POINT('Ctrl Pts',(-0.0820248770474154,2.484651543017,8.13832328376997));
#32607=CARTESIAN_POINT('Ctrl Pts',(-0.102187693641291,2.48035193059618,
8.13936420679882));
#32608=CARTESIAN_POINT('Ctrl Pts',(-0.122033302127519,2.47445807505066,
8.14040512982768));
#32609=CARTESIAN_POINT('Ctrl Pts',(-0.141297067342993,2.46704227108096,
8.14144605285653));
#32610=CARTESIAN_POINT('Ctrl Pts',(-0.160570725926243,2.45962265854761,
8.14248751047632));
#32611=CARTESIAN_POINT('Ctrl Pts',(-0.179261251816834,2.45067978535362,
8.14352896809611));
#32612=CARTESIAN_POINT('Ctrl Pts',(-0.19712187745538,2.44033491655789,8.14457042571591));
#32613=CARTESIAN_POINT('Ctrl Pts',(-0.214987960293711,2.42998688695375,
8.1456122015464));
#32614=CARTESIAN_POINT('Ctrl Pts',(-0.232023020058744,2.41823640873251,
8.1466539773769));
#32615=CARTESIAN_POINT('Ctrl Pts',(-0.248008189011547,2.40524879718553,
8.1476957532074));
#32616=CARTESIAN_POINT('Ctrl Pts',(-0.264027910269793,2.39223311262146,
8.14873978086));
#32617=CARTESIAN_POINT('Ctrl Pts',(-0.278992676830141,2.37797546405646,
8.14978380851259));
#32618=CARTESIAN_POINT('Ctrl Pts',(-0.292719022629805,2.36267939354021,
8.15082783616519));
#32619=CARTESIAN_POINT('Ctrl Pts',(-0.297573851217542,2.35726937389579,
8.15119709506105));
#32620=CARTESIAN_POINT('Ctrl Pts',(-0.302274131644997,2.35172975314699,
8.15156635395692));
#32621=CARTESIAN_POINT('Ctrl Pts',(-0.306813017096715,2.34607044223151,
8.15193561285278));
#32622=CARTESIAN_POINT('Ctrl Pts',(-0.31961886759936,2.3301034630463,8.15297742681074));
#32623=CARTESIAN_POINT('Ctrl Pts',(-0.331215043950816,2.31308411630537,
8.15401924076871));
#32624=CARTESIAN_POINT('Ctrl Pts',(-0.341428155603478,2.29522219279889,
8.15506105472667));
#32625=CARTESIAN_POINT('Ctrl Pts',(-0.351620131549464,2.27739723396966,
8.15610071268409));
#32626=CARTESIAN_POINT('Ctrl Pts',(-0.360434309648539,2.25873376402489,
8.15714037064152));
#32627=CARTESIAN_POINT('Ctrl Pts',(-0.367739873823155,2.23947141356038,
8.15818002859894));
#32628=CARTESIAN_POINT('Ctrl Pts',(-0.375036810917241,2.2202318098468,8.15921845883285));
#32629=CARTESIAN_POINT('Ctrl Pts',(-0.380828381163626,2.20039540589499,
8.16025688906676));
#32630=CARTESIAN_POINT('Ctrl Pts',(-0.385031436584233,2.18022270776957,
8.16129531930067));
#32631=CARTESIAN_POINT('Ctrl Pts',(-0.389234429074351,2.16005031168103,
8.16233373398663));
#32632=CARTESIAN_POINT('Ctrl Pts',(-0.391848790948663,2.13954235110016,
8.16337214867258));
#32633=CARTESIAN_POINT('Ctrl Pts',(-0.392842214006138,2.11897063242898,
8.16441056335854));
#32634=CARTESIAN_POINT('Ctrl Pts',(-0.393152521802127,2.11254480545373,
8.16473492483786));
#32635=CARTESIAN_POINT('Ctrl Pts',(-0.393305055583653,2.10611279720991,
8.16505928631719));
#32636=CARTESIAN_POINT('Ctrl Pts',(-0.39329987220387,2.09968294413829,8.16538364779652));
#32637=CARTESIAN_POINT('',(-0.393299992164447,2.09992149238468,8.29038364779182));
#32638=CARTESIAN_POINT('Ctrl Pts',(-0.393299872203804,2.09968294405636,
8.16538364780065));
#32639=CARTESIAN_POINT('Ctrl Pts',(-0.393280180214925,2.07525553033001,
8.16661591733532));
#32640=CARTESIAN_POINT('Ctrl Pts',(-0.390980683010069,2.05092561102102,
8.16784818686999));
#32641=CARTESIAN_POINT('Ctrl Pts',(-0.386479320274873,2.0270710962658,8.16908045640465));
#32642=CARTESIAN_POINT('Ctrl Pts',(-0.383160656714444,2.0094841756982,8.16998895639496));
#32643=CARTESIAN_POINT('Ctrl Pts',(-0.378646245086477,1.99215525616916,
8.17089745638527));
#32644=CARTESIAN_POINT('Ctrl Pts',(-0.372983863481854,1.97522849851769,
8.17180595637558));
#32645=CARTESIAN_POINT('Ctrl Pts',(-0.366477187692725,1.95577786239148,
8.17284991902312));
#32646=CARTESIAN_POINT('Ctrl Pts',(-0.358425539429026,1.93677961460506,
8.17389388167067));
#32647=CARTESIAN_POINT('Ctrl Pts',(-0.348912986099889,1.91849347634077,
8.17493784431822));
#32648=CARTESIAN_POINT('Ctrl Pts',(-0.339417932137639,1.90024097739826,
8.17597988648398));
#32649=CARTESIAN_POINT('Ctrl Pts',(-0.328467590641094,1.88269866048875,
8.17702192864974));
#32650=CARTESIAN_POINT('Ctrl Pts',(-0.316194084772954,1.8661064542263,8.17806397081551));
#32651=CARTESIAN_POINT('Ctrl Pts',(-0.303933760457306,1.84953206773273,
8.17910489384435));
#32652=CARTESIAN_POINT('Ctrl Pts',(-0.290353505003252,1.83390637187051,
8.1801458168732));
#32653=CARTESIAN_POINT('Ctrl Pts',(-0.275628673858284,1.81944033763364,
8.18118673990205));
#32654=CARTESIAN_POINT('Ctrl Pts',(-0.260896280423819,1.80496687401863,
8.18222819752183));
#32655=CARTESIAN_POINT('Ctrl Pts',(-0.245018650525355,1.79165478898914,
8.18326965514162));
#32656=CARTESIAN_POINT('Ctrl Pts',(-0.228208321034623,1.77967851740703,
8.1843111127614));
#32657=CARTESIAN_POINT('Ctrl Pts',(-0.211392855255364,1.76769858655183,
8.18535288859189));
#32658=CARTESIAN_POINT('Ctrl Pts',(-0.19364474229533,1.75705567877349,8.18639466442239));
#32659=CARTESIAN_POINT('Ctrl Pts',(-0.175205068829557,1.74788059715995,
8.18743644025288));
#32660=CARTESIAN_POINT('Ctrl Pts',(-0.156725537591138,1.73868568339931,
8.18848046790547));
#32661=CARTESIAN_POINT('Ctrl Pts',(-0.137552144677004,1.73096520511339,
8.18952449555806));
#32662=CARTESIAN_POINT('Ctrl Pts',(-0.117946120068504,1.72480191530235,
8.19056852321065));
#32663=CARTESIAN_POINT('Ctrl Pts',(-0.11101172615467,1.72262204048283,8.19093778210655));
#32664=CARTESIAN_POINT('Ctrl Pts',(-0.104023331508305,1.72063649914217,
8.19130704100246));
#32665=CARTESIAN_POINT('Ctrl Pts',(-0.0969927922902984,1.71884742130778,
8.19167629989836));
#32666=CARTESIAN_POINT('Ctrl Pts',(-0.0771161680107532,1.71378937002345,
8.19272026254591));
#32667=CARTESIAN_POINT('Ctrl Pts',(-0.0567835984306736,1.71027524524002,
8.19376422519347));
#32668=CARTESIAN_POINT('Ctrl Pts',(-0.0362589689778868,1.70837495334356,
8.19480818784102));
#32669=CARTESIAN_POINT('Ctrl Pts',(-0.0157720967926314,1.70647815723881,
8.19585023000679));
#32670=CARTESIAN_POINT('Ctrl Pts',(0.00490541506159886,1.70618942731558,
8.19689227217256));
#32671=CARTESIAN_POINT('Ctrl Pts',(0.025500309655024,1.70752754974712,8.19793431433833));
#32672=CARTESIAN_POINT('Ctrl Pts',(0.0460730856551914,1.70886423505619,
8.19897523736719));
#32673=CARTESIAN_POINT('Ctrl Pts',(0.0665626881616451,1.71182428547951,
8.20001616039604));
#32674=CARTESIAN_POINT('Ctrl Pts',(0.0866968059131255,1.71637446142825,
8.20105708342489));
#32675=CARTESIAN_POINT('Ctrl Pts',(0.106841264022724,1.72092697422877,8.20209854104468));
#32676=CARTESIAN_POINT('Ctrl Pts',(0.126629151414903,1.72707109756612,8.20313999866448));
#32677=CARTESIAN_POINT('Ctrl Pts',(0.145798750085708,1.73472255137574,8.20418145628427));
#32678=CARTESIAN_POINT('Ctrl Pts',(0.164974205904633,1.74237634303809,8.20522323211477));
#32679=CARTESIAN_POINT('Ctrl Pts',(0.183530327552762,1.7515380758985,8.20626500794527));
#32680=CARTESIAN_POINT('Ctrl Pts',(0.201226628878443,1.76207584603906,8.20730678377577));
#32681=CARTESIAN_POINT('Ctrl Pts',(0.218961181161015,1.77263639380891,8.20835081142836));
#32682=CARTESIAN_POINT('Ctrl Pts',(0.235831601559906,1.78457849146271,8.20939483908096));
#32683=CARTESIAN_POINT('Ctrl Pts',(0.251626901361927,1.79772728784921,8.21043886673356));
#32684=CARTESIAN_POINT('Ctrl Pts',(0.25721349186098,1.80237784477991,8.21080812562942));
#32685=CARTESIAN_POINT('Ctrl Pts',(0.262665914863867,1.80717900271683,8.21117738452529));
#32686=CARTESIAN_POINT('Ctrl Pts',(0.267975961451293,1.81212194580994,8.21154664342115));
#32687=CARTESIAN_POINT('Ctrl Pts',(0.28298843740279,1.82609655282952,8.2125906060687));
#32688=CARTESIAN_POINT('Ctrl Pts',(0.29694956373887,1.84129028213312,8.21363456871626));
#32689=CARTESIAN_POINT('Ctrl Pts',(0.309657715968291,1.85751909571824,8.21467853136381));
#32690=CARTESIAN_POINT('Ctrl Pts',(0.322342490182303,1.87371805465201,8.21572057352958));
#32691=CARTESIAN_POINT('Ctrl Pts',(0.333778370256915,1.89094778211271,8.21676261569535));
#32692=CARTESIAN_POINT('Ctrl Pts',(0.343801641527771,1.90898868807631,8.21780465786112));
#32693=CARTESIAN_POINT('Ctrl Pts',(0.353814147962746,1.92701021839032,8.21884558088998));
#32694=CARTESIAN_POINT('Ctrl Pts',(0.362416676629305,1.94584057181033,8.21988650391883));
#32695=CARTESIAN_POINT('Ctrl Pts',(0.369489768962802,1.96523279096229,8.22092742694769));
#32696=CARTESIAN_POINT('Ctrl Pts',(0.376566493852174,1.98463496945257,8.22196888456748));
#32697=CARTESIAN_POINT('Ctrl Pts',(0.38211194593321,2.00459890444163,8.22301034218727));
#32698=CARTESIAN_POINT('Ctrl Pts',(0.386055316708674,2.02485891642407,8.22405179980707));
#32699=CARTESIAN_POINT('Ctrl Pts',(0.389999892355826,2.04512511872342,8.22509357563757));
#32700=CARTESIAN_POINT('Ctrl Pts',(0.392341307267576,2.06568684958046,8.22613535146806));
#32701=CARTESIAN_POINT('Ctrl Pts',(0.393060289120565,2.08627050195899,8.22717712729856));
#32702=CARTESIAN_POINT('Ctrl Pts',(0.393780825069144,2.10689864636923,8.22822115495116));
#32703=CARTESIAN_POINT('Ctrl Pts',(0.392871958936984,2.12754807113513,8.22926518260376));
#32704=CARTESIAN_POINT('Ctrl Pts',(0.390366496699893,2.14794672308148,8.23030921025636));
#32705=CARTESIAN_POINT('Ctrl Pts',(0.389480347547631,2.15516145889428,8.23067846915222));
#32706=CARTESIAN_POINT('Ctrl Pts',(0.388394943082999,2.16234490731996,8.23104772804808));
#32707=CARTESIAN_POINT('Ctrl Pts',(0.387113252194205,2.16948539397331,8.23141698694394));
#32708=CARTESIAN_POINT('Ctrl Pts',(0.383489676896194,2.18967285982725,8.23246094959149));
#32709=CARTESIAN_POINT('Ctrl Pts',(0.378271927210641,2.20963626502126,8.23350491223904));
#32710=CARTESIAN_POINT('Ctrl Pts',(0.371505602604905,2.22910645697705,8.2345488748866));
#32711=CARTESIAN_POINT('Ctrl Pts',(0.364751725382394,2.2485408314167,8.23559091705236));
#32712=CARTESIAN_POINT('Ctrl Pts',(0.356455110563429,2.26748308693169,8.23663295921813));
#32713=CARTESIAN_POINT('Ctrl Pts',(0.346711771665886,2.28567670125329,8.2376750013839));
#32714=CARTESIAN_POINT('Ctrl Pts',(0.336978896961253,2.30385077591892,8.23871592441276));
#32715=CARTESIAN_POINT('Ctrl Pts',(0.32580270286489,2.32127714659387,8.23975684744161));
#32716=CARTESIAN_POINT('Ctrl Pts',(0.313326170479009,2.33772168788934,8.24079777047046));
#32717=CARTESIAN_POINT('Ctrl Pts',(0.300843230471275,2.35417467467263,8.24183922809025));
#32718=CARTESIAN_POINT('Ctrl Pts',(0.287059049901972,2.36964422880525,8.24288068571004));
#32719=CARTESIAN_POINT('Ctrl Pts',(0.27215868693709,2.38392699611815,8.24392214332984));
#32720=CARTESIAN_POINT('Ctrl Pts',(0.257253771261723,2.39821412743915,8.24496391916033));
#32721=CARTESIAN_POINT('Ctrl Pts',(0.241232550010455,2.41131326745835,8.24600569499083));
#32722=CARTESIAN_POINT('Ctrl Pts',(0.224314644421214,2.42306010322877,8.24704747082133));
#32723=CARTESIAN_POINT('Ctrl Pts',(0.207360170395124,2.43483233005128,8.24809149847393));
#32724=CARTESIAN_POINT('Ctrl Pts',(0.189505778677255,2.44524604587189,8.24913552612652));
#32725=CARTESIAN_POINT('Ctrl Pts',(0.170997974915739,2.45418156724301,8.25017955377912));
#32726=CARTESIAN_POINT('Ctrl Pts',(0.164452007320945,2.4573419440274,8.25054881267499));
#32727=CARTESIAN_POINT('Ctrl Pts',(0.157824486220507,2.46031784694963,8.25091807157086));
#32728=CARTESIAN_POINT('Ctrl Pts',(0.151126834759383,2.46310545274839,8.25128733046673));
#32729=CARTESIAN_POINT('Ctrl Pts',(0.132191345242563,2.47098652579104,8.25233129311428));
#32730=CARTESIAN_POINT('Ctrl Pts',(0.112581294539392,2.4774059003822,8.25337525576184));
#32731=CARTESIAN_POINT('Ctrl Pts',(0.0925476747723407,2.48225622021654,
8.25441921840939));
#32732=CARTESIAN_POINT('Ctrl Pts',(0.0725509090075942,2.48709761736488,
8.25546126057516));
#32733=CARTESIAN_POINT('Ctrl Pts',(0.0521328139093224,2.49037546025442,
8.25650330274093));
#32734=CARTESIAN_POINT('Ctrl Pts',(0.0315610518460417,2.49203161863091,
8.2575453449067));
#32735=CARTESIAN_POINT('Ctrl Pts',(0.0110113835320483,2.49368599831932,
8.25858626793556));
#32736=CARTESIAN_POINT('Ctrl Pts',(-0.00969089674527533,2.49372206354111,
8.25962719096441));
#32737=CARTESIAN_POINT('Ctrl Pts',(-0.0302715339130159,2.49213329906366,
8.26066811399327));
#32738=CARTESIAN_POINT('Ctrl Pts',(-0.0508627407596095,2.49054371863819,
8.26170957161306));
#32739=CARTESIAN_POINT('Ctrl Pts',(-0.0713314448536748,2.48732768198734,
8.26275102923285));
#32740=CARTESIAN_POINT('Ctrl Pts',(-0.0914064870398968,2.48253071004434,
8.26379248685264));
#32741=CARTESIAN_POINT('Ctrl Pts',(-0.111487663026712,2.47773227241727,
8.26483426268314));
#32742=CARTESIAN_POINT('Ctrl Pts',(-0.13117423103532,2.47135214391792,8.26587603851364));
#32743=CARTESIAN_POINT('Ctrl Pts',(-0.150209148853575,2.46348604044816,
8.26691781434414));
#32744=CARTESIAN_POINT('Ctrl Pts',(-0.169285211078648,2.45560293421725,
8.26796184199674));
#32745=CARTESIAN_POINT('Ctrl Pts',(-0.187706154637065,2.44622777452656,
8.26900586964933));
#32746=CARTESIAN_POINT('Ctrl Pts',(-0.205237909581819,2.43550304092584,
8.27004989730193));
#32747=CARTESIAN_POINT('Ctrl Pts',(-0.211438661503814,2.43170984322845,
8.27041915619779));
#32748=CARTESIAN_POINT('Ctrl Pts',(-0.217528450885799,2.42774821484854,
8.27078841509366));
#32749=CARTESIAN_POINT('Ctrl Pts',(-0.223497879506443,2.42362569097048,
8.27115767398952));
#32750=CARTESIAN_POINT('Ctrl Pts',(-0.24028556491258,2.41203201285784,8.27219613220238));
#32751=CARTESIAN_POINT('Ctrl Pts',(-0.256221330552324,2.39909216363466,
8.27323459041524));
#32752=CARTESIAN_POINT('Ctrl Pts',(-0.271080375257495,2.38495669872852,
8.2742730486281));
#32753=CARTESIAN_POINT('Ctrl Pts',(-0.285912087438807,2.37084723535475,
8.27530959664522));
#32754=CARTESIAN_POINT('Ctrl Pts',(-0.299670433632189,2.35554698333978,
8.27634614466234));
#32755=CARTESIAN_POINT('Ctrl Pts',(-0.312162814572205,2.33924729298021,
8.27738269267946));
#32756=CARTESIAN_POINT('Ctrl Pts',(-0.325220007064758,2.32221065315824,
8.27846610560549));
#32757=CARTESIAN_POINT('Ctrl Pts',(-0.336893256897875,2.30408251658651,
8.27954951853152));
#32758=CARTESIAN_POINT('Ctrl Pts',(-0.347008653253265,2.28512126989451,
8.28063293145755));
#32759=CARTESIAN_POINT('Ctrl Pts',(-0.356681299088095,2.26698995626181,
8.28166892344029));
#32760=CARTESIAN_POINT('Ctrl Pts',(-0.36492945832098,2.24809776107575,8.28270491542302));
#32761=CARTESIAN_POINT('Ctrl Pts',(-0.371647986438992,2.22869601460746,
8.28374090740576));
#32762=CARTESIAN_POINT('Ctrl Pts',(-0.378369177488813,2.20928657813223,
8.28477731001057));
#32763=CARTESIAN_POINT('Ctrl Pts',(-0.383559328269682,2.18936790464986,
8.28581371261539));
#32764=CARTESIAN_POINT('Ctrl Pts',(-0.387163296964183,2.16920600757033,
8.2868501152202));
#32765=CARTESIAN_POINT('Ctrl Pts',(-0.390774685009338,2.14900260397478,
8.28788865142689));
#32766=CARTESIAN_POINT('Ctrl Pts',(-0.392793313258072,2.12855571880385,
8.28892718763358));
#32767=CARTESIAN_POINT('Ctrl Pts',(-0.393215829492166,2.10813642653673,
8.28996572384026));
#32768=CARTESIAN_POINT('Ctrl Pts',(-0.393272505306007,2.10539740750289,
8.29010503182411));
#32769=CARTESIAN_POINT('Ctrl Pts',(-0.393300538581425,2.10265888024152,
8.29024433980797));
#32770=CARTESIAN_POINT('Ctrl Pts',(-0.393299992164447,2.09992149238468,
8.29038364779182));
#32771=CARTESIAN_POINT('',(-0.393299835176423,2.10036006971291,8.41538364626984));
#32772=CARTESIAN_POINT('Ctrl Pts',(-0.393299992164429,2.09992149229233,
8.29038364779652));
#32773=CARTESIAN_POINT('Ctrl Pts',(-0.393299149678696,2.09570089227957,
8.29059843770178));
#32774=CARTESIAN_POINT('Ctrl Pts',(-0.39323037085516,2.09148104825922,8.29081322760705));
#32775=CARTESIAN_POINT('Ctrl Pts',(-0.393093715813908,2.08726341538659,
8.29102801751231));
#32776=CARTESIAN_POINT('Ctrl Pts',(-0.392429519056185,2.06676407592866,
8.29207198015986));
#32777=CARTESIAN_POINT('Ctrl Pts',(-0.390155504155932,2.04625575286325,
8.29311594280742));
#32778=CARTESIAN_POINT('Ctrl Pts',(-0.386277842747431,2.02601136436999,
8.29415990545497));
#32779=CARTESIAN_POINT('Ctrl Pts',(-0.382407314714933,2.00580421761081,
8.29520194762074));
#32780=CARTESIAN_POINT('Ctrl Pts',(-0.376939074411953,1.98586076732159,
8.29624398978651));
#32781=CARTESIAN_POINT('Ctrl Pts',(-0.369931004579584,1.96644872950533,
8.29728603195228));
#32782=CARTESIAN_POINT('Ctrl Pts',(-0.362930461304121,1.94705753991273,
8.29832695498113));
#32783=CARTESIAN_POINT('Ctrl Pts',(-0.354393592969436,1.92819732813193,
8.29936787800998));
#32784=CARTESIAN_POINT('Ctrl Pts',(-0.344427996509661,1.91012044549152,
8.30040880103884));
#32785=CARTESIAN_POINT('Ctrl Pts',(-0.33445728197928,1.89203427903532,8.30145025865863));
#32786=CARTESIAN_POINT('Ctrl Pts',(-0.323056714546065,1.87473289755203,
8.30249171627842));
#32787=CARTESIAN_POINT('Ctrl Pts',(-0.310379978104497,1.85844429381227,
8.30353317389821));
#32788=CARTESIAN_POINT('Ctrl Pts',(-0.297699368367291,1.84215071319395,
8.30457494972871));
#32789=CARTESIAN_POINT('Ctrl Pts',(-0.283742293442603,1.82687108429887,
8.3056167255592));
#32790=CARTESIAN_POINT('Ctrl Pts',(-0.268702285995754,1.81279977106441,
8.3066585013897));
#32791=CARTESIAN_POINT('Ctrl Pts',(-0.253629769231506,1.79869804236707,
8.3077025290423));
#32792=CARTESIAN_POINT('Ctrl Pts',(-0.237470222471159,1.78581030287142,
8.30874655669489));
#32793=CARTESIAN_POINT('Ctrl Pts',(-0.220450237964016,1.77429064707686,
8.30979058434749));
#32794=CARTESIAN_POINT('Ctrl Pts',(-0.214430492537541,1.7702162958191,8.31015984324336));
#32795=CARTESIAN_POINT('Ctrl Pts',(-0.208303357573862,1.76631267554095,
8.31052910213923));
#32796=CARTESIAN_POINT('Ctrl Pts',(-0.202079582739162,1.7625852222561,8.3108983610351));
#32797=CARTESIAN_POINT('Ctrl Pts',(-0.184483829388642,1.75204702793388,
8.31194232368265));
#32798=CARTESIAN_POINT('Ctrl Pts',(-0.166009098811989,1.74285753453965,
8.3129862863302));
#32799=CARTESIAN_POINT('Ctrl Pts',(-0.146888206318207,1.73515928839476,
8.31403024897776));
#32800=CARTESIAN_POINT('Ctrl Pts',(-0.127802488766564,1.72747520400318,
8.31507229114353));
#32801=CARTESIAN_POINT('Ctrl Pts',(-0.108073621407342,1.72127724835857,
8.3161143333093));
#32802=CARTESIAN_POINT('Ctrl Pts',(-0.0879580376227832,1.71666167212559,
8.31715637547507));
#32803=CARTESIAN_POINT('Ctrl Pts',(-0.0678640576591956,1.71205105294898,
8.31819729850392));
#32804=CARTESIAN_POINT('Ctrl Pts',(-0.0473848928324123,1.7090196312728,
8.31923822153277));
#32805=CARTESIAN_POINT('Ctrl Pts',(-0.0267909688223041,1.70761354000225,
8.32027914456163));
#32806=CARTESIAN_POINT('Ctrl Pts',(-0.00618646830957055,1.70620672659988,
8.32132060218142));
#32807=CARTESIAN_POINT('Ctrl Pts',(0.0145321761589518,1.70642697740485,
8.32236205980121));
#32808=CARTESIAN_POINT('Ctrl Pts',(0.03509007231069,1.70826848885336,8.323403517421));
#32809=CARTESIAN_POINT('Ctrl Pts',(0.0556542497959508,1.7101105629639,8.3244452932515));
#32810=CARTESIAN_POINT('Ctrl Pts',(0.0760568521883709,1.71357478224715,
8.325487069082));
#32811=CARTESIAN_POINT('Ctrl Pts',(0.0960296920807883,1.71860363368424,
8.3265288449125));
#32812=CARTESIAN_POINT('Ctrl Pts',(0.116045703719874,1.72364335509783,8.32757287256509));
#32813=CARTESIAN_POINT('Ctrl Pts',(0.135629400480723,1.73025422508501,8.32861690021769));
#32814=CARTESIAN_POINT('Ctrl Pts',(0.154528558470463,1.73832913496241,8.32966092787029));
#32815=CARTESIAN_POINT('Ctrl Pts',(0.161212942925885,1.7411851247421,8.33003018676615));
#32816=CARTESIAN_POINT('Ctrl Pts',(0.167811905613704,1.74422382933159,8.33039944566202));
#32817=CARTESIAN_POINT('Ctrl Pts',(0.174315056847757,1.74743915283151,8.33076870455788));
#32818=CARTESIAN_POINT('Ctrl Pts',(0.192700658537479,1.75652946229004,8.33181266720544));
#32819=CARTESIAN_POINT('Ctrl Pts',(0.210428054593902,1.76708890771966,8.33285662985299));
#32820=CARTESIAN_POINT('Ctrl Pts',(0.227251362384367,1.77899889673951,8.33390059250054));
#32821=CARTESIAN_POINT('Ctrl Pts',(0.244043721887338,1.7908869760512,8.33494263466631));
#32822=CARTESIAN_POINT('Ctrl Pts',(0.259934666343468,1.80412029557966,8.33598467683208));
#32823=CARTESIAN_POINT('Ctrl Pts',(0.274704454447322,1.81853534376977,8.33702671899785));
#32824=CARTESIAN_POINT('Ctrl Pts',(0.289458380030778,1.83293491042458,8.33806764202671));
#32825=CARTESIAN_POINT('Ctrl Pts',(0.303092995607605,1.84851319555014,8.33910856505556));
#32826=CARTESIAN_POINT('Ctrl Pts',(0.315423125498342,1.86506779296815,8.34014948808442));
#32827=CARTESIAN_POINT('Ctrl Pts',(0.327759587822429,1.88163089239593,8.34119094570421));
#32828=CARTESIAN_POINT('Ctrl Pts',(0.338789773615118,1.89917072536003,8.342232403324));
#32829=CARTESIAN_POINT('Ctrl Pts',(0.348369758462629,1.91745301594195,8.34327386094379));
#32830=CARTESIAN_POINT('Ctrl Pts',(0.357952670413164,1.93574089256069,8.34431563677429));
#32831=CARTESIAN_POINT('Ctrl Pts',(0.366084190141754,1.95477101044075,8.34535741260479));
#32832=CARTESIAN_POINT('Ctrl Pts',(0.372667500935047,1.97428673997216,8.34639918843529));
#32833=CARTESIAN_POINT('Ctrl Pts',(0.379265041704014,1.99384465319582,8.34744321608789));
#32834=CARTESIAN_POINT('Ctrl Pts',(0.384307512766835,2.01388955944127,8.34848724374049));
#32835=CARTESIAN_POINT('Ctrl Pts',(0.387748439671595,2.03415140447782,8.34953127139308));
#32836=CARTESIAN_POINT('Ctrl Pts',(0.388965450414985,2.04131775347997,8.34990053028895));
#32837=CARTESIAN_POINT('Ctrl Pts',(0.389982590928619,2.04851118515848,8.35026978918482));
#32838=CARTESIAN_POINT('Ctrl Pts',(0.39079936262898,2.05571966385874,8.35063904808068));
#32839=CARTESIAN_POINT('Ctrl Pts',(0.393108526081241,2.07609935570369,8.35168301072824));
#32840=CARTESIAN_POINT('Ctrl Pts',(0.39382611510272,2.09672088631415,8.35272697337579));
#32841=CARTESIAN_POINT('Ctrl Pts',(0.392918743578669,2.11731331697162,8.35377093602334));
#32842=CARTESIAN_POINT('Ctrl Pts',(0.392013041262312,2.13786786563394,8.35481297818911));
#32843=CARTESIAN_POINT('Ctrl Pts',(0.389488284633596,2.15839269122189,8.35585502035488));
#32844=CARTESIAN_POINT('Ctrl Pts',(0.38536300719655,2.17861451955226,8.35689706252065));
#32845=CARTESIAN_POINT('Ctrl Pts',(0.381242160242664,2.19881462995668,8.3579379855495));
#32846=CARTESIAN_POINT('Ctrl Pts',(0.37552432296311,2.21871166607327,8.35897890857835));
#32847=CARTESIAN_POINT('Ctrl Pts',(0.368279443155349,2.23804036275375,8.36001983160721));
#32848=CARTESIAN_POINT('Ctrl Pts',(0.361030842566146,2.25737898614906,8.361061289227));
#32849=CARTESIAN_POINT('Ctrl Pts',(0.352253875842425,2.27614799236037,8.36210274684679));
#32850=CARTESIAN_POINT('Ctrl Pts',(0.342067617485302,2.2940995493759,8.36314420446658));
#32851=CARTESIAN_POINT('Ctrl Pts',(0.331878246782168,2.31205659137473,8.36418598029708));
#32852=CARTESIAN_POINT('Ctrl Pts',(0.320279121502411,2.32919506541326,8.36522775612758));
#32853=CARTESIAN_POINT('Ctrl Pts',(0.307433611780586,2.34529464802059,8.36626953195807));
#32854=CARTESIAN_POINT('Ctrl Pts',(0.294560336197995,2.36142903024107,8.36731355961067));
#32855=CARTESIAN_POINT('Ctrl Pts',(0.280435800833115,2.37651950013216,8.36835758726327));
#32856=CARTESIAN_POINT('Ctrl Pts',(0.265261914657696,2.39038079590795,8.36940161491586));
#32857=CARTESIAN_POINT('Ctrl Pts',(0.259895110012964,2.39528335453344,8.36977087381173));
#32858=CARTESIAN_POINT('Ctrl Pts',(0.254397340402247,2.40003251903327,8.3701401327076));
#32859=CARTESIAN_POINT('Ctrl Pts',(0.248778455727177,2.40462135507216,8.37050939160347));
#32860=CARTESIAN_POINT('Ctrl Pts',(0.232892837838741,2.41759483648032,8.37155335425102));
#32861=CARTESIAN_POINT('Ctrl Pts',(0.215942329588985,2.42936100530444,8.37259731689857));
#32862=CARTESIAN_POINT('Ctrl Pts',(0.198136668596248,2.43974512587759,8.37364127954613));
#32863=CARTESIAN_POINT('Ctrl Pts',(0.180363763035575,2.450110143742,8.3746833217119));
#32864=CARTESIAN_POINT('Ctrl Pts',(0.161739425814271,2.45909774211519,8.37572536387767));
#32865=CARTESIAN_POINT('Ctrl Pts',(0.142503463278991,2.46657557604605,8.37676740604344));
#32866=CARTESIAN_POINT('Ctrl Pts',(0.123288159865291,2.47404537890074,8.37780832907229));
#32867=CARTESIAN_POINT('Ctrl Pts',(0.103463207020081,2.48000834410828,8.37884925210114));
#32868=CARTESIAN_POINT('Ctrl Pts',(0.08328950843611,2.48437969221132,8.37989017513));
#32869=CARTESIAN_POINT('Ctrl Pts',(0.0631054491663324,2.48875328532482,
8.38093163274979));
#32870=CARTESIAN_POINT('Ctrl Pts',(0.0425730020190756,2.49153345675393,
8.38197309036958));
#32871=CARTESIAN_POINT('Ctrl Pts',(0.0219650057661074,2.49268617052513,
8.38301454798937));
#32872=CARTESIAN_POINT('Ctrl Pts',(0.00135071287185152,2.49383923650065,
8.38405632381987));
#32873=CARTESIAN_POINT('Ctrl Pts',(-0.0193384390504099,2.49336384995985,
8.38509809965037));
#32874=CARTESIAN_POINT('Ctrl Pts',(-0.0398287628758352,2.49127811036113,
8.38613987548087));
#32875=CARTESIAN_POINT('Ctrl Pts',(-0.0603633770011931,2.48918786238894,
8.38718390313347));
#32876=CARTESIAN_POINT('Ctrl Pts',(-0.0806975804783717,2.48548044418256,
8.38822793078606));
#32877=CARTESIAN_POINT('Ctrl Pts',(-0.100566304906113,2.48022533886832,
8.38927195843866));
#32878=CARTESIAN_POINT('Ctrl Pts',(-0.107593612301816,2.47836667700131,
8.38964121733452));
#32879=CARTESIAN_POINT('Ctrl Pts',(-0.114562836872709,2.47631486243418,
8.39001047623039));
#32880=CARTESIAN_POINT('Ctrl Pts',(-0.121462816175818,2.47407442345961,
8.39037973512625));
#32881=CARTESIAN_POINT('Ctrl Pts',(-0.140970323623923,2.46774029141898,
8.39142369777381));
#32882=CARTESIAN_POINT('Ctrl Pts',(-0.160039145429101,2.45985724037983,
8.39246766042136));
#32883=CARTESIAN_POINT('Ctrl Pts',(-0.178408825951557,2.45050703391314,
8.39351162306892));
#32884=CARTESIAN_POINT('Ctrl Pts',(-0.196744713467248,2.44117402815878,
8.39455366523469));
#32885=CARTESIAN_POINT('Ctrl Pts',(-0.214383337355163,2.43037950136081,
8.39559570740046));
#32886=CARTESIAN_POINT('Ctrl Pts',(-0.231083608102391,2.41825344627573,
8.39663774956623));
#32887=CARTESIAN_POINT('Ctrl Pts',(-0.247765943021182,2.40614041438332,
8.39767867259509));
#32888=CARTESIAN_POINT('Ctrl Pts',(-0.263511316120186,2.39269909988827,
8.39871959562394));
#32889=CARTESIAN_POINT('Ctrl Pts',(-0.278107211430637,2.37810298263463,
8.3997605186528));
#32890=CARTESIAN_POINT('Ctrl Pts',(-0.292710602812506,2.36349936919558,
8.40080197627259));
#32891=CARTESIAN_POINT('Ctrl Pts',(-0.306162805365953,2.34774027704241,
8.40184343389239));
#32892=CARTESIAN_POINT('Ctrl Pts',(-0.318287508478008,2.33103668961198,
8.40288489151218));
#32893=CARTESIAN_POINT('Ctrl Pts',(-0.330415916215455,2.31432799850737,
8.40392666734268));
#32894=CARTESIAN_POINT('Ctrl Pts',(-0.341215614465228,2.29667485382037,
8.40496844317318));
#32895=CARTESIAN_POINT('Ctrl Pts',(-0.350553669790102,2.27831717414958,
8.40601021900368));
#32896=CARTESIAN_POINT('Ctrl Pts',(-0.359911909533465,2.25991981393761,
8.40705424665628));
#32897=CARTESIAN_POINT('Ctrl Pts',(-0.367801917684434,2.24081555911867,
8.40809827430888));
#32898=CARTESIAN_POINT('Ctrl Pts',(-0.374138630584593,2.22126489642219,
8.40914230196147));
#32899=CARTESIAN_POINT('Ctrl Pts',(-0.376379842877265,2.21435008329185,
8.40951156085733));
#32900=CARTESIAN_POINT('Ctrl Pts',(-0.378427207638841,2.20737955019393,
8.40988081975319));
#32901=CARTESIAN_POINT('Ctrl Pts',(-0.380278489906803,2.20036513395697,
8.41025007864905));
#32902=CARTESIAN_POINT('Ctrl Pts',(-0.386974892832756,2.17499279704981,
8.41158575089821));
#32903=CARTESIAN_POINT('Ctrl Pts',(-0.391134538405294,2.14892449232814,
8.41292142314736));
#32904=CARTESIAN_POINT('Ctrl Pts',(-0.39264977411344,2.12260630196791,8.41425709539652));
#32905=CARTESIAN_POINT('Ctrl Pts',(-0.393075774356986,2.11520708649083,
8.41463261235429));
#32906=CARTESIAN_POINT('Ctrl Pts',(-0.393293034601751,2.10778825598276,
8.41500812931207));
#32907=CARTESIAN_POINT('Ctrl Pts',(-0.393299835176423,2.10036006971291,
8.41538364626984));
#32908=CARTESIAN_POINT('',(-0.393068738817681,2.09989474590746,8.54038365103395));
#32909=CARTESIAN_POINT('Ctrl Pts',(-0.393200853125335,2.10035994890194,
8.41538364779652));
#32910=CARTESIAN_POINT('Ctrl Pts',(-0.392329112146126,2.00321302993875,
8.42029590592163));
#32911=CARTESIAN_POINT('Ctrl Pts',(-0.306910870380854,1.77370848694128,
8.43183161188765));
#32912=CARTESIAN_POINT('Ctrl Pts',(0.0781045900267053,1.64155184207887,
8.44999076569464));
#32913=CARTESIAN_POINT('Ctrl Pts',(0.427750845253811,1.91750546619381,8.4698611092174));
#32914=CARTESIAN_POINT('Ctrl Pts',(0.384993932979691,2.3608729806885,8.4897314527402));
#32915=CARTESIAN_POINT('Ctrl Pts',(-0.0109425006120916,2.56492505005092,
8.509601796263));
#32916=CARTESIAN_POINT('Ctrl Pts',(-0.338844730225498,2.37590380025287,
8.52648586128176));
#32917=CARTESIAN_POINT('Ctrl Pts',(-0.392506215664613,2.17206643209509,
8.53674647845961));
#32918=CARTESIAN_POINT('Ctrl Pts',(-0.392678456924488,2.09989491469267,
8.54038364779652));
#32919=CARTESIAN_POINT('',(-0.393364049700885,2.09968468653314,8.66538364779653));
#32920=CARTESIAN_POINT('Ctrl Pts',(-0.393299985889287,2.09989464590004,
8.54038365295217));
#32921=CARTESIAN_POINT('Ctrl Pts',(-0.393294038661158,2.07769290206561,
8.5415007688402));
#32922=CARTESIAN_POINT('Ctrl Pts',(-0.391403923263078,2.05554353096737,
8.54261788472822));
#32923=CARTESIAN_POINT('Ctrl Pts',(-0.38768122540452,2.03375683077592,8.54373500061624));
#32924=CARTESIAN_POINT('Ctrl Pts',(-0.383937656161153,2.01184798298596,
8.54485837963828));
#32925=CARTESIAN_POINT('Ctrl Pts',(-0.37834109873788,1.99030641866694,8.54598175866031));
#32926=CARTESIAN_POINT('Ctrl Pts',(-0.370993975156392,1.96943062994079,
8.54710513768235));
#32927=CARTESIAN_POINT('Ctrl Pts',(-0.366116412467435,1.95557174121191,
8.54785091955775));
#32928=CARTESIAN_POINT('Ctrl Pts',(-0.360468356591718,1.94200590930795,
8.54859670143316));
#32929=CARTESIAN_POINT('Ctrl Pts',(-0.354091051801312,1.92881467050521,
8.54934248330856));
#32930=CARTESIAN_POINT('Ctrl Pts',(-0.345163953660686,1.91034927058176,
8.55038644595611));
#32931=CARTESIAN_POINT('Ctrl Pts',(-0.334761946975892,1.89252903725973,
8.55143040860367));
#32932=CARTESIAN_POINT('Ctrl Pts',(-0.32300144151329,1.87560089398499,8.55247437125122));
#32933=CARTESIAN_POINT('Ctrl Pts',(-0.311262570767752,1.85870389185391,
8.55351641341699));
#32934=CARTESIAN_POINT('Ctrl Pts',(-0.298170528088468,1.84269635363174,
8.55455845558276));
#32935=CARTESIAN_POINT('Ctrl Pts',(-0.283886872206727,1.82779946034462,
8.55560049774853));
#32936=CARTESIAN_POINT('Ctrl Pts',(-0.269618556747013,1.81291856608686,
8.55664142077739));
#32937=CARTESIAN_POINT('Ctrl Pts',(-0.25416165451208,1.79914649715438,8.55768234380624));
#32938=CARTESIAN_POINT('Ctrl Pts',(-0.23771692350351,1.78667021482147,8.55872326683509));
#32939=CARTESIAN_POINT('Ctrl Pts',(-0.221263746909695,1.77418752499511,
8.55976472445489));
#32940=CARTESIAN_POINT('Ctrl Pts',(-0.203822304452074,1.7630024088121,8.56080618207468));
#32941=CARTESIAN_POINT('Ctrl Pts',(-0.185625588014758,1.75326086019289,
8.56184763969447));
#32942=CARTESIAN_POINT('Ctrl Pts',(-0.167423311687262,1.74351633510588,
8.56288941552497));
#32943=CARTESIAN_POINT('Ctrl Pts',(-0.148465967176074,1.73521657072913,
8.56393119135547));
#32944=CARTESIAN_POINT('Ctrl Pts',(-0.129009316447134,1.72846065313369,
8.56497296718597));
#32945=CARTESIAN_POINT('Ctrl Pts',(-0.109510609726116,1.72169013246906,
8.56601699483857));
#32946=CARTESIAN_POINT('Ctrl Pts',(-0.089511154700245,1.71647030685164,
8.56706102249117));
#32947=CARTESIAN_POINT('Ctrl Pts',(-0.0692805833476899,1.71285004097765,
8.56810505014377));
#32948=CARTESIAN_POINT('Ctrl Pts',(-0.0621252954376586,1.71156960039158,
8.56847430903963));
#32949=CARTESIAN_POINT('Ctrl Pts',(-0.0549411555171371,1.71048878230323,
8.5688435679355));
#32950=CARTESIAN_POINT('Ctrl Pts',(-0.0477401943522662,1.70960819188512,
8.56921282683136));
#32951=CARTESIAN_POINT('Ctrl Pts',(-0.0273817559590799,1.70711860120878,
8.57025678947892));
#32952=CARTESIAN_POINT('Ctrl Pts',(-0.00676739055080256,1.70621838038248,
8.57130075212647));
#32953=CARTESIAN_POINT('Ctrl Pts',(0.0138322695083255,1.70694331411328,
8.57234471477402));
#32954=CARTESIAN_POINT('Ctrl Pts',(0.0343940342730368,1.70766691425037,
8.57338675693979));
#32955=CARTESIAN_POINT('Ctrl Pts',(0.0549404182758393,1.71000976846255,
8.57442879910556));
#32956=CARTESIAN_POINT('Ctrl Pts',(0.07519799388942,1.71395576456187,8.57547084127133));
#32957=CARTESIAN_POINT('Ctrl Pts',(0.095433813185032,1.71789752272338,8.57651176430019));
#32958=CARTESIAN_POINT('Ctrl Pts',(0.115380715792135,1.72343889311018,8.57755268732904));
#32959=CARTESIAN_POINT('Ctrl Pts',(0.134772827390175,1.73051228031603,8.57859361035789));
#32960=CARTESIAN_POINT('Ctrl Pts',(0.154174898271309,1.7375893002292,8.57963506797769));
#32961=CARTESIAN_POINT('Ctrl Pts',(0.173020912169774,1.74619967183376,8.58067652559748));
#32962=CARTESIAN_POINT('Ctrl Pts',(0.191061992066552,1.75622652052905,8.58171798321727));
#32963=CARTESIAN_POINT('Ctrl Pts',(0.209108584299766,1.76625643286376,8.58275975904776));
#32964=CARTESIAN_POINT('Ctrl Pts',(0.226349127911292,1.77770329512398,8.58380153487826));
#32965=CARTESIAN_POINT('Ctrl Pts',(0.242561860985024,1.79040569515012,8.58484331070876));
#32966=CARTESIAN_POINT('Ctrl Pts',(0.258809638249209,1.80313555170217,8.58588733836136));
#32967=CARTESIAN_POINT('Ctrl Pts',(0.274024627458827,1.81712586564286,8.58693136601395));
#32968=CARTESIAN_POINT('Ctrl Pts',(0.28801978564067,1.83217637692036,8.58797539366655));
#32969=CARTESIAN_POINT('Ctrl Pts',(0.292969689644507,1.83749954548083,8.58834465256242));
#32970=CARTESIAN_POINT('Ctrl Pts',(0.297767365592751,1.84295503259325,8.58871391145828));
#32971=CARTESIAN_POINT('Ctrl Pts',(0.302405792174401,1.84853305016489,8.58908317035415));
#32972=CARTESIAN_POINT('Ctrl Pts',(0.31551947514552,1.86430312925404,8.5901271330017));
#32973=CARTESIAN_POINT('Ctrl Pts',(0.327435325407625,1.88114875097759,8.59117109564925));
#32974=CARTESIAN_POINT('Ctrl Pts',(0.337976756349517,1.89886173370674,8.59221505829681));
#32975=CARTESIAN_POINT('Ctrl Pts',(0.348498795193288,1.91654213149547,8.59325710046258));
#32976=CARTESIAN_POINT('Ctrl Pts',(0.357651010334645,1.93508612835312,8.59429914262835));
#32977=CARTESIAN_POINT('Ctrl Pts',(0.365298937874502,1.95425509961662,8.59534118479412));
#32978=CARTESIAN_POINT('Ctrl Pts',(0.372938651660327,1.97340348370612,8.59638210782297));
#32979=CARTESIAN_POINT('Ctrl Pts',(0.379076987023166,1.99317484047176,8.59742303085183));
#32980=CARTESIAN_POINT('Ctrl Pts',(0.383626856817083,2.01330902740974,8.59846395388068));
#32981=CARTESIAN_POINT('Ctrl Pts',(0.38817906330554,2.03345355474136,8.59950541150047));
#32982=CARTESIAN_POINT('Ctrl Pts',(0.39114099654613,2.05396057038255,8.60054686912027));
#32983=CARTESIAN_POINT('Ctrl Pts',(0.392476205168331,2.0745575477466,8.60158832674006));
#32984=CARTESIAN_POINT('Ctrl Pts',(0.393811821754976,2.0951608183852,8.60263010257056));
#32985=CARTESIAN_POINT('Ctrl Pts',(0.393519712791342,2.11585336950821,8.60367187840105));
#32986=CARTESIAN_POINT('Ctrl Pts',(0.391615552779024,2.13636136440756,8.60471365423155));
#32987=CARTESIAN_POINT('Ctrl Pts',(0.38970727688163,2.15691368780326,8.60575768188415));
#32988=CARTESIAN_POINT('Ctrl Pts',(0.386180119008918,2.17727993287075,8.60680170953675));
#32989=CARTESIAN_POINT('Ctrl Pts',(0.381101211656955,2.19719442614472,8.60784573718934));
#32990=CARTESIAN_POINT('Ctrl Pts',(0.379304868699628,2.20423792138146,8.60821499608521));
#32991=CARTESIAN_POINT('Ctrl Pts',(0.377314866137651,2.21122504696654,8.60858425498108));
#32992=CARTESIAN_POINT('Ctrl Pts',(0.375135633212143,2.21814460078448,8.60895351387694));
#32993=CARTESIAN_POINT('Ctrl Pts',(0.36897454190192,2.23770744897722,8.6099974765245));
#32994=CARTESIAN_POINT('Ctrl Pts',(0.3612607065989,2.25684534864359,8.61104143917205));
#32995=CARTESIAN_POINT('Ctrl Pts',(0.352073580620603,2.27529713012194,8.61208540181961));
#32996=CARTESIAN_POINT('Ctrl Pts',(0.342903355350511,2.29371496755997,8.61312744398538));
#32997=CARTESIAN_POINT('Ctrl Pts',(0.332265490199807,2.3114485144834,8.61416948615115));
#32998=CARTESIAN_POINT('Ctrl Pts',(0.320287837319435,2.32825553939661,8.61521152831692));
#32999=CARTESIAN_POINT('Ctrl Pts',(0.308323048250094,2.3450445138291,8.61625245134577));
#33000=CARTESIAN_POINT('Ctrl Pts',(0.295021729332165,2.36090832876827,8.61729337437462));
#33001=CARTESIAN_POINT('Ctrl Pts',(0.280555471194879,2.37563293994481,8.61833429740348));
#33002=CARTESIAN_POINT('Ctrl Pts',(0.266081783564447,2.39036511329788,8.61937575502327));
#33003=CARTESIAN_POINT('Ctrl Pts',(0.250442465629713,2.403956377903,8.62041721264306));
#33004=CARTESIAN_POINT('Ctrl Pts',(0.2338469308387,2.41622856122956,8.62145867026286));
#33005=CARTESIAN_POINT('Ctrl Pts',(0.217246325388308,2.42850449424316,8.62250044609335));
#33006=CARTESIAN_POINT('Ctrl Pts',(0.199689534056603,2.43946013561006,8.62354222192385));
#33007=CARTESIAN_POINT('Ctrl Pts',(0.181415288541559,2.44896043197386,8.62458399775435));
#33008=CARTESIAN_POINT('Ctrl Pts',(0.163101542830138,2.45848126344384,8.62562802540695));
#33009=CARTESIAN_POINT('Ctrl Pts',(0.144067925044122,2.4665401824026,8.62667205305954));
#33010=CARTESIAN_POINT('Ctrl Pts',(0.124574158222978,2.47304982120762,8.62771608071214));
#33011=CARTESIAN_POINT('Ctrl Pts',(0.117679468417838,2.47535219512621,8.628085339608));
#33012=CARTESIAN_POINT('Ctrl Pts',(0.110727343781885,2.47746122267087,8.62845459850387));
#33013=CARTESIAN_POINT('Ctrl Pts',(0.103729600882616,2.47937456411933,8.62882385739973));
#33014=CARTESIAN_POINT('Ctrl Pts',(0.0839456978113508,2.48478393144011,
8.62986782004729));
#33015=CARTESIAN_POINT('Ctrl Pts',(0.0636785706898904,2.48865769149517,
8.63091178269484));
#33016=CARTESIAN_POINT('Ctrl Pts',(0.0431908251622427,2.49092127419956,
8.63195574534239));
#33017=CARTESIAN_POINT('Ctrl Pts',(0.0227407690501717,2.49318069279964,
8.63299778750816));
#33018=CARTESIAN_POINT('Ctrl Pts',(0.00207161666862456,2.49383567469102,
8.63403982967393));
#33019=CARTESIAN_POINT('Ctrl Pts',(-0.0185437507244163,2.49286259596591,
8.6350818718397));
#33020=CARTESIAN_POINT('Ctrl Pts',(-0.039136977536738,2.49189056231205,
8.63612279486855));
#33021=CARTESIAN_POINT('Ctrl Pts',(-0.0596758014392799,2.48929394488147,
8.6371637178974));
#33022=CARTESIAN_POINT('Ctrl Pts',(-0.079887365070007,2.4851011541169,8.63820464092625));
#33023=CARTESIAN_POINT('Ctrl Pts',(-0.100109308833038,2.48090621004428,
8.63924609854604));
#33024=CARTESIAN_POINT('Ctrl Pts',(-0.120002932838844,2.47511358862173,
8.64028755616583));
#33025=CARTESIAN_POINT('Ctrl Pts',(-0.139305067150353,2.46780292041559,
8.64132901378562));
#33026=CARTESIAN_POINT('Ctrl Pts',(-0.158613099105392,2.46049001848159,
8.64237078961612));
#33027=CARTESIAN_POINT('Ctrl Pts',(-0.177328606899627,2.45165844061416,
8.64341256544661));
#33028=CARTESIAN_POINT('Ctrl Pts',(-0.195208805471213,2.4414358098772,8.64445434127711));
#33029=CARTESIAN_POINT('Ctrl Pts',(-0.213127652497767,2.43119108269193,
8.64549836892971));
#33030=CARTESIAN_POINT('Ctrl Pts',(-0.230206977071488,2.41954971452007,
8.6465423965823));
#33031=CARTESIAN_POINT('Ctrl Pts',(-0.24623272614012,2.40668279145985,8.6475864242349));
#33032=CARTESIAN_POINT('Ctrl Pts',(-0.251900823524189,2.40213192942985,
8.64795568313077));
#33033=CARTESIAN_POINT('Ctrl Pts',(-0.257437442327009,2.39742811328002,
8.64832494202664));
#33034=CARTESIAN_POINT('Ctrl Pts',(-0.2628342187467,2.39258001205792,8.64869420092251));
#33035=CARTESIAN_POINT('Ctrl Pts',(-0.277864808745112,2.37907754019818,
8.64972262578866));
#33036=CARTESIAN_POINT('Ctrl Pts',(-0.291903284089961,2.36436757417959,
8.65075105065482));
#33037=CARTESIAN_POINT('Ctrl Pts',(-0.304747731190058,2.34862363189068,
8.65177947552097));
#33038=CARTESIAN_POINT('Ctrl Pts',(-0.317568308372067,2.33290894789603,
8.65280598917857));
#33039=CARTESIAN_POINT('Ctrl Pts',(-0.329198735141888,2.31616464048174,
8.65383250283615));
#33040=CARTESIAN_POINT('Ctrl Pts',(-0.339474010293861,2.29860082158693,
8.65485901649375));
#33041=CARTESIAN_POINT('Ctrl Pts',(-0.349744380750245,2.28104538642723,
8.65588504016572));
#33042=CARTESIAN_POINT('Ctrl Pts',(-0.358660462020373,2.26267184650269,
8.6569110638377));
#33043=CARTESIAN_POINT('Ctrl Pts',(-0.366100711712632,2.24371902756248,
8.65793708750967));
#33044=CARTESIAN_POINT('Ctrl Pts',(-0.373538861149918,2.22477155867822,
8.65896282155275));
#33045=CARTESIAN_POINT('Ctrl Pts',(-0.379501738069724,2.20524584583435,
8.65998855559583));
#33046=CARTESIAN_POINT('Ctrl Pts',(-0.383916419493351,2.18539948971396,
8.66101428963891));
#33047=CARTESIAN_POINT('Ctrl Pts',(-0.388337722225733,2.16552336726642,
8.6620415621173));
#33048=CARTESIAN_POINT('Ctrl Pts',(-0.391206066234724,2.14532639112539,
8.66306883459569));
#33049=CARTESIAN_POINT('Ctrl Pts',(-0.392499829559989,2.12507536231801,
8.66409610707408));
#33050=CARTESIAN_POINT('Ctrl Pts',(-0.393040345992751,2.11661476242546,
8.6645252873149));
#33051=CARTESIAN_POINT('Ctrl Pts',(-0.393306655044755,2.10814475890454,
8.66495446755571));
#33052=CARTESIAN_POINT('Ctrl Pts',(-0.393299873645868,2.0996847379755,8.66538364779653));
#33053=CARTESIAN_POINT('',(-0.393416716470155,2.1002762343866,8.79038364779653));
#33054=CARTESIAN_POINT('Ctrl Pts',(-0.393587260541253,2.09968450761139,
8.66538364779653));
#33055=CARTESIAN_POINT('Ctrl Pts',(-0.393770050696924,2.0787684143503,8.66644394667946));
#33056=CARTESIAN_POINT('Ctrl Pts',(-0.382732713030496,1.92738745922455,
8.67412769340335));
#33057=CARTESIAN_POINT('Ctrl Pts',(-0.186276276076986,1.67388242296857,
8.68843488796805));
#33058=CARTESIAN_POINT('Ctrl Pts',(0.257452574101791,1.71271042800903,8.70830523149091));
#33059=CARTESIAN_POINT('Ctrl Pts',(0.465003736545269,2.10682389063747,8.72817557501367));
#33060=CARTESIAN_POINT('Ctrl Pts',(0.245977275250812,2.49467736259462,8.74804591853647));
#33061=CARTESIAN_POINT('Ctrl Pts',(-0.198699849304038,2.52046808484241,
8.76791626205924));
#33062=CARTESIAN_POINT('Ctrl Pts',(-0.385062938840621,2.26483280350818,
8.78202883847928));
#33063=CARTESIAN_POINT('Ctrl Pts',(-0.39382877298102,2.11734147947392,8.78951796705837));
#33064=CARTESIAN_POINT('Ctrl Pts',(-0.393692564686641,2.10027642807121,
8.79038364779653));
#33065=CARTESIAN_POINT('',(-0.393299965593714,2.10016451134769,8.91538364779289));
#33066=CARTESIAN_POINT('Ctrl Pts',(-0.393299903050929,2.100276152367,8.79038364779653));
#33067=CARTESIAN_POINT('Ctrl Pts',(-0.393314122120435,2.08002516296271,
8.79141197759652));
#33068=CARTESIAN_POINT('Ctrl Pts',(-0.391759973089012,2.05971329987927,
8.79244030739651));
#33069=CARTESIAN_POINT('Ctrl Pts',(-0.388635608644073,2.03960750300037,
8.79346863719649));
#33070=CARTESIAN_POINT('Ctrl Pts',(-0.385515976401287,2.0195321586173,8.79449540947508));
#33071=CARTESIAN_POINT('Ctrl Pts',(-0.380830912048011,1.99966301204038,
8.79552218175366));
#33072=CARTESIAN_POINT('Ctrl Pts',(-0.37463042075924,1.98026304730053,8.79654895403225));
#33073=CARTESIAN_POINT('Ctrl Pts',(-0.368429200823891,1.96086080278683,
8.79757584697129));
#33074=CARTESIAN_POINT('Ctrl Pts',(-0.360712391440744,1.94192858389374,
8.79860273991033));
#33075=CARTESIAN_POINT('Ctrl Pts',(-0.351580247434861,1.92371551510799,
8.79962963284937));
#33076=CARTESIAN_POINT('Ctrl Pts',(-0.342448079966206,1.90550239952829,
8.80065652842676));
#33077=CARTESIAN_POINT('Ctrl Pts',(-0.331900931995182,1.88800910537307,
8.80168342400414));
#33078=CARTESIAN_POINT('Ctrl Pts',(-0.320085107705698,1.87146025766832,
8.80271031958153));
#33079=CARTESIAN_POINT('Ctrl Pts',(-0.308243682958548,1.85487555482009,
8.80373944005632));
#33080=CARTESIAN_POINT('Ctrl Pts',(-0.295128573858232,1.83923997386343,
8.80476856053111));
#33081=CARTESIAN_POINT('Ctrl Pts',(-0.280926850596252,1.82474558202624,
8.8057976810059));
#33082=CARTESIAN_POINT('Ctrl Pts',(-0.272374301224326,1.81601678204072,
8.80641743703888));
#33083=CARTESIAN_POINT('Ctrl Pts',(-0.263428410976905,1.80770115207403,
8.80703719307185));
#33084=CARTESIAN_POINT('Ctrl Pts',(-0.254135713613598,1.79983349776148,
8.80765694910483));
#33085=CARTESIAN_POINT('Ctrl Pts',(-0.23848241065873,1.78658064213909,8.80870091175239));
#33086=CARTESIAN_POINT('Ctrl Pts',(-0.221742997184422,1.77451604536762,
8.80974487439994));
#33087=CARTESIAN_POINT('Ctrl Pts',(-0.204124082495864,1.76381813114741,
8.81078883704749));
#33088=CARTESIAN_POINT('Ctrl Pts',(-0.186537579699419,1.75313989689317,
8.81183087921326));
#33089=CARTESIAN_POINT('Ctrl Pts',(-0.168075378184561,1.7438237830749,8.81287292137903));
#33090=CARTESIAN_POINT('Ctrl Pts',(-0.148974902208042,1.73600636198952,
8.8139149635448));
#33091=CARTESIAN_POINT('Ctrl Pts',(-0.129894939842656,1.72819733669157,
8.81495588657366));
#33092=CARTESIAN_POINT('Ctrl Pts',(-0.110178730435513,1.7218841127929,8.81599680960251));
#33093=CARTESIAN_POINT('Ctrl Pts',(-0.0900856348904587,1.71715607829511,
8.81703773263137));
#33094=CARTESIAN_POINT('Ctrl Pts',(-0.0699822200552296,1.71242561560202,
8.81807919025116));
#33095=CARTESIAN_POINT('Ctrl Pts',(-0.0495022449195084,1.70928215294598,
8.81912064787095));
#33096=CARTESIAN_POINT('Ctrl Pts',(-0.0289179025022455,1.70776455423449,
8.82016210549074));
#33097=CARTESIAN_POINT('Ctrl Pts',(-0.00832727067096913,1.70624649183043,
8.82120388132124));
#33098=CARTESIAN_POINT('Ctrl Pts',(0.0123670560961123,1.70635530029777,
8.82224565715174));
#33099=CARTESIAN_POINT('Ctrl Pts',(0.0328911129931427,1.70807773132154,
8.82328743298224));
#33100=CARTESIAN_POINT('Ctrl Pts',(0.053459533104898,1.70980388541905,8.82433146063484));
#33101=CARTESIAN_POINT('Ctrl Pts',(0.0738562218082703,1.71315050621404,
8.82537548828743));
#33102=CARTESIAN_POINT('Ctrl Pts',(0.0938149214189155,1.71805281710796,
8.82641951594003));
#33103=CARTESIAN_POINT('Ctrl Pts',(0.100874051857501,1.71978670021287,8.8267887748359));
#33104=CARTESIAN_POINT('Ctrl Pts',(0.107878530240366,1.72171473463223,8.82715803373176));
#33105=CARTESIAN_POINT('Ctrl Pts',(0.114817115658489,1.72383259052403,8.82752729262763));
#33106=CARTESIAN_POINT('Ctrl Pts',(0.134433769676722,1.72982015769892,8.82857125527518));
#33107=CARTESIAN_POINT('Ctrl Pts',(0.153639245627005,1.73736417203118,8.82961521792274));
#33108=CARTESIAN_POINT('Ctrl Pts',(0.172171680317429,1.7463874966907,8.83065918057029));
#33109=CARTESIAN_POINT('Ctrl Pts',(0.190670022597255,1.75539422197218,8.83170122273606));
#33110=CARTESIAN_POINT('Ctrl Pts',(0.208497101165738,1.7658745908189,8.83274326490183));
#33111=CARTESIAN_POINT('Ctrl Pts',(0.225409561550228,1.77770290171686,8.8337853070676));
#33112=CARTESIAN_POINT('Ctrl Pts',(0.242303858217949,1.78951850919473,8.83482623009645));
#33113=CARTESIAN_POINT('Ctrl Pts',(0.258284870307714,1.80267878890176,8.8358671531253));
#33114=CARTESIAN_POINT('Ctrl Pts',(0.273137042043731,1.81701405288672,8.83690807615416));
#33115=CARTESIAN_POINT('Ctrl Pts',(0.287996841468064,1.83135667908964,8.83794953377395));
#33116=CARTESIAN_POINT('Ctrl Pts',(0.301726101741667,1.84687499573061,8.83899099139374));
#33117=CARTESIAN_POINT('Ctrl Pts',(0.314144802395893,1.86336117578122,8.84003244901353));
#33118=CARTESIAN_POINT('Ctrl Pts',(0.326567297504571,1.87985239307857,8.84107422484403));
#33119=CARTESIAN_POINT('Ctrl Pts',(0.337678022398854,1.89731145353291,8.84211600067452));
#33120=CARTESIAN_POINT('Ctrl Pts',(0.347339814399537,1.91550083107804,8.84315777650502));
#33121=CARTESIAN_POINT('Ctrl Pts',(0.357022490582887,1.93372952537551,8.84420180415761));
#33122=CARTESIAN_POINT('Ctrl Pts',(0.365249688039197,1.95269101273338,8.84524583181021));
#33123=CARTESIAN_POINT('Ctrl Pts',(0.371931741996789,1.97212635418025,8.84628985946281));
#33124=CARTESIAN_POINT('Ctrl Pts',(0.37429509689488,1.97900037969637,8.84665911835867));
#33125=CARTESIAN_POINT('Ctrl Pts',(0.376465621746349,1.98593355040014,8.84702837725454));
#33126=CARTESIAN_POINT('Ctrl Pts',(0.378440872252739,1.99291407091225,8.84739763615041));
#33127=CARTESIAN_POINT('Ctrl Pts',(0.3840252678389,2.01264928313513,8.84844159879796));
#33128=CARTESIAN_POINT('Ctrl Pts',(0.388078396670224,2.03288130244609,8.84948556144552));
#33129=CARTESIAN_POINT('Ctrl Pts',(0.390523365497208,2.05334819402495,8.85052952409307));
#33130=CARTESIAN_POINT('Ctrl Pts',(0.392963836540573,2.07377743455131,8.85157156625884));
#33131=CARTESIAN_POINT('Ctrl Pts',(0.393801874513695,2.09443997441952,8.85261360842461));
#33132=CARTESIAN_POINT('Ctrl Pts',(0.393011439326963,2.11506315233106,8.85365565059038));
#33133=CARTESIAN_POINT('Ctrl Pts',(0.392221853055205,2.13566418127351,8.85469657361923));
#33134=CARTESIAN_POINT('Ctrl Pts',(0.389807264853583,2.15622519956534,8.85573749664809));
#33135=CARTESIAN_POINT('Ctrl Pts',(0.385793667153384,2.17647310889682,8.85677841967694));
#33136=CARTESIAN_POINT('Ctrl Pts',(0.381778008174011,2.1967314170268,8.85781987729673));
#33137=CARTESIAN_POINT('Ctrl Pts',(0.376161826354476,2.21667557007474,8.85886133491653));
#33138=CARTESIAN_POINT('Ctrl Pts',(0.369022418048841,2.23604170308176,8.85990279253632));
#33139=CARTESIAN_POINT('Ctrl Pts',(0.361880828342715,2.25541375328672,8.86094456836682));
#33140=CARTESIAN_POINT('Ctrl Pts',(0.35321537386231,2.27420675459767,8.86198634419732));
#33141=CARTESIAN_POINT('Ctrl Pts',(0.343151522140229,2.29217680102667,8.86302812002782));
#33142=CARTESIAN_POINT('Ctrl Pts',(0.33306591717428,2.3101856901188,8.86407214768041));
#33143=CARTESIAN_POINT('Ctrl Pts',(0.321576289749156,2.32736746076212,8.86511617533301));
#33144=CARTESIAN_POINT('Ctrl Pts',(0.308851823227105,2.34350655286725,8.86616020298561));
#33145=CARTESIAN_POINT('Ctrl Pts',(0.30435134620741,2.34921473819762,8.86652946188148));
#33146=CARTESIAN_POINT('Ctrl Pts',(0.299696756466525,2.35479280493104,8.86689872077734));
#33147=CARTESIAN_POINT('Ctrl Pts',(0.294896648627635,2.36023231280567,8.86726797967321));
#33148=CARTESIAN_POINT('Ctrl Pts',(0.281325863078232,2.37561079956858,8.86831194232076));
#33149=CARTESIAN_POINT('Ctrl Pts',(0.266508450871526,2.38997070048114,8.86935590496832));
#33150=CARTESIAN_POINT('Ctrl Pts',(0.250623027788763,2.40310557227143,8.87039986761587));
#33151=CARTESIAN_POINT('Ctrl Pts',(0.23476682765352,2.41621628104969,8.87144190978164));
#33152=CARTESIAN_POINT('Ctrl Pts',(0.217847039279517,2.42810592456112,8.87248395194741));
#33153=CARTESIAN_POINT('Ctrl Pts',(0.200078825197363,2.43860501134455,8.87352599411317));
#33154=CARTESIAN_POINT('Ctrl Pts',(0.182329693897984,2.44909282227373,8.87456691714203));
#33155=CARTESIAN_POINT('Ctrl Pts',(0.163734561363448,2.45819264399749,8.87560784017088));
#33156=CARTESIAN_POINT('Ctrl Pts',(0.14453712371496,2.46577849836781,8.87664876319974));
#33157=CARTESIAN_POINT('Ctrl Pts',(0.125329826762846,2.47336824863521,8.87769022081953));
#33158=CARTESIAN_POINT('Ctrl Pts',(0.105520285095474,2.4794421928199,8.87873167843932));
#33159=CARTESIAN_POINT('Ctrl Pts',(0.0853722030077162,2.48392248821033,
8.87977313605911));
#33160=CARTESIAN_POINT('Ctrl Pts',(0.0652179648025095,2.48840415252632,
8.8808149118896));
#33161=CARTESIAN_POINT('Ctrl Pts',(0.0447257057380876,2.49129107442718,
8.8818566877201));
#33162=CARTESIAN_POINT('Ctrl Pts',(0.0241684241785611,2.49255671854233,
8.8828984635506));
#33163=CARTESIAN_POINT('Ctrl Pts',(0.00356670758843661,2.49382509837597,
8.88394249120319));
#33164=CARTESIAN_POINT('Ctrl Pts',(-0.0170995757271018,2.49346521682634,
8.88498651885579));
#33165=CARTESIAN_POINT('Ctrl Pts',(-0.0375575969745094,2.49150263972226,
8.88603054650839));
#33166=CARTESIAN_POINT('Ctrl Pts',(-0.044793330931032,2.49080850192553,
8.88639980540425));
#33167=CARTESIAN_POINT('Ctrl Pts',(-0.0520030828421718,2.4899143478459,
8.88676906430012));
#33168=CARTESIAN_POINT('Ctrl Pts',(-0.0591751035598244,2.4888228351302,
8.88713832319599));
#33169=CARTESIAN_POINT('Ctrl Pts',(-0.0794517219988305,2.48573692842009,
8.88818228584354));
#33170=CARTESIAN_POINT('Ctrl Pts',(-0.0995467167524269,2.48105145677097,
8.88922624849109));
#33171=CARTESIAN_POINT('Ctrl Pts',(-0.119189818671564,2.47480485205643,
8.89027021113865));
#33172=CARTESIAN_POINT('Ctrl Pts',(-0.138796784988069,2.46856973864436,
8.89131225330442));
#33173=CARTESIAN_POINT('Ctrl Pts',(-0.157952797297252,2.46077935650606,
8.89235429547019));
#33174=CARTESIAN_POINT('Ctrl Pts',(-0.176398872778384,2.45152286935919,
8.89339633763596));
#33175=CARTESIAN_POINT('Ctrl Pts',(-0.194825137464267,2.44227632353407,
8.89443726066481));
#33176=CARTESIAN_POINT('Ctrl Pts',(-0.212542311730008,2.43156710108704,
8.89547818369367));
#33177=CARTESIAN_POINT('Ctrl Pts',(-0.229312553779454,2.41953191183221,
8.89651910672253));
#33178=CARTESIAN_POINT('Ctrl Pts',(-0.24609140858808,2.40749054161789,8.89756056434232));
#33179=CARTESIAN_POINT('Ctrl Pts',(-0.261921752449025,2.39412226004271,
8.89860202196211));
#33180=CARTESIAN_POINT('Ctrl Pts',(-0.276595385917055,2.37960665673298,
8.8996434795819));
#33181=CARTESIAN_POINT('Ctrl Pts',(-0.291273502819832,2.36508661827361,
8.9006852554124));
#33182=CARTESIAN_POINT('Ctrl Pts',(-0.304793708545817,2.34941910293927,
8.9017270312429));
#33183=CARTESIAN_POINT('Ctrl Pts',(-0.316985912733092,2.33281928856684,
8.9027688070734));
#33184=CARTESIAN_POINT('Ctrl Pts',(-0.329204470646399,2.31618359331893,
8.90381283472599));
#33185=CARTESIAN_POINT('Ctrl Pts',(-0.340088908370759,2.2986122019047,8.90485686237859));
#33186=CARTESIAN_POINT('Ctrl Pts',(-0.349513034957119,2.28034835290366,
8.90590089003119));
#33187=CARTESIAN_POINT('Ctrl Pts',(-0.352846225001586,2.27388866891003,
8.90627014892705));
#33188=CARTESIAN_POINT('Ctrl Pts',(-0.355997173223601,2.26734255865735,
8.90663940782292));
#33189=CARTESIAN_POINT('Ctrl Pts',(-0.358961754194026,2.26072133967196,
8.90700866671878));
#33190=CARTESIAN_POINT('Ctrl Pts',(-0.368144946689633,2.2402112139223,8.90815249633764));
#33191=CARTESIAN_POINT('Ctrl Pts',(-0.375583635340145,2.21887369636888,
8.90929632595649));
#33192=CARTESIAN_POINT('Ctrl Pts',(-0.381149004164054,2.19700683803088,
8.91044015557534));
#33193=CARTESIAN_POINT('Ctrl Pts',(-0.386678846079847,2.17527956826132,
8.91157668348049));
#33194=CARTESIAN_POINT('Ctrl Pts',(-0.390358983079574,2.15303014501776,
8.91271321138565));
#33195=CARTESIAN_POINT('Ctrl Pts',(-0.392110001369189,2.13057183060031,
8.9138497392908));
#33196=CARTESIAN_POINT('Ctrl Pts',(-0.392897752034933,2.12046825130662,
8.91436104212483));
#33197=CARTESIAN_POINT('Ctrl Pts',(-0.393295716606341,2.11032263485194,
8.91487234495886));
#33198=CARTESIAN_POINT('Ctrl Pts',(-0.393299965593714,2.10016451134769,
8.91538364779289));
#33199=CARTESIAN_POINT('',(-0.393299846669849,2.09965271125334,9.04038364779943));
#33200=CARTESIAN_POINT('Ctrl Pts',(-0.393299965593744,2.10016451127551,
8.91538364779652));
#33201=CARTESIAN_POINT('Ctrl Pts',(-0.39330879068897,2.07906620273691,8.9164456180457));
#33202=CARTESIAN_POINT('Ctrl Pts',(-0.391615565117182,2.05797632259616,
8.91750758829488));
#33203=CARTESIAN_POINT('Ctrl Pts',(-0.38825045884592,2.03717905440116,8.91856955854406));
#33204=CARTESIAN_POINT('Ctrl Pts',(-0.384882897301465,2.01636661195281,
8.91963230363565));
#33205=CARTESIAN_POINT('Ctrl Pts',(-0.379841181812565,1.99584788544338,
8.92069504872725));
#33206=CARTESIAN_POINT('Ctrl Pts',(-0.373206497384045,1.97589601009503,
8.92175779381885));
#33207=CARTESIAN_POINT('Ctrl Pts',(-0.366552785195639,1.95588691431706,
8.92282358678086));
#33208=CARTESIAN_POINT('Ctrl Pts',(-0.358297246682395,1.93644856117948,
8.92388937974288));
#33209=CARTESIAN_POINT('Ctrl Pts',(-0.34856954930456,1.91783480217776,8.9249551727049));
#33210=CARTESIAN_POINT('Ctrl Pts',(-0.342716470883866,1.9066350508996,8.92559645188379));
#33211=CARTESIAN_POINT('Ctrl Pts',(-0.336331328015612,1.89573336524099,
8.92623773106268));
#33212=CARTESIAN_POINT('Ctrl Pts',(-0.329449863585307,1.88517989529929,
8.92687901024156));
#33213=CARTESIAN_POINT('Ctrl Pts',(-0.318247267177633,1.8679995021352,8.92792297288912));
#33214=CARTESIAN_POINT('Ctrl Pts',(-0.305663770081435,1.85164658008582,
8.92896693553667));
#33215=CARTESIAN_POINT('Ctrl Pts',(-0.291846234603637,1.83635124626185,
8.93001089818423));
#33216=CARTESIAN_POINT('Ctrl Pts',(-0.278054117971273,1.82108404985262,
8.93105294035));
#33217=CARTESIAN_POINT('Ctrl Pts',(-0.263032912637363,1.80687115951435,
8.93209498251577));
#33218=CARTESIAN_POINT('Ctrl Pts',(-0.246970990128869,1.79391141799347,
8.93313702468154));
#33219=CARTESIAN_POINT('Ctrl Pts',(-0.230926317872829,1.7809655950314,8.9341779477104));
#33220=CARTESIAN_POINT('Ctrl Pts',(-0.213843698931939,1.7692707312228,8.93521887073926));
#33221=CARTESIAN_POINT('Ctrl Pts',(-0.195946034721089,1.75898674295992,
8.93625979376811));
#33222=CARTESIAN_POINT('Ctrl Pts',(-0.178039178736364,1.7486974731087,8.9373012513879));
#33223=CARTESIAN_POINT('Ctrl Pts',(-0.159317071170225,1.73982090691943,
8.9383427090077));
#33224=CARTESIAN_POINT('Ctrl Pts',(-0.140029376487857,1.73247222728014,
8.93938416662749));
#33225=CARTESIAN_POINT('Ctrl Pts',(-0.120735788573881,1.72512130229884,
8.94042594245799));
#33226=CARTESIAN_POINT('Ctrl Pts',(-0.10087696938326,1.7192994211612,8.94146771828849));
#33227=CARTESIAN_POINT('Ctrl Pts',(-0.0807192040880046,1.71507234434066,
8.94250949411899));
#33228=CARTESIAN_POINT('Ctrl Pts',(-0.0605178673256378,1.71083613059764,
8.94355352177159));
#33229=CARTESIAN_POINT('Ctrl Pts',(-0.0400170248655094,1.70820169721761,
8.94459754942419));
#33230=CARTESIAN_POINT('Ctrl Pts',(-0.019490333429555,1.70718322731481,
8.94564157707679));
#33231=CARTESIAN_POINT('Ctrl Pts',(-0.0122303117275964,1.70682300786006,
8.94601083597265));
#33232=CARTESIAN_POINT('Ctrl Pts',(-0.00496705512580053,1.70666445921509,
8.94638009486851));
#33233=CARTESIAN_POINT('Ctrl Pts',(0.00228742631401738,1.70670665187311,
8.94674935376437));
#33234=CARTESIAN_POINT('Ctrl Pts',(0.0227971763442628,1.70682593825855,
8.94779331641192));
#33235=CARTESIAN_POINT('Ctrl Pts',(0.0433586803398914,1.70855423573291,
8.94883727905948));
#33236=CARTESIAN_POINT('Ctrl Pts',(0.063698952493744,1.71189262638904,8.94988124170703));
#33237=CARTESIAN_POINT('Ctrl Pts',(0.0840018065251822,1.71522487571582,
8.9509232838728));
#33238=CARTESIAN_POINT('Ctrl Pts',(0.104083509057827,1.72016127975526,8.95196532603857));
#33239=CARTESIAN_POINT('Ctrl Pts',(0.12367490063912,1.72665108952629,8.95300736820434));
#33240=CARTESIAN_POINT('Ctrl Pts',(0.143245251373644,1.73313392934359,8.95404829123319));
#33241=CARTESIAN_POINT('Ctrl Pts',(0.162325632549298,1.74116666011048,8.95508921426204));
#33242=CARTESIAN_POINT('Ctrl Pts',(0.18066092303681,1.75064842795904,8.9561301372909));
#33243=CARTESIAN_POINT('Ctrl Pts',(0.199005630051624,1.76013506539644,8.95717159491069));
#33244=CARTESIAN_POINT('Ctrl Pts',(0.216603820945569,1.7710719029782,8.95821305253048));
#33245=CARTESIAN_POINT('Ctrl Pts',(0.233223499997948,1.78331136893045,8.95925451015027));
#33246=CARTESIAN_POINT('Ctrl Pts',(0.24984825708684,1.79555457457314,8.96029628598077));
#33247=CARTESIAN_POINT('Ctrl Pts',(0.265493336638524,1.80910073585399,8.96133806181127));
#33248=CARTESIAN_POINT('Ctrl Pts',(0.279959301094467,1.82376155276519,8.96237983764176));
#33249=CARTESIAN_POINT('Ctrl Pts',(0.29445653406085,1.83845405936483,8.96342386529436));
#33250=CARTESIAN_POINT('Ctrl Pts',(0.307769089265066,1.85426546837044,8.96446789294695));
#33251=CARTESIAN_POINT('Ctrl Pts',(0.319736905962473,1.87097336188656,8.96551192059955));
#33252=CARTESIAN_POINT('Ctrl Pts',(0.323969765857149,1.87688272482026,8.96588117949542));
#33253=CARTESIAN_POINT('Ctrl Pts',(0.328034808433888,1.88290397576896,8.96625043839128));
#33254=CARTESIAN_POINT('Ctrl Pts',(0.331926313975184,1.88902651329883,8.96661969728715));
#33255=CARTESIAN_POINT('Ctrl Pts',(0.342928314125601,1.90633605021451,8.9676636599347));
#33256=CARTESIAN_POINT('Ctrl Pts',(0.352605444300693,1.92456008956632,8.96870762258225));
#33257=CARTESIAN_POINT('Ctrl Pts',(0.360809022507467,1.94346968575638,8.96975158522981));
#33258=CARTESIAN_POINT('Ctrl Pts',(0.368997509348145,1.96234449570663,8.97079362739558));
#33259=CARTESIAN_POINT('Ctrl Pts',(0.375717480882778,1.9819017154483,8.97183566956135));
#33260=CARTESIAN_POINT('Ctrl Pts',(0.38086590688818,2.00188755955413,8.97287771172712));
#33261=CARTESIAN_POINT('Ctrl Pts',(0.386008803564934,2.02185193917737,8.97391863475597));
#33262=CARTESIAN_POINT('Ctrl Pts',(0.389583294806029,2.04224332759868,8.97495955778483));
#33263=CARTESIAN_POINT('Ctrl Pts',(0.391536078672314,2.06279262038375,8.97600048081368));
#33264=CARTESIAN_POINT('Ctrl Pts',(0.393489865437496,2.08335246675002,8.97704193843347));
#33265=CARTESIAN_POINT('Ctrl Pts',(0.393820195291432,2.10406964853755,8.97808339605326));
#33266=CARTESIAN_POINT('Ctrl Pts',(0.392525565748284,2.12466921632298,8.97912485367306));
#33267=CARTESIAN_POINT('Ctrl Pts',(0.391230540639369,2.14527507817442,8.98016662950356));
#33268=CARTESIAN_POINT('Ctrl Pts',(0.388309649948731,2.16576252304192,8.98120840533405));
#33269=CARTESIAN_POINT('Ctrl Pts',(0.383813260540295,2.18586193005883,8.98225018116455));
#33270=CARTESIAN_POINT('Ctrl Pts',(0.379307152084117,2.20600478240013,8.98329420881715));
#33271=CARTESIAN_POINT('Ctrl Pts',(0.373218962973318,2.2257572185577,8.98433823646975));
#33272=CARTESIAN_POINT('Ctrl Pts',(0.365649062383452,2.24486425776603,8.98538226412234));
#33273=CARTESIAN_POINT('Ctrl Pts',(0.36297168776921,2.25162216708365,8.98575152301821));
#33274=CARTESIAN_POINT('Ctrl Pts',(0.360109393162196,2.25829953959989,8.98612078191408));
#33275=CARTESIAN_POINT('Ctrl Pts',(0.35706799625136,2.26488582732618,8.98649004080994));
#33276=CARTESIAN_POINT('Ctrl Pts',(0.348469409171012,2.28350647113263,8.9875340034575));
#33277=CARTESIAN_POINT('Ctrl Pts',(0.338384716012229,2.30150817723554,8.98857796610505));
#33278=CARTESIAN_POINT('Ctrl Pts',(0.326925934083533,2.31864199876421,8.9896219287526));
#33279=CARTESIAN_POINT('Ctrl Pts',(0.315488231818954,2.3357443007819,8.99066397091837));
#33280=CARTESIAN_POINT('Ctrl Pts',(0.302681813314068,2.35198124958787,8.99170601308414));
#33281=CARTESIAN_POINT('Ctrl Pts',(0.288664293778539,2.36712883688838,8.99274805524991));
#33282=CARTESIAN_POINT('Ctrl Pts',(0.274661828838778,2.38226015591809,8.99378897827876));
#33283=CARTESIAN_POINT('Ctrl Pts',(0.259451321054667,2.39630387915413,8.99482990130762));
#33284=CARTESIAN_POINT('Ctrl Pts',(0.243230184949942,2.40906951827901,8.99587082433647));
#33285=CARTESIAN_POINT('Ctrl Pts',(0.227000718092483,2.42184171350343,8.99691228195626));
#33286=CARTESIAN_POINT('Ctrl Pts',(0.209760154235766,2.43333404559629,8.99795373957605));
#33287=CARTESIAN_POINT('Ctrl Pts',(0.191738862455026,2.44339641614969,8.99899519719585));
#33288=CARTESIAN_POINT('Ctrl Pts',(0.173712064384002,2.45346186119597,9.00003697302634));
#33289=CARTESIAN_POINT('Ctrl Pts',(0.154904723016358,2.46209614809795,9.00107874885684));
#33290=CARTESIAN_POINT('Ctrl Pts',(0.135570804897655,2.46919567556975,9.00212052468734));
#33291=CARTESIAN_POINT('Ctrl Pts',(0.116195096076183,2.47631054883129,9.00316455233994));
#33292=CARTESIAN_POINT('Ctrl Pts',(0.096291247327418,2.48188384101763,9.00420857999253));
#33293=CARTESIAN_POINT('Ctrl Pts',(0.0761279826925704,2.48586191863303,
9.00525260764513));
#33294=CARTESIAN_POINT('Ctrl Pts',(0.0689965002863075,2.48726891254193,
9.005621866541));
#33295=CARTESIAN_POINT('Ctrl Pts',(0.0618326341312234,2.48847682638425,
9.00599112543686));
#33296=CARTESIAN_POINT('Ctrl Pts',(0.0546484023851182,2.48948484196019,
9.00636038433273));
#33297=CARTESIAN_POINT('Ctrl Pts',(0.0343372611282992,2.49233468693674,
9.00740434698029));
#33298=CARTESIAN_POINT('Ctrl Pts',(0.0137420777018276,2.49359994515231,
9.00844830962784));
#33299=CARTESIAN_POINT('Ctrl Pts',(-0.00686719191505303,2.49324004332621,
9.00949227227539));
#33300=CARTESIAN_POINT('Ctrl Pts',(-0.027438548559685,2.49288080357831,
9.01053431444116));
#33301=CARTESIAN_POINT('Ctrl Pts',(-0.0480232115622961,2.49090229138008,
9.01157635660693));
#33302=CARTESIAN_POINT('Ctrl Pts',(-0.0683475107778663,2.48731577268486,
9.0126183987727));
#33303=CARTESIAN_POINT('Ctrl Pts',(-0.0886499820153858,2.48373310585437,
9.01365932180156));
#33304=CARTESIAN_POINT('Ctrl Pts',(-0.10869191865644,2.47854595971636,9.01470024483041));
#33305=CARTESIAN_POINT('Ctrl Pts',(-0.128206290664371,2.47181720916881,
9.01574116785926));
#33306=CARTESIAN_POINT('Ctrl Pts',(-0.147730684745145,2.46508500291036,
9.01678262547906));
#33307=CARTESIAN_POINT('Ctrl Pts',(-0.166726272064796,2.45680983515309,
9.01782408309885));
#33308=CARTESIAN_POINT('Ctrl Pts',(-0.184942144251628,2.44710415335978,
9.01886554071864));
#33309=CARTESIAN_POINT('Ctrl Pts',(-0.203163582181584,2.43739550605754,
9.01990731654914));
#33310=CARTESIAN_POINT('Ctrl Pts',(-0.220604198909779,2.42625585221344,
9.02094909237964));
#33311=CARTESIAN_POINT('Ctrl Pts',(-0.237039407940149,2.41384265019813,
9.02199086821014));
#33312=CARTESIAN_POINT('Ctrl Pts',(-0.253510142047781,2.40140261676498,
9.02303489586274));
#33313=CARTESIAN_POINT('Ctrl Pts',(-0.268970578871846,2.38768402813433,
9.02407892351533));
#33314=CARTESIAN_POINT('Ctrl Pts',(-0.283230157229812,2.37288379951103,
9.02512295116793));
#33315=CARTESIAN_POINT('Ctrl Pts',(-0.288273583183993,2.36764915264471,
9.0254922100638));
#33316=CARTESIAN_POINT('Ctrl Pts',(-0.293167148962151,2.36227951130538,
9.02586146895966));
#33317=CARTESIAN_POINT('Ctrl Pts',(-0.297903660961291,2.35678453766896,
9.02623072785553));
#33318=CARTESIAN_POINT('Ctrl Pts',(-0.311195734804249,2.34136399289811,
9.02726697911213));
#33319=CARTESIAN_POINT('Ctrl Pts',(-0.323330281225145,2.32485858760565,
9.02830323036874));
#33320=CARTESIAN_POINT('Ctrl Pts',(-0.334127681974604,2.30746947278643,
9.02933948162534));
#33321=CARTESIAN_POINT('Ctrl Pts',(-0.344904881002772,2.29011289265395,
9.03037379407653));
#33322=CARTESIAN_POINT('Ctrl Pts',(-0.354349454542564,2.27187647832869,
9.03140810652771));
#33323=CARTESIAN_POINT('Ctrl Pts',(-0.362323150777052,2.25299289006679,
9.0324424189789));
#33324=CARTESIAN_POINT('Ctrl Pts',(-0.370287998041917,2.23413025824642,
9.03347558358106));
#33325=CARTESIAN_POINT('Ctrl Pts',(-0.376784891220112,2.21462255238723,
9.03450874818322));
#33326=CARTESIAN_POINT('Ctrl Pts',(-0.381722503778977,2.1947249708826,9.03554191278537));
#33327=CARTESIAN_POINT('Ctrl Pts',(-0.386661872350672,2.17482031300087,
9.03657544482225));
#33328=CARTESIAN_POINT('Ctrl Pts',(-0.390040661394329,2.15452622553248,
9.03760897685914));
#33329=CARTESIAN_POINT('Ctrl Pts',(-0.391817972917354,2.13411108469304,
9.03864250889602));
#33330=CARTESIAN_POINT('Ctrl Pts',(-0.392816021718496,2.12264696792117,
9.03922288852952));
#33331=CARTESIAN_POINT('Ctrl Pts',(-0.393309994372249,2.11114484999877,
9.03980326816302));
#33332=CARTESIAN_POINT('Ctrl Pts',(-0.3932998466699,2.09965271131105,9.04038364779652));
#33333=CARTESIAN_POINT('',(-0.393299999929551,2.10000744414488,9.1653836477998));
#33334=CARTESIAN_POINT('Ctrl Pts',(-0.393299846669849,2.09965271125334,
9.04038364779943));
#33335=CARTESIAN_POINT('Ctrl Pts',(-0.393277423792018,2.07425910291527,
9.041666083863));
#33336=CARTESIAN_POINT('Ctrl Pts',(-0.390791705111248,2.04897530882568,
9.04294851992656));
#33337=CARTESIAN_POINT('Ctrl Pts',(-0.385929156388464,2.02421361435397,
9.04423095599012));
#33338=CARTESIAN_POINT('Ctrl Pts',(-0.383565548707071,2.01217734806765,
9.04485432778618));
#33339=CARTESIAN_POINT('Ctrl Pts',(-0.38064107672183,2.00026409950309,9.04547769958224));
#33340=CARTESIAN_POINT('Ctrl Pts',(-0.377169671296976,1.98851937812458,
9.04610107137829));
#33341=CARTESIAN_POINT('Ctrl Pts',(-0.371356098047462,1.96885045742165,
9.04714503402584));
#33342=CARTESIAN_POINT('Ctrl Pts',(-0.3639824965963,1.94957891206686,9.0481889966734));
#33343=CARTESIAN_POINT('Ctrl Pts',(-0.355123681233962,1.93096727823632,
9.04923295932095));
#33344=CARTESIAN_POINT('Ctrl Pts',(-0.346281162617074,1.91238988251172,
9.05027500148672));
#33345=CARTESIAN_POINT('Ctrl Pts',(-0.335959112373765,1.89447067102725,
9.05131704365249));
#33346=CARTESIAN_POINT('Ctrl Pts',(-0.324281071518415,1.87745410213875,
9.05235908581827));
#33347=CARTESIAN_POINT('Ctrl Pts',(-0.312615572695485,1.86045580877792,
9.05340000884712));
#33348=CARTESIAN_POINT('Ctrl Pts',(-0.299597364767039,1.84435885342254,
9.05444093187598));
#33349=CARTESIAN_POINT('Ctrl Pts',(-0.285394219692462,1.82938028644215,
9.05548185490483));
#33350=CARTESIAN_POINT('Ctrl Pts',(-0.271183780252756,1.81439402686016,
9.05652331252463));
#33351=CARTESIAN_POINT('Ctrl Pts',(-0.255787682487004,1.80052784812853,
9.05756477014442));
#33352=CARTESIAN_POINT('Ctrl Pts',(-0.239412150697716,1.78796360452938,
9.05860622776421));
#33353=CARTESIAN_POINT('Ctrl Pts',(-0.223031615469557,1.77539552200607,
9.05964800359471));
#33354=CARTESIAN_POINT('Ctrl Pts',(-0.205671655746578,1.76413058534215,
9.06068977942521));
#33355=CARTESIAN_POINT('Ctrl Pts',(-0.18756857332672,1.75430805577772,9.06173155525572));
#33356=CARTESIAN_POINT('Ctrl Pts',(-0.169426360683397,1.74446429459273,
9.06277558290831));
#33357=CARTESIAN_POINT('Ctrl Pts',(-0.150538491489484,1.7360694641524,9.06381961056091));
#33358=CARTESIAN_POINT('Ctrl Pts',(-0.131163100331721,1.72921551932238,
9.06486363821351));
#33359=CARTESIAN_POINT('Ctrl Pts',(-0.124310278447117,1.72679136887584,
9.06523289710938));
#33360=CARTESIAN_POINT('Ctrl Pts',(-0.117396605658614,1.72455951701898,
9.06560215600524));
#33361=CARTESIAN_POINT('Ctrl Pts',(-0.110433855231836,1.72252251243467,
9.0659714149011));
#33362=CARTESIAN_POINT('Ctrl Pts',(-0.0907488823003548,1.71676352673998,
9.06701537754866));
#33363=CARTESIAN_POINT('Ctrl Pts',(-0.0705535582228659,1.71253134714463,
9.06805934019621));
#33364=CARTESIAN_POINT('Ctrl Pts',(-0.0501091264440478,1.70990518402956,
9.06910330284376));
#33365=CARTESIAN_POINT('Ctrl Pts',(-0.0297023044004944,1.70728385202452,
9.07014534500953));
#33366=CARTESIAN_POINT('Ctrl Pts',(-0.00904799824759791,1.7062628237229,
9.0711873871753));
#33367=CARTESIAN_POINT('Ctrl Pts',(0.0115813720688393,1.70687055335297,
9.07222942934107));
#33368=CARTESIAN_POINT('Ctrl Pts',(0.0321885867656339,1.70747763029096,
9.07327035236992));
#33369=CARTESIAN_POINT('Ctrl Pts',(0.0527701862102576,1.70970999981279,
9.07431127539878));
#33370=CARTESIAN_POINT('Ctrl Pts',(0.073052852572784,1.71354408953804,9.07535219842763));
#33371=CARTESIAN_POINT('Ctrl Pts',(0.093345935584124,1.71738014835185,9.07639365604742));
#33372=CARTESIAN_POINT('Ctrl Pts',(0.1133390528375,1.72281944991755,9.07743511366721));
#33373=CARTESIAN_POINT('Ctrl Pts',(0.132767665055326,1.72978703815809,9.078476571287));
#33374=CARTESIAN_POINT('Ctrl Pts',(0.152202213561197,1.7367567553006,9.0795183471175));
#33375=CARTESIAN_POINT('Ctrl Pts',(0.171071233872581,1.7452554064944,9.080560122948));
#33376=CARTESIAN_POINT('Ctrl Pts',(0.189129718212506,1.75515968958247,9.08160189877849));
#33377=CARTESIAN_POINT('Ctrl Pts',(0.207227236376134,1.7650853810032,9.08264592643109));
#33378=CARTESIAN_POINT('Ctrl Pts',(0.224510104991437,1.77642236619478,9.08368995408368));
#33379=CARTESIAN_POINT('Ctrl Pts',(0.240761273844977,1.78900337780525,9.08473398173628));
#33380=CARTESIAN_POINT('Ctrl Pts',(0.246509099252161,1.79345311670307,9.08510324063215));
#33381=CARTESIAN_POINT('Ctrl Pts',(0.252128176255932,1.79805811483161,9.08547249952801));
#33382=CARTESIAN_POINT('Ctrl Pts',(0.257609988796705,1.80280985266641,9.08584175842388));
#33383=CARTESIAN_POINT('Ctrl Pts',(0.273108078612594,1.81624388733971,9.08688572107143));
#33384=CARTESIAN_POINT('Ctrl Pts',(0.287598664820426,1.8309335221233,9.08792968371898));
#33385=CARTESIAN_POINT('Ctrl Pts',(0.300873730116724,1.84670197686194,9.08897364636654));
#33386=CARTESIAN_POINT('Ctrl Pts',(0.31412437449994,1.86244142382894,9.09001568853231));
#33387=CARTESIAN_POINT('Ctrl Pts',(0.326163422497019,1.87925523317644,9.09105773069808));
#33388=CARTESIAN_POINT('Ctrl Pts',(0.336819483444385,1.8969297521244,9.09209977286385));
#33389=CARTESIAN_POINT('Ctrl Pts',(0.347464099949695,1.91458528891667,9.0931406958927));
#33390=CARTESIAN_POINT('Ctrl Pts',(0.356728275351814,1.93309908818909,9.09418161892156));
#33391=CARTESIAN_POINT('Ctrl Pts',(0.364483877850369,1.95222857926122,9.09522254195041));
#33392=CARTESIAN_POINT('Ctrl Pts',(0.372243463424232,1.9713678947414,9.0962639995702));
#33393=CARTESIAN_POINT('Ctrl Pts',(0.378492636902405,1.99112285791194,9.09730545719));
#33394=CARTESIAN_POINT('Ctrl Pts',(0.383151222805638,2.01123046433295,9.09834691480979));
#33395=CARTESIAN_POINT('Ctrl Pts',(0.387811232109963,2.03134421450434,9.09938869064029));
#33396=CARTESIAN_POINT('Ctrl Pts',(0.390879555659226,2.05181009807242,9.10043046647078));
#33397=CARTESIAN_POINT('Ctrl Pts',(0.392327240977996,2.07235536242607,9.10147224230128));
#33398=CARTESIAN_POINT('Ctrl Pts',(0.393778055501434,2.09294503583486,9.10251626995388));
#33399=CARTESIAN_POINT('Ctrl Pts',(0.393601244433702,2.11361369613625,9.10356029760648));
#33400=CARTESIAN_POINT('Ctrl Pts',(0.391819955956773,2.13408829878467,9.10460432525907));
#33401=CARTESIAN_POINT('Ctrl Pts',(0.391189937571169,2.14132989736541,9.10497358415494));
#33402=CARTESIAN_POINT('Ctrl Pts',(0.390359680607458,2.14854728661034,9.10534284305081));
#33403=CARTESIAN_POINT('Ctrl Pts',(0.389331738537403,2.15572869429157,9.10571210194668));
#33404=CARTESIAN_POINT('Ctrl Pts',(0.386425557706031,2.17603185139879,9.10675606459423));
#33405=CARTESIAN_POINT('Ctrl Pts',(0.381918265913698,2.19616756046058,9.10780002724179));
#33406=CARTESIAN_POINT('Ctrl Pts',(0.375845899555068,2.21586522251151,9.10884398988934));
#33407=CARTESIAN_POINT('Ctrl Pts',(0.36978470396869,2.23552664859055,9.10988603205511));
#33408=CARTESIAN_POINT('Ctrl Pts',(0.362164306241021,2.25475091450429,9.11092807422088));
#33409=CARTESIAN_POINT('Ctrl Pts',(0.353071572591811,2.27327825780387,9.11197011638665));
#33410=CARTESIAN_POINT('Ctrl Pts',(0.343988604395694,2.29178570302781,9.1130110394155));
#33411=CARTESIAN_POINT('Ctrl Pts',(0.333436736027456,2.30959704164456,9.11405196244436));
#33412=CARTESIAN_POINT('Ctrl Pts',(0.321550565199549,2.32647323024996,9.11509288547321));
#33413=CARTESIAN_POINT('Ctrl Pts',(0.309658289944099,2.34335808602597,9.116134343093));
#33414=CARTESIAN_POINT('Ctrl Pts',(0.296430753728987,2.35930622148777,9.11717580071279));
#33415=CARTESIAN_POINT('Ctrl Pts',(0.282045694960607,2.37410785460141,9.11821725833258));
#33416=CARTESIAN_POINT('Ctrl Pts',(0.267656240929639,2.38891401025926,9.11925903416308));
#33417=CARTESIAN_POINT('Ctrl Pts',(0.252109098574853,2.40257246420638,9.12030080999358));
#33418=CARTESIAN_POINT('Ctrl Pts',(0.235617930677045,2.41491122676632,9.12134258582408));
#33419=CARTESIAN_POINT('Ctrl Pts',(0.219091116745591,2.42727665984154,9.12238661347667));
#33420=CARTESIAN_POINT('Ctrl Pts',(0.201616826078801,2.43831631321023,9.12343064112927));
#33421=CARTESIAN_POINT('Ctrl Pts',(0.183437169948442,2.44790184633213,9.12447466878187));
#33422=CARTESIAN_POINT('Ctrl Pts',(0.177007263869615,2.45129212375253,9.12484392767773));
#33423=CARTESIAN_POINT('Ctrl Pts',(0.170489320673381,2.4545009320404,9.1252131865736));
#33424=CARTESIAN_POINT('Ctrl Pts',(0.163894620900134,2.45752404568085,9.12558244546946));
#33425=CARTESIAN_POINT('Ctrl Pts',(0.145250194693487,2.46607094260136,9.12662640811701));
#33426=CARTESIAN_POINT('Ctrl Pts',(0.125879851508083,2.47318095410641,9.12767037076457));
#33427=CARTESIAN_POINT('Ctrl Pts',(0.106030622950536,2.47873790013243,9.12871433341212));
#33428=CARTESIAN_POINT('Ctrl Pts',(0.0862179091877993,2.48428462355744,
9.12975637557789));
#33429=CARTESIAN_POINT('Ctrl Pts',(0.0659287432270489,2.48828369920904,
9.13079841774366));
#33430=CARTESIAN_POINT('Ctrl Pts',(0.0454285602405077,2.4906675516529,9.13184045990943));
#33431=CARTESIAN_POINT('Ctrl Pts',(0.0249503941284426,2.49304884387669,
9.13288138293829));
#33432=CARTESIAN_POINT('Ctrl Pts',(0.00426238471054755,2.49381824345169,
9.13392230596714));
#33433=CARTESIAN_POINT('Ctrl Pts',(-0.0163616158652496,2.4929595240305,
9.134963228996));
#33434=CARTESIAN_POINT('Ctrl Pts',(-0.036996208390216,2.4921003635934,9.13600468661579));
#33435=CARTESIAN_POINT('Ctrl Pts',(-0.0575659905876893,2.48961142820284,
9.13704614423558));
#33436=CARTESIAN_POINT('Ctrl Pts',(-0.0777983609566011,2.48552860468773,
9.13808760185537));
#33437=CARTESIAN_POINT('Ctrl Pts',(-0.0980369131967171,2.48144453369203,
9.13912937768587));
#33438=CARTESIAN_POINT('Ctrl Pts',(-0.117937134897336,2.4757657859523,9.14017115351637));
#33439=CARTESIAN_POINT('Ctrl Pts',(-0.137238754535256,2.46857891184061,
9.14121292934687));
#33440=CARTESIAN_POINT('Ctrl Pts',(-0.156582095062032,2.46137650313744,
9.14225695699947));
#33441=CARTESIAN_POINT('Ctrl Pts',(-0.175323582550946,2.45265977052075,
9.14330098465206));
#33442=CARTESIAN_POINT('Ctrl Pts',(-0.193224246771814,2.44256281242929,
9.14434501230466));
#33443=CARTESIAN_POINT('Ctrl Pts',(-0.199555477069242,2.43899165070078,
9.14471427120053));
#33444=CARTESIAN_POINT('Ctrl Pts',(-0.20578178095333,2.43524823326732,9.14508353009639));
#33445=CARTESIAN_POINT('Ctrl Pts',(-0.211893499175158,2.43133975766169,
9.14545278899226));
#33446=CARTESIAN_POINT('Ctrl Pts',(-0.229172447921879,2.4202897800259,9.14649675163981));
#33447=CARTESIAN_POINT('Ctrl Pts',(-0.245636189661819,2.40785162635901,
9.14754071428736));
#33448=CARTESIAN_POINT('Ctrl Pts',(-0.261053315445168,2.39417011489117,
9.14858467693491));
#33449=CARTESIAN_POINT('Ctrl Pts',(-0.276442079764349,2.38051377203795,
9.14962671910068));
#33450=CARTESIAN_POINT('Ctrl Pts',(-0.290787466309704,2.36561904994209,
9.15066876126645));
#33451=CARTESIAN_POINT('Ctrl Pts',(-0.303888971591314,2.34967255144523,
9.15171080343222));
#33452=CARTESIAN_POINT('Ctrl Pts',(-0.316976406062075,2.33374317923725,
9.15275172646107));
#33453=CARTESIAN_POINT('Ctrl Pts',(-0.328822124306866,2.31676482040477,
9.15379264948992));
#33454=CARTESIAN_POINT('Ctrl Pts',(-0.339264241806408,2.29895895112189,
9.15483357251877));
#33455=CARTESIAN_POINT('Ctrl Pts',(-0.34971172210534,2.28114393720863,9.15587503013856));
#33456=CARTESIAN_POINT('Ctrl Pts',(-0.358753775441977,2.26250119034864,
9.15691648775835));
#33457=CARTESIAN_POINT('Ctrl Pts',(-0.366273011986461,2.24327934495371,
9.15795794537814));
#33458=CARTESIAN_POINT('Ctrl Pts',(-0.373794545985521,2.22405162644702,
9.15899972120863));
#33459=CARTESIAN_POINT('Ctrl Pts',(-0.379792102792222,2.20424515498,9.16004149703913));
#33460=CARTESIAN_POINT('Ctrl Pts',(-0.384197565830724,2.18412562278965,
9.16108327286962));
#33461=CARTESIAN_POINT('Ctrl Pts',(-0.388612551377556,2.1639626017739,9.16212730052222));
#33462=CARTESIAN_POINT('Ctrl Pts',(-0.391428472340683,2.14348589867171,
9.16317132817481));
#33463=CARTESIAN_POINT('Ctrl Pts',(-0.392628722184836,2.12296903383913,
9.16421535582741));
#33464=CARTESIAN_POINT('Ctrl Pts',(-0.393053234822147,2.11571248767762,
9.16458461472329));
#33465=CARTESIAN_POINT('Ctrl Pts',(-0.393276113215156,2.10845092039755,
9.16495387361916));
#33466=CARTESIAN_POINT('Ctrl Pts',(-0.393298180452314,2.10119634982288,
9.16532313251504));
#33467=CARTESIAN_POINT('Ctrl Pts',(-0.393299385934505,2.1008000493904,9.16534330427554));
#33468=CARTESIAN_POINT('Ctrl Pts',(-0.393299992428502,2.10040374713497,
9.16536347603603));
#33469=CARTESIAN_POINT('Ctrl Pts',(-0.39329999992955,2.10000744420937,9.16538364779652));
#33470=CARTESIAN_POINT('',(-0.393299850244702,2.10034321639634,9.29038364779335));
#33471=CARTESIAN_POINT('Ctrl Pts',(-0.393299999929551,2.10000744414487,
9.1653836477998));
#33472=CARTESIAN_POINT('Ctrl Pts',(-0.39330038792013,2.07950855577125,9.16642703819617));
#33473=CARTESIAN_POINT('Ctrl Pts',(-0.391693847425995,2.05894822970895,
9.16747042859253));
#33474=CARTESIAN_POINT('Ctrl Pts',(-0.388477579848486,2.03859918603909,
9.16851381898889));
#33475=CARTESIAN_POINT('Ctrl Pts',(-0.385267228201931,2.01828757194696,
9.1695552901962));
#33476=CARTESIAN_POINT('Ctrl Pts',(-0.380453081344955,1.99818719758936,
9.1705967614035));
#33477=CARTESIAN_POINT('Ctrl Pts',(-0.374084194772206,1.97856728109101,
9.1716382326108));
#33478=CARTESIAN_POINT('Ctrl Pts',(-0.367722132165268,1.95896838642086,
9.17267858793014));
#33479=CARTESIAN_POINT('Ctrl Pts',(-0.359808835644594,1.93984963373444,
9.17371894324947));
#33480=CARTESIAN_POINT('Ctrl Pts',(-0.350443549068287,1.92146650477733,
9.17475929856881));
#33481=CARTESIAN_POINT('Ctrl Pts',(-0.341073433052452,1.90307389610927,
9.17580019037285));
#33482=CARTESIAN_POINT('Ctrl Pts',(-0.330250151491237,1.88541833259056,
9.1768410821769));
#33483=CARTESIAN_POINT('Ctrl Pts',(-0.318119796939728,1.86873243894782,
9.17788197398095));
#33484=CARTESIAN_POINT('Ctrl Pts',(-0.305985657120971,1.85204133848557,
9.17892319059444));
#33485=CARTESIAN_POINT('Ctrl Pts',(-0.292544094846466,1.83632108400085,
9.17996440720793));
#33486=CARTESIAN_POINT('Ctrl Pts',(-0.27798210897944,1.8217719692638,9.18100562382141));
#33487=CARTESIAN_POINT('Ctrl Pts',(-0.263388735792879,1.80719149495002,
9.18204908470288));
#33488=CARTESIAN_POINT('Ctrl Pts',(-0.247670679374745,1.79378767756556,
9.18309254558434));
#33489=CARTESIAN_POINT('Ctrl Pts',(-0.231049251744221,1.78172161042817,
9.18413600646581));
#33490=CARTESIAN_POINT('Ctrl Pts',(-0.225434393766891,1.77764559151889,
9.18448849632315));
#33491=CARTESIAN_POINT('Ctrl Pts',(-0.219716686710828,1.77372185895176,
9.18484098618049));
#33492=CARTESIAN_POINT('Ctrl Pts',(-0.2139053238769,1.76995545388975,9.18519347603783));
#33493=CARTESIAN_POINT('Ctrl Pts',(-0.196693918772264,1.75880056214355,
9.18623743868539));
#33494=CARTESIAN_POINT('Ctrl Pts',(-0.178556311766939,1.7489623879815,9.18728140133294));
#33495=CARTESIAN_POINT('Ctrl Pts',(-0.159720122492187,1.74059163550206,
9.1883253639805));
#33496=CARTESIAN_POINT('Ctrl Pts',(-0.140918584417327,1.73223628192382,
9.18936740614627));
#33497=CARTESIAN_POINT('Ctrl Pts',(-0.121421655609795,1.72534334143922,
9.19040944831204));
#33498=CARTESIAN_POINT('Ctrl Pts',(-0.101482198926803,1.72001808819237,
9.1914514904778));
#33499=CARTESIAN_POINT('Ctrl Pts',(-0.0815641569070532,1.71469855418386,
9.19249241350666));
#33500=CARTESIAN_POINT('Ctrl Pts',(-0.061205230328669,1.71094358175297,
9.19353333653551));
#33501=CARTESIAN_POINT('Ctrl Pts',(-0.0406740409346544,1.70880885440229,
9.19457425956436));
#33502=CARTESIAN_POINT('Ctrl Pts',(-0.0201323072568634,1.70667303071129,
9.19561571718416));
#33503=CARTESIAN_POINT('Ctrl Pts',(0.0005811358132983,1.70615920660784,
9.19665717480395));
#33504=CARTESIAN_POINT('Ctrl Pts',(0.021191362947472,1.70727131994667,9.19769863242374));
#33505=CARTESIAN_POINT('Ctrl Pts',(0.0418078874045685,1.70838377308462,
9.19874040825423));
#33506=CARTESIAN_POINT('Ctrl Pts',(0.0623204010020615,1.71112307692653,
9.19978218408473));
#33507=CARTESIAN_POINT('Ctrl Pts',(0.0824588473145895,1.71544125481333,
9.20082395991523));
#33508=CARTESIAN_POINT('Ctrl Pts',(0.10264082333581,1.71976876653961,9.20186798756783));
#33509=CARTESIAN_POINT('Ctrl Pts',(0.122446412133238,1.72568175505601,9.20291201522042));
#33510=CARTESIAN_POINT('Ctrl Pts',(0.141619753901276,1.73308211367536,9.20395604287302));
#33511=CARTESIAN_POINT('Ctrl Pts',(0.148401113565189,1.73569952351694,9.20432530176889));
#33512=CARTESIAN_POINT('Ctrl Pts',(0.155103577558642,1.73850255947007,9.20469456066475));
#33513=CARTESIAN_POINT('Ctrl Pts',(0.161716546775339,1.74148549750525,9.20506381956062));
#33514=CARTESIAN_POINT('Ctrl Pts',(0.180412624050508,1.74991881061851,9.20610778220817));
#33515=CARTESIAN_POINT('Ctrl Pts',(0.198502951430162,1.75984365389283,9.20715174485573));
#33516=CARTESIAN_POINT('Ctrl Pts',(0.215737599590802,1.7711502195184,9.20819570750328));
#33517=CARTESIAN_POINT('Ctrl Pts',(0.232940542759013,1.78243598549814,9.20923774966905));
#33518=CARTESIAN_POINT('Ctrl Pts',(0.249290290382995,1.79509807908818,9.21027979183482));
#33519=CARTESIAN_POINT('Ctrl Pts',(0.26456144684395,1.8089808754672,9.21132183400059));
#33520=CARTESIAN_POINT('Ctrl Pts',(0.27981620232277,1.82284876194101,9.21236275702945));
#33521=CARTESIAN_POINT('Ctrl Pts',(0.293994105192477,1.83793427749729,9.2134036800583));
#33522=CARTESIAN_POINT('Ctrl Pts',(0.306902925963941,1.8540417026511,9.21444460308716));
#33523=CARTESIAN_POINT('Ctrl Pts',(0.319818376369305,1.87015740015865,9.21548606070695));
#33524=CARTESIAN_POINT('Ctrl Pts',(0.33146296987723,1.88729549168208,9.21652751832674));
#33525=CARTESIAN_POINT('Ctrl Pts',(0.34168457342113,1.90522694671485,9.21756897594653));
#33526=CARTESIAN_POINT('Ctrl Pts',(0.351909300110537,1.92316388058887,9.21861075177703));
#33527=CARTESIAN_POINT('Ctrl Pts',(0.360709838642622,1.94189400395128,9.21965252760753));
#33528=CARTESIAN_POINT('Ctrl Pts',(0.36798034222869,1.96116427789198,9.22069430343803));
#33529=CARTESIAN_POINT('Ctrl Pts',(0.375266561173246,1.98047620496709,9.22173833109063));
#33530=CARTESIAN_POINT('Ctrl Pts',(0.38101593764056,2.0003299061597,9.22278235874323));
#33531=CARTESIAN_POINT('Ctrl Pts',(0.385172459953885,2.0204571430418,9.22382638639582));
#33532=CARTESIAN_POINT('Ctrl Pts',(0.386642567413423,2.02757588290406,9.22419564529169));
#33533=CARTESIAN_POINT('Ctrl Pts',(0.387913889462887,2.03472876864225,9.22456490418755));
#33534=CARTESIAN_POINT('Ctrl Pts',(0.388985501480998,2.04190378981744,9.22493416308341));
#33535=CARTESIAN_POINT('Ctrl Pts',(0.392015145267815,2.06218889110064,9.22597812573097));
#33536=CARTESIAN_POINT('Ctrl Pts',(0.393462780426647,2.08277205925253,9.22702208837852));
#33537=CARTESIAN_POINT('Ctrl Pts',(0.393285444071266,2.10338370827154,9.22806605102607));
#33538=CARTESIAN_POINT('Ctrl Pts',(0.393108433945221,2.12395743994115,9.22910809319185));
#33539=CARTESIAN_POINT('Ctrl Pts',(0.391312332757793,2.14455882052535,9.23015013535761));
#33540=CARTESIAN_POINT('Ctrl Pts',(0.387905981924002,2.16491409082454,9.23119217752338));
#33541=CARTESIAN_POINT('Ctrl Pts',(0.384503289457495,2.18524749988319,9.23223310055224));
#33542=CARTESIAN_POINT('Ctrl Pts',(0.379493872882747,2.20533459661122,9.23327402358109));
#33543=CARTESIAN_POINT('Ctrl Pts',(0.372938239351095,2.2249078045188,9.23431494660995));
#33544=CARTESIAN_POINT('Ctrl Pts',(0.366379239016921,2.24449106471581,9.23535640422974));
#33545=CARTESIAN_POINT('Ctrl Pts',(0.358272653687357,2.26355920603384,9.23639786184953));
#33546=CARTESIAN_POINT('Ctrl Pts',(0.348728703935136,2.28186033391512,9.23743931946932));
#33547=CARTESIAN_POINT('Ctrl Pts',(0.339181838090185,2.30016705358884,9.23848109529982));
#33548=CARTESIAN_POINT('Ctrl Pts',(0.328197105538829,2.31770565816276,9.23952287113032));
#33549=CARTESIAN_POINT('Ctrl Pts',(0.315929969147927,2.33425017522766,9.24056464696082));
#33550=CARTESIAN_POINT('Ctrl Pts',(0.30363631706334,2.35083045364164,9.24160867461341));
#33551=CARTESIAN_POINT('Ctrl Pts',(0.290055210998721,2.36641179950358,9.24265270226601));
#33552=CARTESIAN_POINT('Ctrl Pts',(0.275381870494289,2.38080191488497,9.24369672991861));
#33553=CARTESIAN_POINT('Ctrl Pts',(0.270192102292377,2.38589151007331,9.24406598881447));
#33554=CARTESIAN_POINT('Ctrl Pts',(0.264866017492327,2.39083244670933,9.24443524771034));
#33555=CARTESIAN_POINT('Ctrl Pts',(0.25941321417202,2.39561744588732,9.24480450660621));
#33556=CARTESIAN_POINT('Ctrl Pts',(0.243997138744853,2.4091455164803,9.24584846925377));
#33557=CARTESIAN_POINT('Ctrl Pts',(0.227474073502381,2.42150475487572,9.24689243190132));
#33558=CARTESIAN_POINT('Ctrl Pts',(0.21004743459489,2.43251310533587,9.24793639454887));
#33559=CARTESIAN_POINT('Ctrl Pts',(0.192652853867494,2.44350120474914,9.24897843671464));
#33560=CARTESIAN_POINT('Ctrl Pts',(0.174358582191037,2.45314291026621,9.25002047888041));
#33561=CARTESIAN_POINT('Ctrl Pts',(0.155399587219722,2.46129746510589,9.25106252104618));
#33562=CARTESIAN_POINT('Ctrl Pts',(0.136460953911176,2.46944326208177,9.25210344407503));
#33563=CARTESIAN_POINT('Ctrl Pts',(0.116859675628835,2.47610476334489,9.25314436710388));
#33564=CARTESIAN_POINT('Ctrl Pts',(0.0968534890904559,2.4811880004027,9.25418529013274));
#33565=CARTESIAN_POINT('Ctrl Pts',(0.076837027896091,2.48627384807857,9.25522674775253));
#33566=CARTESIAN_POINT('Ctrl Pts',(0.0564159521569811,2.48977961542495,
9.25626820537232));
#33567=CARTESIAN_POINT('Ctrl Pts',(0.0358617237148704,2.49166162279728,
9.25730966299211));
#33568=CARTESIAN_POINT('Ctrl Pts',(0.0153012150598787,2.49354420520491,
9.25835143882261));
#33569=CARTESIAN_POINT('Ctrl Pts',(-0.00539179189535383,2.4938020089592,
9.25939321465311));
#33570=CARTESIAN_POINT('Ctrl Pts',(-0.0259431406443975,2.4924434270739,
9.2604349904836));
#33571=CARTESIAN_POINT('Ctrl Pts',(-0.0465389116001311,2.49108190858302,
9.2614790181362));
#33572=CARTESIAN_POINT('Ctrl Pts',(-0.0669916842830418,2.48809713549467,
9.26252304578879));
#33573=CARTESIAN_POINT('Ctrl Pts',(-0.0870340952873548,2.48354915755026,
9.26356707344139));
#33574=CARTESIAN_POINT('Ctrl Pts',(-0.0941228333486487,2.48194059736508,
9.26393633233726));
#33575=CARTESIAN_POINT('Ctrl Pts',(-0.101160367275178,2.48013694818307,
9.26430559123313));
#33576=CARTESIAN_POINT('Ctrl Pts',(-0.108135381219693,2.47814234003675,
9.264674850129));
#33577=CARTESIAN_POINT('Ctrl Pts',(-0.127855025365576,2.47250321685096,
9.26571881277655));
#33578=CARTESIAN_POINT('Ctrl Pts',(-0.147191128061596,2.46530060682049,
9.2667627754241));
#33579=CARTESIAN_POINT('Ctrl Pts',(-0.165880500746236,2.45660699582619,
9.26780673807166));
#33580=CARTESIAN_POINT('Ctrl Pts',(-0.184535492315925,2.4479293776661,9.26884878023743));
#33581=CARTESIAN_POINT('Ctrl Pts',(-0.202545430758457,2.43776645590382,
9.2698908224032));
#33582=CARTESIAN_POINT('Ctrl Pts',(-0.219664773015213,2.42623960136099,
9.27093286456897));
#33583=CARTESIAN_POINT('Ctrl Pts',(-0.23676572936733,2.41472512647884,9.27197378759782));
#33584=CARTESIAN_POINT('Ctrl Pts',(-0.252977365006309,2.40185001174964,
9.27301471062668));
#33585=CARTESIAN_POINT('Ctrl Pts',(-0.268081151998824,2.38778009997737,
9.27405563365553));
#33586=CARTESIAN_POINT('Ctrl Pts',(-0.283192695902686,2.37370296226511,
9.27509709127532));
#33587=CARTESIAN_POINT('Ctrl Pts',(-0.29719470513914,2.35843029136667,9.27613854889511));
#33588=CARTESIAN_POINT('Ctrl Pts',(-0.309903505881037,2.34216669267809,
9.2771800065149));
#33589=CARTESIAN_POINT('Ctrl Pts',(-0.322616189715624,2.32589812475106,
9.2782217823454));
#33590=CARTESIAN_POINT('Ctrl Pts',(-0.334034454291829,2.30863862783796,
9.2792635581759));
#33591=CARTESIAN_POINT('Ctrl Pts',(-0.344016950735263,2.29062326092797,
9.2803053340064));
#33592=CARTESIAN_POINT('Ctrl Pts',(-0.354021024571285,2.27256895339359,
9.28134936165899));
#33593=CARTESIAN_POINT('Ctrl Pts',(-0.362582829329486,2.25375618432334,
9.28239338931159));
#33594=CARTESIAN_POINT('Ctrl Pts',(-0.369608127265093,2.23444226366582,
9.28343741696419));
#33595=CARTESIAN_POINT('Ctrl Pts',(-0.372092883059036,2.22761118309139,
9.28380667586005));
#33596=CARTESIAN_POINT('Ctrl Pts',(-0.374385886808147,2.22071755067123,
9.28417593475592));
#33597=CARTESIAN_POINT('Ctrl Pts',(-0.376484485645148,2.21377311663354,
9.28454519365178));
#33598=CARTESIAN_POINT('Ctrl Pts',(-0.383718590512525,2.1898348759429,9.28581807035828));
#33599=CARTESIAN_POINT('Ctrl Pts',(-0.38867394028947,2.1651777808366,9.28709094706477));
#33600=CARTESIAN_POINT('Ctrl Pts',(-0.391240571091593,2.14019583973404,
9.28836382377127));
#33601=CARTESIAN_POINT('Ctrl Pts',(-0.392598163313859,2.12698190615625,
9.2890370984453));
#33602=CARTESIAN_POINT('Ctrl Pts',(-0.393288214024346,2.11367743869001,
9.28971037311932));
#33603=CARTESIAN_POINT('Ctrl Pts',(-0.393299850244702,2.10034321639633,
9.29038364779335));
#33604=CARTESIAN_POINT('',(-0.393299960517904,2.09982377112743,9.41538364780035));
#33605=CARTESIAN_POINT('Ctrl Pts',(-0.393299850244757,2.10034321633353,
9.29038364779652));
#33606=CARTESIAN_POINT('Ctrl Pts',(-0.393317722140316,2.07986338143033,
9.29141772041544));
#33607=CARTESIAN_POINT('Ctrl Pts',(-0.391731641870721,2.05935355499808,
9.29245179303436));
#33608=CARTESIAN_POINT('Ctrl Pts',(-0.388554011035329,2.03908472680553,
9.29348586565328));
#33609=CARTESIAN_POINT('Ctrl Pts',(-0.38537523039336,2.01880856445958,9.29452031244514));
#33610=CARTESIAN_POINT('Ctrl Pts',(-0.380603838057588,1.99877431598211,
9.29555475923701));
#33611=CARTESIAN_POINT('Ctrl Pts',(-0.374303944301932,1.97924633637021,
9.29658920602887));
#33612=CARTESIAN_POINT('Ctrl Pts',(-0.368002981927405,1.95971504432665,
9.29762382828868));
#33613=CARTESIAN_POINT('Ctrl Pts',(-0.360173260756547,1.94069089294415,
9.29865845054849));
#33614=CARTESIAN_POINT('Ctrl Pts',(-0.35092797359622,1.92242058861554,9.29969307280829));
#33615=CARTESIAN_POINT('Ctrl Pts',(-0.341662002305568,1.90410940882799,
9.30073000978924));
#33616=CARTESIAN_POINT('Ctrl Pts',(-0.330974525908466,1.88655608541954,
9.30176694677018));
#33617=CARTESIAN_POINT('Ctrl Pts',(-0.319023789824703,1.86998106267987,
9.30280388375113));
#33618=CARTESIAN_POINT('Ctrl Pts',(-0.312832335224616,1.86139385097434,
9.30334110155894));
#33619=CARTESIAN_POINT('Ctrl Pts',(-0.30630249965348,1.85306870619157,9.30387831936676));
#33620=CARTESIAN_POINT('Ctrl Pts',(-0.299460328225751,1.84503254753023,
9.30441553717457));
#33621=CARTESIAN_POINT('Ctrl Pts',(-0.286164098475349,1.82941607065582,
9.30545949982212));
#33622=CARTESIAN_POINT('Ctrl Pts',(-0.271603393677206,1.81479593609752,
9.30650346246968));
#33623=CARTESIAN_POINT('Ctrl Pts',(-0.255953144490233,1.80138171886912,
9.30754742511723));
#33624=CARTESIAN_POINT('Ctrl Pts',(-0.240331685623043,1.78799217853877,
9.308589467283));
#33625=CARTESIAN_POINT('Ctrl Pts',(-0.223625174529091,1.77580467065087,
9.30963150944877));
#33626=CARTESIAN_POINT('Ctrl Pts',(-0.206045737474445,1.76499247162398,
9.31067355161454));
#33627=CARTESIAN_POINT('Ctrl Pts',(-0.188485180459032,1.75419188472898,
9.31171447464339));
#33628=CARTESIAN_POINT('Ctrl Pts',(-0.170054167058535,1.74476408252427,
9.31275539767224));
#33629=CARTESIAN_POINT('Ctrl Pts',(-0.150994123480303,1.73683934040921,
9.3137963207011));
#33630=CARTESIAN_POINT('Ctrl Pts',(-0.131924291160454,1.72891052835315,
9.31483777832089));
#33631=CARTESIAN_POINT('Ctrl Pts',(-0.112225456479429,1.72248661589742,
9.31587923594068));
#33632=CARTESIAN_POINT('Ctrl Pts',(-0.0921599033865566,1.71765010499834,
9.31692069356047));
#33633=CARTESIAN_POINT('Ctrl Pts',(-0.0720882193924271,1.71281211633433,
9.31796246939097));
#33634=CARTESIAN_POINT('Ctrl Pts',(-0.051650317092855,1.70956263188016,
9.31900424522146));
#33635=CARTESIAN_POINT('Ctrl Pts',(-0.0311186819455137,1.7079330189445,
9.32004602105196));
#33636=CARTESIAN_POINT('Ctrl Pts',(-0.0105426672028801,1.7062998835635,
9.32109004870456));
#33637=CARTESIAN_POINT('Ctrl Pts',(0.0101267484021445,1.70629361027658,
9.32213407635715));
#33638=CARTESIAN_POINT('Ctrl Pts',(0.0306163259953106,1.70789347036481,
9.32317810400975));
#33639=CARTESIAN_POINT('Ctrl Pts',(0.0378632210177484,1.70845931990746,
9.32354736290562));
#33640=CARTESIAN_POINT('Ctrl Pts',(0.0450876813134371,1.70922561461252,
9.32391662180149));
#33641=CARTESIAN_POINT('Ctrl Pts',(0.0522779124983442,1.71018990538364,
9.32428588069736));
#33642=CARTESIAN_POINT('Ctrl Pts',(0.0726060152693199,1.71291613231464,
9.32532984334491));
#33643=CARTESIAN_POINT('Ctrl Pts',(0.0927808587729757,1.71724489060391,
9.32637380599247));
#33644=CARTESIAN_POINT('Ctrl Pts',(0.112531535458932,1.72314254216315,9.32741776864002));
#33645=CARTESIAN_POINT('Ctrl Pts',(0.132245878646874,1.72902934435684,9.32845981080579));
#33646=CARTESIAN_POINT('Ctrl Pts',(0.151536889811539,1.73647915977044,9.32950185297157));
#33647=CARTESIAN_POINT('Ctrl Pts',(0.17014404725711,1.74540742649772,9.33054389513734));
#33648=CARTESIAN_POINT('Ctrl Pts',(0.188731220907897,1.75432610440679,9.3315848181662));
#33649=CARTESIAN_POINT('Ctrl Pts',(0.206635326381617,1.76471979078693,9.33262574119505));
#33650=CARTESIAN_POINT('Ctrl Pts',(0.22361613742165,1.77645601058802,9.33366666422391));
#33651=CARTESIAN_POINT('Ctrl Pts',(0.240605669363653,1.7881982578057,9.3347081218437));
#33652=CARTESIAN_POINT('Ctrl Pts',(0.256670345120845,1.80128401081605,9.33574957946349));
#33653=CARTESIAN_POINT('Ctrl Pts',(0.271598816530265,1.81553739637808,9.33679103708329));
#33654=CARTESIAN_POINT('Ctrl Pts',(0.286531849238524,1.8297951369708,9.33783281291379));
#33655=CARTESIAN_POINT('Ctrl Pts',(0.300327479751835,1.84522068650289,9.33887458874429));
#33656=CARTESIAN_POINT('Ctrl Pts',(0.312811832573712,1.86160191401382,9.33991636457479));
#33657=CARTESIAN_POINT('Ctrl Pts',(0.325323170607521,1.87801854991974,9.34096039222739));
#33658=CARTESIAN_POINT('Ctrl Pts',(0.336517173439119,1.89539436879011,9.34200441987999));
#33659=CARTESIAN_POINT('Ctrl Pts',(0.346263361006765,1.91348840565719,9.34304844753258));
#33660=CARTESIAN_POINT('Ctrl Pts',(0.349710459798716,1.91988802932471,9.34341770642844));
#33661=CARTESIAN_POINT('Ctrl Pts',(0.352976876386308,1.92637729406053,9.3437869653243));
#33662=CARTESIAN_POINT('Ctrl Pts',(0.356058285500431,1.93294495719526,9.34415622422015));
#33663=CARTESIAN_POINT('Ctrl Pts',(0.364769994420846,1.95151294586476,9.34520018686771));
#33664=CARTESIAN_POINT('Ctrl Pts',(0.372051304272281,1.97081955057842,9.34624414951526));
#33665=CARTESIAN_POINT('Ctrl Pts',(0.37778385140963,1.99061877851246,9.34728811216281));
#33666=CARTESIAN_POINT('Ctrl Pts',(0.383505852908803,2.01038158363322,9.34833015432858));
#33667=CARTESIAN_POINT('Ctrl Pts',(0.38768448763457,2.03063453090711,9.34937219649435));
#33668=CARTESIAN_POINT('Ctrl Pts',(0.390249831650448,2.05111279414001,9.35041423866012));
#33669=CARTESIAN_POINT('Ctrl Pts',(0.392812420527153,2.0715690640399,9.35145516168897));
#33670=CARTESIAN_POINT('Ctrl Pts',(0.393765038725769,2.09224944672371,9.35249608471783));
#33671=CARTESIAN_POINT('Ctrl Pts',(0.393089034827,2.11288024451545,9.35353700774668));
#33672=CARTESIAN_POINT('Ctrl Pts',(0.392412683750247,2.13352163774723,9.35457846536648));
#33673=CARTESIAN_POINT('Ctrl Pts',(0.390106047584464,2.15411265930102,9.35561992298627));
#33674=CARTESIAN_POINT('Ctrl Pts',(0.38620259712012,2.17438040049418,9.35666138060606));
#33675=CARTESIAN_POINT('Ctrl Pts',(0.382297953981481,2.19465433436588,9.35770315643656));
#33676=CARTESIAN_POINT('Ctrl Pts',(0.376795699818046,2.21460407618743,9.35874493226706));
#33677=CARTESIAN_POINT('Ctrl Pts',(0.369780076191529,2.23396859800635,9.35978670809756));
#33678=CARTESIAN_POINT('Ctrl Pts',(0.36274928813534,2.25337497667862,9.36083073575015));
#33679=CARTESIAN_POINT('Ctrl Pts',(0.354198904521378,2.27219293939679,9.36187476340275));
#33680=CARTESIAN_POINT('Ctrl Pts',(0.344260901793801,2.29018233749778,9.36291879105535));
#33681=CARTESIAN_POINT('Ctrl Pts',(0.340745960493972,2.29654495180546,9.36328804995121));
#33682=CARTESIAN_POINT('Ctrl Pts',(0.337057840837003,2.30280416961069,9.36365730884708));
#33683=CARTESIAN_POINT('Ctrl Pts',(0.333203654514282,2.30895026828967,9.36402656774294));
#33684=CARTESIAN_POINT('Ctrl Pts',(0.322307162641795,2.32632641689679,9.36507053039049));
#33685=CARTESIAN_POINT('Ctrl Pts',(0.310015328313207,2.34289968656694,9.36611449303804));
#33686=CARTESIAN_POINT('Ctrl Pts',(0.296470914319315,2.35843739466778,9.3671584556856));
#33687=CARTESIAN_POINT('Ctrl Pts',(0.282951416734462,2.37394651948028,9.36820049785136));
#33688=CARTESIAN_POINT('Ctrl Pts',(0.26818434653026,2.38842327668046,9.36924254001713));
#33689=CARTESIAN_POINT('Ctrl Pts',(0.252354523221998,2.40166551776661,9.3702845821829));
#33690=CARTESIAN_POINT('Ctrl Pts',(0.236541700895282,2.41489353689388,9.37132550521175));
#33691=CARTESIAN_POINT('Ctrl Pts',(0.219668934308881,2.42688918014886,9.37236642824061));
#33692=CARTESIAN_POINT('Ctrl Pts',(0.201956257018866,2.43748860758688,9.37340735126946));
#33693=CARTESIAN_POINT('Ctrl Pts',(0.184234482959447,2.44809347861457,9.37444880888925));
#33694=CARTESIAN_POINT('Ctrl Pts',(0.165672559532684,2.4573003096507,9.37549026650904));
#33695=CARTESIAN_POINT('Ctrl Pts',(0.146518071588861,2.46498951313412,9.37653172412883));
#33696=CARTESIAN_POINT('Ctrl Pts',(0.127357731113906,2.47268106600442,9.37757349995933));
#33697=CARTESIAN_POINT('Ctrl Pts',(0.10760516140445,2.47885382790631,9.37861527578982));
#33698=CARTESIAN_POINT('Ctrl Pts',(0.0875254409159908,2.48343733150603,
9.37965705162032));
#33699=CARTESIAN_POINT('Ctrl Pts',(0.0674023176560223,2.48803074245278,
9.38070107927292));
#33700=CARTESIAN_POINT('Ctrl Pts',(0.0469513605327151,2.49102793005919,
9.38174510692551));
#33701=CARTESIAN_POINT('Ctrl Pts',(0.026445932075582,2.49240986567192,9.38278913457811));
#33702=CARTESIAN_POINT('Ctrl Pts',(0.0191934308102392,2.49289863818408,
9.38315839347398));
#33703=CARTESIAN_POINT('Ctrl Pts',(0.0119341226015544,2.49318582883786,
9.38352765236985));
#33704=CARTESIAN_POINT('Ctrl Pts',(0.00468003209273598,2.49327215423878,
9.38389691126573));
#33705=CARTESIAN_POINT('Ctrl Pts',(-0.0158286127031104,2.49351621198553,
9.38494087391328));
#33706=CARTESIAN_POINT('Ctrl Pts',(-0.0364175065974294,2.49215242793676,
9.38598483656084));
#33707=CARTESIAN_POINT('Ctrl Pts',(-0.0568137257886784,2.48917488428984,
9.38702879920839));
#33708=CARTESIAN_POINT('Ctrl Pts',(-0.0771724239369054,2.48620281815531,
9.38807084137416));
#33709=CARTESIAN_POINT('Ctrl Pts',(-0.0973384225138492,2.48162293138315,
9.38911288353993));
#33710=CARTESIAN_POINT('Ctrl Pts',(-0.117041705296821,2.47548119689435,
9.3901549257057));
#33711=CARTESIAN_POINT('Ctrl Pts',(-0.136723827063587,2.46934605853191,
9.39119584873456));
#33712=CARTESIAN_POINT('Ctrl Pts',(-0.155943512111755,2.46165259273099,
9.39223677176341));
#33713=CARTESIAN_POINT('Ctrl Pts',(-0.174443892742717,2.45249711812264,
9.39327769479227));
#33714=CARTESIAN_POINT('Ctrl Pts',(-0.192953774687013,2.44333694150115,
9.39431915241206));
#33715=CARTESIAN_POINT('Ctrl Pts',(-0.210742947608435,2.43271356794082,
9.39536061003185));
#33716=CARTESIAN_POINT('Ctrl Pts',(-0.227576837991387,2.42077043630896,
9.39640206765164));
#33717=CARTESIAN_POINT('Ctrl Pts',(-0.244415871861747,2.40882365552972,
9.39744384348214));
#33718=CARTESIAN_POINT('Ctrl Pts',(-0.260298463478385,2.39555676881259,
9.39848561931264));
#33719=CARTESIAN_POINT('Ctrl Pts',(-0.275021870887769,2.38115451362799,
9.39952739514314));
#33720=CARTESIAN_POINT('Ctrl Pts',(-0.289777103276389,2.36672112764198,
9.40057142279574));
#33721=CARTESIAN_POINT('Ctrl Pts',(-0.303367664894849,2.35114802853795,
9.40161545044833));
#33722=CARTESIAN_POINT('Ctrl Pts',(-0.315629580034159,2.33465476387122,
9.40265947810093));
#33723=CARTESIAN_POINT('Ctrl Pts',(-0.319966458692713,2.32882131234833,
9.4030287369968));
#33724=CARTESIAN_POINT('Ctrl Pts',(-0.324137528436977,2.32287301752332,
9.40339799589266));
#33725=CARTESIAN_POINT('Ctrl Pts',(-0.328136882645062,2.316820377843,9.40376725478852));
#33726=CARTESIAN_POINT('Ctrl Pts',(-0.339658331581068,2.29938376798637,
9.40483102591043));
#33727=CARTESIAN_POINT('Ctrl Pts',(-0.349818092913587,2.28097840474098,
9.40589479703233));
#33728=CARTESIAN_POINT('Ctrl Pts',(-0.358459289317414,2.26183889489877,
9.40695856815424));
#33729=CARTESIAN_POINT('Ctrl Pts',(-0.367081814167475,2.24274074094877,
9.40802004072178));
#33730=CARTESIAN_POINT('Ctrl Pts',(-0.374191950452327,2.22291219397477,
9.40908151328933));
#33731=CARTESIAN_POINT('Ctrl Pts',(-0.379677967326944,2.20261350362638,
9.41014298585687));
#33732=CARTESIAN_POINT('Ctrl Pts',(-0.385155640934468,2.182345684017,9.41120284411127));
#33733=CARTESIAN_POINT('Ctrl Pts',(-0.389013881777438,2.16160980076571,
9.41226270236567));
#33734=CARTESIAN_POINT('Ctrl Pts',(-0.391190239428219,2.14068275526673,
9.41332256062008));
#33735=CARTESIAN_POINT('Ctrl Pts',(-0.392601013880606,2.12711727298338,
9.41400958967889));
#33736=CARTESIAN_POINT('Ctrl Pts',(-0.39330607589307,2.11347180629114,9.41469661873771));
#33737=CARTESIAN_POINT('Ctrl Pts',(-0.393299960517938,2.09982377120348,
9.41538364779652));
#33738=CARTESIAN_POINT('',(-0.393426948843716,2.09973322299738,9.54038364779652));
#33739=CARTESIAN_POINT('Ctrl Pts',(-0.393299960517904,2.09982377112743,
9.41538364780035));
#33740=CARTESIAN_POINT('Ctrl Pts',(-0.393289814354333,2.07718000297793,
9.41652351347478));
#33741=CARTESIAN_POINT('Ctrl Pts',(-0.391319955513586,2.05460099316646,
9.41766337914921));
#33742=CARTESIAN_POINT('Ctrl Pts',(-0.387448452243393,2.03240867767088,
9.41880324482365));
#33743=CARTESIAN_POINT('Ctrl Pts',(-0.383550246883438,2.0100632998739,9.4199509722493));
#33744=CARTESIAN_POINT('Ctrl Pts',(-0.377724278371578,1.98811043056177,
9.42109869967495));
#33745=CARTESIAN_POINT('Ctrl Pts',(-0.37007930774543,1.96686023892667,9.42224642710061));
#33746=CARTESIAN_POINT('Ctrl Pts',(-0.366990460804913,1.95827438652418,
9.42271015083751));
#33747=CARTESIAN_POINT('Ctrl Pts',(-0.363605213018767,1.9498029952863,9.42317387457441));
#33748=CARTESIAN_POINT('Ctrl Pts',(-0.359932879358728,1.94146542220533,
9.42363759831132));
#33749=CARTESIAN_POINT('Ctrl Pts',(-0.35166550189812,1.92269537837302,9.42468156095887));
#33750=CARTESIAN_POINT('Ctrl Pts',(-0.341901287220695,1.9045178491005,9.42572552360642));
#33751=CARTESIAN_POINT('Ctrl Pts',(-0.3307478250219,1.88718372655438,9.42676948625397));
#33752=CARTESIAN_POINT('Ctrl Pts',(-0.319614880818674,1.86988149199454,
9.42781152841974));
#33753=CARTESIAN_POINT('Ctrl Pts',(-0.307098105623127,1.85342022836891,
9.42885357058551));
#33754=CARTESIAN_POINT('Ctrl Pts',(-0.293351121657722,1.83802670093661,
9.42989561275128));
#33755=CARTESIAN_POINT('Ctrl Pts',(-0.279618901737133,1.82264970591094,
9.43093653578013));
#33756=CARTESIAN_POINT('Ctrl Pts',(-0.264659562032265,1.80833873581896,
9.43197745880898));
#33757=CARTESIAN_POINT('Ctrl Pts',(-0.248667111632916,1.79528774623894,
9.43301838183783));
#33758=CARTESIAN_POINT('Ctrl Pts',(-0.232666447927859,1.78223005401083,
9.43405983945762));
#33759=CARTESIAN_POINT('Ctrl Pts',(-0.215632173408295,1.77043411273341,
9.43510129707741));
#33760=CARTESIAN_POINT('Ctrl Pts',(-0.197791962042116,1.76005407819547,
9.43614275469719));
#33761=CARTESIAN_POINT('Ctrl Pts',(-0.179946299713597,1.74967087210445,
9.43718453052769));
#33762=CARTESIAN_POINT('Ctrl Pts',(-0.161294863939316,1.74070477244063,
9.43822630635818));
#33763=CARTESIAN_POINT('Ctrl Pts',(-0.142089746140225,1.7332638631907,9.43926808218868));
#33764=CARTESIAN_POINT('Ctrl Pts',(-0.122843116043193,1.72580687024658,
9.44031210984127));
#33765=CARTESIAN_POINT('Ctrl Pts',(-0.103041120146565,1.71988186059964,
9.44135613749387));
#33766=CARTESIAN_POINT('Ctrl Pts',(-0.0829514902189006,1.71554721971292,
9.44240016514646));
#33767=CARTESIAN_POINT('Ctrl Pts',(-0.0758460514431546,1.71401411404864,
9.44276942404234));
#33768=CARTESIAN_POINT('Ctrl Pts',(-0.0687047073434924,1.71267948354105,
9.44313868293822));
#33769=CARTESIAN_POINT('Ctrl Pts',(-0.0615394596976218,1.71154435916037,
9.4435079418341));
#33770=CARTESIAN_POINT('Ctrl Pts',(-0.0412819899758406,1.70833515427195,
9.44455190448165));
#33771=CARTESIAN_POINT('Ctrl Pts',(-0.0207124520729407,1.70670525575265,
9.4455958671292));
#33772=CARTESIAN_POINT('Ctrl Pts',(-0.000100040860850534,1.70670001272333,
9.44663982977675));
#33773=CARTESIAN_POINT('Ctrl Pts',(0.0204744515997068,1.70669477933914,
9.44768187194252));
#33774=CARTESIAN_POINT('Ctrl Pts',(0.0410909333620938,1.70830832859201,
9.44872391410829));
#33775=CARTESIAN_POINT('Ctrl Pts',(0.0614755776515536,1.71153424429892,
9.44976595627406));
#33776=CARTESIAN_POINT('Ctrl Pts',(0.0818383291532756,1.71475669542305,
9.45080687930291));
#33777=CARTESIAN_POINT('Ctrl Pts',(0.101969009916113,1.71958798939108,9.45184780233177));
#33778=CARTESIAN_POINT('Ctrl Pts',(0.121599517991356,1.72596999154577,9.45288872536062));
#33779=CARTESIAN_POINT('Ctrl Pts',(0.141240107783906,1.73235527133043,9.45393018298041));
#33780=CARTESIAN_POINT('Ctrl Pts',(0.160379306996292,1.74029263818211,9.4549716406002));
#33781=CARTESIAN_POINT('Ctrl Pts',(0.178764254648609,1.74967410706611,9.45601309821999));
#33782=CARTESIAN_POINT('Ctrl Pts',(0.197154819703953,1.75905844239786,9.45705487405049));
#33783=CARTESIAN_POINT('Ctrl Pts',(0.214790036028478,1.76988739178421,9.45809664988099));
#33784=CARTESIAN_POINT('Ctrl Pts',(0.231442563029828,1.78200750005985,9.45913842571149));
#33785=CARTESIAN_POINT('Ctrl Pts',(0.248131084846188,1.79415380622457,9.46018245336409));
#33786=CARTESIAN_POINT('Ctrl Pts',(0.263832117219195,1.80759636413703,9.46122648101668));
#33787=CARTESIAN_POINT('Ctrl Pts',(0.278351640562251,1.82214166523873,9.46227050866928));
#33788=CARTESIAN_POINT('Ctrl Pts',(0.283487005650375,1.82728614758221,9.46263976756515));
#33789=CARTESIAN_POINT('Ctrl Pts',(0.288474925473794,1.83256825795341,9.46300902646101));
#33790=CARTESIAN_POINT('Ctrl Pts',(0.293308036395142,1.83797846312559,9.46337828535688));
#33791=CARTESIAN_POINT('Ctrl Pts',(0.306972127713828,1.85327410577244,9.46442224800444));
#33792=CARTESIAN_POINT('Ctrl Pts',(0.319477238105998,1.86968704800722,9.46546621065199));
#33793=CARTESIAN_POINT('Ctrl Pts',(0.330639517170663,1.88701549426038,9.46651017329954));
#33794=CARTESIAN_POINT('Ctrl Pts',(0.341781262020188,1.90431206296942,9.46755221546532));
#33795=CARTESIAN_POINT('Ctrl Pts',(0.351584635012941,1.92252021332621,9.46859425763109));
#33796=CARTESIAN_POINT('Ctrl Pts',(0.359906803609566,1.94140623368005,9.46963629979686));
#33797=CARTESIAN_POINT('Ctrl Pts',(0.368220034327855,1.96027197074473,9.47067722282571));
#33798=CARTESIAN_POINT('Ctrl Pts',(0.375054897093438,1.97981347427841,9.47171814585457));
#33799=CARTESIAN_POINT('Ctrl Pts',(0.380315144137853,1.99977385002204,9.47275906888342));
#33800=CARTESIAN_POINT('Ctrl Pts',(0.385578092708052,2.01974447689443,9.47380052650322));
#33801=CARTESIAN_POINT('Ctrl Pts',(0.389264606902548,2.04013369836372,9.47484198412301));
#33802=CARTESIAN_POINT('Ctrl Pts',(0.391328604254572,2.06067045014027,9.4758834417428));
#33803=CARTESIAN_POINT('Ctrl Pts',(0.393393232247769,2.08121347678982,9.4769252175733));
#33804=CARTESIAN_POINT('Ctrl Pts',(0.393834318962646,2.10190338839271,9.4779669934038));
#33805=CARTESIAN_POINT('Ctrl Pts',(0.392657828679303,2.12246596485476,9.4790087692343));
#33806=CARTESIAN_POINT('Ctrl Pts',(0.391478795385515,2.14307298779246,9.48005279688689));
#33807=CARTESIAN_POINT('Ctrl Pts',(0.388675304535151,2.16355139641863,9.48109682453949));
#33808=CARTESIAN_POINT('Ctrl Pts',(0.384305035280898,2.18363330591187,9.48214085219209));
#33809=CARTESIAN_POINT('Ctrl Pts',(0.382759328330096,2.19073601407084,9.48251011108795));
#33810=CARTESIAN_POINT('Ctrl Pts',(0.38101808648348,2.19778924814953,9.48287936998382));
#33811=CARTESIAN_POINT('Ctrl Pts',(0.379085339378842,2.20478165616189,9.48324862887968));
#33812=CARTESIAN_POINT('Ctrl Pts',(0.373621108707589,2.22455047652922,9.48429259152723));
#33813=CARTESIAN_POINT('Ctrl Pts',(0.36659005522126,2.24394961943798,9.48533655417478));
#33814=CARTESIAN_POINT('Ctrl Pts',(0.358062330703742,2.26271526459126,9.48638051682234));
#33815=CARTESIAN_POINT('Ctrl Pts',(0.34955029385439,2.28144638831817,9.4874225589881));
#33816=CARTESIAN_POINT('Ctrl Pts',(0.339547297965382,2.29954564064235,9.48846460115387));
#33817=CARTESIAN_POINT('Ctrl Pts',(0.328172534142725,2.31676641306794,9.48950664331964));
#33818=CARTESIAN_POINT('Ctrl Pts',(0.316809986637721,2.33396869065449,9.49054756634849));
#33819=CARTESIAN_POINT('Ctrl Pts',(0.304078975301178,2.35029373459713,9.49158848937735));
#33820=CARTESIAN_POINT('Ctrl Pts',(0.290143400769497,2.36552155654468,9.4926294124062));
#33821=CARTESIAN_POINT('Ctrl Pts',(0.276200669289935,2.38075719910471,9.49367087002599));
#33822=CARTESIAN_POINT('Ctrl Pts',(0.261052623566681,2.39489394023539,9.49471232764578));
#33823=CARTESIAN_POINT('Ctrl Pts',(0.244902234035801,2.40774630097578,9.49575378526557));
#33824=CARTESIAN_POINT('Ctrl Pts',(0.228746909856824,2.42060258867269,9.49679556109607));
#33825=CARTESIAN_POINT('Ctrl Pts',(0.211589229949701,2.43217328527357,9.49783733692657));
#33826=CARTESIAN_POINT('Ctrl Pts',(0.193662992051958,2.4423149653601,9.49887911275706));
#33827=CARTESIAN_POINT('Ctrl Pts',(0.175698006184199,2.45247856691827,9.49992314040966));
#33828=CARTESIAN_POINT('Ctrl Pts',(0.156961813304875,2.46120667422723,9.50096716806226));
#33829=CARTESIAN_POINT('Ctrl Pts',(0.137710878535675,2.46840277405705,9.50201119571485));
#33830=CARTESIAN_POINT('Ctrl Pts',(0.130902075244271,2.47094794024218,9.50238045461072));
#33831=CARTESIAN_POINT('Ctrl Pts',(0.124029024073178,2.47330191597236,9.50274971350659));
#33832=CARTESIAN_POINT('Ctrl Pts',(0.117103451291254,2.47546194440406,9.50311897240246));
#33833=CARTESIAN_POINT('Ctrl Pts',(0.0975235863831054,2.48156874108674,
9.50416293505001));
#33834=CARTESIAN_POINT('Ctrl Pts',(0.077406403400487,2.48615801200553,9.50520689769757));
#33835=CARTESIAN_POINT('Ctrl Pts',(0.0570117016007467,2.48914593134271,
9.50625086034512));
#33836=CARTESIAN_POINT('Ctrl Pts',(0.0366545180526232,2.4921283540803,9.50729290251089));
#33837=CARTESIAN_POINT('Ctrl Pts',(0.0160215402250951,2.49351510835516,
9.50833494467666));
#33838=CARTESIAN_POINT('Ctrl Pts',(-0.00461535874382263,2.49327291854851,
9.50937698684243));
#33839=CARTESIAN_POINT('Ctrl Pts',(-0.0252300940074508,2.49303098884992,
9.51041790987129));
#33840=CARTESIAN_POINT('Ctrl Pts',(-0.0458480097155451,2.49116356783821,
9.51145883290014));
#33841=CARTESIAN_POINT('Ctrl Pts',(-0.0661954133476839,2.48768938243358,
9.512499755929));
#33842=CARTESIAN_POINT('Ctrl Pts',(-0.0865532668760106,2.48421341277787,
9.51354121354879));
#33843=CARTESIAN_POINT('Ctrl Pts',(-0.106639602786151,2.47912913812606,
9.51458267116858));
#33844=CARTESIAN_POINT('Ctrl Pts',(-0.126188595482363,2.47250681654191,
9.51562412878838));
#33845=CARTESIAN_POINT('Ctrl Pts',(-0.145743561248111,2.4658824715498,9.51666590461888));
#33846=CARTESIAN_POINT('Ctrl Pts',(-0.164760172269669,2.45771941422547,
9.51770768044937));
#33847=CARTESIAN_POINT('Ctrl Pts',(-0.182991274947575,2.44813658712215,
9.51874945627987));
#33848=CARTESIAN_POINT('Ctrl Pts',(-0.201261784567633,2.43853304652059,
9.51979348393247));
#33849=CARTESIAN_POINT('Ctrl Pts',(-0.218742773211489,2.42750400228088,
9.52083751158507));
#33850=CARTESIAN_POINT('Ctrl Pts',(-0.235214261623028,2.41521285051396,
9.52188153923767));
#33851=CARTESIAN_POINT('Ctrl Pts',(-0.241040011169962,2.41086563124339,
9.52225079813353));
#33852=CARTESIAN_POINT('Ctrl Pts',(-0.246739782897403,2.40636089635743,
9.5226200570294));
#33853=CARTESIAN_POINT('Ctrl Pts',(-0.252304911160714,2.40170701318362,
9.52298931592526));
#33854=CARTESIAN_POINT('Ctrl Pts',(-0.267819426598198,2.38873287513542,
9.52401873925017));
#33855=CARTESIAN_POINT('Ctrl Pts',(-0.282382930556754,2.37451483139563,
9.52504816257507));
#33856=CARTESIAN_POINT('Ctrl Pts',(-0.295787278418756,2.35921955158827,
9.52607758589997));
#33857=CARTESIAN_POINT('Ctrl Pts',(-0.30916686412036,2.34395252710343,9.52710510754747));
#33858=CARTESIAN_POINT('Ctrl Pts',(-0.32139099986214,2.32761273538655,9.52813262919496));
#33859=CARTESIAN_POINT('Ctrl Pts',(-0.332287146187854,2.31040471116002,
9.52916015084246));
#33860=CARTESIAN_POINT('Ctrl Pts',(-0.34317923556318,2.29320309397856,9.53018728991393));
#33861=CARTESIAN_POINT('Ctrl Pts',(-0.352743871297665,2.27513449803517,
9.5312144289854));
#33862=CARTESIAN_POINT('Ctrl Pts',(-0.36085089247073,2.25643376682506,9.53224156805687));
#33863=CARTESIAN_POINT('Ctrl Pts',(-0.368955606577506,2.23773835740031,
9.53326841482888));
#33864=CARTESIAN_POINT('Ctrl Pts',(-0.375603236691946,2.21841186921687,
9.53429526160089));
#33865=CARTESIAN_POINT('Ctrl Pts',(-0.380711562407097,2.19870965631359,
9.5353221083729));
#33866=CARTESIAN_POINT('Ctrl Pts',(-0.385828946432143,2.1789725065719,9.53635077599518));
#33867=CARTESIAN_POINT('Ctrl Pts',(-0.389401416802549,2.15885904512728,
9.53737944361746));
#33868=CARTESIAN_POINT('Ctrl Pts',(-0.391397696698209,2.13863590324215,
9.53840811123974));
#33869=CARTESIAN_POINT('Ctrl Pts',(-0.392675635858218,2.12568985043182,
9.53906662342533));
#33870=CARTESIAN_POINT('Ctrl Pts',(-0.393308701435708,2.11269901741784,
9.53972513561093));
#33871=CARTESIAN_POINT('Ctrl Pts',(-0.393299909580444,2.09973330914082,
9.54038364779652));
#33872=CARTESIAN_POINT('',(-0.39335257410733,2.10032199862207,9.66538364779652));
#33873=CARTESIAN_POINT('Ctrl Pts',(-0.393713022906921,2.09973302901478,
9.54038364779652));
#33874=CARTESIAN_POINT('Ctrl Pts',(-0.39383959327844,2.08346547400357,9.54120898501369));
#33875=CARTESIAN_POINT('Ctrl Pts',(-0.385530294422347,1.93677881389653,
9.54865777007186));
#33876=CARTESIAN_POINT('Ctrl Pts',(-0.201254141221434,1.68074851088445,
9.56273000297078));
#33877=CARTESIAN_POINT('Ctrl Pts',(0.243571655413408,1.7038335082775,9.58260034649366));
#33878=CARTESIAN_POINT('Ctrl Pts',(0.464953617493051,2.09034732862847,9.60247069001639));
#33879=CARTESIAN_POINT('Ctrl Pts',(0.259803933242123,2.48571616087013,9.62234103353921));
#33880=CARTESIAN_POINT('Ctrl Pts',(-0.183680490646769,2.52724292602718,
9.64221137706198));
#33881=CARTESIAN_POINT('Ctrl Pts',(-0.382233828622705,2.27422629591118,
9.65655891514776));
#33882=CARTESIAN_POINT('Ctrl Pts',(-0.393756568946857,2.12203738788098,
9.66428300539261));
#33883=CARTESIAN_POINT('Ctrl Pts',(-0.393564314774363,2.10032217195309,
9.66538364779652));
#33884=CARTESIAN_POINT('',(-0.393065748709506,2.1000925098763,9.7903836449317));
#33885=CARTESIAN_POINT('Ctrl Pts',(-0.393299868223561,2.10032195547701,
9.66538364779652));
#33886=CARTESIAN_POINT('Ctrl Pts',(-0.393316446318738,2.08007020294019,
9.6664108124149));
#33887=CARTESIAN_POINT('Ctrl Pts',(-0.391764536557221,2.05976190594462,
9.66743797703327));
#33888=CARTESIAN_POINT('Ctrl Pts',(-0.38864436446938,2.03966387511456,9.66846514165165));
#33889=CARTESIAN_POINT('Ctrl Pts',(-0.385528386016173,2.01959285683246,
9.66949092572017));
#33890=CARTESIAN_POINT('Ctrl Pts',(-0.380848399549848,1.99973229598539,
9.67051670978869));
#33891=CARTESIAN_POINT('Ctrl Pts',(-0.374656452113087,1.98034452419536,
9.67154249385721));
#33892=CARTESIAN_POINT('Ctrl Pts',(-0.368462833957878,1.96095152117423,
9.67256855470398));
#33893=CARTESIAN_POINT('Ctrl Pts',(-0.360756643960991,1.94203229391291,
9.67359461555075));
#33894=CARTESIAN_POINT('Ctrl Pts',(-0.351640021998056,1.92383477945631,
9.67462067639753));
#33895=CARTESIAN_POINT('Ctrl Pts',(-0.342521947302668,1.90563436522829,
9.67564690074695));
#33896=CARTESIAN_POINT('Ctrl Pts',(-0.331993363300273,1.8881565565742,9.67667312509638));
#33897=CARTESIAN_POINT('Ctrl Pts',(-0.320202169246142,1.87162429899382,
9.6776993494458));
#33898=CARTESIAN_POINT('Ctrl Pts',(-0.308386218692417,1.85505733069404,
9.67872772843051));
#33899=CARTESIAN_POINT('Ctrl Pts',(-0.295302856727771,1.83944045748286,
9.67975610741521));
#33900=CARTESIAN_POINT('Ctrl Pts',(-0.281140214503373,1.82496351189524,
9.68078448639991));
#33901=CARTESIAN_POINT('Ctrl Pts',(-0.275780327539312,1.81948467604632,
9.68117367896913));
#33902=CARTESIAN_POINT('Ctrl Pts',(-0.270266219843183,1.81416871195178,
9.68156287153835));
#33903=CARTESIAN_POINT('Ctrl Pts',(-0.264609301124671,1.8090243863168,9.68195206410757));
#33904=CARTESIAN_POINT('Ctrl Pts',(-0.249435291368448,1.79522534636968,
9.68299602675512));
#33905=CARTESIAN_POINT('Ctrl Pts',(-0.23313375991602,1.78257534514332,9.68403998940267));
#33906=CARTESIAN_POINT('Ctrl Pts',(-0.215904865923144,1.77126001327689,
9.68508395205022));
#33907=CARTESIAN_POINT('Ctrl Pts',(-0.198707666337281,1.75996549718273,
9.68612599421599));
#33908=CARTESIAN_POINT('Ctrl Pts',(-0.180587065928504,1.75000122589602,
9.68716803638176));
#33909=CARTESIAN_POINT('Ctrl Pts',(-0.161775502006798,1.7415120965075,9.68821007854753));
#33910=CARTESIAN_POINT('Ctrl Pts',(-0.142984141409238,1.73303208431059,
9.68925100157639));
#33911=CARTESIAN_POINT('Ctrl Pts',(-0.123503945868713,1.7260243963122,9.69029192460524));
#33912=CARTESIAN_POINT('Ctrl Pts',(-0.103590947029434,1.72058755200502,
9.69133284763409));
#33913=CARTESIAN_POINT('Ctrl Pts',(-0.0836677213929321,1.71514791547629,
9.69237430525388));
#33914=CARTESIAN_POINT('Ctrl Pts',(-0.0633119539506658,1.71128094368098,
9.69341576287367));
#33915=CARTESIAN_POINT('Ctrl Pts',(-0.0427942901722567,1.70903511829238,
9.69445722049347));
#33916=CARTESIAN_POINT('Ctrl Pts',(-0.0222703573530727,1.70678860670622,
9.69549899632396));
#33917=CARTESIAN_POINT('Ctrl Pts',(-0.00158516445215278,1.70616427163879,
9.69654077215446));
#33918=CARTESIAN_POINT('Ctrl Pts',(0.0189870263641044,1.70715857801162,
9.69758254798496));
#33919=CARTESIAN_POINT('Ctrl Pts',(0.0396036844376565,1.70815503360025,
9.69862657563756));
#33920=CARTESIAN_POINT('Ctrl Pts',(0.0601061222521713,1.7107770222481,9.69967060329015));
#33921=CARTESIAN_POINT('Ctrl Pts',(0.0802259545891204,1.71496923991678,
9.70071463094275));
#33922=CARTESIAN_POINT('Ctrl Pts',(0.0873420755609822,1.71645197235565,
9.70108388983862));
#33923=CARTESIAN_POINT('Ctrl Pts',(0.0944104563888153,1.71813067024748,
9.70145314873449));
#33924=CARTESIAN_POINT('Ctrl Pts',(0.101419709838481,1.72000140466539,9.70182240763036));
#33925=CARTESIAN_POINT('Ctrl Pts',(0.121236155347336,1.72529031409351,9.70286637027791));
#33926=CARTESIAN_POINT('Ctrl Pts',(0.140696816394127,1.73214925937274,9.70391033292547));
#33927=CARTESIAN_POINT('Ctrl Pts',(0.159537261646172,1.74051042832032,9.70495429557302));
#33928=CARTESIAN_POINT('Ctrl Pts',(0.178343047869007,1.74885621599665,9.70599633773879));
#33929=CARTESIAN_POINT('Ctrl Pts',(0.19653019399076,1.75869850116809,9.70703837990456));
#33930=CARTESIAN_POINT('Ctrl Pts',(0.213851045427472,1.76992028179608,9.70808042207033));
#33931=CARTESIAN_POINT('Ctrl Pts',(0.231153294541837,1.78113001040797,9.70912134509918));
#33932=CARTESIAN_POINT('Ctrl Pts',(0.247590465910109,1.79371591946494,9.71016226812803));
#33933=CARTESIAN_POINT('Ctrl Pts',(0.262941128023705,1.80751606335797,9.71120319115689));
#33934=CARTESIAN_POINT('Ctrl Pts',(0.278299673837276,1.82132329464522,9.71224464877668));
#33935=CARTESIAN_POINT('Ctrl Pts',(0.292570037680396,1.83634552666361,9.71328610639647));
#33936=CARTESIAN_POINT('Ctrl Pts',(0.30556495001116,1.85238143986228,9.71432756401626));
#33937=CARTESIAN_POINT('Ctrl Pts',(0.318563832854169,1.86842225273154,9.71536933984675));
#33938=CARTESIAN_POINT('Ctrl Pts',(0.330286053632177,1.88547676942525,9.71641111567725));
#33939=CARTESIAN_POINT('Ctrl Pts',(0.340586121636195,1.90331247180155,9.71745289150775));
#33940=CARTESIAN_POINT('Ctrl Pts',(0.350908453470948,1.92118672645329,9.71849691916034));
#33941=CARTESIAN_POINT('Ctrl Pts',(0.359802178515282,1.93984487308267,9.71954094681294));
#33942=CARTESIAN_POINT('Ctrl Pts',(0.367168515626677,1.95903131151741,9.72058497446553));
#33943=CARTESIAN_POINT('Ctrl Pts',(0.36977389250688,1.96581730330075,9.72095423336141));
#33944=CARTESIAN_POINT('Ctrl Pts',(0.372188655523025,1.9726692339568,9.72132349225728));
#33945=CARTESIAN_POINT('Ctrl Pts',(0.374409944071579,1.97957540209609,9.72169275115315));
#33946=CARTESIAN_POINT('Ctrl Pts',(0.380689934344148,1.99910040651919,9.7227367138007));
#33947=CARTESIAN_POINT('Ctrl Pts',(0.385457217804642,2.01917614977143,9.72378067644826));
#33948=CARTESIAN_POINT('Ctrl Pts',(0.388625670692114,2.039543585294,9.72482463909581));
#33949=CARTESIAN_POINT('Ctrl Pts',(0.391788294869081,2.05987355272421,9.72586668126158));
#33950=CARTESIAN_POINT('Ctrl Pts',(0.393357756093461,2.08049343761516,9.72690872342735));
#33951=CARTESIAN_POINT('Ctrl Pts',(0.393298371872983,2.10113167224099,9.72795076559312));
#33952=CARTESIAN_POINT('Ctrl Pts',(0.393239051430224,2.12174774172704,9.72899168862198));
#33953=CARTESIAN_POINT('Ctrl Pts',(0.39155433161465,2.14238138969642,9.73003261165083));
#33954=CARTESIAN_POINT('Ctrl Pts',(0.388260514317251,2.16275876848779,9.73107353467968));
#33955=CARTESIAN_POINT('Ctrl Pts',(0.384965005401136,2.18314661256979,9.73211499229948));
#33956=CARTESIAN_POINT('Ctrl Pts',(0.380058849553642,2.20327719561725,9.73315644991927));
#33957=CARTESIAN_POINT('Ctrl Pts',(0.373609947470832,2.22288408013588,9.73419790753906));
#33958=CARTESIAN_POINT('Ctrl Pts',(0.367159074967286,2.24249695541253,9.73523968336956));
#33959=CARTESIAN_POINT('Ctrl Pts',(0.359164781894791,2.26158512656372,9.73628145920006));
#33960=CARTESIAN_POINT('Ctrl Pts',(0.349743816920492,2.27990039612487,9.73732323503056));
#33961=CARTESIAN_POINT('Ctrl Pts',(0.340302488316614,2.29825525455681,9.73836726268316));
#33962=CARTESIAN_POINT('Ctrl Pts',(0.329428718633892,2.31583324971255,9.73941129033576));
#33963=CARTESIAN_POINT('Ctrl Pts',(0.317283949056236,2.33241296364721,9.74045531798835));
#33964=CARTESIAN_POINT('Ctrl Pts',(0.31298850324731,2.33827699114303,9.74082457688421));
#33965=CARTESIAN_POINT('Ctrl Pts',(0.308534432124841,2.34401644099237,9.74119383578008));
#33966=CARTESIAN_POINT('Ctrl Pts',(0.303930025930211,2.34962257377501,9.74156309467594));
#33967=CARTESIAN_POINT('Ctrl Pts',(0.290912524834874,2.3654721397242,9.74260705732349));
#33968=CARTESIAN_POINT('Ctrl Pts',(0.276613097141096,2.38034791958114,9.74365101997105));
#33969=CARTESIAN_POINT('Ctrl Pts',(0.261202933485644,2.3940372723627,9.7446949826186));
#33970=CARTESIAN_POINT('Ctrl Pts',(0.245821118486778,2.40770144210469,9.74573702478437));
#33971=CARTESIAN_POINT('Ctrl Pts',(0.229333127803274,2.42018298947153,9.74677906695014));
#33972=CARTESIAN_POINT('Ctrl Pts',(0.21194798486347,2.4313049074679,9.74782110911591));
#33973=CARTESIAN_POINT('Ctrl Pts',(0.194581513294059,2.44241488069908,9.74886203214476));
#33974=CARTESIAN_POINT('Ctrl Pts',(0.176320403371528,2.45216770458646,9.74990295517362));
#33975=CARTESIAN_POINT('Ctrl Pts',(0.157403735620761,2.46042884736468,9.75094387820247));
#33976=CARTESIAN_POINT('Ctrl Pts',(0.138477352762478,2.46869423285051,9.75198533582226));
#33977=CARTESIAN_POINT('Ctrl Pts',(0.118895407301652,2.47546609751238,9.75302679344205));
#33978=CARTESIAN_POINT('Ctrl Pts',(0.0989186805275231,2.4806573060414,9.75406825106184));
#33979=CARTESIAN_POINT('Ctrl Pts',(0.0789358499924424,2.48585010071094,
9.75511002689234));
#33980=CARTESIAN_POINT('Ctrl Pts',(0.0585587186387426,2.48946112790821,
9.75615180272284));
#33981=CARTESIAN_POINT('Ctrl Pts',(0.0380591735014942,2.49145419823063,
9.75719357855334));
#33982=CARTESIAN_POINT('Ctrl Pts',(0.0175153181322421,2.49345157661978,
9.75823760620593));
#33983=CARTESIAN_POINT('Ctrl Pts',(-0.00315074292368206,2.49382400277443,
9.75928163385853));
#33984=CARTESIAN_POINT('Ctrl Pts',(-0.0236654464639412,2.49258736179819,
9.76032566151113));
#33985=CARTESIAN_POINT('Ctrl Pts',(-0.030921228204479,2.49214997809448,
9.76069492040699));
#33986=CARTESIAN_POINT('Ctrl Pts',(-0.0381581295777627,2.49151178325602,
9.76106417930286));
#33987=CARTESIAN_POINT('Ctrl Pts',(-0.0453643146653507,2.49067501706014,
9.76143343819873));
#33988=CARTESIAN_POINT('Ctrl Pts',(-0.0657375220463668,2.48830932550062,
9.76247740084628));
#33989=CARTESIAN_POINT('Ctrl Pts',(-0.0859858826766692,2.4843386390981,
9.76352136349384));
#33990=CARTESIAN_POINT('Ctrl Pts',(-0.10583793562551,2.47879179159867,9.76456532614139));
#33991=CARTESIAN_POINT('Ctrl Pts',(-0.125653468583777,2.47325514812292,
9.76560736830716));
#33992=CARTESIAN_POINT('Ctrl Pts',(-0.145073424360301,2.46614823746583,
9.76664941047293));
#33993=CARTESIAN_POINT('Ctrl Pts',(-0.163835824145666,2.4575509931835,9.7676914526387));
#33994=CARTESIAN_POINT('Ctrl Pts',(-0.182578073408403,2.44896298220649,
9.76873237566755));
#33995=CARTESIAN_POINT('Ctrl Pts',(-0.200663491109591,2.43888809382229,
9.76977329869641));
#33996=CARTESIAN_POINT('Ctrl Pts',(-0.217849541924163,2.4274545267414,9.77081422172526));
#33997=CARTESIAN_POINT('Ctrl Pts',(-0.235044419046517,2.41601508767844,
9.77185567934505));
#33998=CARTESIAN_POINT('Ctrl Pts',(-0.251338385001536,2.4032159700336,9.77289713696484));
#33999=CARTESIAN_POINT('Ctrl Pts',(-0.266517009237516,2.38922927546687,
9.77393859458463));
#34000=CARTESIAN_POINT('Ctrl Pts',(-0.281700271204945,2.37523830735516,
9.77498037041513));
#34001=CARTESIAN_POINT('Ctrl Pts',(-0.295766996918788,2.36005956474198,
9.77602214624563));
#34002=CARTESIAN_POINT('Ctrl Pts',(-0.308539580316651,2.34390206513686,
9.77706392207613));
#34003=CARTESIAN_POINT('Ctrl Pts',(-0.321339771943368,2.32770964072969,
9.77810794972873));
#34004=CARTESIAN_POINT('Ctrl Pts',(-0.332839826783865,2.3105348475876,9.77915197738132));
#34005=CARTESIAN_POINT('Ctrl Pts',(-0.342905016613257,2.29261630144269,
9.78019600503392));
#34006=CARTESIAN_POINT('Ctrl Pts',(-0.346464942323886,2.28627874654312,
9.78056526392979));
#34007=CARTESIAN_POINT('Ctrl Pts',(-0.349845802153086,2.27984836389872,
9.78093452282565));
#34008=CARTESIAN_POINT('Ctrl Pts',(-0.353043072349212,2.27333631779356,
9.78130378172152));
#34009=CARTESIAN_POINT('Ctrl Pts',(-0.362743512461029,2.25357892809122,
9.7824241042421));
#34010=CARTESIAN_POINT('Ctrl Pts',(-0.370801759049986,2.23296418808786,
9.78354442676268));
#34011=CARTESIAN_POINT('Ctrl Pts',(-0.377083179295149,2.21177283163928,
9.78466474928327));
#34012=CARTESIAN_POINT('Ctrl Pts',(-0.383333005235826,2.1906880635325,9.78577943680261));
#34013=CARTESIAN_POINT('Ctrl Pts',(-0.387823576188697,2.16903297057527,
9.78689412432196));
#34014=CARTESIAN_POINT('Ctrl Pts',(-0.390468833763719,2.14710604907229,
9.78800881184131));
#34015=CARTESIAN_POINT('Ctrl Pts',(-0.392347399310581,2.13153434835279,
9.78880042230266));
#34016=CARTESIAN_POINT('Ctrl Pts',(-0.393296284805524,2.11582603520907,
9.78959203276402));
#34017=CARTESIAN_POINT('Ctrl Pts',(-0.39329998909922,2.10009259888561,9.79038364322537));
#34018=CARTESIAN_POINT('',(-0.393299834084712,2.09963873979202,9.91538365013564));
#34019=CARTESIAN_POINT('Ctrl Pts',(-0.392672473494722,2.10009236043514,
9.79038364779652));
#34020=CARTESIAN_POINT('Ctrl Pts',(-0.392522896058815,2.02871865682851,
9.79398047361245));
#34021=CARTESIAN_POINT('Ctrl Pts',(-0.339736212547102,1.82570629495234,
9.80420074726931));
#34022=CARTESIAN_POINT('Ctrl Pts',(-0.0137707264308251,1.63515012361188,
9.8210444687671));
#34023=CARTESIAN_POINT('Ctrl Pts',(0.383399755879578,1.8367896892674,9.84091481228989));
#34024=CARTESIAN_POINT('Ctrl Pts',(0.428853157334091,2.279888882172,9.86078515581266));
#34025=CARTESIAN_POINT('Ctrl Pts',(0.0808921700199272,2.55796451534366,
9.88065549933548));
#34026=CARTESIAN_POINT('Ctrl Pts',(-0.305777301598321,2.42786420633564,
9.8988549966634));
#34027=CARTESIAN_POINT('Ctrl Pts',(-0.392338317521313,2.19756855304251,
9.91043104615043));
#34028=CARTESIAN_POINT('Ctrl Pts',(-0.393224617787252,2.09963885513283,
9.91538364779652));
#34029=CARTESIAN_POINT('',(-0.393532055459869,2.10009220002109,10.0403836856852));
#34030=CARTESIAN_POINT('Ctrl Pts',(-0.393299834084712,2.09963873979202,
9.91538365013564));
#34031=CARTESIAN_POINT('Ctrl Pts',(-0.393275337824574,2.07296994307694,
9.91673212643577));
#34032=CARTESIAN_POINT('Ctrl Pts',(-0.390534469167157,2.04642365724893,
9.9180806027359));
#34033=CARTESIAN_POINT('Ctrl Pts',(-0.385173622860435,2.02046277442249,
9.91942907903603));
#34034=CARTESIAN_POINT('Ctrl Pts',(-0.383892049517696,2.01425652013338,
9.91975144815103));
#34035=CARTESIAN_POINT('Ctrl Pts',(-0.382460952053443,2.0080836142271,9.92007381726604));
#34036=CARTESIAN_POINT('Ctrl Pts',(-0.380882036249165,2.00195019396914,
9.92039618638104));
#34037=CARTESIAN_POINT('Ctrl Pts',(-0.375768863036924,1.9820876781355,9.92144014902859));
#34038=CARTESIAN_POINT('Ctrl Pts',(-0.369082564124017,1.96256702585223,
9.92248411167614));
#34039=CARTESIAN_POINT('Ctrl Pts',(-0.360888606771479,1.94365325874026,
9.92352807432368));
#34040=CARTESIAN_POINT('Ctrl Pts',(-0.352709723086441,1.92477428554096,
9.92457011648945));
#34041=CARTESIAN_POINT('Ctrl Pts',(-0.343028920867443,1.90650067260202,
9.92561215865521));
#34042=CARTESIAN_POINT('Ctrl Pts',(-0.331961003905475,1.88908110116429,
9.92665420082097));
#34043=CARTESIAN_POINT('Ctrl Pts',(-0.320904973712453,1.87168023807262,
9.92769512384982));
#34044=CARTESIAN_POINT('Ctrl Pts',(-0.308465154437204,1.85513222895444,
9.92873604687867));
#34045=CARTESIAN_POINT('Ctrl Pts',(-0.294801523954965,1.83965993110197,
9.92977696990752));
#34046=CARTESIAN_POINT('Ctrl Pts',(-0.281130876188233,1.82417968708059,
9.93081842752731));
#34047=CARTESIAN_POINT('Ctrl Pts',(-0.266235636533031,1.809776820191,9.93185988514709));
#34048=CARTESIAN_POINT('Ctrl Pts',(-0.250315457859235,1.7966403758627,9.93290134276688));
#34049=CARTESIAN_POINT('Ctrl Pts',(-0.234390414876792,1.78349991777797,
9.93394311859737));
#34050=CARTESIAN_POINT('Ctrl Pts',(-0.217440399509737,1.77162709255911,
9.93498489442787));
#34051=CARTESIAN_POINT('Ctrl Pts',(-0.199696632060677,1.76116944479043,
9.93602667025836));
#34052=CARTESIAN_POINT('Ctrl Pts',(-0.181914511055617,1.7506891925788,9.93707069791095));
#34053=CARTESIAN_POINT('Ctrl Pts',(-0.163335874611733,1.74163054760894,
9.93811472556354));
#34054=CARTESIAN_POINT('Ctrl Pts',(-0.144215437897276,1.73409455118556,
9.93915875321614));
#34055=CARTESIAN_POINT('Ctrl Pts',(-0.137452790056707,1.73142916803034,
9.93952801211204));
#34056=CARTESIAN_POINT('Ctrl Pts',(-0.130622517524043,1.72895380719259,
9.93989727100793));
#34057=CARTESIAN_POINT('Ctrl Pts',(-0.123736295891238,1.72667143281137,
9.94026652990383));
#34058=CARTESIAN_POINT('Ctrl Pts',(-0.104267683903116,1.72021874168276,
9.94131049255139));
#34059=CARTESIAN_POINT('Ctrl Pts',(-0.0842349555426453,1.71527381972604,
9.94235445519894));
#34060=CARTESIAN_POINT('Ctrl Pts',(-0.063896384345083,1.71192508188801,
9.9433984178465));
#34061=CARTESIAN_POINT('Ctrl Pts',(-0.0435952281408463,1.70858250441409,
9.94444046001226));
#34062=CARTESIAN_POINT('Ctrl Pts',(-0.0229900540417418,1.70683045938156,
9.94548250217804));
#34063=CARTESIAN_POINT('Ctrl Pts',(-0.0023521030540002,1.70670703335653,
9.94652454434381));
#34064=CARTESIAN_POINT('Ctrl Pts',(0.0182636830986,1.70658373988911,9.94756546737266));
#34065=CARTESIAN_POINT('Ctrl Pts',(0.0389114443941607,1.70808562632387,
9.94860639040152));
#34066=CARTESIAN_POINT('Ctrl Pts',(0.0593171995167528,1.71119881707807,
9.94964731343037));
#34067=CARTESIAN_POINT('Ctrl Pts',(0.0797334345033376,1.71431360668591,
9.95068877105016));
#34068=CARTESIAN_POINT('Ctrl Pts',(0.0999066852239352,1.71904125878756,
9.95173022866995));
#34069=CARTESIAN_POINT('Ctrl Pts',(0.1195699231907,1.7253162353822,9.95277168628974));
#34070=CARTESIAN_POINT('Ctrl Pts',(0.139239169133913,1.73159312925575,9.95381346212024));
#34071=CARTESIAN_POINT('Ctrl Pts',(0.158397402739161,1.73941803083677,9.95485523795074));
#34072=CARTESIAN_POINT('Ctrl Pts',(0.176795402150575,1.74867639450442,9.95589701378124));
#34073=CARTESIAN_POINT('Ctrl Pts',(0.195233169255211,1.75795477033522,9.95694104143384));
#34074=CARTESIAN_POINT('Ctrl Pts',(0.21290679173709,1.76867241229492,9.95798506908643));
#34075=CARTESIAN_POINT('Ctrl Pts',(0.229593430335173,1.78066984679343,9.95902909673903));
#34076=CARTESIAN_POINT('Ctrl Pts',(0.235495275682921,1.78491318211611,9.95939835563489));
#34077=CARTESIAN_POINT('Ctrl Pts',(0.241273953331664,1.78931624000458,9.95976761453075));
#34078=CARTESIAN_POINT('Ctrl Pts',(0.246920650771322,1.79387080795411,9.96013687342662));
#34079=CARTESIAN_POINT('Ctrl Pts',(0.262884900448396,1.8067474071866,9.96118083607417));
#34080=CARTESIAN_POINT('Ctrl Pts',(0.277886757195359,1.82091450826151,9.96222479872173));
#34081=CARTESIAN_POINT('Ctrl Pts',(0.291712072010568,1.83620281077445,9.96326876136928));
#34082=CARTESIAN_POINT('Ctrl Pts',(0.305511953669411,1.8514629888075,9.96431080353505));
#34083=CARTESIAN_POINT('Ctrl Pts',(0.31813905755377,1.86783977447944,9.96535284570082));
#34084=CARTESIAN_POINT('Ctrl Pts',(0.329414532139265,1.88512572044223,9.96639488786659));
#34085=CARTESIAN_POINT('Ctrl Pts',(0.340677897042187,1.90239310157061,9.96743581089545));
#34086=CARTESIAN_POINT('Ctrl Pts',(0.350592090308146,1.92056710721788,9.9684767339243));
#34087=CARTESIAN_POINT('Ctrl Pts',(0.359020467738701,1.93940985788448,9.96951765695316));
#34088=CARTESIAN_POINT('Ctrl Pts',(0.367453173764235,1.95826228569671,9.97055911457295));
#34089=CARTESIAN_POINT('Ctrl Pts',(0.374398224354034,1.9777834795981,9.97160057219274));
#34090=CARTESIAN_POINT('Ctrl Pts',(0.379766177687244,1.99771344035104,9.97264202981254));
#34091=CARTESIAN_POINT('Ctrl Pts',(0.385135771164221,2.01764949057586,9.97368380564304));
#34092=CARTESIAN_POINT('Ctrl Pts',(0.388927151832685,2.03799383702034,9.97472558147354));
#34093=CARTESIAN_POINT('Ctrl Pts',(0.391101723407775,2.05847492387162,9.97576735730404));
#34094=CARTESIAN_POINT('Ctrl Pts',(0.393280995368673,2.07900028105691,9.97681138495664));
#34095=CARTESIAN_POINT('Ctrl Pts',(0.393836461307713,2.0996622325233,9.97785541260923));
#34096=CARTESIAN_POINT('Ctrl Pts',(0.392781582556244,2.1201870850945,9.97889944026183));
#34097=CARTESIAN_POINT('Ctrl Pts',(0.392408485768947,2.12744645641409,9.97926869915769));
#34098=CARTESIAN_POINT('Ctrl Pts',(0.391834418487633,2.13468872683798,9.97963795805355));
#34099=CARTESIAN_POINT('Ctrl Pts',(0.391061515562374,2.14190204107271,9.98000721694941));
#34100=CARTESIAN_POINT('Ctrl Pts',(0.388876377186018,2.16229540386114,9.98105117959696));
#34101=CARTESIAN_POINT('Ctrl Pts',(0.385085201072507,2.18257814140808,9.98209514224452));
#34102=CARTESIAN_POINT('Ctrl Pts',(0.379714415309066,2.20247854803077,9.98313910489207));
#34103=CARTESIAN_POINT('Ctrl Pts',(0.374353509684772,2.22234234571108,9.98418114705784));
#34104=CARTESIAN_POINT('Ctrl Pts',(0.367418894565462,2.2418244907315,9.98522318922361));
#34105=CARTESIAN_POINT('Ctrl Pts',(0.358988179833785,2.26066230653027,9.98626523138937));
#34106=CARTESIAN_POINT('Ctrl Pts',(0.350566519557285,2.27947989081081,9.98730615441823));
#34107=CARTESIAN_POINT('Ctrl Pts',(0.340652222167683,2.29765383965664,9.98834707744708));
#34108=CARTESIAN_POINT('Ctrl Pts',(0.329371333033667,2.31494049170788,9.98938800047594));
#34109=CARTESIAN_POINT('Ctrl Pts',(0.318084650329008,2.33223602173306,9.99042945809573));
#34110=CARTESIAN_POINT('Ctrl Pts',(0.305430362355158,2.34864271960023,9.99147091571552));
#34111=CARTESIAN_POINT('Ctrl Pts',(0.29157866465248,2.36394463873979,9.99251237333531));
#34112=CARTESIAN_POINT('Ctrl Pts',(0.277722734652274,2.37925123328275,9.99355414916581));
#34113=CARTESIAN_POINT('Ctrl Pts',(0.262669186770547,2.39345185636053,9.99459592499631));
#34114=CARTESIAN_POINT('Ctrl Pts',(0.246625457130397,2.40636705745759,9.9956377008268));
#34115=CARTESIAN_POINT('Ctrl Pts',(0.230547048604549,2.4193101750549,9.9966817284794));
#34116=CARTESIAN_POINT('Ctrl Pts',(0.213474793621571,2.43096190842826,9.997725756132));
#34117=CARTESIAN_POINT('Ctrl Pts',(0.195646105166284,2.44118542104443,9.9987697837846));
#34118=CARTESIAN_POINT('Ctrl Pts',(0.189340331753627,2.44480134344953,9.99913904268047));
#34119=CARTESIAN_POINT('Ctrl Pts',(0.18294014812053,2.44823902924116,9.99950830157634));
#34120=CARTESIAN_POINT('Ctrl Pts',(0.176456678042913,2.45149385595492,9.99987756047221));
#34121=CARTESIAN_POINT('Ctrl Pts',(0.15812671859372,2.46069584824659,10.0009215231198));
#34122=CARTESIAN_POINT('Ctrl Pts',(0.139020397581867,2.46848757181165,10.0019654857673));
#34123=CARTESIAN_POINT('Ctrl Pts',(0.119380476011277,2.47474416866353,10.0030094484149));
#34124=CARTESIAN_POINT('Ctrl Pts',(0.0997766841927412,2.48098925583132,
10.0040514905806));
#34125=CARTESIAN_POINT('Ctrl Pts',(0.0796419153791249,2.48570454439856,
10.0050935327464));
#34126=CARTESIAN_POINT('Ctrl Pts',(0.0592390443584112,2.48881309857501,
10.0061355749122));
#34127=CARTESIAN_POINT('Ctrl Pts',(0.0388580857006548,2.49191831421311,
10.007176497941));
#34128=CARTESIAN_POINT('Ctrl Pts',(0.0182103158007307,2.49342008235121,
10.0082174209699));
#34129=CARTESIAN_POINT('Ctrl Pts',(-0.00243115987178641,2.49329248589527,
10.0092583439988));
#34130=CARTESIAN_POINT('Ctrl Pts',(-0.023083236468227,2.49316482390911,
10.0102998016186));
#34131=CARTESIAN_POINT('Ctrl Pts',(-0.0437282765154819,2.49140611401917,
10.0113412592383));
#34132=CARTESIAN_POINT('Ctrl Pts',(-0.0640925783502209,2.48804256390301,
10.0123827168581));
#34133=CARTESIAN_POINT('Ctrl Pts',(-0.0844631023669823,2.48467798607565,
10.0134244926886));
#34134=CARTESIAN_POINT('Ctrl Pts',(-0.104551997972933,2.47970774735316,
10.0144662685191));
#34135=CARTESIAN_POINT('Ctrl Pts',(-0.124096091040081,2.47320912393532,
10.0155080443496));
#34136=CARTESIAN_POINT('Ctrl Pts',(-0.143682429107908,2.4666964535955,10.0165520720022));
#34137=CARTESIAN_POINT('Ctrl Pts',(-0.162720935243703,2.45864908974604,
10.0175960996548));
#34138=CARTESIAN_POINT('Ctrl Pts',(-0.180968038901883,2.44919258138742,
10.0186401273074));
#34139=CARTESIAN_POINT('Ctrl Pts',(-0.187421800287246,2.44584793833455,
10.0190093862033));
#34140=CARTESIAN_POINT('Ctrl Pts',(-0.193776803094997,2.44232743077858,
10.0193786450991));
#34141=CARTESIAN_POINT('Ctrl Pts',(-0.200023139173413,2.43863790956597,
10.019747903995));
#34142=CARTESIAN_POINT('Ctrl Pts',(-0.217682677299445,2.42820695617139,
10.0207918666426));
#34143=CARTESIAN_POINT('Ctrl Pts',(-0.234576694771981,2.416359820131,10.0218358292901));
#34144=CARTESIAN_POINT('Ctrl Pts',(-0.250468797842574,2.40323303135921,
10.0228797919377));
#34145=CARTESIAN_POINT('Ctrl Pts',(-0.266331665677096,2.39013039072986,
10.0239218341034));
#34146=CARTESIAN_POINT('Ctrl Pts',(-0.281195678899764,2.37575318751205,
10.0249638762692));
#34147=CARTESIAN_POINT('Ctrl Pts',(-0.294853849648067,2.36028080480073,
10.026005918435));
#34148=CARTESIAN_POINT('Ctrl Pts',(-0.308497351735555,2.34482503918537,
10.0270468414638));
#34149=CARTESIAN_POINT('Ctrl Pts',(-0.320937076202657,2.32827695879629,
10.0280877644927));
#34150=CARTESIAN_POINT('Ctrl Pts',(-0.332003394567297,2.31085216621081,
10.0291286875215));
#34151=CARTESIAN_POINT('Ctrl Pts',(-0.343075396304625,2.293418424706,10.0301701451413));
#34152=CARTESIAN_POINT('Ctrl Pts',(-0.352772174750329,2.27510768395625,
10.0312116027611));
#34153=CARTESIAN_POINT('Ctrl Pts',(-0.3609676061331,2.25616426390996,10.0322530603809));
#34154=CARTESIAN_POINT('Ctrl Pts',(-0.369165541577451,2.23721505582297,
10.0332948362114));
#34155=CARTESIAN_POINT('Ctrl Pts',(-0.375860958045332,2.21763347269119,
10.0343366120419));
#34156=CARTESIAN_POINT('Ctrl Pts',(-0.380976369838367,2.19768262703664,
10.0353783878724));
#34157=CARTESIAN_POINT('Ctrl Pts',(-0.386102838710076,2.17768865717647,
10.036422415525));
#34158=CARTESIAN_POINT('Ctrl Pts',(-0.389642358477646,2.15732455688644,
10.0374664431776));
#34159=CARTESIAN_POINT('Ctrl Pts',(-0.391568643851175,2.13686308658471,
10.0385104708302));
#34160=CARTESIAN_POINT('Ctrl Pts',(-0.39224994573852,2.12962613274288,10.0388797297261));
#34161=CARTESIAN_POINT('Ctrl Pts',(-0.392729917800397,2.12237701824811,
10.0392489886219));
#34162=CARTESIAN_POINT('Ctrl Pts',(-0.393008956889611,2.11512778253875,
10.0396182475178));
#34163=CARTESIAN_POINT('Ctrl Pts',(-0.39320175440833,2.11011904107064,10.0398733809441));
#34164=CARTESIAN_POINT('Ctrl Pts',(-0.393298804877452,2.1051065904132,10.0401285143703));
#34165=CARTESIAN_POINT('Ctrl Pts',(-0.393299989030347,2.10009289095292,
10.0403836477965));
#34166=CARTESIAN_POINT('',(-0.393202477937398,2.10031103147611,10.1653836091462));
#34167=CARTESIAN_POINT('Ctrl Pts',(-0.393923156018864,2.10009103559663,
10.040383749539));
#34168=CARTESIAN_POINT('Ctrl Pts',(-0.39352309280741,1.97474775194909,10.0467520300395));
#34169=CARTESIAN_POINT('Ctrl Pts',(-0.260911319827819,1.7183126572773,10.059743758381));
#34170=CARTESIAN_POINT('Ctrl Pts',(0.176083159449116,1.66957025957435,10.0793589345633));
#34171=CARTESIAN_POINT('Ctrl Pts',(0.457230028159891,2.01505447726103,10.0992292780861));
#34172=CARTESIAN_POINT('Ctrl Pts',(0.318930592281517,2.43846464777199,10.1190996216089));
#34173=CARTESIAN_POINT('Ctrl Pts',(-0.11194424353566,2.55137958175324,10.1389699651317));
#34174=CARTESIAN_POINT('Ctrl Pts',(-0.366754511395233,2.3175460488061,10.1543979270584));
#34175=CARTESIAN_POINT('Ctrl Pts',(-0.393263485699074,2.14351739557072,
10.1632024411441));
#34176=CARTESIAN_POINT('Ctrl Pts',(-0.392946047468718,2.10031284482443,
10.1653835073888));
#34177=CARTESIAN_POINT('',(-0.393130899880172,2.09975969803041,10.2903836983485));
#34178=CARTESIAN_POINT('Ctrl Pts',(-0.393299877558333,2.10031034271459,
10.1653836477965));
#34179=CARTESIAN_POINT('Ctrl Pts',(-0.393316137078467,2.07970451896758,
10.1664229484123));
#34180=CARTESIAN_POINT('Ctrl Pts',(-0.391708693976257,2.05907847120989,
10.1674622490281));
#34181=CARTESIAN_POINT('Ctrl Pts',(-0.388494396308227,2.03870567695858,
10.168501549644));
#34182=CARTESIAN_POINT('Ctrl Pts',(-0.385277877255557,2.0183188031736,10.1695415685151));
#34183=CARTESIAN_POINT('Ctrl Pts',(-0.380452391197413,1.99818626229835,
10.1705815873863));
#34184=CARTESIAN_POINT('Ctrl Pts',(-0.374086359525959,1.97857395000818,
10.1716216062574));
#34185=CARTESIAN_POINT('Ctrl Pts',(-0.367717552787176,1.9589530883595,10.1726620784914));
#34186=CARTESIAN_POINT('Ctrl Pts',(-0.359807131823567,1.93985359354466,
10.1737025507254));
#34187=CARTESIAN_POINT('Ctrl Pts',(-0.350472277064807,1.9215229062064,10.1747430229595));
#34188=CARTESIAN_POINT('Ctrl Pts',(-0.341116449486835,1.90315103491815,
10.1757858328449));
#34189=CARTESIAN_POINT('Ctrl Pts',(-0.330330191756566,1.88555204354073,
10.1768286427302));
#34190=CARTESIAN_POINT('Ctrl Pts',(-0.31827520167265,1.86894635687738,10.1778714526156));
#34191=CARTESIAN_POINT('Ctrl Pts',(-0.315041457108724,1.86449189041959,
10.1781511858029));
#34192=CARTESIAN_POINT('Ctrl Pts',(-0.311716639803177,1.86010871273235,
10.1784309189901));
#34193=CARTESIAN_POINT('Ctrl Pts',(-0.308304338982045,1.85580064585498,
10.1787106521773));
#34194=CARTESIAN_POINT('Ctrl Pts',(-0.295569651922344,1.83972296501987,
10.1797546148249));
#34195=CARTESIAN_POINT('Ctrl Pts',(-0.281535989030201,1.82459620844249,
10.1807985774724));
#34196=CARTESIAN_POINT('Ctrl Pts',(-0.266370747194188,1.81063601634065,
10.18184254012));
#34197=CARTESIAN_POINT('Ctrl Pts',(-0.251233403454677,1.79670150551647,
10.1828845822857));
#34198=CARTESIAN_POINT('Ctrl Pts',(-0.234969107732109,1.78392983584885,
10.1839266244515));
#34199=CARTESIAN_POINT('Ctrl Pts',(-0.217783715017697,1.77250168935842,
10.1849686666173));
#34200=CARTESIAN_POINT('Ctrl Pts',(-0.200616779145092,1.76108581651778,
10.1860095896461));
#34201=CARTESIAN_POINT('Ctrl Pts',(-0.182531303722437,1.75101103175003,
10.187050512675));
#34202=CARTESIAN_POINT('Ctrl Pts',(-0.163763948559705,1.74241608096541,
10.1880914357038));
#34203=CARTESIAN_POINT('Ctrl Pts',(-0.144986954972491,1.73381671603809,
10.1891328933236));
#34204=CARTESIAN_POINT('Ctrl Pts',(-0.125528044281525,1.72669902443544,
10.1901743509434));
#34205=CARTESIAN_POINT('Ctrl Pts',(-0.105646413272996,1.7211547474726,10.1912158085632));
#34206=CARTESIAN_POINT('Ctrl Pts',(-0.0857587075594246,1.71560877649144,
10.1922575843937));
#34207=CARTESIAN_POINT('Ctrl Pts',(-0.0654487422604584,1.71163733982698,
10.1932993602242));
#34208=CARTESIAN_POINT('Ctrl Pts',(-0.0449877206602062,1.70928143761807,
10.1943411360547));
#34209=CARTESIAN_POINT('Ctrl Pts',(-0.0244824720974497,1.70692044307309,
10.1953851637073));
#34210=CARTESIAN_POINT('Ctrl Pts',(-0.00382625137647264,1.70618198093199,
10.1964291913599));
#34211=CARTESIAN_POINT('Ctrl Pts',(0.0167071398267035,1.70705501469186,
10.1974732190125));
#34212=CARTESIAN_POINT('Ctrl Pts',(0.023969531148709,1.70736379528922,10.1978424779084));
#34213=CARTESIAN_POINT('Ctrl Pts',(0.031216602388322,1.70787368997157,10.1982117368043));
#34214=CARTESIAN_POINT('Ctrl Pts',(0.0384364798072488,1.70858266898357,
10.1985809957001));
#34215=CARTESIAN_POINT('Ctrl Pts',(0.0588483979210042,1.71058708272879,
10.1996249583477));
#34216=CARTESIAN_POINT('Ctrl Pts',(0.0791639209822469,1.71419845109411,
10.2006689209952));
#34217=CARTESIAN_POINT('Ctrl Pts',(0.0991111198744934,1.71939275372476,
10.2017128836428));
#34218=CARTESIAN_POINT('Ctrl Pts',(0.119021623744943,1.72457750087599,10.2027549258086));
#34219=CARTESIAN_POINT('Ctrl Pts',(0.138564429422154,1.73133927636122,10.2037969679743));
#34220=CARTESIAN_POINT('Ctrl Pts',(0.157476183201892,1.73960280006059,10.2048390101401));
#34221=CARTESIAN_POINT('Ctrl Pts',(0.176367626055164,1.74785744886533,10.205879933169));
#34222=CARTESIAN_POINT('Ctrl Pts',(0.194628680100807,1.75761037737541,10.2069208561978));
#34223=CARTESIAN_POINT('Ctrl Pts',(0.212014577061992,1.76873770345356,10.2079617792267));
#34224=CARTESIAN_POINT('Ctrl Pts',(0.229409402966725,1.77987074423637,10.2090032368465));
#34225=CARTESIAN_POINT('Ctrl Pts',(0.24592754546134,1.7923792096721,10.2100446944662));
#34226=CARTESIAN_POINT('Ctrl Pts',(0.261351558901751,1.80609482369372,10.211086152086));
#34227=CARTESIAN_POINT('Ctrl Pts',(0.276780285050694,1.81981462843337,10.2121279279165));
#34228=CARTESIAN_POINT('Ctrl Pts',(0.29111369129841,1.83474180046838,10.213169703747));
#34229=CARTESIAN_POINT('Ctrl Pts',(0.304170496756044,1.85067050133773,10.2142114795775));
#34230=CARTESIAN_POINT('Ctrl Pts',(0.317255524794978,1.86663363245548,10.2152555072301));
#34231=CARTESIAN_POINT('Ctrl Pts',(0.329058022495414,1.88360200977445,10.2162995348827));
#34232=CARTESIAN_POINT('Ctrl Pts',(0.339439055752096,1.90133944168475,10.2173435625353));
#34233=CARTESIAN_POINT('Ctrl Pts',(0.343110691142987,1.90761293885359,10.2177128214312));
#34234=CARTESIAN_POINT('Ctrl Pts',(0.346604933172984,1.91398242131096,10.218082080327));
#34235=CARTESIAN_POINT('Ctrl Pts',(0.349917061027627,1.92043680666187,10.2184513392229));
#34236=CARTESIAN_POINT('Ctrl Pts',(0.359281054157792,1.93868453825249,10.2194953018705));
#34237=CARTESIAN_POINT('Ctrl Pts',(0.367241710688164,1.95772109272876,10.220539264518));
#34238=CARTESIAN_POINT('Ctrl Pts',(0.373672027218917,1.97730482456875,10.2215832271656));
#34239=CARTESIAN_POINT('Ctrl Pts',(0.380090514489504,1.99685253002375,10.2226252693313));
#34240=CARTESIAN_POINT('Ctrl Pts',(0.384983966425265,2.01694474218674,10.2236673114971));
#34241=CARTESIAN_POINT('Ctrl Pts',(0.388273121780206,2.03731927805893,10.2247093536629));
#34242=CARTESIAN_POINT('Ctrl Pts',(0.391558744633968,2.05767193199968,10.2257502766917));
#34243=CARTESIAN_POINT('Ctrl Pts',(0.393243346233729,2.07830558962094,10.2267911997206));
#34244=CARTESIAN_POINT('Ctrl Pts',(0.393298591407606,2.09894738573383,10.2278321227494));
#34245=CARTESIAN_POINT('Ctrl Pts',(0.393353864953964,2.1195997829352,10.2288735803692));
#34246=CARTESIAN_POINT('Ctrl Pts',(0.391778092255447,2.14025959124585,10.229915037989));
#34247=CARTESIAN_POINT('Ctrl Pts',(0.388595055585969,2.16065288759934,10.2309564956088));
#34248=CARTESIAN_POINT('Ctrl Pts',(0.385411046360019,2.18105241499393,10.2319982714393));
#34249=CARTESIAN_POINT('Ctrl Pts',(0.380618944641255,2.20118454753727,10.2330400472698));
#34250=CARTESIAN_POINT('Ctrl Pts',(0.374293692472436,2.22078543693405,10.2340818231002));
#34251=CARTESIAN_POINT('Ctrl Pts',(0.367954768127517,2.24042869409806,10.2351258507528));
#34252=CARTESIAN_POINT('Ctrl Pts',(0.360076357932214,2.25953773472292,10.2361698784054));
#34253=CARTESIAN_POINT('Ctrl Pts',(0.35078184847944,2.27786788573924,10.237213906058));
#34254=CARTESIAN_POINT('Ctrl Pts',(0.347494502316144,2.28435101988659,10.2375831649539));
#34255=CARTESIAN_POINT('Ctrl Pts',(0.344030423772152,2.29073695709101,10.2379524238498));
#34256=CARTESIAN_POINT('Ctrl Pts',(0.340396375661423,2.29701572890652,10.2383216827456));
#34257=CARTESIAN_POINT('Ctrl Pts',(0.330122254903612,2.31476696881248,10.2393656453932));
#34258=CARTESIAN_POINT('Ctrl Pts',(0.318425226282013,2.33176526226058,10.2404096080407));
#34259=CARTESIAN_POINT('Ctrl Pts',(0.305439720442846,2.34777301543105,10.2414535706883));
#34260=CARTESIAN_POINT('Ctrl Pts',(0.292478102840944,2.36375132061463,10.2424956128541));
#34261=CARTESIAN_POINT('Ctrl Pts',(0.27823312506752,2.37874210010351,10.2435376550198));
#34262=CARTESIAN_POINT('Ctrl Pts',(0.262882329737576,2.39253678522836,10.2445796971856));
#34263=CARTESIAN_POINT('Ctrl Pts',(0.247548020920653,2.4063166550781,10.2456206202144));
#34264=CARTESIAN_POINT('Ctrl Pts',(0.231110777444544,2.41890246996186,10.2466615432433));
#34265=CARTESIAN_POINT('Ctrl Pts',(0.213784690905028,2.43012269830268,10.2477024662722));
#34266=CARTESIAN_POINT('Ctrl Pts',(0.196449706139038,2.44134868906034,10.248743923892));
#34267=CARTESIAN_POINT('Ctrl Pts',(0.178225575176194,2.4512072786998,10.2497853815117));
#34268=CARTESIAN_POINT('Ctrl Pts',(0.159355491209759,2.45957018427742,10.2508268391315));
#34269=CARTESIAN_POINT('Ctrl Pts',(0.140479641609996,2.46793564508729,10.251868614962));
#34270=CARTESIAN_POINT('Ctrl Pts',(0.120958132865967,2.47480424727279,10.2529103907925));
#34271=CARTESIAN_POINT('Ctrl Pts',(0.101053380830248,2.48009617759559,10.253952166623));
#34272=CARTESIAN_POINT('Ctrl Pts',(0.08110560422132,2.48539954654586,10.2549961942756));
#34273=CARTESIAN_POINT('Ctrl Pts',(0.0607736549357756,2.48911930716426,
10.2560402219282));
#34274=CARTESIAN_POINT('Ctrl Pts',(0.0403300498632668,2.49122675915385,
10.2570842495808));
#34275=CARTESIAN_POINT('Ctrl Pts',(0.0330994147188781,2.49197213729861,
10.2574535084767));
#34276=CARTESIAN_POINT('Ctrl Pts',(0.0258548360733349,2.49251630123194,
10.2578227673726));
#34277=CARTESIAN_POINT('Ctrl Pts',(0.0186083564078811,2.49285954114899,
10.2581920262684));
#34278=CARTESIAN_POINT('Ctrl Pts',(-0.00187877113783579,2.49382994336967,
10.259235988916));
#34279=CARTESIAN_POINT('Ctrl Pts',(-0.0225030535577246,2.49319635565967,
10.2602799515635));
#34280=CARTESIAN_POINT('Ctrl Pts',(-0.0429919479763473,2.49094319588554,
10.2613239142111));
#34281=CARTESIAN_POINT('Ctrl Pts',(-0.0634431508658882,2.48869418104161,
10.2623659563769));
#34282=CARTESIAN_POINT('Ctrl Pts',(-0.0837587305199895,2.48483152848569,
10.2634079985426));
#34283=CARTESIAN_POINT('Ctrl Pts',(-0.103667211641671,2.47939161723797,
10.2644500407084));
#34284=CARTESIAN_POINT('Ctrl Pts',(-0.123554311367365,2.47395754836947,
10.2654909637373));
#34285=CARTESIAN_POINT('Ctrl Pts',(-0.143034466758624,2.46694974876387,
10.2665318867661));
#34286=CARTESIAN_POINT('Ctrl Pts',(-0.161847559345197,2.45845537732611,
10.267572809795));
#34287=CARTESIAN_POINT('Ctrl Pts',(-0.180670313845794,2.44995664340056,
10.2686142674148));
#34288=CARTESIAN_POINT('Ctrl Pts',(-0.198824643905938,2.43997010050044,
10.2696557250345));
#34289=CARTESIAN_POINT('Ctrl Pts',(-0.21607104206007,2.42863078794154,10.2706971826543));
#34290=CARTESIAN_POINT('Ctrl Pts',(-0.233322709740733,2.41728801072829,
10.2717389584848));
#34291=CARTESIAN_POINT('Ctrl Pts',(-0.249665298850806,2.40459207512652,
10.2727807343153));
#34292=CARTESIAN_POINT('Ctrl Pts',(-0.26488965054794,2.39072042073544,10.2738225101458));
#34293=CARTESIAN_POINT('Ctrl Pts',(-0.280146910026749,2.3768187824486,10.2748665377984));
#34294=CARTESIAN_POINT('Ctrl Pts',(-0.294280602877999,2.36173688909286,
10.275910565451));
#34295=CARTESIAN_POINT('Ctrl Pts',(-0.307119079061731,2.34568834175897,
10.2769545931036));
#34296=CARTESIAN_POINT('Ctrl Pts',(-0.311659879804395,2.34001218092731,
10.2773238519995));
#34297=CARTESIAN_POINT('Ctrl Pts',(-0.316039043904594,2.33421537526186,
10.2776931108954));
#34298=CARTESIAN_POINT('Ctrl Pts',(-0.320250296550904,2.32830820738436,
10.2780623697912));
#34299=CARTESIAN_POINT('Ctrl Pts',(-0.332267798420901,2.31145113254785,
10.2791161107668));
#34300=CARTESIAN_POINT('Ctrl Pts',(-0.34298584099648,2.29359358210619,10.2801698517423));
#34301=CARTESIAN_POINT('Ctrl Pts',(-0.352241230061416,2.27496001213083,
10.2812235927178));
#34302=CARTESIAN_POINT('Ctrl Pts',(-0.361477954782044,2.25636401846515,
10.2822752087276));
#34303=CARTESIAN_POINT('Ctrl Pts',(-0.369257510879528,2.2369957190811,10.2833268247374));
#34304=CARTESIAN_POINT('Ctrl Pts',(-0.37546086600497,2.21710690884315,10.2843784407472));
#34305=CARTESIAN_POINT('Ctrl Pts',(-0.381658138137299,2.19723760151826,
10.2854290255452));
#34306=CARTESIAN_POINT('Ctrl Pts',(-0.386282022236364,2.17684946460557,
10.2864796103432));
#34307=CARTESIAN_POINT('Ctrl Pts',(-0.389262129579668,2.15621284973297,
10.2875301951412));
#34308=CARTESIAN_POINT('Ctrl Pts',(-0.391960180934149,2.13752941309972,
10.2884813460263));
#34309=CARTESIAN_POINT('Ctrl Pts',(-0.393311420851984,2.11864292265643,
10.2894324969114));
#34310=CARTESIAN_POINT('Ctrl Pts',(-0.393299927137564,2.09976059743748,
10.2903836477965));
#34311=CARTESIAN_POINT('',(-0.393480327863744,2.09979784797213,10.4153835873822));
#34312=CARTESIAN_POINT('Ctrl Pts',(-0.392802840044818,2.09975795239874,
10.2903837964633));
#34313=CARTESIAN_POINT('Ctrl Pts',(-0.393078666905956,2.04986700265937,
10.2929001020802));
#34314=CARTESIAN_POINT('Ctrl Pts',(-0.36107951247964,1.86899388280721,10.302039855538));
#34315=CARTESIAN_POINT('Ctrl Pts',(-0.0889922105537249,1.64354033371482,
10.3178030568369));
#34316=CARTESIAN_POINT('Ctrl Pts',(0.335626368481811,1.77808389095263,10.3376734003596));
#34317=CARTESIAN_POINT('Ctrl Pts',(0.452353445839552,2.20794165332066,10.3575437438824));
#34318=CARTESIAN_POINT('Ctrl Pts',(0.154107819000222,2.53877764369605,10.3774140874052));
#34319=CARTESIAN_POINT('Ctrl Pts',(-0.272447788613133,2.46922488414649,
10.3966939973457));
#34320=CARTESIAN_POINT('Ctrl Pts',(-0.393070870679608,2.21862714459167,
10.4093504594452));
#34321=CARTESIAN_POINT('Ctrl Pts',(-0.393819740132955,2.09979991159289,
10.4153834737038));
#34322=CARTESIAN_POINT('',(-0.393299843557239,2.10035079602495,10.5403836477997));
#34323=CARTESIAN_POINT('Ctrl Pts',(-0.393299947482771,2.09979675126253,
10.4153836477965));
#34324=CARTESIAN_POINT('Ctrl Pts',(-0.39329394627344,2.08818400845285,10.4159740233479));
#34325=CARTESIAN_POINT('Ctrl Pts',(-0.392773668395661,2.07658491143399,
10.4165643988994));
#34326=CARTESIAN_POINT('Ctrl Pts',(-0.391742435504716,2.06503209721997,
10.4171547744508));
#34327=CARTESIAN_POINT('Ctrl Pts',(-0.389918903658791,2.04460322531887,
10.4181987370984));
#34328=CARTESIAN_POINT('Ctrl Pts',(-0.386487626392958,2.02425651071807,
10.4192426997459));
#34329=CARTESIAN_POINT('Ctrl Pts',(-0.381470214444904,2.00426408463195,
10.4202866623935));
#34330=CARTESIAN_POINT('Ctrl Pts',(-0.376462032566783,1.98430843676791,
10.4213287045592));
#34331=CARTESIAN_POINT('Ctrl Pts',(-0.369873627250801,1.96470650378052,
10.422370746725));
#34332=CARTESIAN_POINT('Ctrl Pts',(-0.361777942947447,1.9457222958535,10.4234127888907));
#34333=CARTESIAN_POINT('Ctrl Pts',(-0.353690953281854,1.92675847666757,
10.4244537119196));
#34334=CARTESIAN_POINT('Ctrl Pts',(-0.344100158875096,1.9084117502013,10.4254946349484));
#34335=CARTESIAN_POINT('Ctrl Pts',(-0.333127268913106,1.89092797244372,
10.4265355579773));
#34336=CARTESIAN_POINT('Ctrl Pts',(-0.322148743560819,1.87343521547356,
10.4275770155971));
#34337=CARTESIAN_POINT('Ctrl Pts',(-0.309787082088958,1.85680692438022,
10.4286184732169));
#34338=CARTESIAN_POINT('Ctrl Pts',(-0.296208627888156,1.84126202682131,
10.4296599308367));
#34339=CARTESIAN_POINT('Ctrl Pts',(-0.282626024877622,1.8257123796185,10.4307017066671));
#34340=CARTESIAN_POINT('Ctrl Pts',(-0.267826399889048,1.81124731481315,
10.4317434824976));
#34341=CARTESIAN_POINT('Ctrl Pts',(-0.252013977571094,1.79804992944396,
10.4327852583281));
#34342=CARTESIAN_POINT('Ctrl Pts',(-0.236167376343474,1.78482401762682,
10.4338292859807));
#34343=CARTESIAN_POINT('Ctrl Pts',(-0.219304208043086,1.77287168163419,
10.4348733136333));
#34344=CARTESIAN_POINT('Ctrl Pts',(-0.201659424373089,1.76233394224247,
10.4359173412859));
#34345=CARTESIAN_POINT('Ctrl Pts',(-0.195418695672471,1.7586068819457,10.4362866001818));
#34346=CARTESIAN_POINT('Ctrl Pts',(-0.189080414146325,1.7550563578388,10.4366558590777));
#34347=CARTESIAN_POINT('Ctrl Pts',(-0.182655619939169,1.75168718871589,
10.4370251179735));
#34348=CARTESIAN_POINT('Ctrl Pts',(-0.164491547941026,1.7421619294548,10.4380690806211));
#34349=CARTESIAN_POINT('Ctrl Pts',(-0.14552625362603,1.7340329645596,10.4391130432686));
#34350=CARTESIAN_POINT('Ctrl Pts',(-0.12600024807438,1.72742943287856,10.4401570059162));
#34351=CARTESIAN_POINT('Ctrl Pts',(-0.106510162713992,1.72083804910561,
10.441199048082));
#34352=CARTESIAN_POINT('Ctrl Pts',(-0.0864620836551864,1.7157668177461,
10.4422410902477));
#34353=CARTESIAN_POINT('Ctrl Pts',(-0.0661174815364688,1.71229731928284,
10.4432831324135));
#34354=CARTESIAN_POINT('Ctrl Pts',(-0.0457947292008156,1.70883154700642,
10.4443240554423));
#34355=CARTESIAN_POINT('Ctrl Pts',(-0.0251768027941027,1.70696424412038,
10.4453649784712));
#34356=CARTESIAN_POINT('Ctrl Pts',(-0.00453630581528488,1.70672616165126,
10.4464059015001));
#34357=CARTESIAN_POINT('Ctrl Pts',(0.0161147915848249,1.70648795690919,
10.4474473591199));
#34358=CARTESIAN_POINT('Ctrl Pts',(0.0367877471711825,1.70788066877968,
10.4484888167396));
#34359=CARTESIAN_POINT('Ctrl Pts',(0.0572084379665225,1.71088294225846,
10.4495302743594));
#34360=CARTESIAN_POINT('Ctrl Pts',(0.0776353681731634,1.71388613306268,
10.4505720501899));
#34361=CARTESIAN_POINT('Ctrl Pts',(0.097809158068138,1.71849972178497,10.4516138260204));
#34362=CARTESIAN_POINT('Ctrl Pts',(0.117465305890651,1.72465110641962,10.4526556018509));
#34363=CARTESIAN_POINT('Ctrl Pts',(0.13716394092274,1.73081578741175,10.4536996295035));
#34364=CARTESIAN_POINT('Ctrl Pts',(0.156342016723673,1.73852462580554,10.4547436571561));
#34365=CARTESIAN_POINT('Ctrl Pts',(0.174753776897547,1.74765640709665,10.4557876848087));
#34366=CARTESIAN_POINT('Ctrl Pts',(0.181265775134261,1.75088619844219,10.4561569437046));
#34367=CARTESIAN_POINT('Ctrl Pts',(0.187682145688885,1.75429357617944,10.4565262026005));
#34368=CARTESIAN_POINT('Ctrl Pts',(0.193992860603331,1.75787186605756,10.4568954614963));
#34369=CARTESIAN_POINT('Ctrl Pts',(0.211834409510512,1.76798834806158,10.4579394241439));
#34370=CARTESIAN_POINT('Ctrl Pts',(0.228935645232347,1.7795343515047,10.4589833867914));
#34371=CARTESIAN_POINT('Ctrl Pts',(0.245057792519578,1.79237755555644,10.460027349439));
#34372=CARTESIAN_POINT('Ctrl Pts',(0.261150281379612,1.80519713315039,10.4610693916048));
#34373=CARTESIAN_POINT('Ctrl Pts',(0.276266650944304,1.81930876780531,10.4621114337705));
#34374=CARTESIAN_POINT('Ctrl Pts',(0.290196768101947,1.83453677131628,10.4631534759363));
#34375=CARTESIAN_POINT('Ctrl Pts',(0.304111924532597,1.8497484201907,10.4641943989652));
#34376=CARTESIAN_POINT('Ctrl Pts',(0.316842842338324,1.86607353707251,10.465235321994));
#34377=CARTESIAN_POINT('Ctrl Pts',(0.328216100305829,1.88329955814527,10.4662762450229));
#34378=CARTESIAN_POINT('Ctrl Pts',(0.339595199282202,1.90053442605349,10.4673177026427));
#34379=CARTESIAN_POINT('Ctrl Pts',(0.34961482660134,1.91867051734725,10.4683591602625));
#34380=CARTESIAN_POINT('Ctrl Pts',(0.358144550212507,1.93746578466956,10.4694006178822));
#34381=CARTESIAN_POINT('Ctrl Pts',(0.366676880026103,1.95626679476545,10.4704423937127));
#34382=CARTESIAN_POINT('Ctrl Pts',(0.37371812901234,1.97572669744607,10.4714841695432));
#34383=CARTESIAN_POINT('Ctrl Pts',(0.379186162655151,1.99558379411767,10.4725259453737));
#34384=CARTESIAN_POINT('Ctrl Pts',(0.384666015576766,2.01548381235434,10.4735699730263));
#34385=CARTESIAN_POINT('Ctrl Pts',(0.388565725190146,2.03578201537182,10.4746140006789));
#34386=CARTESIAN_POINT('Ctrl Pts',(0.390854178443174,2.05620615119093,10.4756580283315));
#34387=CARTESIAN_POINT('Ctrl Pts',(0.39166357436229,2.06342990031563,10.4760272872274));
#34388=CARTESIAN_POINT('Ctrl Pts',(0.392271887471484,2.07066937469568,10.4763965461233));
#34389=CARTESIAN_POINT('Ctrl Pts',(0.392679301285457,2.07791252975181,10.4767658050191));
#34390=CARTESIAN_POINT('Ctrl Pts',(0.393831134886887,2.09839025801692,10.4778097676667));
#34391=CARTESIAN_POINT('Ctrl Pts',(0.393380256363785,2.11901934348574,10.4788537303142));
#34392=CARTESIAN_POINT('Ctrl Pts',(0.391308670082716,2.13952739199715,10.4798976929618));
#34393=CARTESIAN_POINT('Ctrl Pts',(0.389240894707837,2.15999771374345,10.4809397351276));
#34394=CARTESIAN_POINT('Ctrl Pts',(0.385558343610689,2.18034671074249,10.4819817772933));
#34395=CARTESIAN_POINT('Ctrl Pts',(0.380294989729315,2.20030259611187,10.4830238194591));
#34396=CARTESIAN_POINT('Ctrl Pts',(0.375037288607326,2.22023704917385,10.484064742488));
#34397=CARTESIAN_POINT('Ctrl Pts',(0.368202313883265,2.23977851354841,10.4851056655168));
#34398=CARTESIAN_POINT('Ctrl Pts',(0.359874916983526,2.25866610893981,10.4861465885457));
#34399=CARTESIAN_POINT('Ctrl Pts',(0.351543243349778,2.27756340450793,10.4871880461655));
#34400=CARTESIAN_POINT('Ctrl Pts',(0.341717898385468,2.2958054804688,10.4882295037853));
#34401=CARTESIAN_POINT('Ctrl Pts',(0.330531794616224,2.31315164261103,10.489270961405));
#34402=CARTESIAN_POINT('Ctrl Pts',(0.319342273004604,2.33050310476201,10.4903127372355));
#34403=CARTESIAN_POINT('Ctrl Pts',(0.306791593716707,2.34695750991802,10.491354513066));
#34404=CARTESIAN_POINT('Ctrl Pts',(0.293055336718086,2.36230413572998,10.4923962888965));
#34405=CARTESIAN_POINT('Ctrl Pts',(0.27928938848825,2.37768393362188,10.4934403165491));
#34406=CARTESIAN_POINT('Ctrl Pts',(0.264333279241318,2.39195066334533,10.4944843442017));
#34407=CARTESIAN_POINT('Ctrl Pts',(0.248399081258619,2.40493078957343,10.4955283718543));
#34408=CARTESIAN_POINT('Ctrl Pts',(0.2427633642937,2.40952169007999,10.4958976307502));
#34409=CARTESIAN_POINT('Ctrl Pts',(0.237005575494178,2.41395202892457,10.4962668896461));
#34410=CARTESIAN_POINT('Ctrl Pts',(0.231135941497791,2.41821544046122,10.4966361485419));
#34411=CARTESIAN_POINT('Ctrl Pts',(0.214541409272148,2.43026888709514,10.4976801111895));
#34412=CARTESIAN_POINT('Ctrl Pts',(0.196952036167494,2.44105667706841,10.498724073837));
#34413=CARTESIAN_POINT('Ctrl Pts',(0.178587114710008,2.45041622744895,10.4997680364846));
#34414=CARTESIAN_POINT('Ctrl Pts',(0.160255977504472,2.45975855992802,10.5008100786504));
#34415=CARTESIAN_POINT('Ctrl Pts',(0.141152745043059,2.46767748479036,10.5018521208161));
#34416=CARTESIAN_POINT('Ctrl Pts',(0.121524330767905,2.4740544439402,10.5028941629819));
#34417=CARTESIAN_POINT('Ctrl Pts',(0.101916997101322,2.4804245543361,10.5039350860108));
#34418=CARTESIAN_POINT('Ctrl Pts',(0.0817862886590113,2.48525573296991,
10.5049760090396));
#34419=CARTESIAN_POINT('Ctrl Pts',(0.0613974898748184,2.48847810522225,
10.5060169320685));
#34420=CARTESIAN_POINT('Ctrl Pts',(0.0409982199349738,2.491702132401,10.5070583896883));
#34421=CARTESIAN_POINT('Ctrl Pts',(0.0203413190920445,2.49331557176928,
10.5080998473081));
#34422=CARTESIAN_POINT('Ctrl Pts',(-0.000298884699839051,2.49329988643265,
10.5091413049278));
#34423=CARTESIAN_POINT('Ctrl Pts',(-0.0209453949738137,2.49328419630347,
10.5101830807583));
#34424=CARTESIAN_POINT('Ctrl Pts',(-0.0415744629098813,2.49163842726921,
10.5112248565888));
#34425=CARTESIAN_POINT('Ctrl Pts',(-0.0619138647762143,2.4883961422935,
10.5122666324193));
#34426=CARTESIAN_POINT('Ctrl Pts',(-0.0822972307212442,2.48514684904524,
10.5133106600719));
#34427=CARTESIAN_POINT('Ctrl Pts',(-0.102388964684835,2.48029432319326,
10.5143546877245));
#34428=CARTESIAN_POINT('Ctrl Pts',(-0.121928356499301,2.47392294110068,
10.5153987153771));
#34429=CARTESIAN_POINT('Ctrl Pts',(-0.128839183266563,2.47166946676903,
10.515767974273));
#34430=CARTESIAN_POINT('Ctrl Pts',(-0.13568108660344,2.46922643732443,10.5161372331689));
#34431=CARTESIAN_POINT('Ctrl Pts',(-0.142443178297055,2.46659900566782,
10.5165064920647));
#34432=CARTESIAN_POINT('Ctrl Pts',(-0.161560852174292,2.45917077431253,
10.5175504547123));
#34433=CARTESIAN_POINT('Ctrl Pts',(-0.180152864613886,2.45022094011477,
10.5185944173598));
#34434=CARTESIAN_POINT('Ctrl Pts',(-0.197963805968831,2.43984587907805,
10.5196383800074));
#34435=CARTESIAN_POINT('Ctrl Pts',(-0.21574198217792,2.42948990408409,10.5206804221732));
#34436=CARTESIAN_POINT('Ctrl Pts',(-0.232741280890506,2.41771422131281,
10.5217224643389));
#34437=CARTESIAN_POINT('Ctrl Pts',(-0.24872835762929,2.40466226236775,10.5227645065047));
#34438=CARTESIAN_POINT('Ctrl Pts',(-0.264698264498812,2.39162432102156,
10.5238054295336));
#34439=CARTESIAN_POINT('Ctrl Pts',(-0.279657522212033,2.37731326522368,
10.5248463525624));
#34440=CARTESIAN_POINT('Ctrl Pts',(-0.293403775680491,2.36191432648183,
10.5258872755913));
#34441=CARTESIAN_POINT('Ctrl Pts',(-0.307157088866454,2.3465074792464,10.5269287332111));
#34442=CARTESIAN_POINT('Ctrl Pts',(-0.319695651247729,2.33001217105164,
10.5279701908308));
#34443=CARTESIAN_POINT('Ctrl Pts',(-0.330855377993217,2.31264902739718,
10.5290116484506));
#34444=CARTESIAN_POINT('Ctrl Pts',(-0.342018514521751,2.29528057854535,
10.5300534242811));
#34445=CARTESIAN_POINT('Ctrl Pts',(-0.351801609668667,2.27704440435856,
10.5310952001116));
#34446=CARTESIAN_POINT('Ctrl Pts',(-0.360085524149898,2.25818756366318,
10.5321369759421));
#34447=CARTESIAN_POINT('Ctrl Pts',(-0.368387344500269,2.23928996347872,
10.5331810035947));
#34448=CARTESIAN_POINT('Ctrl Pts',(-0.375183272511529,2.21976971390877,
10.5342250312473));
#34449=CARTESIAN_POINT('Ctrl Pts',(-0.380403126216002,2.19989169918012,
10.5352690588999));
#34450=CARTESIAN_POINT('Ctrl Pts',(-0.382249320050743,2.19286110592663,
10.5356383177958));
#34451=CARTESIAN_POINT('Ctrl Pts',(-0.383898823054406,2.18578585511974,
10.5360075766917));
#34452=CARTESIAN_POINT('Ctrl Pts',(-0.385350073891993,2.17867789112219,
10.5363768355876));
#34453=CARTESIAN_POINT('Ctrl Pts',(-0.390599227118804,2.15296848845556,
10.5377124396572));
#34454=CARTESIAN_POINT('Ctrl Pts',(-0.393276326782456,2.1267169504976,10.5390480437269));
#34455=CARTESIAN_POINT('Ctrl Pts',(-0.393299843557183,2.10035079608795,
10.5403836477965));
#34456=CARTESIAN_POINT('',(-0.393299999656376,2.1000164406377,10.6653836477933));
#34457=CARTESIAN_POINT('Ctrl Pts',(-0.393299843557239,2.10035079602495,
10.5403836477997));
#34458=CARTESIAN_POINT('Ctrl Pts',(-0.393317932042654,2.08007063895956,
10.5414109595528));
#34459=CARTESIAN_POINT('Ctrl Pts',(-0.391763135488696,2.05973973232589,
10.542438271306));
#34460=CARTESIAN_POINT('Ctrl Pts',(-0.388638377742624,2.03962532529627,
10.5434655830591));
#34461=CARTESIAN_POINT('Ctrl Pts',(-0.38539857970124,2.01877039131615,10.5445307160634));
#34462=CARTESIAN_POINT('Ctrl Pts',(-0.38047079879135,1.99814908177945,10.5455958490676));
#34463=CARTESIAN_POINT('Ctrl Pts',(-0.373917289109901,1.97805431166006,
10.5466609820719));
#34464=CARTESIAN_POINT('Ctrl Pts',(-0.36760091349782,1.95868665645206,10.5476875739988));
#34465=CARTESIAN_POINT('Ctrl Pts',(-0.359774888340862,1.93980879168581,
10.5487141659257));
#34466=CARTESIAN_POINT('Ctrl Pts',(-0.35054562487635,1.92166701124007,10.5497407578526));
#34467=CARTESIAN_POINT('Ctrl Pts',(-0.341313014370206,1.90351865158086,
10.5507677220785));
#34468=CARTESIAN_POINT('Ctrl Pts',(-0.330676536465045,1.8861075620019,10.5517946863044));
#34469=CARTESIAN_POINT('Ctrl Pts',(-0.318787818793444,1.86965413702669,
10.5528216505303));
#34470=CARTESIAN_POINT('Ctrl Pts',(-0.306874829414054,1.85316712115176,
10.5538507113807));
#34471=CARTESIAN_POINT('Ctrl Pts',(-0.293705002890454,1.83764223713916,
10.554879772231));
#34472=CARTESIAN_POINT('Ctrl Pts',(-0.27946933195069,1.82326586314834,10.5559088330813));
#34473=CARTESIAN_POINT('Ctrl Pts',(-0.277909144740444,1.82169025530203,
10.556021615091));
#34474=CARTESIAN_POINT('Ctrl Pts',(-0.276336188231771,1.82012840325817,
10.5561343971006));
#34475=CARTESIAN_POINT('Ctrl Pts',(-0.274750737366453,1.81858052249961,
10.5562471791103));
#34476=CARTESIAN_POINT('Ctrl Pts',(-0.260075068010066,1.80425261949579,
10.5572911417578));
#34477=CARTESIAN_POINT('Ctrl Pts',(-0.244231881104207,1.79103309274978,
10.5583351044054));
#34478=CARTESIAN_POINT('Ctrl Pts',(-0.227414634405084,1.77911454682644,
10.5593790670529));
#34479=CARTESIAN_POINT('Ctrl Pts',(-0.210628324843434,1.76721792635263,
10.5604211092187));
#34480=CARTESIAN_POINT('Ctrl Pts',(-0.1928720714548,1.75661800526572,10.5614631513845));
#34481=CARTESIAN_POINT('Ctrl Pts',(-0.17437303283508,1.74746782356798,10.5625051935502));
#34482=CARTESIAN_POINT('Ctrl Pts',(-0.155893861892215,1.73832746902163,
10.5635461165791));
#34483=CARTESIAN_POINT('Ctrl Pts',(-0.136674132766392,1.73063411333564,
10.564587039608));
#34484=CARTESIAN_POINT('Ctrl Pts',(-0.116966226458038,1.724495283827,10.5656279626368));
#34485=CARTESIAN_POINT('Ctrl Pts',(-0.0972481986826536,1.71835330157552,
10.5666694202566));
#34486=CARTESIAN_POINT('Ctrl Pts',(-0.0770421905450604,1.71376767466379,
10.5677108778764));
#34487=CARTESIAN_POINT('Ctrl Pts',(-0.0566169602373726,1.71079644167418,
10.5687523354962));
#34488=CARTESIAN_POINT('Ctrl Pts',(-0.0361854891313576,1.70782430084336,
10.5697941113267));
#34489=CARTESIAN_POINT('Ctrl Pts',(-0.015535395219666,1.70646760593883,
10.5708358871572));
#34490=CARTESIAN_POINT('Ctrl Pts',(0.00505910623880618,1.70673253955601,
10.5718776629877));
#34491=CARTESIAN_POINT('Ctrl Pts',(0.0256981231795252,1.70699804583321,
10.5729216906403));
#34492=CARTESIAN_POINT('Ctrl Pts',(0.0462805743857226,1.70889211107832,
10.5739657182929));
#34493=CARTESIAN_POINT('Ctrl Pts',(0.0665362839956814,1.71236897323351,
10.5750097459456));
#34494=CARTESIAN_POINT('Ctrl Pts',(0.0737004629778612,1.71359869380394,
10.5753790048414));
#34495=CARTESIAN_POINT('Ctrl Pts',(0.0808238736536021,1.71502594797986,
10.5757482637373));
#34496=CARTESIAN_POINT('Ctrl Pts',(0.0878949967574936,1.71664721268132,
10.5761175226332));
#34497=CARTESIAN_POINT('Ctrl Pts',(0.107886359130526,1.72123082545024,10.5771614852807));
#34498=CARTESIAN_POINT('Ctrl Pts',(0.12757777724642,1.72739609197389,10.5782054479283));
#34499=CARTESIAN_POINT('Ctrl Pts',(0.146702583559594,1.7350846098382,10.5792494105758));
#34500=CARTESIAN_POINT('Ctrl Pts',(0.165792207730737,1.74275898384541,10.5802914527416));
#34501=CARTESIAN_POINT('Ctrl Pts',(0.184316591960079,1.7519508307966,10.5813334949074));
#34502=CARTESIAN_POINT('Ctrl Pts',(0.202024092421189,1.76255199499568,10.5823755370731));
#34503=CARTESIAN_POINT('Ctrl Pts',(0.219712575304979,1.77314177371095,10.583416460102));
#34504=CARTESIAN_POINT('Ctrl Pts',(0.236585273164828,1.78513751363441,10.5844573831308));
#34505=CARTESIAN_POINT('Ctrl Pts',(0.252415156711633,1.79838521478177,10.5854983061597));
#34506=CARTESIAN_POINT('Ctrl Pts',(0.268253170074052,1.81163971960315,10.5865397637795));
#34507=CARTESIAN_POINT('Ctrl Pts',(0.283046724588536,1.82614701031703,10.5875812213993));
#34508=CARTESIAN_POINT('Ctrl Pts',(0.296601536710333,1.84171252755685,10.5886226790191));
#34509=CARTESIAN_POINT('Ctrl Pts',(0.31016049041818,1.8572828007408,10.5896644548496));
#34510=CARTESIAN_POINT('Ctrl Pts',(0.322479492742613,1.87391136596323,10.5907062306801));
#34511=CARTESIAN_POINT('Ctrl Pts',(0.333404907572315,1.89137100487541,10.5917480065105));
#34512=CARTESIAN_POINT('Ctrl Pts',(0.344353937934095,1.9088683831933,10.5927920341631));
#34513=CARTESIAN_POINT('Ctrl Pts',(0.353903026703146,1.92719976842434,10.5938360618157));
#34514=CARTESIAN_POINT('Ctrl Pts',(0.361944400361301,1.94611322003792,10.5948800894683));
#34515=CARTESIAN_POINT('Ctrl Pts',(0.364788528819829,1.95280265996074,10.5952493483642));
#34516=CARTESIAN_POINT('Ctrl Pts',(0.367444498865245,1.95956474967142,10.5956186072601));
#34517=CARTESIAN_POINT('Ctrl Pts',(0.36990903717972,1.96638789645855,10.5959878661559));
#34518=CARTESIAN_POINT('Ctrl Pts',(0.376876739170362,1.98567818428725,10.5970318288035));
#34519=CARTESIAN_POINT('Ctrl Pts',(0.382352193119457,2.00557245137034,10.598075791451));
#34520=CARTESIAN_POINT('Ctrl Pts',(0.386240152861614,2.02581486457897,10.5991197540986));
#34521=CARTESIAN_POINT('Ctrl Pts',(0.390120960282875,2.04602003968726,10.6001617962644));
#34522=CARTESIAN_POINT('Ctrl Pts',(0.392419874689684,2.06657138645579,10.6012038384301));
#34523=CARTESIAN_POINT('Ctrl Pts',(0.393091615977614,2.08719877161722,10.6022458805959));
#34524=CARTESIAN_POINT('Ctrl Pts',(0.393762635825953,2.10780400329104,10.6032868036247));
#34525=CARTESIAN_POINT('Ctrl Pts',(0.392809899143816,2.12848438051671,10.6043277266536));
#34526=CARTESIAN_POINT('Ctrl Pts',(0.390239996818926,2.14896565002902,10.6053686496825));
#34527=CARTESIAN_POINT('Ctrl Pts',(0.387668774659185,2.16945743818753,10.6064101073023));
#34528=CARTESIAN_POINT('Ctrl Pts',(0.383478803244115,2.18974918228631,10.607451564922));
#34529=CARTESIAN_POINT('Ctrl Pts',(0.377728502379318,2.20957220674184,10.6084930225418));
#34530=CARTESIAN_POINT('Ctrl Pts',(0.37197644454691,2.22940128799557,10.6095347983723));
#34531=CARTESIAN_POINT('Ctrl Pts',(0.364663347732142,2.24876066852812,10.6105765742028));
#34532=CARTESIAN_POINT('Ctrl Pts',(0.355897095187741,2.26739817094857,10.6116183500333));
#34533=CARTESIAN_POINT('Ctrl Pts',(0.347111894189543,2.28607595875343,10.6126623776859));
#34534=CARTESIAN_POINT('Ctrl Pts',(0.3368676315669,2.30402811361368,10.6137064053385));
#34535=CARTESIAN_POINT('Ctrl Pts',(0.325317803676073,2.32102763766411,10.6147504329911));
#34536=CARTESIAN_POINT('Ctrl Pts',(0.321232780943391,2.32704014649516,10.615119691887));
#34537=CARTESIAN_POINT('Ctrl Pts',(0.316984819419497,2.33293377500648,10.6154889507829));
#34538=CARTESIAN_POINT('Ctrl Pts',(0.312581894557631,2.33869949558967,10.6158582096787));
#34539=CARTESIAN_POINT('Ctrl Pts',(0.300134018156454,2.35500024553087,10.6169021723263));
#34540=CARTESIAN_POINT('Ctrl Pts',(0.286370524356214,2.37037323148458,10.6179461349738));
#34541=CARTESIAN_POINT('Ctrl Pts',(0.271454963761862,2.38459988167434,10.6189900976214));
#34542=CARTESIAN_POINT('Ctrl Pts',(0.256566841948458,2.39880036040807,10.6200321397871));
#34543=CARTESIAN_POINT('Ctrl Pts',(0.240531345533421,2.41185814414704,10.6210741819529));
#34544=CARTESIAN_POINT('Ctrl Pts',(0.223551096465811,2.42358893255013,10.6221162241187));
#34545=CARTESIAN_POINT('Ctrl Pts',(0.206589083918966,2.43530712227075,10.6231571471475));
#34546=CARTESIAN_POINT('Ctrl Pts',(0.188684918897334,2.44570070607319,10.6241980701764));
#34547=CARTESIAN_POINT('Ctrl Pts',(0.170072766223247,2.45462676744596,10.6252389932052));
#34548=CARTESIAN_POINT('Ctrl Pts',(0.151451054832624,2.46355741301122,10.626280450825));
#34549=CARTESIAN_POINT('Ctrl Pts',(0.132121285848229,2.4710186977558,10.6273219084448));
#34550=CARTESIAN_POINT('Ctrl Pts',(0.112340990207518,2.47691430315019,10.6283633660646));
#34551=CARTESIAN_POINT('Ctrl Pts',(0.0925546508241235,2.48281170990906,
10.6294051418951));
#34552=CARTESIAN_POINT('Ctrl Pts',(0.072318225609469,2.48714230965479,10.6304469177255));
#34553=CARTESIAN_POINT('Ctrl Pts',(0.05190214898293,2.4898603043796,10.631488693556));
#34554=CARTESIAN_POINT('Ctrl Pts',(0.0314419425434746,2.49258417411169,
10.6325327212086));
#34555=CARTESIAN_POINT('Ctrl Pts',(0.0108020448549819,2.49368844048206,
10.6335767488612));
#34556=CARTESIAN_POINT('Ctrl Pts',(-0.00974358986208664,2.49317928792931,
10.6346207765138));
#34557=CARTESIAN_POINT('Ctrl Pts',(-0.0170103115543989,2.49299920734525,
10.6349900354097));
#34558=CARTESIAN_POINT('Ctrl Pts',(-0.0242652782571971,2.49261777284311,
10.6353592943056));
#34559=CARTESIAN_POINT('Ctrl Pts',(-0.0314965821387619,2.49203680351923,
10.6357285532014));
#34560=CARTESIAN_POINT('Ctrl Pts',(-0.0519408049590046,2.4903942966486,
10.636772515849));
#34561=CARTESIAN_POINT('Ctrl Pts',(-0.0723171146773218,2.48714337970345,
10.6378164784965));
#34562=CARTESIAN_POINT('Ctrl Pts',(-0.0923531993330601,2.48230325210878,
10.6388604411441));
#34563=CARTESIAN_POINT('Ctrl Pts',(-0.112352425452054,2.47747202845037,
10.6399024833098));
#34564=CARTESIAN_POINT('Ctrl Pts',(-0.132011947763811,2.47105751023603,
10.6409445254756));
#34565=CARTESIAN_POINT('Ctrl Pts',(-0.151067120319559,2.46313030052359,
10.6419865676414));
#34566=CARTESIAN_POINT('Ctrl Pts',(-0.170101827919337,2.45521160450986,
10.6430274906702));
#34567=CARTESIAN_POINT('Ctrl Pts',(-0.188532787305078,2.44578369670904,
10.6440684136991));
#34568=CARTESIAN_POINT('Ctrl Pts',(-0.206113074065671,2.43496610380634,
10.6451093367279));
#34569=CARTESIAN_POINT('Ctrl Pts',(-0.223702389603354,2.42414295526986,
10.6461507943477));
#34570=CARTESIAN_POINT('Ctrl Pts',(-0.240439524624304,2.4119290676693,10.6471922519675));
#34571=CARTESIAN_POINT('Ctrl Pts',(-0.256104086634659,2.39848883866742,
10.6482337095873));
#34572=CARTESIAN_POINT('Ctrl Pts',(-0.271773434851617,2.38504450308965,
10.6492754854178));
#34573=CARTESIAN_POINT('Ctrl Pts',(-0.28636902327221,2.37037358633983,10.6503172612483));
#34574=CARTESIAN_POINT('Ctrl Pts',(-0.299705953073875,2.35467868323062,
10.6513590370788));
#34575=CARTESIAN_POINT('Ctrl Pts',(-0.313071710951967,2.33894985523216,
10.6524030647314));
#34576=CARTESIAN_POINT('Ctrl Pts',(-0.325172947445456,2.32219321905018,
10.653447092384));
#34577=CARTESIAN_POINT('Ctrl Pts',(-0.335866566171454,2.30464246804658,
10.6544911200366));
#34578=CARTESIAN_POINT('Ctrl Pts',(-0.339648758945623,2.29843499746736,
10.6548603789325));
#34579=CARTESIAN_POINT('Ctrl Pts',(-0.343255286552126,2.29212841417969,
10.6552296378284));
#34580=CARTESIAN_POINT('Ctrl Pts',(-0.346681232595258,2.28573371521141,
10.6555988967243));
#34581=CARTESIAN_POINT('Ctrl Pts',(-0.356893907206437,2.26667124925972,
10.6566996498895));
#34582=CARTESIAN_POINT('Ctrl Pts',(-0.365553831017984,2.24672094907881,
10.6578004030547));
#34583=CARTESIAN_POINT('Ctrl Pts',(-0.372520334458991,2.22614868376072,
10.6589011562199));
#34584=CARTESIAN_POINT('Ctrl Pts',(-0.379459197939549,2.2056580399626,10.6599975420904));
#34585=CARTESIAN_POINT('Ctrl Pts',(-0.384717760168914,2.18455089922893,
10.6610939279609));
#34586=CARTESIAN_POINT('Ctrl Pts',(-0.388203047708099,2.16311326128591,
10.6621903138313));
#34587=CARTESIAN_POINT('Ctrl Pts',(-0.391586797707641,2.14230017009492,
10.6632547584853));
#34588=CARTESIAN_POINT('Ctrl Pts',(-0.393299115142935,2.12117615124244,
10.6643192031393));
#34589=CARTESIAN_POINT('Ctrl Pts',(-0.393299999656376,2.1000164406377,10.6653836477933));
#34590=CARTESIAN_POINT('',(-0.393299837322886,2.09964228252567,10.7903836477965));
#34591=CARTESIAN_POINT('Ctrl Pts',(-0.393299999656379,2.10001644057314,
10.6653836477965));
#34592=CARTESIAN_POINT('Ctrl Pts',(-0.393300903919296,2.07838418954183,
10.6664718637175));
#34593=CARTESIAN_POINT('Ctrl Pts',(-0.391512781482813,2.05678450351341,
10.6675600796385));
#34594=CARTESIAN_POINT('Ctrl Pts',(-0.387977325474063,2.03551368425788,
10.6686482955595));
#34595=CARTESIAN_POINT('Ctrl Pts',(-0.384283948480357,2.01329274464465,
10.6697851196741));
#34596=CARTESIAN_POINT('Ctrl Pts',(-0.378683490893823,1.99143152671946,
10.6709219437887));
#34597=CARTESIAN_POINT('Ctrl Pts',(-0.371281621402311,1.97025082809948,
10.6720587679033));
#34598=CARTESIAN_POINT('Ctrl Pts',(-0.363879751910796,1.94907012947949,
10.6731955920179));
#34599=CARTESIAN_POINT('Ctrl Pts',(-0.354676875977424,1.92857061784174,
10.6743324161325));
#34600=CARTESIAN_POINT('Ctrl Pts',(-0.343833048533687,1.90904522855914,
10.6754692402471));
#34601=CARTESIAN_POINT('Ctrl Pts',(-0.333874999031955,1.8911147705151,10.6765132028946));
#34602=CARTESIAN_POINT('Ctrl Pts',(-0.322480926677385,1.87391193429824,
10.6775571655422));
#34603=CARTESIAN_POINT('Ctrl Pts',(-0.309781032102686,1.85767665785279,
10.6786011281898));
#34604=CARTESIAN_POINT('Ctrl Pts',(-0.297104500352545,1.84147124794781,
10.6796431703555));
#34605=CARTESIAN_POINT('Ctrl Pts',(-0.283127316027989,1.82623047435161,
10.6806852125213));
#34606=CARTESIAN_POINT('Ctrl Pts',(-0.26802329913917,1.81216601813101,10.6817272546871));
#34607=CARTESIAN_POINT('Ctrl Pts',(-0.252935503727212,1.79811666691546,
10.6827681777159));
#34608=CARTESIAN_POINT('Ctrl Pts',(-0.236723794323403,1.78524164506732,
10.6838091007448));
#34609=CARTESIAN_POINT('Ctrl Pts',(-0.219599190286858,1.77371624982945,
10.6848500237736));
#34610=CARTESIAN_POINT('Ctrl Pts',(-0.202465791499996,1.76218493544898,
10.6858914813934));
#34611=CARTESIAN_POINT('Ctrl Pts',(-0.184419162849741,1.75200505659938,
10.6869329390132));
#34612=CARTESIAN_POINT('Ctrl Pts',(-0.165700186865509,1.74330918420467,
10.687974396633));
#34613=CARTESIAN_POINT('Ctrl Pts',(-0.146975491418038,1.73461065484185,
10.6890161724635));
#34614=CARTESIAN_POINT('Ctrl Pts',(-0.127578721642701,1.7273973115178,10.690057948294));
#34615=CARTESIAN_POINT('Ctrl Pts',(-0.107770838341297,1.72175360358199,
10.6910997241245));
#34616=CARTESIAN_POINT('Ctrl Pts',(-0.0879201398506443,1.71609769664339,
10.6921437517771));
#34617=CARTESIAN_POINT('Ctrl Pts',(-0.06765727571691,1.7120183440099,10.6931877794297));
#34618=CARTESIAN_POINT('Ctrl Pts',(-0.0472542116476989,1.70954906904765,
10.6942318070823));
#34619=CARTESIAN_POINT('Ctrl Pts',(-0.0400379153251642,1.7086757188602,
10.6946010659781));
#34620=CARTESIAN_POINT('Ctrl Pts',(-0.0328041132268868,1.70800330430401,
10.694970324874));
#34621=CARTESIAN_POINT('Ctrl Pts',(-0.0255648510851573,1.70753174855921,
10.6953395837698));
#34622=CARTESIAN_POINT('Ctrl Pts',(-0.0050981288021612,1.70619857395095,
10.6963835464174));
#34623=CARTESIAN_POINT('Ctrl Pts',(0.0155341411384485,1.70646670791081,
10.6974275090649));
#34624=CARTESIAN_POINT('Ctrl Pts',(0.0360597346621666,1.70835655816024,
10.6984714717125));
#34625=CARTESIAN_POINT('Ctrl Pts',(0.0565475691448373,1.71024293182649,
10.6995135138782));
#34626=CARTESIAN_POINT('Ctrl Pts',(0.0769283868876979,1.71374509252851,
10.700555556044));
#34627=CARTESIAN_POINT('Ctrl Pts',(0.0969301107475258,1.71883147607591,
10.7015975982098));
#34628=CARTESIAN_POINT('Ctrl Pts',(0.116910353070145,1.72391239692728,10.7026385212386));
#34629=CARTESIAN_POINT('Ctrl Pts',(0.136511593186629,1.73057401049135,10.7036794442675));
#34630=CARTESIAN_POINT('Ctrl Pts',(0.155472209444625,1.73873377947778,10.7047203672964));
#34631=CARTESIAN_POINT('Ctrl Pts',(0.174442563380965,1.7468977391089,10.7057618249162));
#34632=CARTESIAN_POINT('Ctrl Pts',(0.192770953952402,1.75656111523172,10.7068032825359));
#34633=CARTESIAN_POINT('Ctrl Pts',(0.210215519086775,1.76759313253924,10.7078447401557));
#34634=CARTESIAN_POINT('Ctrl Pts',(0.227665414296312,1.778628520609,10.7088865159862));
#34635=CARTESIAN_POINT('Ctrl Pts',(0.244230344470396,1.7910329588451,10.7099282918167));
#34636=CARTESIAN_POINT('Ctrl Pts',(0.259698040286721,1.8046327406918,10.7109700676472));
#34637=CARTESIAN_POINT('Ctrl Pts',(0.275199169878563,1.81826191877559,10.7120140952998));
#34638=CARTESIAN_POINT('Ctrl Pts',(0.289597817093409,1.83309107044353,10.7130581229525));
#34639=CARTESIAN_POINT('Ctrl Pts',(0.302718574933163,1.84890966886311,10.714102150605));
#34640=CARTESIAN_POINT('Ctrl Pts',(0.30735921499739,1.85450449977778,10.7144714095009));
#34641=CARTESIAN_POINT('Ctrl Pts',(0.31184038097793,1.86022281995002,10.7148406683968));
#34642=CARTESIAN_POINT('Ctrl Pts',(0.316155616893762,1.86605445952845,10.7152099272926));
#34643=CARTESIAN_POINT('Ctrl Pts',(0.328355580556014,1.88254157456363,10.7162538899402));
#34644=CARTESIAN_POINT('Ctrl Pts',(0.339298749242088,1.90003470229508,10.7172978525877));
#34645=CARTESIAN_POINT('Ctrl Pts',(0.348820603964078,1.91831599891533,10.7183418152353));
#34646=CARTESIAN_POINT('Ctrl Pts',(0.358324942208264,1.93656366512051,10.7193838574011));
#34647=CARTESIAN_POINT('Ctrl Pts',(0.366412767688192,1.95559600445267,10.7204258995668));
#34648=CARTESIAN_POINT('Ctrl Pts',(0.372963339866515,1.97516716331183,10.7214679417326));
#34649=CARTESIAN_POINT('Ctrl Pts',(0.379506876833226,1.99471730305384,10.7225088647615));
#34650=CARTESIAN_POINT('Ctrl Pts',(0.384516178323465,2.01480442848181,10.7235497877903));
#34651=CARTESIAN_POINT('Ctrl Pts',(0.387919022641102,2.03516388449967,10.7245907108192));
#34652=CARTESIAN_POINT('Ctrl Pts',(0.391323614570892,2.0555337966035,10.7256321684389));
#34653=CARTESIAN_POINT('Ctrl Pts',(0.393119963899375,2.07617559565587,10.7266736260587));
#34654=CARTESIAN_POINT('Ctrl Pts',(0.393287104536297,2.09681512865945,10.7277150836785));
#34655=CARTESIAN_POINT('Ctrl Pts',(0.39345429624197,2.11746096794018,10.728756859509));
#34656=CARTESIAN_POINT('Ctrl Pts',(0.391991318491797,2.13810380436656,10.7297986353395));
#34657=CARTESIAN_POINT('Ctrl Pts',(0.388929321648321,2.15847112759454,10.73084041117));
#34658=CARTESIAN_POINT('Ctrl Pts',(0.385860706229182,2.17888247525387,10.7318844388226));
#34659=CARTESIAN_POINT('Ctrl Pts',(0.381186337904448,2.19901640337461,10.7329284664752));
#34660=CARTESIAN_POINT('Ctrl Pts',(0.374988280426774,2.21861146463378,10.7339724941278));
#34661=CARTESIAN_POINT('Ctrl Pts',(0.372796108739457,2.22554198095415,10.7343417530237));
#34662=CARTESIAN_POINT('Ctrl Pts',(0.370413778870354,2.23240525557609,10.7347110119195));
#34663=CARTESIAN_POINT('Ctrl Pts',(0.367846347073399,2.23919035507088,10.7350802708154));
#34664=CARTESIAN_POINT('Ctrl Pts',(0.36058774632988,2.25837307622284,10.736124233463));
#34665=CARTESIAN_POINT('Ctrl Pts',(0.351802946269833,2.27704363450668,10.7371681961105));
#34666=CARTESIAN_POINT('Ctrl Pts',(0.341586056766116,2.29494577662257,10.7382121587581));
#34667=CARTESIAN_POINT('Ctrl Pts',(0.331387962331579,2.31281498581896,10.7392542009239));
#34668=CARTESIAN_POINT('Ctrl Pts',(0.319763316728726,2.32991792346314,10.7402962430896));
#34669=CARTESIAN_POINT('Ctrl Pts',(0.306853479031764,2.34601998375356,10.7413382852554));
#34670=CARTESIAN_POINT('Ctrl Pts',(0.293957506297671,2.3621047506842,10.7423792082843));
#34671=CARTESIAN_POINT('Ctrl Pts',(0.279779516999117,2.37719018501119,10.7434201313131));
#34672=CARTESIAN_POINT('Ctrl Pts',(0.264502942970299,2.39107229885383,10.744461054342));
#34673=CARTESIAN_POINT('Ctrl Pts',(0.24921852329122,2.40496154218831,10.7455025119618));
#34674=CARTESIAN_POINT('Ctrl Pts',(0.232834925418655,2.41764572366694,10.7465439695816));
#34675=CARTESIAN_POINT('Ctrl Pts',(0.215571312777791,2.42895881065456,10.7475854272014));
#34676=CARTESIAN_POINT('Ctrl Pts',(0.198302425350644,2.44027535428345,10.7486272030319));
#34677=CARTESIAN_POINT('Ctrl Pts',(0.180153622595453,2.45021959674736,10.7496689788624));
#34678=CARTESIAN_POINT('Ctrl Pts',(0.161370898342717,2.45867021505565,10.7507107546929));
#34679=CARTESIAN_POINT('Ctrl Pts',(0.142547574805271,2.46713909956718,10.7517547823455));
#34680=CARTESIAN_POINT('Ctrl Pts',(0.123088287520985,2.47410766607676,10.7527988099981));
#34681=CARTESIAN_POINT('Ctrl Pts',(0.103257288672177,2.47950338909695,10.7538428376507));
#34682=CARTESIAN_POINT('Ctrl Pts',(0.096243324319536,2.48141178560329,10.7542120965465));
#34683=CARTESIAN_POINT('Ctrl Pts',(0.0891829619311183,2.48312389455941,
10.7545813554424));
#34684=CARTESIAN_POINT('Ctrl Pts',(0.0820881315711749,2.48463804889162,
10.7549506143382));
#34685=CARTESIAN_POINT('Ctrl Pts',(0.0620297444348467,2.488918840995,10.7559945769858));
#34686=CARTESIAN_POINT('Ctrl Pts',(0.0415758337412953,2.49163913437268,
10.7570385396333));
#34687=CARTESIAN_POINT('Ctrl Pts',(0.0209928052276988,2.49273934374935,
10.7580825022809));
#34688=CARTESIAN_POINT('Ctrl Pts',(0.000447641413002693,2.49383752917232,
10.7591245444467));
#34689=CARTESIAN_POINT('Ctrl Pts',(-0.0202254454845265,2.49332144819461,
10.7601665866124));
#34690=CARTESIAN_POINT('Ctrl Pts',(-0.0407526744854151,2.49118296169732,
10.7612086287782));
#34691=CARTESIAN_POINT('Ctrl Pts',(-0.0612578575648515,2.48904677190093,
10.7622495518071));
#34692=CARTESIAN_POINT('Ctrl Pts',(-0.0816167626296247,2.48529168282829,
10.7632904748359));
#34693=CARTESIAN_POINT('Ctrl Pts',(-0.101558578051101,2.47996150492417,
10.7643313978648));
#34694=CARTESIAN_POINT('Ctrl Pts',(-0.12151063506921,2.4746285895796,10.7653728554845));
#34695=CARTESIAN_POINT('Ctrl Pts',(-0.14104445952005,2.4677191437732,10.7664143131043));
#34696=CARTESIAN_POINT('Ctrl Pts',(-0.159901811069196,2.45932756757142,
10.7674557707241));
#34697=CARTESIAN_POINT('Ctrl Pts',(-0.178764924361347,2.45093342737726,
10.7684975465546));
#34698=CARTESIAN_POINT('Ctrl Pts',(-0.196950496329909,2.44105658720445,
10.7695393223851));
#34699=CARTESIAN_POINT('Ctrl Pts',(-0.214223355526875,2.42983820874302,
10.7705810982156));
#34700=CARTESIAN_POINT('Ctrl Pts',(-0.231533550400975,2.41859558150197,
10.7716251258682));
#34701=CARTESIAN_POINT('Ctrl Pts',(-0.247926509704076,2.40600607531257,
10.7726691535208));
#34702=CARTESIAN_POINT('Ctrl Pts',(-0.263198208226789,2.39225261878417,
10.7737131811734));
#34703=CARTESIAN_POINT('Ctrl Pts',(-0.268599607816748,2.38738820148688,
10.7740824400693));
#34704=CARTESIAN_POINT('Ctrl Pts',(-0.27386108141518,2.38237851789273,10.7744516989651));
#34705=CARTESIAN_POINT('Ctrl Pts',(-0.278974769357337,2.37723269659624,
10.774820957861));
#34706=CARTESIAN_POINT('Ctrl Pts',(-0.293233924883227,2.36288393949469,
10.7758506100583));
#34707=CARTESIAN_POINT('Ctrl Pts',(-0.306431222875898,2.34738350856294,
10.7768802622555));
#34708=CARTESIAN_POINT('Ctrl Pts',(-0.318374647887716,2.33091659442832,
10.7779099144527));
#34709=CARTESIAN_POINT('Ctrl Pts',(-0.330432044486473,2.3142925427612,10.7789493922314));
#34710=CARTESIAN_POINT('Ctrl Pts',(-0.341210903503436,2.29668397029978,
10.77998887001));
#34711=CARTESIAN_POINT('Ctrl Pts',(-0.350553101672658,2.27831829100706,
10.7810283477887));
#34712=CARTESIAN_POINT('Ctrl Pts',(-0.359783125904629,2.26017313267945,
10.7820553443169));
#34713=CARTESIAN_POINT('Ctrl Pts',(-0.367610470850558,2.24128964931751,
10.7830823408451));
#34714=CARTESIAN_POINT('Ctrl Pts',(-0.373927706534286,2.22191374116977,
10.7841093373733));
#34715=CARTESIAN_POINT('Ctrl Pts',(-0.380360103757361,2.20218461532995,
10.7851550557771));
#34716=CARTESIAN_POINT('Ctrl Pts',(-0.385226426293683,2.18194566437344,
10.786200774181));
#34717=CARTESIAN_POINT('Ctrl Pts',(-0.388466071386825,2.16147358279201,
10.7872464925849));
#34718=CARTESIAN_POINT('Ctrl Pts',(-0.391705716479968,2.14100150121058,
10.7882922109888));
#34719=CARTESIAN_POINT('Ctrl Pts',(-0.393318623483942,2.12029711383068,
10.7893379293926));
#34720=CARTESIAN_POINT('Ctrl Pts',(-0.393299837322886,2.09964228252567,
10.7903836477965));
#34721=CARTESIAN_POINT('',(-0.393454859789483,2.10017238244214,10.9153836477965));
#34722=CARTESIAN_POINT('Ctrl Pts',(-0.393365501908144,2.09964222280185,
10.7903836477965));
#34723=CARTESIAN_POINT('Ctrl Pts',(-0.393628539003501,2.07127590643749,
10.7918195323256));
#34724=CARTESIAN_POINT('Ctrl Pts',(-0.377873717533349,1.91235128146771,
10.7998788646957));
#34725=CARTESIAN_POINT('Ctrl Pts',(-0.161856479690965,1.66402119264042,
10.8145616449065));
#34726=CARTESIAN_POINT('Ctrl Pts',(0.278962950142402,1.72790496787461,10.8344319884294));
#34727=CARTESIAN_POINT('Ctrl Pts',(0.463871850595977,2.13313527891918,10.8543023319521));
#34728=CARTESIAN_POINT('Ctrl Pts',(0.223241478578169,2.50796848251641,10.8741726754749));
#34729=CARTESIAN_POINT('Ctrl Pts',(-0.22218255845236,2.50854614329848,10.8940430189977));
#34730=CARTESIAN_POINT('Ctrl Pts',(-0.389209440306793,2.2498445668232,10.9077800097716));
#34731=CARTESIAN_POINT('Ctrl Pts',(-0.393910523469697,2.10982310132666,
10.9148935527045));
#34732=CARTESIAN_POINT('Ctrl Pts',(-0.393857559113655,2.10017255887481,
10.9153836477965));
#34733=CARTESIAN_POINT('',(-0.393299911892188,2.10026325956176,11.0403836477918));
#34734=CARTESIAN_POINT('Ctrl Pts',(-0.393299962252333,2.10017231457764,
10.9153836477965));
#34735=CARTESIAN_POINT('Ctrl Pts',(-0.393308860645182,2.07986214918405,
10.9164165483161));
#34736=CARTESIAN_POINT('Ctrl Pts',(-0.391740229032019,2.05948767802324,
10.9174494488357));
#34737=CARTESIAN_POINT('Ctrl Pts',(-0.388590402319534,2.03931730703782,
10.9184823493553));
#34738=CARTESIAN_POINT('Ctrl Pts',(-0.385446002585379,2.01918168849316,
10.9195134702441));
#34739=CARTESIAN_POINT('Ctrl Pts',(-0.380725869940055,1.9992502169752,10.9205445911328));
#34740=CARTESIAN_POINT('Ctrl Pts',(-0.374478210275068,1.97978785406964,
10.9215757120216));
#34741=CARTESIAN_POINT('Ctrl Pts',(-0.368231000004424,1.96032689109242,
10.9226067587418));
#34742=CARTESIAN_POINT('Ctrl Pts',(-0.360456661425524,1.94133570028298,
10.923637805462));
#34743=CARTESIAN_POINT('Ctrl Pts',(-0.351253818214342,1.92306598633998,
10.9246688521823));
#34744=CARTESIAN_POINT('Ctrl Pts',(-0.342052869418203,1.90480003323698,
10.9256996866604));
#34745=CARTESIAN_POINT('Ctrl Pts',(-0.331424349561752,1.88725592944221,
10.9267305211386));
#34746=CARTESIAN_POINT('Ctrl Pts',(-0.319513281200284,1.87066148789044,
10.9277613556167));
#34747=CARTESIAN_POINT('Ctrl Pts',(-0.307574770851816,1.85402881429805,
10.9287945650411));
#34748=CARTESIAN_POINT('Ctrl Pts',(-0.294348272970208,1.8383507713546,10.9298277744654));
#34749=CARTESIAN_POINT('Ctrl Pts',(-0.280020318160216,1.82382340537719,
10.9308609838898));
#34750=CARTESIAN_POINT('Ctrl Pts',(-0.266510107499354,1.81012516460906,
10.9318352246076));
#34751=CARTESIAN_POINT('Ctrl Pts',(-0.25202134251128,1.79745002976386,10.9328094653255));
#34752=CARTESIAN_POINT('Ctrl Pts',(-0.236736783861808,1.78592901253575,
10.9337837060434));
#34753=CARTESIAN_POINT('Ctrl Pts',(-0.22035837961134,1.77358348906557,10.9348276686909));
#34754=CARTESIAN_POINT('Ctrl Pts',(-0.202962869780021,1.76248580027779,
10.9358716313385));
#34755=CARTESIAN_POINT('Ctrl Pts',(-0.184766632364385,1.75280238830786,
10.936915593986));
#34756=CARTESIAN_POINT('Ctrl Pts',(-0.166603868888234,1.7431367900177,10.9379576361518));
#34757=CARTESIAN_POINT('Ctrl Pts',(-0.147643915980189,1.73488069849844,
10.9389996783176));
#34758=CARTESIAN_POINT('Ctrl Pts',(-0.128131548108157,1.72815702725558,
10.9400417204833));
#34759=CARTESIAN_POINT('Ctrl Pts',(-0.108640136212677,1.72144057713001,
10.9410826435122));
#34760=CARTESIAN_POINT('Ctrl Pts',(-0.0885981698533844,1.71625354581778,
10.942123566541));
#34761=CARTESIAN_POINT('Ctrl Pts',(-0.0682696540235158,1.71267049642519,
10.9431644895699));
#34762=CARTESIAN_POINT('Ctrl Pts',(-0.0479306979977496,1.70908560687182,
10.9442059471897));
#34763=CARTESIAN_POINT('Ctrl Pts',(-0.0273056203105137,1.7071064885264,
10.9452474048095));
#34764=CARTESIAN_POINT('Ctrl Pts',(-0.00666837749199288,1.70675653502998,
10.9462888624293));
#34765=CARTESIAN_POINT('Ctrl Pts',(0.0139751709039052,1.70640647460752,
10.9473306382597));
#34766=CARTESIAN_POINT('Ctrl Pts',(0.0346301561646096,1.70768654628708,
10.9483724140902));
#34767=CARTESIAN_POINT('Ctrl Pts',(0.0550238027152715,1.71056801475129,
10.9494141899207));
#34768=CARTESIAN_POINT('Ctrl Pts',(0.0754615305957612,1.71345571157498,
10.9504582175733));
#34769=CARTESIAN_POINT('Ctrl Pts',(0.0956360731470906,1.71795155561728,
10.9515022452259));
#34770=CARTESIAN_POINT('Ctrl Pts',(0.1152852664044,1.72397580217482,10.9525462728785));
#34771=CARTESIAN_POINT('Ctrl Pts',(0.12223492850275,1.72610649921789,10.9529155317744));
#34772=CARTESIAN_POINT('Ctrl Pts',(0.129119035910486,1.72842794259158,10.9532847906703));
#34773=CARTESIAN_POINT('Ctrl Pts',(0.135926610840863,1.73093517308565,10.9536540495661));
#34774=CARTESIAN_POINT('Ctrl Pts',(0.155172874173353,1.73802357370082,10.9546980122137));
#34775=CARTESIAN_POINT('Ctrl Pts',(0.17392051339201,1.74664265035955,10.9557419748612));
#34776=CARTESIAN_POINT('Ctrl Pts',(0.191912451650082,1.75670056670356,10.9567859375088));
#34777=CARTESIAN_POINT('Ctrl Pts',(0.209871291798986,1.76673998042666,10.9578279796746));
#34778=CARTESIAN_POINT('Ctrl Pts',(0.227076526462355,1.77821267678054,10.9588700218403));
#34779=CARTESIAN_POINT('Ctrl Pts',(0.243292306921786,1.79097938031148,10.9599120640061));
#34780=CARTESIAN_POINT('Ctrl Pts',(0.259490671887751,1.8037323726034,10.9609529870349));
#34781=CARTESIAN_POINT('Ctrl Pts',(0.274701099211307,1.81777618298433,10.9619939100638));
#34782=CARTESIAN_POINT('Ctrl Pts',(0.288717984224568,1.83292919368583,10.9630348330927));
#34783=CARTESIAN_POINT('Ctrl Pts',(0.302742067944637,1.84808998657868,10.9640762907124));
#34784=CARTESIAN_POINT('Ctrl Pts',(0.315570873307961,1.86436058865663,10.9651177483322));
#34785=CARTESIAN_POINT('Ctrl Pts',(0.327036432902423,1.88152331576468,10.966159205952));
#34786=CARTESIAN_POINT('Ctrl Pts',(0.338505495725203,1.89869128683411,10.9672009817825));
#34787=CARTESIAN_POINT('Ctrl Pts',(0.348610105271661,1.91675129418567,10.968242757613));
#34788=CARTESIAN_POINT('Ctrl Pts',(0.357226764363725,1.93545842828567,10.9692845334435));
#34789=CARTESIAN_POINT('Ctrl Pts',(0.365862048559952,1.95420599828053,10.9703285610961));
#34790=CARTESIAN_POINT('Ctrl Pts',(0.373002706807748,1.97360279648528,10.9713725887487));
#34791=CARTESIAN_POINT('Ctrl Pts',(0.378573875790318,1.99338522349554,10.9724166164013));
#34792=CARTESIAN_POINT('Ctrl Pts',(0.380544325233959,2.00038200862594,10.9727858752972));
#34793=CARTESIAN_POINT('Ctrl Pts',(0.382318905809099,2.00742692863409,10.973155134193));
#34794=CARTESIAN_POINT('Ctrl Pts',(0.383895844834153,2.01450806869025,10.9735243930889));
#34795=CARTESIAN_POINT('Ctrl Pts',(0.388354140783265,2.03452775082497,10.9745683557365));
#34796=CARTESIAN_POINT('Ctrl Pts',(0.391255502666754,2.05495676347717,10.975612318384));
#34797=CARTESIAN_POINT('Ctrl Pts',(0.392537987796697,2.07552923915117,10.9766562810316));
#34798=CARTESIAN_POINT('Ctrl Pts',(0.393818113657047,2.09606386953937,10.9776983231973));
#34799=CARTESIAN_POINT('Ctrl Pts',(0.393485169553287,2.11674071672829,10.9787403653631));
#34800=CARTESIAN_POINT('Ctrl Pts',(0.39152859160775,2.13728608257315,10.9797824075289));
#34801=CARTESIAN_POINT('Ctrl Pts',(0.38957411499619,2.15780938301784,10.9808233305577));
#34802=CARTESIAN_POINT('Ctrl Pts',(0.385999506927345,2.17820075095957,10.9818642535866));
#34803=CARTESIAN_POINT('Ctrl Pts',(0.380846177350917,2.19818899733266,10.9829051766154));
#34804=CARTESIAN_POINT('Ctrl Pts',(0.375690201158729,2.21818750914814,10.9839466342352));
#34805=CARTESIAN_POINT('Ctrl Pts',(0.368954051761435,2.23778176928542,10.984988091855));
#34806=CARTESIAN_POINT('Ctrl Pts',(0.360729838098909,2.25671271137063,10.9860295494748));
#34807=CARTESIAN_POINT('Ctrl Pts',(0.352503111580559,2.27564943768398,10.9870713253053));
#34808=CARTESIAN_POINT('Ctrl Pts',(0.342787741772241,2.29392178261049,10.9881131011358));
#34809=CARTESIAN_POINT('Ctrl Pts',(0.331722801740919,2.31129333355588,10.9891548769662));
#34810=CARTESIAN_POINT('Ctrl Pts',(0.320633944590629,2.32870243350283,10.9901989046188));
#34811=CARTESIAN_POINT('Ctrl Pts',(0.308190136705372,2.3452062641528,10.9912429322714));
#34812=CARTESIAN_POINT('Ctrl Pts',(0.294572492317858,2.36059918796812,10.992286959924));
#34813=CARTESIAN_POINT('Ctrl Pts',(0.289756109994744,2.36604346335493,10.9926562188199));
#34814=CARTESIAN_POINT('Ctrl Pts',(0.284793227646956,2.37134910496925,10.9930254777158));
#34815=CARTESIAN_POINT('Ctrl Pts',(0.279692903892098,2.37650817259605,10.9933947366116));
#34816=CARTESIAN_POINT('Ctrl Pts',(0.265273352866704,2.39109380332532,10.9944386992592));
#34817=CARTESIAN_POINT('Ctrl Pts',(0.249666832871676,2.40459191402152,10.9954826619067));
#34818=CARTESIAN_POINT('Ctrl Pts',(0.233063359361353,2.41680650328426,10.9965266245543));
#34819=CARTESIAN_POINT('Ctrl Pts',(0.216490429729673,2.42899862249386,10.99756866672));
#34820=CARTESIAN_POINT('Ctrl Pts',(0.198924737747735,2.43991142812055,10.9986107088858));
#34821=CARTESIAN_POINT('Ctrl Pts',(0.180590695298224,2.44938788011564,10.9996527510516));
#34822=CARTESIAN_POINT('Ctrl Pts',(0.162276343322299,2.45885415455016,11.0006936740804));
#34823=CARTESIAN_POINT('Ctrl Pts',(0.143195916125291,2.46688677600022,11.0017345971093));
#34824=CARTESIAN_POINT('Ctrl Pts',(0.123599850283095,2.47337376315161,11.0027755201382));
#34825=CARTESIAN_POINT('Ctrl Pts',(0.103993720412203,2.47986408185054,11.0038169777579));
#34826=CARTESIAN_POINT('Ctrl Pts',(0.0838721162823775,2.48480693388882,
11.0048584353777));
#34827=CARTESIAN_POINT('Ctrl Pts',(0.0635027257726444,2.48813952880304,
11.0058998929975));
#34828=CARTESIAN_POINT('Ctrl Pts',(0.0431271115260769,2.49147314197029,
11.006941668828));
#34829=CARTESIAN_POINT('Ctrl Pts',(0.0225042915339611,2.4931954355568,11.0079834446585));
#34830=CARTESIAN_POINT('Ctrl Pts',(0.00190832850244365,2.49329537027828,
11.009025220489));
#34831=CARTESIAN_POINT('Ctrl Pts',(-0.018732153170544,2.49339552101093,
11.0100692481416));
#34832=CARTESIAN_POINT('Ctrl Pts',(-0.0393449275255872,2.49186636627842,
11.0111132757942));
#34833=CARTESIAN_POINT('Ctrl Pts',(-0.0596590504325071,2.4887488748556,
11.0121573034468));
#34834=CARTESIAN_POINT('Ctrl Pts',(-0.0668438894322014,2.48764625900265,
11.0125265623427));
#34835=CARTESIAN_POINT('Ctrl Pts',(-0.0739914657842849,2.48634541833996,
11.0128958212386));
#34836=CARTESIAN_POINT('Ctrl Pts',(-0.0810901996203999,2.48484967133353,
11.0132650801344));
#34837=CARTESIAN_POINT('Ctrl Pts',(-0.101159622599137,2.48062092011757,
11.014309042782));
#34838=CARTESIAN_POINT('Ctrl Pts',(-0.120957167013114,2.47480544989585,
11.0153530054296));
#34839=CARTESIAN_POINT('Ctrl Pts',(-0.140215172576819,2.46745692996493,
11.0163969680771));
#34840=CARTESIAN_POINT('Ctrl Pts',(-0.159437750964121,2.46012192842828,
11.0174390102429));
#34841=CARTESIAN_POINT('Ctrl Pts',(-0.178122059783856,2.45125967897456,
11.0184810524086));
#34842=CARTESIAN_POINT('Ctrl Pts',(-0.196014578744431,2.44097386251683,
11.0195230945744));
#34843=CARTESIAN_POINT('Ctrl Pts',(-0.213887881420712,2.43069909286439,
11.0205640176033));
#34844=CARTESIAN_POINT('Ctrl Pts',(-0.230970433358254,2.419004131185,11.0216049406321));
#34845=CARTESIAN_POINT('Ctrl Pts',(-0.247032512819492,2.40603893152684,
11.022645863661));
#34846=CARTESIAN_POINT('Ctrl Pts',(-0.263102841346124,2.39306707328003,
11.0236873212808));
#34847=CARTESIAN_POINT('Ctrl Pts',(-0.27815106772843,2.37882412338271,11.0247287789006));
#34848=CARTESIAN_POINT('Ctrl Pts',(-0.29197949233482,2.36350116898394,11.0257702365204));
#34849=CARTESIAN_POINT('Ctrl Pts',(-0.305812142127802,2.34817353275456,
11.0268120123509));
#34850=CARTESIAN_POINT('Ctrl Pts',(-0.318423782504393,2.33176580510451,
11.0278537881814));
#34851=CARTESIAN_POINT('Ctrl Pts',(-0.329656776341884,2.31450244709997,
11.0288955640119));
#34852=CARTESIAN_POINT('Ctrl Pts',(-0.340914050550457,2.29720177395537,
11.0299395916645));
#34853=CARTESIAN_POINT('Ctrl Pts',(-0.350786377080374,2.2790424251318,11.0309836193171));
#34854=CARTESIAN_POINT('Ctrl Pts',(-0.359161536257712,2.26027439244309,
11.0320276469697));
#34855=CARTESIAN_POINT('Ctrl Pts',(-0.362123720279164,2.25363638528795,
11.0323969058655));
#34856=CARTESIAN_POINT('Ctrl Pts',(-0.364899062387056,2.24692240656288,
11.0327661647614));
#34857=CARTESIAN_POINT('Ctrl Pts',(-0.367484084415039,2.24014398917414,
11.0331354236572));
#34858=CARTESIAN_POINT('Ctrl Pts',(-0.375941032129185,2.21796827042949,
11.034343461013));
#34859=CARTESIAN_POINT('Ctrl Pts',(-0.382399795014722,2.19499045153081,
11.0355514983688));
#34860=CARTESIAN_POINT('Ctrl Pts',(-0.386735574710299,2.17155756601153,
11.0367595357245));
#34861=CARTESIAN_POINT('Ctrl Pts',(-0.391071354405876,2.14812468049226,
11.0379675730803));
#34862=CARTESIAN_POINT('Ctrl Pts',(-0.393283864787408,2.12423703226915,
11.0391756104361));
#34863=CARTESIAN_POINT('Ctrl Pts',(-0.393299911892188,2.10026325956174,
11.0403836477918));
#34864=CARTESIAN_POINT('',(-0.393299891708519,2.09970814032956,11.165383647801));
#34865=CARTESIAN_POINT('Ctrl Pts',(-0.39329991189225,2.1002632594691,11.0403836477965));
#34866=CARTESIAN_POINT('Ctrl Pts',(-0.39331388416996,2.07938919324474,11.0414354910785));
#34867=CARTESIAN_POINT('Ctrl Pts',(-0.391661618617504,2.0585053384122,11.0424873343604));
#34868=CARTESIAN_POINT('Ctrl Pts',(-0.388365281852791,2.03789285184939,
11.0435391776424));
#34869=CARTESIAN_POINT('Ctrl Pts',(-0.385083289625895,2.01737006382592,
11.0445864436597));
#34870=CARTESIAN_POINT('Ctrl Pts',(-0.380171680434979,1.99711699783367,
11.045633709677));
#34871=CARTESIAN_POINT('Ctrl Pts',(-0.373703802948097,1.97740164086689,
11.0466809756944));
#34872=CARTESIAN_POINT('Ctrl Pts',(-0.36719352192696,1.95755702962525,11.0477351076086));
#34873=CARTESIAN_POINT('Ctrl Pts',(-0.359106746809468,1.93825789928112,
11.0487892395229));
#34874=CARTESIAN_POINT('Ctrl Pts',(-0.349567488074763,1.91975721573084,
11.0498433714372));
#34875=CARTESIAN_POINT('Ctrl Pts',(-0.340028229340057,1.90125653218055,
11.0508975033515));
#34876=CARTESIAN_POINT('Ctrl Pts',(-0.329036932527729,1.8835548881979,11.0519516352657));
#34877=CARTESIAN_POINT('Ctrl Pts',(-0.316761350199374,1.86687527582886,
11.05300576718));
#34878=CARTESIAN_POINT('Ctrl Pts',(-0.304604191067691,1.85035657256891,
11.0540497298276));
#34879=CARTESIAN_POINT('Ctrl Pts',(-0.291115185860461,1.83474218185906,
11.0550936924751));
#34880=CARTESIAN_POINT('Ctrl Pts',(-0.276453987570692,1.82025353843835,
11.0561376551227));
#34881=CARTESIAN_POINT('Ctrl Pts',(-0.261819760135011,1.80579154843846,
11.0571796972884));
#34882=CARTESIAN_POINT('Ctrl Pts',(-0.246018095568352,1.79245174865092,
11.0582217394542));
#34883=CARTESIAN_POINT('Ctrl Pts',(-0.229248319187245,1.78042199989702,
11.05926378162));
#34884=CARTESIAN_POINT('Ctrl Pts',(-0.212496553282527,1.76840517090429,
11.0603047046488));
#34885=CARTESIAN_POINT('Ctrl Pts',(-0.194779317661103,1.75769604996397,
11.0613456276777));
#34886=CARTESIAN_POINT('Ctrl Pts',(-0.17632820866795,1.7484416793362,11.0623865507065));
#34887=CARTESIAN_POINT('Ctrl Pts',(-0.157867623666118,1.73918255590487,
11.0634280083263));
#34888=CARTESIAN_POINT('Ctrl Pts',(-0.138673062795551,1.73138001964964,
11.0644694659461));
#34889=CARTESIAN_POINT('Ctrl Pts',(-0.119000310322095,1.725134936086,11.0655109235659));
#34890=CARTESIAN_POINT('Ctrl Pts',(-0.0993215469651018,1.71888794437708,
11.0665526993964));
#34891=CARTESIAN_POINT('Ctrl Pts',(-0.0791650127848176,1.71419954065486,
11.0675944752269));
#34892=CARTESIAN_POINT('Ctrl Pts',(-0.0588002884634068,1.7111203064229,
11.0686362510574));
#34893=CARTESIAN_POINT('Ctrl Pts',(-0.0383915453282304,1.70803441635627,
11.06968027871));
#34894=CARTESIAN_POINT('Ctrl Pts',(-0.0177744482470587,1.70656469231682,
11.0707243063626));
#34895=CARTESIAN_POINT('Ctrl Pts',(0.00277698199232742,1.70670980387122,
11.0717683340152));
#34896=CARTESIAN_POINT('Ctrl Pts',(0.0100457534851455,1.70676112792593,
11.0721375929111));
#34897=CARTESIAN_POINT('Ctrl Pts',(0.0173063387704855,1.70701398253939,
11.072506851807));
#34898=CARTESIAN_POINT('Ctrl Pts',(0.0245467996603237,1.70746675984519,
11.0728761107028));
#34899=CARTESIAN_POINT('Ctrl Pts',(0.0450169110224329,1.70874684436091,
11.0739200733504));
#34900=CARTESIAN_POINT('Ctrl Pts',(0.0654476125468863,1.71163628962611,
11.074964035998));
#34901=CARTESIAN_POINT('Ctrl Pts',(0.0855662948905743,1.71612072317107,
11.0760079986455));
#34902=CARTESIAN_POINT('Ctrl Pts',(0.105647966750178,1.72059690711731,11.0770500408113));
#34903=CARTESIAN_POINT('Ctrl Pts',(0.125418035800352,1.72666215494416,11.078092082977));
#34904=CARTESIAN_POINT('Ctrl Pts',(0.144610646903623,1.73425056281367,11.0791341251428));
#34905=CARTESIAN_POINT('Ctrl Pts',(0.163782645444069,1.74183082085234,11.0801750481717));
#34906=CARTESIAN_POINT('Ctrl Pts',(0.182377725842926,1.75093074911251,11.0812159712005));
#34907=CARTESIAN_POINT('Ctrl Pts',(0.20014688504895,1.76143521387303,11.0822568942294));
#34908=CARTESIAN_POINT('Ctrl Pts',(0.217925170032028,1.77194507345288,11.0832983518492));
#34909=CARTESIAN_POINT('Ctrl Pts',(0.234876044837998,1.78386055004182,11.084339809469));
#34910=CARTESIAN_POINT('Ctrl Pts',(0.250776239290656,1.79702117597556,11.0853812670887));
#34911=CARTESIAN_POINT('Ctrl Pts',(0.266681291945907,1.81018582305426,11.0864230429192));
#34912=CARTESIAN_POINT('Ctrl Pts',(0.281534481895788,1.82459588023449,11.0874648187497));
#34913=CARTESIAN_POINT('Ctrl Pts',(0.295147350412218,1.84005205993383,11.0885065945802));
#34914=CARTESIAN_POINT('Ctrl Pts',(0.308789643452868,1.85554164851633,11.0895506222328));
#34915=CARTESIAN_POINT('Ctrl Pts',(0.321185820917087,1.87208128469986,11.0905946498854));
#34916=CARTESIAN_POINT('Ctrl Pts',(0.33218866905337,1.88943984671227,11.091638677538));
#34917=CARTESIAN_POINT('Ctrl Pts',(0.336080232216586,1.89557934256437,11.0920079364339));
#34918=CARTESIAN_POINT('Ctrl Pts',(0.3397979135357,1.90182104743952,11.0923771953298));
#34919=CARTESIAN_POINT('Ctrl Pts',(0.343336602576712,1.90815405312835,11.0927464542256));
#34920=CARTESIAN_POINT('Ctrl Pts',(0.353341125748525,1.92605862214438,11.0937904168732));
#34921=CARTESIAN_POINT('Ctrl Pts',(0.361971136330359,1.9448012307163,11.0948343795207));
#34922=CARTESIAN_POINT('Ctrl Pts',(0.369091150588893,1.96414488394997,11.0958783421683));
#34923=CARTESIAN_POINT('Ctrl Pts',(0.376198066813973,1.98345295244912,11.0969203843341));
#34924=CARTESIAN_POINT('Ctrl Pts',(0.381800193445969,2.00335920871818,11.0979624264998));
#34925=CARTESIAN_POINT('Ctrl Pts',(0.385809031422191,2.0236044420593,11.0990044686656));
#34926=CARTESIAN_POINT('Ctrl Pts',(0.389813563969406,2.04382793233787,11.1000453916945));
#34927=CARTESIAN_POINT('Ctrl Pts',(0.392228034371326,2.06438896446323,11.1010863147233));
#34928=CARTESIAN_POINT('Ctrl Pts',(0.393014459271252,2.08501584824805,11.1021272377522));
#34929=CARTESIAN_POINT('Ctrl Pts',(0.393801288058509,2.10565332546277,11.103168695372));
#34930=CARTESIAN_POINT('Ctrl Pts',(0.392958356818582,2.12635598727122,11.1042101529918));
#34931=CARTESIAN_POINT('Ctrl Pts',(0.390499729456089,2.14684924006557,11.1052516106116));
#34932=CARTESIAN_POINT('Ctrl Pts',(0.388040350875748,2.16734875444209,11.1062933864421));
#34933=CARTESIAN_POINT('Ctrl Pts',(0.383964416895371,2.18763800681407,11.1073351622726));
#34934=CARTESIAN_POINT('Ctrl Pts',(0.378337475967636,2.20745065973943,11.1083769381031));
#34935=CARTESIAN_POINT('Ctrl Pts',(0.372698372279397,2.22730613816368,11.1094209657557));
#34936=CARTESIAN_POINT('Ctrl Pts',(0.365501824890359,2.24668227003993,11.1104649934083));
#34937=CARTESIAN_POINT('Ctrl Pts',(0.356862475660956,2.26533016501877,11.1115090210608));
#34938=CARTESIAN_POINT('Ctrl Pts',(0.353806851081012,2.2719256810407,11.1118782799567));
#34939=CARTESIAN_POINT('Ctrl Pts',(0.350571161940436,2.27843032168585,11.1122475388526));
#34940=CARTESIAN_POINT('Ctrl Pts',(0.347161813686725,2.28483388519896,11.1126167977484));
#34941=CARTESIAN_POINT('Ctrl Pts',(0.337522960650935,2.30293793413005,11.113660760396));
#34942=CARTESIAN_POINT('Ctrl Pts',(0.326435420451159,2.32033991421969,11.1147047230435));
#34943=CARTESIAN_POINT('Ctrl Pts',(0.314025122844744,2.33679761870075,11.1157486856911));
#34944=CARTESIAN_POINT('Ctrl Pts',(0.301637655318063,2.35322504746099,11.1167907278569));
#34945=CARTESIAN_POINT('Ctrl Pts',(0.287932651007697,2.36871103203746,11.1178327700226));
#34946=CARTESIAN_POINT('Ctrl Pts',(0.273080152767697,2.38304084539934,11.1188748121884));
#34947=CARTESIAN_POINT('Ctrl Pts',(0.258243605877466,2.3973552687668,11.1199157352173));
#34948=CARTESIAN_POINT('Ctrl Pts',(0.24226251838913,2.41051545691407,11.1209566582461));
#34949=CARTESIAN_POINT('Ctrl Pts',(0.225344771199342,2.42234240194724,11.121997581275));
#34950=CARTESIAN_POINT('Ctrl Pts',(0.208418335495539,2.43417542099113,11.1230390388948));
#34951=CARTESIAN_POINT('Ctrl Pts',(0.190554872867629,2.44467339422271,11.1240804965146));
#34952=CARTESIAN_POINT('Ctrl Pts',(0.17199287958319,2.45369950434328,11.1251219541343));
#34953=CARTESIAN_POINT('Ctrl Pts',(0.153425214800552,2.46272837233401,11.1261637299648));
#34954=CARTESIAN_POINT('Ctrl Pts',(0.134159271428605,2.4702841929787,11.1272055057953));
#34955=CARTESIAN_POINT('Ctrl Pts',(0.114454473319069,2.47627790732018,11.1282472816258));
#34956=CARTESIAN_POINT('Ctrl Pts',(0.0947070828412857,2.48228457721121,
11.1292913092784));
#34957=CARTESIAN_POINT('Ctrl Pts',(0.0745196631070063,2.48672224160587,
11.130335336931));
#34958=CARTESIAN_POINT('Ctrl Pts',(0.054163543288737,2.4895525645897,11.1313793645836));
#34959=CARTESIAN_POINT('Ctrl Pts',(0.0469638505320102,2.4905536127299,11.1317486234795));
#34960=CARTESIAN_POINT('Ctrl Pts',(0.039743095218919,2.49135406688011,11.1321178823754));
#34961=CARTESIAN_POINT('Ctrl Pts',(0.0325133225523991,2.49195379046082,
11.1324871412712));
#34962=CARTESIAN_POINT('Ctrl Pts',(0.0120734287579877,2.4936493190564,11.1335311039188));
#34963=CARTESIAN_POINT('Ctrl Pts',(-0.00856035352241005,2.49374672299721,
11.1345750665663));
#34964=CARTESIAN_POINT('Ctrl Pts',(-0.0291162044493577,2.49222077537844,
11.1356190292139));
#34965=CARTESIAN_POINT('Ctrl Pts',(-0.0496342406735042,2.49069763490475,
11.1366610713797));
#34966=CARTESIAN_POINT('Ctrl Pts',(-0.0700739002393444,2.48755706516615,
11.1377031135454));
#34967=CARTESIAN_POINT('Ctrl Pts',(-0.0901625895454327,2.48282580561721,
11.1387451557112));
#34968=CARTESIAN_POINT('Ctrl Pts',(-0.11022970391479,2.47809962736669,11.1397860787401));
#34969=CARTESIAN_POINT('Ctrl Pts',(-0.129945877151433,2.47178629050859,
11.1408270017689));
#34970=CARTESIAN_POINT('Ctrl Pts',(-0.149048066527609,2.46396368481537,
11.1418679247978));
#34971=CARTESIAN_POINT('Ctrl Pts',(-0.168160066290393,2.45613706163574,
11.1429093824176));
#34972=CARTESIAN_POINT('Ctrl Pts',(-0.186656765236036,2.44679988502048,
11.1439508400374));
#34973=CARTESIAN_POINT('Ctrl Pts',(-0.204294022591169,2.43607862522558,
11.1449922976571));
#34974=CARTESIAN_POINT('Ctrl Pts',(-0.221936668897339,2.42535408961841,
11.1460340734876));
#34975=CARTESIAN_POINT('Ctrl Pts',(-0.238718741438448,2.41324504172642,
11.1470758493181));
#34976=CARTESIAN_POINT('Ctrl Pts',(-0.254424927030318,2.39992140054624,
11.1481176251486));
#34977=CARTESIAN_POINT('Ctrl Pts',(-0.270165061898765,2.38656896001329,
11.1491616528012));
#34978=CARTESIAN_POINT('Ctrl Pts',(-0.284824144641143,2.37199720397771,
11.1502056804538));
#34979=CARTESIAN_POINT('Ctrl Pts',(-0.29822306635052,2.35641351894253,11.1512497081064));
#34980=CARTESIAN_POINT('Ctrl Pts',(-0.302962089329329,2.35090177381274,
11.1516189670023));
#34981=CARTESIAN_POINT('Ctrl Pts',(-0.307543850832177,2.34526373375715,
11.1519882258981));
#34982=CARTESIAN_POINT('Ctrl Pts',(-0.311961715734576,2.33950945266511,
11.152357484794));
#34983=CARTESIAN_POINT('Ctrl Pts',(-0.324948951561612,2.32259354255731,
11.1534429983775));
#34984=CARTESIAN_POINT('Ctrl Pts',(-0.336597542900089,2.30456456151901,
11.1545285119611));
#34985=CARTESIAN_POINT('Ctrl Pts',(-0.346718674991621,2.28566381018404,
11.1556140255446));
#34986=CARTESIAN_POINT('Ctrl Pts',(-0.356448637914021,2.267493549384,11.156657585378));
#34987=CARTESIAN_POINT('Ctrl Pts',(-0.364766744947935,2.24851841758935,
11.1577011452115));
#34988=CARTESIAN_POINT('Ctrl Pts',(-0.371548357285401,2.22898336403785,
11.1587447050449));
#34989=CARTESIAN_POINT('Ctrl Pts',(-0.378321739649224,2.20947201767689,
11.1597869984435));
#34990=CARTESIAN_POINT('Ctrl Pts',(-0.383562061465708,2.18940277634239,
11.1608292918422));
#34991=CARTESIAN_POINT('Ctrl Pts',(-0.387192915306281,2.16904010672517,
11.1618715852408));
#34992=CARTESIAN_POINT('Ctrl Pts',(-0.390822952250089,2.14868201845429,
11.1629136441364));
#34993=CARTESIAN_POINT('Ctrl Pts',(-0.392844102813498,2.12803135043112,
11.1639557030321));
#34994=CARTESIAN_POINT('Ctrl Pts',(-0.393231083751943,2.10736238896501,
11.1649977619277));
#34995=CARTESIAN_POINT('Ctrl Pts',(-0.393278851517683,2.10481107438773,
11.1651263905506));
#34996=CARTESIAN_POINT('Ctrl Pts',(-0.393301785008165,2.10225948554673,
11.1652550191736));
#34997=CARTESIAN_POINT('Ctrl Pts',(-0.393299891708585,2.09970814041908,
11.1653836477965));
#34998=CARTESIAN_POINT('',(-0.393441883900895,2.09987214517031,11.2903836477965));
#34999=CARTESIAN_POINT('Ctrl Pts',(-0.393299891708519,2.09970814032956,
11.165383647801));
#35000=CARTESIAN_POINT('Ctrl Pts',(-0.393282117129534,2.07575573889103,
11.1665912321375));
#35001=CARTESIAN_POINT('Ctrl Pts',(-0.391072133920177,2.05189347906682,
11.1677988164739));
#35002=CARTESIAN_POINT('Ctrl Pts',(-0.386743192868008,2.02848361886771,
11.1690064008103));
#35003=CARTESIAN_POINT('Ctrl Pts',(-0.382893808230515,2.0076670831075,11.1700802099791));
#35004=CARTESIAN_POINT('Ctrl Pts',(-0.377369766906101,1.98720811105829,
11.1711540191479));
#35005=CARTESIAN_POINT('Ctrl Pts',(-0.370254349587689,1.96734779831681,
11.1722278283167));
#35006=CARTESIAN_POINT('Ctrl Pts',(-0.363336705263321,1.94803950288335,
11.1732717909643));
#35007=CARTESIAN_POINT('Ctrl Pts',(-0.35488402826661,1.92921625368693,11.1743157536118));
#35008=CARTESIAN_POINT('Ctrl Pts',(-0.344985874235674,1.91113593095073,
11.1753597162594));
#35009=CARTESIAN_POINT('Ctrl Pts',(-0.335105928925666,1.89308886891648,
11.1764017584251));
#35010=CARTESIAN_POINT('Ctrl Pts',(-0.32378608197909,1.8757826871725,11.1774438005909));
#35011=CARTESIAN_POINT('Ctrl Pts',(-0.31116351430148,1.85945445884916,11.1784858427567));
#35012=CARTESIAN_POINT('Ctrl Pts',(-0.298554503063261,1.84314376678652,
11.1795267657855));
#35013=CARTESIAN_POINT('Ctrl Pts',(-0.284645973490244,1.82780953989057,
11.1805676888144));
#35014=CARTESIAN_POINT('Ctrl Pts',(-0.269617715035238,1.81365898348442,
11.1816086118432));
#35015=CARTESIAN_POINT('Ctrl Pts',(-0.254581738458369,1.7995011597213,11.182650069463));
#35016=CARTESIAN_POINT('Ctrl Pts',(-0.238425408781422,1.78652873703318,
11.1836915270828));
#35017=CARTESIAN_POINT('Ctrl Pts',(-0.221364913809522,1.77491160443027,
11.1847329847026));
#35018=CARTESIAN_POINT('Ctrl Pts',(-0.204299206112636,1.76329092228688,
11.1857747605331));
#35019=CARTESIAN_POINT('Ctrl Pts',(-0.186329411169498,1.75302673847489,
11.1868165363636));
#35020=CARTESIAN_POINT('Ctrl Pts',(-0.167699335001218,1.74424471467011,
11.1878583121941));
#35021=CARTESIAN_POINT('Ctrl Pts',(-0.149028989500528,1.73544370832159,
11.1889023398467));
#35022=CARTESIAN_POINT('Ctrl Pts',(-0.129696202265947,1.72813151859826,
11.1899463674993));
#35023=CARTESIAN_POINT('Ctrl Pts',(-0.10996389924166,1.72238534077241,11.1909903951519));
#35024=CARTESIAN_POINT('Ctrl Pts',(-0.10298484230805,1.72035299299486,11.1913596540478));
#35025=CARTESIAN_POINT('Ctrl Pts',(-0.0959559174314416,1.71851608003603,
11.1917289129437));
#35026=CARTESIAN_POINT('Ctrl Pts',(-0.0888890232722175,1.7168764800463,
11.1920981718396));
#35027=CARTESIAN_POINT('Ctrl Pts',(-0.0689096169019349,1.7122410300535,
11.1931421344871));
#35028=CARTESIAN_POINT('Ctrl Pts',(-0.0485071051703846,1.70915882730775,
11.1941860971347));
#35029=CARTESIAN_POINT('Ctrl Pts',(-0.0279467964714988,1.70769416704951,
11.1952300597822));
#35030=CARTESIAN_POINT('Ctrl Pts',(-0.00742431067596596,1.70623220119164,
11.196272101948));
#35031=CARTESIAN_POINT('Ctrl Pts',(0.0132546744797402,1.70638198229833,
11.1973141441138));
#35032=CARTESIAN_POINT('Ctrl Pts',(0.033816565160104,1.70815649817718,11.1983561862795));
#35033=CARTESIAN_POINT('Ctrl Pts',(0.0543563726929092,1.70992910825385,
11.1993971093084));
#35034=CARTESIAN_POINT('Ctrl Pts',(0.0747786035859954,1.71332295485183,
11.2004380323372));
#35035=CARTESIAN_POINT('Ctrl Pts',(0.0948117126143965,1.71829903176554,
11.2014789553661));
#35036=CARTESIAN_POINT('Ctrl Pts',(0.114855110125461,1.72327766426266,11.2025204129859));
#35037=CARTESIAN_POINT('Ctrl Pts',(0.13450826856536,1.7298399887263,11.2035618706057));
#35038=CARTESIAN_POINT('Ctrl Pts',(0.153511315847371,1.73789619457011,11.2046033282255));
#35039=CARTESIAN_POINT('Ctrl Pts',(0.172520169388787,1.74595486193603,11.205645104056));
#35040=CARTESIAN_POINT('Ctrl Pts',(0.19087785360811,1.75550799910288,11.2066868798864));
#35041=CARTESIAN_POINT('Ctrl Pts',(0.208346733313902,1.76641863253859,11.2077286557169));
#35042=CARTESIAN_POINT('Ctrl Pts',(0.225853372399599,1.77735284955607,11.2087726833695));
#35043=CARTESIAN_POINT('Ctrl Pts',(0.242466779490609,1.78964998278444,11.2098167110221));
#35044=CARTESIAN_POINT('Ctrl Pts',(0.257979720855493,1.80313074657802,11.2108607386747));
#35045=CARTESIAN_POINT('Ctrl Pts',(0.263466444876461,1.8078987160293,11.2112299975706));
#35046=CARTESIAN_POINT('Ctrl Pts',(0.268815838221317,1.81281440773856,11.2115992564665));
#35047=CARTESIAN_POINT('Ctrl Pts',(0.274019880747731,1.81786883377585,11.2119685153623));
#35048=CARTESIAN_POINT('Ctrl Pts',(0.288732663769763,1.83215862353258,11.2130124780099));
#35049=CARTESIAN_POINT('Ctrl Pts',(0.302368483273617,1.84764496865274,11.2140564406574));
#35050=CARTESIAN_POINT('Ctrl Pts',(0.3147296624425,1.86413959726391,11.215100403305));
#35051=CARTESIAN_POINT('Ctrl Pts',(0.327068101890308,1.88060388222836,11.2161424454707));
#35052=CARTESIAN_POINT('Ctrl Pts',(0.338136071564399,1.8980722224112,11.2171844876365));
#35053=CARTESIAN_POINT('Ctrl Pts',(0.347774549796921,1.91632160575193,11.2182265298023));
#35054=CARTESIAN_POINT('Ctrl Pts',(0.357402676455242,1.93455138954165,11.2192674528311));
#35055=CARTESIAN_POINT('Ctrl Pts',(0.365603992059651,1.95355991741043,11.22030837586));
#35056=CARTESIAN_POINT('Ctrl Pts',(0.37226430138939,1.97309775450738,11.2213492988889));
#35057=CARTESIAN_POINT('Ctrl Pts',(0.378928031280413,1.99264562572825,11.2223907565087));
#35058=CARTESIAN_POINT('Ctrl Pts',(0.384048921150567,2.01272265802806,11.2234322141284));
#35059=CARTESIAN_POINT('Ctrl Pts',(0.387561811892712,2.0330617302103,11.2244736717482));
#35060=CARTESIAN_POINT('Ctrl Pts',(0.391075775976127,2.0534070168658,11.2255154475787));
#35061=CARTESIAN_POINT('Ctrl Pts',(0.392980673373426,2.07401377220309,11.2265572234092));
#35062=CARTESIAN_POINT('Ctrl Pts',(0.393263037659875,2.09460804205064,11.2275989992397));
#35063=CARTESIAN_POINT('Ctrl Pts',(0.393546012283137,2.11524682687982,11.2286430268923));
#35064=CARTESIAN_POINT('Ctrl Pts',(0.392199499935705,2.13587233742638,11.2296870545449));
#35065=CARTESIAN_POINT('Ctrl Pts',(0.389262067835153,2.15621327729906,11.2307310821975));
#35066=CARTESIAN_POINT('Ctrl Pts',(0.388223136604324,2.16340760110799,11.2311003410934));
#35067=CARTESIAN_POINT('Ctrl Pts',(0.386985658277728,2.17056641955304,11.2314695999893));
#35068=CARTESIAN_POINT('Ctrl Pts',(0.385552848619826,2.17767812382607,11.2318388588851));
#35069=CARTESIAN_POINT('Ctrl Pts',(0.381502032835427,2.19778421660975,11.2328828215327));
#35070=CARTESIAN_POINT('Ctrl Pts',(0.375862152065989,2.21763249622357,11.2339267841802));
#35071=CARTESIAN_POINT('Ctrl Pts',(0.368684502639998,2.23695483749433,11.2349707468278));
#35072=CARTESIAN_POINT('Ctrl Pts',(0.361520057273563,2.25624163323621,11.2360127889936));
#35073=CARTESIAN_POINT('Ctrl Pts',(0.352823656058063,2.27500370847721,11.2370548311593));
#35074=CARTESIAN_POINT('Ctrl Pts',(0.342696730224722,2.29298663449391,11.2380968733251));
#35075=CARTESIAN_POINT('Ctrl Pts',(0.332580680550633,2.31095024713056,11.239137796354));
#35076=CARTESIAN_POINT('Ctrl Pts',(0.321037490307621,2.32813571972793,11.2401787193828));
#35077=CARTESIAN_POINT('Ctrl Pts',(0.308215072847903,2.344312011308,11.2412196424117));
#35078=CARTESIAN_POINT('Ctrl Pts',(0.29538607012877,2.36049661060983,11.2422611000315));
#35079=CARTESIAN_POINT('Ctrl Pts',(0.281276972119512,2.37567040685188,11.2433025576513));
#35080=CARTESIAN_POINT('Ctrl Pts',(0.266077107302757,2.38963401555998,11.2443440152711));
#35081=CARTESIAN_POINT('Ctrl Pts',(0.25087259826464,2.4036018907593,11.2453857911015));
#35082=CARTESIAN_POINT('Ctrl Pts',(0.234577224806245,2.41635837160149,11.246427566932));
#35083=CARTESIAN_POINT('Ctrl Pts',(0.217414042880951,2.42774383893242,11.2474693427625));
#35084=CARTESIAN_POINT('Ctrl Pts',(0.200213762348447,2.43915391620935,11.2485133704151));
#35085=CARTESIAN_POINT('Ctrl Pts',(0.182142572330235,2.44918670605734,11.2495573980677));
#35086=CARTESIAN_POINT('Ctrl Pts',(0.163449460821231,2.45772777884482,11.2506014257203));
#35087=CARTESIAN_POINT('Ctrl Pts',(0.156837952305214,2.46074864433547,11.2509706846162));
#35088=CARTESIAN_POINT('Ctrl Pts',(0.150148820204391,2.46358334817812,11.2513399435121));
#35089=CARTESIAN_POINT('Ctrl Pts',(0.143393566163912,2.46622831018751,11.2517092024079));
#35090=CARTESIAN_POINT('Ctrl Pts',(0.124295223586484,2.47370610306648,11.2527531650555));
#35091=CARTESIAN_POINT('Ctrl Pts',(0.104553465349265,2.47970822272757,11.253797127703));
#35092=CARTESIAN_POINT('Ctrl Pts',(0.084421503527998,2.48413265904121,11.2548410903506));
#35093=CARTESIAN_POINT('Ctrl Pts',(0.0643265766198458,2.4885489561275,11.2558831325164));
#35094=CARTESIAN_POINT('Ctrl Pts',(0.0438435687218423,2.49139311661894,
11.2569251746821));
#35095=CARTESIAN_POINT('Ctrl Pts',(0.0232413146182522,2.49261269884559,
11.2579672168479));
#35096=CARTESIAN_POINT('Ctrl Pts',(0.00266118701191055,2.49383097126008,
11.2590081398768));
#35097=CARTESIAN_POINT('Ctrl Pts',(-0.0180372034940253,2.49342805706877,
11.2600490629056));
#35098=CARTESIAN_POINT('Ctrl Pts',(-0.0385795253384346,2.49140325781048,
11.2610899859345));
#35099=CARTESIAN_POINT('Ctrl Pts',(-0.059132397183938,2.48937741866807,
11.2621314435543));
#35100=CARTESIAN_POINT('Ctrl Pts',(-0.0795283064293706,2.48572808652609,
11.2631729011741));
#35101=CARTESIAN_POINT('Ctrl Pts',(-0.0994971201104013,2.48050652174403,
11.2642143587939));
#35102=CARTESIAN_POINT('Ctrl Pts',(-0.119472035134574,2.47528336154628,
11.2652561346244));
#35103=CARTESIAN_POINT('Ctrl Pts',(-0.139018892715362,2.46848723335869,
11.2662979104549));
#35104=CARTESIAN_POINT('Ctrl Pts',(-0.157882737992171,2.46021928188826,
11.2673396862854));
#35105=CARTESIAN_POINT('Ctrl Pts',(-0.176787357898624,2.45193345905311,
11.268383713938));
#35106=CARTESIAN_POINT('Ctrl Pts',(-0.195005368916282,2.44216980935798,
11.2694277415906));
#35107=CARTESIAN_POINT('Ctrl Pts',(-0.212305774861567,2.4310757435398,11.2704717692432));
#35108=CARTESIAN_POINT('Ctrl Pts',(-0.218424701674887,2.42715191787823,
11.270841028139));
#35109=CARTESIAN_POINT('Ctrl Pts',(-0.224429119490491,2.42306205225298,
11.2712102870349));
#35110=CARTESIAN_POINT('Ctrl Pts',(-0.230309791976158,2.41881387943422,
11.2715795459307));
#35111=CARTESIAN_POINT('Ctrl Pts',(-0.246801243074373,2.4069005252272,11.2726150763124));
#35112=CARTESIAN_POINT('Ctrl Pts',(-0.262418861882085,2.39366574277209,
11.2736506066941));
#35113=CARTESIAN_POINT('Ctrl Pts',(-0.276941775913723,2.37926357219257,
11.2746861370758));
#35114=CARTESIAN_POINT('Ctrl Pts',(-0.291437973362016,2.36488789607482,
11.2757197624794));
#35115=CARTESIAN_POINT('Ctrl Pts',(-0.304842892466673,2.34934956990205,
11.2767533878829));
#35116=CARTESIAN_POINT('Ctrl Pts',(-0.316968640225888,2.33284280343904,
11.2777870132865));
#35117=CARTESIAN_POINT('Ctrl Pts',(-0.329283192815779,2.31607901717742,
11.278836732829));
#35118=CARTESIAN_POINT('Ctrl Pts',(-0.340277802284048,2.29831690485719,
11.2798864523715));
#35119=CARTESIAN_POINT('Ctrl Pts',(-0.349797924201985,2.27979516740998,
11.280936171914));
#35120=CARTESIAN_POINT('Ctrl Pts',(-0.359166996768876,2.26156730187384,
11.2819692362648));
#35121=CARTESIAN_POINT('Ctrl Pts',(-0.367107770865079,2.24260447085751,
11.2830023006156));
#35122=CARTESIAN_POINT('Ctrl Pts',(-0.373519603111344,2.22315841867913,
11.2840353649664));
#35123=CARTESIAN_POINT('Ctrl Pts',(-0.380086493890814,2.20324209899973,
11.2850934121047));
#35124=CARTESIAN_POINT('Ctrl Pts',(-0.385049188178705,2.18281963576225,
11.2861514592431));
#35125=CARTESIAN_POINT('Ctrl Pts',(-0.388354250310891,2.1621760907863,11.2872095063814));
#35126=CARTESIAN_POINT('Ctrl Pts',(-0.391659312443079,2.14153254581033,
11.2882675535198));
#35127=CARTESIAN_POINT('Ctrl Pts',(-0.393306737388483,2.12066875645485,
11.2893256006581));
#35128=CARTESIAN_POINT('Ctrl Pts',(-0.393299979233323,2.09987219128435,
11.2903836477965));
#35129=CARTESIAN_POINT('',(-0.393299833502872,2.10036189309685,11.4153836477965));
#35130=CARTESIAN_POINT('Ctrl Pts',(-0.393899443331936,2.09987199647952,
11.2903836477965));
#35131=CARTESIAN_POINT('Ctrl Pts',(-0.393929117802885,2.09287546046937,
11.2907390616822));
#35132=CARTESIAN_POINT('Ctrl Pts',(-0.39375888735456,2.08588039805356,11.2910944755679));
#35133=CARTESIAN_POINT('Ctrl Pts',(-0.386401867339676,1.94874160309987,
11.2980733372944));
#35134=CARTESIAN_POINT('Ctrl Pts',(-0.230433513831742,1.69605020585767,
11.3113202329764));
#35135=CARTESIAN_POINT('Ctrl Pts',(0.214910394680641,1.68758205332127,11.3311905764991));
#35136=CARTESIAN_POINT('Ctrl Pts',(0.463103273481829,2.05745122122909,11.3510609200219));
#35137=CARTESIAN_POINT('Ctrl Pts',(0.286461944681156,2.46635310116605,11.3709312635446));
#35138=CARTESIAN_POINT('Ctrl Pts',(-0.152969220092249,2.53917588525426,
11.3908016070675));
#35139=CARTESIAN_POINT('Ctrl Pts',(-0.376012290477261,2.29304678368391,
11.4056190660244));
#35140=CARTESIAN_POINT('Ctrl Pts',(-0.393569766291279,2.13140534042234,
11.4138130771406));
#35141=CARTESIAN_POINT('Ctrl Pts',(-0.393284377485805,2.10036202476101,
11.4153836404157));
#35142=CARTESIAN_POINT('',(-0.39306000785858,2.09993937222327,11.5403836637865));
#35143=CARTESIAN_POINT('Ctrl Pts',(-0.393299833502872,2.10036189309685,
11.4153836477965));
#35144=CARTESIAN_POINT('Ctrl Pts',(-0.393318545155974,2.08002635723286,
11.4164124453626));
#35145=CARTESIAN_POINT('Ctrl Pts',(-0.39175578397594,2.05964716809563,11.4174412429287));
#35146=CARTESIAN_POINT('Ctrl Pts',(-0.388617730630256,2.03949256706991,
11.4184700404948));
#35147=CARTESIAN_POINT('Ctrl Pts',(-0.385479911390416,2.0193394696228,11.4194987613102));
#35148=CARTESIAN_POINT('Ctrl Pts',(-0.380767098308162,1.99941168018583,
11.4205274821257));
#35149=CARTESIAN_POINT('Ctrl Pts',(-0.374537338097605,1.97997220167494,
11.4215562029412));
#35150=CARTESIAN_POINT('Ctrl Pts',(-0.368308813458114,1.96053657866674,
11.4225847197267));
#35151=CARTESIAN_POINT('Ctrl Pts',(-0.360564182220411,1.94158979100163,
11.4236132365122));
#35152=CARTESIAN_POINT('Ctrl Pts',(-0.351411029419831,1.92337843166223,
11.4246417532978));
#35153=CARTESIAN_POINT('Ctrl Pts',(-0.342236955454333,1.90512544700962,
11.425672620942));
#35154=CARTESIAN_POINT('Ctrl Pts',(-0.331648297244273,1.88761191302799,
11.4267034885863));
#35155=CARTESIAN_POINT('Ctrl Pts',(-0.319798523303929,1.87105940837714,
11.4277343562306));
#35156=CARTESIAN_POINT('Ctrl Pts',(-0.309039486379814,1.85603051334321,
11.4286703355247));
#35157=CARTESIAN_POINT('Ctrl Pts',(-0.297241658399242,1.84179382727624,
11.4296063148189));
#35158=CARTESIAN_POINT('Ctrl Pts',(-0.284547292283978,1.82848991095384,
11.430542294113));
#35159=CARTESIAN_POINT('Ctrl Pts',(-0.270388384986038,1.81365113001762,
11.4315862567606));
#35160=CARTESIAN_POINT('Ctrl Pts',(-0.255023429813726,1.79987867158512,
11.4326302194081));
#35161=CARTESIAN_POINT('Ctrl Pts',(-0.238638940285526,1.78737187237966,
11.4336741820557));
#35162=CARTESIAN_POINT('Ctrl Pts',(-0.222284591791345,1.77488808077901,
11.4347162242214));
#35163=CARTESIAN_POINT('Ctrl Pts',(-0.204914973989729,1.76366581546066,
11.4357582663872));
#35164=CARTESIAN_POINT('Ctrl Pts',(-0.186751681621276,1.75386606723462,
11.436800308553));
#35165=CARTESIAN_POINT('Ctrl Pts',(-0.168607896343485,1.74407684378423,
11.4378412315818));
#35166=CARTESIAN_POINT('Ctrl Pts',(-0.149672759229649,1.73570747750828,
11.4388821546107));
#35167=CARTESIAN_POINT('Ctrl Pts',(-0.130194683834731,1.72887436857423,
11.4399230776396));
#35168=CARTESIAN_POINT('Ctrl Pts',(-0.11070660500795,1.72203775033353,11.4409645352593));
#35169=CARTESIAN_POINT('Ctrl Pts',(-0.0906757198006848,1.71673922442125,
11.4420059928791));
#35170=CARTESIAN_POINT('Ctrl Pts',(-0.070368561768369,1.71304631347582,
11.4430474504989));
#35171=CARTESIAN_POINT('Ctrl Pts',(-0.050055199013961,1.70935227418511,
11.4440892263294));
#35172=CARTESIAN_POINT('Ctrl Pts',(-0.029466125156578,1.70726492243702,
11.4451310021599));
#35173=CARTESIAN_POINT('Ctrl Pts',(-0.00887516433844985,1.70680015074015,
11.4461727779904));
#35174=CARTESIAN_POINT('Ctrl Pts',(0.0117603043087581,1.70633437442872,
11.447216805643));
#35175=CARTESIAN_POINT('Ctrl Pts',(0.0323969327501948,1.70749813874247,
11.4482608332956));
#35176=CARTESIAN_POINT('Ctrl Pts',(0.0527630936196593,1.71025528104709,
11.4493048609482));
#35177=CARTESIAN_POINT('Ctrl Pts',(0.0599663377646051,1.7112304461403,11.4496741198441));
#35178=CARTESIAN_POINT('Ctrl Pts',(0.0671358366151855,1.71240446503712,
11.45004337874));
#35179=CARTESIAN_POINT('Ctrl Pts',(0.0742599533342948,1.71377422492694,
11.4504126376358));
#35180=CARTESIAN_POINT('Ctrl Pts',(0.0944011383803014,1.71764678744903,
11.4514566002834));
#35181=CARTESIAN_POINT('Ctrl Pts',(0.11429859587963,1.72311063625593,11.4525005629309));
#35182=CARTESIAN_POINT('Ctrl Pts',(0.133683756808683,1.73011685201199,11.4535445255785));
#35183=CARTESIAN_POINT('Ctrl Pts',(0.153033256645336,1.73711017907921,11.4545865677443));
#35184=CARTESIAN_POINT('Ctrl Pts',(0.171871626217857,1.74564004972883,11.45562860991));
#35185=CARTESIAN_POINT('Ctrl Pts',(0.189943548333678,1.75560729036983,11.4566706520758));
#35186=CARTESIAN_POINT('Ctrl Pts',(0.20799606148904,1.76556382635095,11.4577115751047));
#35187=CARTESIAN_POINT('Ctrl Pts',(0.225283106358137,1.77695433946821,11.4587524981335));
#35188=CARTESIAN_POINT('Ctrl Pts',(0.241572340850244,1.78963296867075,11.4597934211624));
#35189=CARTESIAN_POINT('Ctrl Pts',(0.257869941068643,1.80231810928681,11.4608348787822));
#35190=CARTESIAN_POINT('Ctrl Pts',(0.273168116620351,1.81629224839513,11.461876336402));
#35191=CARTESIAN_POINT('Ctrl Pts',(0.287265813832512,1.83136783103443,11.4629177940217));
#35192=CARTESIAN_POINT('Ctrl Pts',(0.301367818505782,1.84644801992148,11.4639595698522));
#35193=CARTESIAN_POINT('Ctrl Pts',(0.314268138928285,1.86262976063816,11.4650013456827));
#35194=CARTESIAN_POINT('Ctrl Pts',(0.325805186438368,1.87969141984512,11.4660431215132));
#35195=CARTESIAN_POINT('Ctrl Pts',(0.33736717153845,1.89678995821562,11.4670871491658));
#35196=CARTESIAN_POINT('Ctrl Pts',(0.347559637522531,1.91477157154622,11.4681311768184));
#35197=CARTESIAN_POINT('Ctrl Pts',(0.356265953779684,1.93338829519673,11.469175204471));
#35198=CARTESIAN_POINT('Ctrl Pts',(0.359345263719599,1.9399727863285,11.4695444633669));
#35199=CARTESIAN_POINT('Ctrl Pts',(0.362239106883503,1.94663654696954,11.4699137222628));
#35200=CARTESIAN_POINT('Ctrl Pts',(0.364943801348106,1.95336810763823,11.4702829811586));
#35201=CARTESIAN_POINT('Ctrl Pts',(0.372590468837211,1.9723994647064,11.4713269438062));
#35202=CARTESIAN_POINT('Ctrl Pts',(0.378767220202153,1.99208728330822,11.4723709064537));
#35203=CARTESIAN_POINT('Ctrl Pts',(0.383369806431004,2.01217926487979,11.4734148691013));
#35204=CARTESIAN_POINT('Ctrl Pts',(0.38796392570653,2.03223428508622,11.4744569112671));
#35205=CARTESIAN_POINT('Ctrl Pts',(0.390989407579595,2.05269129661982,11.4754989534328));
#35206=CARTESIAN_POINT('Ctrl Pts',(0.392391431171545,2.07328193975703,11.4765409955986));
#35207=CARTESIAN_POINT('Ctrl Pts',(0.393791949012181,2.09385046886697,11.4775819186275));
#35208=CARTESIAN_POINT('Ctrl Pts',(0.393572391387792,2.1145516162707,11.4786228416563));
#35209=CARTESIAN_POINT('Ctrl Pts',(0.391729629909612,2.13511106735601,11.4796637646852));
#35210=CARTESIAN_POINT('Ctrl Pts',(0.389885922037165,2.15568107723956,11.480705222305));
#35211=CARTESIAN_POINT('Ctrl Pts',(0.386417394523157,2.17610851114386,11.4817466799248));
#35212=CARTESIAN_POINT('Ctrl Pts',(0.38137291295117,2.19612279265158,11.4827881375445));
#35213=CARTESIAN_POINT('Ctrl Pts',(0.376326890070137,2.21614318939487,11.4838299133751));
#35214=CARTESIAN_POINT('Ctrl Pts',(0.369704169290134,2.23574947841387,11.4848716892055));
#35215=CARTESIAN_POINT('Ctrl Pts',(0.361603633028839,2.25468581893743,11.485913465036));
#35216=CARTESIAN_POINT('Ctrl Pts',(0.353485587274598,2.27366309079075,11.4869574926886));
#35217=CARTESIAN_POINT('Ctrl Pts',(0.343883690839864,2.29196687088298,11.4880015203412));
#35218=CARTESIAN_POINT('Ctrl Pts',(0.332943302576687,2.30936486636809,11.4890455479938));
#35219=CARTESIAN_POINT('Ctrl Pts',(0.329073830651941,2.3155183093225,11.4894148068897));
#35220=CARTESIAN_POINT('Ctrl Pts',(0.32503731098751,2.32155871850864,11.4897840657856));
#35221=CARTESIAN_POINT('Ctrl Pts',(0.320841394237289,2.32747678946185,11.4901533246814));
#35222=CARTESIAN_POINT('Ctrl Pts',(0.308978767748014,2.34420826185136,11.491197287329));
#35223=CARTESIAN_POINT('Ctrl Pts',(0.295768484490001,2.36005915693541,11.4922412499765));
#35224=CARTESIAN_POINT('Ctrl Pts',(0.281366249739214,2.37480524650685,11.4932852126241));
#35225=CARTESIAN_POINT('Ctrl Pts',(0.266990509451176,2.38952420905755,11.4943272547899));
#35226=CARTESIAN_POINT('Ctrl Pts',(0.251427635888406,2.4031418383637,11.4953692969556));
#35227=CARTESIAN_POINT('Ctrl Pts',(0.234873595179144,2.41546677208166,11.4964113391214));
#35228=CARTESIAN_POINT('Ctrl Pts',(0.218337333249554,2.42777846901443,11.4974522621503));
#35229=CARTESIAN_POINT('Ctrl Pts',(0.200812587361982,2.43879976616843,11.4984931851791));
#35230=CARTESIAN_POINT('Ctrl Pts',(0.182528312700421,2.44837954168225,11.499534108208));
#35231=CARTESIAN_POINT('Ctrl Pts',(0.164234647711941,2.4579642371191,11.5005755658278));
#35232=CARTESIAN_POINT('Ctrl Pts',(0.145181318928943,2.46610557615619,11.5016170234476));
#35233=CARTESIAN_POINT('Ctrl Pts',(0.125622283670958,2.47269817794738,11.5026584810673));
#35234=CARTESIAN_POINT('Ctrl Pts',(0.106057272275004,2.47929279406582,11.5037002568978));
#35235=CARTESIAN_POINT('Ctrl Pts',(0.0859869550061474,2.4843375303674,11.5047420327283));
#35236=CARTESIAN_POINT('Ctrl Pts',(0.0656799742048062,2.48777703772717,
11.5057838085588));
#35237=CARTESIAN_POINT('Ctrl Pts',(0.0453290994036211,2.49122397966014,
11.5068278362114));
#35238=CARTESIAN_POINT('Ctrl Pts',(0.024741273348776,2.49305870011403,11.507871863864));
#35239=CARTESIAN_POINT('Ctrl Pts',(0.00419049739736034,2.49327767509937,
11.5089158915166));
#35240=CARTESIAN_POINT('Ctrl Pts',(-0.00307804268214043,2.49335512368141,
11.5092851504125));
#35241=CARTESIAN_POINT('Ctrl Pts',(-0.010341967905338,2.49323092831189,
11.5096544093084));
#35242=CARTESIAN_POINT('Ctrl Pts',(-0.01758931347456,2.49290648512272,11.5100236682042));
#35243=CARTESIAN_POINT('Ctrl Pts',(-0.0380788890890574,2.49198922470049,
11.5110676308518));
#35244=CARTESIAN_POINT('Ctrl Pts',(-0.0585575704984534,2.48946215793166,
11.5121115934993));
#35245=CARTESIAN_POINT('Ctrl Pts',(-0.0787525365322312,2.48533482582001,
11.5131555561469));
#35246=CARTESIAN_POINT('Ctrl Pts',(-0.0989103517498564,2.48121508638053,
11.5141975983127));
#35247=CARTESIAN_POINT('Ctrl Pts',(-0.11878476294852,2.47550101244367,11.5152396404784));
#35248=CARTESIAN_POINT('Ctrl Pts',(-0.138108789237371,2.46825378794438,
11.5162816826442));
#35249=CARTESIAN_POINT('Ctrl Pts',(-0.157412061825551,2.46101434685037,
11.5173226056731));
#35250=CARTESIAN_POINT('Ctrl Pts',(-0.176165427403162,2.45224525402999,
11.5183635287019));
#35251=CARTESIAN_POINT('Ctrl Pts',(-0.194117882425333,2.44205721410709,
11.5194044517308));
#35252=CARTESIAN_POINT('Ctrl Pts',(-0.212079557360518,2.43186394187241,
11.5204459093505));
#35253=CARTESIAN_POINT('Ctrl Pts',(-0.229238852130596,2.420250615819,11.5214873669703));
#35254=CARTESIAN_POINT('Ctrl Pts',(-0.245369688947589,2.40737372325195,
11.5225288245901));
#35255=CARTESIAN_POINT('Ctrl Pts',(-0.261505454438471,2.39449289623283,
11.5235706004206));
#35256=CARTESIAN_POINT('Ctrl Pts',(-0.276611584428988,2.38034822103917,
11.5246123762511));
#35257=CARTESIAN_POINT('Ctrl Pts',(-0.290496119430963,2.36513561547923,
11.5256541520816));
#35258=CARTESIAN_POINT('Ctrl Pts',(-0.304410666170423,2.34989012752716,
11.5266981797342));
#35259=CARTESIAN_POINT('Ctrl Pts',(-0.317097894219481,2.33357268210092,
11.5277422073868));
#35260=CARTESIAN_POINT('Ctrl Pts',(-0.328406518659218,2.31641175684822,
11.5287862350394));
#35261=CARTESIAN_POINT('Ctrl Pts',(-0.33240623089295,2.31034216252743,11.5291554939353));
#35262=CARTESIAN_POINT('Ctrl Pts',(-0.336233899176785,2.30416729494598,
11.5295247528311));
#35263=CARTESIAN_POINT('Ctrl Pts',(-0.339884220642279,2.29789797007143,
11.529894011727));
#35264=CARTESIAN_POINT('Ctrl Pts',(-0.350604217101314,2.2794866764111,11.5309784241804));
#35265=CARTESIAN_POINT('Ctrl Pts',(-0.35985098890901,2.26015666987324,11.5320628366339));
#35266=CARTESIAN_POINT('Ctrl Pts',(-0.367477689652263,2.24016075630445,
11.5331472490873));
#35267=CARTESIAN_POINT('Ctrl Pts',(-0.375085032562881,2.22021559568392,
11.5342289091219));
#35268=CARTESIAN_POINT('Ctrl Pts',(-0.381080186982307,2.19960846920468,
11.5353105691565));
#35269=CARTESIAN_POINT('Ctrl Pts',(-0.38536290260287,2.17861503226159,11.5363922291911));
#35270=CARTESIAN_POINT('Ctrl Pts',(-0.389634913556175,2.15767406851004,
11.5374711856115));
#35271=CARTESIAN_POINT('Ctrl Pts',(-0.392202824028884,2.13634934251665,
11.5385501420318));
#35272=CARTESIAN_POINT('Ctrl Pts',(-0.393016510875971,2.11493024376485,
11.5396290984522));
#35273=CARTESIAN_POINT('Ctrl Pts',(-0.393206190108389,2.10993721945226,
11.5398806149003));
#35274=CARTESIAN_POINT('Ctrl Pts',(-0.39330076247864,2.10493911161085,11.5401321313484));
#35275=CARTESIAN_POINT('Ctrl Pts',(-0.393299995370208,2.09993965272061,
11.5403836477965));
#35276=CARTESIAN_POINT('',(-0.393506066767946,2.09966341860499,11.6653836477965));
#35277=CARTESIAN_POINT('Ctrl Pts',(-0.39266098561946,2.09993890584618,11.5403836903727));
#35278=CARTESIAN_POINT('Ctrl Pts',(-0.392745546116008,2.03788589116262,
11.543510578665));
#35279=CARTESIAN_POINT('Ctrl Pts',(-0.34960937735406,1.84450213648791,11.5532609147986));
#35280=CARTESIAN_POINT('Ctrl Pts',(-0.0466491534524713,1.63729177988004,
11.5696346987724));
#35281=CARTESIAN_POINT('Ctrl Pts',(0.363801326322039,1.81030423639476,11.5895050422954));
#35282=CARTESIAN_POINT('Ctrl Pts',(0.440513616274446,2.24907311750052,11.6093753858181));
#35283=CARTESIAN_POINT('Ctrl Pts',(0.113114633808556,2.55108770777179,11.629245729341));
#35284=CARTESIAN_POINT('Ctrl Pts',(-0.291992820397266,2.44604751618319,
11.6479151500004));
#35285=CARTESIAN_POINT('Ctrl Pts',(-0.392534688237482,2.20668854395861,
11.6599611228189));
#35286=CARTESIAN_POINT('Ctrl Pts',(-0.393506066767946,2.09966341860499,
11.6653836477965));
#35287=CARTESIAN_POINT('',(-0.393451127689227,2.10024138252102,11.7903836477965));
#35288=CARTESIAN_POINT('Ctrl Pts',(-0.393506066767946,2.09966341860499,
11.6653836477965));
#35289=CARTESIAN_POINT('Ctrl Pts',(-0.393721197300494,2.07596063797799,
11.6665845706598));
#35290=CARTESIAN_POINT('Ctrl Pts',(-0.38096993553427,1.9217609719386,11.6744089413645));
#35291=CARTESIAN_POINT('Ctrl Pts',(-0.177198995273587,1.67002842354576,
11.688856759909));
#35292=CARTESIAN_POINT('Ctrl Pts',(0.265606781934669,1.71825652870706,11.7087271034323));
#35293=CARTESIAN_POINT('Ctrl Pts',(0.4647544958161,2.11668229909881,11.7285974469549));
#35294=CARTESIAN_POINT('Ctrl Pts',(0.237553230397542,2.49980433115734,11.7484677904776));
#35295=CARTESIAN_POINT('Ctrl Pts',(-0.207570783958694,2.51616031782387,
11.7683381340004));
#35296=CARTESIAN_POINT('Ctrl Pts',(-0.386668906132234,2.25921693343521,
11.7823100864401));
#35297=CARTESIAN_POINT('Ctrl Pts',(-0.393864405022987,2.11452798323012,
11.7896585910388));
#35298=CARTESIAN_POINT('Ctrl Pts',(-0.393761364200694,2.10024157285132,
11.7903836477965));
#35299=CARTESIAN_POINT('',(-0.39310814853926,2.10020427938886,11.9153836449369));
#35300=CARTESIAN_POINT('Ctrl Pts',(-0.393299925984296,2.10024128975868,
11.7903836477965));
#35301=CARTESIAN_POINT('Ctrl Pts',(-0.393312358087271,2.07997708456835,
11.7914132981653));
#35302=CARTESIAN_POINT('Ctrl Pts',(-0.391754378673078,2.05965018812199,
11.792442948534));
#35303=CARTESIAN_POINT('Ctrl Pts',(-0.388623230446764,2.03952790100285,
11.7934725989028));
#35304=CARTESIAN_POINT('Ctrl Pts',(-0.385497099732515,2.01943785886577,
11.7945005993072));
#35305=CARTESIAN_POINT('Ctrl Pts',(-0.380802862960053,1.99955252466687,
11.7955285997115));
#35306=CARTESIAN_POINT('Ctrl Pts',(-0.374589626192585,1.98013548503039,
11.7965566001159));
#35307=CARTESIAN_POINT('Ctrl Pts',(-0.368376152079289,1.96071770366243,
11.7975846397899));
#35308=CARTESIAN_POINT('Ctrl Pts',(-0.360643749500282,1.94176898604104,
11.7986126794639));
#35309=CARTESIAN_POINT('Ctrl Pts',(-0.351491849216906,1.92353932468088,
11.7996407191379));
#35310=CARTESIAN_POINT('Ctrl Pts',(-0.342340698207265,1.90531115579835,
11.8006686746454));
#35311=CARTESIAN_POINT('Ctrl Pts',(-0.331770637105692,1.88780259463896,
11.801696630153));
#35312=CARTESIAN_POINT('Ctrl Pts',(-0.319927294380957,1.87123939082508,
11.8027245856605));
#35313=CARTESIAN_POINT('Ctrl Pts',(-0.308057729623245,1.85463951485819,
11.8037548171372));
#35314=CARTESIAN_POINT('Ctrl Pts',(-0.294909727505328,1.8389897697705,11.8047850486139));
#35315=CARTESIAN_POINT('Ctrl Pts',(-0.280669978286549,1.82448366057777,
11.8058152800907));
#35316=CARTESIAN_POINT('Ctrl Pts',(-0.270241171337324,1.81385977879227,
11.8065697937425));
#35317=CARTESIAN_POINT('Ctrl Pts',(-0.259227669239505,1.80384861854286,
11.8073243073943));
#35318=CARTESIAN_POINT('Ctrl Pts',(-0.247713843480614,1.79451228871187,
11.8080788210461));
#35319=CARTESIAN_POINT('Ctrl Pts',(-0.231783046212682,1.78159432548412,
11.8091227836936));
#35320=CARTESIAN_POINT('Ctrl Pts',(-0.214791578465285,1.76988738384627,
11.8101667463412));
#35321=CARTESIAN_POINT('Ctrl Pts',(-0.196949786389058,1.7595654664384,11.8112107089887));
#35322=CARTESIAN_POINT('Ctrl Pts',(-0.179140816211926,1.74926253730985,
11.8122527511545));
#35323=CARTESIAN_POINT('Ctrl Pts',(-0.160485226611759,1.74033999069353,
11.8132947933203));
#35324=CARTESIAN_POINT('Ctrl Pts',(-0.141223284345155,1.73292933383507,
11.814336835486));
#35325=CARTESIAN_POINT('Ctrl Pts',(-0.12198202910195,1.72552663590565,11.8153777585149));
#35326=CARTESIAN_POINT('Ctrl Pts',(-0.102136386848528,1.71963289406112,
11.8164186815437));
#35327=CARTESIAN_POINT('Ctrl Pts',(-0.0819475555604086,1.71533197671541,
11.8174596045726));
#35328=CARTESIAN_POINT('Ctrl Pts',(-0.061748355814717,1.71102885053065,
11.8185010621924));
#35329=CARTESIAN_POINT('Ctrl Pts',(-0.0412063311912306,1.70832035216473,
11.8195425198122));
#35330=CARTESIAN_POINT('Ctrl Pts',(-0.0205944375822625,1.7072395652046,
11.820583977432));
#35331=CARTESIAN_POINT('Ctrl Pts',(2.3753858809171E-5,1.70615844801694,
11.8216257532625));
#35332=CARTESIAN_POINT('Ctrl Pts',(0.0207111207399054,1.70670603467909,
11.8226675290929));
#35333=CARTESIAN_POINT('Ctrl Pts',(0.0411940407681122,1.70886327070295,
11.8237093049234));
#35334=CARTESIAN_POINT('Ctrl Pts',(0.0617212350927722,1.71102516964142,
11.824753332576));
#35335=CARTESIAN_POINT('Ctrl Pts',(0.0820423762315913,1.71480352955339,
11.8257973602286));
#35336=CARTESIAN_POINT('Ctrl Pts',(0.10189263988648,1.72012794267416,11.8268413878812));
#35337=CARTESIAN_POINT('Ctrl Pts',(0.10891341794883,1.72201111780388,11.8272106467771));
#35338=CARTESIAN_POINT('Ctrl Pts',(0.115875439456983,1.72408724175438,11.827579905673));
#35339=CARTESIAN_POINT('Ctrl Pts',(0.122767557839216,1.72635174730477,11.8279491645688));
#35340=CARTESIAN_POINT('Ctrl Pts',(0.142252841021652,1.7327539199708,11.8289931272164));
#35341=CARTESIAN_POINT('Ctrl Pts',(0.161294035664333,1.740703471235,11.8300370898639));
#35342=CARTESIAN_POINT('Ctrl Pts',(0.179630973060031,1.75011772906089,11.8310810525115));
#35343=CARTESIAN_POINT('Ctrl Pts',(0.197934177683471,1.75951466834507,11.8321230946773));
#35344=CARTESIAN_POINT('Ctrl Pts',(0.215535022366861,1.77037068639414,11.833165136843));
#35345=CARTESIAN_POINT('Ctrl Pts',(0.232192872726832,1.78255494986555,11.8342071790088));
#35346=CARTESIAN_POINT('Ctrl Pts',(0.248832832817209,1.79472612762942,11.8352481020377));
#35347=CARTESIAN_POINT('Ctrl Pts',(0.264531201223698,1.8082223100065,11.8362890250665));
#35348=CARTESIAN_POINT('Ctrl Pts',(0.279076068698541,1.82286927655028,11.8373299480954));
#35349=CARTESIAN_POINT('Ctrl Pts',(0.293628406038229,1.83752376539432,11.8383714057152));
#35350=CARTESIAN_POINT('Ctrl Pts',(0.307025529057808,1.85332970838511,11.839412863335));
#35351=CARTESIAN_POINT('Ctrl Pts',(0.319091864528525,1.87007550806469,11.8404543209547));
#35352=CARTESIAN_POINT('Ctrl Pts',(0.331161886790774,1.88682642431613,11.8414960967852));
#35353=CARTESIAN_POINT('Ctrl Pts',(0.341899911610759,1.9045171513388,11.8425378726157));
#35354=CARTESIAN_POINT('Ctrl Pts',(0.351173843652062,1.92290730807106,11.8435796484462));
#35355=CARTESIAN_POINT('Ctrl Pts',(0.360467821507927,1.94133721554444,11.8446236760988));
#35356=CARTESIAN_POINT('Ctrl Pts',(0.368291109722894,1.96046888934245,11.8456677037514));
#35357=CARTESIAN_POINT('Ctrl Pts',(0.374559554228507,1.98004154745854,11.846711731404));
#35358=CARTESIAN_POINT('Ctrl Pts',(0.376776620884906,1.98696414008059,11.8470809902999));
#35359=CARTESIAN_POINT('Ctrl Pts',(0.378799646733713,1.99394177582292,11.8474502491958));
#35360=CARTESIAN_POINT('Ctrl Pts',(0.380626438135335,2.00096261012927,11.8478195080916));
#35361=CARTESIAN_POINT('Ctrl Pts',(0.385791112594161,2.02081179684508,11.8488634707392));
#35362=CARTESIAN_POINT('Ctrl Pts',(0.389414330272041,2.04112520996009,11.8499074333867));
#35363=CARTESIAN_POINT('Ctrl Pts',(0.391424769275268,2.06163934309995,11.8509513960343));
#35364=CARTESIAN_POINT('Ctrl Pts',(0.393431509859312,2.08211573828138,11.8519934382001));
#35365=CARTESIAN_POINT('Ctrl Pts',(0.393831230767547,2.10279140234921,11.8530354803658));
#35366=CARTESIAN_POINT('Ctrl Pts',(0.392603679277159,2.12339318315316,11.8540775225316));
#35367=CARTESIAN_POINT('Ctrl Pts',(0.391377446157789,2.14397283796818,11.8551184455605));
#35368=CARTESIAN_POINT('Ctrl Pts',(0.38852742484426,2.16447803457521,11.8561593685893));
#35369=CARTESIAN_POINT('Ctrl Pts',(0.38408539270256,2.18463628720898,11.8572002916182));
#35370=CARTESIAN_POINT('Ctrl Pts',(0.379641079248923,2.20480489259592,11.858241749238));
#35371=CARTESIAN_POINT('Ctrl Pts',(0.373603264147745,2.2246254760342,11.8592832068578));
#35372=CARTESIAN_POINT('Ctrl Pts',(0.366054821369077,2.24383587088224,11.8603246644775));
#35373=CARTESIAN_POINT('Ctrl Pts',(0.358504072212052,2.26305213534342,11.861366440308));
#35374=CARTESIAN_POINT('Ctrl Pts',(0.349442079048673,2.28165716905833,11.8624082161385));
#35375=CARTESIAN_POINT('Ctrl Pts',(0.338999452987024,2.29940978129094,11.863449991969));
#35376=CARTESIAN_POINT('Ctrl Pts',(0.328534254952179,2.31720076619773,11.8644940196216));
#35377=CARTESIAN_POINT('Ctrl Pts',(0.316682888350589,2.3341350477143,11.8655380472742));
#35378=CARTESIAN_POINT('Ctrl Pts',(0.303619069244698,2.35000070158098,11.8665820749268));
#35379=CARTESIAN_POINT('Ctrl Pts',(0.298998567664272,2.35561217539054,11.8669513338227));
#35380=CARTESIAN_POINT('Ctrl Pts',(0.294226747047553,2.36109029205047,11.8673205927186));
#35381=CARTESIAN_POINT('Ctrl Pts',(0.289312379052769,2.366426795437,11.8676898516144));
#35382=CARTESIAN_POINT('Ctrl Pts',(0.275418559078957,2.38151406961361,11.868733814262));
#35383=CARTESIAN_POINT('Ctrl Pts',(0.260299990829136,2.39555655346789,11.8697777769095));
#35384=CARTESIAN_POINT('Ctrl Pts',(0.244139627350994,2.40835163751295,11.8708217395571));
#35385=CARTESIAN_POINT('Ctrl Pts',(0.228008992602849,2.42112318362216,11.8718637817229));
#35386=CARTESIAN_POINT('Ctrl Pts',(0.210840900219715,2.43265138666402,11.8729058238886));
#35387=CARTESIAN_POINT('Ctrl Pts',(0.192854058255359,2.44277135559209,11.8739478660544));
#35388=CARTESIAN_POINT('Ctrl Pts',(0.174886533876714,2.45288045583251,11.8749887890833));
#35389=CARTESIAN_POINT('Ctrl Pts',(0.15610262940298,2.46158394031299,11.8760297121121));
#35390=CARTESIAN_POINT('Ctrl Pts',(0.136748657406688,2.46876102654357,11.877070635141));
#35391=CARTESIAN_POINT('Ctrl Pts',(0.117384745714798,2.47594179873858,11.8781120927608));
#35392=CARTESIAN_POINT('Ctrl Pts',(0.0974508658738936,2.48159433564851,
11.8791535503805));
#35393=CARTESIAN_POINT('Ctrl Pts',(0.0772123134675798,2.48564640365104,
11.8801950080003));
#35394=CARTESIAN_POINT('Ctrl Pts',(0.0569675773011836,2.48969970973701,
11.8812367838308));
#35395=CARTESIAN_POINT('Ctrl Pts',(0.0364187112028805,2.49215146455734,
11.8822785596613));
#35396=CARTESIAN_POINT('Ctrl Pts',(0.0158392148146877,2.49298092736678,
11.8833203354918));
#35397=CARTESIAN_POINT('Ctrl Pts',(-0.00478476462195937,2.49381218307891,
11.8843643631444));
#35398=CARTESIAN_POINT('Ctrl Pts',(-0.0254387706010218,2.49301417441685,
11.885408390797));
#35399=CARTESIAN_POINT('Ctrl Pts',(-0.0458505777671413,2.4906182465252,
11.8864524184496));
#35400=CARTESIAN_POINT('Ctrl Pts',(-0.0530699664088936,2.48977083823515,
11.8868216773455));
#35401=CARTESIAN_POINT('Ctrl Pts',(-0.0602591377000667,2.4887240095554,
11.8871909362414));
#35402=CARTESIAN_POINT('Ctrl Pts',(-0.0674064014868825,2.48748066666427,
11.8875601951372));
#35403=CARTESIAN_POINT('Ctrl Pts',(-0.0876130275401507,2.48396550819155,
11.8886041577848));
#35404=CARTESIAN_POINT('Ctrl Pts',(-0.107604153555675,2.47885499556035,
11.8896481204323));
#35405=CARTESIAN_POINT('Ctrl Pts',(-0.127110386058818,2.47219328279266,
11.8906920830799));
#35406=CARTESIAN_POINT('Ctrl Pts',(-0.146580734745346,2.46554382496345,
11.8917341252457));
#35407=CARTESIAN_POINT('Ctrl Pts',(-0.165567252883045,2.45734901011157,
11.8927761674114));
#35408=CARTESIAN_POINT('Ctrl Pts',(-0.183812906506485,2.44770347338161,
11.8938182095772));
#35409=CARTESIAN_POINT('Ctrl Pts',(-0.202038964584578,2.43806829580657,
11.8948591326061));
#35410=CARTESIAN_POINT('Ctrl Pts',(-0.219525077061563,2.42698580602208,
11.8959000556349));
#35411=CARTESIAN_POINT('Ctrl Pts',(-0.236036354411226,2.41459772630497,
11.8969409786638));
#35412=CARTESIAN_POINT('Ctrl Pts',(-0.252556111522601,2.40220328439299,
11.8979824362836));
#35413=CARTESIAN_POINT('Ctrl Pts',(-0.2680994351019,2.38850234168312,11.8990238939034));
#35414=CARTESIAN_POINT('Ctrl Pts',(-0.282461980533189,2.37367886208706,
11.9000653515231));
#35415=CARTESIAN_POINT('Ctrl Pts',(-0.296828914348269,2.35885085327173,
11.9011071273536));
#35416=CARTESIAN_POINT('Ctrl Pts',(-0.310013866211834,2.34290017792611,
11.9021489031841));
#35417=CARTESIAN_POINT('Ctrl Pts',(-0.321851346635873,2.32604557210588,
11.9031906790146));
#35418=CARTESIAN_POINT('Ctrl Pts',(-0.333714414042464,2.30915453467271,
11.9042347066672));
#35419=CARTESIAN_POINT('Ctrl Pts',(-0.34422382070222,2.29135630014038,11.9052787343198));
#35420=CARTESIAN_POINT('Ctrl Pts',(-0.353258561670272,2.27289672815485,
11.9063227619724));
#35421=CARTESIAN_POINT('Ctrl Pts',(-0.35645403112551,2.26636781950709,11.9066920208683));
#35422=CARTESIAN_POINT('Ctrl Pts',(-0.359465467148731,2.25975636828849,
11.9070612797642));
#35423=CARTESIAN_POINT('Ctrl Pts',(-0.36228898521523,2.25307377695647,11.90743053866));
#35424=CARTESIAN_POINT('Ctrl Pts',(-0.371160264491516,2.23207758263456,
11.9085907220601));
#35425=CARTESIAN_POINT('Ctrl Pts',(-0.378217950532817,2.21027158304454,
11.9097509054601));
#35426=CARTESIAN_POINT('Ctrl Pts',(-0.383336557191521,2.18796575424875,
11.9109110888601));
#35427=CARTESIAN_POINT('Ctrl Pts',(-0.388417242785302,2.16582517760815,
11.9120626770715));
#35428=CARTESIAN_POINT('Ctrl Pts',(-0.391587266064288,2.1431925567704,11.9132142652829));
#35429=CARTESIAN_POINT('Ctrl Pts',(-0.392771028312522,2.12039140304942,
11.9143658534942));
#35430=CARTESIAN_POINT('Ctrl Pts',(-0.393119770227964,2.11367407612434,
11.9147051167873));
#35431=CARTESIAN_POINT('Ctrl Pts',(-0.393296445026141,2.10694223489702,
11.9150443800805));
#35432=CARTESIAN_POINT('Ctrl Pts',(-0.393299946880902,2.1002044100772,11.9153836433736));
#35433=CARTESIAN_POINT('',(-0.393236352003104,2.09966893770289,12.0403836508529));
#35434=CARTESIAN_POINT('Ctrl Pts',(-0.392757315398087,2.10020404033675,
11.9153836477965));
#35435=CARTESIAN_POINT('Ctrl Pts',(-0.392387812223022,2.02141992873627,
11.9193560592586));
#35436=CARTESIAN_POINT('Ctrl Pts',(-0.331161934722823,1.81074557558215,
11.9299519185616));
#35437=CARTESIAN_POINT('Ctrl Pts',(0.0125649746725957,1.63511596941171,
11.9471712257055));
#35438=CARTESIAN_POINT('Ctrl Pts',(0.397684464205737,1.85891472999403,11.9670415692284));
#35439=CARTESIAN_POINT('Ctrl Pts',(0.417982597681194,2.30387640501092,11.9869119127511));
#35440=CARTESIAN_POINT('Ctrl Pts',(0.0548386009764254,2.5618092336966,12.0067822562739));
#35441=CARTESIAN_POINT('Ctrl Pts',(-0.316031342189213,2.41316174940269,
12.0246061679557));
#35442=CARTESIAN_POINT('Ctrl Pts',(-0.392293930819629,2.19029546669872,
12.0358066317966));
#35443=CARTESIAN_POINT('Ctrl Pts',(-0.39301380866462,2.09966918558721,12.0403836477965));
#35444=CARTESIAN_POINT('',(-0.393542333918762,2.09995565468233,12.1653836477965));
#35445=CARTESIAN_POINT('Ctrl Pts',(-0.393299860603728,2.09966886696257,
12.0403836517251));
#35446=CARTESIAN_POINT('Ctrl Pts',(-0.393278992343729,2.07488280571045,
12.0416345529641));
#35447=CARTESIAN_POINT('Ctrl Pts',(-0.390911039572184,2.05019917076539,
12.042885454203));
#35448=CARTESIAN_POINT('Ctrl Pts',(-0.386277243284786,2.02600823478044,
12.044136355442));
#35449=CARTESIAN_POINT('Ctrl Pts',(-0.383330311450925,2.01062364838013,
12.0449318847345));
#35450=CARTESIAN_POINT('Ctrl Pts',(-0.379467960270538,1.99543790614008,
12.045727414027));
#35451=CARTESIAN_POINT('Ctrl Pts',(-0.374721036216391,1.98054693383209,
12.0465229433195));
#35452=CARTESIAN_POINT('Ctrl Pts',(-0.368491710093453,1.96100570634752,
12.0475669059671));
#35453=CARTESIAN_POINT('Ctrl Pts',(-0.360711132460197,1.94189484371864,
12.0486108686146));
#35454=CARTESIAN_POINT('Ctrl Pts',(-0.351459667605607,1.92347523673276,
12.0496548312622));
#35455=CARTESIAN_POINT('Ctrl Pts',(-0.34222522181752,1.90508951459875,12.050696873428));
#35456=CARTESIAN_POINT('Ctrl Pts',(-0.33152553318996,1.88739320072474,12.0517389155937));
#35457=CARTESIAN_POINT('Ctrl Pts',(-0.319489298458345,1.87062807894035,
12.0527809577595));
#35458=CARTESIAN_POINT('Ctrl Pts',(-0.307465990453748,1.85388096263339,
12.0538218807884));
#35459=CARTESIAN_POINT('Ctrl Pts',(-0.294109389451292,1.83806366453776,
12.0548628038172));
#35460=CARTESIAN_POINT('Ctrl Pts',(-0.2795918320278,1.82338962878565,12.0559037268461));
#35461=CARTESIAN_POINT('Ctrl Pts',(-0.265066818765183,1.80870805683123,
12.0569451844659));
#35462=CARTESIAN_POINT('Ctrl Pts',(-0.249380163951019,1.79517145460707,
12.0579866420857));
#35463=CARTESIAN_POINT('Ctrl Pts',(-0.232741901561904,1.78295726272733,
12.0590280997055));
#35464=CARTESIAN_POINT('Ctrl Pts',(-0.216098555458261,1.77073933887947,
12.060069875536));
#35465=CARTESIAN_POINT('Ctrl Pts',(-0.198503636978505,1.75984503562868,
12.0611116513665));
#35466=CARTESIAN_POINT('Ctrl Pts',(-0.180196347689156,1.75040857235984,
12.062153427197));
#35467=CARTESIAN_POINT('Ctrl Pts',(-0.161849486778567,1.7409517119615,12.0631974548496));
#35468=CARTESIAN_POINT('Ctrl Pts',(-0.142787860101782,1.73295926745141,
12.0642414825022));
#35469=CARTESIAN_POINT('Ctrl Pts',(-0.123271494020737,1.7265176995333,12.0652855101548));
#35470=CARTESIAN_POINT('Ctrl Pts',(-0.116368811154175,1.72423940139535,
12.0656547690507));
#35471=CARTESIAN_POINT('Ctrl Pts',(-0.109409368565569,1.72215464889553,
12.0660240279465));
#35472=CARTESIAN_POINT('Ctrl Pts',(-0.102404990915842,1.72026574050327,
12.0663932868423));
#35473=CARTESIAN_POINT('Ctrl Pts',(-0.0826023301861622,1.71492544991475,
12.0674372494899));
#35474=CARTESIAN_POINT('Ctrl Pts',(-0.0623218074606997,1.71112244364286,
12.0684812121374));
#35475=CARTESIAN_POINT('Ctrl Pts',(-0.041826287026211,1.70893037485174,
12.069525174785));
#35476=CARTESIAN_POINT('Ctrl Pts',(-0.0213684703100815,1.70674233860736,
12.0705672169508));
#35477=CARTESIAN_POINT('Ctrl Pts',(-0.000697157978116574,1.70615949392462,
12.0716092591165));
#35478=CARTESIAN_POINT('Ctrl Pts',(0.019914687928456,1.70720451223988,12.0726513012823));
#35479=CARTESIAN_POINT('Ctrl Pts',(0.0405043970363343,1.70824840822188,
12.0736922243112));
#35480=CARTESIAN_POINT('Ctrl Pts',(0.0610340339351239,1.7109166882268,12.07473314734));
#35481=CARTESIAN_POINT('Ctrl Pts',(0.08123084207394,1.71517998974071,12.0757740703689));
#35482=CARTESIAN_POINT('Ctrl Pts',(0.101438022767024,1.71944548077517,12.0768155279887));
#35483=CARTESIAN_POINT('Ctrl Pts',(0.121311309972315,1.72530749362791,12.0778569856085));
#35484=CARTESIAN_POINT('Ctrl Pts',(0.140587813257872,1.73268547978147,12.0788984432282));
#35485=CARTESIAN_POINT('Ctrl Pts',(0.159870206355562,1.74006572023145,12.0799402190587));
#35486=CARTESIAN_POINT('Ctrl Pts',(0.178554778877644,1.74896255951808,12.0809819948892));
#35487=CARTESIAN_POINT('Ctrl Pts',(0.196399192632152,1.75924752805968,12.0820237707197));
#35488=CARTESIAN_POINT('Ctrl Pts',(0.214282177491934,1.76955472779418,12.0830677983723));
#35489=CARTESIAN_POINT('Ctrl Pts',(0.231320770877661,1.78125563016296,12.0841118260249));
#35490=CARTESIAN_POINT('Ctrl Pts',(0.247301518113519,1.79417840308646,12.0851558536775));
#35491=CARTESIAN_POINT('Ctrl Pts',(0.252953698939172,1.798749018481,12.0855251125734));
#35492=CARTESIAN_POINT('Ctrl Pts',(0.258473868190067,1.80347212821718,12.0858943714693));
#35493=CARTESIAN_POINT('Ctrl Pts',(0.263853692369344,1.80833903411141,12.0862636303651));
#35494=CARTESIAN_POINT('Ctrl Pts',(0.279063442375129,1.82209867001886,12.0873075930127));
#35495=CARTESIAN_POINT('Ctrl Pts',(0.293239291536087,1.83709226062575,12.0883515556602));
#35496=CARTESIAN_POINT('Ctrl Pts',(0.306177017765042,1.85313865472192,12.0893955183078));
#35497=CARTESIAN_POINT('Ctrl Pts',(0.319090943652483,1.86915552974705,12.0904375604736));
#35498=CARTESIAN_POINT('Ctrl Pts',(0.330770764769411,1.88622083490477,12.0914796026393));
#35499=CARTESIAN_POINT('Ctrl Pts',(0.341049659281186,1.90411733128174,12.0925216448051));
#35500=CARTESIAN_POINT('Ctrl Pts',(0.351317514421732,1.92199460710275,12.0935625678339));
#35501=CARTESIAN_POINT('Ctrl Pts',(0.360187040219998,1.94070068155717,12.0946034908628));
#35502=CARTESIAN_POINT('Ctrl Pts',(0.367535277154023,1.95999032159413,12.0956444138917));
#35503=CARTESIAN_POINT('Ctrl Pts',(0.374887287951018,1.97928986828746,12.0966858715114));
#35504=CARTESIAN_POINT('Ctrl Pts',(0.380716172040446,1.99917289746567,12.0977273291312));
#35505=CARTESIAN_POINT('Ctrl Pts',(0.384947348717024,2.01937476377874,12.098768786751));
#35506=CARTESIAN_POINT('Ctrl Pts',(0.389179818202539,2.0395828026427,12.0998105625815));
#35507=CARTESIAN_POINT('Ctrl Pts',(0.39181349315293,2.06010914561655,12.100852338412));
#35508=CARTESIAN_POINT('Ctrl Pts',(0.392825211050546,2.08068048750372,12.1018941142425));
#35509=CARTESIAN_POINT('Ctrl Pts',(0.393839115799356,2.10129629481321,12.1029381418951));
#35510=CARTESIAN_POINT('Ctrl Pts',(0.393224086057792,2.12195655907155,12.1039821695477));
#35511=CARTESIAN_POINT('Ctrl Pts',(0.391009054441986,2.14238878795606,12.1050261972003));
#35512=CARTESIAN_POINT('Ctrl Pts',(0.39022562679355,2.14961539949202,12.1053954560962));
#35513=CARTESIAN_POINT('Ctrl Pts',(0.389242518921626,2.15681356127486,12.105764714992));
#35514=CARTESIAN_POINT('Ctrl Pts',(0.388062533342288,2.16397155786727,12.1061339738879));
#35515=CARTESIAN_POINT('Ctrl Pts',(0.38472649761437,2.18420852753092,12.1071779365355));
#35516=CARTESIAN_POINT('Ctrl Pts',(0.379793261473248,2.20424413682783,12.108221899183));
#35517=CARTESIAN_POINT('Ctrl Pts',(0.373304590993985,2.22380861174738,12.1092658618306));
#35518=CARTESIAN_POINT('Ctrl Pts',(0.366827857123262,2.24333709570713,12.1103079039963));
#35519=CARTESIAN_POINT('Ctrl Pts',(0.358801541214424,2.26239545645464,12.1113499461621));
#35520=CARTESIAN_POINT('Ctrl Pts',(0.34931799796196,2.28072583185546,12.1123919883279));
#35521=CARTESIAN_POINT('Ctrl Pts',(0.339844639885968,2.29903652072106,12.1134329113567));
#35522=CARTESIAN_POINT('Ctrl Pts',(0.328917472140692,2.31662011291515,12.1144738343856));
#35523=CARTESIAN_POINT('Ctrl Pts',(0.316676130855067,2.33324047278863,12.1155147574144));
#35524=CARTESIAN_POINT('Ctrl Pts',(0.304428502735605,2.34986936844577,12.1165562150342));
#35525=CARTESIAN_POINT('Ctrl Pts',(0.290865776088012,2.36553344150845,12.117597672654));
#35526=CARTESIAN_POINT('Ctrl Pts',(0.276170097577517,2.38002672587456,12.1186391302738));
#35527=CARTESIAN_POINT('Ctrl Pts',(0.261469928896557,2.3945244385709,12.1196809061043));
#35528=CARTESIAN_POINT('Ctrl Pts',(0.245636668050709,2.40785015996275,12.1207226819348));
#35529=CARTESIAN_POINT('Ctrl Pts',(0.228887576653288,2.41983646954934,12.1217644577653));
#35530=CARTESIAN_POINT('Ctrl Pts',(0.21210228171473,2.4318486878161,12.1228084854178));
#35531=CARTESIAN_POINT('Ctrl Pts',(0.194397834904987,2.44251533414798,12.1238525130704));
#35532=CARTESIAN_POINT('Ctrl Pts',(0.176019014395658,2.45171323058876,12.124896540723));
#35533=CARTESIAN_POINT('Ctrl Pts',(0.169518666486625,2.45496640599607,12.1252657996189));
#35534=CARTESIAN_POINT('Ctrl Pts',(0.162934149126423,2.45803628633091,12.1256350585148));
#35535=CARTESIAN_POINT('Ctrl Pts',(0.156276829917091,2.46091888622108,12.1260043174106));
#35536=CARTESIAN_POINT('Ctrl Pts',(0.137455367075572,2.46906852498915,12.1270482800582));
#35537=CARTESIAN_POINT('Ctrl Pts',(0.117938618192391,2.47576620904804,12.1280922427057));
#35538=CARTESIAN_POINT('Ctrl Pts',(0.097976022816915,2.48090102251501,12.1291362053533));
#35539=CARTESIAN_POINT('Ctrl Pts',(0.0780501507867196,2.4860263899393,12.130178247519));
#35540=CARTESIAN_POINT('Ctrl Pts',(0.0576807500142376,2.48959435485226,
12.1312202896848));
#35541=CARTESIAN_POINT('Ctrl Pts',(0.0371346288638493,2.49154298530193,
12.1322623318506));
#35542=CARTESIAN_POINT('Ctrl Pts',(0.0166105739248071,2.4934895229531,12.1333032548794));
#35543=CARTESIAN_POINT('Ctrl Pts',(-0.00408909855726484,2.49382008083868,
12.1343441779083));
#35544=CARTESIAN_POINT('Ctrl Pts',(-0.0246902539410924,2.49252424302242,
12.1353851009372));
#35545=CARTESIAN_POINT('Ctrl Pts',(-0.0453019895413941,2.49122773969763,
12.1364265585569));
#35546=CARTESIAN_POINT('Ctrl Pts',(-0.0658143716253239,2.48830320208075,
12.1374680161767));
#35547=CARTESIAN_POINT('Ctrl Pts',(-0.0859556209254608,2.48379228917647,
12.1385094737965));
#35548=CARTESIAN_POINT('Ctrl Pts',(-0.106103024255346,2.47927999799165,
12.139551249627));
#35549=CARTESIAN_POINT('Ctrl Pts',(-0.125878359575164,2.4731805625576,12.1405930254575));
#35550=CARTESIAN_POINT('Ctrl Pts',(-0.145023249093352,2.4655860325866,12.141634801288));
#35551=CARTESIAN_POINT('Ctrl Pts',(-0.164209520724682,2.45797508686672,
12.1426788289406));
#35552=CARTESIAN_POINT('Ctrl Pts',(-0.18276196489742,2.4488629193954,12.1437228565932));
#35553=CARTESIAN_POINT('Ctrl Pts',(-0.200444508533405,2.43838866558855,
12.1447668842458));
#35554=CARTESIAN_POINT('Ctrl Pts',(-0.206698592439045,2.434684059311,12.1451361431417));
#35555=CARTESIAN_POINT('Ctrl Pts',(-0.21284412101073,2.43080946091724,12.1455054020376));
#35556=CARTESIAN_POINT('Ctrl Pts',(-0.218871589787769,2.4267722711366,12.1458746609334));
#35557=CARTESIAN_POINT('Ctrl Pts',(-0.235859404920921,2.41539385737989,
12.1469153800299));
#35558=CARTESIAN_POINT('Ctrl Pts',(-0.252009714550351,2.40265218981606,
12.1479560991263));
#35559=CARTESIAN_POINT('Ctrl Pts',(-0.267095036879578,2.38869556850478,
12.1489968182227));
#35560=CARTESIAN_POINT('Ctrl Pts',(-0.282152609210813,2.374764620905,12.1500356228785));
#35561=CARTESIAN_POINT('Ctrl Pts',(-0.296148503569641,2.35962360806551,
12.1510744275344));
#35562=CARTESIAN_POINT('Ctrl Pts',(-0.308886923198884,2.34346202717616,
12.1521132321902));
#35563=CARTESIAN_POINT('Ctrl Pts',(-0.321611824317927,2.32731759758991,
12.1531509344259));
#35564=CARTESIAN_POINT('Ctrl Pts',(-0.333081420598854,2.31015531091151,
12.1541886366615));
#35565=CARTESIAN_POINT('Ctrl Pts',(-0.343139227393768,2.29219875291897,
12.1552263388971));
#35566=CARTESIAN_POINT('Ctrl Pts',(-0.353202254929823,2.27423287415273,
12.1562645797765));
#35567=CARTESIAN_POINT('Ctrl Pts',(-0.361851654557597,2.25547253991361,
12.1573028206559));
#35568=CARTESIAN_POINT('Ctrl Pts',(-0.368976013497073,2.23616751251237,
12.1583410615353));
#35569=CARTESIAN_POINT('Ctrl Pts',(-0.376102798245648,2.21685591184447,
12.1593796559306));
#35570=CARTESIAN_POINT('Ctrl Pts',(-0.38170328924997,2.19699995663281,12.1604182503259));
#35571=CARTESIAN_POINT('Ctrl Pts',(-0.385715712151455,2.17686533288483,
12.1614568447212));
#35572=CARTESIAN_POINT('Ctrl Pts',(-0.389736625277397,2.15668810458615,
12.162497636766));
#35573=CARTESIAN_POINT('Ctrl Pts',(-0.392162681036991,2.13623176724534,
12.1635384288109));
#35574=CARTESIAN_POINT('Ctrl Pts',(-0.392983771039473,2.11576850340379,
12.1645792208558));
#35575=CARTESIAN_POINT('Ctrl Pts',(-0.393195310870127,2.1104964925955,12.1648473631694));
#35576=CARTESIAN_POINT('Ctrl Pts',(-0.393300591151716,2.10522401439645,
12.1651155054829));
#35577=CARTESIAN_POINT('Ctrl Pts',(-0.393299997503069,2.09995568198939,
12.1653836477965));
#35578=CARTESIAN_POINT('',(-0.393299839507982,2.10035530690372,12.2903836477965));
#35579=CARTESIAN_POINT('Ctrl Pts',(-0.393943705169969,2.09995560945483,
12.1653836477965));
#35580=CARTESIAN_POINT('Ctrl Pts',(-0.393947486574571,2.09758514782183,
12.1655041000164));
#35581=CARTESIAN_POINT('Ctrl Pts',(-0.393927945909171,2.0952147502193,12.1656245522363));
#35582=CARTESIAN_POINT('Ctrl Pts',(-0.391517524700006,1.96252442555434,
12.1723684522972));
#35583=CARTESIAN_POINT('Ctrl Pts',(-0.244598393841188,1.70446660543666,
12.185615347979));
#35584=CARTESIAN_POINT('Ctrl Pts',(0.200166029731868,1.68022791776267,12.2054856915018));
#35585=CARTESIAN_POINT('Ctrl Pts',(0.461305371170257,2.04107296873276,12.2253560350246));
#35586=CARTESIAN_POINT('Ctrl Pts',(0.299259835615228,2.45597554869975,12.2452263785474));
#35587=CARTESIAN_POINT('Ctrl Pts',(-0.137315858568866,2.54431902442941,
12.2650967220702));
#35588=CARTESIAN_POINT('Ctrl Pts',(-0.372610321006317,2.30247066778261,
12.2801491210047));
#35589=CARTESIAN_POINT('Ctrl Pts',(-0.393458625209538,2.13607564144017,
12.2885780720982));
#35590=CARTESIAN_POINT('Ctrl Pts',(-0.393146135639666,2.10035660126003,
12.2903835753508));
#35591=CARTESIAN_POINT('',(-0.393077234676447,2.09986488121323,12.4153836834263));
#35592=CARTESIAN_POINT('Ctrl Pts',(-0.393299839507982,2.10035530690372,
12.2903836477965));
#35593=CARTESIAN_POINT('Ctrl Pts',(-0.39331828485987,2.07993759516899,12.291415314833));
#35594=CARTESIAN_POINT('Ctrl Pts',(-0.391742474161141,2.059484472507,12.2924469818694));
#35595=CARTESIAN_POINT('Ctrl Pts',(-0.388582344254501,2.03926572850789,
12.2934786489059));
#35596=CARTESIAN_POINT('Ctrl Pts',(-0.385421623636996,2.01904320509715,
12.2945105087879));
#35597=CARTESIAN_POINT('Ctrl Pts',(-0.380676071652342,1.99905589466593,
12.2955423686699));
#35598=CARTESIAN_POINT('Ctrl Pts',(-0.374407400948638,1.97956749560486,
12.2965742285519));
#35599=CARTESIAN_POINT('Ctrl Pts',(-0.368138578638465,1.960078625221,12.2976061133892));
#35600=CARTESIAN_POINT('Ctrl Pts',(-0.360346816786855,1.941089398043,12.2986379982265));
#35601=CARTESIAN_POINT('Ctrl Pts',(-0.351143090919384,1.92284633873504,
12.2996698830638));
#35602=CARTESIAN_POINT('Ctrl Pts',(-0.341918686932898,1.90456229253145,
12.3007040862489));
#35603=CARTESIAN_POINT('Ctrl Pts',(-0.331276362675052,1.88702841307074,
12.3017382894339));
#35604=CARTESIAN_POINT('Ctrl Pts',(-0.319372463074704,1.87046542781185,
12.302772492619));
#35605=CARTESIAN_POINT('Ctrl Pts',(-0.311449919737479,1.85944206799592,
12.3034607981179));
#35606=CARTESIAN_POINT('Ctrl Pts',(-0.302969490447348,1.84884816990448,
12.3041491036168));
#35607=CARTESIAN_POINT('Ctrl Pts',(-0.293986668735287,1.83874011290302,
12.3048374091157));
#35608=CARTESIAN_POINT('Ctrl Pts',(-0.280362296487944,1.82340908043909,
12.3058813717633));
#35609=CARTESIAN_POINT('Ctrl Pts',(-0.265494859934947,1.80910097822167,
12.3069253344108));
#35610=CARTESIAN_POINT('Ctrl Pts',(-0.249563694235651,1.79602162491477,
12.3079692970584));
#35611=CARTESIAN_POINT('Ctrl Pts',(-0.233661835632341,1.78296633248767,
12.3090113392242));
#35612=CARTESIAN_POINT('Ctrl Pts',(-0.216700656659647,1.77113580970523,
12.3100533813899));
#35613=CARTESIAN_POINT('Ctrl Pts',(-0.1988959100457,1.76069879610132,12.3110954235557));
#35614=CARTESIAN_POINT('Ctrl Pts',(-0.181110285449925,1.75027299168607,
12.3121363465845));
#35615=CARTESIAN_POINT('Ctrl Pts',(-0.162483508710738,1.74123812048123,
12.3131772696134));
#35616=CARTESIAN_POINT('Ctrl Pts',(-0.143259714116111,1.73371930939323,
12.3142181926422));
#35617=CARTESIAN_POINT('Ctrl Pts',(-0.124026046681599,1.72619663683982,
12.315259650262));
#35618=CARTESIAN_POINT('Ctrl Pts',(-0.104195428206946,1.72019186291053,
12.3163011078818));
#35619=CARTESIAN_POINT('Ctrl Pts',(-0.0840318330442134,1.71578190954195,
12.3173425655016));
#35620=CARTESIAN_POINT('Ctrl Pts',(-0.0638620770240899,1.71137060874035,
12.3183843413321));
#35621=CARTESIAN_POINT('Ctrl Pts',(-0.0433598676905176,1.70855522030048,
12.3194261171626));
#35622=CARTESIAN_POINT('Ctrl Pts',(-0.0227982943508453,1.70736132669502,
12.3204678929931));
#35623=CARTESIAN_POINT('Ctrl Pts',(-0.0021922767038096,1.70616485246145,
12.3215119206457));
#35624=CARTESIAN_POINT('Ctrl Pts',(0.018472624810372,1.70659685502673,12.3225559482983));
#35625=CARTESIAN_POINT('Ctrl Pts',(0.0389236722817217,1.70863081657327,
12.3235999759509));
#35626=CARTESIAN_POINT('Ctrl Pts',(0.0461569397051607,1.70935020211163,
12.3239692348468));
#35627=CARTESIAN_POINT('Ctrl Pts',(0.0533635272051451,1.71026951204017,
12.3243384937427));
#35628=CARTESIAN_POINT('Ctrl Pts',(0.0605316949800335,1.71138604772494,
12.3247077526385));
#35629=CARTESIAN_POINT('Ctrl Pts',(0.0807974204426804,1.7145426989596,12.3257517152861));
#35630=CARTESIAN_POINT('Ctrl Pts',(0.100875941008522,1.71929827154436,12.3267956779336));
#35631=CARTESIAN_POINT('Ctrl Pts',(0.120497123297663,1.7256133906281,12.3278396405812));
#35632=CARTESIAN_POINT('Ctrl Pts',(0.140082210307686,1.73191689236979,12.328881682747));
#35633=CARTESIAN_POINT('Ctrl Pts',(0.159210918328371,1.73977407958339,12.3299237249127));
#35634=CARTESIAN_POINT('Ctrl Pts',(0.17762457728834,1.74909488527076,12.3309657670785));
#35635=CARTESIAN_POINT('Ctrl Pts',(0.196018460267855,1.75840568055925,12.3320066901074));
#35636=CARTESIAN_POINT('Ctrl Pts',(0.213698152554131,1.7691766689096,12.3330476131362));
#35637=CARTESIAN_POINT('Ctrl Pts',(0.230426290902619,1.78127031129676,12.3340885361651));
#35638=CARTESIAN_POINT('Ctrl Pts',(0.247163020386969,1.79337016466345,12.3351299937849));
#35639=CARTESIAN_POINT('Ctrl Pts',(0.262946613915361,1.80679361110466,12.3361714514047));
#35640=CARTESIAN_POINT('Ctrl Pts',(0.277569500059795,1.82136033549303,12.3372129090244));
#35641=CARTESIAN_POINT('Ctrl Pts',(0.292196854133464,1.83593151065078,12.3382546848549));
#35642=CARTESIAN_POINT('Ctrl Pts',(0.305662299505186,1.85164611470455,12.3392964606854));
#35643=CARTESIAN_POINT('Ctrl Pts',(0.317796497797404,1.86828837752995,12.3403382365159));
#35644=CARTESIAN_POINT('Ctrl Pts',(0.329956924434584,1.88496661298409,12.3413822641685));
#35645=CARTESIAN_POINT('Ctrl Pts',(0.340779973523657,1.90257588296395,12.3424262918211));
#35646=CARTESIAN_POINT('Ctrl Pts',(0.350140303761709,1.92087250997779,12.3434703194737));
#35647=CARTESIAN_POINT('Ctrl Pts',(0.353450929874014,1.92734378712492,12.3438395783696));
#35648=CARTESIAN_POINT('Ctrl Pts',(0.356579013654895,1.93390085399953,12.3442088372655));
#35649=CARTESIAN_POINT('Ctrl Pts',(0.35952046919734,1.94053237874689,12.3445780961613));
#35650=CARTESIAN_POINT('Ctrl Pts',(0.367836503692704,1.95928091591162,12.3456220588089));
#35651=CARTESIAN_POINT('Ctrl Pts',(0.374706799095974,1.97873757286482,12.3466660214564));
#35652=CARTESIAN_POINT('Ctrl Pts',(0.38001823440743,1.99865390230571,12.347709984104));
#35653=CARTESIAN_POINT('Ctrl Pts',(0.38531989876129,2.0185335935125,12.3487520262698));
#35654=CARTESIAN_POINT('Ctrl Pts',(0.389068150359415,2.03887059111312,12.3497940684355));
#35655=CARTESIAN_POINT('Ctrl Pts',(0.391198696362921,2.05939864578673,12.3508361106013));
#35656=CARTESIAN_POINT('Ctrl Pts',(0.393326954193488,2.0799046536521,12.3518770336302));
#35657=CARTESIAN_POINT('Ctrl Pts',(0.393840851226927,2.10060058608385,12.352917956659));
#35658=CARTESIAN_POINT('Ctrl Pts',(0.392727543724899,2.12121241145669,12.3539588796879));
#35659=CARTESIAN_POINT('Ctrl Pts',(0.391613664457153,2.14183482252585,12.3550003373077));
#35660=CARTESIAN_POINT('Ctrl Pts',(0.388870934719196,2.16237230466497,12.3560417949275));
#35661=CARTESIAN_POINT('Ctrl Pts',(0.384538604533982,2.18255272026443,12.3570832525472));
#35662=CARTESIAN_POINT('Ctrl Pts',(0.380204950633023,2.20273930186065,12.3581250283777));
#35663=CARTESIAN_POINT('Ctrl Pts',(0.374280919069172,2.22256788853888,12.3591668042082));
#35664=CARTESIAN_POINT('Ctrl Pts',(0.366856267302736,2.24177929729232,12.3602085800387));
#35665=CARTESIAN_POINT('Ctrl Pts',(0.35941556698302,2.26103223194173,12.3612526076913));
#35666=CARTESIAN_POINT('Ctrl Pts',(0.350468089532821,2.27966466141527,12.3622966353439));
#35667=CARTESIAN_POINT('Ctrl Pts',(0.340150873838033,2.29743928947204,12.3633406629965));
#35668=CARTESIAN_POINT('Ctrl Pts',(0.336501809882322,2.30372594243024,12.3637099218924));
#35669=CARTESIAN_POINT('Ctrl Pts',(0.332681798925405,2.30990555005749,12.3640791807883));
#35670=CARTESIAN_POINT('Ctrl Pts',(0.328698157218337,2.31596854271229,12.3644484396841));
#35671=CARTESIAN_POINT('Ctrl Pts',(0.317435671222777,2.3331097353413,12.3654924023317));
#35672=CARTESIAN_POINT('Ctrl Pts',(0.304795180737228,2.34941864269302,12.3665363649792));
#35673=CARTESIAN_POINT('Ctrl Pts',(0.290924350259353,2.36466566159246,12.3675803276268));
#35674=CARTESIAN_POINT('Ctrl Pts',(0.277079036668816,2.37988463195767,12.3686223697926));
#35675=CARTESIAN_POINT('Ctrl Pts',(0.262008321281486,2.39404501327894,12.3696644119583));
#35676=CARTESIAN_POINT('Ctrl Pts',(0.245901268417969,2.40694862141804,12.3707064541241));
#35677=CARTESIAN_POINT('Ctrl Pts',(0.229811514276188,2.41983837128471,12.371747377153));
#35678=CARTESIAN_POINT('Ctrl Pts',(0.212688185489378,2.43147354728851,12.3727883001818));
#35679=CARTESIAN_POINT('Ctrl Pts',(0.194754740206817,2.4416950119141,12.3738292232107));
#35680=CARTESIAN_POINT('Ctrl Pts',(0.176812084774155,2.45192172601751,12.3748706808305));
#35681=CARTESIAN_POINT('Ctrl Pts',(0.158059112915481,2.46073289991761,12.3759121384503));
#35682=CARTESIAN_POINT('Ctrl Pts',(0.138745889552052,2.46801422273115,12.37695359607));
#35683=CARTESIAN_POINT('Ctrl Pts',(0.119426765156904,2.47529777030624,12.3779953719005));
#35684=CARTESIAN_POINT('Ctrl Pts',(0.0995477491332538,2.48105031074997,
12.379037147731));
#35685=CARTESIAN_POINT('Ctrl Pts',(0.0793753545288147,2.4852070132973,12.3800789235615));
#35686=CARTESIAN_POINT('Ctrl Pts',(0.0591593568356653,2.48937270065151,
12.3811229512141));
#35687=CARTESIAN_POINT('Ctrl Pts',(0.0386494453176911,2.49193557215298,
12.3821669788667));
#35688=CARTESIAN_POINT('Ctrl Pts',(0.0181193245279482,2.49288239980769,
12.3832110065193));
#35689=CARTESIAN_POINT('Ctrl Pts',(0.0108580899083783,2.49321728033838,
12.3835802654152));
#35690=CARTESIAN_POINT('Ctrl Pts',(0.00359432421909314,2.49335047999792,
12.3839495243111));
#35691=CARTESIAN_POINT('Ctrl Pts',(-0.00365996579511119,2.49328297020133,
12.3843187832069));
#35692=CARTESIAN_POINT('Ctrl Pts',(-0.0241691746296765,2.49309210762017,
12.3853627458545));
#35693=CARTESIAN_POINT('Ctrl Pts',(-0.0447245218309344,2.49129206313246,
12.386406708502));
#35694=CARTESIAN_POINT('Ctrl Pts',(-0.0650530194777359,2.48788270734441,
12.3874506711496));
#35695=CARTESIAN_POINT('Ctrl Pts',(-0.0853441206626011,2.48447962343371,
12.3884927133154));
#35696=CARTESIAN_POINT('Ctrl Pts',(-0.105408473360152,2.47947316637522,
12.3895347554811));
#35697=CARTESIAN_POINT('Ctrl Pts',(-0.124977096865666,2.47291502417981,
12.3905767976469));
#35698=CARTESIAN_POINT('Ctrl Pts',(-0.144524703976956,2.46636392532609,
12.3916177206758));
#35699=CARTESIAN_POINT('Ctrl Pts',(-0.163576935552843,2.45826465490463,
12.3926586437046));
#35700=CARTESIAN_POINT('Ctrl Pts',(-0.181879023987313,2.44871895651573,
12.3936995667335));
#35701=CARTESIAN_POINT('Ctrl Pts',(-0.200190511897392,2.43916835570493,
12.3947410243533));
#35702=CARTESIAN_POINT('Ctrl Pts',(-0.217750427183038,2.42817016884568,
12.395782481973));
#35703=CARTESIAN_POINT('Ctrl Pts',(-0.234327290546682,2.41587277645446,
12.3968239395928));
#35704=CARTESIAN_POINT('Ctrl Pts',(-0.250909218864775,2.40357162667374,
12.3978657154233));
#35705=CARTESIAN_POINT('Ctrl Pts',(-0.266506928430191,2.38997094816352,
12.3989074912538));
#35706=CARTESIAN_POINT('Ctrl Pts',(-0.280921640046613,2.37525973580152,
12.3999492670843));
#35707=CARTESIAN_POINT('Ctrl Pts',(-0.295367509389291,2.36051672482017,
12.4009932947369));
#35708=CARTESIAN_POINT('Ctrl Pts',(-0.308624803329615,2.34465895265043,
12.4020373223895));
#35709=CARTESIAN_POINT('Ctrl Pts',(-0.320534238313284,2.32790939442884,
12.4030813500421));
#35710=CARTESIAN_POINT('Ctrl Pts',(-0.324746449361074,2.32198529523495,
12.403450608938));
#35711=CARTESIAN_POINT('Ctrl Pts',(-0.328790453635197,2.31594989437262,
12.4038198678338));
#35712=CARTESIAN_POINT('Ctrl Pts',(-0.332660568450896,2.30981381317236,
12.4041891267297));
#35713=CARTESIAN_POINT('Ctrl Pts',(-0.343883239717833,2.29202022681716,
12.4052599143931));
#35714=CARTESIAN_POINT('Ctrl Pts',(-0.353704393768988,2.27327671702817,
12.4063307020566));
#35715=CARTESIAN_POINT('Ctrl Pts',(-0.361970923399411,2.25382438237606,
12.40740148972));
#35716=CARTESIAN_POINT('Ctrl Pts',(-0.370218634500474,2.23441633043353,
12.4084698397645));
#35717=CARTESIAN_POINT('Ctrl Pts',(-0.376918430054792,2.21430325676297,
12.409538189809));
#35718=CARTESIAN_POINT('Ctrl Pts',(-0.381962909938574,2.19375086896268,
12.4106065398535));
#35719=CARTESIAN_POINT('Ctrl Pts',(-0.386997980238035,2.17323681800393,
12.4116728970801));
#35720=CARTESIAN_POINT('Ctrl Pts',(-0.390383670121265,2.15228573180286,
12.4127392543067));
#35721=CARTESIAN_POINT('Ctrl Pts',(-0.392062200302088,2.13117885652627,
12.4138056115333));
#35722=CARTESIAN_POINT('Ctrl Pts',(-0.392890184717364,2.12076726906489,
12.414331623621));
#35723=CARTESIAN_POINT('Ctrl Pts',(-0.393303551202367,2.1103179756868,12.4148576357088));
#35724=CARTESIAN_POINT('Ctrl Pts',(-0.393299977006061,2.09986551196329,
12.4153836477965));
#35725=CARTESIAN_POINT('',(-0.393390187309037,2.09970304505391,12.5403836071275));
#35726=CARTESIAN_POINT('Ctrl Pts',(-0.392695458149876,2.09986380011846,
12.4153837444951));
#35727=CARTESIAN_POINT('Ctrl Pts',(-0.392870617776604,2.04248652105401,
12.4182756530809));
#35728=CARTESIAN_POINT('Ctrl Pts',(-0.354200996982992,1.85392122723629,
12.4277910095078));
#35729=CARTESIAN_POINT('Ctrl Pts',(-0.0630108380886311,1.63923468580215,
12.4439298137753));
#35730=CARTESIAN_POINT('Ctrl Pts',(0.353310820705713,1.79759876908859,12.4638001572982));
#35731=CARTESIAN_POINT('Ctrl Pts',(0.445517900427544,2.23337481352617,12.4836705008209));
#35732=CARTESIAN_POINT('Ctrl Pts',(0.129022958292381,2.5467976238947,12.5035408443436));
#35733=CARTESIAN_POINT('Ctrl Pts',(-0.284692123815817,2.45503358678244,
12.5224451756817));
#35734=CARTESIAN_POINT('Ctrl Pts',(-0.392699784792383,2.21126854754101,
12.534726059179));
#35735=CARTESIAN_POINT('Ctrl Pts',(-0.393639516850345,2.09970507070382,
12.5403834948351));
#35736=CARTESIAN_POINT('',(-0.393391798196894,2.10029574838795,12.6653836890739));
#35737=CARTESIAN_POINT('Ctrl Pts',(-0.393299887339814,2.09970231142193,
12.5403836477965));
#35738=CARTESIAN_POINT('Ctrl Pts',(-0.3932854820339,2.08067032426963,12.5413496089941));
#35739=CARTESIAN_POINT('Ctrl Pts',(-0.391889466207624,2.06168959049348,
12.5423155701917));
#35740=CARTESIAN_POINT('Ctrl Pts',(-0.389134880197745,2.04291291727994,
12.5432815313893));
#35741=CARTESIAN_POINT('Ctrl Pts',(-0.386157861130145,2.02262002608602,
12.5443254940369));
#35742=CARTESIAN_POINT('Ctrl Pts',(-0.381580325228403,2.00250016963069,
12.5453694566844));
#35743=CARTESIAN_POINT('Ctrl Pts',(-0.375439253030338,1.9828238194682,12.546413419332));
#35744=CARTESIAN_POINT('Ctrl Pts',(-0.369309477996323,1.96318366607209,
12.5474554614977));
#35745=CARTESIAN_POINT('Ctrl Pts',(-0.36162203596023,1.94398611163449,12.5484975036635));
#35746=CARTESIAN_POINT('Ctrl Pts',(-0.352464699157093,1.92549061386819,
12.5495395458292));
#35747=CARTESIAN_POINT('Ctrl Pts',(-0.343317197189826,1.90701497997595,
12.5505804688581));
#35748=CARTESIAN_POINT('Ctrl Pts',(-0.332703233336234,1.88924057476259,
12.5516213918869));
#35749=CARTESIAN_POINT('Ctrl Pts',(-0.320758238726044,1.87240597044438,
12.5526623149158));
#35750=CARTESIAN_POINT('Ctrl Pts',(-0.308807109477952,1.85556272031216,
12.5537037725355));
#35751=CARTESIAN_POINT('Ctrl Pts',(-0.295523996459302,1.83966084471345,
12.5547452301553));
#35752=CARTESIAN_POINT('Ctrl Pts',(-0.281087369111873,1.82490950411589,
12.5557866877751));
#35753=CARTESIAN_POINT('Ctrl Pts',(-0.266646330745397,1.81015365634067,
12.5568284636056));
#35754=CARTESIAN_POINT('Ctrl Pts',(-0.251051616466253,1.79654954350039,
12.557870239436));
#35755=CARTESIAN_POINT('Ctrl Pts',(-0.234517487980402,1.78426840856297,
12.5589120152665));
#35756=CARTESIAN_POINT('Ctrl Pts',(-0.21794762060063,1.77196072767368,12.5599560429191));
#35757=CARTESIAN_POINT('Ctrl Pts',(-0.200434909090465,1.76098212501383,
12.5610000705717));
#35758=CARTESIAN_POINT('Ctrl Pts',(-0.182221911142592,1.75146009539862,
12.5620440982243));
#35759=CARTESIAN_POINT('Ctrl Pts',(-0.17578021249898,1.74809227833564,12.5624133571202));
#35760=CARTESIAN_POINT('Ctrl Pts',(-0.169251110582697,1.74490623654066,
12.5627826160161));
#35761=CARTESIAN_POINT('Ctrl Pts',(-0.162645900612064,1.74190615613489,
12.563151874912));
#35762=CARTESIAN_POINT('Ctrl Pts',(-0.143971760151691,1.73342437839599,
12.5641958375595));
#35763=CARTESIAN_POINT('Ctrl Pts',(-0.124576721715779,1.72638201069807,
12.5652398002071));
#35764=CARTESIAN_POINT('Ctrl Pts',(-0.104708220863087,1.72089437028226,
12.5662837628547));
#35765=CARTESIAN_POINT('Ctrl Pts',(-0.0848762702586617,1.71541682497231,
12.5673258050204));
#35766=CARTESIAN_POINT('Ctrl Pts',(-0.0645732714895317,1.71148858078031,
12.5683678471862));
#35767=CARTESIAN_POINT('Ctrl Pts',(-0.0440648939428253,1.70917628638757,
12.569409889352));
#35768=CARTESIAN_POINT('Ctrl Pts',(-0.0235785420714202,1.70686647536269,
12.5704508123808));
#35769=CARTESIAN_POINT('Ctrl Pts',(-0.00288797351194347,1.70616927950223,
12.5714917354097));
#35770=CARTESIAN_POINT('Ctrl Pts',(0.0177329046270695,1.70709996933891,
12.5725326584386));
#35771=CARTESIAN_POINT('Ctrl Pts',(0.038364373111642,1.70803113715363,12.5735741160583));
#35772=CARTESIAN_POINT('Ctrl Pts',(0.0589253439161157,1.71059184381556,
12.5746155736781));
#35773=CARTESIAN_POINT('Ctrl Pts',(0.0791433424408346,1.71474525136308,
12.5756570312979));
#35774=CARTESIAN_POINT('Ctrl Pts',(0.0993675184455364,1.71889992795769,
12.5766988071285));
#35775=CARTESIAN_POINT('Ctrl Pts',(0.119247800712942,1.72464809084637,12.577740582959));
#35776=CARTESIAN_POINT('Ctrl Pts',(0.138524221356739,1.73190228186321,12.5787823587895));
#35777=CARTESIAN_POINT('Ctrl Pts',(0.157842308421191,1.73917215297855,12.5798263864421));
#35778=CARTESIAN_POINT('Ctrl Pts',(0.176553261277886,1.7479542383803,12.5808704140947));
#35779=CARTESIAN_POINT('Ctrl Pts',(0.194418579141684,1.75811360646477,12.5819144417473));
#35780=CARTESIAN_POINT('Ctrl Pts',(0.200737307895772,1.76170684178966,12.5822837006431));
#35781=CARTESIAN_POINT('Ctrl Pts',(0.206950509720769,1.76547196558809,12.582652959539));
#35782=CARTESIAN_POINT('Ctrl Pts',(0.213048550545228,1.76940174666133,12.5830222184349));
#35783=CARTESIAN_POINT('Ctrl Pts',(0.230288830780609,1.78051195876333,12.5840661810824));
#35784=CARTESIAN_POINT('Ctrl Pts',(0.246709064381734,1.79300749345407,12.58511014373));
#35785=CARTESIAN_POINT('Ctrl Pts',(0.262078349208762,1.80674272579182,12.5861541063775));
#35786=CARTESIAN_POINT('Ctrl Pts',(0.277419360580215,1.82045269068964,12.5871961485433));
#35787=CARTESIAN_POINT('Ctrl Pts',(0.291712678715274,1.8353973860074,12.5882381907091));
#35788=CARTESIAN_POINT('Ctrl Pts',(0.30475845256979,1.85138951030323,12.5892802328748));
#35789=CARTESIAN_POINT('Ctrl Pts',(0.317790215468133,1.8673644593088,12.5903211559037));
#35790=CARTESIAN_POINT('Ctrl Pts',(0.329576608846557,1.88438405508869,12.5913620789325));
#35791=CARTESIAN_POINT('Ctrl Pts',(0.339956522100723,1.90222625785717,12.5924030019614));
#35792=CARTESIAN_POINT('Ctrl Pts',(0.350341766207803,1.92007762391596,12.5934444595812));
#35793=CARTESIAN_POINT('Ctrl Pts',(0.359318703208209,1.93875181308501,12.594485917201));
#35794=CARTESIAN_POINT('Ctrl Pts',(0.366770811695528,1.95799978278818,12.5955273748208));
#35795=CARTESIAN_POINT('Ctrl Pts',(0.374225197126873,1.97725363358524,12.5965691506513));
#35796=CARTESIAN_POINT('Ctrl Pts',(0.38015359485801,1.99708091529422,12.5976109264818));
#35797=CARTESIAN_POINT('Ctrl Pts',(0.384488815966542,2.01721569957627,12.5986527023123));
#35798=CARTESIAN_POINT('Ctrl Pts',(0.388833407753879,2.03739400565147,12.5996967299648));
#35799=CARTESIAN_POINT('Ctrl Pts',(0.39157784997706,2.05788041133163,12.6007407576174));
#35800=CARTESIAN_POINT('Ctrl Pts',(0.39270649075991,2.07840133997127,12.60178478527));
#35801=CARTESIAN_POINT('Ctrl Pts',(0.393105676210853,2.08565932344772,12.6021540441659));
#35802=CARTESIAN_POINT('Ctrl Pts',(0.393303211122216,2.09292162432936,12.6025233030618));
#35803=CARTESIAN_POINT('Ctrl Pts',(0.393299960518412,2.10017622773788,12.6028925619576));
#35804=CARTESIAN_POINT('Ctrl Pts',(0.39329077046506,2.12068632259594,12.6039365246052));
#35805=CARTESIAN_POINT('Ctrl Pts',(0.391672870315327,2.14125680770998,12.6049804872527));
#35806=CARTESIAN_POINT('Ctrl Pts',(0.388443712627104,2.16161470701441,12.6060244499003));
#35807=CARTESIAN_POINT('Ctrl Pts',(0.385220495322409,2.18193515576939,12.607066492066));
#35808=CARTESIAN_POINT('Ctrl Pts',(0.380391959294063,2.2020430671794,12.6081085342318));
#35809=CARTESIAN_POINT('Ctrl Pts',(0.37400740796664,2.22166901325348,12.6091505763976));
#35810=CARTESIAN_POINT('Ctrl Pts',(0.367629713547045,2.24127388136979,12.6101914994264));
#35811=CARTESIAN_POINT('Ctrl Pts',(0.359699520392321,2.26039710667069,12.6112324224553));
#35812=CARTESIAN_POINT('Ctrl Pts',(0.350316311448575,2.27878303032745,12.6122733454842));
#35813=CARTESIAN_POINT('Ctrl Pts',(0.340928283533272,2.2971783965154,12.6133148031039));
#35814=CARTESIAN_POINT('Ctrl Pts',(0.330086069131397,2.31483504189024,12.6143562607237));
#35815=CARTESIAN_POINT('Ctrl Pts',(0.317935992557206,2.33152018192085,12.6153977183435));
#35816=CARTESIAN_POINT('Ctrl Pts',(0.305782203604921,2.34821041998915,12.616439494174));
#35817=CARTESIAN_POINT('Ctrl Pts',(0.292320218959994,2.36392798879112,12.6174812700045));
#35818=CARTESIAN_POINT('Ctrl Pts',(0.277737265353293,2.37847244286298,12.618523045835));
#35819=CARTESIAN_POINT('Ctrl Pts',(0.263122790361445,2.39304833510237,12.6195670734876));
#35820=CARTESIAN_POINT('Ctrl Pts',(0.247383069833464,2.4064455728217,12.6206111011402));
#35821=CARTESIAN_POINT('Ctrl Pts',(0.23073965926772,2.41850290366183,12.6216551287928));
#35822=CARTESIAN_POINT('Ctrl Pts',(0.224853103108243,2.42276742353553,12.6220243876887));
#35823=CARTESIAN_POINT('Ctrl Pts',(0.218853759716514,2.42686472911455,12.6223936465846));
#35824=CARTESIAN_POINT('Ctrl Pts',(0.212752199670672,2.43078904385619,12.6227629054804));
#35825=CARTESIAN_POINT('Ctrl Pts',(0.195501969951427,2.44188380163538,12.623806868128));
#35826=CARTESIAN_POINT('Ctrl Pts',(0.177330139180993,2.4516586174993,12.6248508307755));
#35827=CARTESIAN_POINT('Ctrl Pts',(0.158464851546329,2.45996358263636,12.6258947934231));
#35828=CARTESIAN_POINT('Ctrl Pts',(0.13963426864112,2.46825326989513,12.6269368355889));
#35829=CARTESIAN_POINT('Ctrl Pts',(0.120113402909539,2.47507812612367,12.6279788777546));
#35830=CARTESIAN_POINT('Ctrl Pts',(0.100155483064891,2.48033376028436,12.6290209199204));
#35831=CARTESIAN_POINT('Ctrl Pts',(0.080218997712619,2.48558374997652,12.6300618429493));
#35832=CARTESIAN_POINT('Ctrl Pts',(0.0598470906458656,2.48926764897692,
12.6311027659781));
#35833=CARTESIAN_POINT('Ctrl Pts',(0.039308576301513,2.49133071158439,12.632143689007));
#35834=CARTESIAN_POINT('Ctrl Pts',(0.018759513911499,2.49339483372705,12.6331851466268));
#35835=CARTESIAN_POINT('Ctrl Pts',(-0.00195559621317298,2.4938363669115,
12.6342266042466));
#35836=CARTESIAN_POINT('Ctrl Pts',(-0.0225618166756512,2.49265233276818,
12.6352680618664));
#35837=CARTESIAN_POINT('Ctrl Pts',(-0.0431743332368318,2.49146793685081,
12.6363098376969));
#35838=CARTESIAN_POINT('Ctrl Pts',(-0.0636771620298553,2.48865706312374,
12.6373516135274));
#35839=CARTESIAN_POINT('Ctrl Pts',(-0.0838004157075394,2.4842686304231,
12.6383933893579));
#35840=CARTESIAN_POINT('Ctrl Pts',(-0.103967166254713,2.47987071202559,
12.6394374170105));
#35841=CARTESIAN_POINT('Ctrl Pts',(-0.123751998718944,2.47388864004582,
12.640481444663));
#35842=CARTESIAN_POINT('Ctrl Pts',(-0.142899397235013,2.466421413498,12.6415254723156));
#35843=CARTESIAN_POINT('Ctrl Pts',(-0.14967158111068,2.46378035334663,12.6418947312115));
#35844=CARTESIAN_POINT('Ctrl Pts',(-0.156364221980266,2.46095394355193,
12.6422639901074));
#35845=CARTESIAN_POINT('Ctrl Pts',(-0.162966740778297,2.45794794509831,
12.6426332490032));
#35846=CARTESIAN_POINT('Ctrl Pts',(-0.181633272802725,2.44944943595106,
12.6436772116508));
#35847=CARTESIAN_POINT('Ctrl Pts',(-0.199688853333332,2.43946151973071,
12.6447211742983));
#35848=CARTESIAN_POINT('Ctrl Pts',(-0.216883937786604,2.42809487580603,
12.6457651369459));
#35849=CARTESIAN_POINT('Ctrl Pts',(-0.234047390029146,2.41674914204768,
12.6468071791117));
#35850=CARTESIAN_POINT('Ctrl Pts',(-0.250352848681105,2.40403006662534,
12.6478492212774));
#35851=CARTESIAN_POINT('Ctrl Pts',(-0.265575462610926,2.39009406002018,
12.6488912634432));
#35852=CARTESIAN_POINT('Ctrl Pts',(-0.280781727692532,2.37617302046718,
12.6499321864721));
#35853=CARTESIAN_POINT('Ctrl Pts',(-0.294906897322246,2.36103811735178,
12.6509731095009));
#35854=CARTESIAN_POINT('Ctrl Pts',(-0.307759426222471,2.34488573982822,
12.6520140325298));
#35855=CARTESIAN_POINT('Ctrl Pts',(-0.320618555846558,2.32872506686456,
12.6530554901495));
#35856=CARTESIAN_POINT('Ctrl Pts',(-0.332203268262198,2.31154644127121,
12.6540969477693));
#35857=CARTESIAN_POINT('Ctrl Pts',(-0.342362230622209,2.29357942308878,
12.6551384053891));
#35858=CARTESIAN_POINT('Ctrl Pts',(-0.35252429698812,2.27560691519899,12.6561801812196));
#35859=CARTESIAN_POINT('Ctrl Pts',(-0.361259415719716,2.25684619292158,
12.6572219570501));
#35860=CARTESIAN_POINT('Ctrl Pts',(-0.368462623752698,2.23755066302013,
12.6582637328806));
#35861=CARTESIAN_POINT('Ctrl Pts',(-0.375681401683303,2.21821342539294,
12.6593077605332));
#35862=CARTESIAN_POINT('Ctrl Pts',(-0.381361455759539,2.19833978036997,
12.6603517881858));
#35863=CARTESIAN_POINT('Ctrl Pts',(-0.385447710770332,2.17819816022075,
12.6613958158384));
#35864=CARTESIAN_POINT('Ctrl Pts',(-0.386892965606033,2.17107433318533,
12.6617650747343));
#35865=CARTESIAN_POINT('Ctrl Pts',(-0.388139317076599,2.1639170542226,12.6621343336301));
#35866=CARTESIAN_POINT('Ctrl Pts',(-0.389185882481578,2.15673833692518,
12.662503592526));
#35867=CARTESIAN_POINT('Ctrl Pts',(-0.391906797485739,2.13807473547968,
12.6634636109495));
#35868=CARTESIAN_POINT('Ctrl Pts',(-0.393285629476647,2.1192108351539,12.664423629373));
#35869=CARTESIAN_POINT('Ctrl Pts',(-0.393299888242884,2.10029649306013,
12.6653836477965));
#35870=CARTESIAN_POINT('',(-0.393077839436675,2.10013693750963,12.7903836117785));
#35871=CARTESIAN_POINT('Ctrl Pts',(-0.393642737751318,2.10029371522729,
12.6653838017726));
#35872=CARTESIAN_POINT('Ctrl Pts',(-0.392704612486157,1.98861543350834,
12.6710471798646));
#35873=CARTESIAN_POINT('Ctrl Pts',(-0.284503920525053,1.74474015797601,
12.6833340057978));
#35874=CARTESIAN_POINT('Ctrl Pts',(0.129423303771996,1.6533181793209,12.7022442795714));
#35875=CARTESIAN_POINT('Ctrl Pts',(0.445637245252665,1.9670244904942,12.7221146230944));
#35876=CARTESIAN_POINT('Ctrl Pts',(0.353039682245798,2.40271772865816,12.7419849666171));
#35877=CARTESIAN_POINT('Ctrl Pts',(-0.0634237272071889,2.56070866207559,
12.7618553101399));
#35878=CARTESIAN_POINT('Ctrl Pts',(-0.354314217530218,2.34584041188345,
12.7779881712589));
#35879=CARTESIAN_POINT('Ctrl Pts',(-0.39287385494239,2.15739695435976,12.787497584537));
#35880=CARTESIAN_POINT('Ctrl Pts',(-0.392696668310428,2.10013803163933,
12.7903835499741));
#35881=CARTESIAN_POINT('',(-0.393299839860298,2.09964508330049,12.9153836477965));
#35882=CARTESIAN_POINT('Ctrl Pts',(-0.393299976382332,2.10013629987835,
12.7903836477965));
#35883=CARTESIAN_POINT('Ctrl Pts',(-0.393307320618343,2.07894414707162,
12.7914501378907));
#35884=CARTESIAN_POINT('Ctrl Pts',(-0.391597482747587,2.0577651672122,12.7925166279849));
#35885=CARTESIAN_POINT('Ctrl Pts',(-0.388202863252538,2.03688560415776,
12.7935831180791));
#35886=CARTESIAN_POINT('Ctrl Pts',(-0.384805099452868,2.01598670117238,
12.7946505960218));
#35887=CARTESIAN_POINT('Ctrl Pts',(-0.379719606119362,1.99538843537396,
12.7957180739645));
#35888=CARTESIAN_POINT('Ctrl Pts',(-0.373029699516558,1.97536560154361,
12.7967855519072));
#35889=CARTESIAN_POINT('Ctrl Pts',(-0.366320071011017,1.95528374022532,
12.7978561767842));
#35890=CARTESIAN_POINT('Ctrl Pts',(-0.357996851840173,1.93578133184653,
12.7989268016611));
#35891=CARTESIAN_POINT('Ctrl Pts',(-0.348191675533187,1.9171135677821,12.799997426538));
#35892=CARTESIAN_POINT('Ctrl Pts',(-0.34331157626416,1.90782250162348,12.8005302834205));
#35893=CARTESIAN_POINT('Ctrl Pts',(-0.338065089716678,1.89873778525007,
12.8010631403031));
#35894=CARTESIAN_POINT('Ctrl Pts',(-0.332472410414027,1.8898881576077,12.8015959971856));
#35895=CARTESIAN_POINT('Ctrl Pts',(-0.321515343921992,1.87255014245255,
12.8026399598332));
#35896=CARTESIAN_POINT('Ctrl Pts',(-0.309165745435914,1.85601987094724,
12.8036839224809));
#35897=CARTESIAN_POINT('Ctrl Pts',(-0.295567188915755,1.84052952607967,
12.8047278851286));
#35898=CARTESIAN_POINT('Ctrl Pts',(-0.281993648405637,1.82506767737067,
12.8057699272944));
#35899=CARTESIAN_POINT('Ctrl Pts',(-0.267176145730319,1.81064254388779,
12.8068119694603));
#35900=CARTESIAN_POINT('Ctrl Pts',(-0.25130020475716,1.79745562790062,12.8078540116262));
#35901=CARTESIAN_POINT('Ctrl Pts',(-0.235441314295202,1.78428287445405,
12.8088949346552));
#35902=CARTESIAN_POINT('Ctrl Pts',(-0.21852678689345,1.77234618847189,12.8099358576841));
#35903=CARTESIAN_POINT('Ctrl Pts',(-0.200777226552667,1.76180864100658,
12.8109767807131));
#35904=CARTESIAN_POINT('Ctrl Pts',(-0.183018550500336,1.75126568173155,
12.812018238333));
#35905=CARTESIAN_POINT('Ctrl Pts',(-0.164424609212882,1.74212368596976,
12.8130596959529));
#35906=CARTESIAN_POINT('Ctrl Pts',(-0.145243403381224,1.73450137650842,
12.8141011535728));
#35907=CARTESIAN_POINT('Ctrl Pts',(-0.126056336854973,1.72687673809925,
12.8151429294034));
#35908=CARTESIAN_POINT('Ctrl Pts',(-0.106282345125238,1.72077294822902,
12.816184705234));
#35909=CARTESIAN_POINT('Ctrl Pts',(-0.0861867509570695,1.71625954870582,
12.8172264810646));
#35910=CARTESIAN_POINT('Ctrl Pts',(-0.066047719706139,1.71173639336713,
12.8182705087173));
#35911=CARTESIAN_POINT('Ctrl Pts',(-0.0455864272438703,1.70881059575511,
12.81931453637));
#35912=CARTESIAN_POINT('Ctrl Pts',(-0.0250763008431699,1.70750023040004,
12.8203585640227));
#35913=CARTESIAN_POINT('Ctrl Pts',(-0.0178221379903036,1.70703677135075,
12.8207278229179));
#35914=CARTESIAN_POINT('Ctrl Pts',(-0.0105618717355667,1.70677491668709,
12.8210970818131));
#35915=CARTESIAN_POINT('Ctrl Pts',(-0.00330752414799727,1.70671390784314,
12.8214663407083));
#35916=CARTESIAN_POINT('Ctrl Pts',(0.0172018474903776,1.70654142464756,
12.8225103033557));
#35917=CARTESIAN_POINT('Ctrl Pts',(0.0377858565357733,1.70797705351697,
12.8235542660032));
#35918=CARTESIAN_POINT('Ctrl Pts',(0.0581715601962042,1.71102575974193,
12.8245982286506));
#35919=CARTESIAN_POINT('Ctrl Pts',(0.0785197621580826,1.71406885754328,
12.8256402708162));
#35920=CARTESIAN_POINT('Ctrl Pts',(0.0986696545932957,1.71871909368904,
12.8266823129819));
#35921=CARTESIAN_POINT('Ctrl Pts',(0.118351383364296,1.72492955320932,12.8277243551475));
#35922=CARTESIAN_POINT('Ctrl Pts',(0.138011974267798,1.73113334279365,12.8287652781763));
#35923=CARTESIAN_POINT('Ctrl Pts',(0.157204692866169,1.73889383646972,12.829806201205));
#35924=CARTESIAN_POINT('Ctrl Pts',(0.175673009167233,1.74811381975115,12.8308471242337));
#35925=CARTESIAN_POINT('Ctrl Pts',(0.194150810314275,1.75733853817572,12.8318885818534));
#35926=CARTESIAN_POINT('Ctrl Pts',(0.211902800420434,1.76802392942791,12.8329300394731));
#35927=CARTESIAN_POINT('Ctrl Pts',(0.22869490798557,1.78002573687643,12.8339714970928));
#35928=CARTESIAN_POINT('Ctrl Pts',(0.245492146271674,1.79203121140039,12.8350132729231));
#35929=CARTESIAN_POINT('Ctrl Pts',(0.261328341094543,1.80535344593764,12.8360550487535));
#35930=CARTESIAN_POINT('Ctrl Pts',(0.27600139645014,1.81980699659418,12.8370968245839));
#35931=CARTESIAN_POINT('Ctrl Pts',(0.290706167947926,1.83429178892853,12.8381408522364));
#35932=CARTESIAN_POINT('Ctrl Pts',(0.304242298286553,1.84991222285872,12.8391848798889));
#35933=CARTESIAN_POINT('Ctrl Pts',(0.316446578954081,1.86644817990806,12.8402289075414));
#35934=CARTESIAN_POINT('Ctrl Pts',(0.320763073064432,1.87229673117929,12.840598166438));
#35935=CARTESIAN_POINT('Ctrl Pts',(0.324913358478234,1.87825954639764,12.8409674253346));
#35936=CARTESIAN_POINT('Ctrl Pts',(0.328891565248036,1.88432610656666,12.8413366842311));
#35937=CARTESIAN_POINT('Ctrl Pts',(0.340138685655048,1.90147738517673,12.8423806468785));
#35938=CARTESIAN_POINT('Ctrl Pts',(0.350074079222775,1.91956192037248,12.843424609526));
#35939=CARTESIAN_POINT('Ctrl Pts',(0.358545822180928,1.93835290476905,12.8444685721734));
#35940=CARTESIAN_POINT('Ctrl Pts',(0.367001980455002,1.95710932112493,12.845510614339));
#35941=CARTESIAN_POINT('Ctrl Pts',(0.373999479504436,1.97656896830518,12.8465526565046));
#35942=CARTESIAN_POINT('Ctrl Pts',(0.37943168935525,1.99647955219851,12.8475946986702));
#35943=CARTESIAN_POINT('Ctrl Pts',(0.384858065098019,2.01636875243751,12.8486356216989));
#35944=CARTESIAN_POINT('Ctrl Pts',(0.388722268436086,2.03670722931816,12.8496765447276));
#35945=CARTESIAN_POINT('Ctrl Pts',(0.39096717473016,2.05722666387203,12.8507174677563));
#35946=CARTESIAN_POINT('Ctrl Pts',(0.393213233949594,2.07775663667264,12.851758925376));
#35947=CARTESIAN_POINT('Ctrl Pts',(0.393838238672249,2.09846702314922,12.8528003829956));
#35948=CARTESIAN_POINT('Ctrl Pts',(0.392836775324064,2.11908292307251,12.8538418406152));
#35949=CARTESIAN_POINT('Ctrl Pts',(0.391835005985166,2.13970512205198,12.8548836164456));
#35950=CARTESIAN_POINT('Ctrl Pts',(0.389205851059815,2.1602320444683,12.8559253922759));
#35951=CARTESIAN_POINT('Ctrl Pts',(0.384995836875683,2.18039338025231,12.8569671681063));
#35952=CARTESIAN_POINT('Ctrl Pts',(0.38077672265035,2.20059829522116,12.8580111957587));
#35953=CARTESIAN_POINT('Ctrl Pts',(0.374970134062881,2.22043533909527,12.8590552234111));
#35954=CARTESIAN_POINT('Ctrl Pts',(0.367672802953046,2.23964812912693,12.8600992510636));
#35955=CARTESIAN_POINT('Ctrl Pts',(0.365091832584362,2.24644344114239,12.8604685099604));
#35956=CARTESIAN_POINT('Ctrl Pts',(0.36232481527227,2.25316085504905,12.8608377688571));
#35957=CARTESIAN_POINT('Ctrl Pts',(0.359377418068716,2.25978974116715,12.8612070277539));
#35958=CARTESIAN_POINT('Ctrl Pts',(0.351044585421646,2.27853081841046,12.8622509904022));
#35959=CARTESIAN_POINT('Ctrl Pts',(0.341216992486097,2.29667416089257,12.8632949530506));
#35960=CARTESIAN_POINT('Ctrl Pts',(0.330003103890568,2.3139692534515,12.8643389156989));
#35961=CARTESIAN_POINT('Ctrl Pts',(0.318809844451445,2.33123252982406,12.8653809578654));
#35962=CARTESIAN_POINT('Ctrl Pts',(0.306235697347738,2.34765001095391,12.866423000032));
#35963=CARTESIAN_POINT('Ctrl Pts',(0.292435075254193,2.36299546908849,12.8674650421985));
#35964=CARTESIAN_POINT('Ctrl Pts',(0.278649274811979,2.37832444644209,12.8685059652281));
#35965=CARTESIAN_POINT('Ctrl Pts',(0.263640082374575,2.39258312282989,12.8695468882577));
#35966=CARTESIAN_POINT('Ctrl Pts',(0.247602182735681,2.40557822092637,12.8705878112874));
#35967=CARTESIAN_POINT('Ctrl Pts',(0.231556046449694,2.41857999296641,12.8716292689079));
#35968=CARTESIAN_POINT('Ctrl Pts',(0.214480709023903,2.43031641454184,12.8726707265285));
#35969=CARTESIAN_POINT('Ctrl Pts',(0.196604381027897,2.44063412536127,12.873712184149));
#35970=CARTESIAN_POINT('Ctrl Pts',(0.178722591034438,2.45095498869111,12.8747539599803));
#35971=CARTESIAN_POINT('Ctrl Pts',(0.160039978057417,2.4598559421548,12.8757957358115));
#35972=CARTESIAN_POINT('Ctrl Pts',(0.140809009184932,2.46722978219687,12.8768375116428));
#35973=CARTESIAN_POINT('Ctrl Pts',(0.121536472137206,2.47461956096137,12.8778815392961));
#35974=CARTESIAN_POINT('Ctrl Pts',(0.10171391913597,2.48047542758616,12.8789255669495));
#35975=CARTESIAN_POINT('Ctrl Pts',(0.0816092840789526,2.48473993132,12.8799695946028));
#35976=CARTESIAN_POINT('Ctrl Pts',(0.0744985382792814,2.48624823037279,
12.8803388534941));
#35977=CARTESIAN_POINT('Ctrl Pts',(0.0673525800331886,2.48755793017658,
12.8807081123853));
#35978=CARTESIAN_POINT('Ctrl Pts',(0.0601834146428161,2.48866804165242,
12.8810773712766));
#35979=CARTESIAN_POINT('Ctrl Pts',(0.0399148685066659,2.49180653050562,
12.8821213339231));
#35980=CARTESIAN_POINT('Ctrl Pts',(0.0193397677068456,2.49336463352435,
12.8831652965696));
#35981=CARTESIAN_POINT('Ctrl Pts',(-0.00127253626072525,2.49329794132625,
12.8842092592161));
#35982=CARTESIAN_POINT('Ctrl Pts',(-0.021846921674124,2.49323137181563,
12.8852513013808));
#35983=CARTESIAN_POINT('Ctrl Pts',(-0.0424576467489466,2.49154588299042,
12.8862933435455));
#35984=CARTESIAN_POINT('Ctrl Pts',(-0.0628309087702101,2.48824884662174,
12.8873353857102));
#35985=CARTESIAN_POINT('Ctrl Pts',(-0.0831822902282565,2.4849553512183,
12.888376308738));
#35986=CARTESIAN_POINT('Ctrl Pts',(-0.103295987665238,2.48005383267414,
12.8894172317658));
#35987=CARTESIAN_POINT('Ctrl Pts',(-0.122904103649506,2.4736033609406,12.8904581547936));
#35988=CARTESIAN_POINT('Ctrl Pts',(-0.142522289851617,2.46714957641273,
12.8914996124124));
#35989=CARTESIAN_POINT('Ctrl Pts',(-0.161633671903684,2.45914546407377,
12.8925410700312));
#35990=CARTESIAN_POINT('Ctrl Pts',(-0.179985767222745,2.44969989075955,
12.89358252765));
#35991=CARTESIAN_POINT('Ctrl Pts',(-0.198343469907265,2.44025143141075,
12.8946243034795));
#35992=CARTESIAN_POINT('Ctrl Pts',(-0.215940786907783,2.4293610028965,12.8956660793089));
#35993=CARTESIAN_POINT('Ctrl Pts',(-0.232550914559593,2.4171828528428,12.8967078551384));
#35994=CARTESIAN_POINT('Ctrl Pts',(-0.249196945379844,2.40497837944097,
12.8977518827901));
#35995=CARTESIAN_POINT('Ctrl Pts',(-0.264850968986824,2.3914811084241,12.8987959104417));
#35996=CARTESIAN_POINT('Ctrl Pts',(-0.279319642300925,2.37688522428054,
12.8998399380933));
#35997=CARTESIAN_POINT('Ctrl Pts',(-0.284437022490672,2.37172285128706,
12.9002091969954));
#35998=CARTESIAN_POINT('Ctrl Pts',(-0.289406478001018,2.3664233656682,12.9005784558974));
#35999=CARTESIAN_POINT('Ctrl Pts',(-0.294220678509066,2.36099632629151,
12.9009477147994));
#36000=CARTESIAN_POINT('Ctrl Pts',(-0.307707358188683,2.34579281709828,
12.9019821703694));
#36001=CARTESIAN_POINT('Ctrl Pts',(-0.320056576268256,2.32949124904495,
12.9030166259395));
#36002=CARTESIAN_POINT('Ctrl Pts',(-0.331086220149197,2.31228943644778,
12.9040510815095));
#36003=CARTESIAN_POINT('Ctrl Pts',(-0.3420960322969,2.29511855338582,12.9050836770877));
#36004=CARTESIAN_POINT('Ctrl Pts',(-0.351790522206156,2.27705122675409,
12.9061162726659));
#36005=CARTESIAN_POINT('Ctrl Pts',(-0.360028444154879,2.2583174323927,12.9071488682442));
#36006=CARTESIAN_POINT('Ctrl Pts',(-0.368257398146856,2.23960403199214,
12.9081803397194));
#36007=CARTESIAN_POINT('Ctrl Pts',(-0.375032603801925,2.22022627634804,
12.9092118111947));
#36008=CARTESIAN_POINT('Ctrl Pts',(-0.380259424142445,2.20043734539929,
12.91024328267));
#36009=CARTESIAN_POINT('Ctrl Pts',(-0.38548888546593,2.18063841559347,12.9112752753222));
#36010=CARTESIAN_POINT('Ctrl Pts',(-0.389168195733384,2.16042861870346,
12.9123072679745));
#36011=CARTESIAN_POINT('Ctrl Pts',(-0.391252958431796,2.14007508600573,
12.9133392606268));
#36012=CARTESIAN_POINT('Ctrl Pts',(-0.39262960328261,2.12663490597684,12.9140207230167));
#36013=CARTESIAN_POINT('Ctrl Pts',(-0.393312010835634,2.11313231187333,
12.9147021854066));
#36014=CARTESIAN_POINT('Ctrl Pts',(-0.393299839860298,2.09964508330049,
12.9153836477965));
#36015=CARTESIAN_POINT('',(-0.393541630724459,2.10004216970008,13.0403836477965));
#36016=CARTESIAN_POINT('Ctrl Pts',(-0.393142733542287,2.09964376269932,
12.9153837217147));
#36017=CARTESIAN_POINT('Ctrl Pts',(-0.393455688614957,2.06380637641479,
12.9171951672506));
#36018=CARTESIAN_POINT('Ctrl Pts',(-0.372521700895207,1.8972908910741,12.9256300606271));
#36019=CARTESIAN_POINT('Ctrl Pts',(-0.136917627666675,1.65555809852058,
12.9406884018452));
#36020=CARTESIAN_POINT('Ctrl Pts',(0.299578723250621,1.74429277563225,12.9605587453678));
#36021=CARTESIAN_POINT('Ctrl Pts',(0.461252377310549,2.15934040607319,12.9804290888907));
#36022=CARTESIAN_POINT('Ctrl Pts',(0.19978977333452,2.5199512921437,13.0002994324134));
#36023=CARTESIAN_POINT('Ctrl Pts',(-0.244952757047327,2.49531403938879,
13.0201697759362));
#36024=CARTESIAN_POINT('Ctrl Pts',(-0.392908567496978,2.23489280799354,
13.0335311810639));
#36025=CARTESIAN_POINT('Ctrl Pts',(-0.39394771448153,2.10229571354889,13.0402691383507));
#36026=CARTESIAN_POINT('Ctrl Pts',(-0.393944288396229,2.1000422128466,13.0403836477965));
#36027=CARTESIAN_POINT('',(-0.393238269502415,2.10033186658782,13.1653836447486));
#36028=CARTESIAN_POINT('Ctrl Pts',(-0.393299997742054,2.10004214380805,
13.0403836477965));
#36029=CARTESIAN_POINT('Ctrl Pts',(-0.393302189049272,2.07959213788605,
13.0414244974294));
#36030=CARTESIAN_POINT('Ctrl Pts',(-0.391705092139561,2.05907940249458,
13.0424653470622));
#36031=CARTESIAN_POINT('Ctrl Pts',(-0.388505413481191,2.03877554658628,
13.0435061966951));
#36032=CARTESIAN_POINT('Ctrl Pts',(-0.385311597575711,2.01850889331693,
13.0445451391851));
#36033=CARTESIAN_POINT('Ctrl Pts',(-0.380521082138016,1.99845109263691,
13.0455840816752));
#36034=CARTESIAN_POINT('Ctrl Pts',(-0.374182434352757,1.97887033467459,
13.0466230241652));
#36035=CARTESIAN_POINT('Ctrl Pts',(-0.367850471108373,1.95931022597083,
13.0476608710188));
#36036=CARTESIAN_POINT('Ctrl Pts',(-0.359973815974987,1.9402268713692,13.0486987178724));
#36037=CARTESIAN_POINT('Ctrl Pts',(-0.350651231867759,1.92187475308193,
13.049736564726));
#36038=CARTESIAN_POINT('Ctrl Pts',(-0.341323709487897,1.90351291348107,
13.0507749613382));
#36039=CARTESIAN_POINT('Ctrl Pts',(-0.330549051033115,1.88588375069158,
13.0518133579503));
#36040=CARTESIAN_POINT('Ctrl Pts',(-0.318472847162838,1.86921885774614,
13.0528517545625));
#36041=CARTESIAN_POINT('Ctrl Pts',(-0.306392475521783,1.85254821336966,
13.0538905095488));
#36042=CARTESIAN_POINT('Ctrl Pts',(-0.293010130277935,1.83684307719353,
13.0549292645352));
#36043=CARTESIAN_POINT('Ctrl Pts',(-0.278512250093498,1.82230265296936,
13.0559680195215));
#36044=CARTESIAN_POINT('Ctrl Pts',(-0.263983526389957,1.80773129471575,
13.0570089844074));
#36045=CARTESIAN_POINT('Ctrl Pts',(-0.248335096783645,1.79433007213102,
13.0580499492932));
#36046=CARTESIAN_POINT('Ctrl Pts',(-0.231787549495608,1.78225887597162,
13.0590909141791));
#36047=CARTESIAN_POINT('Ctrl Pts',(-0.227444936614511,1.77909100275031,
13.0593640971133));
#36048=CARTESIAN_POINT('Ctrl Pts',(-0.223040549547636,1.77601449326531,
13.0596372800476));
#36049=CARTESIAN_POINT('Ctrl Pts',(-0.218578668352261,1.77303172058845,
13.0599104629818));
#36050=CARTESIAN_POINT('Ctrl Pts',(-0.201527694796042,1.76163312528515,
13.0609544251097));
#36051=CARTESIAN_POINT('Ctrl Pts',(-0.183531882943273,1.75153793738519,
13.0619983872377));
#36052=CARTESIAN_POINT('Ctrl Pts',(-0.164816685327661,1.74290008367741,
13.0630423493656));
#36053=CARTESIAN_POINT('Ctrl Pts',(-0.14613591633572,1.73427812023275,13.0640843910126));
#36054=CARTESIAN_POINT('Ctrl Pts',(-0.126739024042769,1.72710852830456,
13.0651264326597));
#36055=CARTESIAN_POINT('Ctrl Pts',(-0.10687734793002,1.72150016842878,13.0661684743068));
#36056=CARTESIAN_POINT('Ctrl Pts',(-0.0870370029068725,1.71589783183251,
13.0672093968195));
#36057=CARTESIAN_POINT('Ctrl Pts',(-0.0667335616766056,1.71185362533106,
13.0682503193322));
#36058=CARTESIAN_POINT('Ctrl Pts',(-0.0462348264664314,1.70942704801584,
13.0692912418449));
#36059=CARTESIAN_POINT('Ctrl Pts',(-0.0257255634438634,1.70699922445052,
13.0703326989583));
#36060=CARTESIAN_POINT('Ctrl Pts',(-0.00502153484719317,1.70619079230346,
13.0713741560716));
#36061=CARTESIAN_POINT('Ctrl Pts',(0.015602418044393,1.70700959992492,13.072415613185));
#36062=CARTESIAN_POINT('Ctrl Pts',(0.0362326725539908,1.70782865773183,
13.073457388514));
#36063=CARTESIAN_POINT('Ctrl Pts',(0.056782069505377,1.71027587979938,13.074499163843));
#36064=CARTESIAN_POINT('Ctrl Pts',(0.0769798975387362,1.7143071359554,13.075540939172));
#36065=CARTESIAN_POINT('Ctrl Pts',(0.0972213839447773,1.71834710582476,
13.076584966338));
#36066=CARTESIAN_POINT('Ctrl Pts',(0.117109075645695,1.72397774490345,13.077628993504));
#36067=CARTESIAN_POINT('Ctrl Pts',(0.136385743363226,1.73110459611529,13.0786730206699));
#36068=CARTESIAN_POINT('Ctrl Pts',(0.143203707534823,1.73362529196017,13.0790422826148));
#36069=CARTESIAN_POINT('Ctrl Pts',(0.149945423373895,1.73633272053559,13.0794115445597));
#36070=CARTESIAN_POINT('Ctrl Pts',(0.15660021115429,1.73922130901835,13.0797808065045));
#36071=CARTESIAN_POINT('Ctrl Pts',(0.175414365851484,1.74738781294976,13.0808247693751));
#36072=CARTESIAN_POINT('Ctrl Pts',(0.193644049227042,1.75705431354917,13.0818687322457));
#36073=CARTESIAN_POINT('Ctrl Pts',(0.211037795122978,1.76811456942247,13.0829126951163));
#36074=CARTESIAN_POINT('Ctrl Pts',(0.228399543248293,1.77915447869921,13.0839547374986));
#36075=CARTESIAN_POINT('Ctrl Pts',(0.244927760586449,1.79158271370629,13.084996779881));
#36076=CARTESIAN_POINT('Ctrl Pts',(0.260394860435468,1.80524687167259,13.0860388222633));
#36077=CARTESIAN_POINT('Ctrl Pts',(0.275845348761198,1.81889635445864,13.0870797455017));
#36078=CARTESIAN_POINT('Ctrl Pts',(0.290236414266017,1.83377866206034,13.0881206687401));
#36079=CARTESIAN_POINT('Ctrl Pts',(0.303373062655239,1.84970082929586,13.0891615919785));
#36080=CARTESIAN_POINT('Ctrl Pts',(0.316516457524256,1.86563117354704,13.0902030497953));
#36081=CARTESIAN_POINT('Ctrl Pts',(0.328403667579282,1.88260188702379,13.091244507612));
#36082=CARTESIAN_POINT('Ctrl Pts',(0.33887931702491,1.90038612650236,13.0922859654287));
#36083=CARTESIAN_POINT('Ctrl Pts',(0.349358167166871,1.91817579972042,13.0933277414491));
#36084=CARTESIAN_POINT('Ctrl Pts',(0.358424256170585,1.93677884197119,13.0943695174695));
#36085=CARTESIAN_POINT('Ctrl Pts',(0.365968148299018,1.95594374560406,13.0954112934899));
#36086=CARTESIAN_POINT('Ctrl Pts',(0.373528346623202,1.97515007436137,13.0964553213193));
#36087=CARTESIAN_POINT('Ctrl Pts',(0.379559564362063,1.99491998470172,13.0974993491486));
#36088=CARTESIAN_POINT('Ctrl Pts',(0.384001979624431,2.01498606205734,13.098543376978));
#36089=CARTESIAN_POINT('Ctrl Pts',(0.385573198246311,2.02208314608645,13.0989126346611));
#36090=CARTESIAN_POINT('Ctrl Pts',(0.386946138599605,2.02921720008482,13.0992818923442));
#36091=CARTESIAN_POINT('Ctrl Pts',(0.388119705309467,2.03637622810229,13.0996511500273));
#36092=CARTESIAN_POINT('Ctrl Pts',(0.391437609261143,2.05661620862466,13.1006951141375));
#36093=CARTESIAN_POINT('Ctrl Pts',(0.393177899969202,2.07717673006261,13.1017390782477));
#36094=CARTESIAN_POINT('Ctrl Pts',(0.393293784326227,2.09778884411339,13.1027830423579));
#36095=CARTESIAN_POINT('Ctrl Pts',(0.393409455502914,2.1183630402123,13.1038250859964));
#36096=CARTESIAN_POINT('Ctrl Pts',(0.391906588329872,2.13898791341175,13.1048671296349));
#36097=CARTESIAN_POINT('Ctrl Pts',(0.388790129405108,2.15938960580067,13.1059091732735));
#36098=CARTESIAN_POINT('Ctrl Pts',(0.385677017488246,2.17976938722356,13.1069500977802));
#36099=CARTESIAN_POINT('Ctrl Pts',(0.380953836115718,2.1999257356621,13.1079910222869));
#36100=CARTESIAN_POINT('Ctrl Pts',(0.374677280338413,2.21959024039699,13.1090319467936));
#36101=CARTESIAN_POINT('Ctrl Pts',(0.36839750114873,2.23926484411135,13.1100734058816));
#36102=CARTESIAN_POINT('Ctrl Pts',(0.360562962183608,2.25844639365872,13.1111148649695));
#36103=CARTESIAN_POINT('Ctrl Pts',(0.351280289951746,2.27688145151886,13.1121563240575));
#36104=CARTESIAN_POINT('Ctrl Pts',(0.341994781496254,2.29532214201854,13.1131981013524));
#36105=CARTESIAN_POINT('Ctrl Pts',(0.331260621878094,2.31301524643091,13.1142398786473));
#36106=CARTESIAN_POINT('Ctrl Pts',(0.319230044069069,2.32973260317957,13.1152816559422));
#36107=CARTESIAN_POINT('Ctrl Pts',(0.307173462249178,2.34648609437941,13.1163256850316));
#36108=CARTESIAN_POINT('Ctrl Pts',(0.293815343749129,2.36225906524756,13.1173697141209));
#36109=CARTESIAN_POINT('Ctrl Pts',(0.279348153227717,2.37685645971923,13.1184137432102));
#36110=CARTESIAN_POINT('Ctrl Pts',(0.274231426314988,2.3820192369038,13.1187829933235));
#36111=CARTESIAN_POINT('Ctrl Pts',(0.26897628854097,2.38703531663029,13.1191522434368));
#36112=CARTESIAN_POINT('Ctrl Pts',(0.263592232763096,2.3918972847201,13.1195214935501));
#36113=CARTESIAN_POINT('Ctrl Pts',(0.248370213741312,2.40564323643377,13.1205654523203));
#36114=CARTESIAN_POINT('Ctrl Pts',(0.232024695912387,2.41823623162151,13.1216094110905));
#36115=CARTESIAN_POINT('Ctrl Pts',(0.214756483154807,2.42949133970862,13.1226533698606));
#36116=CARTESIAN_POINT('Ctrl Pts',(0.197520037206229,2.4407257427654,13.1236954081519));
#36117=CARTESIAN_POINT('Ctrl Pts',(0.179364842576409,2.45062669703958,13.1247374464431));
#36118=CARTESIAN_POINT('Ctrl Pts',(0.160523839093104,2.45905011778693,13.1257794847343));
#36119=CARTESIAN_POINT('Ctrl Pts',(0.141703070347353,2.46746449200403,13.1268204039041));
#36120=CARTESIAN_POINT('Ctrl Pts',(0.122198611456366,2.47440415774629,13.1278613230739));
#36121=CARTESIAN_POINT('Ctrl Pts',(0.102266834682567,2.47977148987781,13.1289022422437));
#36122=CARTESIAN_POINT('Ctrl Pts',(0.0823248201470075,2.48514157888686,
13.1299436960714));
#36123=CARTESIAN_POINT('Ctrl Pts',(0.061955755525126,2.48893751396757,13.1309851498991));
#36124=CARTESIAN_POINT('Ctrl Pts',(0.0414304522452797,2.49111175848695,
13.1320266037268));
#36125=CARTESIAN_POINT('Ctrl Pts',(0.0208988768998916,2.49328666740597,
13.133068375799));
#36126=CARTESIAN_POINT('Ctrl Pts',(0.000211702737125122,2.49383885777713,
13.1341101478713));
#36127=CARTESIAN_POINT('Ctrl Pts',(-0.0203568237301628,2.49277282203281,
13.1351519199436));
#36128=CARTESIAN_POINT('Ctrl Pts',(-0.0409698117976874,2.49170448191073,
13.1361959439445));
#36129=CARTESIAN_POINT('Ctrl Pts',(-0.0614629099310601,2.48901102804192,
13.1372399679454));
#36130=CARTESIAN_POINT('Ctrl Pts',(-0.0815679292918496,2.48474870098681,
13.1382839919463));
#36131=CARTESIAN_POINT('Ctrl Pts',(-0.0886792752952678,2.48324107336783,
13.1386532736552));
#36132=CARTESIAN_POINT('Ctrl Pts',(-0.095742191761906,2.48153762390391,
13.1390225553641));
#36133=CARTESIAN_POINT('Ctrl Pts',(-0.102745303105613,2.47964232204766,
13.1393918370729));
#36134=CARTESIAN_POINT('Ctrl Pts',(-0.122543211064429,2.47428427333719,
13.1404358023798));
#36135=CARTESIAN_POINT('Ctrl Pts',(-0.141979855005472,2.46735743365101,
13.1414797676867));
#36136=CARTESIAN_POINT('Ctrl Pts',(-0.160791040950966,2.45893053805702,
13.1425237329936));
#36137=CARTESIAN_POINT('Ctrl Pts',(-0.179567620997308,2.45051914495714,
13.1435657777751));
#36138=CARTESIAN_POINT('Ctrl Pts',(-0.197720338777932,2.44061341671961,
13.1446078225567));
#36139=CARTESIAN_POINT('Ctrl Pts',(-0.215001948648293,2.42933121940903,
13.1456498673383));
#36140=CARTESIAN_POINT('Ctrl Pts',(-0.232264997538626,2.41806113952503,
13.1466907929318));
#36141=CARTESIAN_POINT('Ctrl Pts',(-0.248658167111771,2.40541790144835,
13.1477317185253));
#36142=CARTESIAN_POINT('Ctrl Pts',(-0.263960591461509,2.39156422303721,
13.1487726441188));
#36143=CARTESIAN_POINT('Ctrl Pts',(-0.279270873193604,2.37770343113569,
13.1498141041995));
#36144=CARTESIAN_POINT('Ctrl Pts',(-0.293488734540599,2.36263143908251,
13.1508555642802));
#36145=CARTESIAN_POINT('Ctrl Pts',(-0.306427608728904,2.34655021924283,
13.1518970243609));
#36146=CARTESIAN_POINT('Ctrl Pts',(-0.319370435593064,2.33046408677717,
13.1529388025956));
#36147=CARTESIAN_POINT('Ctrl Pts',(-0.331033064811712,2.3133687082097,13.1539805808302));
#36148=CARTESIAN_POINT('Ctrl Pts',(-0.341270816983217,2.29549710861189,
13.1550223590649));
#36149=CARTESIAN_POINT('Ctrl Pts',(-0.351530697063042,2.27758688128498,
13.1560663890022));
#36150=CARTESIAN_POINT('Ctrl Pts',(-0.360359236985173,2.25889774933996,
13.1571104189395));
#36151=CARTESIAN_POINT('Ctrl Pts',(-0.367658547116141,2.23968565686014,
13.1581544488767));
#36152=CARTESIAN_POINT('Ctrl Pts',(-0.370240106983396,2.23289088228254,
13.1585236927831));
#36153=CARTESIAN_POINT('Ctrl Pts',(-0.372630839426149,2.22603083974788,
13.1588929366894));
#36154=CARTESIAN_POINT('Ctrl Pts',(-0.374827924988285,2.21911723909232,
13.1592621805957));
#36155=CARTESIAN_POINT('Ctrl Pts',(-0.382278322486661,2.19567296640825,
13.160514300187));
#36156=CARTESIAN_POINT('Ctrl Pts',(-0.387534363760182,2.17149952030509,
13.1617664197783));
#36157=CARTESIAN_POINT('Ctrl Pts',(-0.390484665621148,2.14697463054394,
13.1630185393695));
#36158=CARTESIAN_POINT('Ctrl Pts',(-0.392342255036592,2.13153310022531,
13.1638069075465));
#36159=CARTESIAN_POINT('Ctrl Pts',(-0.393286676415921,2.11595266695904,
13.1645952757234));
#36160=CARTESIAN_POINT('Ctrl Pts',(-0.393299859927403,2.10033193536341,
13.1653836439004));
#36161=CARTESIAN_POINT('',(-0.393168444855454,2.09979799896453,13.2903836510805));
#36162=CARTESIAN_POINT('Ctrl Pts',(-0.393016960555868,2.1003316194609,13.1653836477965));
#36163=CARTESIAN_POINT('Ctrl Pts',(-0.392294146464799,2.00958948971456,
13.1699666065705));
#36164=CARTESIAN_POINT('Ctrl Pts',(-0.31587487389345,1.7866046526642,13.1811730131854));
#36165=CARTESIAN_POINT('Ctrl Pts',(0.0552540808467619,1.63823999361116,
13.1990028676414));
#36166=CARTESIAN_POINT('Ctrl Pts',(0.41816195164139,1.89649844744964,13.2188732111641));
#36167=CARTESIAN_POINT('Ctrl Pts',(0.397474384784138,2.34144118050984,13.2387435546869));
#36168=CARTESIAN_POINT('Ctrl Pts',(0.0121365597886237,2.56489583068018,
13.2586138982096));
#36169=CARTESIAN_POINT('Ctrl Pts',(-0.331284324819889,2.3890171423689,13.2758272625795));
#36170=CARTESIAN_POINT('Ctrl Pts',(-0.392396098076996,2.17846515087843,
13.2864171791085));
#36171=CARTESIAN_POINT('Ctrl Pts',(-0.392766706913104,2.09979827052114,
13.2903836477965));
#36172=CARTESIAN_POINT('',(0.386061278380631,2.17511044757631,13.3566999406454));
#36173=CARTESIAN_POINT('Ctrl Pts',(-0.393299948079913,2.09979791007433,
13.2903836521554));
#36174=CARTESIAN_POINT('Ctrl Pts',(-0.393288194121441,2.07692279029185,
13.2915354796105));
#36175=CARTESIAN_POINT('Ctrl Pts',(-0.391276592848532,2.05411783564869,
13.2926873070656));
#36176=CARTESIAN_POINT('Ctrl Pts',(-0.387326160418207,2.03171138121407,
13.2938391345206));
#36177=CARTESIAN_POINT('Ctrl Pts',(-0.38334552455176,2.0091336159351,13.2949997683906));
#36178=CARTESIAN_POINT('Ctrl Pts',(-0.377396497655504,1.98696088882726,
13.2961604022605));
#36179=CARTESIAN_POINT('Ctrl Pts',(-0.369590783055106,1.96551006327344,
13.2973210361305));
#36180=CARTESIAN_POINT('Ctrl Pts',(-0.367273776316445,1.95914271449086,
13.2976655525054));
#36181=CARTESIAN_POINT('Ctrl Pts',(-0.364793491675445,1.95283882330262,
13.2980100688803));
#36182=CARTESIAN_POINT('Ctrl Pts',(-0.362153634920279,1.94660627550636,
13.2983545852552));
#36183=CARTESIAN_POINT('Ctrl Pts',(-0.354165085623896,1.92774577664974,
13.2993971365372));
#36184=CARTESIAN_POINT('Ctrl Pts',(-0.344675022130477,1.90945389785774,
13.3004396878193));
#36185=CARTESIAN_POINT('Ctrl Pts',(-0.33378684723082,1.8919826194384,13.3014822391013));
#36186=CARTESIAN_POINT('Ctrl Pts',(-0.322918758472639,1.87454357145008,
13.3025228671195));
#36187=CARTESIAN_POINT('Ctrl Pts',(-0.310658012177592,1.85792277018594,
13.3035634951377));
#36188=CARTESIAN_POINT('Ctrl Pts',(-0.297154417031168,1.84234879693883,
13.304604123156));
#36189=CARTESIAN_POINT('Ctrl Pts',(-0.283665320897661,1.8267915457007,13.3056436338363));
#36190=CARTESIAN_POINT('Ctrl Pts',(-0.268936483837422,1.81227946511035,
13.3066831445166));
#36191=CARTESIAN_POINT('Ctrl Pts',(-0.253158594444117,1.79900894355633,
13.3077226551969));
#36192=CARTESIAN_POINT('Ctrl Pts',(-0.237372305983092,1.7857313576855,13.3087627192415));
#36193=CARTESIAN_POINT('Ctrl Pts',(-0.220536403997549,1.77369713855338,
13.3098027832861));
#36194=CARTESIAN_POINT('Ctrl Pts',(-0.202875827346148,1.76306337587223,
13.3108428473307));
#36195=CARTESIAN_POINT('Ctrl Pts',(-0.185209694911656,1.75242626795043,
13.3118832385656));
#36196=CARTESIAN_POINT('Ctrl Pts',(-0.166719022153088,1.74319084209225,
13.3129236298006));
#36197=CARTESIAN_POINT('Ctrl Pts',(-0.147653809061824,1.73546846135137,
13.3139640210355));
#36198=CARTESIAN_POINT('Ctrl Pts',(-0.128546706716977,1.72772911333279,
13.3150066981727));
#36199=CARTESIAN_POINT('Ctrl Pts',(-0.108863248517147,1.72150966889204,
13.3160493753098));
#36200=CARTESIAN_POINT('Ctrl Pts',(-0.0888697560011624,1.71687201033037,
13.3170920524469));
#36201=CARTESIAN_POINT('Ctrl Pts',(-0.0816287307463324,1.71519239368803,
13.3174696778906));
#36202=CARTESIAN_POINT('Ctrl Pts',(-0.0743471254598987,1.71371976480426,
13.3178473033343));
#36203=CARTESIAN_POINT('Ctrl Pts',(-0.0670377807939903,1.71245538844384,
13.318224928778));
#36204=CARTESIAN_POINT('Ctrl Pts',(-0.0467922450206122,1.70895329926814,
13.3192708815657));
#36205=CARTESIAN_POINT('Ctrl Pts',(-0.0262122163330918,1.707031660208,13.3203168343534));
#36206=CARTESIAN_POINT('Ctrl Pts',(-0.00556709706753582,1.70673940264725,
13.3213627871411));
#36207=CARTESIAN_POINT('Ctrl Pts',(0.0150398900019641,1.70644768489557,
13.3224068080205));
#36208=CARTESIAN_POINT('Ctrl Pts',(0.0357110053059775,1.70777944339817,
13.3234508288999));
#36209=CARTESIAN_POINT('Ctrl Pts',(0.0561715495447083,1.7107319085492,13.3244948497794));
#36210=CARTESIAN_POINT('Ctrl Pts',(0.0766098110257722,1.71368115828892,
13.3255377336575));
#36211=CARTESIAN_POINT('Ctrl Pts',(0.0968372310438449,1.71824753486853,
13.3265806175357));
#36212=CARTESIAN_POINT('Ctrl Pts',(0.116584129853373,1.72437647748533,13.3276235014139));
#36213=CARTESIAN_POINT('Ctrl Pts',(0.136340226437917,1.73050827486103,13.3286668710499));
#36214=CARTESIAN_POINT('Ctrl Pts',(0.155614649935592,1.73820389117585,13.3297102406859));
#36215=CARTESIAN_POINT('Ctrl Pts',(0.174152259224977,1.7473587083071,13.3307536103219));
#36216=CARTESIAN_POINT('Ctrl Pts',(0.192695060688043,1.75651608959858,13.3317972721939));
#36217=CARTESIAN_POINT('Ctrl Pts',(0.210499995805076,1.76713313037676,13.3328409340659));
#36218=CARTESIAN_POINT('Ctrl Pts',(0.227336745970714,1.77905936073559,13.3338845959379));
#36219=CARTESIAN_POINT('Ctrl Pts',(0.244208748436968,1.79101056189067,13.334930442999));
#36220=CARTESIAN_POINT('Ctrl Pts',(0.260107954319876,1.80427595693448,13.33597629006));
#36221=CARTESIAN_POINT('Ctrl Pts',(0.27483673790471,1.81866451077424,13.3370221371211));
#36222=CARTESIAN_POINT('Ctrl Pts',(0.279874432996801,1.82358583687312,13.3373798488477));
#36223=CARTESIAN_POINT('Ctrl Pts',(0.284775536428784,1.82863824945768,13.3377375605743));
#36224=CARTESIAN_POINT('Ctrl Pts',(0.289533219254565,1.83381321417454,13.3380952723008));
#36225=CARTESIAN_POINT('Ctrl Pts',(0.303298904154541,1.84878624543143,13.3391302607802));
#36226=CARTESIAN_POINT('Ctrl Pts',(0.315943783334727,1.86487772602899,13.3401652492595));
#36227=CARTESIAN_POINT('Ctrl Pts',(0.327282668995372,1.88189235553226,13.3412002377389));
#36228=CARTESIAN_POINT('Ctrl Pts',(0.338601061227082,1.89887623350394,13.3422333556233));
#36229=CARTESIAN_POINT('Ctrl Pts',(0.348617681618409,1.91677936705804,13.3432664735076));
#36230=CARTESIAN_POINT('Ctrl Pts',(0.357187760401041,1.93537377541932,13.344299591392));
#36231=CARTESIAN_POINT('Ctrl Pts',(0.365759867841031,1.95397258533679,13.3453329538297));
#36232=CARTESIAN_POINT('Ctrl Pts',(0.372884379614551,1.97326234353729,13.3463663162675));
#36233=CARTESIAN_POINT('Ctrl Pts',(0.378462415407803,1.99299023351258,13.3473996787053));
#36234=CARTESIAN_POINT('Ctrl Pts',(0.384036418815935,2.01270386211471,13.3484322941211));
#36235=CARTESIAN_POINT('Ctrl Pts',(0.388065981863659,2.03285426537309,13.3494649095369));
#36236=CARTESIAN_POINT('Ctrl Pts',(0.390502626407998,2.0531749130438,13.3504975249528));
#36237=CARTESIAN_POINT('Ctrl Pts',(0.392944704640702,2.07354087551722,13.3515324430887));
#36238=CARTESIAN_POINT('Ctrl Pts',(0.393786700096242,2.09407709007872,13.3525673612246));
#36239=CARTESIAN_POINT('Ctrl Pts',(0.393032175547103,2.11451202896604,13.3536022793605));
#36240=CARTESIAN_POINT('Ctrl Pts',(0.392279374784967,2.13490028218605,13.3546348331221));
#36241=CARTESIAN_POINT('Ctrl Pts',(0.389937501447389,2.15518699244151,13.3556673868838));
#36242=CARTESIAN_POINT('Ctrl Pts',(0.386061278380631,2.17511044757631,13.3566999406454));
#36243=CARTESIAN_POINT('Ctrl Pts',(0.386061278380631,2.17511044757631,13.3567));
#36244=CARTESIAN_POINT('Ctrl Pts',(0.385531328553113,2.17769530268049,13.3567));
#36245=CARTESIAN_POINT('Ctrl Pts',(0.385001378725595,2.18028015778468,13.3567));
#36246=CARTESIAN_POINT('Ctrl Pts',(0.384471428898077,2.18286501288886,13.3567));
#36247=CARTESIAN_POINT('',(-0.3933,2.1,13.4067));
#36248=CARTESIAN_POINT('Origin',(0.,2.1,13.4067));
#36249=CARTESIAN_POINT('Origin',(0.,2.1,4.03722265507267));
#36250=CARTESIAN_POINT('',(-0.322274998938081,2.10002616218071,13.100028292361));
#36251=CARTESIAN_POINT('',(-0.304247867982273,1.99372483614108,13.3567));
#36252=CARTESIAN_POINT('Ctrl Pts',(-0.322274998940427,2.10002613326275,
13.1000282941516));
#36253=CARTESIAN_POINT('Ctrl Pts',(-0.322275002368696,2.09998385590746,
13.1000309118996));
#36254=CARTESIAN_POINT('Ctrl Pts',(-0.322274997477792,2.09994157852145,
13.1000335291818));
#36255=CARTESIAN_POINT('Ctrl Pts',(-0.322274843812231,2.09944978993456,
13.1000639690949));
#36256=CARTESIAN_POINT('Ctrl Pts',(-0.322273762884423,2.0990002763328,13.1000917395794));
#36257=CARTESIAN_POINT('Ctrl Pts',(-0.322263476054635,2.09671275874497,
13.1002327981922));
#36258=CARTESIAN_POINT('Ctrl Pts',(-0.322239486612913,2.09487480804254,
13.1003452742039));
#36259=CARTESIAN_POINT('Ctrl Pts',(-0.321507714129348,2.06101285841063,
13.1024032971133));
#36260=CARTESIAN_POINT('Ctrl Pts',(-0.316045174157482,2.02926498944136,
13.104112479787));
#36261=CARTESIAN_POINT('Ctrl Pts',(-0.300735410555515,1.98295606854878,
13.1068806919687));
#36262=CARTESIAN_POINT('Ctrl Pts',(-0.294255879988497,1.96750688529557,
13.1078528274757));
#36263=CARTESIAN_POINT('Ctrl Pts',(-0.286004525178468,1.95145934939636,
13.1089488438727));
#36264=CARTESIAN_POINT('Ctrl Pts',(-0.285394560335216,1.95029075461181,
13.1090291601988));
#36265=CARTESIAN_POINT('Ctrl Pts',(-0.284516939401083,1.94863422952304,
13.1091437417129));
#36266=CARTESIAN_POINT('Ctrl Pts',(-0.284255156766297,1.94814318874716,
13.1091777986978));
#36267=CARTESIAN_POINT('Ctrl Pts',(-0.283802169922842,1.94729877077789,
13.1092365240531));
#36268=CARTESIAN_POINT('Ctrl Pts',(-0.283611573614604,1.94694506748116,
13.1092611707669));
#36269=CARTESIAN_POINT('Ctrl Pts',(-0.283246264998223,1.94627016332486,
13.1093082920872));
#36270=CARTESIAN_POINT('Ctrl Pts',(-0.283071666396078,1.94594890132931,
13.1093307626127));
#36271=CARTESIAN_POINT('Ctrl Pts',(-0.282662705435276,1.94519945462188,
13.1093832767361));
#36272=CARTESIAN_POINT('Ctrl Pts',(-0.28242791671866,1.94477150471925,13.1094133355378));
#36273=CARTESIAN_POINT('Ctrl Pts',(-0.281618205814068,1.94330356129304,
13.1095166917221));
#36274=CARTESIAN_POINT('Ctrl Pts',(-0.28103850947434,1.94226622466587,13.1095901600136));
#36275=CARTESIAN_POINT('Ctrl Pts',(-0.27476257576315,1.93118019684787,13.1103799954219));
#36276=CARTESIAN_POINT('Ctrl Pts',(-0.26853643292989,1.92144264618825,13.1111155954051));
#36277=CARTESIAN_POINT('Ctrl Pts',(-0.259453713912288,1.9087902781968,13.1121309662091));
#36278=CARTESIAN_POINT('Ctrl Pts',(-0.257044660048004,1.90556381979863,
13.1123954170968));
#36279=CARTESIAN_POINT('Ctrl Pts',(-0.253968458756467,1.90160096071808,
13.1127270520547));
#36280=CARTESIAN_POINT('Ctrl Pts',(-0.253357455578584,1.90082129504387,
13.1127926350144));
#36281=CARTESIAN_POINT('Ctrl Pts',(-0.23874504855636,1.88235128025021,13.1143542303163));
#36282=CARTESIAN_POINT('Ctrl Pts',(-0.222929361289476,1.86617837262526,
13.11590202832));
#36283=CARTESIAN_POINT('Ctrl Pts',(-0.202226214283227,1.84903303288053,
13.1176948547406));
#36284=CARTESIAN_POINT('Ctrl Pts',(-0.19884178749188,1.84634313208145,13.1179811821564));
#36285=CARTESIAN_POINT('Ctrl Pts',(-0.190315934567189,1.83984242850949,
13.1186841043337));
#36286=CARTESIAN_POINT('Ctrl Pts',(-0.185112877733177,1.83611488722322,
13.1190971017542));
#36287=CARTESIAN_POINT('Ctrl Pts',(-0.178877127044097,1.83192278968225,
13.1195705224224));
#36288=CARTESIAN_POINT('Ctrl Pts',(-0.177949143736069,1.83130589957853,
13.119640429617));
#36289=CARTESIAN_POINT('Ctrl Pts',(-0.176712515090817,1.83049304972884,
13.1197328456181));
#36290=CARTESIAN_POINT('Ctrl Pts',(-0.176406723529106,1.83029279369831,
13.1197556381718));
#36291=CARTESIAN_POINT('Ctrl Pts',(-0.175929208574289,1.82998123941053,
13.1197911361329));
#36292=CARTESIAN_POINT('Ctrl Pts',(-0.175757719987975,1.82986958452437,
13.1198038655069));
#36293=CARTESIAN_POINT('Ctrl Pts',(-0.175410654143129,1.82964408305688,
13.1198295893424));
#36294=CARTESIAN_POINT('Ctrl Pts',(-0.175235073691105,1.82953024501472,
13.1198425831398));
#36295=CARTESIAN_POINT('Ctrl Pts',(-0.174832512429986,1.82926979992011,
13.1198723292715));
#36296=CARTESIAN_POINT('Ctrl Pts',(-0.174605458371492,1.82912330748837,
13.1198890738459));
#36297=CARTESIAN_POINT('Ctrl Pts',(-0.173937633682946,1.8286936239447,13.1199382280543));
#36298=CARTESIAN_POINT('Ctrl Pts',(-0.173496353764188,1.82841122015232,
13.1199705851969));
#36299=CARTESIAN_POINT('Ctrl Pts',(-0.170655059918173,1.82660264194096,
13.1201781513914));
#36300=CARTESIAN_POINT('Ctrl Pts',(-0.168235524922132,1.82510715841391,
13.1203513660593));
#36301=CARTESIAN_POINT('Ctrl Pts',(-0.146263235101439,1.81192515877966,
13.1218957105008));
#36302=CARTESIAN_POINT('Ctrl Pts',(-0.12553966536828,1.80230863438546,13.123152969081));
#36303=CARTESIAN_POINT('Ctrl Pts',(-0.0801845046078889,1.7868495092839,
13.1258331491801));
#36304=CARTESIAN_POINT('Ctrl Pts',(-0.0555340376343538,1.78155300784509,
13.1272548768699));
#36305=CARTESIAN_POINT('Ctrl Pts',(-0.0293712670059871,1.77906412332862,
13.1288529741022));
#36306=CARTESIAN_POINT('Ctrl Pts',(-0.0282214899131648,1.77896097478164,
13.1289233627152));
#36307=CARTESIAN_POINT('Ctrl Pts',(-0.0265459716102778,1.7788197315584,
13.1290261734174));
#36308=CARTESIAN_POINT('Ctrl Pts',(-0.0260206428446681,1.7787767449488,
13.1290584417069));
#36309=CARTESIAN_POINT('Ctrl Pts',(-0.025099767409725,1.778703665344,13.1291150665734));
#36310=CARTESIAN_POINT('Ctrl Pts',(-0.0247042651843215,1.77867301347875,
13.1291394055409));
#36311=CARTESIAN_POINT('Ctrl Pts',(-0.0239371262816572,1.77861498405498,
13.1291866528768));
#36312=CARTESIAN_POINT('Ctrl Pts',(-0.0235654965410722,1.77858752068477,
13.1292095585108));
#36313=CARTESIAN_POINT('Ctrl Pts',(-0.0226795762349534,1.778523596089,13.1292642044297));
#36314=CARTESIAN_POINT('Ctrl Pts',(-0.022165245357576,1.77848772442867,
13.1292959631807));
#36315=CARTESIAN_POINT('Ctrl Pts',(-0.0206141440500869,1.77838328357096,
13.1293918421999));
#36316=CARTESIAN_POINT('Ctrl Pts',(-0.0195771334775212,1.77831849443,13.1294560809539));
#36317=CARTESIAN_POINT('Ctrl Pts',(-0.00882555581054929,1.77769895160184,
13.1301235550778));
#36318=CARTESIAN_POINT('Ctrl Pts',(0.000908137531323761,1.77757946929876,
13.1307403894243));
#36319=CARTESIAN_POINT('Ctrl Pts',(0.0396114779545556,1.77885695122998,
13.1332464644097));
#36320=CARTESIAN_POINT('Ctrl Pts',(0.0683277008459709,1.78372044169004,
13.1352406106739));
#36321=CARTESIAN_POINT('Ctrl Pts',(0.101923147754386,1.79420372707678,13.1375914010035));
#36322=CARTESIAN_POINT('Ctrl Pts',(0.107793009829547,1.79622316732652,13.1380020943538));
#36323=CARTESIAN_POINT('Ctrl Pts',(0.118451622629756,1.80023800524931,13.1387435707093));
#36324=CARTESIAN_POINT('Ctrl Pts',(0.123257618230174,1.80218192235977,13.1390762569213));
#36325=CARTESIAN_POINT('Ctrl Pts',(0.128917104841652,1.80463154860443,13.1394643046045));
#36326=CARTESIAN_POINT('Ctrl Pts',(0.129817488808469,1.80502616783916,13.139525926346));
#36327=CARTESIAN_POINT('Ctrl Pts',(0.131034367354442,1.80556615095718,13.1396090402527));
#36328=CARTESIAN_POINT('Ctrl Pts',(0.131352440572687,1.80570791167876,13.1396307492936));
#36329=CARTESIAN_POINT('Ctrl Pts',(0.13185664158092,1.80593360718472,13.1396651363002));
#36330=CARTESIAN_POINT('Ctrl Pts',(0.132042919289206,1.80601720326092,13.1396778350777));
#36331=CARTESIAN_POINT('Ctrl Pts',(0.132426478835396,1.80618977185241,13.1397039711755));
#36332=CARTESIAN_POINT('Ctrl Pts',(0.132623750025104,1.80627876585039,13.13971740704));
#36333=CARTESIAN_POINT('Ctrl Pts',(0.133079752809487,1.8064850332405,13.1397484502752));
#36334=CARTESIAN_POINT('Ctrl Pts',(0.133338419930862,1.80660245043373,13.1397660487443));
#36335=CARTESIAN_POINT('Ctrl Pts',(0.134132668270098,1.8069642521859,13.1398200534769));
#36336=CARTESIAN_POINT('Ctrl Pts',(0.134667739178919,1.80720976411161,13.1398563905862));
#36337=CARTESIAN_POINT('Ctrl Pts',(0.138983883981192,1.80920451872364,13.1401491640672));
#36338=CARTESIAN_POINT('Ctrl Pts',(0.142731601938089,1.81102556211661,13.1404012727305));
#36339=CARTESIAN_POINT('Ctrl Pts',(0.172774049806691,1.82635053717589,13.1424134214274));
#36340=CARTESIAN_POINT('Ctrl Pts',(0.197135322277393,1.84334248799633,13.1440006445294));
#36341=CARTESIAN_POINT('Ctrl Pts',(0.231247387429444,1.87489678116242,13.1466382850647));
#36342=CARTESIAN_POINT('Ctrl Pts',(0.242730402707627,1.88732973862727,13.1476207852567));
#36343=CARTESIAN_POINT('Ctrl Pts',(0.253910992039204,1.90152642215609,13.1487194874641));
#36344=CARTESIAN_POINT('Ctrl Pts',(0.254632068482555,1.9024523788456,13.148791040873));
#36345=CARTESIAN_POINT('Ctrl Pts',(0.255671819258296,1.90380270626667,13.1488952402997));
#36346=CARTESIAN_POINT('Ctrl Pts',(0.255994534219415,1.90422396552286,13.1489277265531));
#36347=CARTESIAN_POINT('Ctrl Pts',(0.256557018170268,1.90496197838828,13.1489846047204));
#36348=CARTESIAN_POINT('Ctrl Pts',(0.256797245317798,1.90527838270614,13.14900897854));
#36349=CARTESIAN_POINT('Ctrl Pts',(0.257261074819815,1.90589164590104,13.1490561991587));
#36350=CARTESIAN_POINT('Ctrl Pts',(0.257484750028722,1.90618844913343,13.1490790430485));
#36351=CARTESIAN_POINT('Ctrl Pts',(0.258015219121175,1.90689488807573,13.1491333926211));
#36352=CARTESIAN_POINT('Ctrl Pts',(0.258321550915546,1.90730486805008,13.149164916309));
#36353=CARTESIAN_POINT('Ctrl Pts',(0.259401953665918,1.90875803419428,13.1492765894412));
#36354=CARTESIAN_POINT('Ctrl Pts',(0.260170684701439,1.90980515834106,13.1493569464142));
#36355=CARTESIAN_POINT('Ctrl Pts',(0.273056757340544,1.92758218595751,13.1507193709368));
#36356=CARTESIAN_POINT('Ctrl Pts',(0.28354192636524,1.94543099935899,13.1520653646861));
#36357=CARTESIAN_POINT('Ctrl Pts',(0.304068469423984,1.98959080521796,13.155329549031));
#36358=CARTESIAN_POINT('Ctrl Pts',(0.312520218092005,2.01645930589435,13.1572707371285));
#36359=CARTESIAN_POINT('Ctrl Pts',(0.317726993876248,2.0460132057395,13.1591756431431));
#36360=CARTESIAN_POINT('Ctrl Pts',(0.318049436064414,2.04794643846475,13.1592991715826));
#36361=CARTESIAN_POINT('Ctrl Pts',(0.318423607378717,2.05032323574633,13.1594496203989));
#36362=CARTESIAN_POINT('Ctrl Pts',(0.318492068609554,2.05076406920446,13.1594774647636));
#36363=CARTESIAN_POINT('Ctrl Pts',(0.31859147974066,2.05141307836185,13.1595183685132));
#36364=CARTESIAN_POINT('Ctrl Pts',(0.318623141064951,2.05162114205434,13.1595314681635));
#36365=CARTESIAN_POINT('Ctrl Pts',(0.318687011110921,2.0520436490427,13.1595580414137));
#36366=CARTESIAN_POINT('Ctrl Pts',(0.318719207152378,2.05225809345008,13.1595715142184));
#36367=CARTESIAN_POINT('Ctrl Pts',(0.318787251917256,2.05271444782472,13.1596001544743));
#36368=CARTESIAN_POINT('Ctrl Pts',(0.31882304162232,2.05295636534958,13.1596153184984));
#36369=CARTESIAN_POINT('Ctrl Pts',(0.318918332434982,2.05360557909043,13.1596559640351));
#36370=CARTESIAN_POINT('Ctrl Pts',(0.318977328901456,2.05401295067085,13.1596814168783));
#36371=CARTESIAN_POINT('Ctrl Pts',(0.319239256268139,2.05584631927787,13.1597957393549));
#36372=CARTESIAN_POINT('Ctrl Pts',(0.319433410440474,2.05727358264205,13.1598841193034));
#36373=CARTESIAN_POINT('Ctrl Pts',(0.323121445303702,2.08581651541562,13.1616400716805));
#36374=CARTESIAN_POINT('Ctrl Pts',(0.323161033818841,2.11327156868801,13.1631282644955));
#36375=CARTESIAN_POINT('Ctrl Pts',(0.316950491520289,2.16241599995751,13.1659079770247));
#36376=CARTESIAN_POINT('Ctrl Pts',(0.311904261492362,2.18407662552179,13.1671761672507));
#36377=CARTESIAN_POINT('Ctrl Pts',(0.304300538618862,2.20613045917093,13.168594768159));
#36378=CARTESIAN_POINT('Ctrl Pts',(0.303920754150156,2.20721318627414,13.1686647329452));
#36379=CARTESIAN_POINT('Ctrl Pts',(0.303358515084277,2.20878907765674,13.1687670394483));
#36380=CARTESIAN_POINT('Ctrl Pts',(0.303180619710128,2.20928386851932,13.1687992295271));
#36381=CARTESIAN_POINT('Ctrl Pts',(0.302866449162211,2.21015101823665,13.1688557653961));
#36382=CARTESIAN_POINT('Ctrl Pts',(0.30273069582072,2.21052356604963,13.168880093755));
#36383=CARTESIAN_POINT('Ctrl Pts',(0.302465885548909,2.21124613645369,13.1689273560864));
#36384=CARTESIAN_POINT('Ctrl Pts',(0.302336907644422,2.21159618752874,13.1689502873901));
#36385=CARTESIAN_POINT('Ctrl Pts',(0.302027710623407,2.21243088991442,13.1690050512688));
#36386=CARTESIAN_POINT('Ctrl Pts',(0.301846932761477,2.21291533185923,13.169036902488));
#36387=CARTESIAN_POINT('Ctrl Pts',(0.30119681906715,2.21464476477485,13.1691508526744));
#36388=CARTESIAN_POINT('Ctrl Pts',(0.300720945040233,2.21588726865104,13.1692331704195));
#36389=CARTESIAN_POINT('Ctrl Pts',(0.292334952281257,2.23738353731727,13.17066527293));
#36390=CARTESIAN_POINT('Ctrl Pts',(0.282404457371426,2.25678437813968,13.1720862914891));
#36391=CARTESIAN_POINT('Ctrl Pts',(0.262028823322614,2.28828456714812,13.174606664647));
#36392=CARTESIAN_POINT('Ctrl Pts',(0.252496981220199,2.3008866584972,13.1756825023987));
#36393=CARTESIAN_POINT('Ctrl Pts',(0.234455428947308,2.32141647237794,13.1775126468732));
#36394=CARTESIAN_POINT('Ctrl Pts',(0.226368457612949,2.32967800313671,13.1782741659965));
#36395=CARTESIAN_POINT('Ctrl Pts',(0.217088154515517,2.33819107873137,13.179070995298));
#36396=CARTESIAN_POINT('Ctrl Pts',(0.21631850115342,2.33889027386052,13.1791365336938));
#36397=CARTESIAN_POINT('Ctrl Pts',(0.214986406528519,2.34008870475396,13.1792490081594));
#36398=CARTESIAN_POINT('Ctrl Pts',(0.214425582467213,2.34058971456196,13.1792960715749));
#36399=CARTESIAN_POINT('Ctrl Pts',(0.21363175387852,2.3412938973872,13.1793622747434));
#36400=CARTESIAN_POINT('Ctrl Pts',(0.213400208352938,2.34149870032436,13.1793815356462));
#36401=CARTESIAN_POINT('Ctrl Pts',(0.213014552338626,2.34183882686326,13.179413533527));
#36402=CARTESIAN_POINT('Ctrl Pts',(0.212860607346183,2.34197433650576,13.1794262845246));
#36403=CARTESIAN_POINT('Ctrl Pts',(0.212539549983822,2.34225640285186,13.1794528315255));
#36404=CARTESIAN_POINT('Ctrl Pts',(0.212372415099037,2.34240293384303,13.1794666255679));
#36405=CARTESIAN_POINT('Ctrl Pts',(0.21196793764384,2.34275680908801,13.1794999463602));
#36406=CARTESIAN_POINT('Ctrl Pts',(0.211730441615963,2.34296397889956,13.1795194599925));
#36407=CARTESIAN_POINT('Ctrl Pts',(0.210927328858837,2.34366246916725,13.1795852756171));
#36408=CARTESIAN_POINT('Ctrl Pts',(0.210360297414463,2.34415217025104,13.179631457841));
#36409=CARTESIAN_POINT('Ctrl Pts',(0.201177618098627,2.35202679996756,13.1803748344916));
#36410=CARTESIAN_POINT('Ctrl Pts',(0.19217842681585,2.3589545488804,13.1810395216439));
#36411=CARTESIAN_POINT('Ctrl Pts',(0.178016111897704,2.36871105466462,13.1820242125751));
#36412=CARTESIAN_POINT('Ctrl Pts',(0.173111284483999,2.37189677126632,13.1823548795258));
#36413=CARTESIAN_POINT('Ctrl Pts',(0.154200742874493,2.38346002092454,13.1836011716372));
#36414=CARTESIAN_POINT('Ctrl Pts',(0.139652925356227,2.39090292206267,13.1845034252282));
#36415=CARTESIAN_POINT('Ctrl Pts',(0.109073237023004,2.40372323925584,13.1863858614907));
#36416=CARTESIAN_POINT('Ctrl Pts',(0.0930582244146317,2.40900618144362,
13.1873650263045));
#36417=CARTESIAN_POINT('Ctrl Pts',(0.0755658154721046,2.41329276963923,
13.1884600329017));
#36418=CARTESIAN_POINT('Ctrl Pts',(0.0744248458547879,2.41356577338527,
13.1885315600744));
#36419=CARTESIAN_POINT('Ctrl Pts',(0.072765774141958,2.41395317997857,13.1886357257984));
#36420=CARTESIAN_POINT('Ctrl Pts',(0.0722488309123698,2.41407254501407,
13.1886682046928));
#36421=CARTESIAN_POINT('Ctrl Pts',(0.071344352680709,2.41427904279586,13.1887250718279));
#36422=CARTESIAN_POINT('Ctrl Pts',(0.0709569459069465,2.41436673683038,
13.1887494419835));
#36423=CARTESIAN_POINT('Ctrl Pts',(0.0702067813063998,2.41453508799919,
13.1887966568519));
#36424=CARTESIAN_POINT('Ctrl Pts',(0.0698440439528597,2.41461583438628,
13.1888194986584));
#36425=CARTESIAN_POINT('Ctrl Pts',(0.0689814297210626,2.41480628947348,
13.1888738453948));
#36426=CARTESIAN_POINT('Ctrl Pts',(0.0684814307218341,2.41491543496611,
13.1889053683344));
#36427=CARTESIAN_POINT('Ctrl Pts',(0.0667112453192996,2.41529743608114,
13.1890170500196));
#36428=CARTESIAN_POINT('Ctrl Pts',(0.065439684174189,2.41556379879081,13.189097416381));
#36429=CARTESIAN_POINT('Ctrl Pts',(0.0438295462181028,2.41995439293981,
13.190465764114));
#36430=CARTESIAN_POINT('Ctrl Pts',(0.0231450745828925,2.4221115472394,13.1918183050712));
#36431=CARTESIAN_POINT('Ctrl Pts',(-0.00216728645454903,2.4223000820675,
13.1935154006768));
#36432=CARTESIAN_POINT('Ctrl Pts',(-0.00673504506051571,2.42223699013039,
13.1938230864147));
#36433=CARTESIAN_POINT('Ctrl Pts',(-0.0271023102383277,2.42152241881947,
13.195199387668));
#36434=CARTESIAN_POINT('Ctrl Pts',(-0.0428429370357241,2.41980574345981,
13.196275987723));
#36435=CARTESIAN_POINT('Ctrl Pts',(-0.0646624397054319,2.41578563541496,
13.1977443581534));
#36436=CARTESIAN_POINT('Ctrl Pts',(-0.0708953762043883,2.41444499626468,
13.1981608138686));
#36437=CARTESIAN_POINT('Ctrl Pts',(-0.0800195295578282,2.41219735016752,
13.1987621617263));
#36438=CARTESIAN_POINT('Ctrl Pts',(-0.0829440210275808,2.41143314139955,
13.1989536302863));
#36439=CARTESIAN_POINT('Ctrl Pts',(-0.0863457283848059,2.41049291044949,
13.1991745000902));
#36440=CARTESIAN_POINT('Ctrl Pts',(-0.0868336868203381,2.41035679965358,
13.1992061382819));
#36441=CARTESIAN_POINT('Ctrl Pts',(-0.0875775841786026,2.41014740567287,
13.1992543008954));
#36442=CARTESIAN_POINT('Ctrl Pts',(-0.0878337537599031,2.41007495577335,
13.199270873542));
#36443=CARTESIAN_POINT('Ctrl Pts',(-0.088279135392221,2.40994839668533,
13.1992996646235));
#36444=CARTESIAN_POINT('Ctrl Pts',(-0.088468387136638,2.40989443175303,
13.1993118914649));
#36445=CARTESIAN_POINT('Ctrl Pts',(-0.0888962129169217,2.40977201383681,
13.1993395156271));
#36446=CARTESIAN_POINT('Ctrl Pts',(-0.0891347568762895,2.40970345872316,
13.1993549068576));
#36447=CARTESIAN_POINT('Ctrl Pts',(-0.0897804840358736,2.40951707544482,
13.199396540317));
#36448=CARTESIAN_POINT('Ctrl Pts',(-0.0901875161493704,2.40939871887472,
13.1994227516542));
#36449=CARTESIAN_POINT('Ctrl Pts',(-0.0920105050184408,2.40886472810304,
13.1995400058776));
#36450=CARTESIAN_POINT('Ctrl Pts',(-0.0934238595329029,2.40844016594039,
13.1996305352916));
#36451=CARTESIAN_POINT('Ctrl Pts',(-0.125906286536871,2.39843890444091,
13.2017034876592));
#36452=CARTESIAN_POINT('Ctrl Pts',(-0.155357663903889,2.38422353518025,
13.2034360692372));
#36453=CARTESIAN_POINT('Ctrl Pts',(-0.194804724683445,2.35718923139032,
13.206150109739));
#36454=CARTESIAN_POINT('Ctrl Pts',(-0.206789772936656,2.3476551642339,13.2070370015348));
#36455=CARTESIAN_POINT('Ctrl Pts',(-0.219846175937913,2.33565817071051,
13.2081066420595));
#36456=CARTESIAN_POINT('Ctrl Pts',(-0.221621845306997,2.33398904178676,
13.2082544908054));
#36457=CARTESIAN_POINT('Ctrl Pts',(-0.223887445556888,2.33181045300906,
13.2084463055136));
#36458=CARTESIAN_POINT('Ctrl Pts',(-0.224394899915125,2.33131926699224,
13.2084894773868));
#36459=CARTESIAN_POINT('Ctrl Pts',(-0.225211372436159,2.33052375464129,
13.2085592791024));
#36460=CARTESIAN_POINT('Ctrl Pts',(-0.225521399900627,2.33022046371347,
13.2085858636074));
#36461=CARTESIAN_POINT('Ctrl Pts',(-0.226111638489387,2.32964071396988,
13.2086366287326));
#36462=CARTESIAN_POINT('Ctrl Pts',(-0.226391957385034,2.3293643655892,13.2086608044731));
#36463=CARTESIAN_POINT('Ctrl Pts',(-0.227031178984468,2.32873188460738,
13.2087160850871));
#36464=CARTESIAN_POINT('Ctrl Pts',(-0.227389750644248,2.32837542022823,
13.2087472045869));
#36465=CARTESIAN_POINT('Ctrl Pts',(-0.228485278063448,2.32728119309091,
13.208842620816));
#36466=CARTESIAN_POINT('Ctrl Pts',(-0.229219487703784,2.32654070150954,
13.208907038621));
#36467=CARTESIAN_POINT('Ctrl Pts',(-0.234652677725241,2.32100757066395,
13.209387276282));
#36468=CARTESIAN_POINT('Ctrl Pts',(-0.239204201552291,2.31607305361624,
13.2098094698477));
#36469=CARTESIAN_POINT('Ctrl Pts',(-0.244863527809933,2.30953940908034,
13.2103614634661));
#36470=CARTESIAN_POINT('Ctrl Pts',(-0.246115761277302,2.30806715985257,
13.2104854022711));
#36471=CARTESIAN_POINT('Ctrl Pts',(-0.263521375524284,2.28722641365731,
13.2122336704529));
#36472=CARTESIAN_POINT('Ctrl Pts',(-0.277357893443123,2.26604055207158,
13.2139468567067));
#36473=CARTESIAN_POINT('Ctrl Pts',(-0.292298157336018,2.23598773543766,
13.2162121926337));
#36474=CARTESIAN_POINT('Ctrl Pts',(-0.295722949980194,2.22836988379563,
13.216772671429));
#36475=CARTESIAN_POINT('Ctrl Pts',(-0.301737337741392,2.21346953571121,
13.2178332323034));
#36476=CARTESIAN_POINT('Ctrl Pts',(-0.304368693351965,2.20620959036298,
13.2183343352683));
#36477=CARTESIAN_POINT('Ctrl Pts',(-0.307119522869414,2.19767460973626,
13.2189000436941));
#36478=CARTESIAN_POINT('Ctrl Pts',(-0.307495179388808,2.19648546775468,
13.2189783409417));
#36479=CARTESIAN_POINT('Ctrl Pts',(-0.307976702761597,2.19492982478192,
13.2190800639565));
#36480=CARTESIAN_POINT('Ctrl Pts',(-0.308088828191964,2.19456529502895,
13.2191038499748));
#36481=CARTESIAN_POINT('Ctrl Pts',(-0.308270085292133,2.19397226786407,
13.2191424627275));
#36482=CARTESIAN_POINT('Ctrl Pts',(-0.308339610219882,2.19374389251507,
13.2191573125466));
#36483=CARTESIAN_POINT('Ctrl Pts',(-0.30847306478934,2.19330376653323,13.219185892396));
#36484=CARTESIAN_POINT('Ctrl Pts',(-0.308537030028967,2.19309202785927,
13.2191996244642));
#36485=CARTESIAN_POINT('Ctrl Pts',(-0.308684432511372,2.19260227321381,
13.2192313472234));
#36486=CARTESIAN_POINT('Ctrl Pts',(-0.308767712465595,2.19232420928218,
13.2192493286352));
#36487=CARTESIAN_POINT('Ctrl Pts',(-0.308990620692099,2.1915762645651,13.2192976170855));
#36488=CARTESIAN_POINT('Ctrl Pts',(-0.309129553480925,2.19110617476075,
13.2193278835812));
#36489=CARTESIAN_POINT('Ctrl Pts',(-0.310112108354956,2.18775350044511,
13.2195431631885));
#36490=CARTESIAN_POINT('Ctrl Pts',(-0.310916505185332,2.18485944231975,
13.2197259380808));
#36491=CARTESIAN_POINT('Ctrl Pts',(-0.320491591038072,2.14844449924624,
13.2219924530133));
#36492=CARTESIAN_POINT('Ctrl Pts',(-0.323842776910861,2.11372797121006,
13.2238224967533));
#36493=CARTESIAN_POINT('Ctrl Pts',(-0.320833182380519,2.06733103721908,
13.2264943429057));
#36494=CARTESIAN_POINT('Ctrl Pts',(-0.31941758761162,2.05557535261493,13.2271885200427));
#36495=CARTESIAN_POINT('Ctrl Pts',(-0.317003691010174,2.04191380023851,
13.2280271387493));
#36496=CARTESIAN_POINT('Ctrl Pts',(-0.316629228389137,2.03990608891751,
13.2281511864198));
#36497=CARTESIAN_POINT('Ctrl Pts',(-0.316103296798389,2.03722776368256,
13.2283177883289));
#36498=CARTESIAN_POINT('Ctrl Pts',(-0.315968722900876,2.03655384932107,
13.2283598033556));
#36499=CARTESIAN_POINT('Ctrl Pts',(-0.315755076555664,2.03550149832686,
13.2284255622288));
#36500=CARTESIAN_POINT('Ctrl Pts',(-0.3156774763623,2.03512276204876,13.2284492590064));
#36501=CARTESIAN_POINT('Ctrl Pts',(-0.315527743167163,2.03439860186007,
13.2284946269214));
#36502=CARTESIAN_POINT('Ctrl Pts',(-0.315455723909256,2.03405315475784,
13.2285162943932));
#36503=CARTESIAN_POINT('Ctrl Pts',(-0.315286018791363,2.03324578745157,
13.2285669949671));
#36504=CARTESIAN_POINT('Ctrl Pts',(-0.315187885113132,2.03278396313053,
13.2285960423648));
#36505=CARTESIAN_POINT('Ctrl Pts',(-0.314903928008363,2.03146193589925,
13.2286793267996));
#36506=CARTESIAN_POINT('Ctrl Pts',(-0.314715596556258,2.03060228126632,
13.2287336440924));
#36507=CARTESIAN_POINT('Ctrl Pts',(-0.313471512159119,2.025032780693,13.2290866116284));
#36508=CARTESIAN_POINT('Ctrl Pts',(-0.312313631880659,2.02034659973759,
13.2293885277008));
#36509=CARTESIAN_POINT('Ctrl Pts',(-0.308526419612287,2.00637443043774,
13.2303042101087));
#36510=CARTESIAN_POINT('Ctrl Pts',(-0.30558500700906,1.99717941853793,13.2309277713388));
#36511=CARTESIAN_POINT('Ctrl Pts',(-0.296506832716131,1.97265299170292,
13.2326475297276));
#36512=CARTESIAN_POINT('Ctrl Pts',(-0.28959778341036,1.95763918347249,13.2337634509625));
#36513=CARTESIAN_POINT('Ctrl Pts',(-0.273472215704942,1.92867801569639,
13.2360063135293));
#36514=CARTESIAN_POINT('Ctrl Pts',(-0.264258759393619,1.91478204835129,
13.2371296950493));
#36515=CARTESIAN_POINT('Ctrl Pts',(-0.251867972717343,1.89891336124446,
13.2384228471367));
#36516=CARTESIAN_POINT('Ctrl Pts',(-0.249679458469861,1.89620234930712,
13.2386441080038));
#36517=CARTESIAN_POINT('Ctrl Pts',(-0.247082166797389,1.89308962496345,
13.2388980274663));
#36518=CARTESIAN_POINT('Ctrl Pts',(-0.246715863689308,1.89265298877747,
13.2389336429125));
#36519=CARTESIAN_POINT('Ctrl Pts',(-0.246168322665017,1.89200382082237,
13.2389865866025));
#36520=CARTESIAN_POINT('Ctrl Pts',(-0.245987966144664,1.89179055220853,
13.2390039787743));
#36521=CARTESIAN_POINT('Ctrl Pts',(-0.245665770348604,1.8914105639849,13.2390349644316));
#36522=CARTESIAN_POINT('Ctrl Pts',(-0.245524038407464,1.89124375433705,
13.2390485658056));
#36523=CARTESIAN_POINT('Ctrl Pts',(-0.245222359741969,1.89088942960377,
13.2390774547672));
#36524=CARTESIAN_POINT('Ctrl Pts',(-0.245062368216546,1.89070195401311,
13.239092738922));
#36525=CARTESIAN_POINT('Ctrl Pts',(-0.244631233432553,1.89019792904867,
13.2391338274935));
#36526=CARTESIAN_POINT('Ctrl Pts',(-0.244359689722565,1.88988172047741,
13.2391596023144));
#36527=CARTESIAN_POINT('Ctrl Pts',(-0.243041871773518,1.88835315100923,
13.2392841907315));
#36528=CARTESIAN_POINT('Ctrl Pts',(-0.241987160764741,1.88714804582244,
13.2393823888207));
#36529=CARTESIAN_POINT('Ctrl Pts',(-0.233010240374893,1.87704405485538,
13.2402059929506));
#36530=CARTESIAN_POINT('Ctrl Pts',(-0.224608174224842,1.86858184652406,
13.2408977411943));
#36531=CARTESIAN_POINT('Ctrl Pts',(-0.192015589123711,1.83920781575204,
13.2433939586018));
#36532=CARTESIAN_POINT('Ctrl Pts',(-0.165226656512624,1.82146314127373,
13.2451183260423));
#36533=CARTESIAN_POINT('Ctrl Pts',(-0.131041458441012,1.80551311970321,
13.2473538942219));
#36534=CARTESIAN_POINT('Ctrl Pts',(-0.125754903120121,1.80321710890451,
13.2476997988164));
#36535=CARTESIAN_POINT('Ctrl Pts',(-0.11949788015101,1.80069681099245,13.2481104516411));
#36536=CARTESIAN_POINT('Ctrl Pts',(-0.118584213644656,1.80033364127531,
13.2481704461446));
#36537=CARTESIAN_POINT('Ctrl Pts',(-0.117203327516454,1.79979206247822,
13.2482611700817));
#36538=CARTESIAN_POINT('Ctrl Pts',(-0.116737325271348,1.79961054842747,
13.2482917949193));
#36539=CARTESIAN_POINT('Ctrl Pts',(-0.115904710359728,1.79928846396228,
13.2483465289436));
#36540=CARTESIAN_POINT('Ctrl Pts',(-0.11553825896239,1.79914747715282,13.2483706240814));
#36541=CARTESIAN_POINT('Ctrl Pts',(-0.114764357424741,1.79885135236284,
13.2484215222192));
#36542=CARTESIAN_POINT('Ctrl Pts',(-0.114356848583648,1.79869637093482,
13.2484483304136));
#36543=CARTESIAN_POINT('Ctrl Pts',(-0.113277746132655,1.79828847741656,
13.2485193390946));
#36544=CARTESIAN_POINT('Ctrl Pts',(-0.112605622895469,1.79803698188767,
13.2485635869149));
#36545=CARTESIAN_POINT('Ctrl Pts',(-0.109538973172311,1.79690116335904,
13.2487655682254));
#36546=CARTESIAN_POINT('Ctrl Pts',(-0.107134885553436,1.79604308346307,
13.2489241747789));
#36547=CARTESIAN_POINT('Ctrl Pts',(-0.0966104146836363,1.792427001985,13.2496198301654));
#36548=CARTESIAN_POINT('Ctrl Pts',(-0.0883926046461903,1.78996541088462,
13.2501665460423));
#36549=CARTESIAN_POINT('Ctrl Pts',(-0.0660917983424246,1.78424406978137,
13.251660491625));
#36550=CARTESIAN_POINT('Ctrl Pts',(-0.0518723850401837,1.78159913439141,
13.2526245763627));
#36551=CARTESIAN_POINT('Ctrl Pts',(-0.0129311996467933,1.77703386832622,
13.2552704081916));
#36552=CARTESIAN_POINT('Ctrl Pts',(0.0119147229375276,1.77699444672677,
13.2569688229929));
#36553=CARTESIAN_POINT('Ctrl Pts',(0.0378626493634233,1.77995403862979,
13.2586184066659));
#36554=CARTESIAN_POINT('Ctrl Pts',(0.0392028157741224,1.78011543176669,
13.258703232091));
#36555=CARTESIAN_POINT('Ctrl Pts',(0.0409479913379044,1.78033673162865,
13.2588131714256));
#36556=CARTESIAN_POINT('Ctrl Pts',(0.0413539306085327,1.78038899335582,
13.2588387072496));
#36557=CARTESIAN_POINT('Ctrl Pts',(0.0419782888144332,1.78047058436149,
13.2588779250693));
#36558=CARTESIAN_POINT('Ctrl Pts',(0.0421967771750812,1.78049936434053,
13.2588916380938));
#36559=CARTESIAN_POINT('Ctrl Pts',(0.0426313411542964,1.78055706002362,
13.2589188908167));
#36560=CARTESIAN_POINT('Ctrl Pts',(0.0428474154018679,1.78058597065381,
13.2589324306268));
#36561=CARTESIAN_POINT('Ctrl Pts',(0.0433301604808671,1.78065106037633,
13.258962656751));
#36562=CARTESIAN_POINT('Ctrl Pts',(0.0435968147746435,1.78068735416706,
13.2589793364339));
#36563=CARTESIAN_POINT('Ctrl Pts',(0.0443789317289334,1.78079480454234,
13.2590282120503));
#36564=CARTESIAN_POINT('Ctrl Pts',(0.0448942709807827,1.78086687600528,
13.2590603562572));
#36565=CARTESIAN_POINT('Ctrl Pts',(0.0487283439531174,1.78141255144116,
13.2592990737063));
#36566=CARTESIAN_POINT('Ctrl Pts',(0.0520398374056291,1.78193668655603,
13.2595028429308));
#36567=CARTESIAN_POINT('Ctrl Pts',(0.0631478979208892,1.78387298318018,
13.2601800572255));
#36568=CARTESIAN_POINT('Ctrl Pts',(0.0709009005361706,1.78552101824546,
13.2606422488961));
#36569=CARTESIAN_POINT('Ctrl Pts',(0.107840562099311,1.79480902034258,13.2628272620334));
#36570=CARTESIAN_POINT('Ctrl Pts',(0.135917534323478,1.80623526056136,13.2644508740788));
#36571=CARTESIAN_POINT('Ctrl Pts',(0.170125446169387,1.82612610334544,13.2667573100406));
#36572=CARTESIAN_POINT('Ctrl Pts',(0.178042120665504,1.83120536488094,13.2673158022855));
#36573=CARTESIAN_POINT('Ctrl Pts',(0.186660537323343,1.83728279454425,13.2679571344166));
#36574=CARTESIAN_POINT('Ctrl Pts',(0.187592601095877,1.83794752014631,13.2680269443166));
#36575=CARTESIAN_POINT('Ctrl Pts',(0.188942657742257,1.83892124201081,13.2681287274504));
#36576=CARTESIAN_POINT('Ctrl Pts',(0.189363483330773,1.83922631082924,13.2681605490507));
#36577=CARTESIAN_POINT('Ctrl Pts',(0.190104537932795,1.83976626275833,13.268216753822));
#36578=CARTESIAN_POINT('Ctrl Pts',(0.190425075033036,1.84000072281287,13.2682411205599));
#36579=CARTESIAN_POINT('Ctrl Pts',(0.191086565153946,1.84048645578685,13.2682915219504));
#36580=CARTESIAN_POINT('Ctrl Pts',(0.191427457688659,1.84073780944277,13.2683175597141));
#36581=CARTESIAN_POINT('Ctrl Pts',(0.192298300361876,1.84138257034721,13.2683842399728));
#36582=CARTESIAN_POINT('Ctrl Pts',(0.192827537364962,1.84177693351349,13.2684249197307));
#36583=CARTESIAN_POINT('Ctrl Pts',(0.194978415629963,1.84338996911338,13.2685908878316));
#36584=CARTESIAN_POINT('Ctrl Pts',(0.196589717470629,1.84462229307194,13.2687167109769));
#36585=CARTESIAN_POINT('Ctrl Pts',(0.207120971923618,1.85283533028714,13.2695490916004));
#36586=CARTESIAN_POINT('Ctrl Pts',(0.215678256035746,1.86026616855722,13.2702736652006));
#36587=CARTESIAN_POINT('Ctrl Pts',(0.246927706024237,1.89043167323565,13.2731144002436));
#36588=CARTESIAN_POINT('Ctrl Pts',(0.266563150661782,1.9160548621442,13.2753496251217));
#36589=CARTESIAN_POINT('Ctrl Pts',(0.28277181708008,1.94539314521262,13.2775349921177));
#36590=CARTESIAN_POINT('Ctrl Pts',(0.283448303490417,1.94663690318856,13.277626957818));
#36591=CARTESIAN_POINT('Ctrl Pts',(0.284291970606341,1.94821268449843,13.2777425819444));
#36592=CARTESIAN_POINT('Ctrl Pts',(0.284466792532364,1.94854057425565,13.2777665926034));
#36593=CARTESIAN_POINT('Ctrl Pts',(0.286623869228038,1.95260321940963,13.2780634849976));
#36594=CARTESIAN_POINT('Ctrl Pts',(0.288533126039736,1.95637655908958,13.278332902583));
#36595=CARTESIAN_POINT('Ctrl Pts',(0.290624353423767,1.96071966804988,13.2786349390143));
#36596=CARTESIAN_POINT('Ctrl Pts',(0.290879563145679,1.96125344894926,13.2786719229933));
#36597=CARTESIAN_POINT('Ctrl Pts',(0.291255517372583,1.96204536820673,13.2787265862069));
#36598=CARTESIAN_POINT('Ctrl Pts',(0.291377389951216,1.96230296495601,13.2787443348773));
#36599=CARTESIAN_POINT('Ctrl Pts',(0.291591273284423,1.96275659628188,13.2787755333272));
#36600=CARTESIAN_POINT('Ctrl Pts',(0.29168342801291,1.96295256170431,13.2787889920552));
#36601=CARTESIAN_POINT('Ctrl Pts',(0.29187480401475,1.96336058687352,13.2788169757109));
#36602=CARTESIAN_POINT('Ctrl Pts',(0.291973991410148,1.96357266117431,13.278831498507));
#36603=CARTESIAN_POINT('Ctrl Pts',(0.29223140406459,1.96412460616443,13.2788692390282));
#36604=CARTESIAN_POINT('Ctrl Pts',(0.292389268108418,1.96446464642047,13.2788924343716));
#36605=CARTESIAN_POINT('Ctrl Pts',(0.293042812909677,1.96587884234628,13.2789886735287));
#36606=CARTESIAN_POINT('Ctrl Pts',(0.293533178692765,1.96695546521373,13.2790613939057));
#36607=CARTESIAN_POINT('Ctrl Pts',(0.301129965871642,1.98388105587522,13.2801964606125));
#36608=CARTESIAN_POINT('Ctrl Pts',(0.306950749323379,2.00027895469877,13.2811848256562));
#36609=CARTESIAN_POINT('Ctrl Pts',(0.317610770460845,2.04030905876824,13.2835123068745));
#36610=CARTESIAN_POINT('Ctrl Pts',(0.321178432826951,2.06416768577558,13.2848377434887));
#36611=CARTESIAN_POINT('Ctrl Pts',(0.32215438466193,2.09080622367152,13.2863991425299));
#36612=CARTESIAN_POINT('Ctrl Pts',(0.322218217573961,2.09341267798522,13.2865526905281));
#36613=CARTESIAN_POINT('Ctrl Pts',(0.322322909530261,2.10188840214809,13.2870548552787));
#36614=CARTESIAN_POINT('Ctrl Pts',(0.322235059836258,2.10775780721272,13.2874070753915));
#36615=CARTESIAN_POINT('Ctrl Pts',(0.3219451268441,2.11461140096026,13.2878246840979));
#36616=CARTESIAN_POINT('Ctrl Pts',(0.321898674125451,2.1156013236187,13.2878851565429));
#36617=CARTESIAN_POINT('Ctrl Pts',(0.321821772788813,2.11709312661381,13.2879765248342));
#36618=CARTESIAN_POINT('Ctrl Pts',(0.321794714040184,2.11759518200107,13.2880073146335));
#36619=CARTESIAN_POINT('Ctrl Pts',(0.321744349462104,2.11849066086518,13.2880623050691));
#36620=CARTESIAN_POINT('Ctrl Pts',(0.321721496563834,2.1188841096313,13.2880864914868));
#36621=CARTESIAN_POINT('Ctrl Pts',(0.321671783293538,2.11971371119004,13.2881375428814));
#36622=CARTESIAN_POINT('Ctrl Pts',(0.321644757457155,2.12014985293917,13.2881644129906));
#36623=CARTESIAN_POINT('Ctrl Pts',(0.321570993652707,2.12130227473176,13.2882354951546));
#36624=CARTESIAN_POINT('Ctrl Pts',(0.321522749715472,2.12201845293495,13.2882797542807));
#36625=CARTESIAN_POINT('Ctrl Pts',(0.321293041500956,2.12526659638077,13.2884808759018));
#36626=CARTESIAN_POINT('Ctrl Pts',(0.32108406240864,2.1277964689326,13.2886385979543));
#36627=CARTESIAN_POINT('Ctrl Pts',(0.320041679956877,2.13882563301227,13.2893310641673));
#36628=CARTESIAN_POINT('Ctrl Pts',(0.318900579807654,2.14729169995432,13.2898753681984));
#36629=CARTESIAN_POINT('Ctrl Pts',(0.314941127734568,2.16985518027476,13.2913614172381));
#36630=CARTESIAN_POINT('Ctrl Pts',(0.311513939663806,2.1838251083527,13.2923198015192));
#36631=CARTESIAN_POINT('Ctrl Pts',(0.300361758639017,2.2189525790881,13.2948062389792));
#36632=CARTESIAN_POINT('Ctrl Pts',(0.291331775562052,2.23961671405938,13.2963461465302));
#36633=CARTESIAN_POINT('Ctrl Pts',(0.278482219273848,2.2622382665128,13.2980176282241));
#36634=CARTESIAN_POINT('Ctrl Pts',(0.276690920222358,2.26527473723107,13.2982415535531));
#36635=CARTESIAN_POINT('Ctrl Pts',(0.274557315584081,2.26875950467236,13.2984974856627));
#36636=CARTESIAN_POINT('Ctrl Pts',(0.274263310686198,2.26923689426567,13.2985325233897));
#36637=CARTESIAN_POINT('Ctrl Pts',(0.273821605988517,2.2699499369256,13.2985848190297));
#36638=CARTESIAN_POINT('Ctrl Pts',(0.273674846480638,2.27018616680665,13.2986021382795));
#36639=CARTESIAN_POINT('Ctrl Pts',(0.273413885318743,2.27060500968234,13.2986328343962));
#36640=CARTESIAN_POINT('Ctrl Pts',(0.273299806298809,2.27078769830258,13.2986462193896));
#36641=CARTESIAN_POINT('Ctrl Pts',(0.273061216871858,2.27116892938551,13.2986741426149));
#36642=CARTESIAN_POINT('Ctrl Pts',(0.272936673235062,2.27136745008958,13.2986886784835));
#36643=CARTESIAN_POINT('Ctrl Pts',(0.272607423120428,2.2718910004424,13.2987270011957));
#36644=CARTESIAN_POINT('Ctrl Pts',(0.272402350927641,2.27221580179012,13.298750763591));
#36645=CARTESIAN_POINT('Ctrl Pts',(0.271506096007834,2.2736297191016,13.2988541552198));
#36646=CARTESIAN_POINT('Ctrl Pts',(0.270808946155987,2.274715066149,13.2989333902238));
#36647=CARTESIAN_POINT('Ctrl Pts',(0.265630958450031,2.28267087910922,13.2995134654401));
#36648=CARTESIAN_POINT('Ctrl Pts',(0.260895364419495,2.2893728882114,13.2999980971152));
#36649=CARTESIAN_POINT('Ctrl Pts',(0.246455521633568,2.30823719723952,13.3013730589431));
#36650=CARTESIAN_POINT('Ctrl Pts',(0.236120113209579,2.31988726984462,13.3022367865324));
#36651=CARTESIAN_POINT('Ctrl Pts',(0.213426316652339,2.34201429321112,13.3040064251962));
#36652=CARTESIAN_POINT('Ctrl Pts',(0.201039831968825,2.35239778410238,13.3049106062132));
#36653=CARTESIAN_POINT('Ctrl Pts',(0.185592405341932,2.36348606082858,13.3060154871071));
#36654=CARTESIAN_POINT('Ctrl Pts',(0.183233974858488,2.36513158043407,13.3061835478911));
#36655=CARTESIAN_POINT('Ctrl Pts',(0.180368195179146,2.36707458532761,13.3063871989529));
#36656=CARTESIAN_POINT('Ctrl Pts',(0.179881607027661,2.36740255684497,13.3064217580238));
#36657=CARTESIAN_POINT('Ctrl Pts',(0.177786687557818,2.36880627469434,13.3065704680477));
#36658=CARTESIAN_POINT('Ctrl Pts',(0.1761696049791,2.3698688378451,13.3066850617583));
#36659=CARTESIAN_POINT('Ctrl Pts',(0.170403142930759,2.37358398647841,13.307093148083));
#36660=CARTESIAN_POINT('Ctrl Pts',(0.166202802667764,2.37615584929755,13.3073894136506));
#36661=CARTESIAN_POINT('Ctrl Pts',(0.161211239626043,2.37905704223633,13.3077409690505));
#36662=CARTESIAN_POINT('Ctrl Pts',(0.160475448754023,2.3794808167457,13.3077927773409));
#36663=CARTESIAN_POINT('Ctrl Pts',(0.159294650871496,2.38015469012894,13.3078759013984));
#36664=CARTESIAN_POINT('Ctrl Pts',(0.158850706008351,2.38040665005201,13.3079071495277));
#36665=CARTESIAN_POINT('Ctrl Pts',(0.158063695002334,2.38085084759829,13.307962538832));
#36666=CARTESIAN_POINT('Ctrl Pts',(0.157720871288638,2.38104351448171,13.3079866644034));
#36667=CARTESIAN_POINT('Ctrl Pts',(0.157008938695551,2.38144190761101,13.308036761302));
#36668=CARTESIAN_POINT('Ctrl Pts',(0.156639776306437,2.38164753623273,13.3080627360959));
#36669=CARTESIAN_POINT('Ctrl Pts',(0.155688534258917,2.38217494269321,13.3081296617048));
#36670=CARTESIAN_POINT('Ctrl Pts',(0.155105863127844,2.38249564456165,13.3081706511882));
#36671=CARTESIAN_POINT('Ctrl Pts',(0.152682693196762,2.38381959900697,13.3083410982904));
#36672=CARTESIAN_POINT('Ctrl Pts',(0.150833453699553,2.38480666862155,13.308471134781));
#36673=CARTESIAN_POINT('Ctrl Pts',(0.138336650841771,2.39132124871586,13.3093497799342));
#36674=CARTESIAN_POINT('Ctrl Pts',(0.127398486029302,2.39626789231732,13.3101188123888));
#36675=CARTESIAN_POINT('Ctrl Pts',(0.0997208249173376,2.40696825237916,
13.3120654669599));
#36676=CARTESIAN_POINT('Ctrl Pts',(0.0827351846189903,2.4119752107131,13.3132620137301));
#36677=CARTESIAN_POINT('Ctrl Pts',(0.0594515538423541,2.41680265712882,
13.3148714962036));
#36678=CARTESIAN_POINT('Ctrl Pts',(0.0534424711182091,2.41787153975798,
13.3152839441848));
#36679=CARTESIAN_POINT('Ctrl Pts',(0.0343476700455006,2.42071127159424,
13.3165796962642));
#36680=CARTESIAN_POINT('Ctrl Pts',(0.0211799489830165,2.421849317678,13.3174516881898));
#36681=CARTESIAN_POINT('Ctrl Pts',(0.00714357649414458,2.42219689889339,
13.3183341627897));
#36682=CARTESIAN_POINT('Ctrl Pts',(0.00630904854883794,2.42221432042184,
13.3183864520476));
#36683=CARTESIAN_POINT('Ctrl Pts',(0.005145336440725,2.42223409112913,13.3184591100335));
#36684=CARTESIAN_POINT('Ctrl Pts',(0.00481621137220232,2.42223917838035,
13.3184796307488));
#36685=CARTESIAN_POINT('Ctrl Pts',(0.00426235170572277,2.42224689058909,
13.3185141146055));
#36686=CARTESIAN_POINT('Ctrl Pts',(0.00403762212661081,2.42224978470929,
13.3185280929315));
#36687=CARTESIAN_POINT('Ctrl Pts',(0.00359227569525369,2.42225505404386,
13.3185557667465));
#36688=CARTESIAN_POINT('Ctrl Pts',(0.00337166025017408,2.42225743778746,
13.3185694626837));
#36689=CARTESIAN_POINT('Ctrl Pts',(0.00292761510799275,2.42226177964352,
13.3185970032096));
#36690=CARTESIAN_POINT('Ctrl Pts',(0.00270418546231148,2.42226373195093,
13.3186108474634));
#36691=CARTESIAN_POINT('Ctrl Pts',(0.00190994003425121,2.42226984593815,
13.3186600142412));
#36692=CARTESIAN_POINT('Ctrl Pts',(0.00133911108802614,2.42227272342722,
13.3186952650754));
#36693=CARTESIAN_POINT('Ctrl Pts',(-0.00425503190026124,2.42228605935975,
13.3190399114128));
#36694=CARTESIAN_POINT('Ctrl Pts',(-0.0092782734663582,2.42218058577684,
13.3193429620839));
#36695=CARTESIAN_POINT('Ctrl Pts',(-0.0236659034809866,2.42154166748611,
13.3201977314319));
#36696=CARTESIAN_POINT('Ctrl Pts',(-0.0330126164451058,2.42071687438639,
13.3207369834546));
#36697=CARTESIAN_POINT('Ctrl Pts',(-0.0485215048691819,2.41866297208185,
13.3216238336867));
#36698=CARTESIAN_POINT('Ctrl Pts',(-0.0547071341289445,2.4176595016193,
13.3219754068292));
#36699=CARTESIAN_POINT('Ctrl Pts',(-0.0836978928970217,2.41208446015627,
13.323627611145));
#36700=CARTESIAN_POINT('Ctrl Pts',(-0.105991362608536,2.40523395823029,
13.324917175608));
#36701=CARTESIAN_POINT('Ctrl Pts',(-0.133922292476707,2.39321858326136,
13.3267079426474));
#36702=CARTESIAN_POINT('Ctrl Pts',(-0.14039530966298,2.3901748836482,13.3271356157394));
#36703=CARTESIAN_POINT('Ctrl Pts',(-0.147710583639609,2.3864330564264,13.3276357136852));
#36704=CARTESIAN_POINT('Ctrl Pts',(-0.148657356723442,2.38594283096855,
13.3277007670064));
#36705=CARTESIAN_POINT('Ctrl Pts',(-0.15005016218335,2.38521286935792,13.3277969596101));
#36706=CARTESIAN_POINT('Ctrl Pts',(-0.150498096721495,2.38497676203023,
13.3278279711796));
#36707=CARTESIAN_POINT('Ctrl Pts',(-0.151295902465212,2.38455383117248,
13.3278833406439));
#36708=CARTESIAN_POINT('Ctrl Pts',(-0.15164598948692,2.38436741516568,13.3279076841217));
#36709=CARTESIAN_POINT('Ctrl Pts',(-0.152377363899488,2.38397623475382,
13.327958638715));
#36710=CARTESIAN_POINT('Ctrl Pts',(-0.152758584496747,2.38377134773188,
13.3279852541323));
#36711=CARTESIAN_POINT('Ctrl Pts',(-0.153751313946428,2.38323522511471,
13.3280547093998));
#36712=CARTESIAN_POINT('Ctrl Pts',(-0.154362162974006,2.38290277820476,
13.3280975921348));
#36713=CARTESIAN_POINT('Ctrl Pts',(-0.157001188711173,2.38145542965283,
13.3282834908116));
#36714=CARTESIAN_POINT('Ctrl Pts',(-0.159018358734871,2.38032069719605,
13.328427211055));
#36715=CARTESIAN_POINT('Ctrl Pts',(-0.173161401824821,2.37216293482577,
13.3294466283498));
#36716=CARTESIAN_POINT('Ctrl Pts',(-0.184828488828499,2.36437827139864,
13.330349998307));
#36717=CARTESIAN_POINT('Ctrl Pts',(-0.208509633131971,2.34624203535987,
13.3323203537741));
#36718=CARTESIAN_POINT('Ctrl Pts',(-0.220342473068241,2.33571283128132,
13.3333910432132));
#36719=CARTESIAN_POINT('Ctrl Pts',(-0.237272731053398,2.31825470799072,
13.3350340857633));
#36720=CARTESIAN_POINT('Ctrl Pts',(-0.242948202527085,2.3119189642645,13.3356069872501));
#36721=CARTESIAN_POINT('Ctrl Pts',(-0.254953255373636,2.29740022822919,
13.336858826803));
#36722=CARTESIAN_POINT('Ctrl Pts',(-0.261153638419859,2.28912122889594,
13.3375333369435));
#36723=CARTESIAN_POINT('Ctrl Pts',(-0.267361038546912,2.27994387918258,
13.3382285982005));
#36724=CARTESIAN_POINT('Ctrl Pts',(-0.267774033371893,2.27932872515409,
13.338274957594));
#36725=CARTESIAN_POINT('Ctrl Pts',(-0.268360279763345,2.27844897277762,
13.3383409045595));
#36726=CARTESIAN_POINT('Ctrl Pts',(-0.268535265125195,2.27818554101334,
13.3383606066346));
#36727=CARTESIAN_POINT('Ctrl Pts',(-0.268834518137468,2.27773358845282,
13.3383943305701));
#36728=CARTESIAN_POINT('Ctrl Pts',(-0.268958975100083,2.27754519514732,
13.3384083650659));
#36729=CARTESIAN_POINT('Ctrl Pts',(-0.269210146181475,2.27716412164922,
13.338436707058));
#36730=CARTESIAN_POINT('Ctrl Pts',(-0.269336851848363,2.2769714356725,13.3384510140019));
#36731=CARTESIAN_POINT('Ctrl Pts',(-0.269650757755236,2.27649294941179,
13.3384864828059));
#36732=CARTESIAN_POINT('Ctrl Pts',(-0.269837711091967,2.27620698631211,
13.3385076284309));
#36733=CARTESIAN_POINT('Ctrl Pts',(-0.270513702732569,2.27516939333368,
13.3385841673609));
#36734=CARTESIAN_POINT('Ctrl Pts',(-0.271000063826336,2.27441601181311,
13.3386393877078));
#36735=CARTESIAN_POINT('Ctrl Pts',(-0.281811921276165,2.25751385592853,
13.3398706030303));
#36736=CARTESIAN_POINT('Ctrl Pts',(-0.290681186503799,2.24047510466773,
13.3409570247485));
#36737=CARTESIAN_POINT('Ctrl Pts',(-0.306018856020226,2.20324082872203,
13.3432232905128));
#36738=CARTESIAN_POINT('Ctrl Pts',(-0.312118573380971,2.18299479425078,
13.3443981638694));
#36739=CARTESIAN_POINT('Ctrl Pts',(-0.317875867065161,2.15377362982812,
13.3461416142945));
#36740=CARTESIAN_POINT('Ctrl Pts',(-0.319209911596244,2.14518497722302,
13.3466590579368));
#36741=CARTESIAN_POINT('Ctrl Pts',(-0.32032380239195,2.13542768839048,13.3472564584957));
#36742=CARTESIAN_POINT('Ctrl Pts',(-0.320446380109866,2.1343012668521,13.3473255654185));
#36743=CARTESIAN_POINT('Ctrl Pts',(-0.320616793409913,2.13265456108935,
13.3474268054853));
#36744=CARTESIAN_POINT('Ctrl Pts',(-0.320669308925578,2.13213476131231,
13.3474587939726));
#36745=CARTESIAN_POINT('Ctrl Pts',(-0.320760051283632,2.13121421446549,
13.3475155002185));
#36746=CARTESIAN_POINT('Ctrl Pts',(-0.320798791732582,2.13081351821522,
13.3475402020509));
#36747=CARTESIAN_POINT('Ctrl Pts',(-0.320877611296746,2.12998201781723,
13.3475915010323));
#36748=CARTESIAN_POINT('Ctrl Pts',(-0.320917573814974,2.12955120365997,
13.3476181017331));
#36749=CARTESIAN_POINT('Ctrl Pts',(-0.321018221485092,2.12844189065102,
13.3476866533823));
#36750=CARTESIAN_POINT('Ctrl Pts',(-0.321077622921942,2.12776328000895,
13.3477286439287));
#36751=CARTESIAN_POINT('Ctrl Pts',(-0.321315490036934,2.12494294169138,
13.3479033902646));
#36752=CARTESIAN_POINT('Ctrl Pts',(-0.321474678016385,2.12279968240715,
13.3480367404471));
#36753=CARTESIAN_POINT('Ctrl Pts',(-0.322400548880522,2.10838326463028,
13.3489376106644));
#36754=CARTESIAN_POINT('Ctrl Pts',(-0.322485575474556,2.09607794736713,
13.349726153015));
#36755=CARTESIAN_POINT('Ctrl Pts',(-0.320321010611323,2.05307409786068,
13.3525523025489));
#36756=CARTESIAN_POINT('Ctrl Pts',(-0.314384246460146,2.02274357795218,
13.3546890337174));
#36757=CARTESIAN_POINT('Ctrl Pts',(-0.304247867982273,1.99372483614108,
13.3567));
#36758=CARTESIAN_POINT('',(-0.203204102907281,2.3501384980099,13.3567));
#36759=CARTESIAN_POINT('Origin',(0.,2.1,13.3567));
#36760=CARTESIAN_POINT('',(-0.322274957492435,2.09983447583549,13.2493773449307));
#36761=CARTESIAN_POINT('Ctrl Pts',(-0.322274957492435,2.09983447583549,
13.2493773449307));
#36762=CARTESIAN_POINT('Ctrl Pts',(-0.32226483878068,2.08013338016583,13.2505879758328));
#36763=CARTESIAN_POINT('Ctrl Pts',(-0.320444039314449,2.06049592730386,
13.2517986067348));
#36764=CARTESIAN_POINT('Ctrl Pts',(-0.316871812603967,2.04123410851458,
13.2530092376369));
#36765=CARTESIAN_POINT('Ctrl Pts',(-0.313271733721456,2.02182210791043,
13.2542293076656));
#36766=CARTESIAN_POINT('Ctrl Pts',(-0.307893024034668,2.00279206168637,
13.2554493776942));
#36767=CARTESIAN_POINT('Ctrl Pts',(-0.300845432144591,1.98444394614416,
13.2566694477229));
#36768=CARTESIAN_POINT('Ctrl Pts',(-0.299538362453334,1.98104104397687,
13.2568957259439));
#36769=CARTESIAN_POINT('Ctrl Pts',(-0.29817401836561,1.97766153425079,13.257122004165));
#36770=CARTESIAN_POINT('Ctrl Pts',(-0.296753274075577,1.97430723986472,
13.2573482823861));
#36771=CARTESIAN_POINT('Ctrl Pts',(-0.289873171352211,1.95806371870298,
13.2584440583226));
#36772=CARTESIAN_POINT('Ctrl Pts',(-0.281633490705982,1.94233506417864,
13.2595398342591));
#36773=CARTESIAN_POINT('Ctrl Pts',(-0.272133799288446,1.92736057544745,
13.2606356101957));
#36774=CARTESIAN_POINT('Ctrl Pts',(-0.262652330660647,1.91241481153979,
13.2617292841592));
#36775=CARTESIAN_POINT('Ctrl Pts',(-0.251916004330233,1.89822102456005,
13.2628229581228));
#36776=CARTESIAN_POINT('Ctrl Pts',(-0.24007054260555,1.88499462751346,13.2639166320864));
#36777=CARTESIAN_POINT('Ctrl Pts',(-0.228064507295878,1.87158893733,13.2650251315716));
#36778=CARTESIAN_POINT('Ctrl Pts',(-0.21491946217764,1.85917776405065,13.2661336310568));
#36779=CARTESIAN_POINT('Ctrl Pts',(-0.200829887600173,1.84795133035165,
13.267242130542));
#36780=CARTESIAN_POINT('Ctrl Pts',(-0.1869352002943,1.83688018090353,13.2683352972406));
#36781=CARTESIAN_POINT('Ctrl Pts',(-0.172122628296553,1.8269616217329,13.2694284639392));
#36782=CARTESIAN_POINT('Ctrl Pts',(-0.156611467290689,1.81833703839863,
13.2705216306378));
#36783=CARTESIAN_POINT('Ctrl Pts',(-0.14077396631965,1.80953100209484,13.2716377965163));
#36784=CARTESIAN_POINT('Ctrl Pts',(-0.124208846012644,1.80207448238125,
13.2727539623948));
#36785=CARTESIAN_POINT('Ctrl Pts',(-0.107173813964848,1.7960675252211,13.2738701282733));
#36786=CARTESIAN_POINT('Ctrl Pts',(-0.0901387819170519,1.79006056806095,
13.2749862941518));
#36787=CARTESIAN_POINT('Ctrl Pts',(-0.0726346771758236,1.78550332968368,
13.2761024600303));
#36788=CARTESIAN_POINT('Ctrl Pts',(-0.0549316064210603,1.78244103816614,
13.2772186259088));
#36789=CARTESIAN_POINT('Ctrl Pts',(-0.0374952283451083,1.77942487936417,
13.2783179770057));
#36790=CARTESIAN_POINT('Ctrl Pts',(-0.0197559757355919,1.77783976901579,
13.2794173281027));
#36791=CARTESIAN_POINT('Ctrl Pts',(-0.00197043232130345,1.77773102379927,
13.2805166791996));
#36792=CARTESIAN_POINT('Ctrl Pts',(0.0157809453715159,1.77762248748043,
13.281613918462));
#36793=CARTESIAN_POINT('Ctrl Pts',(0.0335776760126947,1.77898475464975,
13.2827111577245));
#36794=CARTESIAN_POINT('Ctrl Pts',(0.0511584206520158,1.78181138986225,
13.283808396987));
#36795=CARTESIAN_POINT('Ctrl Pts',(0.0688909821816445,1.78466243422106,
13.2849151113574));
#36796=CARTESIAN_POINT('Ctrl Pts',(0.0864030118068149,1.78900325792153,
13.2860218257277));
#36797=CARTESIAN_POINT('Ctrl Pts',(0.10343179270322,1.79477378899708,13.2871285400981));
#36798=CARTESIAN_POINT('Ctrl Pts',(0.120305488659644,1.80049176654746,13.2882251753717));
#36799=CARTESIAN_POINT('Ctrl Pts',(0.136703982565598,1.80761320475385,13.2893218106452));
#36800=CARTESIAN_POINT('Ctrl Pts',(0.152388340046847,1.81602998495833,13.2904184459188));
#36801=CARTESIAN_POINT('Ctrl Pts',(0.168288928250003,1.82456280220557,13.2915301998376));
#36802=CARTESIAN_POINT('Ctrl Pts',(0.183454807723234,1.83442659769339,13.2926419537564));
#36803=CARTESIAN_POINT('Ctrl Pts',(0.197665413300553,1.84546206567641,13.2937537076752));
#36804=CARTESIAN_POINT('Ctrl Pts',(0.211876018877872,1.85649753365943,13.294865461594));
#36805=CARTESIAN_POINT('Ctrl Pts',(0.225130784671371,1.86870408322537,13.2959772155128));
#36806=CARTESIAN_POINT('Ctrl Pts',(0.237247185952831,1.88188317721353,13.2970889694316));
#36807=CARTESIAN_POINT('Ctrl Pts',(0.249220469872859,1.89490660145175,13.2981875914572));
#36808=CARTESIAN_POINT('Ctrl Pts',(0.26015467709715,1.9089585061543,13.2992862134828));
#36809=CARTESIAN_POINT('Ctrl Pts',(0.269873121224844,1.92384758285689,13.3003848355085));
#36810=CARTESIAN_POINT('Ctrl Pts',(0.279573317837768,1.93870870357769,13.3014813947428));
#36811=CARTESIAN_POINT('Ctrl Pts',(0.288061813739083,1.95440327127342,13.3025779539772));
#36812=CARTESIAN_POINT('Ctrl Pts',(0.295202914764986,1.97070802523259,13.3036745132115));
#36813=CARTESIAN_POINT('Ctrl Pts',(0.302412442995074,1.98716901402506,13.3047815798568));
#36814=CARTESIAN_POINT('Ctrl Pts',(0.308248181548252,2.00425127227537,13.305888646502));
#36815=CARTESIAN_POINT('Ctrl Pts',(0.312618619957343,2.02170074022721,13.3069957131473));
#36816=CARTESIAN_POINT('Ctrl Pts',(0.316945703283351,2.03897710812319,13.3080917976067));
#36817=CARTESIAN_POINT('Ctrl Pts',(0.3198363087186,2.0566126553897,13.3091878820662));
#36818=CARTESIAN_POINT('Ctrl Pts',(0.321252477112893,2.07434806880895,13.3102839665257));
#36819=CARTESIAN_POINT('Ctrl Pts',(0.322689929393039,2.09235003140153,13.3113965242639));
#36820=CARTESIAN_POINT('Ctrl Pts',(0.322608154631673,2.11045407645896,13.312509082002));
#36821=CARTESIAN_POINT('Ctrl Pts',(0.321022286249014,2.12838780295226,13.3136216397401));
#36822=CARTESIAN_POINT('Ctrl Pts',(0.319436417866355,2.14632152944555,13.3147341974782));
#36823=CARTESIAN_POINT('Ctrl Pts',(0.316346651383024,2.16408413715393,13.3158467552163));
#36824=CARTESIAN_POINT('Ctrl Pts',(0.311821906718333,2.18141421322806,13.3169593129544));
#36825=CARTESIAN_POINT('Ctrl Pts',(0.307406464415695,2.19832565391172,13.3180449951011));
#36826=CARTESIAN_POINT('Ctrl Pts',(0.301595565345558,2.21493620643441,13.3191306772479));
#36827=CARTESIAN_POINT('Ctrl Pts',(0.294449846721818,2.23099795185612,13.3202163593946));
#36828=CARTESIAN_POINT('Ctrl Pts',(0.287317896864584,2.24702874861695,13.3212999495888));
#36829=CARTESIAN_POINT('Ctrl Pts',(0.278856483092462,2.2625120937275,13.3223835397831));
#36830=CARTESIAN_POINT('Ctrl Pts',(0.269175515635444,2.27721658333066,13.3234671299773));
#36831=CARTESIAN_POINT('Ctrl Pts',(0.259226937221565,2.29232754909959,13.3245806738523));
#36832=CARTESIAN_POINT('Ctrl Pts',(0.247990648795134,2.3066151140032,13.3256942177273));
#36833=CARTESIAN_POINT('Ctrl Pts',(0.235635590836591,2.31985687152348,13.3268077616023));
#36834=CARTESIAN_POINT('Ctrl Pts',(0.223616150494876,2.33273892477394,13.3278910567368));
#36835=CARTESIAN_POINT('Ctrl Pts',(0.210538642062222,2.34463078399106,13.3289743518713));
#36836=CARTESIAN_POINT('Ctrl Pts',(0.196597171399358,2.35536391253028,13.3300576470059));
#36837=CARTESIAN_POINT('Ctrl Pts',(0.182071771323903,2.36654659116323,13.3311863152511));
#36838=CARTESIAN_POINT('Ctrl Pts',(0.166609069782128,2.37647061849798,13.3323149834963));
#36839=CARTESIAN_POINT('Ctrl Pts',(0.150461755109173,2.38499550149865,13.3334436517415));
#36840=CARTESIAN_POINT('Ctrl Pts',(0.134314440436219,2.39352038449932,13.3345723199868));
#36841=CARTESIAN_POINT('Ctrl Pts',(0.117483428649364,2.40064583038671,13.335700988232));
#36842=CARTESIAN_POINT('Ctrl Pts',(0.100242319425589,2.40628851271502,13.3368296564772));
#36843=CARTESIAN_POINT('Ctrl Pts',(0.0830172659067363,2.41192594032095,
13.3379572736552));
#36844=CARTESIAN_POINT('Ctrl Pts',(0.0652712419742939,2.41612062749411,
13.3390848908333));
#36845=CARTESIAN_POINT('Ctrl Pts',(0.0472633934003619,2.41879044413107,
13.3402125080113));
#36846=CARTESIAN_POINT('Ctrl Pts',(0.0292958691642339,2.42145428234214,
13.3413376001561));
#36847=CARTESIAN_POINT('Ctrl Pts',(0.0110683824425036,2.42259987165385,
13.3424626923009));
#36848=CARTESIAN_POINT('Ctrl Pts',(-0.0071482943072423,2.42219571305884,
13.3435877844457));
#36849=CARTESIAN_POINT('Ctrl Pts',(-0.0253420927399112,2.42179206204646,
13.3447114635877));
#36850=CARTESIAN_POINT('Ctrl Pts',(-0.0435243899744615,2.4198425030032,
13.3458351427298));
#36851=CARTESIAN_POINT('Ctrl Pts',(-0.0614226686174823,2.41636755744688,
13.3469588218718));
#36852=CARTESIAN_POINT('Ctrl Pts',(-0.0793049610672264,2.41289571560531,
13.3480814973781));
#36853=CARTESIAN_POINT('Ctrl Pts',(-0.0969030296939914,2.40790131785739,
13.3492041728844));
#36854=CARTESIAN_POINT('Ctrl Pts',(-0.113953079311686,2.40145625112176,
13.3503268483907));
#36855=CARTESIAN_POINT('Ctrl Pts',(-0.131016296558478,2.39500620690804,
13.3514503909311));
#36856=CARTESIAN_POINT('Ctrl Pts',(-0.147529969748812,2.38710350153777,
13.3525739334715));
#36857=CARTESIAN_POINT('Ctrl Pts',(-0.163248172020791,2.37786905181555,
13.3536974760119));
#36858=CARTESIAN_POINT('Ctrl Pts',(-0.177249801591024,2.36964308919856,
13.3546983173413));
#36859=CARTESIAN_POINT('Ctrl Pts',(-0.1906201923099,2.36036124374616,13.3556991586706));
#36860=CARTESIAN_POINT('Ctrl Pts',(-0.203204102907283,2.35013849800989,
13.3567));
#36861=CARTESIAN_POINT('',(-0.32227499814981,2.10003453317044,12.9993773449273));
#36862=CARTESIAN_POINT('Ctrl Pts',(-0.322274964711977,2.0998491858969,13.2496290980342));
#36863=CARTESIAN_POINT('Ctrl Pts',(-0.322279096760105,2.10867896797313,
13.2491131692747));
#36864=CARTESIAN_POINT('Ctrl Pts',(-0.321920350415243,2.11750462929075,
13.2485878344569));
#36865=CARTESIAN_POINT('Ctrl Pts',(-0.321135494975524,2.12708854194888,
13.2480030121234));
#36866=CARTESIAN_POINT('Ctrl Pts',(-0.321068373910397,2.12787282718828,
13.2479550502186));
#36867=CARTESIAN_POINT('Ctrl Pts',(-0.320953752144539,2.12915675745422,
13.2478763601958));
#36868=CARTESIAN_POINT('Ctrl Pts',(-0.320907956107554,2.12965655447462,
13.247845685479));
#36869=CARTESIAN_POINT('Ctrl Pts',(-0.320824851200874,2.1305407868138,13.2477913394896));
#36870=CARTESIAN_POINT('Ctrl Pts',(-0.320788018295633,2.13092526674389,
13.2477676831771));
#36871=CARTESIAN_POINT('Ctrl Pts',(-0.320713928190224,2.13168427926963,
13.2477209314442));
#36872=CARTESIAN_POINT('Ctrl Pts',(-0.320676705866237,2.13205881471408,
13.2476978371539));
#36873=CARTESIAN_POINT('Ctrl Pts',(-0.320601295512739,2.13280432935961,
13.2476518185281));
#36874=CARTESIAN_POINT('Ctrl Pts',(-0.320563119470224,2.13317530923575,
13.2476288946017));
#36875=CARTESIAN_POINT('Ctrl Pts',(-0.32047071803939,2.13405817780325,13.2475742812828));
#36876=CARTESIAN_POINT('Ctrl Pts',(-0.320415910126827,2.13457000330722,
13.2475425736246));
#36877=CARTESIAN_POINT('Ctrl Pts',(-0.32021696124988,2.13638676961118,13.2474298575485));
#36878=CARTESIAN_POINT('Ctrl Pts',(-0.320066074203459,2.13769094502954,
13.2473486372935));
#36879=CARTESIAN_POINT('Ctrl Pts',(-0.319526418107202,2.14211827317617,
13.2470718543437));
#36880=CARTESIAN_POINT('Ctrl Pts',(-0.319099879757327,2.14523656059779,
13.2468751088991));
#36881=CARTESIAN_POINT('Ctrl Pts',(-0.318214624174351,2.15107065737437,
13.246503519785));
#36882=CARTESIAN_POINT('Ctrl Pts',(-0.317766625696212,2.15378782325487,
13.246329027528));
#36883=CARTESIAN_POINT('Ctrl Pts',(-0.317111742987272,2.15746548616636,
13.2460908843058));
#36884=CARTESIAN_POINT('Ctrl Pts',(-0.316935198554853,2.15843132314595,
13.2460281577341));
#36885=CARTESIAN_POINT('Ctrl Pts',(-0.316346789335334,2.16156924627687,
13.2458237618279));
#36886=CARTESIAN_POINT('Ctrl Pts',(-0.315916993487235,2.16373786995476,
13.2456815626518));
#36887=CARTESIAN_POINT('Ctrl Pts',(-0.310324212617377,2.19050989458346,
13.2439144471589));
#36888=CARTESIAN_POINT('Ctrl Pts',(-0.302322265015784,2.21442925934373,
13.2422036375887));
#36889=CARTESIAN_POINT('Ctrl Pts',(-0.285036700002335,2.25117822255731,
13.2394677211623));
#36890=CARTESIAN_POINT('Ctrl Pts',(-0.27744678242937,2.26469421964319,13.2384376730576));
#36891=CARTESIAN_POINT('Ctrl Pts',(-0.268397569404883,2.27839505939664,
13.2374050602449));
#36892=CARTESIAN_POINT('Ctrl Pts',(-0.26787808281707,2.27917417581001,13.2373463839986));
#36893=CARTESIAN_POINT('Ctrl Pts',(-0.267163986518146,2.28023511644934,
13.2372665565599));
#36894=CARTESIAN_POINT('Ctrl Pts',(-0.266972319121646,2.28051890127954,
13.2372452111875));
#36895=CARTESIAN_POINT('Ctrl Pts',(-0.266650739143972,2.28099340371458,
13.2372095334631));
#36896=CARTESIAN_POINT('Ctrl Pts',(-0.266521073965429,2.28118428741845,
13.2371951844409));
#36897=CARTESIAN_POINT('Ctrl Pts',(-0.266265313025881,2.2815599315386,13.2371669538127));
#36898=CARTESIAN_POINT('Ctrl Pts',(-0.266139230206618,2.28174469952761,
13.2371530714535));
#36899=CARTESIAN_POINT('Ctrl Pts',(-0.265860228253173,2.28215264986376,
13.2371224277996));
#36900=CARTESIAN_POINT('Ctrl Pts',(-0.265707219923848,2.28237577169351,
13.2371056725679));
#36901=CARTESIAN_POINT('Ctrl Pts',(-0.265183414701852,2.28313754345954,
13.2370484831727));
#36902=CARTESIAN_POINT('Ctrl Pts',(-0.264811256220294,2.28367526195429,
13.2370081409302));
#36903=CARTESIAN_POINT('Ctrl Pts',(-0.261040237666083,2.28908858672199,
13.2366022348204));
#36904=CARTESIAN_POINT('Ctrl Pts',(-0.257508494216956,2.29387079632716,
13.236245516732));
#36905=CARTESIAN_POINT('Ctrl Pts',(-0.251490179513832,2.30156509945613,
13.2356697645654));
#36906=CARTESIAN_POINT('Ctrl Pts',(-0.249080618848116,2.30453519774991,
13.2354470507446));
#36907=CARTESIAN_POINT('Ctrl Pts',(-0.227921873930415,2.3296874985036,13.2335502049417));
#36908=CARTESIAN_POINT('Ctrl Pts',(-0.206306182745667,2.34928439089276,
13.2319863617403));
#36909=CARTESIAN_POINT('Ctrl Pts',(-0.175724206183174,2.37027184458794,
13.2298440779071));
#36910=CARTESIAN_POINT('Ctrl Pts',(-0.168924958401285,2.37457277729758,
13.2293725702221));
#36911=CARTESIAN_POINT('Ctrl Pts',(-0.159612980318856,2.37998628535088,
13.2287287631247));
#36912=CARTESIAN_POINT('Ctrl Pts',(-0.157236357768794,2.38132783470637,
13.2285646240746));
#36913=CARTESIAN_POINT('Ctrl Pts',(-0.153239324349628,2.38351759894937,
13.2282887090762));
#36914=CARTESIAN_POINT('Ctrl Pts',(-0.151628188883919,2.38438250924227,
13.2281775291729));
#36915=CARTESIAN_POINT('Ctrl Pts',(-0.149450151561957,2.38552798053293,
13.2280272467451));
#36916=CARTESIAN_POINT('Ctrl Pts',(-0.148889635844594,2.38582066370049,
13.227988573316));
#36917=CARTESIAN_POINT('Ctrl Pts',(-0.148002691761106,2.38628048020011,
13.2279273787445));
#36918=CARTESIAN_POINT('Ctrl Pts',(-0.147676831227424,2.38644871029385,
13.2279048962942));
#36919=CARTESIAN_POINT('Ctrl Pts',(-0.147000794286862,2.38679626372173,
13.2278582539206));
#36920=CARTESIAN_POINT('Ctrl Pts',(-0.146650575398872,2.38697550268047,
13.2278340910791));
#36921=CARTESIAN_POINT('Ctrl Pts',(-0.145851351666812,2.38738269330252,
13.2277789495913));
#36922=CARTESIAN_POINT('Ctrl Pts',(-0.145402139816339,2.38761023438864,
13.2277479566028));
#36923=CARTESIAN_POINT('Ctrl Pts',(-0.144030454665508,2.38830100467042,
13.2276533167197));
#36924=CARTESIAN_POINT('Ctrl Pts',(-0.143106294166735,2.38876085208229,
13.2275895516774));
#36925=CARTESIAN_POINT('Ctrl Pts',(-0.136364047529785,2.39207536947543,
13.2271243128556));
#36926=CARTESIAN_POINT('Ctrl Pts',(-0.130463600126605,2.39475822995283,
13.2267169066211));
#36927=CARTESIAN_POINT('Ctrl Pts',(-0.105322239585872,2.40528689077244,
13.224978134888));
#36928=CARTESIAN_POINT('Ctrl Pts',(-0.0854296244791532,2.41143921684941,
13.2235911177663));
#36929=CARTESIAN_POINT('Ctrl Pts',(-0.062997392440134,2.41606495390252,
13.2220422259398));
#36930=CARTESIAN_POINT('Ctrl Pts',(-0.0609038418287308,2.41647503622835,
13.221897863492));
#36931=CARTESIAN_POINT('Ctrl Pts',(-0.0564022552593713,2.41731047904094,
13.2215879942009));
#36932=CARTESIAN_POINT('Ctrl Pts',(-0.0539931288313977,2.4177292819042,
13.2214224910965));
#36933=CARTESIAN_POINT('Ctrl Pts',(-0.0435408139573372,2.41942400013965,
13.2207062958807));
#36934=CARTESIAN_POINT('Ctrl Pts',(-0.0354553710290919,2.42042225236733,
13.2201569582779));
#36935=CARTESIAN_POINT('Ctrl Pts',(-0.0217979875431622,2.42158508388674,
13.2192443399585));
#36936=CARTESIAN_POINT('Ctrl Pts',(-0.016243823534985,2.42191344044718,
13.2188774446051));
#36937=CARTESIAN_POINT('Ctrl Pts',(-0.00533430417689137,2.42227529849871,
13.2181683785087));
#36938=CARTESIAN_POINT('Ctrl Pts',(1.90551163048386E-5,2.42231945467463,
13.2178259027443));
#36939=CARTESIAN_POINT('Ctrl Pts',(0.00594829671087206,2.42222061741735,
13.217454434595));
#36940=CARTESIAN_POINT('Ctrl Pts',(0.00652516779550501,2.42220945163058,
13.2174183759355));
#36941=CARTESIAN_POINT('Ctrl Pts',(0.00738255421381879,2.42219055271838,
13.2173649086578));
#36942=CARTESIAN_POINT('Ctrl Pts',(0.00766309044230832,2.42218400241788,
13.2173474341973));
#36943=CARTESIAN_POINT('Ctrl Pts',(0.00814210509455091,2.42217219180168,
13.2173176311726));
#36944=CARTESIAN_POINT('Ctrl Pts',(0.00834058738309613,2.42216711447422,
13.217305292268));
#36945=CARTESIAN_POINT('Ctrl Pts',(0.00874875374904936,2.42215629581398,
13.217279939067));
#36946=CARTESIAN_POINT('Ctrl Pts',(0.00895843649401029,2.42215053319981,
13.2172669260097));
#36947=CARTESIAN_POINT('Ctrl Pts',(0.00952459711261236,2.42213442047981,
13.2172318200005));
#36948=CARTESIAN_POINT('Ctrl Pts',(0.00988106501800944,2.4221236833346,
13.2172097488915));
#36949=CARTESIAN_POINT('Ctrl Pts',(0.011197895396698,2.42208183125278,13.2171283333454));
#36950=CARTESIAN_POINT('Ctrl Pts',(0.0121581474168493,2.42204701270314,
13.2170691947901));
#36951=CARTESIAN_POINT('Ctrl Pts',(0.0133507180898196,2.42199842870043,
13.2169960194764));
#36952=CARTESIAN_POINT('Ctrl Pts',(0.0135831830166143,2.42198870616678,
13.2169817683792));
#36953=CARTESIAN_POINT('Ctrl Pts',(0.0327486286671742,2.42116634483214,
13.2158078839908));
#36954=CARTESIAN_POINT('Ctrl Pts',(0.0515763005692398,2.4186854391674,13.2147372668815));
#36955=CARTESIAN_POINT('Ctrl Pts',(0.0863009112098291,2.41094940647918,
13.2127445220053));
#36956=CARTESIAN_POINT('Ctrl Pts',(0.102218588373151,2.4060861281953,13.2118230268691));
#36957=CARTESIAN_POINT('Ctrl Pts',(0.126801722989407,2.39644275553252,13.2103120140148));
#36958=CARTESIAN_POINT('Ctrl Pts',(0.135745619543746,2.39245527165815,13.2097428740567));
#36959=CARTESIAN_POINT('Ctrl Pts',(0.147383728801952,2.38661762997997,13.2089676883943));
#36960=CARTESIAN_POINT('Ctrl Pts',(0.150251698682107,2.38512463107413,13.2087737800204));
#36961=CARTESIAN_POINT('Ctrl Pts',(0.154319881571491,2.38292840467492,13.2084943467172));
#36962=CARTESIAN_POINT('Ctrl Pts',(0.155538817366452,2.38226013572395,13.2084100511051));
#36963=CARTESIAN_POINT('Ctrl Pts',(0.15740539956484,2.3812210388538,13.2082800720528));
#36964=CARTESIAN_POINT('Ctrl Pts',(0.158056155129065,2.38085580698524,13.208234588334));
#36965=CARTESIAN_POINT('Ctrl Pts',(0.159263304780322,2.38017277872948,13.208149899586));
#36966=CARTESIAN_POINT('Ctrl Pts',(0.159820032024022,2.37985557622644,13.208110716023));
#36967=CARTESIAN_POINT('Ctrl Pts',(0.160735856784765,2.37933014924153,13.2080460492966));
#36968=CARTESIAN_POINT('Ctrl Pts',(0.161095506356642,2.37912288648688,13.2080206009424));
#36969=CARTESIAN_POINT('Ctrl Pts',(0.16179753380385,2.37871650570222,13.2079708215053));
#36970=CARTESIAN_POINT('Ctrl Pts',(0.162139947139263,2.37851745014507,13.2079464927194));
#36971=CARTESIAN_POINT('Ctrl Pts',(0.162928257195209,2.37805723450644,13.2078903692799));
#36972=CARTESIAN_POINT('Ctrl Pts',(0.163373893592153,2.37779563268996,13.207858558606));
#36973=CARTESIAN_POINT('Ctrl Pts',(0.16479336888695,2.37695776148477,13.20775696395));
#36974=CARTESIAN_POINT('Ctrl Pts',(0.165764794604688,2.37637743918968,13.2076870323102));
#36975=CARTESIAN_POINT('Ctrl Pts',(0.174463034386662,2.37111882153216,13.2070571750442));
#36976=CARTESIAN_POINT('Ctrl Pts',(0.181992345668761,2.36612313963779,13.2064855800994));
#36977=CARTESIAN_POINT('Ctrl Pts',(0.190088539838872,2.3602469378859,13.2058400666763));
#36978=CARTESIAN_POINT('Ctrl Pts',(0.190873105205912,2.35967206113675,13.2057771818182));
#36979=CARTESIAN_POINT('Ctrl Pts',(0.213642754672032,2.3428290456307,13.203942479105));
#36980=CARTESIAN_POINT('Ctrl Pts',(0.23346866267692,2.3238328322786,13.2020678405428));
#36981=CARTESIAN_POINT('Ctrl Pts',(0.253567017407664,2.2989633489604,13.1999235837407));
#36982=CARTESIAN_POINT('Ctrl Pts',(0.25640156704276,2.29529691709814,13.1996146376598));
#36983=CARTESIAN_POINT('Ctrl Pts',(0.262571558963039,2.28695016637314,13.1989291453272));
#36984=CARTESIAN_POINT('Ctrl Pts',(0.265863020899388,2.28223899394042,13.1985542713795));
#36985=CARTESIAN_POINT('Ctrl Pts',(0.270738766509925,2.27484668186106,13.1979872136151));
#36986=CARTESIAN_POINT('Ctrl Pts',(0.272413020193182,2.27222656602066,13.197790177345));
#36987=CARTESIAN_POINT('Ctrl Pts',(0.27431747495842,2.2691489241659,13.1975636664284));
#36988=CARTESIAN_POINT('Ctrl Pts',(0.274584754747601,2.26871469432964,13.1975318205444));
#36989=CARTESIAN_POINT('Ctrl Pts',(0.274990271116812,2.26805236550117,13.1974834201294));
#36990=CARTESIAN_POINT('Ctrl Pts',(0.275129255395169,2.26782472876896,13.1974668165278));
#36991=CARTESIAN_POINT('Ctrl Pts',(0.275370255986218,2.26742889965142,13.1974379996797));
#36992=CARTESIAN_POINT('Ctrl Pts',(0.275472400489772,2.26726078706444,13.1974257779592));
#36993=CARTESIAN_POINT('Ctrl Pts',(0.275686360584953,2.26690791727649,13.1974001602889));
#36994=CARTESIAN_POINT('Ctrl Pts',(0.275798144013824,2.266723141829,13.1973867664853));
#36995=CARTESIAN_POINT('Ctrl Pts',(0.276109705297572,2.26620696736693,13.1973494074915));
#36996=CARTESIAN_POINT('Ctrl Pts',(0.276309072990298,2.26587531928466,13.1973254693052));
#36997=CARTESIAN_POINT('Ctrl Pts',(0.27710915226221,2.26453894275921,13.1972292699536));
#36998=CARTESIAN_POINT('Ctrl Pts',(0.277704994491041,2.26353128778696,13.1971573232983));
#36999=CARTESIAN_POINT('Ctrl Pts',(0.288224106363828,2.24551865660134,13.1958812809199));
#37000=CARTESIAN_POINT('Ctrl Pts',(0.296575668554731,2.22763988250608,13.1947726313028));
#37001=CARTESIAN_POINT('Ctrl Pts',(0.308784109651684,2.19370899862269,13.192754278719));
#37002=CARTESIAN_POINT('Ctrl Pts',(0.313143591071176,2.17791063254559,13.1918453988327));
#37003=CARTESIAN_POINT('Ctrl Pts',(0.318671921027294,2.14964035505235,13.1901940816162));
#37004=CARTESIAN_POINT('Ctrl Pts',(0.320350329878614,2.13730375395253,13.189465719512));
#37005=CARTESIAN_POINT('Ctrl Pts',(0.321421511985437,2.12348222747628,13.188628039931));
#37006=CARTESIAN_POINT('Ctrl Pts',(0.32152213037569,2.12206179849046,13.188541706775));
#37007=CARTESIAN_POINT('Ctrl Pts',(0.321661985134296,2.1198826568207,13.1884088655862));
#37008=CARTESIAN_POINT('Ctrl Pts',(0.321707958718722,2.11912438245705,13.1883625679059));
#37009=CARTESIAN_POINT('Ctrl Pts',(0.321779171870183,2.11787680686395,13.1882862724147));
#37010=CARTESIAN_POINT('Ctrl Pts',(0.321805977575803,2.11738759515941,13.1882563236448));
#37011=CARTESIAN_POINT('Ctrl Pts',(0.321855651404073,2.11644154815703,13.1881983473708));
#37012=CARTESIAN_POINT('Ctrl Pts',(0.321878662741033,2.11598472130233,13.1881703244192));
#37013=CARTESIAN_POINT('Ctrl Pts',(0.321919150891103,2.11514538006495,13.1881187861475));
#37014=CARTESIAN_POINT('Ctrl Pts',(0.321936918697785,2.11476287997605,13.188095279992));
#37015=CARTESIAN_POINT('Ctrl Pts',(0.321974403078859,2.11392366213582,13.1880436637399));
#37016=CARTESIAN_POINT('Ctrl Pts',(0.321993829631447,2.11346693287672,13.1880155446054));
#37017=CARTESIAN_POINT('Ctrl Pts',(0.322044177814712,2.11222077399748,13.1879387462635));
#37018=CARTESIAN_POINT('Ctrl Pts',(0.322073168321577,2.11143127337538,13.1878900066494));
#37019=CARTESIAN_POINT('Ctrl Pts',(0.322198926036979,2.1076248755538,13.1876546069605));
#37020=CARTESIAN_POINT('Ctrl Pts',(0.322256205657304,2.10460690621253,13.1874667145118));
#37021=CARTESIAN_POINT('Ctrl Pts',(0.322276998411832,2.1003889410247,13.1872022789311));
#37022=CARTESIAN_POINT('Ctrl Pts',(0.322276213121028,2.09918921377692,13.1871268577795));
#37023=CARTESIAN_POINT('Ctrl Pts',(0.322263229994967,2.09710807890913,13.1869956629524));
#37024=CARTESIAN_POINT('Ctrl Pts',(0.322254114776638,2.09622665940697,13.1869399850383));
#37025=CARTESIAN_POINT('Ctrl Pts',(0.322218656853498,2.09377193648883,13.1867846063821));
#37026=CARTESIAN_POINT('Ctrl Pts',(0.322184407674301,2.09219878778271,13.1866846659551));
#37027=CARTESIAN_POINT('Ctrl Pts',(0.32123049791921,2.05941765234215,13.1845944719271));
#37028=CARTESIAN_POINT('Ctrl Pts',(0.315791810869729,2.02851068592621,13.1824553493103));
#37029=CARTESIAN_POINT('Ctrl Pts',(0.302228035049034,1.98746631691699,13.1795571754119));
#37030=CARTESIAN_POINT('Ctrl Pts',(0.297821129502904,1.9762734584719,13.1787635063836));
#37031=CARTESIAN_POINT('Ctrl Pts',(0.292126235947137,1.96388964734301,13.1779008269239));
#37032=CARTESIAN_POINT('Ctrl Pts',(0.291442855257529,1.96243245948172,13.1777995718464));
#37033=CARTESIAN_POINT('Ctrl Pts',(0.290568308307015,1.96060341303054,13.1776728572627));
#37034=CARTESIAN_POINT('Ctrl Pts',(0.290387312074675,1.96022675777576,13.1776467833436));
#37035=CARTESIAN_POINT('Ctrl Pts',(0.290098206548865,1.95962811126287,13.1776053758506));
#37036=CARTESIAN_POINT('Ctrl Pts',(0.289990574648707,1.95940589199261,13.1775900126853));
#37037=CARTESIAN_POINT('Ctrl Pts',(0.289787030902136,1.95898687907789,13.1775610584638));
#37038=CARTESIAN_POINT('Ctrl Pts',(0.289691174682163,1.95879006103359,13.1775474641382));
#37039=CARTESIAN_POINT('Ctrl Pts',(0.289472680526909,1.95834259384912,13.1775165708343));
#37040=CARTESIAN_POINT('Ctrl Pts',(0.289349917800132,1.95809200671105,13.1774992798084));
#37041=CARTESIAN_POINT('Ctrl Pts',(0.288984145472422,1.95734782870726,13.1774479576333));
#37042=CARTESIAN_POINT('Ctrl Pts',(0.288740195667025,1.95685469715812,13.1774139850255));
#37043=CARTESIAN_POINT('Ctrl Pts',(0.287053077269109,1.95346613820736,13.1771807745509));
#37044=CARTESIAN_POINT('Ctrl Pts',(0.285567579417923,1.9505918297393,13.1769841269981));
#37045=CARTESIAN_POINT('Ctrl Pts',(0.267766696179407,1.917384467472,13.1747202927847));
#37046=CARTESIAN_POINT('Ctrl Pts',(0.246731427960973,1.88982893112825,13.1729000995787));
#37047=CARTESIAN_POINT('Ctrl Pts',(0.213156448041101,1.85799791883507,13.170241273147));
#37048=CARTESIAN_POINT('Ctrl Pts',(0.204145711070526,1.8503499248823,13.1695483304205));
#37049=CARTESIAN_POINT('Ctrl Pts',(0.193636140072587,1.84237987789917,13.1687510075561));
#37050=CARTESIAN_POINT('Ctrl Pts',(0.192530646211191,1.84155265094913,13.1686672719658));
#37051=CARTESIAN_POINT('Ctrl Pts',(0.190822306579979,1.84029136577644,13.1685380631465));
#37052=CARTESIAN_POINT('Ctrl Pts',(0.190223209779657,1.83985223847697,13.1684927864428));
#37053=CARTESIAN_POINT('Ctrl Pts',(0.189106138489201,1.83903936697325,13.1684084268837));
#37054=CARTESIAN_POINT('Ctrl Pts',(0.188588559705034,1.83866508319182,13.1683693651045));
#37055=CARTESIAN_POINT('Ctrl Pts',(0.187733104604984,1.83805033108631,13.1683048433984));
#37056=CARTESIAN_POINT('Ctrl Pts',(0.187395869067517,1.83780897066737,13.1682794179192));
#37057=CARTESIAN_POINT('Ctrl Pts',(0.186735091745805,1.83733797658044,13.1682296187032));
#37058=CARTESIAN_POINT('Ctrl Pts',(0.18641158982547,1.83710828804872,13.1682052471355));
#37059=CARTESIAN_POINT('Ctrl Pts',(0.185663919414702,1.83657951099812,13.1681489404626));
#37060=CARTESIAN_POINT('Ctrl Pts',(0.18523945175659,1.83628084918552,13.1681169890894));
#37061=CARTESIAN_POINT('Ctrl Pts',(0.183878627009978,1.83532825888816,13.1680146011897));
#37062=CARTESIAN_POINT('Ctrl Pts',(0.182939522369073,1.83467828751532,13.1679440139995));
#37063=CARTESIAN_POINT('Ctrl Pts',(0.17429067854855,1.82876001380216,13.1672945380636));
#37064=CARTESIAN_POINT('Ctrl Pts',(0.166359545756294,1.82382461523632,13.1667031769179));
#37065=CARTESIAN_POINT('Ctrl Pts',(0.152383581031761,1.81594825377416,13.1656666821713));
#37066=CARTESIAN_POINT('Ctrl Pts',(0.146440157357755,1.81283903243551,13.1652275873111));
#37067=CARTESIAN_POINT('Ctrl Pts',(0.12042370678694,1.80024666675599,13.1633146309699));
#37068=CARTESIAN_POINT('Ctrl Pts',(0.0994977094055758,1.79266628304339,
13.161793517804));
#37069=CARTESIAN_POINT('Ctrl Pts',(0.0671131119549469,1.78459230919784,
13.159560977551));
#37070=CARTESIAN_POINT('Ctrl Pts',(0.0561298973154182,1.7824536686134,13.1588249075766));
#37071=CARTESIAN_POINT('Ctrl Pts',(0.0440448436074629,1.78074732351417,
13.1580528492691));
#37072=CARTESIAN_POINT('Ctrl Pts',(0.0430323937090804,1.78060927870665,
13.1579884575212));
#37073=CARTESIAN_POINT('Ctrl Pts',(0.0412840281338727,1.78037935829573,
13.1578777799429));
#37074=CARTESIAN_POINT('Ctrl Pts',(0.040548427256948,1.78028520419719,13.1578313719749));
#37075=CARTESIAN_POINT('Ctrl Pts',(0.0395038875445841,1.78015517010413,
13.1577657041466));
#37076=CARTESIAN_POINT('Ctrl Pts',(0.0391952187420621,1.78011719775523,
13.1577463274058));
#37077=CARTESIAN_POINT('Ctrl Pts',(0.0386644096994556,1.78005267762069,
13.1577130554387));
#37078=CARTESIAN_POINT('Ctrl Pts',(0.0384422963018082,1.78002591428169,
13.1576991479614));
#37079=CARTESIAN_POINT('Ctrl Pts',(0.0380164320243075,1.77997505001049,
13.1576725116372));
#37080=CARTESIAN_POINT('Ctrl Pts',(0.0378126863099761,1.77995091239896,
13.1576597806995));
#37081=CARTESIAN_POINT('Ctrl Pts',(0.0373319664819103,1.77989442731473,
13.157629772725));
#37082=CARTESIAN_POINT('Ctrl Pts',(0.0370549726278806,1.77986224466571,
13.1576125050623));
#37083=CARTESIAN_POINT('Ctrl Pts',(0.0362345377804529,1.77976800116962,
13.1575614271024));
#37084=CARTESIAN_POINT('Ctrl Pts',(0.0356909766952838,1.77970696386599,
13.1575276742666));
#37085=CARTESIAN_POINT('Ctrl Pts',(0.0308395887537717,1.77917469743018,
13.1572271853582));
#37086=CARTESIAN_POINT('Ctrl Pts',(0.0265225662064618,1.77878898996396,
13.1569651504885));
#37087=CARTESIAN_POINT('Ctrl Pts',(-0.00745675486368154,1.77644286677046,
13.1549354959716));
#37088=CARTESIAN_POINT('Ctrl Pts',(-0.0372567417464889,1.77850774781622,
13.1533404233214));
#37089=CARTESIAN_POINT('Ctrl Pts',(-0.080973642123726,1.78770586424096,
13.1508021649634));
#37090=CARTESIAN_POINT('Ctrl Pts',(-0.0953594772313317,1.79179415623468,
13.1499349706324));
#37091=CARTESIAN_POINT('Ctrl Pts',(-0.110899772519987,1.79740302611123,
13.1489381186997));
#37092=CARTESIAN_POINT('Ctrl Pts',(-0.112386717573886,1.797952133385,13.1488421243433));
#37093=CARTESIAN_POINT('Ctrl Pts',(-0.114985459082477,1.79893365720745,
13.1486732500931));
#37094=CARTESIAN_POINT('Ctrl Pts',(-0.116099026324078,1.79936132219953,
13.1486005291913));
#37095=CARTESIAN_POINT('Ctrl Pts',(-0.117707671663017,1.79998939205323,
13.1484949494165));
#37096=CARTESIAN_POINT('Ctrl Pts',(-0.118204675336389,1.80018486433785,
13.1484622564439));
#37097=CARTESIAN_POINT('Ctrl Pts',(-0.119070908759118,1.80052804395081,
13.1484051466468));
#37098=CARTESIAN_POINT('Ctrl Pts',(-0.119440356285209,1.80067520139351,
13.1483807483987));
#37099=CARTESIAN_POINT('Ctrl Pts',(-0.120153470884081,1.800960777946,13.1483335748189));
#37100=CARTESIAN_POINT('Ctrl Pts',(-0.120497173692491,1.80109910668836,
13.1483108025689));
#37101=CARTESIAN_POINT('Ctrl Pts',(-0.121311385508265,1.80142843197987,
13.1482567711376));
#37102=CARTESIAN_POINT('Ctrl Pts',(-0.12178168208099,1.80161994807168,13.1482254944164));
#37103=CARTESIAN_POINT('Ctrl Pts',(-0.123432484548044,1.80229674761582,
13.1481154697758));
#37104=CARTESIAN_POINT('Ctrl Pts',(-0.124610546548384,1.80278792700235,
13.1480365221996));
#37105=CARTESIAN_POINT('Ctrl Pts',(-0.141732461682995,1.81004640413557,
13.1468827293306));
#37106=CARTESIAN_POINT('Ctrl Pts',(-0.157105573400245,1.81808008338434,
13.1457636687784));
#37107=CARTESIAN_POINT('Ctrl Pts',(-0.181832283745838,1.83365439735847,
13.1438210455253));
#37108=CARTESIAN_POINT('Ctrl Pts',(-0.191547690559377,1.84055363580459,
13.1430164424767));
#37109=CARTESIAN_POINT('Ctrl Pts',(-0.210159366238616,1.85538670186657,
13.1414058370563));
#37110=CARTESIAN_POINT('Ctrl Pts',(-0.219043076928487,1.86330868294766,
13.1406010764666));
#37111=CARTESIAN_POINT('Ctrl Pts',(-0.233378553863066,1.87759221472451,
13.139261565831));
#37112=CARTESIAN_POINT('Ctrl Pts',(-0.239057998629047,1.88370836184933,
13.1387185403232));
#37113=CARTESIAN_POINT('Ctrl Pts',(-0.245345128406196,1.89102954823742,
13.1381094099944));
#37114=CARTESIAN_POINT('Ctrl Pts',(-0.246190089423904,1.89202567045372,
13.1380273700341));
#37115=CARTESIAN_POINT('Ctrl Pts',(-0.247278040055303,1.89332417432803,
13.1379215393394));
#37116=CARTESIAN_POINT('Ctrl Pts',(-0.247526557228097,1.89362187741586,
13.1378973512053));
#37117=CARTESIAN_POINT('Ctrl Pts',(-0.247928042885322,1.8941045925644,13.1378582537083));
#37118=CARTESIAN_POINT('Ctrl Pts',(-0.248081342120482,1.89428932710085,
13.1378433201413));
#37119=CARTESIAN_POINT('Ctrl Pts',(-0.248375036564697,1.89464405184302,
13.1378147007844));
#37120=CARTESIAN_POINT('Ctrl Pts',(-0.248515463315888,1.89481401430634,
13.1378010127143));
#37121=CARTESIAN_POINT('Ctrl Pts',(-0.24883809811766,1.89520532539957,13.1377695543678));
#37122=CARTESIAN_POINT('Ctrl Pts',(-0.249020185838086,1.89542677382854,
13.1377517929243));
#37123=CARTESIAN_POINT('Ctrl Pts',(-0.249583483061063,1.89611370178924,
13.137696824039));
#37124=CARTESIAN_POINT('Ctrl Pts',(-0.249963687524055,1.89658000946777,
13.13765968937));
#37125=CARTESIAN_POINT('Ctrl Pts',(-0.25310157907732,1.90045060697281,13.1373529126579));
#37126=CARTESIAN_POINT('Ctrl Pts',(-0.255791054563873,1.90390994258175,
13.1370880602181));
#37127=CARTESIAN_POINT('Ctrl Pts',(-0.258519376379704,1.90757094400929,
13.1368160750597));
#37128=CARTESIAN_POINT('Ctrl Pts',(-0.258629317155157,1.90771873242204,
13.1368051093541));
#37129=CARTESIAN_POINT('Ctrl Pts',(-0.259217291643297,1.90851053655655,
13.1367464322878));
#37130=CARTESIAN_POINT('Ctrl Pts',(-0.259693050873104,1.90915624650303,
13.1366988426192));
#37131=CARTESIAN_POINT('Ctrl Pts',(-0.260341359482322,1.91004305736347,
13.1366338299425));
#37132=CARTESIAN_POINT('Ctrl Pts',(-0.260515990228434,1.91028262507251,
13.1366163015428));
#37133=CARTESIAN_POINT('Ctrl Pts',(-0.277871270752546,1.9341606662873,13.1348726132801));
#37134=CARTESIAN_POINT('Ctrl Pts',(-0.29175920876836,1.9600281575405,13.1333031384424));
#37135=CARTESIAN_POINT('Ctrl Pts',(-0.307457857108944,2.00213483659472,
13.1307435365567));
#37136=CARTESIAN_POINT('Ctrl Pts',(-0.311861221815125,2.01723286754563,
13.12982714177));
#37137=CARTESIAN_POINT('Ctrl Pts',(-0.315393806445226,2.03374802692001,
13.1288003774934));
#37138=CARTESIAN_POINT('Ctrl Pts',(-0.315635042852909,2.03490701461971,
13.1287282041958));
#37139=CARTESIAN_POINT('Ctrl Pts',(-0.315975515215974,2.0365891734354,13.1286232722474));
#37140=CARTESIAN_POINT('Ctrl Pts',(-0.316079850795476,2.03711131216712,
13.1285906765864));
#37141=CARTESIAN_POINT('Ctrl Pts',(-0.316259809667588,2.03802366259876,
13.128533676587));
#37142=CARTESIAN_POINT('Ctrl Pts',(-0.316336006158008,2.03841376116076,
13.1285092905967));
#37143=CARTESIAN_POINT('Ctrl Pts',(-0.316481931661086,2.03916826314085,
13.1284620970564));
#37144=CARTESIAN_POINT('Ctrl Pts',(-0.316551753491421,2.03953264817315,
13.1284392925077));
#37145=CARTESIAN_POINT('Ctrl Pts',(-0.316715987653266,2.04039783139133,
13.1283851160599));
#37146=CARTESIAN_POINT('Ctrl Pts',(-0.316809841422015,2.04089873341936,
13.12835372641));
#37147=CARTESIAN_POINT('Ctrl Pts',(-0.317136477369064,2.04266514112886,
13.1282429465762));
#37148=CARTESIAN_POINT('Ctrl Pts',(-0.317362865792543,2.04393180350001,
13.1281633531708));
#37149=CARTESIAN_POINT('Ctrl Pts',(-0.320721263789985,2.06339459902744,
13.126937904173));
#37150=CARTESIAN_POINT('Ctrl Pts',(-0.322290923176652,2.08182222789064,
13.1257415472982));
#37151=CARTESIAN_POINT('Ctrl Pts',(-0.322253006248937,2.1254414566591,13.1228329141351));
#37152=CARTESIAN_POINT('Ctrl Pts',(-0.319284709249872,2.15051232414512,
13.1210974374452));
#37153=CARTESIAN_POINT('Ctrl Pts',(-0.313323395040868,2.17543101939966,
13.1194202283871));
#37154=CARTESIAN_POINT('Ctrl Pts',(-0.313215065641186,2.17587958373119,
13.1193900557357));
#37155=CARTESIAN_POINT('Ctrl Pts',(-0.311632950742687,2.1823695985687,13.118953794462));
#37156=CARTESIAN_POINT('Ctrl Pts',(-0.30998544133701,2.18836789935263,13.118554197901));
#37157=CARTESIAN_POINT('Ctrl Pts',(-0.307969276497932,2.19495550916034,
13.1181221692465));
#37158=CARTESIAN_POINT('Ctrl Pts',(-0.307771318510728,2.19559518558902,
13.118080290219));
#37159=CARTESIAN_POINT('Ctrl Pts',(-0.307491176693233,2.19649053837735,
13.1180217781899));
#37160=CARTESIAN_POINT('Ctrl Pts',(-0.30741066653164,2.19674673040679,13.1180050480017));
#37161=CARTESIAN_POINT('Ctrl Pts',(-0.307262748794474,2.19721537175826,
13.117974466834));
#37162=CARTESIAN_POINT('Ctrl Pts',(-0.307195440914091,2.19742785220539,
13.1179606099689));
#37163=CARTESIAN_POINT('Ctrl Pts',(-0.30705812660608,2.19785977501212,13.1179324598245));
#37164=CARTESIAN_POINT('Ctrl Pts',(-0.306988105311617,2.19807921226357,
13.1179181674523));
#37165=CARTESIAN_POINT('Ctrl Pts',(-0.30681304730563,2.19862579624533,13.1178825899624));
#37166=CARTESIAN_POINT('Ctrl Pts',(-0.306707722241865,2.19895285140819,
13.1178613219114));
#37167=CARTESIAN_POINT('Ctrl Pts',(-0.306309056872683,2.20018403462883,
13.1177813331873));
#37168=CARTESIAN_POINT('Ctrl Pts',(-0.306012236388668,2.20108704343583,
13.1177228156871));
#37169=CARTESIAN_POINT('Ctrl Pts',(-0.303709753905448,2.2079887386341,13.1172766221947));
#37170=CARTESIAN_POINT('Ctrl Pts',(-0.301531721568479,2.21392899514777,
13.1168986965569));
#37171=CARTESIAN_POINT('Ctrl Pts',(-0.294696281257612,2.23099909341191,
13.11582010347));
#37172=CARTESIAN_POINT('Ctrl Pts',(-0.289587036975815,2.24193679376754,
13.1151381732785));
#37173=CARTESIAN_POINT('Ctrl Pts',(-0.272109580616609,2.27445735314753,
13.1130676153323));
#37174=CARTESIAN_POINT('Ctrl Pts',(-0.257850809630431,2.29491499395365,
13.1116967463171));
#37175=CARTESIAN_POINT('Ctrl Pts',(-0.241062068602797,2.31389364109768,
13.1102041849633));
#37176=CARTESIAN_POINT('Ctrl Pts',(-0.240740059711737,2.31425600170733,
13.1101756000938));
#37177=CARTESIAN_POINT('Ctrl Pts',(-0.236027419658964,2.31953515737534,
13.1097578665379));
#37178=CARTESIAN_POINT('Ctrl Pts',(-0.231488026074143,2.32431654530755,
13.1093631427797));
#37179=CARTESIAN_POINT('Ctrl Pts',(-0.226068716071867,2.32968497266832,
13.1088988886345));
#37180=CARTESIAN_POINT('Ctrl Pts',(-0.225328463125049,2.33041122959249,
13.1088356196183));
#37181=CARTESIAN_POINT('Ctrl Pts',(-0.224223004852126,2.33148536474811,
13.1087413467001));
#37182=CARTESIAN_POINT('Ctrl Pts',(-0.223860462286072,2.33183598387218,
13.108710462523));
#37183=CARTESIAN_POINT('Ctrl Pts',(-0.223213707639791,2.33245853623972,
13.1086554252819));
#37184=CARTESIAN_POINT('Ctrl Pts',(-0.222929817313236,2.33273080350381,
13.108631286793));
#37185=CARTESIAN_POINT('Ctrl Pts',(-0.222331578477663,2.33330245022302,
13.1085804613781));
#37186=CARTESIAN_POINT('Ctrl Pts',(-0.222017122330506,2.33360171544228,
13.1085537695836));
#37187=CARTESIAN_POINT('Ctrl Pts',(-0.22118787285423,2.3343877182231,13.1084834430083));
#37188=CARTESIAN_POINT('Ctrl Pts',(-0.220672079589491,2.33487339318971,
13.1084397626066));
#37189=CARTESIAN_POINT('Ctrl Pts',(-0.218358157672523,2.33703784968652,
13.1082440812253));
#37190=CARTESIAN_POINT('Ctrl Pts',(-0.216542482121872,2.33869767511017,
13.1080912735306));
#37191=CARTESIAN_POINT('Ctrl Pts',(-0.203113995651687,2.35069420324249,
13.1069662180705));
#37192=CARTESIAN_POINT('Ctrl Pts',(-0.190787464491034,2.3601977997522,13.1059594533601));
#37193=CARTESIAN_POINT('Ctrl Pts',(-0.150962634025548,2.38654652239965,
13.1027875471387));
#37194=CARTESIAN_POINT('Ctrl Pts',(-0.121589723911327,2.40019076005394,
13.1005384838953));
#37195=CARTESIAN_POINT('Ctrl Pts',(-0.0892470126214924,2.40967464362763,
13.09840682535));
#37196=CARTESIAN_POINT('Ctrl Pts',(-0.0878083411675966,2.41008564880571,
13.0983127252413));
#37197=CARTESIAN_POINT('Ctrl Pts',(-0.0859563561977601,2.41060080807551,
13.0981925618348));
#37198=CARTESIAN_POINT('Ctrl Pts',(-0.0855456567573275,2.41071417373993,
13.0981659753228));
#37199=CARTESIAN_POINT('Ctrl Pts',(-0.0848949273519165,2.41089240703937,
13.0981239486413));
#37200=CARTESIAN_POINT('Ctrl Pts',(-0.0846550468944974,2.41095781141678,
13.0981084772973));
#37201=CARTESIAN_POINT('Ctrl Pts',(-0.084225280111226,2.41107445490901,
13.0980807970893));
#37202=CARTESIAN_POINT('Ctrl Pts',(-0.0840354239436804,2.41112579743518,
13.0980685822451));
#37203=CARTESIAN_POINT('Ctrl Pts',(-0.0835892051609647,2.41124602948818,
13.0980399048934));
#37204=CARTESIAN_POINT('Ctrl Pts',(-0.0833328047323441,2.41131477598768,
13.0980234508257));
#37205=CARTESIAN_POINT('Ctrl Pts',(-0.0825901501201167,2.41151291451913,
13.0979758613039));
#37206=CARTESIAN_POINT('Ctrl Pts',(-0.082103674687822,2.41164148539618,
13.0979447735235));
#37207=CARTESIAN_POINT('Ctrl Pts',(-0.0787640224052549,2.41251576130564,
13.097731931086));
#37208=CARTESIAN_POINT('Ctrl Pts',(-0.075900909784012,2.4132234436762,13.0975523366848));
#37209=CARTESIAN_POINT('Ctrl Pts',(-0.0668910435168518,2.41531963065269,
13.096995011878));
#37210=CARTESIAN_POINT('Ctrl Pts',(-0.0607127345015744,2.41656730078298,
13.0966241992132));
#37211=CARTESIAN_POINT('Ctrl Pts',(-0.0392078355984223,2.42025724177956,
13.0953603168399));
#37212=CARTESIAN_POINT('Ctrl Pts',(-0.0237436830089551,2.42177361073879,
13.0944974048763));
#37213=CARTESIAN_POINT('Ctrl Pts',(0.00791816849111961,2.42258239136098,
13.0927267098881));
#37214=CARTESIAN_POINT('Ctrl Pts',(0.0240732424119309,2.42178023592525,
13.0918206258763));
#37215=CARTESIAN_POINT('Ctrl Pts',(0.0498711807509808,2.41854518807796,
13.0903080928411));
#37216=CARTESIAN_POINT('Ctrl Pts',(0.0595811165778582,2.41687258058835,
13.0897238604599));
#37217=CARTESIAN_POINT('Ctrl Pts',(0.0702162387756829,2.41453448319897,
13.089061727398));
#37218=CARTESIAN_POINT('Ctrl Pts',(0.0712327970479158,2.41430582223988,
13.0889982127875));
#37219=CARTESIAN_POINT('Ctrl Pts',(0.0727513047835294,2.41395650935331,
13.0889029939564));
#37220=CARTESIAN_POINT('Ctrl Pts',(0.0732541091407909,2.41383957303393,
13.0888714090847));
#37221=CARTESIAN_POINT('Ctrl Pts',(0.0741194658921079,2.4136361256758,13.088816951874));
#37222=CARTESIAN_POINT('Ctrl Pts',(0.0744821542365156,2.41355019255528,
13.0887940981617));
#37223=CARTESIAN_POINT('Ctrl Pts',(0.0752302827170993,2.41337156435153,
13.0887468956383));
#37224=CARTESIAN_POINT('Ctrl Pts',(0.0756157023975147,2.4132787869144,13.0887225442077));
#37225=CARTESIAN_POINT('Ctrl Pts',(0.07651225269705,2.4130612202743,13.088665819798));
#37226=CARTESIAN_POINT('Ctrl Pts',(0.0770232497612231,2.41293589030885,
13.0886334294292));
#37227=CARTESIAN_POINT('Ctrl Pts',(0.0786501089781209,2.41253265168059,
13.0885301164451));
#37228=CARTESIAN_POINT('Ctrl Pts',(0.0797647821857898,2.41225002398189,
13.0884590416309));
#37229=CARTESIAN_POINT('Ctrl Pts',(0.103335565093096,2.40613915463422,13.0869499064733));
#37230=CARTESIAN_POINT('Ctrl Pts',(0.125093999268113,2.39791021857387,13.0854299383529));
#37231=CARTESIAN_POINT('Ctrl Pts',(0.167131032246705,2.37658938942965,13.0822569474135));
#37232=CARTESIAN_POINT('Ctrl Pts',(0.18721232471678,2.36341247202198,13.0806119040556));
#37233=CARTESIAN_POINT('Ctrl Pts',(0.208387877028438,2.34586240063223,13.0788445023761));
#37234=CARTESIAN_POINT('Ctrl Pts',(0.211088871349678,2.34354736361537,13.0786185171938));
#37235=CARTESIAN_POINT('Ctrl Pts',(0.214180244910568,2.34080765582103,13.0783597825881));
#37236=CARTESIAN_POINT('Ctrl Pts',(0.21460836056838,2.34042619657217,13.0783239492136));
#37237=CARTESIAN_POINT('Ctrl Pts',(0.215243955217368,2.33985681921156,13.0782707499646));
#37238=CARTESIAN_POINT('Ctrl Pts',(0.215452208195212,2.33966977273978,13.0782533192241));
#37239=CARTESIAN_POINT('Ctrl Pts',(0.215819219694456,2.33933926927883,13.0782226008915));
#37240=CARTESIAN_POINT('Ctrl Pts',(0.21597807896954,2.33919592558004,13.0782093047717));
#37241=CARTESIAN_POINT('Ctrl Pts',(0.216314533114263,2.33889172401483,13.0781811448852));
#37242=CARTESIAN_POINT('Ctrl Pts',(0.216492090888996,2.33873082671207,13.0781662842343));
#37243=CARTESIAN_POINT('Ctrl Pts',(0.216855957544523,2.33840036234422,13.0781358305881));
#37244=CARTESIAN_POINT('Ctrl Pts',(0.217042247442515,2.33823077449094,13.0781202391854));
#37245=CARTESIAN_POINT('Ctrl Pts',(0.217504479164869,2.33780899249834,13.0780815525566));
#37246=CARTESIAN_POINT('Ctrl Pts',(0.217780182271521,2.33755653555087,13.078058477083));
#37247=CARTESIAN_POINT('Ctrl Pts',(0.218548874194158,2.33685019370729,13.0779941367495));
#37248=CARTESIAN_POINT('Ctrl Pts',(0.219040891016237,2.33639524688971,13.077952950656));
#37249=CARTESIAN_POINT('Ctrl Pts',(0.223433722231753,2.33230789487173,13.0775851598428));
#37250=CARTESIAN_POINT('Ctrl Pts',(0.227245548325914,2.32858052159811,13.077265497385));
#37251=CARTESIAN_POINT('Ctrl Pts',(0.23555682967224,2.32003984970661,13.0765624730784));
#37252=CARTESIAN_POINT('Ctrl Pts',(0.240004739919378,2.31517966925828,13.076182002696));
#37253=CARTESIAN_POINT('Ctrl Pts',(0.262616274645169,2.28889814962329,13.0742039340899));
#37254=CARTESIAN_POINT('Ctrl Pts',(0.278070515415464,2.26530790843284,13.0726836389549));
#37255=CARTESIAN_POINT('Ctrl Pts',(0.29137208088291,2.23773125916035,13.0709041826914));
#37256=CARTESIAN_POINT('Ctrl Pts',(0.292445386241801,2.23543738359043,13.0707562524421));
#37257=CARTESIAN_POINT('Ctrl Pts',(0.296656654435833,2.22615351838009,13.070157470565));
#37258=CARTESIAN_POINT('Ctrl Pts',(0.299571723524877,2.21906573273273,13.0697000858954));
#37259=CARTESIAN_POINT('Ctrl Pts',(0.302569700958455,2.21096712023805,13.069174691213));
#37260=CARTESIAN_POINT('Ctrl Pts',(0.302903935112911,2.21005149600274,13.0691152524391));
#37261=CARTESIAN_POINT('Ctrl Pts',(0.303403045243259,2.20866469957226,13.0690251646235));
#37262=CARTESIAN_POINT('Ctrl Pts',(0.303570990791344,2.20819463175939,13.0689946177078));
#37263=CARTESIAN_POINT('Ctrl Pts',(0.303860955567561,2.2073770504376,13.0689414684775));
#37264=CARTESIAN_POINT('Ctrl Pts',(0.303983472752198,2.20702971349488,13.0689188827426));
#37265=CARTESIAN_POINT('Ctrl Pts',(0.304237567888071,2.20630539655903,13.0688717706871));
#37266=CARTESIAN_POINT('Ctrl Pts',(0.304369041149942,2.20592838070719,13.0688472409385));
#37267=CARTESIAN_POINT('Ctrl Pts',(0.304677723340702,2.20503787696982,13.0687892843774));
#37268=CARTESIAN_POINT('Ctrl Pts',(0.304854334911626,2.20452418465708,13.0687558378483));
#37269=CARTESIAN_POINT('Ctrl Pts',(0.305430864233008,2.20283340060768,13.068645703436));
#37270=CARTESIAN_POINT('Ctrl Pts',(0.305825266099085,2.2016544522028,13.0685688335494));
#37271=CARTESIAN_POINT('Ctrl Pts',(0.306733067795013,2.19888774077777,13.0683882497277));
#37272=CARTESIAN_POINT('Ctrl Pts',(0.307240972822584,2.19729822508886,13.0682843569049));
#37273=CARTESIAN_POINT('Ctrl Pts',(0.310271565259121,2.187553433495,13.0676464781159));
#37274=CARTESIAN_POINT('Ctrl Pts',(0.31248154029603,2.17930518827934,13.0671023839154));
#37275=CARTESIAN_POINT('Ctrl Pts',(0.317526473993992,2.15696167328448,13.0656164428712));
#37276=CARTESIAN_POINT('Ctrl Pts',(0.319750092552013,2.14274921581793,13.0646579277367));
#37277=CARTESIAN_POINT('Ctrl Pts',(0.322992987195578,2.10614126152995,13.0621784741338));
#37278=CARTESIAN_POINT('Ctrl Pts',(0.322640031807941,2.08369904038748,13.0606459833613));
#37279=CARTESIAN_POINT('Ctrl Pts',(0.319536149627843,2.05792118456938,13.0589772314738));
#37280=CARTESIAN_POINT('Ctrl Pts',(0.319049266320506,2.05437603780318,13.0587498865492));
#37281=CARTESIAN_POINT('Ctrl Pts',(0.318415788733078,2.0502718278368,13.0584897628732));
#37282=CARTESIAN_POINT('Ctrl Pts',(0.31832664197396,2.04970432779171,13.0584538633312));
#37283=CARTESIAN_POINT('Ctrl Pts',(0.318191765364524,2.04886044041541,13.058400584733));
#37284=CARTESIAN_POINT('Ctrl Pts',(0.31814719238745,2.04858387336923,13.0583831405327));
#37285=CARTESIAN_POINT('Ctrl Pts',(0.318067965212445,2.04809633113808,13.0583524193016));
#37286=CARTESIAN_POINT('Ctrl Pts',(0.318033461695653,2.04788533240428,13.0583391336911));
#37287=CARTESIAN_POINT('Ctrl Pts',(0.317959877205087,2.04743813713453,13.0583109970614));
#37288=CARTESIAN_POINT('Ctrl Pts',(0.317920743111636,2.047201950411,13.0582961491507));
#37289=CARTESIAN_POINT('Ctrl Pts',(0.317839933054891,2.04671758347836,13.0582657245643));
#37290=CARTESIAN_POINT('Ctrl Pts',(0.317798229495703,2.0464694079506,13.0582501494724));
#37291=CARTESIAN_POINT('Ctrl Pts',(0.317693960495412,2.04585332550601,13.0582115183003));
#37292=CARTESIAN_POINT('Ctrl Pts',(0.317631046428263,2.04548547677745,13.0581884818852));
#37293=CARTESIAN_POINT('Ctrl Pts',(0.317453649135773,2.04445899555445,13.0581242787384));
#37294=CARTESIAN_POINT('Ctrl Pts',(0.317337754528671,2.04380060415333,13.0580831903538));
#37295=CARTESIAN_POINT('Ctrl Pts',(0.316283443627598,2.03791837710243,13.0577168804707));
#37296=CARTESIAN_POINT('Ctrl Pts',(0.315218100570476,2.03271774801417,13.0573985426621));
#37297=CARTESIAN_POINT('Ctrl Pts',(0.312556923473534,2.0211839590057,13.0567001487743));
#37298=CARTESIAN_POINT('Ctrl Pts',(0.310896088541645,2.01486815856367,13.0563228910691));
#37299=CARTESIAN_POINT('Ctrl Pts',(0.300901074344268,1.98107018423994,13.0543113624356));
#37300=CARTESIAN_POINT('Ctrl Pts',(0.289114371763786,1.95474593840934,13.0527584892853));
#37301=CARTESIAN_POINT('Ctrl Pts',(0.268968128504277,1.92221219030782,13.0505295305729));
#37302=CARTESIAN_POINT('Ctrl Pts',(0.263582917995622,1.91432184430516,13.0499625820578));
#37303=CARTESIAN_POINT('Ctrl Pts',(0.25717567109151,1.90577555432751,13.0493130376319));
#37304=CARTESIAN_POINT('Ctrl Pts',(0.256490791181818,1.90487200332691,13.0492439062031));
#37305=CARTESIAN_POINT('Ctrl Pts',(0.255510205231541,1.90359241496058,13.0491453414699));
#37306=CARTESIAN_POINT('Ctrl Pts',(0.255218402321414,1.90321338574209,13.0491160621781));
#37307=CARTESIAN_POINT('Ctrl Pts',(0.254681324888904,1.90251896798081,13.049062265996));
#37308=CARTESIAN_POINT('Ctrl Pts',(0.254436305283572,1.90220338272382,13.0490377592348));
#37309=CARTESIAN_POINT('Ctrl Pts',(0.253938331920387,1.90156444938872,13.0489880236215));
#37310=CARTESIAN_POINT('Ctrl Pts',(0.253685345948721,1.90124112746016,13.0489627935157));
#37311=CARTESIAN_POINT('Ctrl Pts',(0.253060502880787,1.900445699949,13.0489005691146));
#37312=CARTESIAN_POINT('Ctrl Pts',(0.252687942804198,1.89997415081872,13.0488635468015));
#37313=CARTESIAN_POINT('Ctrl Pts',(0.251320872298043,1.8982537647919,13.0487279817749));
#37314=CARTESIAN_POINT('Ctrl Pts',(0.250318417745873,1.89701129621758,13.0486291207624));
#37315=CARTESIAN_POINT('Ctrl Pts',(0.236771416629674,1.88047374417353,13.0473002457689));
#37316=CARTESIAN_POINT('Ctrl Pts',(0.222856206323393,1.86636067777752,13.0460120568462));
#37317=CARTESIAN_POINT('Ctrl Pts',(0.185539591629949,1.83489757100428,13.0427438513796));
#37318=CARTESIAN_POINT('Ctrl Pts',(0.160913873015246,1.81926690872778,13.0407305193064));
#37319=CARTESIAN_POINT('Ctrl Pts',(0.13315434731878,1.80651511377369,13.03879822242));
#37320=CARTESIAN_POINT('Ctrl Pts',(0.131776865250896,1.80589403839773,13.0387031840369));
#37321=CARTESIAN_POINT('Ctrl Pts',(0.130008523928478,1.80511165169672,13.0385823057028));
#37322=CARTESIAN_POINT('Ctrl Pts',(0.129621674802877,1.80494140296332,13.0385559305887));
#37323=CARTESIAN_POINT('Ctrl Pts',(0.129005175166487,1.80467153359935,13.0385140086579));
#37324=CARTESIAN_POINT('Ctrl Pts',(0.128775743263671,1.8045714194019,13.038498431649));
#37325=CARTESIAN_POINT('Ctrl Pts',(0.128350200187613,1.80438632065108,13.0384695853292));
#37326=CARTESIAN_POINT('Ctrl Pts',(0.12815412259156,1.80430126451135,13.0384563116932));
#37327=CARTESIAN_POINT('Ctrl Pts',(0.127714004802703,1.80411086661788,13.0384265575442));
#37328=CARTESIAN_POINT('Ctrl Pts',(0.127469919388127,1.80400563193066,13.0384100836778));
#37329=CARTESIAN_POINT('Ctrl Pts',(0.126960483511842,1.80378674138531,13.0383757575334));
#37330=CARTESIAN_POINT('Ctrl Pts',(0.126695109803024,1.80367313974897,13.0383579085725));
#37331=CARTESIAN_POINT('Ctrl Pts',(0.12600503124198,1.8033788261836,13.0383115765733));
#37332=CARTESIAN_POINT('Ctrl Pts',(0.125580088328562,1.8031986690123,13.0382831269264));
#37333=CARTESIAN_POINT('Ctrl Pts',(0.124327276875871,1.8026707041373,13.0381994865187));
#37334=CARTESIAN_POINT('Ctrl Pts',(0.12349833189717,1.80232543942091,13.0381444453988));
#37335=CARTESIAN_POINT('Ctrl Pts',(0.114453106214344,1.79860229069937,13.0375470115137));
#37336=CARTESIAN_POINT('Ctrl Pts',(0.106101123925351,1.7955617044105,13.037023679848));
#37337=CARTESIAN_POINT('Ctrl Pts',(0.0819762463610353,1.78789266429104,
13.0355630691195));
#37338=CARTESIAN_POINT('Ctrl Pts',(0.0659605269880235,1.78411969386218,
13.0346528875474));
#37339=CARTESIAN_POINT('Ctrl Pts',(0.0385740729033675,1.77984282292276,
13.0331015182396));
#37340=CARTESIAN_POINT('Ctrl Pts',(0.0273386758454484,1.77868838453489,
13.0324666541269));
#37341=CARTESIAN_POINT('Ctrl Pts',(0.0154194326313917,1.77809343549193,
13.0317807120393));
#37342=CARTESIAN_POINT('Ctrl Pts',(0.0147724170681609,1.77806309490285,
13.0317434394454));
#37343=CARTESIAN_POINT('Ctrl Pts',(0.00895827483731269,1.7778080158524,
13.0314081496997));
#37344=CARTESIAN_POINT('Ctrl Pts',(0.00378672053054447,1.77770575192817,
13.0311073823492));
#37345=CARTESIAN_POINT('Ctrl Pts',(-0.00221113729222063,1.77773152619727,
13.0307545336235));
#37346=CARTESIAN_POINT('Ctrl Pts',(-0.00303737053497946,1.7777382543671,
13.0307058388947));
#37347=CARTESIAN_POINT('Ctrl Pts',(-0.0104114484344289,1.777826664162,13.0302704251714));
#37348=CARTESIAN_POINT('Ctrl Pts',(-0.0169550291985275,1.77810471530703,
13.029878256878));
#37349=CARTESIAN_POINT('Ctrl Pts',(-0.0245175380833472,1.77865729007696,
13.0294167650025));
#37350=CARTESIAN_POINT('Ctrl Pts',(-0.0255494286636264,1.77873768731747,
13.0293536178997));
#37351=CARTESIAN_POINT('Ctrl Pts',(-0.0270831415515609,1.77886461883149,
13.0292594917865));
#37352=CARTESIAN_POINT('Ctrl Pts',(-0.0275852779382948,1.77890736222851,
13.0292286319535));
#37353=CARTESIAN_POINT('Ctrl Pts',(-0.0284791133003946,1.77898556042512,
13.0291736220837));
#37354=CARTESIAN_POINT('Ctrl Pts',(-0.0288708523799717,1.7790205548783,
13.029149486569));
#37355=CARTESIAN_POINT('Ctrl Pts',(-0.0296950436186146,1.77909570174745,
13.0290986510387));
#37356=CARTESIAN_POINT('Ctrl Pts',(-0.0301274803351692,1.77913601140329,
13.0290719461219));
#37357=CARTESIAN_POINT('Ctrl Pts',(-0.0312660519308131,1.77924446553055,
13.02900154786));
#37358=CARTESIAN_POINT('Ctrl Pts',(-0.0319720426862349,1.77931406739657,
13.0289578087248));
#37359=CARTESIAN_POINT('Ctrl Pts',(-0.0351342189382954,1.77963636443293,
13.0287615017033));
#37360=CARTESIAN_POINT('Ctrl Pts',(-0.0375876290833089,1.77991494579042,
13.0286081207465));
#37361=CARTESIAN_POINT('Ctrl Pts',(-0.055561697716967,1.78216537209679,
13.0274762778186));
#37362=CARTESIAN_POINT('Ctrl Pts',(-0.070921326847603,1.78523661447709,
13.0264628455106));
#37363=CARTESIAN_POINT('Ctrl Pts',(-0.0995741890199547,1.79316995814285,
13.0244873830651));
#37364=CARTESIAN_POINT('Ctrl Pts',(-0.112891171137942,1.79781588693697,
13.0235326116357));
#37365=CARTESIAN_POINT('Ctrl Pts',(-0.139325694513887,1.80903013221806,
13.021590467278));
#37366=CARTESIAN_POINT('Ctrl Pts',(-0.152387464847363,1.81565294516366,
13.0206055100016));
#37367=CARTESIAN_POINT('Ctrl Pts',(-0.168832614573602,1.82545110249935,
13.0193676139911));
#37368=CARTESIAN_POINT('Ctrl Pts',(-0.172661495499823,1.8278427623984,13.0190796351122));
#37369=CARTESIAN_POINT('Ctrl Pts',(-0.176953441869582,1.83065072337242,
13.0187582110946));
#37370=CARTESIAN_POINT('Ctrl Pts',(-0.177466826844408,1.83098870136393,
13.0187197866268));
#37371=CARTESIAN_POINT('Ctrl Pts',(-0.178216765169868,1.83148549125072,
13.0186636946089));
#37372=CARTESIAN_POINT('Ctrl Pts',(-0.178454075929436,1.83164314880713,
13.0186459503258));
#37373=CARTESIAN_POINT('Ctrl Pts',(-0.17887009584438,1.831920327777,13.0186148536351));
#37374=CARTESIAN_POINT('Ctrl Pts',(-0.179048894663105,1.8320397134507,13.0186014920557));
#37375=CARTESIAN_POINT('Ctrl Pts',(-0.179422552713927,1.83228974946524,
13.0185735757498));
#37376=CARTESIAN_POINT('Ctrl Pts',(-0.179617388360722,1.83242043339769,
13.0185590233876));
#37377=CARTESIAN_POINT('Ctrl Pts',(-0.180015156777663,1.8326878625357,13.0185293216267));
#37378=CARTESIAN_POINT('Ctrl Pts',(-0.18021807690784,1.83282462639305,13.0185141735055));
#37379=CARTESIAN_POINT('Ctrl Pts',(-0.180716181781151,1.83316116416408,
13.0184769992732));
#37380=CARTESIAN_POINT('Ctrl Pts',(-0.181011192113998,1.83336119749714,
13.0184549905759));
#37381=CARTESIAN_POINT('Ctrl Pts',(-0.181823879645668,1.83391421496085,
13.0183943827026));
#37382=CARTESIAN_POINT('Ctrl Pts',(-0.182340863583443,1.8342682222764,13.0183558512888));
#37383=CARTESIAN_POINT('Ctrl Pts',(-0.183979226213123,1.83539713174827,
13.0182338065228));
#37384=CARTESIAN_POINT('Ctrl Pts',(-0.185096740101167,1.83617765349205,
13.0181506568005));
#37385=CARTESIAN_POINT('Ctrl Pts',(-0.209487237327741,1.85344433520756,
13.0163371731466));
#37386=CARTESIAN_POINT('Ctrl Pts',(-0.230478768121008,1.87294337030669,
13.0147946684863));
#37387=CARTESIAN_POINT('Ctrl Pts',(-0.261393140611049,1.91042908455911,
13.0120590819876));
#37388=CARTESIAN_POINT('Ctrl Pts',(-0.272680515351522,1.92705879364602,
13.0109057066521));
#37389=CARTESIAN_POINT('Ctrl Pts',(-0.282973628979109,1.94576387642268,
13.0096089577418));
#37390=CARTESIAN_POINT('Ctrl Pts',(-0.28359181294541,1.94690349426797,13.0095299713568));
#37391=CARTESIAN_POINT('Ctrl Pts',(-0.284444155350767,1.94849765844747,
13.0094194955218));
#37392=CARTESIAN_POINT('Ctrl Pts',(-0.284684139749583,1.94894908944532,
13.0093882129521));
#37393=CARTESIAN_POINT('Ctrl Pts',(-0.285096616000628,1.94972946686435,
13.0093341376605));
#37394=CARTESIAN_POINT('Ctrl Pts',(-0.285269615754226,1.95005814490462,
13.0093113629625));
#37395=CARTESIAN_POINT('Ctrl Pts',(-0.285626434377593,1.95073890874086,
13.009264192583));
#37396=CARTESIAN_POINT('Ctrl Pts',(-0.285810171270957,1.95109103661971,
13.0092397940537));
#37397=CARTESIAN_POINT('Ctrl Pts',(-0.286237941058301,1.95191455680242,
13.0091827341107));
#37398=CARTESIAN_POINT('Ctrl Pts',(-0.286481460661861,1.95238621311006,
13.0091500546756));
#37399=CARTESIAN_POINT('Ctrl Pts',(-0.287260284378128,1.95390384922752,
13.0090449034622));
#37400=CARTESIAN_POINT('Ctrl Pts',(-0.287791029086278,1.95495214661916,
13.0089722717302));
#37401=CARTESIAN_POINT('Ctrl Pts',(-0.296028904342663,1.97144635541009,
13.0078294069265));
#37402=CARTESIAN_POINT('Ctrl Pts',(-0.302487259792097,1.98748141111869,
13.006715226017));
#37403=CARTESIAN_POINT('Ctrl Pts',(-0.311719902453299,2.01705310471501,
13.0046572594936));
#37404=CARTESIAN_POINT('Ctrl Pts',(-0.314968563061163,2.03039933803388,
13.0037279718904));
#37405=CARTESIAN_POINT('Ctrl Pts',(-0.32062983445731,2.0624314153751,13.0015273956094));
#37406=CARTESIAN_POINT('Ctrl Pts',(-0.322275899729781,2.08120454186863,
13.0002603718331));
#37407=CARTESIAN_POINT('Ctrl Pts',(-0.322274999631057,2.10001542082731,
12.9990742422863));
#37408=CARTESIAN_POINT('',(-0.322274868779446,2.0997091767017,12.8743773449311));
#37409=CARTESIAN_POINT('Ctrl Pts',(-0.322274868779446,2.0997091767017,12.8743773449311));
#37410=CARTESIAN_POINT('Ctrl Pts',(-0.32225477015569,2.07743695377,12.8757506912526));
#37411=CARTESIAN_POINT('Ctrl Pts',(-0.319921917552464,2.05526885992465,
12.8771240375741));
#37412=CARTESIAN_POINT('Ctrl Pts',(-0.315363309840923,2.03361356741639,
12.8784973838957));
#37413=CARTESIAN_POINT('Ctrl Pts',(-0.313909026430378,2.02670511320448,
12.8789355077481));
#37414=CARTESIAN_POINT('Ctrl Pts',(-0.312228581490867,2.01984867270576,
12.8793736316006));
#37415=CARTESIAN_POINT('Ctrl Pts',(-0.310325794918933,2.01305704955011,
12.879811755453));
#37416=CARTESIAN_POINT('Ctrl Pts',(-0.305560360746364,1.99604776771548,
12.8809090148141));
#37417=CARTESIAN_POINT('Ctrl Pts',(-0.299377391867214,1.97937816504062,
12.8820062741752));
#37418=CARTESIAN_POINT('Ctrl Pts',(-0.291845741122565,1.96329872343822,
12.8831035335364));
#37419=CARTESIAN_POINT('Ctrl Pts',(-0.284328498231357,1.94725004139251,
12.8841986938686));
#37420=CARTESIAN_POINT('Ctrl Pts',(-0.275467960777509,1.93178999933012,
12.8852938542009));
#37421=CARTESIAN_POINT('Ctrl Pts',(-0.265381773584942,1.917151183012,12.8863890145332));
#37422=CARTESIAN_POINT('Ctrl Pts',(-0.255179573497405,1.90234398875011,
12.8874967715701));
#37423=CARTESIAN_POINT('Ctrl Pts',(-0.243723683465363,1.88837777039137,
12.888604528607));
#37424=CARTESIAN_POINT('Ctrl Pts',(-0.231182240909558,1.87546504255899,
12.8897122856439));
#37425=CARTESIAN_POINT('Ctrl Pts',(-0.218789416356174,1.86270533251606,
12.8908069155913));
#37426=CARTESIAN_POINT('Ctrl Pts',(-0.205337238028378,1.85097478606144,
12.8919015455388));
#37427=CARTESIAN_POINT('Ctrl Pts',(-0.191025630177961,1.84044194437446,
12.8929961754862));
#37428=CARTESIAN_POINT('Ctrl Pts',(-0.176456579495077,1.82971963378739,
12.8941104960678));
#37429=CARTESIAN_POINT('Ctrl Pts',(-0.160997509866063,1.82023907717878,
12.8952248166494));
#37430=CARTESIAN_POINT('Ctrl Pts',(-0.144889561086191,1.81213164343184,
12.896339137231));
#37431=CARTESIAN_POINT('Ctrl Pts',(-0.128781612306314,1.80402420968491,
12.8974534578126));
#37432=CARTESIAN_POINT('Ctrl Pts',(-0.112025581744362,1.79729015799452,
12.8985677783942));
#37433=CARTESIAN_POINT('Ctrl Pts',(-0.0948817706989104,1.79200872542548,
12.8996820989758));
#37434=CARTESIAN_POINT('Ctrl Pts',(-0.0780004465863533,1.78680815626729,
12.9007793583222));
#37435=CARTESIAN_POINT('Ctrl Pts',(-0.0606373936470627,1.7829833500994,
12.9018766176687));
#37436=CARTESIAN_POINT('Ctrl Pts',(-0.0430404928385636,1.78061200460691,
12.9029738770151));
#37437=CARTESIAN_POINT('Ctrl Pts',(-0.0254772544471081,1.77824519543715,
12.9040690373328));
#37438=CARTESIAN_POINT('Ctrl Pts',(-0.00768180547187218,1.7773264938092,
12.9051641976504));
#37439=CARTESIAN_POINT('Ctrl Pts',(0.0100866085518973,1.77788288472526,
12.906259357968));
#37440=CARTESIAN_POINT('Ctrl Pts',(0.0280593979987197,1.77844567534749,
12.9073671150122));
#37441=CARTESIAN_POINT('Ctrl Pts',(0.0460037248759171,1.7805178263984,12.9084748720565));
#37442=CARTESIAN_POINT('Ctrl Pts',(0.0636498872489975,1.78407300292917,
12.9095826291007));
#37443=CARTESIAN_POINT('Ctrl Pts',(0.0810869395700782,1.78758605000803,
12.9106772590338));
#37444=CARTESIAN_POINT('Ctrl Pts',(0.0982321000672225,1.79254692552035,
12.911771888967));
#37445=CARTESIAN_POINT('Ctrl Pts',(0.114835433694952,1.79887876396193,12.9128665189002));
#37446=CARTESIAN_POINT('Ctrl Pts',(0.131737435115925,1.80532450219358,12.9139808394999));
#37447=CARTESIAN_POINT('Ctrl Pts',(0.14807713087735,1.81319076820556,12.9150951600996));
#37448=CARTESIAN_POINT('Ctrl Pts',(0.163613530327581,1.82234591967928,12.9162094806994));
#37449=CARTESIAN_POINT('Ctrl Pts',(0.179149929777806,1.83150107115299,12.9173238012991));
#37450=CARTESIAN_POINT('Ctrl Pts',(0.193882383350925,1.84194457795324,12.9184381218989));
#37451=CARTESIAN_POINT('Ctrl Pts',(0.207603361298644,1.8535004665268,12.9195524424986));
#37452=CARTESIAN_POINT('Ctrl Pts',(0.22111425879022,1.86487942410084,12.9206497018524));
#37453=CARTESIAN_POINT('Ctrl Pts',(0.233729158635664,1.87740815327334,12.9217469612061));
#37454=CARTESIAN_POINT('Ctrl Pts',(0.245248548787146,1.89092029045649,12.9228442205599));
#37455=CARTESIAN_POINT('Ctrl Pts',(0.256745902640785,1.90440657926784,12.9239393808846));
#37456=CARTESIAN_POINT('Ctrl Pts',(0.26715136151924,1.91887200168266,12.9250345412094));
#37457=CARTESIAN_POINT('Ctrl Pts',(0.276301901655129,1.93411318688106,12.9261297015342));
#37458=CARTESIAN_POINT('Ctrl Pts',(0.285557692822547,1.94952967872147,12.9272374585748));
#37459=CARTESIAN_POINT('Ctrl Pts',(0.293528979425782,1.96573928278836,12.9283452156154));
#37460=CARTESIAN_POINT('Ctrl Pts',(0.3000919098322,1.98250097328802,12.929452972656));
#37461=CARTESIAN_POINT('Ctrl Pts',(0.306577068447082,1.99906403503214,12.9305476025957));
#37462=CARTESIAN_POINT('Ctrl Pts',(0.311686860661269,2.01616540460373,12.9316422325354));
#37463=CARTESIAN_POINT('Ctrl Pts',(0.31535062200815,2.03355332345352,12.9327368624751));
#37464=CARTESIAN_POINT('Ctrl Pts',(0.319080288593584,2.05125402330382,12.9338511830661));
#37465=CARTESIAN_POINT('Ctrl Pts',(0.321311163799205,2.06925088384046,12.9349655036572));
#37466=CARTESIAN_POINT('Ctrl Pts',(0.322023482246868,2.08727001545166,12.9360798242482));
#37467=CARTESIAN_POINT('Ctrl Pts',(0.322735800694531,2.10528914706285,12.9371941448393));
#37468=CARTESIAN_POINT('Ctrl Pts',(0.321929656509605,2.12332971661026,12.9383084654303));
#37469=CARTESIAN_POINT('Ctrl Pts',(0.319640671798446,2.14112197170903,12.9394227860214));
#37470=CARTESIAN_POINT('Ctrl Pts',(0.317386733394382,2.15864181221583,12.9405200454143));
#37471=CARTESIAN_POINT('Ctrl Pts',(0.313681026625055,2.17603067396092,12.9416173048073));
#37472=CARTESIAN_POINT('Ctrl Pts',(0.308555433511349,2.19303074801174,12.9427145642002));
#37473=CARTESIAN_POINT('Ctrl Pts',(0.303439645524016,2.20999830136286,12.9438097245645));
#37474=CARTESIAN_POINT('Ctrl Pts',(0.296909521902379,2.22657779252613,12.9449048849287));
#37475=CARTESIAN_POINT('Ctrl Pts',(0.28904781277566,2.24252205988761,12.946000045293));
#37476=CARTESIAN_POINT('Ctrl Pts',(0.281095677393468,2.25864971999111,12.9471078023139));
#37477=CARTESIAN_POINT('Ctrl Pts',(0.271781353589384,2.27412667164002,12.9482155593348));
#37478=CARTESIAN_POINT('Ctrl Pts',(0.261240457029716,2.28871830657333,12.9493233163558));
#37479=CARTESIAN_POINT('Ctrl Pts',(0.250824471247107,2.30313702903684,12.9504179463349));
#37480=CARTESIAN_POINT('Ctrl Pts',(0.23921135584914,2.31669071449423,12.9515125763139));
#37481=CARTESIAN_POINT('Ctrl Pts',(0.226574541989169,2.32918366553356,12.952607206293));
#37482=CARTESIAN_POINT('Ctrl Pts',(0.213710412980391,2.34190134387014,12.9537215268349));
#37483=CARTESIAN_POINT('Ctrl Pts',(0.199785944014845,2.35351912880811,12.9548358473767));
#37484=CARTESIAN_POINT('Ctrl Pts',(0.185020726982867,2.36387213989304,12.9559501679186));
#37485=CARTESIAN_POINT('Ctrl Pts',(0.170255509950889,2.37422515097797,12.9570644884605));
#37486=CARTESIAN_POINT('Ctrl Pts',(0.154650296321501,2.38331301635944,12.9581788090023));
#37487=CARTESIAN_POINT('Ctrl Pts',(0.138451181570716,2.39101966591052,12.9592931295442));
#37488=CARTESIAN_POINT('Ctrl Pts',(0.122500089953329,2.39860831966992,12.9603903888283));
#37489=CARTESIAN_POINT('Ctrl Pts',(0.105873259244491,2.40490539970148,12.9614876481124));
#37490=CARTESIAN_POINT('Ctrl Pts',(0.0888047180756005,2.40979815634137,
12.9625849073965));
#37491=CARTESIAN_POINT('Ctrl Pts',(0.0717688285844593,2.41468155326437,
12.9636800676519));
#37492=CARTESIAN_POINT('Ctrl Pts',(0.054293623314285,2.41816568666105,12.9647752279074));
#37493=CARTESIAN_POINT('Ctrl Pts',(0.0366317142711716,2.42018634126795,
12.9658703881629));
#37494=CARTESIAN_POINT('Ctrl Pts',(0.0187666533278381,2.42223023797298,
12.9669781452382));
#37495=CARTESIAN_POINT('Ctrl Pts',(0.000711342416110285,2.42277654184563,
12.9680859023136));
#37496=CARTESIAN_POINT('Ctrl Pts',(-0.0172635443498445,2.42181228326694,
12.9691936593889));
#37497=CARTESIAN_POINT('Ctrl Pts',(-0.0350254241429703,2.42085945139728,
12.9702882892616));
#37498=CARTESIAN_POINT('Ctrl Pts',(-0.0527079932519415,2.41843179160619,
12.9713829191343));
#37499=CARTESIAN_POINT('Ctrl Pts',(-0.0700528244136611,2.41456919336875,
12.972477549007));
#37500=CARTESIAN_POINT('Ctrl Pts',(-0.0877096639345393,2.41063711259056,
12.9735918696836));
#37501=CARTESIAN_POINT('Ctrl Pts',(-0.105015674487834,2.4052180864362,12.9747061903603));
#37502=CARTESIAN_POINT('Ctrl Pts',(-0.121713352459767,2.3984074989976,12.975820511037));
#37503=CARTESIAN_POINT('Ctrl Pts',(-0.138411030431706,2.391596911559,12.9769348317137));
#37504=CARTESIAN_POINT('Ctrl Pts',(-0.154499656379204,2.38339519339613,
12.9780491523903));
#37505=CARTESIAN_POINT('Ctrl Pts',(-0.169748420447812,2.37394643523958,
12.979163473067));
#37506=CARTESIAN_POINT('Ctrl Pts',(-0.184763711413957,2.36464234657043,
12.9802607324327));
#37507=CARTESIAN_POINT('Ctrl Pts',(-0.19905881373056,2.35407093203492,12.9813579917984));
#37508=CARTESIAN_POINT('Ctrl Pts',(-0.2124122415145,2.34236793368716,12.9824552511641));
#37509=CARTESIAN_POINT('Ctrl Pts',(-0.225740124523122,2.33068732288426,
12.9835504115));
#37510=CARTESIAN_POINT('Ctrl Pts',(-0.238129291142844,2.31787988075899,
12.9846455718358));
#37511=CARTESIAN_POINT('Ctrl Pts',(-0.249389004567557,2.30412324714692,
12.9857407321716));
#37512=CARTESIAN_POINT('Ctrl Pts',(-0.260778228910836,2.29020838266447,
12.9868484892065));
#37513=CARTESIAN_POINT('Ctrl Pts',(-0.271011236232546,2.2753228786545,12.9879562462413));
#37514=CARTESIAN_POINT('Ctrl Pts',(-0.279930600684152,2.25968730201744,
12.9890640032762));
#37515=CARTESIAN_POINT('Ctrl Pts',(-0.288744269334159,2.2442370093,12.9901586332246));
#37516=CARTESIAN_POINT('Ctrl Pts',(-0.296274943808381,2.22805505132666,
12.9912532631731));
#37517=CARTESIAN_POINT('Ctrl Pts',(-0.302416272518608,2.21138031128054,
12.9923478931215));
#37518=CARTESIAN_POINT('Ctrl Pts',(-0.308668073840186,2.19440561951984,
12.9934622136996));
#37519=CARTESIAN_POINT('Ctrl Pts',(-0.313479715083512,2.17692100071793,
12.9945765342776));
#37520=CARTESIAN_POINT('Ctrl Pts',(-0.31679200553615,2.15919460155609,12.9956908548557));
#37521=CARTESIAN_POINT('Ctrl Pts',(-0.320104295988786,2.14146820239425,
12.9968051754337));
#37522=CARTESIAN_POINT('Ctrl Pts',(-0.321917208225557,2.12350086086223,
12.9979194960118));
#37523=CARTESIAN_POINT('Ctrl Pts',(-0.322226954727219,2.10556464484248,
12.9990338165898));
#37524=CARTESIAN_POINT('Ctrl Pts',(-0.32225878479565,2.10372148929352,12.9991483260357));
#37525=CARTESIAN_POINT('Ctrl Pts',(-0.322274800607892,2.10187805985517,
12.9992628354815));
#37526=CARTESIAN_POINT('Ctrl Pts',(-0.32227499814981,2.10003453317044,12.9993773449273));
#37527=CARTESIAN_POINT('',(-0.322555864543089,2.10024316196973,12.6243773449273));
#37528=CARTESIAN_POINT('Ctrl Pts',(-0.322274872504986,2.09971333487317,
12.8744514725916));
#37529=CARTESIAN_POINT('Ctrl Pts',(-0.322294798337445,2.12211436839394,
12.8731948915496));
#37530=CARTESIAN_POINT('Ctrl Pts',(-0.319979252500182,2.14445352842172,
12.8719154443998));
#37531=CARTESIAN_POINT('Ctrl Pts',(-0.315200854949327,2.16715834777632,
12.8705046719139));
#37532=CARTESIAN_POINT('Ctrl Pts',(-0.315032253003373,2.16794484664868,
12.870455670392));
#37533=CARTESIAN_POINT('Ctrl Pts',(-0.314752217117301,2.16922771292375,
12.8703755245491));
#37534=CARTESIAN_POINT('Ctrl Pts',(-0.314642548503174,2.16972446545997,
12.8703444367166));
#37535=CARTESIAN_POINT('Ctrl Pts',(-0.314447146601967,2.17059970411111,
12.8702895669105));
#37536=CARTESIAN_POINT('Ctrl Pts',(-0.314361904779475,2.17097829983898,
12.870265800726));
#37537=CARTESIAN_POINT('Ctrl Pts',(-0.314188225474058,2.17174323436838,
12.8702177181107));
#37538=CARTESIAN_POINT('Ctrl Pts',(-0.314099758743251,2.17212956577808,
12.8701934007776));
#37539=CARTESIAN_POINT('Ctrl Pts',(-0.313926666095136,2.17287909862558,
12.8701461572907));
#37540=CARTESIAN_POINT('Ctrl Pts',(-0.313842121908859,2.17324231847787,
12.8701232337988));
#37541=CARTESIAN_POINT('Ctrl Pts',(-0.313638876291029,2.17410869151184,
12.8700684844704));
#37542=CARTESIAN_POINT('Ctrl Pts',(-0.313519594545015,2.17461170625347,
12.8700366399912));
#37543=CARTESIAN_POINT('Ctrl Pts',(-0.313088972824143,2.17640838449785,
12.8699226915661));
#37544=CARTESIAN_POINT('Ctrl Pts',(-0.312770835197441,2.17770039054188,
12.8698403687799));
#37545=CARTESIAN_POINT('Ctrl Pts',(-0.307111492576687,2.2000857973967,12.8684072984508));
#37546=CARTESIAN_POINT('Ctrl Pts',(-0.299656721557315,2.2205825125988,12.8669852048862));
#37547=CARTESIAN_POINT('Ctrl Pts',(-0.287724429957582,2.24528636866053,
12.8651420378203));
#37548=CARTESIAN_POINT('Ctrl Pts',(-0.285117622275454,2.25033767293752,
12.8647582171332));
#37549=CARTESIAN_POINT('Ctrl Pts',(-0.279787039351144,2.26002907664861,
12.8640100273077));
#37550=CARTESIAN_POINT('Ctrl Pts',(-0.277077891269175,2.26467524177196,
12.8636458371482));
#37551=CARTESIAN_POINT('Ctrl Pts',(-0.266632672176858,2.28160059456275,
12.862302458274));
#37552=CARTESIAN_POINT('Ctrl Pts',(-0.258185362980705,2.29342224180021,
12.8613301513551));
#37553=CARTESIAN_POINT('Ctrl Pts',(-0.24697580343239,2.30706033594075,12.8601994571681));
#37554=CARTESIAN_POINT('Ctrl Pts',(-0.24494708254618,2.30945634095366,12.8600004798228));
#37555=CARTESIAN_POINT('Ctrl Pts',(-0.24254565442415,2.31220990901419,12.8597718040688));
#37556=CARTESIAN_POINT('Ctrl Pts',(-0.242206795593599,2.31259658544019,
12.8597396916465));
#37557=CARTESIAN_POINT('Ctrl Pts',(-0.24169004535362,2.31318341705031,12.8596909590196));
#37558=CARTESIAN_POINT('Ctrl Pts',(-0.24151282944834,2.31338416188037,12.8596742888225));
#37559=CARTESIAN_POINT('Ctrl Pts',(-0.24119091964426,2.31374789684954,12.8596440847185));
#37560=CARTESIAN_POINT('Ctrl Pts',(-0.24104631111361,2.31391096050881,12.859630544534));
#37561=CARTESIAN_POINT('Ctrl Pts',(-0.240754565061393,2.31423926806511,
12.859603283995));
#37562=CARTESIAN_POINT('Ctrl Pts',(-0.240607423445389,2.31440450639542,
12.8595895640782));
#37563=CARTESIAN_POINT('Ctrl Pts',(-0.240184933232937,2.31487797536065,
12.85955025216));
#37564=CARTESIAN_POINT('Ctrl Pts',(-0.239909160424916,2.31518582944966,
12.8595246920494));
#37565=CARTESIAN_POINT('Ctrl Pts',(-0.238708080539584,2.3165214548443,12.8594137988775));
#37566=CARTESIAN_POINT('Ctrl Pts',(-0.237776737929243,2.3175438144005,12.8593289137375));
#37567=CARTESIAN_POINT('Ctrl Pts',(-0.220167182346014,2.33662609483042,
12.8577437933958));
#37568=CARTESIAN_POINT('Ctrl Pts',(-0.201480136395958,2.3527284638963,12.8563897808667));
#37569=CARTESIAN_POINT('Ctrl Pts',(-0.17388286426215,2.37148283091152,12.8545233038542));
#37570=CARTESIAN_POINT('Ctrl Pts',(-0.166426831463961,2.37611642503389,
12.8540310146772));
#37571=CARTESIAN_POINT('Ctrl Pts',(-0.149192108432061,2.38587510396397,
12.8529044601625));
#37572=CARTESIAN_POINT('Ctrl Pts',(-0.139321065774814,2.39081345803224,
12.8522668597802));
#37573=CARTESIAN_POINT('Ctrl Pts',(-0.125872574071606,2.39669950746404,
12.8513954682407));
#37574=CARTESIAN_POINT('Ctrl Pts',(-0.122503724504924,2.39810625372167,
12.8511770017648));
#37575=CARTESIAN_POINT('Ctrl Pts',(-0.116980424016449,2.40030320932826,
12.8508181425325));
#37576=CARTESIAN_POINT('Ctrl Pts',(-0.114840098055629,2.4011281929577,12.8506789191371));
#37577=CARTESIAN_POINT('Ctrl Pts',(-0.112210384543954,2.40210969630715,
12.8505076064953));
#37578=CARTESIAN_POINT('Ctrl Pts',(-0.111729153557894,2.40228800049416,
12.8504762463275));
#37579=CARTESIAN_POINT('Ctrl Pts',(-0.110881791546671,2.40259966253182,
12.8504210075836));
#37580=CARTESIAN_POINT('Ctrl Pts',(-0.110515839819288,2.40273350757374,
12.8503971452843));
#37581=CARTESIAN_POINT('Ctrl Pts',(-0.109776402774381,2.40300243358327,
12.8503489164489));
#37582=CARTESIAN_POINT('Ctrl Pts',(-0.109402908753309,2.40313748847263,
12.8503245490949));
#37583=CARTESIAN_POINT('Ctrl Pts',(-0.108679610914486,2.4033975210493,12.850277346658));
#37584=CARTESIAN_POINT('Ctrl Pts',(-0.10832983860777,2.40352258511156,12.8502545144928));
#37585=CARTESIAN_POINT('Ctrl Pts',(-0.10749803075371,2.4038183841019,12.8502002017231));
#37586=CARTESIAN_POINT('Ctrl Pts',(-0.107015804611268,2.40398857658275,
12.8501687031532));
#37587=CARTESIAN_POINT('Ctrl Pts',(-0.105308886907108,2.40458643557149,
12.8500571661655));
#37588=CARTESIAN_POINT('Ctrl Pts',(-0.104082032870247,2.40500785030952,
12.8499769208359));
#37589=CARTESIAN_POINT('Ctrl Pts',(-0.0836837798919911,2.41187708736274,
12.8486413420139));
#37590=CARTESIAN_POINT('Ctrl Pts',(-0.063953534988268,2.41651217980907,
12.8473248596033));
#37591=CARTESIAN_POINT('Ctrl Pts',(-0.0259853823046345,2.4217355477075,
12.8447582876782));
#37592=CARTESIAN_POINT('Ctrl Pts',(-0.00787289940778402,2.42268715141514,
12.8435211252291));
#37593=CARTESIAN_POINT('Ctrl Pts',(0.0193635842491699,2.4218227074341,12.841700225228));
#37594=CARTESIAN_POINT('Ctrl Pts',(0.0284881730753215,2.42114367072974,
12.841097395038));
#37595=CARTESIAN_POINT('Ctrl Pts',(0.0406020883521112,2.41972167962587,
12.8403166783615));
#37596=CARTESIAN_POINT('Ctrl Pts',(0.0436268559760407,2.41932300434967,
12.8401233918411));
#37597=CARTESIAN_POINT('Ctrl Pts',(0.0471505928940003,2.41880755582274,
12.8399005101506));
#37598=CARTESIAN_POINT('Ctrl Pts',(0.0476553753261181,2.4187324917089,12.8398686369114));
#37599=CARTESIAN_POINT('Ctrl Pts',(0.0484239556834199,2.41861633262442,
12.8398201928404));
#37600=CARTESIAN_POINT('Ctrl Pts',(0.0486878814064416,2.4185761088099,12.8398035729111));
#37601=CARTESIAN_POINT('Ctrl Pts',(0.0491463023560506,2.41850565981011,
12.8397747324617));
#37602=CARTESIAN_POINT('Ctrl Pts',(0.0493408194042368,2.41847558447639,
12.8397625034295));
#37603=CARTESIAN_POINT('Ctrl Pts',(0.0497486927689843,2.41841213831531,
12.8397368789214));
#37604=CARTESIAN_POINT('Ctrl Pts',(0.0499620424284265,2.41837873134961,
12.8397234855741));
#37605=CARTESIAN_POINT('Ctrl Pts',(0.0505576321794122,2.41828485860364,
12.8396861248128));
#37606=CARTESIAN_POINT('Ctrl Pts',(0.0509397988042087,2.41822391847477,
12.8396621844141));
#37607=CARTESIAN_POINT('Ctrl Pts',(0.0524778680162669,2.41797581688993,
12.8395659614733));
#37608=CARTESIAN_POINT('Ctrl Pts',(0.0536328748788254,2.41778304169577,
12.8394939936818));
#37609=CARTESIAN_POINT('Ctrl Pts',(0.07415216161304,2.41424323272159,12.8382202074648));
#37610=CARTESIAN_POINT('Ctrl Pts',(0.0931746927149973,2.40913763883687,
12.8371134851007));
#37611=CARTESIAN_POINT('Ctrl Pts',(0.122599371135456,2.3982744552928,12.8353578368062));
#37612=CARTESIAN_POINT('Ctrl Pts',(0.133353684710301,2.39362398612088,12.8347063708794));
#37613=CARTESIAN_POINT('Ctrl Pts',(0.155540500420522,2.38255892655562,12.8333047490035));
#37614=CARTESIAN_POINT('Ctrl Pts',(0.166882479261162,2.37601192186967,12.8325531344663));
#37615=CARTESIAN_POINT('Ctrl Pts',(0.182574784628207,2.36563221398936,12.8314373372663));
#37616=CARTESIAN_POINT('Ctrl Pts',(0.18726965939977,2.36234346468265,12.8310930913317));
#37617=CARTESIAN_POINT('Ctrl Pts',(0.192611641789871,2.35838493309092,12.8306880940477));
#37618=CARTESIAN_POINT('Ctrl Pts',(0.193346798810902,2.35783528378327,12.8306320595801));
#37619=CARTESIAN_POINT('Ctrl Pts',(0.194391635989917,2.35704711681272,12.8305519890433));
#37620=CARTESIAN_POINT('Ctrl Pts',(0.194703250722833,2.35681116128472,12.8305280535126));
#37621=CARTESIAN_POINT('Ctrl Pts',(0.195331146289716,2.35633391731906,12.8304797123047));
#37622=CARTESIAN_POINT('Ctrl Pts',(0.195647411114207,2.35609260903237,12.8304553058722));
#37623=CARTESIAN_POINT('Ctrl Pts',(0.196257294313261,2.35562548241471,12.8304081291823));
#37624=CARTESIAN_POINT('Ctrl Pts',(0.196550971917827,2.35539974210498,12.8303853620308));
#37625=CARTESIAN_POINT('Ctrl Pts',(0.197245982518356,2.35486360160357,12.830331362526));
#37626=CARTESIAN_POINT('Ctrl Pts',(0.197646972082191,2.35455275968651,12.8303001126906));
#37627=CARTESIAN_POINT('Ctrl Pts',(0.199051955638438,2.35345831338486,12.8301902858797));
#37628=CARTESIAN_POINT('Ctrl Pts',(0.200052027068166,2.3526697133782,12.8301115102332));
#37629=CARTESIAN_POINT('Ctrl Pts',(0.214377880965699,2.3412347832568,12.8289742993041));
#37630=CARTESIAN_POINT('Ctrl Pts',(0.226840364854264,2.32955473259397,12.8278730427438));
#37631=CARTESIAN_POINT('Ctrl Pts',(0.253516605080675,2.30025035121218,12.825240734852));
#37632=CARTESIAN_POINT('Ctrl Pts',(0.266916867367605,2.28200594613907,12.82369097945));
#37633=CARTESIAN_POINT('Ctrl Pts',(0.282141150478601,2.25593447543346,12.8216815462283));
#37634=CARTESIAN_POINT('Ctrl Pts',(0.285747900495652,2.24922246768539,12.8211811816926));
#37635=CARTESIAN_POINT('Ctrl Pts',(0.290568133186489,2.23943519259995,12.8204816332445));
#37636=CARTESIAN_POINT('Ctrl Pts',(0.291977353175279,2.23645966536536,12.8202728153829));
#37637=CARTESIAN_POINT('Ctrl Pts',(0.293558289813493,2.23298489360371,12.8200338469683));
#37638=CARTESIAN_POINT('Ctrl Pts',(0.293774616617726,2.23250632469958,12.8200010411197));
#37639=CARTESIAN_POINT('Ctrl Pts',(0.294100421651276,2.23178084290423,12.81995147289));
#37640=CARTESIAN_POINT('Ctrl Pts',(0.29421075961816,2.23153432060948,12.8199346578796));
#37641=CARTESIAN_POINT('Ctrl Pts',(0.294401110194699,2.23110759252099,12.8199056009178));
#37642=CARTESIAN_POINT('Ctrl Pts',(0.29448126720316,2.23092745230739,12.8198933500404));
#37643=CARTESIAN_POINT('Ctrl Pts',(0.294648231685222,2.23055129699269,12.8198678006857));
#37644=CARTESIAN_POINT('Ctrl Pts',(0.294735008631728,2.23035526943408,12.8198545041202));
#37645=CARTESIAN_POINT('Ctrl Pts',(0.294947952123556,2.22987293425737,12.8198218314042));
#37646=CARTESIAN_POINT('Ctrl Pts',(0.295073897776521,2.22958652849506,12.819802468867));
#37647=CARTESIAN_POINT('Ctrl Pts',(0.295561422485904,2.22847348067334,12.8197273675001));
#37648=CARTESIAN_POINT('Ctrl Pts',(0.295919950993991,2.22764549481936,12.81967181384));
#37649=CARTESIAN_POINT('Ctrl Pts',(0.302546739078168,2.21216360281485,12.8186387015698));
#37650=CARTESIAN_POINT('Ctrl Pts',(0.307723861557192,2.19706379715061,12.8177248300039));
#37651=CARTESIAN_POINT('Ctrl Pts',(0.316212620434076,2.1646476848214,12.8158363005609));
#37652=CARTESIAN_POINT('Ctrl Pts',(0.319265758241281,2.14731938135108,12.8148671895422));
#37653=CARTESIAN_POINT('Ctrl Pts',(0.322281284058626,2.11487875086428,12.8130164791697));
#37654=CARTESIAN_POINT('Ctrl Pts',(0.322624385960057,2.09985196986792,12.8121451498433));
#37655=CARTESIAN_POINT('Ctrl Pts',(0.321844346021484,2.08326919318544,12.8111435318882));
#37656=CARTESIAN_POINT('Ctrl Pts',(0.321757899432826,2.08168178567307,12.8110472575976));
#37657=CARTESIAN_POINT('Ctrl Pts',(0.321586465717361,2.07891144613579,12.8108785248203));
#37658=CARTESIAN_POINT('Ctrl Pts',(0.32150668659176,2.07772821393267,12.8108062298208));
#37659=CARTESIAN_POINT('Ctrl Pts',(0.321381679545725,2.07601512067632,12.8107012214256));
#37660=CARTESIAN_POINT('Ctrl Pts',(0.321341667437633,2.07548487922013,12.8106686718477));
#37661=CARTESIAN_POINT('Ctrl Pts',(0.321269321853031,2.07455677295298,12.8106116154829));
#37662=CARTESIAN_POINT('Ctrl Pts',(0.321237561056537,2.0741588635969,12.810587126736));
#37663=CARTESIAN_POINT('Ctrl Pts',(0.321175062986253,2.07339379219501,12.8105399895523));
#37664=CARTESIAN_POINT('Ctrl Pts',(0.321144435160048,2.07302662160633,12.8105173445917));
#37665=CARTESIAN_POINT('Ctrl Pts',(0.321070784690939,2.07216159935117,12.8104639403661));
#37666=CARTESIAN_POINT('Ctrl Pts',(0.321027233731924,2.07166379470218,12.8104331645303));
#37667=CARTESIAN_POINT('Ctrl Pts',(0.320895129117275,2.07019319009003,12.8103421199722));
#37668=CARTESIAN_POINT('Ctrl Pts',(0.320803310768753,2.06922069568139,12.8102817486766));
#37669=CARTESIAN_POINT('Ctrl Pts',(0.319946577898176,2.06056719828913,12.8097430619174));
#37670=CARTESIAN_POINT('Ctrl Pts',(0.318910415135014,2.05291614794123,12.8092562430717));
#37671=CARTESIAN_POINT('Ctrl Pts',(0.31678603845607,2.04057923964921,12.8084531337641));
#37672=CARTESIAN_POINT('Ctrl Pts',(0.315865818340726,2.03586730899957,12.8081420660488));
#37673=CARTESIAN_POINT('Ctrl Pts',(0.308981607262987,2.00437409448425,12.8060342900635));
#37674=CARTESIAN_POINT('Ctrl Pts',(0.299723488107712,1.97842923616108,12.8041442608572));
#37675=CARTESIAN_POINT('Ctrl Pts',(0.282898017303006,1.945326029564,12.8016727225593));
#37676=CARTESIAN_POINT('Ctrl Pts',(0.278112616825124,1.93687815089933,12.801037605369));
#37677=CARTESIAN_POINT('Ctrl Pts',(0.272197009653912,1.92745439978341,12.8003345075261));
#37678=CARTESIAN_POINT('Ctrl Pts',(0.271433289850888,1.92625545891521,12.8002451616514));
#37679=CARTESIAN_POINT('Ctrl Pts',(0.270442207240963,1.92472207329882,12.8001310695506));
#37680=CARTESIAN_POINT('Ctrl Pts',(0.270222128836323,1.92438297309927,12.8001058498632));
#37681=CARTESIAN_POINT('Ctrl Pts',(0.269868321454398,1.9238400609642,12.8000654913053));
#37682=CARTESIAN_POINT('Ctrl Pts',(0.269734999180581,1.92363598648333,12.8000503253229));
#37683=CARTESIAN_POINT('Ctrl Pts',(0.269481210209441,1.92324847630247,12.800021535702));
#37684=CARTESIAN_POINT('Ctrl Pts',(0.269360788691905,1.92306501391504,12.8000079092662));
#37685=CARTESIAN_POINT('Ctrl Pts',(0.26908398215702,1.92264423622231,12.7999766647861));
#37686=CARTESIAN_POINT('Ctrl Pts',(0.268927470763725,1.92240700501213,12.7999590553954));
#37687=CARTESIAN_POINT('Ctrl Pts',(0.26844228150179,1.92167369445557,12.7999046401988));
#37688=CARTESIAN_POINT('Ctrl Pts',(0.268112540915502,1.92117831461427,12.7998679055396));
#37689=CARTESIAN_POINT('Ctrl Pts',(0.26553705631142,1.91733221972438,12.7995828708176));
#37690=CARTESIAN_POINT('Ctrl Pts',(0.263229831986759,1.91402283627209,12.7993386212626));
#37691=CARTESIAN_POINT('Ctrl Pts',(0.260362541519931,1.91007042612646,12.7990470087596));
#37692=CARTESIAN_POINT('Ctrl Pts',(0.259861411499974,1.90938535496712,12.7989964671431));
#37693=CARTESIAN_POINT('Ctrl Pts',(0.257822019165564,1.90662038835086,12.7987924588947));
#37694=CARTESIAN_POINT('Ctrl Pts',(0.256261408480435,1.90455701846726,12.7986401685053));
#37695=CARTESIAN_POINT('Ctrl Pts',(0.251532889154093,1.89845920760348,12.7981892328105));
#37696=CARTESIAN_POINT('Ctrl Pts',(0.248293244609554,1.89448125560719,12.7978938899385));
#37697=CARTESIAN_POINT('Ctrl Pts',(0.229027081004777,1.87194526764538,12.7962030526133));
#37698=CARTESIAN_POINT('Ctrl Pts',(0.211019549998739,1.8551874390649,12.7948681101692));
#37699=CARTESIAN_POINT('Ctrl Pts',(0.181451524726275,1.8333807551702,12.7927601774063));
#37700=CARTESIAN_POINT('Ctrl Pts',(0.17121428858235,1.82669413979487,12.792044300411));
#37701=CARTESIAN_POINT('Ctrl Pts',(0.159401752754256,1.81990315747046,12.7912208624954));
#37702=CARTESIAN_POINT('Ctrl Pts',(0.158175938246972,1.81920909480776,12.7911354497365));
#37703=CARTESIAN_POINT('Ctrl Pts',(0.15600551226607,1.81799891071448,12.7909842639244));
#37704=CARTESIAN_POINT('Ctrl Pts',(0.15506278575154,1.81747944031178,12.7909186114017));
#37705=CARTESIAN_POINT('Ctrl Pts',(0.153669483224819,1.81672076362164,12.7908215959574));
#37706=CARTESIAN_POINT('Ctrl Pts',(0.153220906514812,1.81647788509581,12.7907903640199));
#37707=CARTESIAN_POINT('Ctrl Pts',(0.152423451174443,1.81604855408418,12.790734845027));
#37708=CARTESIAN_POINT('Ctrl Pts',(0.152074801549055,1.81586167657782,12.7907105731414));
#37709=CARTESIAN_POINT('Ctrl Pts',(0.151395480458144,1.81549916641149,12.7906632828383));
#37710=CARTESIAN_POINT('Ctrl Pts',(0.151064845093423,1.81532346708805,12.7906402668332));
#37711=CARTESIAN_POINT('Ctrl Pts',(0.150272021668474,1.81490393162464,12.7905850789375));
#37712=CARTESIAN_POINT('Ctrl Pts',(0.149809546366781,1.81466064324797,12.7905528877185));
#37713=CARTESIAN_POINT('Ctrl Pts',(0.148137278417831,1.81378612118715,12.7904364906724));
#37714=CARTESIAN_POINT('Ctrl Pts',(0.146924084400398,1.81316145479842,12.7903520535319));
#37715=CARTESIAN_POINT('Ctrl Pts',(0.125250447984287,1.80217540580457,12.7888435831714));
#37716=CARTESIAN_POINT('Ctrl Pts',(0.103749911909894,1.79402169774127,12.7873397614731));
#37717=CARTESIAN_POINT('Ctrl Pts',(0.0673270662363956,1.78449245784487,
12.7848049970899));
#37718=CARTESIAN_POINT('Ctrl Pts',(0.0528449351368403,1.7817463954164,12.7838021723191));
#37719=CARTESIAN_POINT('Ctrl Pts',(0.0293869323174163,1.77894420343887,
12.7822209543241));
#37720=CARTESIAN_POINT('Ctrl Pts',(0.0205073360428285,1.77825492783069,
12.7816324253688));
#37721=CARTESIAN_POINT('Ctrl Pts',(0.00778265093736817,1.77779622428641,
12.7808130616387));
#37722=CARTESIAN_POINT('Ctrl Pts',(0.00395300021213832,1.77772648300974,
12.7805695799996));
#37723=CARTESIAN_POINT('Ctrl Pts',(-0.000414578155192063,1.7777248186117,
12.7802961344325));
#37724=CARTESIAN_POINT('Ctrl Pts',(-0.000951973252704545,1.77772595796316,
12.7802625623382));
#37725=CARTESIAN_POINT('Ctrl Pts',(-0.00176198122830027,1.77772970138882,
12.7802120724391));
#37726=CARTESIAN_POINT('Ctrl Pts',(-0.00203459437469886,1.77773130718012,
12.7801950990197));
#37727=CARTESIAN_POINT('Ctrl Pts',(-0.00252545891919314,1.77773482142982,
12.7801645719383));
#37728=CARTESIAN_POINT('Ctrl Pts',(-0.00274370991875125,1.77773660568031,
12.7801510113279));
#37729=CARTESIAN_POINT('Ctrl Pts',(-0.00321292090836895,1.77774091828092,
12.7801218847612));
#37730=CARTESIAN_POINT('Ctrl Pts',(-0.00346387904177128,1.77774351805712,
12.7801063229106));
#37731=CARTESIAN_POINT('Ctrl Pts',(-0.00414022903178649,1.77775131480055,
12.7800644265646));
#37732=CARTESIAN_POINT('Ctrl Pts',(-0.00456561592331929,1.77775706095342,
12.780038122924));
#37733=CARTESIAN_POINT('Ctrl Pts',(-0.00652796604187311,1.77778745502861,
12.779916992775));
#37734=CARTESIAN_POINT('Ctrl Pts',(-0.00806478485520179,1.77782225721948,
12.7798227266898));
#37735=CARTESIAN_POINT('Ctrl Pts',(-0.0386408573612863,1.77873359498489,
12.7779580846699));
#37736=CARTESIAN_POINT('Ctrl Pts',(-0.0674354029734516,1.78352201012447,
12.776388274738));
#37737=CARTESIAN_POINT('Ctrl Pts',(-0.114665652532731,1.79812580354504,
12.7736052269428));
#37738=CARTESIAN_POINT('Ctrl Pts',(-0.133511925421488,1.805975140956,12.7724335132134));
#37739=CARTESIAN_POINT('Ctrl Pts',(-0.152496191545028,1.81608559883235,
12.7711254711677));
#37740=CARTESIAN_POINT('Ctrl Pts',(-0.153499686134291,1.81662688566048,
12.7710559449282));
#37741=CARTESIAN_POINT('Ctrl Pts',(-0.154960410723947,1.81742483895959,
12.7709541698236));
#37742=CARTESIAN_POINT('Ctrl Pts',(-0.155419927956753,1.81767731845009,
12.7709220704237));
#37743=CARTESIAN_POINT('Ctrl Pts',(-0.156225552197426,1.81812252768252,
12.7708656474279));
#37744=CARTESIAN_POINT('Ctrl Pts',(-0.156571924684937,1.81831477682053,
12.7708413410783));
#37745=CARTESIAN_POINT('Ctrl Pts',(-0.157243979830494,1.81868941405107,
12.7707940871838));
#37746=CARTESIAN_POINT('Ctrl Pts',(-0.157569701974109,1.81887173038303,
12.770771142242));
#37747=CARTESIAN_POINT('Ctrl Pts',(-0.158346910146726,1.81930853188089,
12.7707162909197));
#37748=CARTESIAN_POINT('Ctrl Pts',(-0.158798099423586,1.81956354045466,
12.7706843657373));
#37749=CARTESIAN_POINT('Ctrl Pts',(-0.160412303274585,1.82048102022052,
12.770569850424));
#37750=CARTESIAN_POINT('Ctrl Pts',(-0.161571791127033,1.82114963990678,
12.7704870385978));
#37751=CARTESIAN_POINT('Ctrl Pts',(-0.17700632936119,1.83017856499719,12.769377160884));
#37752=CARTESIAN_POINT('Ctrl Pts',(-0.19061886661846,1.83961732083457,12.7683099364981));
#37753=CARTESIAN_POINT('Ctrl Pts',(-0.209923162783697,1.85533041284295,
12.7666585372885));
#37754=CARTESIAN_POINT('Ctrl Pts',(-0.216193343477245,1.86085283167352,
12.7660977226627));
#37755=CARTESIAN_POINT('Ctrl Pts',(-0.233885142392716,1.87769971653058,
12.7644485746494));
#37756=CARTESIAN_POINT('Ctrl Pts',(-0.244682821479849,1.88964311045779,
12.7633533654514));
#37757=CARTESIAN_POINT('Ctrl Pts',(-0.259691931728857,1.90897193653139,
12.7617331682992));
#37758=CARTESIAN_POINT('Ctrl Pts',(-0.264579190612359,1.91580038043099,
12.7611867309191));
#37759=CARTESIAN_POINT('Ctrl Pts',(-0.269915437390255,1.92390755000385,
12.7605740719818));
#37760=CARTESIAN_POINT('Ctrl Pts',(-0.270629541952309,1.92500701314151,
12.7604917287081));
#37761=CARTESIAN_POINT('Ctrl Pts',(-0.271546472468741,1.92643779291042,
12.7603855630568));
#37762=CARTESIAN_POINT('Ctrl Pts',(-0.271755423229029,1.92676514095191,
12.7603613402616));
#37763=CARTESIAN_POINT('Ctrl Pts',(-0.272092655439282,1.92729556989709,
12.7603221991707));
#37764=CARTESIAN_POINT('Ctrl Pts',(-0.272221301649726,1.92749841667333,
12.7603072565806));
#37765=CARTESIAN_POINT('Ctrl Pts',(-0.272467573732861,1.92788769514869,
12.7602786302581));
#37766=CARTESIAN_POINT('Ctrl Pts',(-0.272585234733785,1.92807410310701,
12.7602649442258));
#37767=CARTESIAN_POINT('Ctrl Pts',(-0.272855354150572,1.92850302221004,
12.760233502966));
#37768=CARTESIAN_POINT('Ctrl Pts',(-0.273007680997734,1.92874561670577,
12.7602157565404));
#37769=CARTESIAN_POINT('Ctrl Pts',(-0.273478318129193,1.92949737332277,
12.7601608757268));
#37770=CARTESIAN_POINT('Ctrl Pts',(-0.273795531305651,1.93000722591426,
12.7601238137817));
#37771=CARTESIAN_POINT('Ctrl Pts',(-0.276398715824301,1.93421747955254,
12.7598190473085));
#37772=CARTESIAN_POINT('Ctrl Pts',(-0.27861111930298,1.93796314331041,12.7595560630485));
#37773=CARTESIAN_POINT('Ctrl Pts',(-0.281261584416215,1.94266534272298,
12.759234447152));
#37774=CARTESIAN_POINT('Ctrl Pts',(-0.281771579301667,1.94358053062314,
12.7591722451662));
#37775=CARTESIAN_POINT('Ctrl Pts',(-0.298003790445098,1.97304630936764,
12.7571816555366));
#37776=CARTESIAN_POINT('Ctrl Pts',(-0.309310561368489,2.00381759938031,
12.7554484724751));
#37777=CARTESIAN_POINT('Ctrl Pts',(-0.318092910704573,2.04699607174501,
12.7529126429641));
#37778=CARTESIAN_POINT('Ctrl Pts',(-0.31977625636406,2.05833924538311,12.7522394874613));
#37779=CARTESIAN_POINT('Ctrl Pts',(-0.321043663119327,2.07178094364901,
12.7514231559741));
#37780=CARTESIAN_POINT('Ctrl Pts',(-0.321216083520347,2.07381649067866,
12.7512990480815));
#37781=CARTESIAN_POINT('Ctrl Pts',(-0.321418694191573,2.07651306478306,
12.7511339502529));
#37782=CARTESIAN_POINT('Ctrl Pts',(-0.321466220303422,2.0771727729399,12.7510935052819));
#37783=CARTESIAN_POINT('Ctrl Pts',(-0.321540852753819,2.07825522859776,
12.7510270520601));
#37784=CARTESIAN_POINT('Ctrl Pts',(-0.321569157189131,2.07867789374977,
12.7510010814739));
#37785=CARTESIAN_POINT('Ctrl Pts',(-0.321622348306308,2.07949639062806,
12.7509507446949));
#37786=CARTESIAN_POINT('Ctrl Pts',(-0.321647337796222,2.07989221509692,
12.7509263817767));
#37787=CARTESIAN_POINT('Ctrl Pts',(-0.321703294719823,2.08080535577262,
12.7508701313624));
#37788=CARTESIAN_POINT('Ctrl Pts',(-0.321733745071581,2.0813227015386,12.7508382276983));
#37789=CARTESIAN_POINT('Ctrl Pts',(-0.321811944325856,2.08270826229849,
12.7507526891531));
#37790=CARTESIAN_POINT('Ctrl Pts',(-0.321857427274629,2.08357659633482,
12.7506989833232));
#37791=CARTESIAN_POINT('Ctrl Pts',(-0.322151852056877,2.08966954076648,
12.7503214346279));
#37792=CARTESIAN_POINT('Ctrl Pts',(-0.322277069779807,2.09489908999244,
12.7499937336023));
#37793=CARTESIAN_POINT('Ctrl Pts',(-0.322270858283079,2.11040090480719,
12.7490107673536));
#37794=CARTESIAN_POINT('Ctrl Pts',(-0.32177566869535,2.12066562122389,12.7483446080737));
#37795=CARTESIAN_POINT('Ctrl Pts',(-0.317483520666422,2.16524176671075,
12.745388357424));
#37796=CARTESIAN_POINT('Ctrl Pts',(-0.308679940777706,2.19883680377138,
12.7429673497424));
#37797=CARTESIAN_POINT('Ctrl Pts',(-0.294193486321486,2.2315790475234,12.7407070839352));
#37798=CARTESIAN_POINT('Ctrl Pts',(-0.293662297977832,2.23276034054669,
12.7406257194122));
#37799=CARTESIAN_POINT('Ctrl Pts',(-0.292956578761065,2.23430480575694,
12.740519611485));
#37800=CARTESIAN_POINT('Ctrl Pts',(-0.292788477815313,2.23467087714721,
12.7404944816792));
#37801=CARTESIAN_POINT('Ctrl Pts',(-0.292527867487607,2.2352356106612,12.7404557463465));
#37802=CARTESIAN_POINT('Ctrl Pts',(-0.292435841857345,2.23543449355916,
12.7404421110324));
#37803=CARTESIAN_POINT('Ctrl Pts',(-0.292251793430961,2.23583119104158,
12.7404149261675));
#37804=CARTESIAN_POINT('Ctrl Pts',(-0.292159773263715,2.23602900466564,
12.7404013766651));
#37805=CARTESIAN_POINT('Ctrl Pts',(-0.291952818973589,2.23647271078912,
12.7403709983576));
#37806=CARTESIAN_POINT('Ctrl Pts',(-0.291837775319167,2.23671855102661,
12.7403541764921));
#37807=CARTESIAN_POINT('Ctrl Pts',(-0.291496483398094,2.23744547434984,
12.7403044635083));
#37808=CARTESIAN_POINT('Ctrl Pts',(-0.291269353764116,2.2379261462526,12.7402716268644));
#37809=CARTESIAN_POINT('Ctrl Pts',(-0.289469286846647,2.24171133157789,
12.7400133098462));
#37810=CARTESIAN_POINT('Ctrl Pts',(-0.287841273360165,2.24498956392793,
12.7397911798443));
#37811=CARTESIAN_POINT('Ctrl Pts',(-0.281843657943182,2.25656720370941,
12.7390098917046));
#37812=CARTESIAN_POINT('Ctrl Pts',(-0.277167769857751,2.26470335392474,
12.7384667421102));
#37813=CARTESIAN_POINT('Ctrl Pts',(-0.264265181171557,2.28504432835819,
12.737094776661));
#37814=CARTESIAN_POINT('Ctrl Pts',(-0.255545947242584,2.29691060871783,
12.7362800029481));
#37815=CARTESIAN_POINT('Ctrl Pts',(-0.237041839132695,2.31878466718948,
12.7346741001606));
#37816=CARTESIAN_POINT('Ctrl Pts',(-0.227356549554287,2.32883294675853,
12.7338855995298));
#37817=CARTESIAN_POINT('Ctrl Pts',(-0.21034972029776,2.34432841998635,12.7325426643839));
#37818=CARTESIAN_POINT('Ctrl Pts',(-0.203393526719695,2.35014881845531,
12.7320036011275));
#37819=CARTESIAN_POINT('Ctrl Pts',(-0.195302537861792,2.35635791183437,
12.7313833309925));
#37820=CARTESIAN_POINT('Ctrl Pts',(-0.194399749656025,2.35704318224302,
12.7313142147422));
#37821=CARTESIAN_POINT('Ctrl Pts',(-0.193079620064435,2.35803430707788,
12.7312132748753));
#37822=CARTESIAN_POINT('Ctrl Pts',(-0.192665120293248,2.35834394657286,
12.7311815995305));
#37823=CARTESIAN_POINT('Ctrl Pts',(-0.19193167579708,2.3588890971858,12.7311255822123));
#37824=CARTESIAN_POINT('Ctrl Pts',(-0.191613037968386,2.35912502097299,
12.7311012563954));
#37825=CARTESIAN_POINT('Ctrl Pts',(-0.190952768598169,2.35961200961382,
12.7310508703488));
#37826=CARTESIAN_POINT('Ctrl Pts',(-0.190611075522273,2.35986298939353,
12.7310248068777));
#37827=CARTESIAN_POINT('Ctrl Pts',(-0.189733764755043,2.36050472878076,
12.7309579169297));
#37828=CARTESIAN_POINT('Ctrl Pts',(-0.189197436589199,2.36089450968321,
12.7309170526456));
#37829=CARTESIAN_POINT('Ctrl Pts',(-0.186993168925861,2.36248610780821,
12.7307492133639));
#37830=CARTESIAN_POINT('Ctrl Pts',(-0.185314979742844,2.36367358605934,
12.7306216876413));
#37831=CARTESIAN_POINT('Ctrl Pts',(-0.174109977673614,2.37144237792792,
12.7297717653415));
#37832=CARTESIAN_POINT('Ctrl Pts',(-0.164246846310098,2.37752147305494,
12.7290305104738));
#37833=CARTESIAN_POINT('Ctrl Pts',(-0.124942825128483,2.39891624594211,
12.7261005811851));
#37834=CARTESIAN_POINT('Ctrl Pts',(-0.0935381426399251,2.41018025238688,
12.7237844048989));
#37835=CARTESIAN_POINT('Ctrl Pts',(-0.0608254647214458,2.41648295436013,
12.7216279247192));
#37836=CARTESIAN_POINT('Ctrl Pts',(-0.0606800181313171,2.41651087336589,
12.7216183420291));
#37837=CARTESIAN_POINT('Ctrl Pts',(-0.0603166475295293,2.41658036400689,
12.7215944151184));
#37838=CARTESIAN_POINT('Ctrl Pts',(-0.0600986994030898,2.41662181095834,
12.7215800760894));
#37839=CARTESIAN_POINT('Ctrl Pts',(-0.0556300762085716,2.4174668237735,
12.7212863337734));
#37840=CARTESIAN_POINT('Ctrl Pts',(-0.0513634264563727,2.4181849973752,
12.7210105550523));
#37841=CARTESIAN_POINT('Ctrl Pts',(-0.0465424715136856,2.41889696284348,
12.7207051798045));
#37842=CARTESIAN_POINT('Ctrl Pts',(-0.0460013764860825,2.41897546604275,
12.7206709931862));
#37843=CARTESIAN_POINT('Ctrl Pts',(-0.045184049981826,2.41909192247915,
12.720619489867));
#37844=CARTESIAN_POINT('Ctrl Pts',(-0.0449079681481661,2.41913089440299,
12.7206021161082));
#37845=CARTESIAN_POINT('Ctrl Pts',(-0.0444286350722031,2.41919792309505,
12.720571992766));
#37846=CARTESIAN_POINT('Ctrl Pts',(-0.044225407561986,2.41922614405636,
12.7205592338562));
#37847=CARTESIAN_POINT('Ctrl Pts',(-0.043800496915967,2.41928473524476,
12.7205325842717));
#37848=CARTESIAN_POINT('Ctrl Pts',(-0.0435788092353001,2.41931506866474,
12.7205186957714));
#37849=CARTESIAN_POINT('Ctrl Pts',(-0.0430488143718693,2.41938702539646,
12.7204855284205));
#37850=CARTESIAN_POINT('Ctrl Pts',(-0.04274047709039,2.4194284333469,12.720466261838));
#37851=CARTESIAN_POINT('Ctrl Pts',(-0.0416963825037867,2.41956711049236,
12.7204011189465));
#37852=CARTESIAN_POINT('Ctrl Pts',(-0.0409603423033512,2.41966228555527,
12.7203553604523));
#37853=CARTESIAN_POINT('Ctrl Pts',(-0.0392092061358328,2.41988257192766,
12.7202468716592));
#37854=CARTESIAN_POINT('Ctrl Pts',(-0.0381938234744561,2.4200053961753,
12.7201842659374));
#37855=CARTESIAN_POINT('Ctrl Pts',(-0.0260526719490014,2.42141542126039,
12.7194390827068));
#37856=CARTESIAN_POINT('Ctrl Pts',(-0.0148663570043847,2.42212678279148,
12.7187865790783));
#37857=CARTESIAN_POINT('Ctrl Pts',(0.0239225773776201,2.42256787326939,
12.7165729937292));
#37858=CARTESIAN_POINT('Ctrl Pts',(0.0514353445574283,2.41933810346185,
12.7150784566859));
#37859=CARTESIAN_POINT('Ctrl Pts',(0.0884705579172079,2.4100744909077,12.7128643718395));
#37860=CARTESIAN_POINT('Ctrl Pts',(0.0986059675968008,2.4070017203914,12.7122377628991));
#37861=CARTESIAN_POINT('Ctrl Pts',(0.109680877358072,2.40303905690927,12.7115226275228));
#37862=CARTESIAN_POINT('Ctrl Pts',(0.110788441748999,2.40263589672669,12.7114507676475));
#37863=CARTESIAN_POINT('Ctrl Pts',(0.112342347476113,2.40206059227251,12.7113494592059));
#37864=CARTESIAN_POINT('Ctrl Pts',(0.112790564475416,2.40189351268598,12.7113201797891));
#37865=CARTESIAN_POINT('Ctrl Pts',(0.113612467228913,2.40158505026827,12.711266383435));
#37866=CARTESIAN_POINT('Ctrl Pts',(0.113986265795373,2.40144396902725,12.7112418766272));
#37867=CARTESIAN_POINT('Ctrl Pts',(0.114743619069936,2.401156514204,12.7111921409791));
#37868=CARTESIAN_POINT('Ctrl Pts',(0.115127158289912,2.40101010213343,12.7111669108853));
#37869=CARTESIAN_POINT('Ctrl Pts',(0.116071452568792,2.40064755891778,12.7111046866247));
#37870=CARTESIAN_POINT('Ctrl Pts',(0.116631883181514,2.40043059198818,12.7110676644404));
#37871=CARTESIAN_POINT('Ctrl Pts',(0.118678841640688,2.39963153500491,12.7109321005294));
#37872=CARTESIAN_POINT('Ctrl Pts',(0.120161626574517,2.39903997654881,12.7108332405108));
#37873=CARTESIAN_POINT('Ctrl Pts',(0.139958245769743,2.39097108445333,12.7095043638443));
#37874=CARTESIAN_POINT('Ctrl Pts',(0.157546728757828,2.38183550461061,12.7082161720322));
#37875=CARTESIAN_POINT('Ctrl Pts',(0.198618277278576,2.35545124590271,12.7049475942317));
#37876=CARTESIAN_POINT('Ctrl Pts',(0.220818504250289,2.33652452852572,12.7029338638387));
#37877=CARTESIAN_POINT('Ctrl Pts',(0.241187353923832,2.31375711571281,12.7010016026221));
#37878=CARTESIAN_POINT('Ctrl Pts',(0.242183755866325,2.312627544818,12.7009068678861));
#37879=CARTESIAN_POINT('Ctrl Pts',(0.243449252418657,2.31117247766962,12.7007863216411));
#37880=CARTESIAN_POINT('Ctrl Pts',(0.243725655883097,2.31085340523103,12.7007599785039));
#37881=CARTESIAN_POINT('Ctrl Pts',(0.244164884948457,2.31034435382241,12.7007180958952));
#37882=CARTESIAN_POINT('Ctrl Pts',(0.244328116418331,2.31015472812991,12.7007025263277));
#37883=CARTESIAN_POINT('Ctrl Pts',(0.24463202642518,2.3098008437612,12.7006735299879));
#37884=CARTESIAN_POINT('Ctrl Pts',(0.244772759380092,2.30963663482715,12.7006600991993));
#37885=CARTESIAN_POINT('Ctrl Pts',(0.245086986398828,2.30926924309419,12.7006301034972));
#37886=CARTESIAN_POINT('Ctrl Pts',(0.245260392734177,2.30906598662717,12.7006135451364));
#37887=CARTESIAN_POINT('Ctrl Pts',(0.245769457081035,2.30846778704644,12.7005649190285));
#37888=CARTESIAN_POINT('Ctrl Pts',(0.246104417332713,2.30807224718382,12.7005329027107));
#37889=CARTESIAN_POINT('Ctrl Pts',(0.246863601991946,2.30717136136361,12.700460286179));
#37890=CARTESIAN_POINT('Ctrl Pts',(0.247287233242557,2.30666551538809,12.7004197285185));
#37891=CARTESIAN_POINT('Ctrl Pts',(0.251025882491353,2.30217334634081,12.7000614312949));
#37892=CARTESIAN_POINT('Ctrl Pts',(0.254246032364896,2.29810860135809,12.6997502627613));
#37893=CARTESIAN_POINT('Ctrl Pts',(0.261105646015792,2.28900689039399,12.6990772124062));
#37894=CARTESIAN_POINT('Ctrl Pts',(0.264700385988307,2.28393878625517,12.6987176277412));
#37895=CARTESIAN_POINT('Ctrl Pts',(0.279536150612351,2.26168579952436,12.6971884363827));
#37896=CARTESIAN_POINT('Ctrl Pts',(0.289267370979552,2.24355213158384,12.6960629947269));
#37897=CARTESIAN_POINT('Ctrl Pts',(0.304143724761689,2.20807201516693,12.6938863882927));
#37898=CARTESIAN_POINT('Ctrl Pts',(0.309685754581759,2.19098107927744,12.6928478260964));
#37899=CARTESIAN_POINT('Ctrl Pts',(0.314069602660388,2.17227104789943,12.6916805379382));
#37900=CARTESIAN_POINT('Ctrl Pts',(0.314354651685597,2.17102093050411,12.6916024166488));
#37901=CARTESIAN_POINT('Ctrl Pts',(0.314742386399003,2.16927239520752,12.6914929585882));
#37902=CARTESIAN_POINT('Ctrl Pts',(0.314851365817075,2.16877537329861,12.691461823697));
#37903=CARTESIAN_POINT('Ctrl Pts',(0.315037724818665,2.16791572023286,12.6914079348117));
#37904=CARTESIAN_POINT('Ctrl Pts',(0.315115656704324,2.16755320874398,12.6913851985492));
#37905=CARTESIAN_POINT('Ctrl Pts',(0.315275851077469,2.16680173211615,12.6913380425478));
#37906=CARTESIAN_POINT('Ctrl Pts',(0.315358019742335,2.16641274778478,12.6913136198477));
#37907=CARTESIAN_POINT('Ctrl Pts',(0.315548697814019,2.16550174964194,12.691256390038));
#37908=CARTESIAN_POINT('Ctrl Pts',(0.315656631745686,2.1649796177874,12.691223564586));
#37909=CARTESIAN_POINT('Ctrl Pts',(0.31600083677188,2.16329342500347,12.6911174759556));
#37910=CARTESIAN_POINT('Ctrl Pts',(0.316231966110548,2.16212833523045,12.6910440487884));
#37911=CARTESIAN_POINT('Ctrl Pts',(0.319789327093048,2.14366190689422,12.6898782062644));
#37912=CARTESIAN_POINT('Ctrl Pts',(0.321697211899241,2.12612072780041,12.6887399424266));
#37913=CARTESIAN_POINT('Ctrl Pts',(0.322896336572627,2.08074693582228,12.6857215332683));
#37914=CARTESIAN_POINT('Ctrl Pts',(0.320037440726205,2.05300341902457,12.6837975962204));
#37915=CARTESIAN_POINT('Ctrl Pts',(0.313477510586859,2.02520937129726,12.6819436929028));
#37916=CARTESIAN_POINT('Ctrl Pts',(0.313295011307161,2.02444853609156,12.6818930120875));
#37917=CARTESIAN_POINT('Ctrl Pts',(0.312894083096318,2.0228035113205,12.681783591494));
#37918=CARTESIAN_POINT('Ctrl Pts',(0.312674672367909,2.02191956455509,12.6817248937903));
#37919=CARTESIAN_POINT('Ctrl Pts',(0.31157987672749,2.01758755329321,12.681437755011));
#37920=CARTESIAN_POINT('Ctrl Pts',(0.310651145150706,2.01415304568063,12.6812117370444));
#37921=CARTESIAN_POINT('Ctrl Pts',(0.309506854177506,2.01018345550559,12.6809529685311));
#37922=CARTESIAN_POINT('Ctrl Pts',(0.309346550333297,2.00963288066616,12.6809171331943));
#37923=CARTESIAN_POINT('Ctrl Pts',(0.309105805559018,2.00881417349964,12.680863931437));
#37924=CARTESIAN_POINT('Ctrl Pts',(0.309026484527284,2.00854571717531,12.6808465001436));
#37925=CARTESIAN_POINT('Ctrl Pts',(0.308884498576148,2.00806746983367,12.680815471657));
#37926=CARTESIAN_POINT('Ctrl Pts',(0.308821969686714,2.00785763947397,12.6808018665102));
#37927=CARTESIAN_POINT('Ctrl Pts',(0.30869010871261,2.00741679102963,12.680773300529));
#37928=CARTESIAN_POINT('Ctrl Pts',(0.308620731321345,2.00718578772705,12.6807583424441));
#37929=CARTESIAN_POINT('Ctrl Pts',(0.308442352732378,2.00659425860689,12.6807200654912));
#37930=CARTESIAN_POINT('Ctrl Pts',(0.308332978348298,2.00623384432227,12.6806967685287));
#37931=CARTESIAN_POINT('Ctrl Pts',(0.308087707462199,2.00543068880162,12.6806449068712));
#37932=CARTESIAN_POINT('Ctrl Pts',(0.307951487610129,2.0049880460427,12.6806163609016));
#37933=CARTESIAN_POINT('Ctrl Pts',(0.307547099997746,2.00368400537686,12.6805323670296));
#37934=CARTESIAN_POINT('Ctrl Pts',(0.307276266163541,2.00282342960248,12.6804770702883));
#37935=CARTESIAN_POINT('Ctrl Pts',(0.30427741567572,1.9934324664209,12.6798749926308));
#37936=CARTESIAN_POINT('Ctrl Pts',(0.301198279006492,1.98501733199069,12.679347580168));
#37937=CARTESIAN_POINT('Ctrl Pts',(0.291768628981438,1.96223701163983,12.677925578984));
#37938=CARTESIAN_POINT('Ctrl Pts',(0.284713056773765,1.94819055658742,12.6770545096981));
#37939=CARTESIAN_POINT('Ctrl Pts',(0.264125894669908,1.91373112846354,12.6748090552013));
#37940=CARTESIAN_POINT('Ctrl Pts',(0.249246347445778,1.89424628660456,12.6734262111375));
#37941=CARTESIAN_POINT('Ctrl Pts',(0.231270508978587,1.87555095633149,12.6718531054586));
#37942=CARTESIAN_POINT('Ctrl Pts',(0.230224297779887,1.87447795203033,12.6717618851207));
#37943=CARTESIAN_POINT('Ctrl Pts',(0.228788339010278,1.87302562426727,12.6716371196519));
#37944=CARTESIAN_POINT('Ctrl Pts',(0.228405047547426,1.8726399209283,12.6716038587613));
#37945=CARTESIAN_POINT('Ctrl Pts',(0.227752117998115,1.87198620017677,12.6715472696857));
#37946=CARTESIAN_POINT('Ctrl Pts',(0.22748297753402,1.87171768554549,12.6715239635638));
#37947=CARTESIAN_POINT('Ctrl Pts',(0.226962325160456,1.87120007891595,12.6714789163482));
#37948=CARTESIAN_POINT('Ctrl Pts',(0.226710876605779,1.87095092369237,12.6714571780889));
#37949=CARTESIAN_POINT('Ctrl Pts',(0.226114488235349,1.87036191884447,12.6714056595011));
#37950=CARTESIAN_POINT('Ctrl Pts',(0.225769192675481,1.87002243209101,12.6713758633001));
#37951=CARTESIAN_POINT('Ctrl Pts',(0.224752604973225,1.86902744210202,12.6712882325723));
#37952=CARTESIAN_POINT('Ctrl Pts',(0.224079218108836,1.86837409487254,12.6712303040307));
#37953=CARTESIAN_POINT('Ctrl Pts',(0.218950725517841,1.8634415184044,12.6707899955996));
#37954=CARTESIAN_POINT('Ctrl Pts',(0.21437652834929,1.8592884901205,12.6704022100983));
#37955=CARTESIAN_POINT('Ctrl Pts',(0.205611153919882,1.85177827690984,12.6696673542998));
#37956=CARTESIAN_POINT('Ctrl Pts',(0.201449877432279,1.84838936424058,12.669321742861));
#37957=CARTESIAN_POINT('Ctrl Pts',(0.185326038360252,1.83591468623627,12.667994811072));
#37958=CARTESIAN_POINT('Ctrl Pts',(0.172819057310317,1.82756599952935,12.6669891042642));
#37959=CARTESIAN_POINT('Ctrl Pts',(0.145573845088344,1.81201233009996,12.6648691191675));
#37960=CARTESIAN_POINT('Ctrl Pts',(0.13077376418729,1.80499676526009,12.6637560853862));
#37961=CARTESIAN_POINT('Ctrl Pts',(0.11425437003661,1.79865483582613,12.6625909335711));
#37962=CARTESIAN_POINT('Ctrl Pts',(0.113001153961262,1.79818265731498,12.6625030144126));
#37963=CARTESIAN_POINT('Ctrl Pts',(0.105573479386464,1.79543685564542,12.6619848581212));
#37964=CARTESIAN_POINT('Ctrl Pts',(0.0993329737775362,1.79334474788145,
12.6615614341212));
#37965=CARTESIAN_POINT('Ctrl Pts',(0.0924467617944067,1.79126848904973,
12.6611103419266));
#37966=CARTESIAN_POINT('Ctrl Pts',(0.0918607387770176,1.79109361562805,
12.6610720800819));
#37967=CARTESIAN_POINT('Ctrl Pts',(0.0909912654010182,1.79083685166463,
12.6610155026688));
#37968=CARTESIAN_POINT('Ctrl Pts',(0.0907081989301965,1.79075368180613,
12.6609971132553));
#37969=CARTESIAN_POINT('Ctrl Pts',(0.0902239783409053,1.7906121314146,12.6609657075822));
#37970=CARTESIAN_POINT('Ctrl Pts',(0.0900228814852149,1.79055355826065,
12.6609526800409));
#37971=CARTESIAN_POINT('Ctrl Pts',(0.0896307847982094,1.79043976745867,
12.6609273089579));
#37972=CARTESIAN_POINT('Ctrl Pts',(0.0894397915376084,1.79038453067644,
12.6609149643517));
#37973=CARTESIAN_POINT('Ctrl Pts',(0.0890437692126625,1.79027039486817,
12.6608893964575));
#37974=CARTESIAN_POINT('Ctrl Pts',(0.088838732379173,1.79021152255029,12.6608761747367));
#37975=CARTESIAN_POINT('Ctrl Pts',(0.0881847645862222,1.7900244511367,12.660834053848));
#37976=CARTESIAN_POINT('Ctrl Pts',(0.0877356108046971,1.78989702323027,
12.6608051997071));
#37977=CARTESIAN_POINT('Ctrl Pts',(0.0850872172821791,1.78915187100529,
12.6606354972821));
#37978=CARTESIAN_POINT('Ctrl Pts',(0.0828816657773448,1.78855654762444,
12.6604959303619));
#37979=CARTESIAN_POINT('Ctrl Pts',(0.0762912027958152,1.78685261842885,
12.6600836031961));
#37980=CARTESIAN_POINT('Ctrl Pts',(0.0718889212248584,1.78581276652288,
12.6598143622473));
#37981=CARTESIAN_POINT('Ctrl Pts',(0.0547956051997901,1.78215331756569,
12.6587876189092));
#37982=CARTESIAN_POINT('Ctrl Pts',(0.0419720889116463,1.78020714458005,
12.6580565142472));
#37983=CARTESIAN_POINT('Ctrl Pts',(0.005409857505952,1.77689618010248,12.6559995533956));
#37984=CARTESIAN_POINT('Ctrl Pts',(-0.0184077162975488,1.77737575342825,
12.6546865021522));
#37985=CARTESIAN_POINT('Ctrl Pts',(-0.0493395550389234,1.78143722189983,
12.6528522675982));
#37986=CARTESIAN_POINT('Ctrl Pts',(-0.0566869767453593,1.78266231153574,
12.6524074304611));
#37987=CARTESIAN_POINT('Ctrl Pts',(-0.0649325281241641,1.78433264796437,
12.6518955500821));
#37988=CARTESIAN_POINT('Ctrl Pts',(-0.0658792161887074,1.78452886155427,
12.6518365911073));
#37989=CARTESIAN_POINT('Ctrl Pts',(-0.0673113236936698,1.78483241209612,
12.6517471092636));
#37990=CARTESIAN_POINT('Ctrl Pts',(-0.0677974070490249,1.78493661851049,
12.651716686581));
#37991=CARTESIAN_POINT('Ctrl Pts',(-0.0686426883493315,1.78511987640807,
12.6516636932915));
#37992=CARTESIAN_POINT('Ctrl Pts',(-0.0690019966403035,1.78519841907175,
12.6516411390238));
#37993=CARTESIAN_POINT('Ctrl Pts',(-0.0697514783881423,1.78536359614808,
12.6515940339977));
#37994=CARTESIAN_POINT('Ctrl Pts',(-0.0701416265266435,1.78545034161177,
12.6515694797097));
#37995=CARTESIAN_POINT('Ctrl Pts',(-0.0710638396406129,1.78565718739193,
12.6515113599366));
#37996=CARTESIAN_POINT('Ctrl Pts',(-0.0715957618047044,1.78577791288869,
12.6514777744244));
#37997=CARTESIAN_POINT('Ctrl Pts',(-0.0733513243900375,1.7861810460031,
12.6513667196834));
#37998=CARTESIAN_POINT('Ctrl Pts',(-0.0745736090558756,1.7864692528024,
12.6512890642116));
#37999=CARTESIAN_POINT('Ctrl Pts',(-0.0950365845363402,1.79142071770933,
12.6499832722463));
#38000=CARTESIAN_POINT('Ctrl Pts',(-0.113805296649084,1.7978390851135,12.6486966595016));
#38001=CARTESIAN_POINT('Ctrl Pts',(-0.139903283602466,1.80954195707377,
12.6467835617785));
#38002=CARTESIAN_POINT('Ctrl Pts',(-0.147791214723686,1.81347504213293,
12.6461883148161));
#38003=CARTESIAN_POINT('Ctrl Pts',(-0.164165111723942,1.82249560916032,
12.6449233106211));
#38004=CARTESIAN_POINT('Ctrl Pts',(-0.172598591702555,1.82766086073706,
12.6442539267819));
#38005=CARTESIAN_POINT('Ctrl Pts',(-0.184296708382683,1.8355875777654,12.6433098837101));
#38006=CARTESIAN_POINT('Ctrl Pts',(-0.187764609461418,1.83803882030308,
12.6430279864428));
#38007=CARTESIAN_POINT('Ctrl Pts',(-0.191705027663266,1.84094251947338,
12.6427061257315));
#38008=CARTESIAN_POINT('Ctrl Pts',(-0.192225729275967,1.8413286547306,12.6426635621124));
#38009=CARTESIAN_POINT('Ctrl Pts',(-0.194282966337951,1.8428638766497,12.6424952823922));
#38010=CARTESIAN_POINT('Ctrl Pts',(-0.195810421801844,1.84402512629723,
12.6423700822728));
#38011=CARTESIAN_POINT('Ctrl Pts',(-0.198185554477325,1.84586452510421,
12.6421751088282));
#38012=CARTESIAN_POINT('Ctrl Pts',(-0.199040310760639,1.84653341766826,
12.6421048822281));
#38013=CARTESIAN_POINT('Ctrl Pts',(-0.203096257690227,1.84974058263086,
12.6417714218089));
#38014=CARTESIAN_POINT('Ctrl Pts',(-0.206252549160517,1.8523353967536,12.6415112532114));
#38015=CARTESIAN_POINT('Ctrl Pts',(-0.20976783025766,1.85533916854319,12.6412215417368));
#38016=CARTESIAN_POINT('Ctrl Pts',(-0.210175967488279,1.85568968961498,
12.6411879059524));
#38017=CARTESIAN_POINT('Ctrl Pts',(-0.21079258546576,1.85622194925309,12.6411370924412));
#38018=CARTESIAN_POINT('Ctrl Pts',(-0.211001710642537,1.85640293470438,
12.6411198597673));
#38019=CARTESIAN_POINT('Ctrl Pts',(-0.211365142854505,1.8567182829014,12.6410899131889));
#38020=CARTESIAN_POINT('Ctrl Pts',(-0.211519554966323,1.85685252344359,
12.641077190221));
#38021=CARTESIAN_POINT('Ctrl Pts',(-0.211829823873968,1.85712277971408,
12.6410516264236));
#38022=CARTESIAN_POINT('Ctrl Pts',(-0.211985677444673,1.85725879835744,
12.6410387858907));
#38023=CARTESIAN_POINT('Ctrl Pts',(-0.21230658669911,1.85753941140907,12.6410123476971));
#38024=CARTESIAN_POINT('Ctrl Pts',(-0.212471626170902,1.85768402477619,
12.6409987514317));
#38025=CARTESIAN_POINT('Ctrl Pts',(-0.212856360537317,1.85802183777206,
12.6409670572247));
#38026=CARTESIAN_POINT('Ctrl Pts',(-0.213075940750248,1.85821516860771,
12.6409489690446));
#38027=CARTESIAN_POINT('Ctrl Pts',(-0.214322703550612,1.85931590651822,
12.6408462675182));
#38028=CARTESIAN_POINT('Ctrl Pts',(-0.215344373102298,1.86022957804808,
12.6407621158182));
#38029=CARTESIAN_POINT('Ctrl Pts',(-0.222733415671263,1.86692287150594,
12.6401532915388));
#38030=CARTESIAN_POINT('Ctrl Pts',(-0.22887364789554,1.87294933499325,12.6396461842112));
#38031=CARTESIAN_POINT('Ctrl Pts',(-0.239115342780323,1.88383956437788,
12.6387825210659));
#38032=CARTESIAN_POINT('Ctrl Pts',(-0.243327269256387,1.88859203560086,
12.6384215133403));
#38033=CARTESIAN_POINT('Ctrl Pts',(-0.261554233234643,1.91042515595422,
12.6368169446537));
#38034=CARTESIAN_POINT('Ctrl Pts',(-0.27393050852774,1.92879453648479,12.6356046307471));
#38035=CARTESIAN_POINT('Ctrl Pts',(-0.286391385280005,1.9521476635516,12.6340807282555));
#38036=CARTESIAN_POINT('Ctrl Pts',(-0.288373216098588,1.95605131132475,
12.6338267181539));
#38037=CARTESIAN_POINT('Ctrl Pts',(-0.291064666902309,1.96163150468679,
12.6334637986043));
#38038=CARTESIAN_POINT('Ctrl Pts',(-0.291840587455013,1.96327563440083,
12.6333568925903));
#38039=CARTESIAN_POINT('Ctrl Pts',(-0.295345725427335,1.97086861273787,
12.6328631156283));
#38040=CARTESIAN_POINT('Ctrl Pts',(-0.297907083236376,1.97689283849018,
12.6324711441923));
#38041=CARTESIAN_POINT('Ctrl Pts',(-0.30065887570407,1.98395480606048,12.6320098650307));
#38042=CARTESIAN_POINT('Ctrl Pts',(-0.301029958345309,1.98492085021364,
12.6319467272545));
#38043=CARTESIAN_POINT('Ctrl Pts',(-0.301574807989261,1.98635993333962,
12.6318526123332));
#38044=CARTESIAN_POINT('Ctrl Pts',(-0.301752131290522,1.98683162623151,
12.6318217543231));
#38045=CARTESIAN_POINT('Ctrl Pts',(-0.302065878713144,1.98767219745387,
12.6317667464572));
#38046=CARTESIAN_POINT('Ctrl Pts',(-0.302202735570087,1.98804091408301,
12.6317426111193));
#38047=CARTESIAN_POINT('Ctrl Pts',(-0.302489306685563,1.98881734124193,
12.6316917746865));
#38048=CARTESIAN_POINT('Ctrl Pts',(-0.302638872267206,1.98922510547277,
12.631665068688));
#38049=CARTESIAN_POINT('Ctrl Pts',(-0.303030586127574,1.99029975900531,
12.6315946646836));
#38050=CARTESIAN_POINT('Ctrl Pts',(-0.303271356258478,1.99096714502778,
12.6315509208745));
#38051=CARTESIAN_POINT('Ctrl Pts',(-0.304340411217701,1.99396137500652,
12.6313545645777));
#38052=CARTESIAN_POINT('Ctrl Pts',(-0.305144116780036,1.9962968499079,12.6312011385203));
#38053=CARTESIAN_POINT('Ctrl Pts',(-0.310843940760075,2.01350005836985,
12.6300687619498));
#38054=CARTESIAN_POINT('Ctrl Pts',(-0.314677184054625,2.02869547292112,
12.6290548053835));
#38055=CARTESIAN_POINT('Ctrl Pts',(-0.320654555095514,2.06263845251039,
12.6267647108128));
#38056=CARTESIAN_POINT('Ctrl Pts',(-0.322288461322062,2.08141875410052,
12.6254806111673));
#38057=CARTESIAN_POINT('Ctrl Pts',(-0.322274916475093,2.10023202580047,
12.6242160103981));
#38058=CARTESIAN_POINT('',(-0.322553225215846,2.09975585955174,12.4993773449273));
#38059=CARTESIAN_POINT('Ctrl Pts',(-0.322553225215846,2.09975585955174,
12.4993773449273));
#38060=CARTESIAN_POINT('Ctrl Pts',(-0.322684578197607,2.08414723200036,
12.5003433061249));
#38061=CARTESIAN_POINT('Ctrl Pts',(-0.314554479716074,1.96165005111452,
12.5079327151634));
#38062=CARTESIAN_POINT('Ctrl Pts',(-0.157588690559167,1.75304050246825,
12.5221455720428));
#38063=CARTESIAN_POINT('Ctrl Pts',(0.206424151974156,1.77968116227517,12.5420159155657));
#38064=CARTESIAN_POINT('Ctrl Pts',(0.38107093718189,2.10017074822258,12.5618862590884));
#38065=CARTESIAN_POINT('Ctrl Pts',(0.206137015648765,2.42050369592105,12.5817566026112));
#38066=CARTESIAN_POINT('Ctrl Pts',(-0.157899554721464,2.44681813525015,
12.601626946134));
#38067=CARTESIAN_POINT('Ctrl Pts',(-0.314612782206414,2.23815528960921,
12.6158338602394));
#38068=CARTESIAN_POINT('Ctrl Pts',(-0.322686048272827,2.11575543190525,
12.6234173265038));
#38069=CARTESIAN_POINT('Ctrl Pts',(-0.322555864543089,2.10024316196973,
12.6243773449273));
#38070=CARTESIAN_POINT('',(-0.322274864054643,2.10029601277207,12.2494497673494));
#38071=CARTESIAN_POINT('Ctrl Pts',(-0.322274900757235,2.09974708318754,
12.4992173059391));
#38072=CARTESIAN_POINT('Ctrl Pts',(-0.322290026286624,2.11902052901133,
12.4981254716813));
#38073=CARTESIAN_POINT('Ctrl Pts',(-0.320576212832934,2.13825717465125,
12.4970659124543));
#38074=CARTESIAN_POINT('Ctrl Pts',(-0.314206619257685,2.17355803539727,
12.4950292330845));
#38075=CARTESIAN_POINT('Ctrl Pts',(-0.310003156025341,2.18963542280539,
12.4940645046333));
#38076=CARTESIAN_POINT('Ctrl Pts',(-0.304151340170072,2.20655921977322,
12.4929768269527));
#38077=CARTESIAN_POINT('Ctrl Pts',(-0.303713988176344,2.20779943576773,
12.4928967005569));
#38078=CARTESIAN_POINT('Ctrl Pts',(-0.303081013869604,2.20955995426099,
12.4927823501861));
#38079=CARTESIAN_POINT('Ctrl Pts',(-0.302891613247663,2.21008249254088,
12.4927483333191));
#38080=CARTESIAN_POINT('Ctrl Pts',(-0.30256304839729,2.21098170397983,12.49268966222));
#38081=CARTESIAN_POINT('Ctrl Pts',(-0.302424529723917,2.21135861301506,
12.4926650295648));
#38082=CARTESIAN_POINT('Ctrl Pts',(-0.302158550878916,2.21207818440519,
12.4926179248569));
#38083=CARTESIAN_POINT('Ctrl Pts',(-0.302031211250172,2.2124208909316,12.4925954568629));
#38084=CARTESIAN_POINT('Ctrl Pts',(-0.30173242725774,2.21322083033487,12.4925429334093));
#38085=CARTESIAN_POINT('Ctrl Pts',(-0.301560526636234,2.21367789077588,
12.4925128627138));
#38086=CARTESIAN_POINT('Ctrl Pts',(-0.300966146598159,2.21524743090018,
12.4924093912459));
#38087=CARTESIAN_POINT('Ctrl Pts',(-0.300538548479867,2.21635795006759,
12.492335819011));
#38088=CARTESIAN_POINT('Ctrl Pts',(-0.295864224466337,2.22830001311935,
12.491540699915));
#38089=CARTESIAN_POINT('Ctrl Pts',(-0.291040592977938,2.23889510499578,
12.4907996357478));
#38090=CARTESIAN_POINT('Ctrl Pts',(-0.275061774079559,2.2694867432541,12.4885488944374));
#38091=CARTESIAN_POINT('Ctrl Pts',(-0.262339239984499,2.28858055893766,
12.4869902824885));
#38092=CARTESIAN_POINT('Ctrl Pts',(-0.243632780222619,2.31105630630737,
12.4850189630426));
#38093=CARTESIAN_POINT('Ctrl Pts',(-0.239416423400156,2.31582742674833,
12.4845919886044));
#38094=CARTESIAN_POINT('Ctrl Pts',(-0.229124665998932,2.32680028979355,
12.4835947001165));
#38095=CARTESIAN_POINT('Ctrl Pts',(-0.222934096261984,2.33288817645456,
12.4830289971766));
#38096=CARTESIAN_POINT('Ctrl Pts',(-0.215508708151894,2.33962257899729,
12.4823959998899));
#38097=CARTESIAN_POINT('Ctrl Pts',(-0.214507033841069,2.3405196795231,12.4823115224198));
#38098=CARTESIAN_POINT('Ctrl Pts',(-0.213281847524685,2.34160321554687,
12.4822093312029));
#38099=CARTESIAN_POINT('Ctrl Pts',(-0.213063679794022,2.34179563395634,
12.4821911775951));
#38100=CARTESIAN_POINT('Ctrl Pts',(-0.212680939456152,2.34213228100004,
12.4821594065718));
#38101=CARTESIAN_POINT('Ctrl Pts',(-0.212516480358375,2.34227663751795,
12.4821457796296));
#38102=CARTESIAN_POINT('Ctrl Pts',(-0.212195998997101,2.34255736759563,
12.4821192730835));
#38103=CARTESIAN_POINT('Ctrl Pts',(-0.212039991817014,2.34269375854451,
12.4821063921715));
#38104=CARTESIAN_POINT('Ctrl Pts',(-0.211729254575457,2.34296489556985,
12.4820807801458));
#38105=CARTESIAN_POINT('Ctrl Pts',(-0.211574527559349,2.34309964420167,
12.4820680488256));
#38106=CARTESIAN_POINT('Ctrl Pts',(-0.211209237752952,2.34341715480014,
12.4820380429911));
#38107=CARTESIAN_POINT('Ctrl Pts',(-0.210998565859277,2.34359979180998,
12.4820207778431));
#38108=CARTESIAN_POINT('Ctrl Pts',(-0.210374074214234,2.34413976213594,
12.4819697163317));
#38109=CARTESIAN_POINT('Ctrl Pts',(-0.2099595792029,2.3444963183129,12.4819359773638));
#38110=CARTESIAN_POINT('Ctrl Pts',(-0.206257636224627,2.34766444091444,
12.4816359798046));
#38111=CARTESIAN_POINT('Ctrl Pts',(-0.20291460438456,2.35041077369261,12.4813744047309));
#38112=CARTESIAN_POINT('Ctrl Pts',(-0.199342750985433,2.35322656365423,
12.4811033563741));
#38113=CARTESIAN_POINT('Ctrl Pts',(-0.199168264649428,2.35336382391263,
12.4810901363439));
#38114=CARTESIAN_POINT('Ctrl Pts',(-0.198876360551659,2.35359296336294,
12.4810680545548));
#38115=CARTESIAN_POINT('Ctrl Pts',(-0.198759020869685,2.35368494136734,
12.4810591873984));
#38116=CARTESIAN_POINT('Ctrl Pts',(-0.196494501763941,2.35545747404113,
12.4808882397285));
#38117=CARTESIAN_POINT('Ctrl Pts',(-0.194326080410058,2.35711084304287,
12.4807276329801));
#38118=CARTESIAN_POINT('Ctrl Pts',(-0.18797264894187,2.3618288796417,12.4802650956061));
#38119=CARTESIAN_POINT('Ctrl Pts',(-0.183734199615987,2.3648203679699,12.4799664510617));
#38120=CARTESIAN_POINT('Ctrl Pts',(-0.168619979991341,2.37495031770507,
12.4789289373896));
#38121=CARTESIAN_POINT('Ctrl Pts',(-0.157385817704502,2.38153171016061,
12.4782057642214));
#38122=CARTESIAN_POINT('Ctrl Pts',(-0.13280015327219,2.39400213602806,12.4766636875476));
#38123=CARTESIAN_POINT('Ctrl Pts',(-0.119385368028905,2.39970022859808,
12.4758451034907));
#38124=CARTESIAN_POINT('Ctrl Pts',(-0.0975152182488424,2.40728776891555,
12.474501508541));
#38125=CARTESIAN_POINT('Ctrl Pts',(-0.089289508312883,2.40977791272939,
12.4739944467603));
#38126=CARTESIAN_POINT('Ctrl Pts',(-0.0793419929761372,2.41236015899325,
12.4733749100982));
#38127=CARTESIAN_POINT('Ctrl Pts',(-0.0777060693319513,2.41277114220925,
12.4732728270014));
#38128=CARTESIAN_POINT('Ctrl Pts',(-0.0748484897124004,2.41346523192363,
12.4730941345731));
#38129=CARTESIAN_POINT('Ctrl Pts',(-0.0736282578422544,2.41375408780568,
12.4730177108634));
#38130=CARTESIAN_POINT('Ctrl Pts',(-0.0718751972222612,2.41415828623365,
12.4729077347383));
#38131=CARTESIAN_POINT('Ctrl Pts',(-0.0713437025634769,2.41427941212203,
12.4728743682547));
#38132=CARTESIAN_POINT('Ctrl Pts',(-0.0704220533971347,2.41448699450864,
12.4728164662337));
#38133=CARTESIAN_POINT('Ctrl Pts',(-0.0700320395028736,2.41457407515638,
12.4727919507851));
#38134=CARTESIAN_POINT('Ctrl Pts',(-0.0692826901099888,2.41473992406874,
12.4727448227742));
#38135=CARTESIAN_POINT('Ctrl Pts',(-0.0689233794986877,2.41481880297786,
12.4727222138016));
#38136=CARTESIAN_POINT('Ctrl Pts',(-0.0680779000958508,2.41500289296054,
12.4726689867348));
#38137=CARTESIAN_POINT('Ctrl Pts',(-0.0675916222496276,2.41510759377109,
12.4726383523395));
#38138=CARTESIAN_POINT('Ctrl Pts',(-0.0661583709685047,2.41541271772961,
12.47254799839));
#38139=CARTESIAN_POINT('Ctrl Pts',(-0.0652107409874402,2.41560999949604,
12.4724881784425));
#38140=CARTESIAN_POINT('Ctrl Pts',(-0.0569343896900057,2.41729414087804,
12.4719650063401));
#38141=CARTESIAN_POINT('Ctrl Pts',(-0.0495574007219953,2.41852966194042,
12.4714936802498));
#38142=CARTESIAN_POINT('Ctrl Pts',(-0.0186826131266899,2.42260219662153,
12.469497956932));
#38143=CARTESIAN_POINT('Ctrl Pts',(0.00504550425815098,2.42310279770829,
12.4679016658535));
#38144=CARTESIAN_POINT('Ctrl Pts',(0.0415061952087167,2.41985315812628,
12.4654252927583));
#38145=CARTESIAN_POINT('Ctrl Pts',(0.0543222232273812,2.41792758160035,
12.4645520674005));
#38146=CARTESIAN_POINT('Ctrl Pts',(0.0705689334140489,2.41447511945697,
12.4634654619567));
#38147=CARTESIAN_POINT('Ctrl Pts',(0.074136451731667,2.4136532544204,12.4632281838213));
#38148=CARTESIAN_POINT('Ctrl Pts',(0.0797086102165182,2.41226918209775,
12.4628604486367));
#38149=CARTESIAN_POINT('Ctrl Pts',(0.0817230325195258,2.41174805709163,
12.4627281013187));
#38150=CARTESIAN_POINT('Ctrl Pts',(0.0845583286985679,2.41098520277602,
12.4625427996151));
#38151=CARTESIAN_POINT('Ctrl Pts',(0.0853834549580555,2.4107596707358,12.4624889905468));
#38152=CARTESIAN_POINT('Ctrl Pts',(0.0868115907755423,2.41036320036786,
12.4623960726099));
#38153=CARTESIAN_POINT('Ctrl Pts',(0.0874150129769259,2.41019378452422,
12.4623568792882));
#38154=CARTESIAN_POINT('Ctrl Pts',(0.0883028957406706,2.40994170737687,
12.4622993121272));
#38155=CARTESIAN_POINT('Ctrl Pts',(0.0885877380825749,2.40986041378495,
12.4622808595028));
#38156=CARTESIAN_POINT('Ctrl Pts',(0.0890860327096472,2.40971745795855,
12.4622486067419));
#38157=CARTESIAN_POINT('Ctrl Pts',(0.0892995337620247,2.4096559675823,12.4622347965273));
#38158=CARTESIAN_POINT('Ctrl Pts',(0.0897121036771894,2.40953668126229,
12.4622081270728));
#38159=CARTESIAN_POINT('Ctrl Pts',(0.0899111798673848,2.40947891419049,
12.462195266163));
#38160=CARTESIAN_POINT('Ctrl Pts',(0.090385693998628,2.40934072521842,12.4621646295082));
#38161=CARTESIAN_POINT('Ctrl Pts',(0.0906610811077255,2.40926012729114,
12.4621468641018));
#38162=CARTESIAN_POINT('Ctrl Pts',(0.0916404506219502,2.40897207327173,
12.4620837356401));
#38163=CARTESIAN_POINT('Ctrl Pts',(0.0923438384569645,2.40876257832882,
12.4620384908834));
#38164=CARTESIAN_POINT('Ctrl Pts',(0.102784348805078,2.40561413905456,12.4613682345227));
#38165=CARTESIAN_POINT('Ctrl Pts',(0.112378875572752,2.40221790261043,12.4607693152175));
#38166=CARTESIAN_POINT('Ctrl Pts',(0.143209097334117,2.38963282032531,12.458852532942));
#38167=CARTESIAN_POINT('Ctrl Pts',(0.163618345664013,2.37861294966487,12.4575916325838));
#38168=CARTESIAN_POINT('Ctrl Pts',(0.196750278942803,2.35581727309351,12.4553100454899));
#38169=CARTESIAN_POINT('Ctrl Pts',(0.210032812175859,2.3450290576798,12.4543172764806));
#38170=CARTESIAN_POINT('Ctrl Pts',(0.223246425643824,2.33242974796044,12.4532072132991));
#38171=CARTESIAN_POINT('Ctrl Pts',(0.224091763809188,2.33161484329695,12.4531356258133));
#38172=CARTESIAN_POINT('Ctrl Pts',(0.225312649999349,2.33042497038078,12.4530313925262));
#38173=CARTESIAN_POINT('Ctrl Pts',(0.225691761636345,2.33005365884696,12.452998906682));
#38174=CARTESIAN_POINT('Ctrl Pts',(0.226353001772631,2.32940281590998,12.452942035723));
#38175=CARTESIAN_POINT('Ctrl Pts',(0.226635534617074,2.32912369542555,12.4529176687143));
#38176=CARTESIAN_POINT('Ctrl Pts',(0.227181326279846,2.32858249846448,12.4528704660266));
#38177=CARTESIAN_POINT('Ctrl Pts',(0.227444649490961,2.32832048754037,12.4528476332635));
#38178=CARTESIAN_POINT('Ctrl Pts',(0.228069422328669,2.32769667492192,12.4527933176231));
#38179=CARTESIAN_POINT('Ctrl Pts',(0.228430464078042,2.32733446779604,12.452761816776));
#38180=CARTESIAN_POINT('Ctrl Pts',(0.229704395509317,2.32605032546645,12.4526502640619));
#38181=CARTESIAN_POINT('Ctrl Pts',(0.230612569078438,2.32512374788962,12.4525700052067));
#38182=CARTESIAN_POINT('Ctrl Pts',(0.245623124152832,2.30962286183139,12.4512310856986));
#38183=CARTESIAN_POINT('Ctrl Pts',(0.258321717526134,2.29375776996131,12.449910934293));
#38184=CARTESIAN_POINT('Ctrl Pts',(0.284978085243346,2.25313513107307,12.4466567642006));
#38185=CARTESIAN_POINT('Ctrl Pts',(0.297324711375373,2.22751857426121,12.4446957041301));
#38186=CARTESIAN_POINT('Ctrl Pts',(0.306588638485943,2.19932985946696,12.4428106627899));
#38187=CARTESIAN_POINT('Ctrl Pts',(0.307003857071948,2.19803900306387,12.4427249369398));
#38188=CARTESIAN_POINT('Ctrl Pts',(0.307687621994381,2.19586632606344,12.4425816945084));
#38189=CARTESIAN_POINT('Ctrl Pts',(0.307960550560082,2.19498591763744,12.4425239369798));
#38190=CARTESIAN_POINT('Ctrl Pts',(0.308328608240422,2.19378038012545,12.4424452534898));
#38191=CARTESIAN_POINT('Ctrl Pts',(0.308427004144702,2.19345626502695,12.4424241388146));
#38192=CARTESIAN_POINT('Ctrl Pts',(0.308583865830456,2.19293661831519,12.4423903505375));
#38193=CARTESIAN_POINT('Ctrl Pts',(0.308642656847939,2.19274118636902,12.4423776578203));
#38194=CARTESIAN_POINT('Ctrl Pts',(0.308764860524416,2.19233355608487,12.4423512140617));
#38195=CARTESIAN_POINT('Ctrl Pts',(0.308828239955441,2.19212134866684,12.4423374650717));
#38196=CARTESIAN_POINT('Ctrl Pts',(0.308974925122138,2.19162836376462,12.4423055643036));
#38197=CARTESIAN_POINT('Ctrl Pts',(0.309058067190835,2.19134753694711,12.4422874221764));
#38198=CARTESIAN_POINT('Ctrl Pts',(0.309326623957569,2.19043587597952,12.4422286227424));
#38199=CARTESIAN_POINT('Ctrl Pts',(0.309510492462696,2.18980458243663,12.4421880555103));
#38200=CARTESIAN_POINT('Ctrl Pts',(0.31129414499497,2.18361004602388,12.4417914142068));
#38201=CARTESIAN_POINT('Ctrl Pts',(0.312745817945078,2.1780047950456,12.4414437396001));
#38202=CARTESIAN_POINT('Ctrl Pts',(0.320479924283225,2.14443983202386,12.4394116308283));
#38203=CARTESIAN_POINT('Ctrl Pts',(0.323161959155335,2.11578050504518,12.4378701329498));
#38204=CARTESIAN_POINT('Ctrl Pts',(0.321377099112435,2.07108185415861,12.4353249612468));
#38205=CARTESIAN_POINT('Ctrl Pts',(0.319535478305687,2.05509491381871,12.434388354495));
#38206=CARTESIAN_POINT('Ctrl Pts',(0.316286256584576,2.03814867899337,12.4333393448164));
#38207=CARTESIAN_POINT('Ctrl Pts',(0.316056516197759,2.03698523566139,12.433267045383));
#38208=CARTESIAN_POINT('Ctrl Pts',(0.315714256426155,2.03530094422519,12.4331619645296));
#38209=CARTESIAN_POINT('Ctrl Pts',(0.315606856684791,2.03477905599402,12.4331293467709));
#38210=CARTESIAN_POINT('Ctrl Pts',(0.315417073123507,2.0338682857997,12.4330723222247));
#38211=CARTESIAN_POINT('Ctrl Pts',(0.315335262907165,2.03347928438561,12.4330479338382));
#38212=CARTESIAN_POINT('Ctrl Pts',(0.315175731403202,2.03272763185277,12.433000745886));
#38213=CARTESIAN_POINT('Ctrl Pts',(0.315098103343966,2.03236496138148,12.4329779493404));
#38214=CARTESIAN_POINT('Ctrl Pts',(0.314912415842221,2.03150470643102,12.432923807928));
#38215=CARTESIAN_POINT('Ctrl Pts',(0.314803803104114,2.03100724357499,12.4328924453605));
#38216=CARTESIAN_POINT('Ctrl Pts',(0.314417092773972,2.02925597720847,12.4327818449955));
#38217=CARTESIAN_POINT('Ctrl Pts',(0.31413268268596,2.0280035932764,12.4327024048208));
#38218=CARTESIAN_POINT('Ctrl Pts',(0.30971062648175,2.00905645776845,12.4314952245629));
#38219=CARTESIAN_POINT('Ctrl Pts',(0.304091886191966,1.99174418950717,12.4303186304509));
#38220=CARTESIAN_POINT('Ctrl Pts',(0.290663614268348,1.95983373276787,12.428011793656));
#38221=CARTESIAN_POINT('Ctrl Pts',(0.283129557936342,1.94517904450121,12.4268915142553));
#38222=CARTESIAN_POINT('Ctrl Pts',(0.266491842701544,1.91812771905889,12.424751469655));
#38223=CARTESIAN_POINT('Ctrl Pts',(0.25755390985221,1.90567671745366,12.4237332386531));
#38224=CARTESIAN_POINT('Ctrl Pts',(0.247362680939358,1.89342489802427,12.4227309828571));
#38225=CARTESIAN_POINT('Ctrl Pts',(0.246960347169611,1.89294407610735,12.4226916501911));
#38226=CARTESIAN_POINT('Ctrl Pts',(0.246236392167622,1.89208400239844,12.4226212998441));
#38227=CARTESIAN_POINT('Ctrl Pts',(0.245915292804973,1.89170431675404,12.4225902453808));
#38228=CARTESIAN_POINT('Ctrl Pts',(0.245423232877895,1.89112520165268,12.4225428850124));
#38229=CARTESIAN_POINT('Ctrl Pts',(0.245252906964426,1.89092523765994,12.4225265328323));
#38230=CARTESIAN_POINT('Ctrl Pts',(0.244954447611766,1.89057571056123,12.4224979521194));
#38231=CARTESIAN_POINT('Ctrl Pts',(0.244826421815556,1.89042605697884,12.422485715683));
#38232=CARTESIAN_POINT('Ctrl Pts',(0.24455809955657,1.89011298764975,12.4224601190365));
#38233=CARTESIAN_POINT('Ctrl Pts',(0.244417776896874,1.88994959569315,12.4224467608771));
#38234=CARTESIAN_POINT('Ctrl Pts',(0.244026715316692,1.88949516535379,12.4224096106649));
#38235=CARTESIAN_POINT('Ctrl Pts',(0.243775618600757,1.88920443321279,12.4223858451214));
#38236=CARTESIAN_POINT('Ctrl Pts',(0.242771979841304,1.88804656249271,12.4222912017266));
#38237=CARTESIAN_POINT('Ctrl Pts',(0.242015314317958,1.88718298565185,12.4222206256285));
#38238=CARTESIAN_POINT('Ctrl Pts',(0.228353229259573,1.87175764647997,12.4209598091936));
#38239=CARTESIAN_POINT('Ctrl Pts',(0.214157565312173,1.85838760035137,12.419862942759));
#38240=CARTESIAN_POINT('Ctrl Pts',(0.185954565646599,1.83627633873239,12.4178565601304));
#38241=CARTESIAN_POINT('Ctrl Pts',(0.172318068100565,1.82717088161644,12.4169476693011));
#38242=CARTESIAN_POINT('Ctrl Pts',(0.145963516883332,1.81234021676456,12.4152155501483));
#38243=CARTESIAN_POINT('Ctrl Pts',(0.133452758760993,1.80632707829239,12.414402548287));
#38244=CARTESIAN_POINT('Ctrl Pts',(0.119429354491756,1.80066843774786,12.4134836604013));
#38245=CARTESIAN_POINT('Ctrl Pts',(0.118261244617346,1.80020501534176,12.413407071664));
#38246=CARTESIAN_POINT('Ctrl Pts',(0.116582145275752,1.7995502093278,12.4132969001715));
#38247=CARTESIAN_POINT('Ctrl Pts',(0.116073323491315,1.79935326896843,12.4132635042679));
#38248=CARTESIAN_POINT('Ctrl Pts',(0.115190884527432,1.79901429351208,12.4132055675852));
#38249=CARTESIAN_POINT('Ctrl Pts',(0.114817497567415,1.79887165919118,12.4131810469619));
#38250=CARTESIAN_POINT('Ctrl Pts',(0.114100058219928,1.79859912477645,12.4131339205454));
#38251=CARTESIAN_POINT('Ctrl Pts',(0.113756046713933,1.79846911815605,12.4131113183636));
#38252=CARTESIAN_POINT('Ctrl Pts',(0.112946614506063,1.79816480507354,12.4130581248289));
#38253=CARTESIAN_POINT('Ctrl Pts',(0.112481012624485,1.79799098619539,12.413027517226));
#38254=CARTESIAN_POINT('Ctrl Pts',(0.111108983577949,1.79748239211648,12.4129372938686));
#38255=CARTESIAN_POINT('Ctrl Pts',(0.110201456668662,1.79715061791905,12.4128775781307));
#38256=CARTESIAN_POINT('Ctrl Pts',(0.102300268360973,1.79430231441866,12.4123573281569));
#38257=CARTESIAN_POINT('Ctrl Pts',(0.0952234886330571,1.7920245264706,12.4118889177847));
#38258=CARTESIAN_POINT('Ctrl Pts',(0.0841737473577247,1.78888522694789,
12.4111529321127));
#38259=CARTESIAN_POINT('Ctrl Pts',(0.080252315188744,1.78785070011569,12.4108908774919));
#38260=CARTESIAN_POINT('Ctrl Pts',(0.0496201198374673,1.78038487634848,
12.4088374199338));
#38261=CARTESIAN_POINT('Ctrl Pts',(0.0222067609649575,1.77731985982936,
12.4069482854065));
#38262=CARTESIAN_POINT('Ctrl Pts',(-0.0168461864125599,1.77795693509862,
12.4043402650436));
#38263=CARTESIAN_POINT('Ctrl Pts',(-0.0284186537932631,1.7787711457504,
12.4035799449124));
#38264=CARTESIAN_POINT('Ctrl Pts',(-0.0406630980736328,1.78029975942349,
12.4028054495856));
#38265=CARTESIAN_POINT('Ctrl Pts',(-0.0414025247065735,1.78039467722863,
12.4027587968817));
#38266=CARTESIAN_POINT('Ctrl Pts',(-0.0424506183693955,1.78053291599362,
12.4026928433818));
#38267=CARTESIAN_POINT('Ctrl Pts',(-0.0427595550149776,1.78057411936356,
12.4026734243439));
#38268=CARTESIAN_POINT('Ctrl Pts',(-0.0432902825347482,1.78064568708836,
12.4026401014833));
#38269=CARTESIAN_POINT('Ctrl Pts',(-0.0435121020223595,1.78067583443164,
12.4026261853172));
#38270=CARTESIAN_POINT('Ctrl Pts',(-0.043937048360315,1.78073403962603,
12.4025995474618));
#38271=CARTESIAN_POINT('Ctrl Pts',(-0.0441401795365313,1.78076206017579,
12.4025868236526));
#38272=CARTESIAN_POINT('Ctrl Pts',(-0.0446189727882375,1.78082857213866,
12.4025568549538));
#38273=CARTESIAN_POINT('Ctrl Pts',(-0.0448946125427213,1.78086722690749,
12.4025396193738));
#38274=CARTESIAN_POINT('Ctrl Pts',(-0.0457096991685293,1.78098260875728,
12.4024887027934));
#38275=CARTESIAN_POINT('Ctrl Pts',(-0.0462490053559496,1.78106034735832,
12.4024550787309));
#38276=CARTESIAN_POINT('Ctrl Pts',(-0.0510157849502292,1.78175980246951,
12.4021584405468));
#38277=CARTESIAN_POINT('Ctrl Pts',(-0.0552309486542478,1.78246420634107,
12.4018999953036));
#38278=CARTESIAN_POINT('Ctrl Pts',(-0.0596870585361504,1.78330030235255,
12.4016297022023));
#38279=CARTESIAN_POINT('Ctrl Pts',(-0.0599429604798284,1.7833486381895,
12.4016141903038));
#38280=CARTESIAN_POINT('Ctrl Pts',(-0.0603204949564488,1.78342042255194,
12.4015913202584));
#38281=CARTESIAN_POINT('Ctrl Pts',(-0.0604421723909528,1.7834436309822,
12.4015839516291));
#38282=CARTESIAN_POINT('Ctrl Pts',(-0.0614290730691154,1.78363245955405,
12.4015242043827));
#38283=CARTESIAN_POINT('Ctrl Pts',(-0.0622936358762339,1.78380155815278,
12.4014719769428));
#38284=CARTESIAN_POINT('Ctrl Pts',(-0.0883293179160923,1.78900476838662,
12.3999023136815));
#38285=CARTESIAN_POINT('Ctrl Pts',(-0.11281270690571,1.79702523189865,12.3985082595602));
#38286=CARTESIAN_POINT('Ctrl Pts',(-0.147102073554181,1.81299857443853,
12.3963745956976));
#38287=CARTESIAN_POINT('Ctrl Pts',(-0.157817272638603,1.81874831816142,
12.3956799637302));
#38288=CARTESIAN_POINT('Ctrl Pts',(-0.174608347743744,1.82902055400519,
12.3945223613654));
#38289=CARTESIAN_POINT('Ctrl Pts',(-0.18089472592584,1.83317605157413,12.394072135403));
#38290=CARTESIAN_POINT('Ctrl Pts',(-0.18782941374598,1.83811786611662,12.3935536718632));
#38291=CARTESIAN_POINT('Ctrl Pts',(-0.188626828305283,1.83869163747512,
12.3934937193264));
#38292=CARTESIAN_POINT('Ctrl Pts',(-0.18982073281737,1.83955901165978,12.3934034475937));
#38293=CARTESIAN_POINT('Ctrl Pts',(-0.190219197384165,1.83984989725697,
12.3933732336415));
#38294=CARTESIAN_POINT('Ctrl Pts',(-0.190903406482155,1.84035179339406,
12.3933212042604));
#38295=CARTESIAN_POINT('Ctrl Pts',(-0.191189473786501,1.84056236411855,
12.3932994059581));
#38296=CARTESIAN_POINT('Ctrl Pts',(-0.191777974666696,1.84099705454615,
12.3932544694453));
#38297=CARTESIAN_POINT('Ctrl Pts',(-0.192080364794332,1.84122123197673,
12.3932313290028));
#38298=CARTESIAN_POINT('Ctrl Pts',(-0.192807580535545,1.84176233150446,
12.3931755561862));
#38299=CARTESIAN_POINT('Ctrl Pts',(-0.193232017392648,1.84207977203989,
12.3931429035605));
#38300=CARTESIAN_POINT('Ctrl Pts',(-0.194783643135526,1.84324622811512,
12.3930231621745));
#38301=CARTESIAN_POINT('Ctrl Pts',(-0.19590602259413,1.84410158808627,12.3929358244279));
#38302=CARTESIAN_POINT('Ctrl Pts',(-0.215881062186123,1.85953290464592,
12.3913683610573));
#38303=CARTESIAN_POINT('Ctrl Pts',(-0.2330612849956,1.87614502260686,12.3898016482174));
#38304=CARTESIAN_POINT('Ctrl Pts',(-0.257863258200955,1.90610587732993,
12.3871792712474));
#38305=CARTESIAN_POINT('Ctrl Pts',(-0.266648866503839,1.91837735945161,
12.3861525365442));
#38306=CARTESIAN_POINT('Ctrl Pts',(-0.278769650686272,1.93809330566276,
12.3846094623814));
#38307=CARTESIAN_POINT('Ctrl Pts',(-0.282736560540412,1.94512471438944,
12.3840783999449));
#38308=CARTESIAN_POINT('Ctrl Pts',(-0.287984080354277,1.95530113757531,
12.38334385278));
#38309=CARTESIAN_POINT('Ctrl Pts',(-0.289485335073529,1.95832842788299,
12.383129471457));
#38310=CARTESIAN_POINT('Ctrl Pts',(-0.291162997825407,1.96184951658988,
12.3828853311461));
#38311=CARTESIAN_POINT('Ctrl Pts',(-0.291386081890458,1.96232066727819,
12.3828527697961));
#38312=CARTESIAN_POINT('Ctrl Pts',(-0.291722666349328,1.96303601177082,
12.3828034960315));
#38313=CARTESIAN_POINT('Ctrl Pts',(-0.291837004147715,1.96327980710604,
12.3827867319244));
#38314=CARTESIAN_POINT('Ctrl Pts',(-0.292043367533353,1.96372126122609,
12.3827564286768));
#38315=CARTESIAN_POINT('Ctrl Pts',(-0.292135497806559,1.96391886947774,
12.3827428830503));
#38316=CARTESIAN_POINT('Ctrl Pts',(-0.292320340948617,1.9643163884191,12.3827156722394));
#38317=CARTESIAN_POINT('Ctrl Pts',(-0.292413048901168,1.96451629981072,
12.3827020073775));
#38318=CARTESIAN_POINT('Ctrl Pts',(-0.292677185669697,1.96508740686366,
12.3826630245014));
#38319=CARTESIAN_POINT('Ctrl Pts',(-0.292848114015169,1.96545883559131,
12.3826377375316));
#38320=CARTESIAN_POINT('Ctrl Pts',(-0.293578379517358,1.96705369379375,
12.3825294385826));
#38321=CARTESIAN_POINT('Ctrl Pts',(-0.294130770780488,1.96828031626675,
12.3824468491483));
#38322=CARTESIAN_POINT('Ctrl Pts',(-0.303997422645833,1.99056147924542,
12.3809587312885));
#38323=CARTESIAN_POINT('Ctrl Pts',(-0.31103842916825,2.01255469288941,12.379681987296));
#38324=CARTESIAN_POINT('Ctrl Pts',(-0.318730994436393,2.04997944678461,
12.3775463056297));
#38325=CARTESIAN_POINT('Ctrl Pts',(-0.320732575812288,2.06504179493686,
12.3766965896928));
#38326=CARTESIAN_POINT('Ctrl Pts',(-0.322069846210219,2.08675385496259,
12.3754388283474));
#38327=CARTESIAN_POINT('Ctrl Pts',(-0.322273096087557,2.09332994929834,
12.3750537678569));
#38328=CARTESIAN_POINT('Ctrl Pts',(-0.322276461705378,2.1050389730816,12.3743576554723));
#38329=CARTESIAN_POINT('Ctrl Pts',(-0.32215537060393,2.11016964417602,12.3740490550513));
#38330=CARTESIAN_POINT('Ctrl Pts',(-0.321870831240938,2.11615829627295,
12.373683958331));
#38331=CARTESIAN_POINT('Ctrl Pts',(-0.321826342566203,2.11702139094832,
12.3736312216135));
#38332=CARTESIAN_POINT('Ctrl Pts',(-0.321749710133317,2.11840017986138,
12.3735467821712));
#38333=CARTESIAN_POINT('Ctrl Pts',(-0.321719796728216,2.11891599793951,
12.3735151494289));
#38334=CARTESIAN_POINT('Ctrl Pts',(-0.321664744458097,2.11982737749388,
12.3734591816648));
#38335=CARTESIAN_POINT('Ctrl Pts',(-0.321640116001363,2.12022296966275,
12.3734348627071));
#38336=CARTESIAN_POINT('Ctrl Pts',(-0.321587614932111,2.12104189961484,
12.373384465578));
#38337=CARTESIAN_POINT('Ctrl Pts',(-0.321559636043543,2.12146522960347,
12.373358384116));
#38338=CARTESIAN_POINT('Ctrl Pts',(-0.321485701802137,2.12255128555685,
12.3732913952818));
#38339=CARTESIAN_POINT('Ctrl Pts',(-0.321438533224841,2.12321392451062,
12.3732504498849));
#38340=CARTESIAN_POINT('Ctrl Pts',(-0.321236209336698,2.12593731295027,
12.3730818630893));
#38341=CARTESIAN_POINT('Ctrl Pts',(-0.321063285472976,2.12799665683,12.3729536647719));
#38342=CARTESIAN_POINT('Ctrl Pts',(-0.319781573546354,2.14168074161831,
12.3720968790595));
#38343=CARTESIAN_POINT('Ctrl Pts',(-0.318061596280838,2.15323818446407,
12.3713491044441));
#38344=CARTESIAN_POINT('Ctrl Pts',(-0.308959903202273,2.19766864721991,
12.368378481486));
#38345=CARTESIAN_POINT('Ctrl Pts',(-0.297073256600571,2.22939244412999,
12.3660239643655));
#38346=CARTESIAN_POINT('Ctrl Pts',(-0.278475297815029,2.26226356671525,
12.3635881606904));
#38347=CARTESIAN_POINT('Ctrl Pts',(-0.27639016025259,2.26579034890125,12.3633272734452));
#38348=CARTESIAN_POINT('Ctrl Pts',(-0.273955425703913,2.26973476436015,
12.3630368396401));
#38349=CARTESIAN_POINT('Ctrl Pts',(-0.273671475562494,2.27019221186175,
12.3630031778772));
#38350=CARTESIAN_POINT('Ctrl Pts',(-0.273239876536263,2.27088365060094,
12.3629523318112));
#38351=CARTESIAN_POINT('Ctrl Pts',(-0.273093072271738,2.27111816400035,
12.3629350924626));
#38352=CARTESIAN_POINT('Ctrl Pts',(-0.272837163323071,2.27152579925237,
12.3629051375315));
#38353=CARTESIAN_POINT('Ctrl Pts',(-0.27272819571163,2.27169900629816,12.3628924128735));
#38354=CARTESIAN_POINT('Ctrl Pts',(-0.272499476948899,2.2720617940404,12.3628657679937));
#38355=CARTESIAN_POINT('Ctrl Pts',(-0.272379692942661,2.27225135348857,
12.3628518500565));
#38356=CARTESIAN_POINT('Ctrl Pts',(-0.272091874502325,2.27270577825777,
12.3628184947943));
#38357=CARTESIAN_POINT('Ctrl Pts',(-0.27192365043759,2.27297052450779,12.3627990701009));
#38358=CARTESIAN_POINT('Ctrl Pts',(-0.271347965626978,2.27387360543697,
12.3627328358612));
#38359=CARTESIAN_POINT('Ctrl Pts',(-0.270938637579908,2.27451075557445,
12.3626861495704));
#38360=CARTESIAN_POINT('Ctrl Pts',(-0.263550196199281,2.28592276637011,
12.3618506281738));
#38361=CARTESIAN_POINT('Ctrl Pts',(-0.255934672004761,2.29627407750246,
12.3611034909171));
#38362=CARTESIAN_POINT('Ctrl Pts',(-0.227817783086908,2.33006171692015,
12.3586011541544));
#38363=CARTESIAN_POINT('Ctrl Pts',(-0.20455732329365,2.35096956232152,12.3569210539585));
#38364=CARTESIAN_POINT('Ctrl Pts',(-0.173124994607485,2.37190649017438,
12.3546922815772));
#38365=CARTESIAN_POINT('Ctrl Pts',(-0.167477629447395,2.3754208363688,12.3542941209579));
#38366=CARTESIAN_POINT('Ctrl Pts',(-0.160826570176197,2.37927955699399,
12.3538261519073));
#38367=CARTESIAN_POINT('Ctrl Pts',(-0.159924739146724,2.37979695208943,
12.3537627200538));
#38368=CARTESIAN_POINT('Ctrl Pts',(-0.158581285565393,2.38055909609915,
12.3536682511151));
#38369=CARTESIAN_POINT('Ctrl Pts',(-0.158141559866103,2.38080718932049,
12.3536373344888));
#38370=CARTESIAN_POINT('Ctrl Pts',(-0.157358158821926,2.38124676043204,
12.3535822607654));
#38371=CARTESIAN_POINT('Ctrl Pts',(-0.157014711674405,2.38143864467583,
12.3535581183145));
#38372=CARTESIAN_POINT('Ctrl Pts',(-0.156291808879971,2.38184079602012,
12.3535073063399));
#38373=CARTESIAN_POINT('Ctrl Pts',(-0.155912278559379,2.38205092663511,
12.353480631991));
#38374=CARTESIAN_POINT('Ctrl Pts',(-0.154912926458348,2.38260159409755,
12.3534104006092));
#38375=CARTESIAN_POINT('Ctrl Pts',(-0.154292408544179,2.38294085675854,
12.3533667981793));
#38376=CARTESIAN_POINT('Ctrl Pts',(-0.151519091321392,2.3844453072291,12.3531719439067));
#38377=CARTESIAN_POINT('Ctrl Pts',(-0.149354220142093,2.38558796234007,
12.3530198937103));
#38378=CARTESIAN_POINT('Ctrl Pts',(-0.133460614693063,2.39374673162533,
12.3519037430355));
#38379=CARTESIAN_POINT('Ctrl Pts',(-0.119259160883542,2.39979327276105,
12.3509057154518));
#38380=CARTESIAN_POINT('Ctrl Pts',(-0.0883844415753198,2.41039697703056,
12.3487381981583));
#38381=CARTESIAN_POINT('Ctrl Pts',(-0.0716654959918706,2.41467775159411,
12.3475654738115));
#38382=CARTESIAN_POINT('Ctrl Pts',(-0.0390890883744199,2.42028688794024,
12.3453362534991));
#38383=CARTESIAN_POINT('Ctrl Pts',(-0.0233134248564113,2.42182023995543,
12.3442815894348));
#38384=CARTESIAN_POINT('Ctrl Pts',(-0.00658607211306412,2.42220895644832,
12.3432294321605));
#38385=CARTESIAN_POINT('Ctrl Pts',(-0.00568492162010916,2.42222611575352,
12.3431729545758));
#38386=CARTESIAN_POINT('Ctrl Pts',(-0.00447100000889573,2.42224413661959,
12.3430971618197));
#38387=CARTESIAN_POINT('Ctrl Pts',(-0.00415829349260601,2.42224832353952,
12.3430776632413));
#38388=CARTESIAN_POINT('Ctrl Pts',(-0.00363125913339092,2.42225461287934,
12.3430448442142));
#38389=CARTESIAN_POINT('Ctrl Pts',(-0.00341693525146551,2.42225695666504,
12.3430315102305));
#38390=CARTESIAN_POINT('Ctrl Pts',(-0.00300543908141589,2.42226104611096,
12.3430059329806));
#38391=CARTESIAN_POINT('Ctrl Pts',(-0.00280826898654971,2.42226282461703,
12.3429936879865));
#38392=CARTESIAN_POINT('Ctrl Pts',(-0.00234093621502636,2.42226661110576,
12.3429646895244));
#38393=CARTESIAN_POINT('Ctrl Pts',(-0.00207077286777499,2.42226846031991,
12.3429479451057));
#38394=CARTESIAN_POINT('Ctrl Pts',(-0.00127503832141977,2.42227290629625,
12.3428986829334));
#38395=CARTESIAN_POINT('Ctrl Pts',(-0.000749459525098847,2.42227455713259,
12.3428662181729));
#38396=CARTESIAN_POINT('Ctrl Pts',(0.00326785903834728,2.42227734784248,
12.3426186097039));
#38397=CARTESIAN_POINT('Ctrl Pts',(0.00675957556747228,2.42222302585975,
12.3424065116362));
#38398=CARTESIAN_POINT('Ctrl Pts',(0.0188651441933347,2.42183781586057,
12.3416798627528));
#38399=CARTESIAN_POINT('Ctrl Pts',(0.0274666734445083,2.4212181189898,12.3411787685483));
#38400=CARTESIAN_POINT('Ctrl Pts',(0.0718192360720136,2.41622775382,12.3386274515187));
#38401=CARTESIAN_POINT('Ctrl Pts',(0.106674869151872,2.40623302521987,12.3366996135462));
#38402=CARTESIAN_POINT('Ctrl Pts',(0.139751374585636,2.39039827991158,12.3344977435956));
#38403=CARTESIAN_POINT('Ctrl Pts',(0.140343369906351,2.39011264396422,12.3344582166111));
#38404=CARTESIAN_POINT('Ctrl Pts',(0.143333897636095,2.38865842783097,12.3342579352018));
#38405=CARTESIAN_POINT('Ctrl Pts',(0.145718671783204,2.38746193174845,12.3340962424619));
#38406=CARTESIAN_POINT('Ctrl Pts',(0.148758020935467,2.38588948123213,12.333887515734));
#38407=CARTESIAN_POINT('Ctrl Pts',(0.149426557726388,2.38554062425975,12.333841437929));
#38408=CARTESIAN_POINT('Ctrl Pts',(0.150490887341073,2.38498047256803,12.3337678128664));
#38409=CARTESIAN_POINT('Ctrl Pts',(0.150887476772373,2.38477069067558,12.3337403192061));
#38410=CARTESIAN_POINT('Ctrl Pts',(0.151628943197061,2.38437649719668,12.3336888047028));
#38411=CARTESIAN_POINT('Ctrl Pts',(0.151973925452723,2.38419228447172,12.3336647909542));
#38412=CARTESIAN_POINT('Ctrl Pts',(0.152734150101069,2.38378456159807,12.3336117716826));
#38413=CARTESIAN_POINT('Ctrl Pts',(0.153149238382994,2.38356076736291,12.3335827560863));
#38414=CARTESIAN_POINT('Ctrl Pts',(0.154345502208729,2.38291241058491,12.3334989410395));
#38415=CARTESIAN_POINT('Ctrl Pts',(0.155125409331093,2.38248552789397,12.3334440588869));
#38416=CARTESIAN_POINT('Ctrl Pts',(0.156878872580975,2.38151631726688,12.3333201238913));
#38417=CARTESIAN_POINT('Ctrl Pts',(0.15785139845159,2.38097215788493,12.3332510057651));
#38418=CARTESIAN_POINT('Ctrl Pts',(0.165923145325354,2.3764006226304,12.3326741410611));
#38419=CARTESIAN_POINT('Ctrl Pts',(0.172869272585666,2.3721102524518,12.3321569242951));
#38420=CARTESIAN_POINT('Ctrl Pts',(0.186104822008574,2.36322370498861,12.3311288096778));
#38421=CARTESIAN_POINT('Ctrl Pts',(0.192405396613111,2.3586539627675,12.3306190863669));
#38422=CARTESIAN_POINT('Ctrl Pts',(0.216913149678283,2.33948747143721,12.3285560766956));
#38423=CARTESIAN_POINT('Ctrl Pts',(0.23367538902042,2.32316196148891,12.3269532314582));
#38424=CARTESIAN_POINT('Ctrl Pts',(0.255162546005965,2.29713411745301,12.3247079394858));
#38425=CARTESIAN_POINT('Ctrl Pts',(0.261404353680891,2.28877923655543,12.3240271832591));
#38426=CARTESIAN_POINT('Ctrl Pts',(0.26764303197325,2.27952416771744,12.3233265712654));
#38427=CARTESIAN_POINT('Ctrl Pts',(0.268053097212222,2.2789113089181,12.3232804200175));
#38428=CARTESIAN_POINT('Ctrl Pts',(0.268620131858981,2.27805752737708,12.3232164683218));
#38429=CARTESIAN_POINT('Ctrl Pts',(0.26877888374771,2.27781779986406,12.3231985491066));
#38430=CARTESIAN_POINT('Ctrl Pts',(0.26905161903196,2.27740474896056,12.3231677389522));
#38431=CARTESIAN_POINT('Ctrl Pts',(0.269165755925846,2.27723152793705,12.3231548376485));
#38432=CARTESIAN_POINT('Ctrl Pts',(0.269401736500291,2.27687263585666,12.323128148415));
#38433=CARTESIAN_POINT('Ctrl Pts',(0.269523555304116,2.27668694937862,12.3231143622353));
#38434=CARTESIAN_POINT('Ctrl Pts',(0.269810422084073,2.27624869585435,12.3230818771019));
#38435=CARTESIAN_POINT('Ctrl Pts',(0.269975308030901,2.27599602186112,12.3230631891056));
#38436=CARTESIAN_POINT('Ctrl Pts',(0.27049929600999,2.27519058474166,12.3230037481725));
#38437=CARTESIAN_POINT('Ctrl Pts',(0.270857060027102,2.27463694676547,12.3229630844526));
#38438=CARTESIAN_POINT('Ctrl Pts',(0.275594818122077,2.26725570895044,12.3224234743239));
#38439=CARTESIAN_POINT('Ctrl Pts',(0.279717654045023,2.26026551744576,12.3219411581942));
#38440=CARTESIAN_POINT('Ctrl Pts',(0.287302177045821,2.24621985476806,12.3210122207659));
#38441=CARTESIAN_POINT('Ctrl Pts',(0.29077833374161,2.23917887879653,12.3205652549226));
#38442=CARTESIAN_POINT('Ctrl Pts',(0.304150427732204,2.20940016272012,12.3187240484361));
#38443=CARTESIAN_POINT('Ctrl Pts',(0.311662495319964,2.1856874934315,12.3173667496005));
#38444=CARTESIAN_POINT('Ctrl Pts',(0.318242538080686,2.15175313277524,12.3153552292708));
#38445=CARTESIAN_POINT('Ctrl Pts',(0.31966544401802,2.14207938440594,12.3147753200863));
#38446=CARTESIAN_POINT('Ctrl Pts',(0.320750987375719,2.13132189719268,12.3141178572602));
#38447=CARTESIAN_POINT('Ctrl Pts',(0.320850390211302,2.1302867001808,12.3140544637939));
#38448=CARTESIAN_POINT('Ctrl Pts',(0.320991589559972,2.1287374499988,12.3139593968405));
#38449=CARTESIAN_POINT('Ctrl Pts',(0.321037166119318,2.12822374117423,12.3139278421692));
#38450=CARTESIAN_POINT('Ctrl Pts',(0.321113546448796,2.12733870416159,12.3138734229338));
#38451=CARTESIAN_POINT('Ctrl Pts',(0.321144939784693,2.12696742677662,12.3138505769352));
#38452=CARTESIAN_POINT('Ctrl Pts',(0.321208411436013,2.12620094020098,12.3138033771844));
#38453=CARTESIAN_POINT('Ctrl Pts',(0.32124040439261,2.12580572471652,12.3137790207896));
#38454=CARTESIAN_POINT('Ctrl Pts',(0.321312358587386,2.12489598711545,12.3137229105413));
#38455=CARTESIAN_POINT('Ctrl Pts',(0.321351813382894,2.12438142707116,12.3136911408363));
#38456=CARTESIAN_POINT('Ctrl Pts',(0.321471696455759,2.12276708153775,12.3135913640183));
#38457=CARTESIAN_POINT('Ctrl Pts',(0.321547715459162,2.12166698544912,12.3135232186595));
#38458=CARTESIAN_POINT('Ctrl Pts',(0.321710850975623,2.1191158828462,12.3133648291437));
#38459=CARTESIAN_POINT('Ctrl Pts',(0.321793798738509,2.11766464249429,12.3132744553582));
#38460=CARTESIAN_POINT('Ctrl Pts',(0.322515221507821,2.10334259081287,12.3123798281188));
#38461=CARTESIAN_POINT('Ctrl Pts',(0.322390911846858,2.090446631611,12.3115517077522));
#38462=CARTESIAN_POINT('Ctrl Pts',(0.320181833962088,2.05874934582598,12.3094606026357));
#38463=CARTESIAN_POINT('Ctrl Pts',(0.31721420442595,2.04005787319945,12.3081772277891));
#38464=CARTESIAN_POINT('Ctrl Pts',(0.309706361623461,2.01006766575015,12.3060891857521));
#38465=CARTESIAN_POINT('Ctrl Pts',(0.306134117098912,1.99857119530979,12.3052823131422));
#38466=CARTESIAN_POINT('Ctrl Pts',(0.301550693359492,1.98629197902112,12.3044304182303));
#38467=CARTESIAN_POINT('Ctrl Pts',(0.301169148885928,1.98528522972201,12.3043606502367));
#38468=CARTESIAN_POINT('Ctrl Pts',(0.299224737321257,1.98023124506068,12.3040108613566));
#38469=CARTESIAN_POINT('Ctrl Pts',(0.297585209461193,1.97621370920541,12.3037342692817));
#38470=CARTESIAN_POINT('Ctrl Pts',(0.295627082900686,1.97167945033083,12.3034247713452));
#38471=CARTESIAN_POINT('Ctrl Pts',(0.295387670153801,1.97112928980316,12.3033872639484));
#38472=CARTESIAN_POINT('Ctrl Pts',(0.295031725050041,1.97031754614533,12.3033319934783));
#38473=CARTESIAN_POINT('Ctrl Pts',(0.294916379989371,1.97005544859725,12.3033141585056));
#38474=CARTESIAN_POINT('Ctrl Pts',(0.294711630388784,1.969591874779,12.3032826333765));
#38475=CARTESIAN_POINT('Ctrl Pts',(0.294622368380299,1.969390336264,12.3032689344561));
#38476=CARTESIAN_POINT('Ctrl Pts',(0.294435383065221,1.96896932213148,12.3032403313998));
#38477=CARTESIAN_POINT('Ctrl Pts',(0.294337621315708,1.96874986467602,12.3032254297132));
#38478=CARTESIAN_POINT('Ctrl Pts',(0.294081105505361,1.96817576100857,12.30318646691));
#38479=CARTESIAN_POINT('Ctrl Pts',(0.293921954705788,1.96782129087247,12.3031624302255));
#38480=CARTESIAN_POINT('Ctrl Pts',(0.293266573671614,1.96636862394841,12.3030640041036));
#38481=CARTESIAN_POINT('Ctrl Pts',(0.292764818389349,1.9652729087392,12.3029899499804));
#38482=CARTESIAN_POINT('Ctrl Pts',(0.289433497539623,1.95810458546837,12.302506539083));
#38483=CARTESIAN_POINT('Ctrl Pts',(0.286421083364148,1.95211816935647,12.3021078400876));
#38484=CARTESIAN_POINT('Ctrl Pts',(0.279790509090775,1.93990556451551,12.3012961121901));
#38485=CARTESIAN_POINT('Ctrl Pts',(0.276146000741318,1.93369800260942,12.3008844282648));
#38486=CARTESIAN_POINT('Ctrl Pts',(0.261866043913477,1.91114130508282,12.2993730652622));
#38487=CARTESIAN_POINT('Ctrl Pts',(0.249961758877574,1.89564596255504,12.2983012611015));
#38488=CARTESIAN_POINT('Ctrl Pts',(0.233222372681876,1.87752479522032,12.2968987906593));
#38489=CARTESIAN_POINT('Ctrl Pts',(0.229624393963316,1.87381307177378,12.2966027559472));
#38490=CARTESIAN_POINT('Ctrl Pts',(0.223433738157265,1.86772670962211,12.2961004177346));
#38491=CARTESIAN_POINT('Ctrl Pts',(0.220888623953633,1.86530502480585,12.295895783679));
#38492=CARTESIAN_POINT('Ctrl Pts',(0.216994154326212,1.86171889403754,12.2955850208604));
#38493=CARTESIAN_POINT('Ctrl Pts',(0.215673855374263,1.86052320277745,12.295480064171));
#38494=CARTESIAN_POINT('Ctrl Pts',(0.214035704254371,1.85906419304752,12.2953502850332));
#38495=CARTESIAN_POINT('Ctrl Pts',(0.213727153566522,1.85879044464686,12.2953258599934));
#38496=CARTESIAN_POINT('Ctrl Pts',(0.213165611263555,1.85829416365103,12.2952814422058));
#38497=CARTESIAN_POINT('Ctrl Pts',(0.212912794274646,1.85807143371757,12.295261457017));
#38498=CARTESIAN_POINT('Ctrl Pts',(0.208572337142748,1.85425959569122,12.294918554917));
#38499=CARTESIAN_POINT('Ctrl Pts',(0.204395021423741,1.85077432725717,12.2945917241251));
#38500=CARTESIAN_POINT('Ctrl Pts',(0.199441583216768,1.84684983567982,12.2942069347975));
#38501=CARTESIAN_POINT('Ctrl Pts',(0.198749245222525,1.84630591589338,12.2941532147827));
#38502=CARTESIAN_POINT('Ctrl Pts',(0.197643333775411,1.84544438692515,12.2940674986986));
#38503=CARTESIAN_POINT('Ctrl Pts',(0.197231199929601,1.84512493000873,12.2940355760091));
#38504=CARTESIAN_POINT('Ctrl Pts',(0.196503813049271,1.84456393205277,12.2939792701984));
#38505=CARTESIAN_POINT('Ctrl Pts',(0.196188884664472,1.84432197027684,12.293954903771));
#38506=CARTESIAN_POINT('Ctrl Pts',(0.195538136832002,1.84382390620373,12.2939045781487));
#38507=CARTESIAN_POINT('Ctrl Pts',(0.195202259756554,1.84356788077216,12.2938786159918));
#38508=CARTESIAN_POINT('Ctrl Pts',(0.194354123655839,1.84292401303357,12.2938130898862));
#38509=CARTESIAN_POINT('Ctrl Pts',(0.193841207944696,1.8425370423735,12.293773491825));
#38510=CARTESIAN_POINT('Ctrl Pts',(0.19180392251793,1.84100954565989,12.2936163222143));
#38511=CARTESIAN_POINT('Ctrl Pts',(0.190270640570015,1.83988102103127,12.2934982834932));
#38512=CARTESIAN_POINT('Ctrl Pts',(0.186397567777461,1.8370829330404,12.293200694271));
#38513=CARTESIAN_POINT('Ctrl Pts',(0.184045308669641,1.83543099034943,12.2930204769172));
#38514=CARTESIAN_POINT('Ctrl Pts',(0.174556488715929,1.82895497121465,12.2922953860837));
#38515=CARTESIAN_POINT('Ctrl Pts',(0.167250415221558,1.8243867710029,12.2917411705884));
#38516=CARTESIAN_POINT('Ctrl Pts',(0.146200563886629,1.8123705051892,12.2901557531709));
#38517=CARTESIAN_POINT('Ctrl Pts',(0.132086239725396,1.80562188765775,12.2891046297023));
#38518=CARTESIAN_POINT('Ctrl Pts',(0.10041966889317,1.79321811506809,12.2868036894158));
#38519=CARTESIAN_POINT('Ctrl Pts',(0.0827559233496249,1.7879891000378,12.2855554124849));
#38520=CARTESIAN_POINT('Ctrl Pts',(0.0607357642610242,1.78347344068038,
12.2841057500113));
#38521=CARTESIAN_POINT('Ctrl Pts',(0.0567145821016261,1.78272826178682,
12.2838453439549));
#38522=CARTESIAN_POINT('Ctrl Pts',(0.0521491910143933,1.7819718140105,12.2835553937908));
#38523=CARTESIAN_POINT('Ctrl Pts',(0.0516180766465092,1.78188517893618,
12.2835217494151));
#38524=CARTESIAN_POINT('Ctrl Pts',(0.0508136401664482,1.78175602738491,
12.2834709251376));
#38525=CARTESIAN_POINT('Ctrl Pts',(0.0505404794985263,1.78171253234494,
12.2834536902561));
#38526=CARTESIAN_POINT('Ctrl Pts',(0.0500651520789352,1.78163747387719,
12.2834237409152));
#38527=CARTESIAN_POINT('Ctrl Pts',(0.049863011192974,1.78160575129675,12.2834110173884));
#38528=CARTESIAN_POINT('Ctrl Pts',(0.0494392676495891,1.78153966537809,
12.2833843726261));
#38529=CARTESIAN_POINT('Ctrl Pts',(0.0492176593973558,1.78150534083437,
12.2833704536787));
#38530=CARTESIAN_POINT('Ctrl Pts',(0.0486859051418298,1.78142354652447,
12.2833370920217));
#38531=CARTESIAN_POINT('Ctrl Pts',(0.0483757241973754,1.78137629815266,
12.283317661956));
#38532=CARTESIAN_POINT('Ctrl Pts',(0.0477189829142257,1.78127724103635,
12.283276586237));
#38533=CARTESIAN_POINT('Ctrl Pts',(0.0473724057203805,1.7812255443252,12.2832549469167));
#38534=CARTESIAN_POINT('Ctrl Pts',(0.0444003026821778,1.78078716873952,
12.283069691129));
#38535=CARTESIAN_POINT('Ctrl Pts',(0.041770077282181,1.78043235417886,12.2829078458918));
#38536=CARTESIAN_POINT('Ctrl Pts',(0.0298089336753,1.77896901543558,12.2821801443013));
#38537=CARTESIAN_POINT('Ctrl Pts',(0.020435847663643,1.7782363056478,12.2816327291349));
#38538=CARTESIAN_POINT('Ctrl Pts',(-0.00712414928507726,1.77729135873321,
12.280055637314));
#38539=CARTESIAN_POINT('Ctrl Pts',(-0.0253123740940854,1.77820664955439,
12.2790546045622));
#38540=CARTESIAN_POINT('Ctrl Pts',(-0.0634717890011353,1.78338384563155,
12.2768876884808));
#38541=CARTESIAN_POINT('Ctrl Pts',(-0.0833095118123769,1.78801635332981,
12.2757197626134));
#38542=CARTESIAN_POINT('Ctrl Pts',(-0.103807366950076,1.79489855778915,
12.2744064894633));
#38543=CARTESIAN_POINT('Ctrl Pts',(-0.105034992433163,1.79531900328397,
12.274327434013));
#38544=CARTESIAN_POINT('Ctrl Pts',(-0.106742880670442,1.79591548110399,
12.2742168769918));
#38545=CARTESIAN_POINT('Ctrl Pts',(-0.107225325634724,1.79608526402327,
12.2741855827038));
#38546=CARTESIAN_POINT('Ctrl Pts',(-0.108057480004907,1.79638034543847,
12.274131492634));
#38547=CARTESIAN_POINT('Ctrl Pts',(-0.108407381708901,1.79650510183823,
12.2741087148992));
#38548=CARTESIAN_POINT('Ctrl Pts',(-0.109130919859783,1.79676448808675,
12.2740615433948));
#38549=CARTESIAN_POINT('Ctrl Pts',(-0.109504524570909,1.79689920413989,
12.2740371467862));
#38550=CARTESIAN_POINT('Ctrl Pts',(-0.110244172821911,1.79716745583784,
12.2739887691711));
#38551=CARTESIAN_POINT('Ctrl Pts',(-0.110610225120833,1.79730096541035,
12.2739647890702));
#38552=CARTESIAN_POINT('Ctrl Pts',(-0.11145779460694,1.79761184056866,12.2739091762592));
#38553=CARTESIAN_POINT('Ctrl Pts',(-0.111939131127701,1.79778969266352,
12.2738775273313));
#38554=CARTESIAN_POINT('Ctrl Pts',(-0.114568944040615,1.79876854373663,
12.2737042464412));
#38555=CARTESIAN_POINT('Ctrl Pts',(-0.11670920590725,1.79959128840738,12.2735618881268));
#38556=CARTESIAN_POINT('Ctrl Pts',(-0.122232166625808,1.80178231578794,
12.2731909846474));
#38557=CARTESIAN_POINT('Ctrl Pts',(-0.125600656724107,1.80318530526818,
12.2729612843199));
#38558=CARTESIAN_POINT('Ctrl Pts',(-0.139059090113749,1.80906091828334,
12.2720291402559));
#38559=CARTESIAN_POINT('Ctrl Pts',(-0.148939151080029,1.81399289355591,
12.271311505751));
#38560=CARTESIAN_POINT('Ctrl Pts',(-0.166247880318986,1.8237735026707,12.2699949973283));
#38561=CARTESIAN_POINT('Ctrl Pts',(-0.173766948893,1.8284406711377,12.2694014357622));
#38562=CARTESIAN_POINT('Ctrl Pts',(-0.201371345133162,1.84719132991211,
12.2671491173728));
#38563=CARTESIAN_POINT('Ctrl Pts',(-0.220020846834212,1.86324341739304,
12.265468116185));
#38564=CARTESIAN_POINT('Ctrl Pts',(-0.237601176571995,1.882264520404,12.2638318294844));
#38565=CARTESIAN_POINT('Ctrl Pts',(-0.238526035780492,1.88327808463892,
12.263745596696));
#38566=CARTESIAN_POINT('Ctrl Pts',(-0.239720194637914,1.88460368229058,
12.2636340925793));
#38567=CARTESIAN_POINT('Ctrl Pts',(-0.239995390756795,1.88491034934239,
12.2636083849277));
#38568=CARTESIAN_POINT('Ctrl Pts',(-0.240417286702995,1.88538231032765,
12.2635689569453));
#38569=CARTESIAN_POINT('Ctrl Pts',(-0.240564404610092,1.88554722734081,
12.2635552050967));
#38570=CARTESIAN_POINT('Ctrl Pts',(-0.240856286568796,1.88587510103593,
12.2635279155951));
#38571=CARTESIAN_POINT('Ctrl Pts',(-0.241001054010817,1.88603805220957,
12.2635143777422));
#38572=CARTESIAN_POINT('Ctrl Pts',(-0.241323580563573,1.88640183282966,
12.2634842104317));
#38573=CARTESIAN_POINT('Ctrl Pts',(-0.241501253893264,1.88660273684092,
12.2634675874784));
#38574=CARTESIAN_POINT('Ctrl Pts',(-0.242020126930007,1.88719093018711,
12.2634190285126));
#38575=CARTESIAN_POINT('Ctrl Pts',(-0.242360649297349,1.8875788199949,12.2633871432225));
#38576=CARTESIAN_POINT('Ctrl Pts',(-0.244797174068739,1.89036775674494,
12.2631588567562));
#38577=CARTESIAN_POINT('Ctrl Pts',(-0.246858481669566,1.89279906918405,
12.2629649846397));
#38578=CARTESIAN_POINT('Ctrl Pts',(-0.25804471650477,1.90639718441898,12.2619061468094));
#38579=CARTESIAN_POINT('Ctrl Pts',(-0.266449291991257,1.91813741883173,
12.2610848142352));
#38580=CARTESIAN_POINT('Ctrl Pts',(-0.276856558504016,1.93495373522362,
12.2599729298432));
#38581=CARTESIAN_POINT('Ctrl Pts',(-0.279559457379286,1.93957452076478,
12.2596736637416));
#38582=CARTESIAN_POINT('Ctrl Pts',(-0.284878868591628,1.94921145279089,
12.2590583792889));
#38583=CARTESIAN_POINT('Ctrl Pts',(-0.287480892726333,1.95423343546623,
12.2587424775959));
#38584=CARTESIAN_POINT('Ctrl Pts',(-0.2917277738155,1.96298657431101,12.2581965109031));
#38585=CARTESIAN_POINT('Ctrl Pts',(-0.293436447127396,1.96668524663971,
12.2579671965251));
#38586=CARTESIAN_POINT('Ctrl Pts',(-0.302247550410876,1.98674881454398,
12.2567271385163));
#38587=CARTESIAN_POINT('Ctrl Pts',(-0.308051008610819,2.00364727176851,
12.2556940009228));
#38588=CARTESIAN_POINT('Ctrl Pts',(-0.3127407994431,2.02217963188986,12.2545327916796));
#38589=CARTESIAN_POINT('Ctrl Pts',(-0.313047719423597,2.02342361578632,
12.2544547259284));
#38590=CARTESIAN_POINT('Ctrl Pts',(-0.313466110480629,2.02516396619935,
12.2543453332399));
#38591=CARTESIAN_POINT('Ctrl Pts',(-0.313583839660738,2.02565882786899,
12.254314207863));
#38592=CARTESIAN_POINT('Ctrl Pts',(-0.313785350715879,2.02651485347623,
12.2542603309783));
#38593=CARTESIAN_POINT('Ctrl Pts',(-0.313869682102774,2.02687588811926,
12.2542375971832));
#38594=CARTESIAN_POINT('Ctrl Pts',(-0.314043158577843,2.02762439459965,
12.2541904420627));
#38595=CARTESIAN_POINT('Ctrl Pts',(-0.314132209969285,2.0280118873409,12.2541660177685));
#38596=CARTESIAN_POINT('Ctrl Pts',(-0.314307294999275,2.02878025272953,
12.2541175609856));
#38597=CARTESIAN_POINT('Ctrl Pts',(-0.314393353965068,2.02916111892832,
12.2540935293596));
#38598=CARTESIAN_POINT('Ctrl Pts',(-0.314591414144997,2.03004513259632,
12.2540377213459));
#38599=CARTESIAN_POINT('Ctrl Pts',(-0.314702900589451,2.03054839323059,
12.2540059284872));
#38600=CARTESIAN_POINT('Ctrl Pts',(-0.314988697414981,2.03185332591277,
12.253923433308));
#38601=CARTESIAN_POINT('Ctrl Pts',(-0.315161154041282,2.03265539626854,
12.2538726716854));
#38602=CARTESIAN_POINT('Ctrl Pts',(-0.319969153789331,2.05543967834303,
12.252429054407));
#38603=CARTESIAN_POINT('Ctrl Pts',(-0.322295489667893,2.07784050634339,
12.2509596929231));
#38604=CARTESIAN_POINT('Ctrl Pts',(-0.322274864054643,2.10029601277207,
12.2494497673494));
#38605=CARTESIAN_POINT('',(-0.322274852789156,2.09973668262869,11.999512253058));
#38606=CARTESIAN_POINT('Ctrl Pts',(-0.322274864232108,2.10029581950008,
12.2494497803451));
#38607=CARTESIAN_POINT('Ctrl Pts',(-0.322250804242316,2.12650751258178,
12.2476872860856));
#38608=CARTESIAN_POINT('Ctrl Pts',(-0.319029134840591,2.15262041363499,
12.2458804051903));
#38609=CARTESIAN_POINT('Ctrl Pts',(-0.312335749251866,2.17943278422205,
12.2441234271947));
#38610=CARTESIAN_POINT('Ctrl Pts',(-0.311983118138568,2.18080669301348,
12.244033702601));
#38611=CARTESIAN_POINT('Ctrl Pts',(-0.311456902473738,2.18280211221575,
12.2439038798979));
#38612=CARTESIAN_POINT('Ctrl Pts',(-0.311290509892046,2.18342547784592,
12.2438633933506));
#38613=CARTESIAN_POINT('Ctrl Pts',(-0.310988428232003,2.18454369526298,
12.2437908977568));
#38614=CARTESIAN_POINT('Ctrl Pts',(-0.310853427789059,2.18503872849104,
12.2437588501594));
#38615=CARTESIAN_POINT('Ctrl Pts',(-0.310646233430755,2.18579140322462,
12.2437101957219));
#38616=CARTESIAN_POINT('Ctrl Pts',(-0.310574900793226,2.18604927780341,
12.2436935391326));
#38617=CARTESIAN_POINT('Ctrl Pts',(-0.310444881871579,2.18651704133597,
12.2436633493241));
#38618=CARTESIAN_POINT('Ctrl Pts',(-0.310386304035035,2.18672695884262,
12.2436498098575));
#38619=CARTESIAN_POINT('Ctrl Pts',(-0.310267791099378,2.18714999967907,
12.2436225418471));
#38620=CARTESIAN_POINT('Ctrl Pts',(-0.310207849597125,2.18736311971762,
12.2436088137578));
#38621=CARTESIAN_POINT('Ctrl Pts',(-0.310035195816046,2.18797456648244,
12.2435694529774));
#38622=CARTESIAN_POINT('Ctrl Pts',(-0.309921935076539,2.18837273988864,
12.2435438523035));
#38623=CARTESIAN_POINT('Ctrl Pts',(-0.309425415538343,2.19010558287245,
12.243432569365));
#38624=CARTESIAN_POINT('Ctrl Pts',(-0.309034292726241,2.19143801139799,
12.2433473389029));
#38625=CARTESIAN_POINT('Ctrl Pts',(-0.300978091751989,2.21824062416167,
12.2416389227375));
#38626=CARTESIAN_POINT('Ctrl Pts',(-0.290196131766033,2.24267227207735,
12.2401863497874));
#38627=CARTESIAN_POINT('Ctrl Pts',(-0.272379716501707,2.27244079019132,
12.2382417670585));
#38628=CARTESIAN_POINT('Ctrl Pts',(-0.267968456496069,2.27921895814117,
12.2377863219828));
#38629=CARTESIAN_POINT('Ctrl Pts',(-0.255609014495846,2.29673193404628,
12.2365620763112));
#38630=CARTESIAN_POINT('Ctrl Pts',(-0.247241377281068,2.30714984607449,
12.2357831466496));
#38631=CARTESIAN_POINT('Ctrl Pts',(-0.236703618400437,2.31871868643102,
12.2348384449069));
#38632=CARTESIAN_POINT('Ctrl Pts',(-0.235136515747221,2.32040255283496,
12.234698832962));
#38633=CARTESIAN_POINT('Ctrl Pts',(-0.233197724706082,2.32244158893129,
12.2345271102168));
#38634=CARTESIAN_POINT('Ctrl Pts',(-0.232843009565415,2.32281286360105,
12.2344957327835));
#38635=CARTESIAN_POINT('Ctrl Pts',(-0.232217490047426,2.32346445993949,
12.2344404706035));
#38636=CARTESIAN_POINT('Ctrl Pts',(-0.231947060957858,2.32374514173693,
12.2344166021647));
#38637=CARTESIAN_POINT('Ctrl Pts',(-0.231400004059731,2.32431088142892,
12.2343683639391));
#38638=CARTESIAN_POINT('Ctrl Pts',(-0.231123357125802,2.32459591980906,
12.2343439933396));
#38639=CARTESIAN_POINT('Ctrl Pts',(-0.230587046640819,2.32514645780451,
12.2342967932374));
#38640=CARTESIAN_POINT('Ctrl Pts',(-0.23032744961418,2.3254120216246,12.2342739666683));
#38641=CARTESIAN_POINT('Ctrl Pts',(-0.229709536040932,2.32604195591522,
12.2342196807777));
#38642=CARTESIAN_POINT('Ctrl Pts',(-0.229350811508963,2.32640592315021,
12.2341882035323));
#38643=CARTESIAN_POINT('Ctrl Pts',(-0.228079868694,2.32768932038622,12.2340768137432));
#38644=CARTESIAN_POINT('Ctrl Pts',(-0.22716298434059,2.32860409355114,12.2339966950039));
#38645=CARTESIAN_POINT('Ctrl Pts',(-0.212148286912016,2.34340469295182,
12.2326884795065));
#38646=CARTESIAN_POINT('Ctrl Pts',(-0.196809271708206,2.3559659932542,12.2314019909232));
#38647=CARTESIAN_POINT('Ctrl Pts',(-0.173047426057694,2.37202002073897,
12.2294834996321));
#38648=CARTESIAN_POINT('Ctrl Pts',(-0.16547382187034,2.37669244426367,12.2288823993777));
#38649=CARTESIAN_POINT('Ctrl Pts',(-0.150621434502374,2.38502729611989,
12.227729892546));
#38650=CARTESIAN_POINT('Ctrl Pts',(-0.143377607654854,2.38873905573101,
12.2271790412801));
#38651=CARTESIAN_POINT('Ctrl Pts',(-0.127034843866261,2.39634630763618,
12.2259696778447));
#38652=CARTESIAN_POINT('Ctrl Pts',(-0.117880532467543,2.40010531447949,
12.2253141148235));
#38653=CARTESIAN_POINT('Ctrl Pts',(-0.106203351810587,2.40428329927523,
12.2245163542929));
#38654=CARTESIAN_POINT('Ctrl Pts',(-0.103829724148162,2.40510140513925,
12.2243561447867));
#38655=CARTESIAN_POINT('Ctrl Pts',(-0.100040925568022,2.40635793181671,
12.2241037752353));
#38656=CARTESIAN_POINT('Ctrl Pts',(-0.0986319240098715,2.40681446012524,
12.2240106546567));
#38657=CARTESIAN_POINT('Ctrl Pts',(-0.0968297941768319,2.40738466765821,
12.223892529625));
#38658=CARTESIAN_POINT('Ctrl Pts',(-0.0964395577434483,2.40750732456046,
12.2238670089029));
#38659=CARTESIAN_POINT('Ctrl Pts',(-0.0958153736175292,2.40770220953033,
12.2238262827595));
#38660=CARTESIAN_POINT('Ctrl Pts',(-0.0955815769472646,2.40777491405335,
12.2238110493515));
#38661=CARTESIAN_POINT('Ctrl Pts',(-0.0951382946752794,2.40791220918779,
12.2237822068922));
#38662=CARTESIAN_POINT('Ctrl Pts',(-0.0949288277662168,2.40797685195456,
12.2237685948769));
#38663=CARTESIAN_POINT('Ctrl Pts',(-0.0944495052593821,2.40812423833353,
12.2237374854126));
#38664=CARTESIAN_POINT('Ctrl Pts',(-0.0941796072273278,2.40820684106023,
12.2237199963553));
#38665=CARTESIAN_POINT('Ctrl Pts',(-0.0933498478083672,2.40845959854538,
12.2236663144005));
#38666=CARTESIAN_POINT('Ctrl Pts',(-0.0927896272933311,2.40862858438597,
12.2236301899016));
#38667=CARTESIAN_POINT('Ctrl Pts',(-0.0885802610561344,2.40988580710984,
12.223359633033));
#38668=CARTESIAN_POINT('Ctrl Pts',(-0.0849123539528292,2.41091087362385,
12.2231288051788));
#38669=CARTESIAN_POINT('Ctrl Pts',(-0.0801491223111135,2.4121514605577,
12.2228343566469));
#38670=CARTESIAN_POINT('Ctrl Pts',(-0.0790698348165592,2.41242659525752,
12.2227679881324));
#38671=CARTESIAN_POINT('Ctrl Pts',(-0.0590812300213608,2.41741192670176,
12.2215449267224));
#38672=CARTESIAN_POINT('Ctrl Pts',(-0.0397823280552906,2.42040359528464,
12.2204630903205));
#38673=CARTESIAN_POINT('Ctrl Pts',(-0.00804815058294582,2.42240942696339,
12.2186855301368));
#38674=CARTESIAN_POINT('Ctrl Pts',(0.0042672199520332,2.42248159880663,
12.2179963541319));
#38675=CARTESIAN_POINT('Ctrl Pts',(0.0261215335935303,2.42135740472693,
12.2167425664218));
#38676=CARTESIAN_POINT('Ctrl Pts',(0.035659595430544,2.42043920724829,12.2161849462941));
#38677=CARTESIAN_POINT('Ctrl Pts',(0.0498771597140101,2.4184278795096,12.2153294109509));
#38678=CARTESIAN_POINT('Ctrl Pts',(0.0545965565166873,2.41765273148977,
12.2150413906576));
#38679=CARTESIAN_POINT('Ctrl Pts',(0.0601296352072875,2.41661699346929,
12.214698382625));
#38680=CARTESIAN_POINT('Ctrl Pts',(0.060961869112126,2.41645780773511,12.2146466482518));
#38681=CARTESIAN_POINT('Ctrl Pts',(0.0621766979386902,2.41622047108946,
12.2145709193467));
#38682=CARTESIAN_POINT('Ctrl Pts',(0.0625597987679584,2.4161449029774,12.2145470072282));
#38683=CARTESIAN_POINT('Ctrl Pts',(0.063332705772376,2.41599098419503,12.2144987020316));
#38684=CARTESIAN_POINT('Ctrl Pts',(0.0637225061250163,2.41591260804826,
12.2144743081783));
#38685=CARTESIAN_POINT('Ctrl Pts',(0.064475490071809,2.4157597571795,12.2144271237479));
#38686=CARTESIAN_POINT('Ctrl Pts',(0.0648386923591865,2.41568537667339,
12.214404336217));
#38687=CARTESIAN_POINT('Ctrl Pts',(0.0656998717638844,2.41550746611676,
12.2143502382763));
#38688=CARTESIAN_POINT('Ctrl Pts',(0.066197732608585,2.41540338380866,12.2143189102327));
#38689=CARTESIAN_POINT('Ctrl Pts',(0.0679486142395856,2.41503301798155,
12.2142085468187));
#38690=CARTESIAN_POINT('Ctrl Pts',(0.0692002792039081,2.41476044522338,
12.2141293102095));
#38691=CARTESIAN_POINT('Ctrl Pts',(0.087828832837606,2.41058725486211,12.212944868522));
#38692=CARTESIAN_POINT('Ctrl Pts',(0.104851695093844,2.40526099663527,12.2117928196736));
#38693=CARTESIAN_POINT('Ctrl Pts',(0.139086622981571,2.39134659077768,12.209332885756));
#38694=CARTESIAN_POINT('Ctrl Pts',(0.156149579701987,2.3825688798747,12.2080244026759));
#38695=CARTESIAN_POINT('Ctrl Pts',(0.180610036853933,2.36709021070331,12.2060829640449));
#38696=CARTESIAN_POINT('Ctrl Pts',(0.188646652213701,2.36147588809568,12.2054337561444));
#38697=CARTESIAN_POINT('Ctrl Pts',(0.199386534870449,2.35321972326171,12.2045624920863));
#38698=CARTESIAN_POINT('Ctrl Pts',(0.202317611698718,2.35088404803902,12.2043243265548));
#38699=CARTESIAN_POINT('Ctrl Pts',(0.205621469516025,2.34815574792004,12.2040560681335));
#38700=CARTESIAN_POINT('Ctrl Pts',(0.206034653917612,2.34781280303211,12.2040225230517));
#38701=CARTESIAN_POINT('Ctrl Pts',(0.206656251727172,2.34729424481476,12.2039720656141));
#38702=CARTESIAN_POINT('Ctrl Pts',(0.206865300057859,2.3471193993391,12.2039550977502));
#38703=CARTESIAN_POINT('Ctrl Pts',(0.207225435419358,2.34681740929815,12.2039258693378));
#38704=CARTESIAN_POINT('Ctrl Pts',(0.207376627210429,2.34669039118906,12.2039135995398));
#38705=CARTESIAN_POINT('Ctrl Pts',(0.207690843875046,2.34642592084633,12.2038881014997));
#38706=CARTESIAN_POINT('Ctrl Pts',(0.207853848592266,2.34628844617744,12.2038748750081));
#38707=CARTESIAN_POINT('Ctrl Pts',(0.20830198834681,2.34590973297768,12.2038385145462));
#38708=CARTESIAN_POINT('Ctrl Pts',(0.208586841799942,2.34566815942173,12.2038154052217));
#38709=CARTESIAN_POINT('Ctrl Pts',(0.209688630620329,2.34473047574918,12.2037260277778));
#38710=CARTESIAN_POINT('Ctrl Pts',(0.210502518383633,2.34403077142529,12.2036600208582));
#38711=CARTESIAN_POINT('Ctrl Pts',(0.225125678314963,2.33133155420441,12.2024740383108));
#38712=CARTESIAN_POINT('Ctrl Pts',(0.237894279003523,2.31817970358389,12.2014370338216));
#38713=CARTESIAN_POINT('Ctrl Pts',(0.259096788216579,2.29225206439306,12.1995588905049));
#38714=CARTESIAN_POINT('Ctrl Pts',(0.267870622983788,2.27982580697308,12.1987166418511));
#38715=CARTESIAN_POINT('Ctrl Pts',(0.280867591647279,2.25834416493337,12.1972895732924));
#38716=CARTESIAN_POINT('Ctrl Pts',(0.28560546553727,2.24962945234911,12.196718004842));
#38717=CARTESIAN_POINT('Ctrl Pts',(0.292792061107095,2.2348214985129,12.1957469240929));
#38718=CARTESIAN_POINT('Ctrl Pts',(0.295469947551666,2.22884691841445,12.1953552084476));
#38719=CARTESIAN_POINT('Ctrl Pts',(0.298388592006374,2.22176479766612,12.1948893996792));
#38720=CARTESIAN_POINT('Ctrl Pts',(0.298807902691788,2.22073216236912,12.1948214458469));
#38721=CARTESIAN_POINT('Ctrl Pts',(0.299419525000876,2.21920321703179,12.1947207729682));
#38722=CARTESIAN_POINT('Ctrl Pts',(0.2996159801839,2.21870856462594,12.1946881937081));
#38723=CARTESIAN_POINT('Ctrl Pts',(0.29995766127044,2.21784199794879,12.1946311023845));
#38724=CARTESIAN_POINT('Ctrl Pts',(0.300103423458345,2.217470295231,12.1946066084267));
#38725=CARTESIAN_POINT('Ctrl Pts',(0.300382326988072,2.21675516659423,12.1945594731608));
#38726=CARTESIAN_POINT('Ctrl Pts',(0.300515571129466,2.21641178119159,12.1945368353513));
#38727=CARTESIAN_POINT('Ctrl Pts',(0.300828033805284,2.21560241761011,12.1944834662569));
#38728=CARTESIAN_POINT('Ctrl Pts',(0.301006758400135,2.21513625090918,12.1944527184548));
#38729=CARTESIAN_POINT('Ctrl Pts',(0.301531338127078,2.21375842165901,12.1943618109359));
#38730=CARTESIAN_POINT('Ctrl Pts',(0.301874137554118,2.21284560874719,12.1943015490802));
#38731=CARTESIAN_POINT('Ctrl Pts',(0.304877158035974,2.20473749695399,12.193765932672));
#38732=CARTESIAN_POINT('Ctrl Pts',(0.307283622332338,2.19745144409209,12.1932821808523));
#38733=CARTESIAN_POINT('Ctrl Pts',(0.310853718739578,2.1851889937031,12.1924630099013));
#38734=CARTESIAN_POINT('Ctrl Pts',(0.312163153298217,2.18025808638123,12.1921323142605));
#38735=CARTESIAN_POINT('Ctrl Pts',(0.313439924575449,2.17494479002986,12.1917746960576));
#38736=CARTESIAN_POINT('Ctrl Pts',(0.313524292624309,2.17459105712778,12.1917508816788));
#38737=CARTESIAN_POINT('Ctrl Pts',(0.318895616440199,2.15190040026306,12.1902229019562));
#38738=CARTESIAN_POINT('Ctrl Pts',(0.321781203752501,2.12906404462975,12.1886549049665));
#38739=CARTESIAN_POINT('Ctrl Pts',(0.32242591360832,2.09511207005607,12.1863712952104));
#38740=CARTESIAN_POINT('Ctrl Pts',(0.322070845718145,2.08410105736389,12.1856393320636));
#38741=CARTESIAN_POINT('Ctrl Pts',(0.32089073715439,2.06999684966461,12.1847290903559));
#38742=CARTESIAN_POINT('Ctrl Pts',(0.320582857158575,2.0668686300036,12.1845289620307));
#38743=CARTESIAN_POINT('Ctrl Pts',(0.320123001118662,2.06280683191284,12.1842718267559));
#38744=CARTESIAN_POINT('Ctrl Pts',(0.3200126285265,2.06186884169009,12.1842126356778));
#38745=CARTESIAN_POINT('Ctrl Pts',(0.319856098208919,2.0605871557641,12.1841320272075));
#38746=CARTESIAN_POINT('Ctrl Pts',(0.319813508291047,2.06024304124477,12.1841104117294));
#38747=CARTESIAN_POINT('Ctrl Pts',(0.319741618123637,2.059669780189,12.1840744478115));
#38748=CARTESIAN_POINT('Ctrl Pts',(0.319712626839636,2.05944059627617,12.1840600818874));
#38749=CARTESIAN_POINT('Ctrl Pts',(0.31965524333122,2.05899084870637,12.184031914366));
#38750=CARTESIAN_POINT('Ctrl Pts',(0.319626869241094,2.05877028330721,12.1840181117807));
#38751=CARTESIAN_POINT('Ctrl Pts',(0.319563971740581,2.05828531806241,12.1839877881367));
#38752=CARTESIAN_POINT('Ctrl Pts',(0.319529348372247,2.0580209307658,12.183971272759));
#38753=CARTESIAN_POINT('Ctrl Pts',(0.319408122027109,2.0571040745269,12.1839140547224));
#38754=CARTESIAN_POINT('Ctrl Pts',(0.319319847631485,2.05645182247572,12.183873446173));
#38755=CARTESIAN_POINT('Ctrl Pts',(0.318432441939038,2.05004265714018,12.1834753257096));
#38756=CARTESIAN_POINT('Ctrl Pts',(0.317479650560253,2.04430764891223,12.1831262818762));
#38757=CARTESIAN_POINT('Ctrl Pts',(0.316309290210392,2.03827709090472,12.1827639166509));
#38758=CARTESIAN_POINT('Ctrl Pts',(0.316245905530741,2.03795314820902,12.1827444658467));
#38759=CARTESIAN_POINT('Ctrl Pts',(0.314836485356429,2.03080823339121,12.1823157616421));
#38760=CARTESIAN_POINT('Ctrl Pts',(0.313270491373051,2.02403209002309,12.1819152944566));
#38761=CARTESIAN_POINT('Ctrl Pts',(0.306311920104847,1.99781923183642,12.1803720175568));
#38762=CARTESIAN_POINT('Ctrl Pts',(0.299319123247003,1.97885541356391,12.1792656071151));
#38763=CARTESIAN_POINT('Ctrl Pts',(0.2838720343976,1.94663774137063,12.1772394782223));
#38764=CARTESIAN_POINT('Ctrl Pts',(0.276138037124895,1.93311379908045,12.176338122323));
#38765=CARTESIAN_POINT('Ctrl Pts',(0.266090193366134,1.91816711402503,12.1752518150215));
#38766=CARTESIAN_POINT('Ctrl Pts',(0.264698893619078,1.91614765535498,12.1751030522891));
#38767=CARTESIAN_POINT('Ctrl Pts',(0.262877421778093,1.91356734319342,12.1749103155457));
#38768=CARTESIAN_POINT('Ctrl Pts',(0.262468239007734,1.91299171701678,12.1748671465374));
#38769=CARTESIAN_POINT('Ctrl Pts',(0.261802911860804,1.91206223960147,12.1747971586335));
#38770=CARTESIAN_POINT('Ctrl Pts',(0.261547932810234,1.91170755383678,12.1747703846795));
#38771=CARTESIAN_POINT('Ctrl Pts',(0.261062328387458,1.9110349487793,12.1747194846121));
#38772=CARTESIAN_POINT('Ctrl Pts',(0.260831841235791,1.9107169302835,12.1746953638743));
#38773=CARTESIAN_POINT('Ctrl Pts',(0.260306970437709,1.90999551015389,12.1746405222584));
#38774=CARTESIAN_POINT('Ctrl Pts',(0.260012229837511,1.90959237055573,12.1746097875637));
#38775=CARTESIAN_POINT('Ctrl Pts',(0.259136874365433,1.90840090149541,12.1745186885712));
#38776=CARTESIAN_POINT('Ctrl Pts',(0.258553606675946,1.9076145362959,12.1744582210376));
#38777=CARTESIAN_POINT('Ctrl Pts',(0.254563678343172,1.90228620662541,12.1740461449688));
#38778=CARTESIAN_POINT('Ctrl Pts',(0.251041275456718,1.89783254016515,12.1736900014085));
#38779=CARTESIAN_POINT('Ctrl Pts',(0.227545942908155,1.86968676522925,12.1713601176505));
#38780=CARTESIAN_POINT('Ctrl Pts',(0.204364147588138,1.84889075130435,12.1692427519275));
#38781=CARTESIAN_POINT('Ctrl Pts',(0.170836805670864,1.82657268743745,12.1665364750497));
#38782=CARTESIAN_POINT('Ctrl Pts',(0.162873046236269,1.82175531227858,12.1659177552412));
#38783=CARTESIAN_POINT('Ctrl Pts',(0.150346199277729,1.81490009088923,12.1649921089536));
#38784=CARTESIAN_POINT('Ctrl Pts',(0.145925882047167,1.81261248882104,12.1646741610063));
#38785=CARTESIAN_POINT('Ctrl Pts',(0.140931396430074,1.81017271437321,12.1643259532111));
#38786=CARTESIAN_POINT('Ctrl Pts',(0.140408034509772,1.80991880817402,12.1642895987867));
#38787=CARTESIAN_POINT('Ctrl Pts',(0.139630318786893,1.80954410148359,12.1642357772598));
#38788=CARTESIAN_POINT('Ctrl Pts',(0.139376493185796,1.8094222168572,12.164218243068));
#38789=CARTESIAN_POINT('Ctrl Pts',(0.138943231789713,1.80921486718607,12.1641883679928));
#38790=CARTESIAN_POINT('Ctrl Pts',(0.138763876597136,1.80912923543541,12.1641760166591));
#38791=CARTESIAN_POINT('Ctrl Pts',(0.138395197330561,1.80895363098148,12.1641506602807));
#38792=CARTESIAN_POINT('Ctrl Pts',(0.13820586514329,1.80886367728561,12.1641376564394));
#38793=CARTESIAN_POINT('Ctrl Pts',(0.137749300413533,1.80864730436267,12.1641063407173));
#38794=CARTESIAN_POINT('Ctrl Pts',(0.137481980834658,1.80852106771337,12.1640880402419));
#38795=CARTESIAN_POINT('Ctrl Pts',(0.136658929270486,1.80813378123072,12.1640318011251));
#38796=CARTESIAN_POINT('Ctrl Pts',(0.136102620547022,1.80787394963331,12.1639939374812));
#38797=CARTESIAN_POINT('Ctrl Pts',(0.12948205741262,1.80480474240426,12.1635450549818));
#38798=CARTESIAN_POINT('Ctrl Pts',(0.123332048445309,1.80218283401148,12.1631452764038));
#38799=CARTESIAN_POINT('Ctrl Pts',(0.0917936320983183,1.78988196354108,
12.1611594158225));
#38800=CARTESIAN_POINT('Ctrl Pts',(0.0653340231711807,1.78324924108288,
12.1596921107348));
#38801=CARTESIAN_POINT('Ctrl Pts',(0.0234432435491287,1.77822818313575,
12.1572955251619));
#38802=CARTESIAN_POINT('Ctrl Pts',(0.0084280757097688,1.77748555327846,
12.1564240409192));
#38803=CARTESIAN_POINT('Ctrl Pts',(-0.0081725582554667,1.77782471727114,
12.1554222443731));
#38804=CARTESIAN_POINT('Ctrl Pts',(-0.00976187437105561,1.77786895651076,
12.1553259597712));
#38805=CARTESIAN_POINT('Ctrl Pts',(-0.0125458590993433,1.77796707149617,
12.1551566146936));
#38806=CARTESIAN_POINT('Ctrl Pts',(-0.0137406851767255,1.77801584024699,
12.1550837143999));
#38807=CARTESIAN_POINT('Ctrl Pts',(-0.0154692699800852,1.77809603426448,
12.1549779188142));
#38808=CARTESIAN_POINT('Ctrl Pts',(-0.0160032752173329,1.77812214017294,
12.1549451903418));
#38809=CARTESIAN_POINT('Ctrl Pts',(-0.0169345002865394,1.77816998806678,
12.1548880366442));
#38810=CARTESIAN_POINT('Ctrl Pts',(-0.0173317505223976,1.77819113700455,
12.1548636300678));
#38811=CARTESIAN_POINT('Ctrl Pts',(-0.0180988077204094,1.7782333982725,
12.1548164534638));
#38812=CARTESIAN_POINT('Ctrl Pts',(-0.0184686196537694,1.77825441275059,
12.1547936865428));
#38813=CARTESIAN_POINT('Ctrl Pts',(-0.0193448742813105,1.77830572142715,
12.1547396881524));
#38814=CARTESIAN_POINT('Ctrl Pts',(-0.0198512821545668,1.77833657401006,
12.1547084392025));
#38815=CARTESIAN_POINT('Ctrl Pts',(-0.0216285799493489,1.77844906782366,
12.1545986184576));
#38816=CARTESIAN_POINT('Ctrl Pts',(-0.022899044229911,1.77853704544257,
12.1545198480204));
#38817=CARTESIAN_POINT('Ctrl Pts',(-0.0411450457737177,1.77990926438546,
12.1533846502993));
#38818=CARTESIAN_POINT('Ctrl Pts',(-0.0579903969458637,1.78252883832415,
12.152285570243));
#38819=CARTESIAN_POINT('Ctrl Pts',(-0.0911875576247426,1.79042200291301,
12.1500191617782));
#38820=CARTESIAN_POINT('Ctrl Pts',(-0.10748522584018,1.79569657715043,12.1488551765193));
#38821=CARTESIAN_POINT('Ctrl Pts',(-0.130820924110811,1.805358579614,12.1471518794098));
#38822=CARTESIAN_POINT('Ctrl Pts',(-0.1382349412377,1.80876333489777,12.1466052785176));
#38823=CARTESIAN_POINT('Ctrl Pts',(-0.152033408991192,1.81574582668419,
12.1455865815941));
#38824=CARTESIAN_POINT('Ctrl Pts',(-0.158441140355762,1.81926700121857,
12.1451129415581));
#38825=CARTESIAN_POINT('Ctrl Pts',(-0.165761188492736,1.82362008047841,
12.1445758691809));
#38826=CARTESIAN_POINT('Ctrl Pts',(-0.166794819787399,1.82424264338602,
12.1445001279929));
#38827=CARTESIAN_POINT('Ctrl Pts',(-0.168146458673976,1.82506712475546,
12.1444012361979));
#38828=CARTESIAN_POINT('Ctrl Pts',(-0.168467625909909,1.82526380566341,
12.1443777495246));
#38829=CARTESIAN_POINT('Ctrl Pts',(-0.168990835316154,1.82558547843364,
12.1443395071253));
#38830=CARTESIAN_POINT('Ctrl Pts',(-0.169193084176494,1.82571013081948,
12.1443247291086));
#38831=CARTESIAN_POINT('Ctrl Pts',(-0.169583531184181,1.82595137185702,
12.1442962092028));
#38832=CARTESIAN_POINT('Ctrl Pts',(-0.169771746558197,1.82606793048867,
12.1442824654443));
#38833=CARTESIAN_POINT('Ctrl Pts',(-0.170208244731394,1.82633886916924,
12.1442506013793));
#38834=CARTESIAN_POINT('Ctrl Pts',(-0.170456438526596,1.82649339373872,
12.1442324906558));
#38835=CARTESIAN_POINT('Ctrl Pts',(-0.171259754222359,1.82699505339711,
12.1441738949846));
#38836=CARTESIAN_POINT('Ctrl Pts',(-0.171814033209855,1.82734354528852,
12.1441334992411));
#38837=CARTESIAN_POINT('Ctrl Pts',(-0.177179836772807,1.8307400473474,12.1437427378237));
#38838=CARTESIAN_POINT('Ctrl Pts',(-0.181911182404739,1.83391364538554,
12.1434005020155));
#38839=CARTESIAN_POINT('Ctrl Pts',(-0.195745284064745,1.84373460618117,
12.142398973718));
#38840=CARTESIAN_POINT('Ctrl Pts',(-0.204586613609977,1.85073602891783,
12.1417576053892));
#38841=CARTESIAN_POINT('Ctrl Pts',(-0.22128263679001,1.86544564942136,12.1405054370517));
#38842=CARTESIAN_POINT('Ctrl Pts',(-0.229145399952628,1.87312087174949,
12.1398950542117));
#38843=CARTESIAN_POINT('Ctrl Pts',(-0.251952900995127,1.89778197137217,
12.1380112652371));
#38844=CARTESIAN_POINT('Ctrl Pts',(-0.265512703365968,1.91594791907097,
12.1367206890951));
#38845=CARTESIAN_POINT('Ctrl Pts',(-0.277645959975347,1.936368660818,12.1352762218622));
#38846=CARTESIAN_POINT('Ctrl Pts',(-0.27822723456428,1.93735898381281,12.1352062020391));
#38847=CARTESIAN_POINT('Ctrl Pts',(-0.279066951837687,1.93880729381427,
12.1351038377163));
#38848=CARTESIAN_POINT('Ctrl Pts',(-0.279329590453365,1.93926284801754,
12.1350716451628));
#38849=CARTESIAN_POINT('Ctrl Pts',(-0.27978825219837,1.94006292899954,12.1350151144643));
#38850=CARTESIAN_POINT('Ctrl Pts',(-0.279984757338678,1.94040717934645,
12.1349907937725));
#38851=CARTESIAN_POINT('Ctrl Pts',(-0.280364853781442,1.94107591941838,
12.1349435533605));
#38852=CARTESIAN_POINT('Ctrl Pts',(-0.280548518191308,1.94140036707656,
12.13492063632));
#38853=CARTESIAN_POINT('Ctrl Pts',(-0.280985316710408,1.94217511518753,
12.1348659177072));
#38854=CARTESIAN_POINT('Ctrl Pts',(-0.281237931362542,1.94262570594003,
12.13483409754));
#38855=CARTESIAN_POINT('Ctrl Pts',(-0.28199748553383,1.94398819810244,12.1347378908009));
#38856=CARTESIAN_POINT('Ctrl Pts',(-0.28250107743314,1.94490194911993,12.1346733845903));
#38857=CARTESIAN_POINT('Ctrl Pts',(-0.287736591034372,1.95451171326688,
12.1339951036527));
#38858=CARTESIAN_POINT('Ctrl Pts',(-0.292069387199294,1.96341806184594,
12.133367244534));
#38859=CARTESIAN_POINT('Ctrl Pts',(-0.296869168429375,1.97456130509599,
12.132581496512));
#38860=CARTESIAN_POINT('Ctrl Pts',(-0.297731807523742,1.97662277450443,
12.1324361396497));
#38861=CARTESIAN_POINT('Ctrl Pts',(-0.298895556221969,1.97948710948933,
12.1322341931402));
#38862=CARTESIAN_POINT('Ctrl Pts',(-0.299215018163668,1.9802824858496,12.1321781184354));
#38863=CARTESIAN_POINT('Ctrl Pts',(-0.308750751162532,2.00430056038684,
12.1304849230833));
#38864=CARTESIAN_POINT('Ctrl Pts',(-0.315237930365231,2.02851427611628,
12.1287711660902));
#38865=CARTESIAN_POINT('Ctrl Pts',(-0.320147128974368,2.06198330959738,
12.1265069835472));
#38866=CARTESIAN_POINT('Ctrl Pts',(-0.321070208798186,2.07078699950152,
12.1259219516109));
#38867=CARTESIAN_POINT('Ctrl Pts',(-0.321876437882674,2.0835094746295,12.1251012450242));
#38868=CARTESIAN_POINT('Ctrl Pts',(-0.322052405675305,2.0874051564045,12.1248532804103));
#38869=CARTESIAN_POINT('Ctrl Pts',(-0.322172199007007,2.09184273151272,
12.1245753430664));
#38870=CARTESIAN_POINT('Ctrl Pts',(-0.32218540670297,2.09238222080429,12.1245416294158));
#38871=CARTESIAN_POINT('Ctrl Pts',(-0.322203257140202,2.09319476037057,
12.1244909694424));
#38872=CARTESIAN_POINT('Ctrl Pts',(-0.322208907938681,2.09346778410821,
12.1244739669452));
#38873=CARTESIAN_POINT('Ctrl Pts',(-0.322218412677592,2.09395707503039,
12.1244435325245));
#38874=CARTESIAN_POINT('Ctrl Pts',(-0.322222395911609,2.09417333847038,
12.1244300933561));
#38875=CARTESIAN_POINT('Ctrl Pts',(-0.322229951516671,2.09460728560368,
12.1244031522037));
#38876=CARTESIAN_POINT('Ctrl Pts',(-0.322233521017299,2.09482496797487,
12.1243896504294));
#38877=CARTESIAN_POINT('Ctrl Pts',(-0.322242957230069,2.09543833972952,
12.1243516416435));
#38878=CARTESIAN_POINT('Ctrl Pts',(-0.322248315737617,2.09583403828043,
12.1243271632287));
#38879=CARTESIAN_POINT('Ctrl Pts',(-0.322267433478843,2.0974680799195,12.1242262483593));
#38880=CARTESIAN_POINT('Ctrl Pts',(-0.322274783835762,2.09870650839261,
12.124150166534));
#38881=CARTESIAN_POINT('Ctrl Pts',(-0.322276342644679,2.10783575717569,
12.1235920718815));
#38882=CARTESIAN_POINT('Ctrl Pts',(-0.321987884382043,2.11572467674183,
12.1231249473739));
#38883=CARTESIAN_POINT('Ctrl Pts',(-0.320794431443524,2.13198133051904,
12.1221792048649));
#38884=CARTESIAN_POINT('Ctrl Pts',(-0.319850850105213,2.14034006637319,
12.121702180975));
#38885=CARTESIAN_POINT('Ctrl Pts',(-0.314846686075205,2.17310768393261,
12.1198374257963));
#38886=CARTESIAN_POINT('Ctrl Pts',(-0.30830907175252,2.19704965078469,12.1184794041006));
#38887=CARTESIAN_POINT('Ctrl Pts',(-0.298222415858701,2.22218873643454,
12.1168961651712));
#38888=CARTESIAN_POINT('Ctrl Pts',(-0.297323639458718,2.2243597590333,12.1167581572311));
#38889=CARTESIAN_POINT('Ctrl Pts',(-0.293834214327468,2.23253446624093,
12.1162333473793));
#38890=CARTESIAN_POINT('Ctrl Pts',(-0.291084937616096,2.23846833617486,
12.1158417462099));
#38891=CARTESIAN_POINT('Ctrl Pts',(-0.287693952721533,2.24523923553649,
12.1153808672837));
#38892=CARTESIAN_POINT('Ctrl Pts',(-0.28722622410126,2.24616204063013,12.1153177472294));
#38893=CARTESIAN_POINT('Ctrl Pts',(-0.28652410589395,2.24753089929728,12.1152236536467));
#38894=CARTESIAN_POINT('Ctrl Pts',(-0.286293097303326,2.24797868744418,
12.1151927991736));
#38895=CARTESIAN_POINT('Ctrl Pts',(-0.285879908224683,2.24877502604746,
12.1151377952781));
#38896=CARTESIAN_POINT('Ctrl Pts',(-0.285698137645992,2.24912378899897,
12.1151136603659));
#38897=CARTESIAN_POINT('Ctrl Pts',(-0.285314271613702,2.24985703422972,
12.1150628224405));
#38898=CARTESIAN_POINT('Ctrl Pts',(-0.285112036492967,2.25024144214723,
12.1150361145187));
#38899=CARTESIAN_POINT('Ctrl Pts',(-0.284577357507929,2.25125279102775,
12.1149657000253));
#38900=CARTESIAN_POINT('Ctrl Pts',(-0.284243620340959,2.25187904227533,
12.1149219476256));
#38901=CARTESIAN_POINT('Ctrl Pts',(-0.282738413854348,2.25468119422699,
12.1147254996966));
#38902=CARTESIAN_POINT('Ctrl Pts',(-0.281544033866004,2.25684463320035,
12.1145719896642));
#38903=CARTESIAN_POINT('Ctrl Pts',(-0.272595332374421,2.27262222748544,
12.1134386165789));
#38904=CARTESIAN_POINT('Ctrl Pts',(-0.263883444601653,2.28566649216866,
12.1124236805742));
#38905=CARTESIAN_POINT('Ctrl Pts',(-0.236605405955893,2.32069093170012,
12.1094737416403));
#38906=CARTESIAN_POINT('Ctrl Pts',(-0.216001620746892,2.34089377680088,
12.1074804842746));
#38907=CARTESIAN_POINT('Ctrl Pts',(-0.192765426186075,2.35826875051136,
12.105604309327));
#38908=CARTESIAN_POINT('Ctrl Pts',(-0.192536709343627,2.35843930153844,
12.1055858757837));
#38909=CARTESIAN_POINT('Ctrl Pts',(-0.188905269226977,2.36113972051574,
12.1052937389265));
#38910=CARTESIAN_POINT('Ctrl Pts',(-0.185452962391017,2.36360265062239,
12.1050235322111));
#38911=CARTESIAN_POINT('Ctrl Pts',(-0.181504106688871,2.366303831138,12.1047237410441));
#38912=CARTESIAN_POINT('Ctrl Pts',(-0.181054580133359,2.36660965895231,
12.1046897470741));
#38913=CARTESIAN_POINT('Ctrl Pts',(-0.180374006908891,2.36707016036639,
12.1046384848981));
#38914=CARTESIAN_POINT('Ctrl Pts',(-0.180143533298982,2.36722567305274,
12.1046211603767));
#38915=CARTESIAN_POINT('Ctrl Pts',(-0.179742795404267,2.367495317979,12.1045910987732));
#38916=CARTESIAN_POINT('Ctrl Pts',(-0.179572623437434,2.36760958606291,
12.1045783524571));
#38917=CARTESIAN_POINT('Ctrl Pts',(-0.179216320076034,2.36784834587156,
12.1045517048543));
#38918=CARTESIAN_POINT('Ctrl Pts',(-0.179030168039897,2.36797280589582,
12.1045378057822));
#38919=CARTESIAN_POINT('Ctrl Pts',(-0.178584310861066,2.36827023111519,
12.1045045705911));
#38920=CARTESIAN_POINT('Ctrl Pts',(-0.178324483040512,2.36844301395011,
12.1044852468717));
#38921=CARTESIAN_POINT('Ctrl Pts',(-0.177441278281839,2.36902848789052,
12.1044197110749));
#38922=CARTESIAN_POINT('Ctrl Pts',(-0.176816710423165,2.36943939109999,
12.1043736187561));
#38923=CARTESIAN_POINT('Ctrl Pts',(-0.175326403644068,2.37041245034939,
12.1042642203409));
#38924=CARTESIAN_POINT('Ctrl Pts',(-0.174459376618461,2.37097263163358,
12.1042010416293));
#38925=CARTESIAN_POINT('Ctrl Pts',(-0.163988764406526,2.37766654786409,
12.1034434792377));
#38926=CARTESIAN_POINT('Ctrl Pts',(-0.154067913270634,2.3832916613998,12.1027802092355));
#38927=CARTESIAN_POINT('Ctrl Pts',(-0.121248992365313,2.39966457572549,
12.1006890229254));
#38928=CARTESIAN_POINT('Ctrl Pts',(-0.0973802288642483,2.40824883565762,
12.0993143269129));
#38929=CARTESIAN_POINT('Ctrl Pts',(-0.0673866300508326,2.41519923857274,
12.0975427651838));
#38930=CARTESIAN_POINT('Ctrl Pts',(-0.0619896586598934,2.41630490929118,
12.0972226972234));
#38931=CARTESIAN_POINT('Ctrl Pts',(-0.0556434249638426,2.41743639576912,
12.0968434854783));
#38932=CARTESIAN_POINT('Ctrl Pts',(-0.0547189477608854,2.41759706048924,
12.0967881747857));
#38933=CARTESIAN_POINT('Ctrl Pts',(-0.0474315267750385,2.41883077705468,
12.0963515881348));
#38934=CARTESIAN_POINT('Ctrl Pts',(-0.0410387246194138,2.41971648117848,
12.0959650359531));
#38935=CARTESIAN_POINT('Ctrl Pts',(-0.0335993630445958,2.42052039014624,
12.0955096149025));
#38936=CARTESIAN_POINT('Ctrl Pts',(-0.0325742437269905,2.42062619403822,
12.0954467380287));
#38937=CARTESIAN_POINT('Ctrl Pts',(-0.0310479922440137,2.42077632531076,
12.095352937302));
#38938=CARTESIAN_POINT('Ctrl Pts',(-0.0305472283189572,2.420824399851,12.0953221314156));
#38939=CARTESIAN_POINT('Ctrl Pts',(-0.0296548761251554,2.4209079596199,
12.0952671820205));
#38940=CARTESIAN_POINT('Ctrl Pts',(-0.0292633307583247,2.42094390116679,
12.0952430529162));
#38941=CARTESIAN_POINT('Ctrl Pts',(-0.0284386802876307,2.42101807757636,
12.0951921942891));
#38942=CARTESIAN_POINT('Ctrl Pts',(-0.0280055619243542,2.42105615266753,
12.0951654597923));
#38943=CARTESIAN_POINT('Ctrl Pts',(-0.0268634325159719,2.42115422761673,
12.095094900364));
#38944=CARTESIAN_POINT('Ctrl Pts',(-0.0261543004354624,2.42121275578406,
12.0950510292621));
#38945=CARTESIAN_POINT('Ctrl Pts',(-0.0229629466071878,2.42146551582734,
12.0948533108662));
#38946=CARTESIAN_POINT('Ctrl Pts',(-0.0204787716737362,2.42163332248732,
12.0946986360709));
#38947=CARTESIAN_POINT('Ctrl Pts',(-0.00214820910588213,2.42265833610814,
12.0935513645042));
#38948=CARTESIAN_POINT('Ctrl Pts',(0.0137378763777866,2.42237269203914,
12.0925227540347));
#38949=CARTESIAN_POINT('Ctrl Pts',(0.0564403062377369,2.41844249300545,
12.0896714181599));
#38950=CARTESIAN_POINT('Ctrl Pts',(0.082924205436861,2.41259337476701,12.0878025395995));
#38951=CARTESIAN_POINT('Ctrl Pts',(0.108647696570679,2.40340887004453,12.086021597949));
#38952=CARTESIAN_POINT('Ctrl Pts',(0.108928147269132,2.40330829715905,12.0860021868571));
#38953=CARTESIAN_POINT('Ctrl Pts',(0.110229349414959,2.40283963342715,12.0859121530276));
#38954=CARTESIAN_POINT('Ctrl Pts',(0.111248389420634,2.40246677331318,12.0858417213046));
#38955=CARTESIAN_POINT('Ctrl Pts',(0.112389400507216,2.40204273826556,12.0857629623433));
#38956=CARTESIAN_POINT('Ctrl Pts',(0.112513233101716,2.40199663154147,12.0857544160885));
#38957=CARTESIAN_POINT('Ctrl Pts',(0.113001208460231,2.40181460134739,12.0857207441392));
#38958=CARTESIAN_POINT('Ctrl Pts',(0.113365135129699,2.40167809472999,12.0856956439717));
#38959=CARTESIAN_POINT('Ctrl Pts',(0.117575462687778,2.40009013263181,12.0854054020905));
#38960=CARTESIAN_POINT('Ctrl Pts',(0.121394225358391,2.39856577686673,12.0851435626341));
#38961=CARTESIAN_POINT('Ctrl Pts',(0.125679617542044,2.39675932980752,12.0848521719234));
#38962=CARTESIAN_POINT('Ctrl Pts',(0.126175726413537,2.39654873489412,12.0848184758354));
#38963=CARTESIAN_POINT('Ctrl Pts',(0.126925842305621,2.39622809253203,12.0847675867588));
#38964=CARTESIAN_POINT('Ctrl Pts',(0.127180236604031,2.39611896202188,12.084750338594));
#38965=CARTESIAN_POINT('Ctrl Pts',(0.127622478347012,2.39592857336603,12.0847203726292));
#38966=CARTESIAN_POINT('Ctrl Pts',(0.127810389052439,2.395847464016,12.0847076457372));
#38967=CARTESIAN_POINT('Ctrl Pts',(0.128203982621281,2.39567712919892,12.0846810006182));
#38968=CARTESIAN_POINT('Ctrl Pts',(0.128409649579512,2.39558786813145,12.0846670846682));
#38969=CARTESIAN_POINT('Ctrl Pts',(0.128902674474397,2.3953732797994,12.0846337419977));
#38970=CARTESIAN_POINT('Ctrl Pts',(0.129189944022693,2.39524774727593,12.0846143278844));
#38971=CARTESIAN_POINT('Ctrl Pts',(0.13016958531043,2.39481795507537,12.084548167074));
#38972=CARTESIAN_POINT('Ctrl Pts',(0.130861075784829,2.39451167455012,12.0845015432624));
#38973=CARTESIAN_POINT('Ctrl Pts',(0.142600617937084,2.38926239267484,12.0837112007433));
#38974=CARTESIAN_POINT('Ctrl Pts',(0.153364144754091,2.3837026318528,12.0830045167327));
#38975=CARTESIAN_POINT('Ctrl Pts',(0.191346715704932,2.36128795671964,12.0804868447398));
#38976=CARTESIAN_POINT('Ctrl Pts',(0.216326639293571,2.34101426935919,12.0787643842795));
#38977=CARTESIAN_POINT('Ctrl Pts',(0.242308366819171,2.31258014371959,12.0764899334645));
#38978=CARTESIAN_POINT('Ctrl Pts',(0.246557969961256,2.3076362695811,12.0760995388745));
#38979=CARTESIAN_POINT('Ctrl Pts',(0.25130423633888,2.30176328902512,12.0756399642001));
#38980=CARTESIAN_POINT('Ctrl Pts',(0.251950046323989,2.30095625921681,12.0755769019998));
#38981=CARTESIAN_POINT('Ctrl Pts',(0.252904760717497,2.2997513737652,12.0754828780808));
#38982=CARTESIAN_POINT('Ctrl Pts',(0.25321663718779,2.29935587265344,12.0754520351579));
#38983=CARTESIAN_POINT('Ctrl Pts',(0.253770370881625,2.29865026842742,12.0753970442252));
#38984=CARTESIAN_POINT('Ctrl Pts',(0.254012590589035,2.29834044999383,12.0753729107006));
#38985=CARTESIAN_POINT('Ctrl Pts',(0.254515789257966,2.2976943848864,12.0753226096125));
#38986=CARTESIAN_POINT('Ctrl Pts',(0.254776670233835,2.29735806317201,12.0752964382295));
#38987=CARTESIAN_POINT('Ctrl Pts',(0.255444997307883,2.29649293784218,12.0752291520355));
#38988=CARTESIAN_POINT('Ctrl Pts',(0.255851466518521,2.2959633852052,12.0751879987387));
#38989=CARTESIAN_POINT('Ctrl Pts',(0.256740117558838,2.29479816281396,12.0750975165));
#38990=CARTESIAN_POINT('Ctrl Pts',(0.257221588966973,2.29416195907221,12.0750481599284));
#38991=CARTESIAN_POINT('Ctrl Pts',(0.258615602521586,2.29230566065964,12.0749042785559));
#38992=CARTESIAN_POINT('Ctrl Pts',(0.259521851473747,2.29108088724055,12.074809508858));
#38993=CARTESIAN_POINT('Ctrl Pts',(0.268641970442819,2.27857070155952,12.0738430620765));
#38994=CARTESIAN_POINT('Ctrl Pts',(0.276122002535642,2.26677095102367,12.0729432997772));
#38995=CARTESIAN_POINT('Ctrl Pts',(0.292517403551519,2.23676392951125,12.0706840739576));
#38996=CARTESIAN_POINT('Ctrl Pts',(0.300526584624002,2.21812901149954,12.0693029557718));
#38997=CARTESIAN_POINT('Ctrl Pts',(0.311166577221818,2.18511888572013,12.0669694528979));
#38998=CARTESIAN_POINT('Ctrl Pts',(0.314669488683918,2.17108507123702,12.0660112204675));
#38999=CARTESIAN_POINT('Ctrl Pts',(0.317378876897357,2.1559700374265,12.0650455373233));
#39000=CARTESIAN_POINT('Ctrl Pts',(0.317534983662659,2.15507749801205,12.0649887586903));
#39001=CARTESIAN_POINT('Ctrl Pts',(0.317740022986055,2.15387533437661,12.0649126234802));
#39002=CARTESIAN_POINT('Ctrl Pts',(0.317792269155838,2.15356629096906,12.0648930814105));
#39003=CARTESIAN_POINT('Ctrl Pts',(0.317879516614113,2.15304558950056,12.0648602067882));
#39004=CARTESIAN_POINT('Ctrl Pts',(0.317914757412299,2.15283397267269,12.0648468606096));
#39005=CARTESIAN_POINT('Ctrl Pts',(0.317981975588801,2.15242783313206,12.0648212739914));
#39006=CARTESIAN_POINT('Ctrl Pts',(0.318013985555463,2.15223331769722,12.0648090317966));
#39007=CARTESIAN_POINT('Ctrl Pts',(0.318089377464563,2.15177254430247,12.0647800609023));
#39008=CARTESIAN_POINT('Ctrl Pts',(0.318132603531913,2.1515062614701,12.0647633412003));
#39009=CARTESIAN_POINT('Ctrl Pts',(0.318258753060684,2.15072293304063,12.0647142224976));
#39010=CARTESIAN_POINT('Ctrl Pts',(0.318340751250185,2.15020573611238,12.0646818760227));
#39011=CARTESIAN_POINT('Ctrl Pts',(0.31895192772459,2.14628908819037,12.0644375446238));
#39012=CARTESIAN_POINT('Ctrl Pts',(0.319427926279899,2.14288139592922,12.0642285151055));
#39013=CARTESIAN_POINT('Ctrl Pts',(0.32087536591281,2.13115089764422,12.0635191224879));
#39014=CARTESIAN_POINT('Ctrl Pts',(0.321576846406159,2.12279766927815,12.0630314413043));
#39015=CARTESIAN_POINT('Ctrl Pts',(0.323251811739511,2.0854165583293,12.0608899003674));
#39016=CARTESIAN_POINT('Ctrl Pts',(0.320625212844513,2.05636490487368,12.0593223774467));
#39017=CARTESIAN_POINT('Ctrl Pts',(0.311931257958311,2.01840243405245,12.0570572898398));
#39018=CARTESIAN_POINT('Ctrl Pts',(0.30927657115139,2.00885591194299,12.0564698452399));
#39019=CARTESIAN_POINT('Ctrl Pts',(0.30586122654522,1.99845604637467,12.0558042407609));
#39020=CARTESIAN_POINT('Ctrl Pts',(0.305530850052019,1.99746627848342,12.0557406356672));
#39021=CARTESIAN_POINT('Ctrl Pts',(0.305029731543204,1.99598891704386,12.0556453029613));
#39022=CARTESIAN_POINT('Ctrl Pts',(0.30486261210656,1.99550009455654,12.0556136950926));
#39023=CARTESIAN_POINT('Ctrl Pts',(0.304572859679391,1.9946591827585,12.0555592085317));
#39024=CARTESIAN_POINT('Ctrl Pts',(0.304450789345346,1.99430689948966,12.0555363485114));
#39025=CARTESIAN_POINT('Ctrl Pts',(0.30419767758189,1.99358052011555,12.0554891425613));
#39026=CARTESIAN_POINT('Ctrl Pts',(0.304066556779484,1.99320645248343,12.0554647940285));
#39027=CARTESIAN_POINT('Ctrl Pts',(0.303763412812162,1.99234671332916,12.0554087431974));
#39028=CARTESIAN_POINT('Ctrl Pts',(0.303590914737119,1.99186121149888,12.0553770251585));
#39029=CARTESIAN_POINT('Ctrl Pts',(0.303046059274321,1.99033927580699,12.0552773889728));
#39030=CARTESIAN_POINT('Ctrl Pts',(0.302669556041228,1.98930434394344,12.0552093329133));
#39031=CARTESIAN_POINT('Ctrl Pts',(0.301785139409619,1.98691150759013,12.0550512721788));
#39032=CARTESIAN_POINT('Ctrl Pts',(0.301273355848217,1.98555506813573,12.0549611390311));
#39033=CARTESIAN_POINT('Ctrl Pts',(0.299523426295115,1.98101011699842,12.0546573177753));
#39034=CARTESIAN_POINT('Ctrl Pts',(0.298243708771523,1.97783796053585,12.0544422438788));
#39035=CARTESIAN_POINT('Ctrl Pts',(0.295809896633002,1.9720713472433,12.0540455887641));
#39036=CARTESIAN_POINT('Ctrl Pts',(0.29467152676829,1.96947059471199,12.0538645463809));
#39037=CARTESIAN_POINT('Ctrl Pts',(0.289349290332363,1.957735821964,12.053037800909));
#39038=CARTESIAN_POINT('Ctrl Pts',(0.284774405934017,1.94878619648626,12.0523796310785));
#39039=CARTESIAN_POINT('Ctrl Pts',(0.272736844017015,1.92772768819283,12.0507664571177));
#39040=CARTESIAN_POINT('Ctrl Pts',(0.264876196253862,1.91587043053461,12.0498028038996));
#39041=CARTESIAN_POINT('Ctrl Pts',(0.24813767994117,1.89392176240011,12.0479363997521));
#39042=CARTESIAN_POINT('Ctrl Pts',(0.239359483924502,1.88378796914508,12.0470352881193));
#39043=CARTESIAN_POINT('Ctrl Pts',(0.229885608055355,1.87413765410015,12.0461568304018));
#39044=CARTESIAN_POINT('Ctrl Pts',(0.229795670977447,1.87404615142359,12.0461484991051));
#39045=CARTESIAN_POINT('Ctrl Pts',(0.229130367416071,1.87337007451341,12.0460869285154));
#39046=CARTESIAN_POINT('Ctrl Pts',(0.228552820111591,1.87278763932374,12.0460338087481));
#39047=CARTESIAN_POINT('Ctrl Pts',(0.224892119606804,1.86912403877662,12.0456992245402));
#39048=CARTESIAN_POINT('Ctrl Pts',(0.22174875870577,1.86610329715778,12.0454213116809));
#39049=CARTESIAN_POINT('Ctrl Pts',(0.21810335814314,1.86273967519813,12.0451104867994));
#39050=CARTESIAN_POINT('Ctrl Pts',(0.217660680020132,1.86233350058245,12.0450729298607));
#39051=CARTESIAN_POINT('Ctrl Pts',(0.217005210459183,1.86173544882039,12.0450176000678));
#39052=CARTESIAN_POINT('Ctrl Pts',(0.216793298041192,1.86154261671903,12.0449997550948));
#39053=CARTESIAN_POINT('Ctrl Pts',(0.216417884953318,1.86120191941071,12.0449682184425));
#39054=CARTESIAN_POINT('Ctrl Pts',(0.216254489534505,1.86105393918679,12.0449545179779));
#39055=CARTESIAN_POINT('Ctrl Pts',(0.215912759735543,1.86074508679979,12.0449259180504));
#39056=CARTESIAN_POINT('Ctrl Pts',(0.215734397737667,1.86058424667384,12.0449110210242));
#39057=CARTESIAN_POINT('Ctrl Pts',(0.215267257675232,1.86016394326313,12.0448720837695));
#39058=CARTESIAN_POINT('Ctrl Pts',(0.214978189188748,1.85990480114132,12.044848067914));
#39059=CARTESIAN_POINT('Ctrl Pts',(0.213711821596809,1.85877365726831,12.044743197888));
#39060=CARTESIAN_POINT('Ctrl Pts',(0.212729662234632,1.85790707969616,12.044662746984));
#39061=CARTESIAN_POINT('Ctrl Pts',(0.205424639930517,1.85154050472333,12.0440706370197));
#39062=CARTESIAN_POINT('Ctrl Pts',(0.19889407030068,1.84628248118893,12.0435757369528));
#39063=CARTESIAN_POINT('Ctrl Pts',(0.170912706136436,1.8254988411915,12.0415590738294));
#39064=CARTESIAN_POINT('Ctrl Pts',(0.147795140849095,1.81239117588283,12.0401266825216));
#39065=CARTESIAN_POINT('Ctrl Pts',(0.11788420284448,1.8000012067781,12.038277335202));
#39066=CARTESIAN_POINT('Ctrl Pts',(0.112374536890905,1.79789419130619,12.0379372667046));
#39067=CARTESIAN_POINT('Ctrl Pts',(0.0983432297810051,1.79296527299348,
12.0370688533339));
#39068=CARTESIAN_POINT('Ctrl Pts',(0.0897562555820195,1.7903461511095,12.0365351426031));
#39069=CARTESIAN_POINT('Ctrl Pts',(0.0800870385554768,1.78783293408209,
12.0359275320927));
#39070=CARTESIAN_POINT('Ctrl Pts',(0.0791011302280017,1.78758165555159,
12.0358655042935));
#39071=CARTESIAN_POINT('Ctrl Pts',(0.0776192087016818,1.78721142248327,
12.0357721539934));
#39072=CARTESIAN_POINT('Ctrl Pts',(0.0771240695528598,1.78708896843463,
12.035740944406));
#39073=CARTESIAN_POINT('Ctrl Pts',(0.07626817291972,1.78687944949197,12.035686961273));
#39074=CARTESIAN_POINT('Ctrl Pts',(0.0759075508650327,1.7867918310919,12.0356642056069));
#39075=CARTESIAN_POINT('Ctrl Pts',(0.0751604803441865,1.78661168540692,
12.0356170425145));
#39076=CARTESIAN_POINT('Ctrl Pts',(0.0747740106253885,1.78651924961515,
12.0355926321846));
#39077=CARTESIAN_POINT('Ctrl Pts',(0.0740078524348358,1.78633749738929,
12.0355442152473));
#39078=CARTESIAN_POINT('Ctrl Pts',(0.0736281707917203,1.78624815501775,
12.0355202095241));
#39079=CARTESIAN_POINT('Ctrl Pts',(0.0724221234276676,1.78596667141361,
12.0354439175581));
#39080=CARTESIAN_POINT('Ctrl Pts',(0.071595165802398,1.78577710516814,12.0353915486317));
#39081=CARTESIAN_POINT('Ctrl Pts',(0.0661184774266329,1.78454440771338,
12.0350443346611));
#39082=CARTESIAN_POINT('Ctrl Pts',(0.0614470571647858,1.78360129740196,
12.0347462998338));
#39083=CARTESIAN_POINT('Ctrl Pts',(0.0473622213240797,1.78108139661734,
12.0338414748463));
#39084=CARTESIAN_POINT('Ctrl Pts',(0.0378986335420009,1.7798189266956,12.0332250847503));
#39085=CARTESIAN_POINT('Ctrl Pts',(0.0177634636829779,1.77803801319208,
12.031896591862));
#39086=CARTESIAN_POINT('Ctrl Pts',(0.00709377815959828,1.77762643989674,
12.0311825477377));
#39087=CARTESIAN_POINT('Ctrl Pts',(-0.0285418148810626,1.77802188151593,
12.0287786998688));
#39088=CARTESIAN_POINT('Ctrl Pts',(-0.0533926499421487,1.78119916394683,
12.0270651365555));
#39089=CARTESIAN_POINT('Ctrl Pts',(-0.0790127093065122,1.78755768447728,
12.0253966855016));
#39090=CARTESIAN_POINT('Ctrl Pts',(-0.0803943417724939,1.78791033539869,
12.0253070424605));
#39091=CARTESIAN_POINT('Ctrl Pts',(-0.0821781723505735,1.78837827652663,
12.0251917758363));
#39092=CARTESIAN_POINT('Ctrl Pts',(-0.082582522253957,1.78848518883642,
12.0251656792093));
#39093=CARTESIAN_POINT('Ctrl Pts',(-0.0832014200565644,1.78865011848357,
12.0251257851231));
#39094=CARTESIAN_POINT('Ctrl Pts',(-0.083416116021289,1.78870757058941,
12.0251119549578));
#39095=CARTESIAN_POINT('Ctrl Pts',(-0.0838391513241743,1.78882124285904,
12.0250847223095));
#39096=CARTESIAN_POINT('Ctrl Pts',(-0.0840474924058254,1.7888774498507,
12.0250713192196));
#39097=CARTESIAN_POINT('Ctrl Pts',(-0.0845117840499707,1.78900320849143,
12.025041469623));
#39098=CARTESIAN_POINT('Ctrl Pts',(-0.0847677046050711,1.78907286668878,
12.0250250294524));
#39099=CARTESIAN_POINT('Ctrl Pts',(-0.0855078496417092,1.78927530613499,
12.024977520208));
#39100=CARTESIAN_POINT('Ctrl Pts',(-0.0859918529482133,1.78940890392279,
12.0249464985578));
#39101=CARTESIAN_POINT('Ctrl Pts',(-0.0892937978903761,1.79032863861711,
12.0247351664773));
#39102=CARTESIAN_POINT('Ctrl Pts',(-0.0921013497681738,1.79115201599534,
12.0245569813659));
#39103=CARTESIAN_POINT('Ctrl Pts',(-0.100876649826322,1.79385587943207,
12.0240036554662));
#39104=CARTESIAN_POINT('Ctrl Pts',(-0.106801380480692,1.79587207157472,
12.0236353465943));
#39105=CARTESIAN_POINT('Ctrl Pts',(-0.124372230523878,1.80242834231529,
12.0225486147373));
#39106=CARTESIAN_POINT('Ctrl Pts',(-0.135817159314458,1.80747464904349,
12.0218479521593));
#39107=CARTESIAN_POINT('Ctrl Pts',(-0.158129126622751,1.8189050158856,12.0204459340571));
#39108=CARTESIAN_POINT('Ctrl Pts',(-0.168972423408227,1.8252864791507,12.0197457025576));
#39109=CARTESIAN_POINT('Ctrl Pts',(-0.182305698061113,1.83422205232534,
12.0188335876833));
#39110=CARTESIAN_POINT('Ctrl Pts',(-0.185164806383448,1.83620599209155,
12.018634852377));
#39111=CARTESIAN_POINT('Ctrl Pts',(-0.188146863647378,1.83834761597694,
12.0184238482138));
#39112=CARTESIAN_POINT('Ctrl Pts',(-0.188302451619603,1.83845956511626,
12.0184128283133));
#39113=CARTESIAN_POINT('Ctrl Pts',(-0.190293104905162,1.83989458324062,
12.0182716960996));
#39114=CARTESIAN_POINT('Ctrl Pts',(-0.192114262601391,1.84123678117422,
12.0181410633676));
#39115=CARTESIAN_POINT('Ctrl Pts',(-0.196424308197925,1.84448387681834,
12.0178280509826));
#39116=CARTESIAN_POINT('Ctrl Pts',(-0.19889980335659,1.84640610138056,12.0176451471927));
#39117=CARTESIAN_POINT('Ctrl Pts',(-0.20725270393119,1.85308968599336,12.0170165166834));
#39118=CARTESIAN_POINT('Ctrl Pts',(-0.212989990671481,1.85802141359263,
12.0165648631693));
#39119=CARTESIAN_POINT('Ctrl Pts',(-0.219261865361007,1.86380865156669,
12.0160456431915));
#39120=CARTESIAN_POINT('Ctrl Pts',(-0.219972576534066,1.86447041753324,
12.0159864236756));
#39121=CARTESIAN_POINT('Ctrl Pts',(-0.221043380533475,1.86547655173177,
12.0158966128076));
#39122=CARTESIAN_POINT('Ctrl Pts',(-0.221405687971875,1.86581856351412,
12.0158661226934));
#39123=CARTESIAN_POINT('Ctrl Pts',(-0.22203426873031,1.86641469521266,12.0158130448627));
#39124=CARTESIAN_POINT('Ctrl Pts',(-0.222300903220632,1.86666843435003,
12.0157904736159));
#39125=CARTESIAN_POINT('Ctrl Pts',(-0.22285600012287,1.86719850000163,12.0157433651372));
#39126=CARTESIAN_POINT('Ctrl Pts',(-0.22314438450359,1.86747490704329,12.0157188244313));
#39127=CARTESIAN_POINT('Ctrl Pts',(-0.22371608023761,1.86802490180203,12.0156700412862));
#39128=CARTESIAN_POINT('Ctrl Pts',(-0.223999405455169,1.86829847412162,
12.0156457995407));
#39129=CARTESIAN_POINT('Ctrl Pts',(-0.224659066693588,1.86893776864342,
12.0155892045921));
#39130=CARTESIAN_POINT('Ctrl Pts',(-0.225035011544603,1.86930389127467,
12.0155568338936));
#39131=CARTESIAN_POINT('Ctrl Pts',(-0.22717827703285,1.87140138420925,12.0153716162313));
#39132=CARTESIAN_POINT('Ctrl Pts',(-0.228926468791885,1.87315210374666,
12.0152179192767));
#39133=CARTESIAN_POINT('Ctrl Pts',(-0.238144629100653,1.88259867437034,
12.0143931471996));
#39134=CARTESIAN_POINT('Ctrl Pts',(-0.245246334995195,1.89064290602669,
12.0137063221318));
#39135=CARTESIAN_POINT('Ctrl Pts',(-0.256415188918639,1.90464371245674,
12.0125350940816));
#39136=CARTESIAN_POINT('Ctrl Pts',(-0.260707645703019,1.91041006977626,
12.012059041826));
#39137=CARTESIAN_POINT('Ctrl Pts',(-0.280008198590011,1.93823406195168,
12.0097955623566));
#39138=CARTESIAN_POINT('Ctrl Pts',(-0.292432174307986,1.96195564328845,
12.007951472455));
#39139=CARTESIAN_POINT('Ctrl Pts',(-0.303300762439068,1.99096633662732,
12.0059507881019));
#39140=CARTESIAN_POINT('Ctrl Pts',(-0.304729646377609,1.99502600631241,
12.0056764943609));
#39141=CARTESIAN_POINT('Ctrl Pts',(-0.306247780501256,1.99963182463911,
12.0053726061509));
#39142=CARTESIAN_POINT('Ctrl Pts',(-0.306417371473822,2.00015077287905,
12.0053384700555));
#39143=CARTESIAN_POINT('Ctrl Pts',(-0.306671516496781,2.00093520191837,
12.0052870299657));
#39144=CARTESIAN_POINT('Ctrl Pts',(-0.306757045284716,2.00120036225258,
12.0052696691088));
#39145=CARTESIAN_POINT('Ctrl Pts',(-0.306904946481427,2.00166093590926,
12.0052395619487));
#39146=CARTESIAN_POINT('Ctrl Pts',(-0.306967476196906,2.0018562979155,12.0052268063435));
#39147=CARTESIAN_POINT('Ctrl Pts',(-0.307097837914521,2.00226493127482,
12.0052001573061));
#39148=CARTESIAN_POINT('Ctrl Pts',(-0.307165634245588,2.00247821346319,
12.0051862660588));
#39149=CARTESIAN_POINT('Ctrl Pts',(-0.307327216762531,2.00298838008869,
12.0051530810403));
#39150=CARTESIAN_POINT('Ctrl Pts',(-0.307420795324083,2.00328533117939,
12.0051337995716));
#39151=CARTESIAN_POINT('Ctrl Pts',(-0.307736404660327,2.00429193464956,
12.0050685544739));
#39152=CARTESIAN_POINT('Ctrl Pts',(-0.307956411812107,2.00500222646802,
12.0050227091639));
#39153=CARTESIAN_POINT('Ctrl Pts',(-0.308473906375646,2.00669364549663,
12.0049139839374));
#39154=CARTESIAN_POINT('Ctrl Pts',(-0.308769176331079,2.00767545008129,
12.0048512293244));
#39155=CARTESIAN_POINT('Ctrl Pts',(-0.312248405336297,2.01944766304421,
12.0041028513507));
#39156=CARTESIAN_POINT('Ctrl Pts',(-0.314870292802718,2.03039753573283,
12.0034475684549));
#39157=CARTESIAN_POINT('Ctrl Pts',(-0.320464631777269,2.06068495306943,
12.0016903915568));
#39158=CARTESIAN_POINT('Ctrl Pts',(-0.322258901590674,2.08018952259875,
12.0006170278004));
#39159=CARTESIAN_POINT('Ctrl Pts',(-0.322274892162095,2.09973635836811,
11.9995123401165));
#39160=CARTESIAN_POINT('',(-0.322274947886789,2.10018327456701,11.7491602604485));
#39161=CARTESIAN_POINT('Ctrl Pts',(-0.322274892430336,2.09973668646922,
11.9995123215739));
#39162=CARTESIAN_POINT('Ctrl Pts',(-0.322290032118282,2.11826646460107,
11.998465112534));
#39163=CARTESIAN_POINT('Ctrl Pts',(-0.320707131607427,2.13676088898733,
11.9973934805508));
#39164=CARTESIAN_POINT('Ctrl Pts',(-0.317403585914504,2.15582848056797,
11.9962171031456));
#39165=CARTESIAN_POINT('Ctrl Pts',(-0.317259700147515,2.15664042934577,
11.996166878222));
#39166=CARTESIAN_POINT('Ctrl Pts',(-0.317020494760566,2.15796075441193,
11.9960849888164));
#39167=CARTESIAN_POINT('Ctrl Pts',(-0.316927064028642,2.1584694726462,11.9960533843397));
#39168=CARTESIAN_POINT('Ctrl Pts',(-0.316760835545571,2.15936245995073,
11.9959978134875));
#39169=CARTESIAN_POINT('Ctrl Pts',(-0.316688562009118,2.15974682650481,
11.9959738638287));
#39170=CARTESIAN_POINT('Ctrl Pts',(-0.316541340729173,2.16052200912937,
11.9959255008523));
#39171=CARTESIAN_POINT('Ctrl Pts',(-0.316466368453675,2.16091281979292,
11.9959010867913));
#39172=CARTESIAN_POINT('Ctrl Pts',(-0.316320249528839,2.16166694758491,
11.995853914557));
#39173=CARTESIAN_POINT('Ctrl Pts',(-0.316249200246406,2.16203028315394,
11.9958311595252));
#39174=CARTESIAN_POINT('Ctrl Pts',(-0.316079443948475,2.16289051909309,
11.9957772186689));
#39175=CARTESIAN_POINT('Ctrl Pts',(-0.315980191234422,2.1633873096239,11.9957460154522));
#39176=CARTESIAN_POINT('Ctrl Pts',(-0.315628179142087,2.1651278665488,11.9956365076957));
#39177=CARTESIAN_POINT('Ctrl Pts',(-0.315369246679688,2.16637035968056,
11.995558006003));
#39178=CARTESIAN_POINT('Ctrl Pts',(-0.311603227944133,2.18392192505371,
11.994444337203));
#39179=CARTESIAN_POINT('Ctrl Pts',(-0.306842957685684,2.19993348265979,
11.9933682752765));
#39180=CARTESIAN_POINT('Ctrl Pts',(-0.300002591723112,2.21775153115264,
11.99210186751));
#39181=CARTESIAN_POINT('Ctrl Pts',(-0.29911409550308,2.2199905649123,11.9919414789931));
#39182=CARTESIAN_POINT('Ctrl Pts',(-0.291147692691763,2.23942762755785,
11.9905385877598));
#39183=CARTESIAN_POINT('Ctrl Pts',(-0.282618870641937,2.2559922311082,11.9892677428592));
#39184=CARTESIAN_POINT('Ctrl Pts',(-0.2665949560937,2.2814386367926,11.987254522305));
#39185=CARTESIAN_POINT('Ctrl Pts',(-0.259965399447129,2.29081640651409,
11.9864982388604));
#39186=CARTESIAN_POINT('Ctrl Pts',(-0.251875316259416,2.30105339186343,
11.9856727066131));
#39187=CARTESIAN_POINT('Ctrl Pts',(-0.250892691281396,2.30227827125091,
11.9855739349673));
#39188=CARTESIAN_POINT('Ctrl Pts',(-0.249639607953026,2.30381710748217,
11.9854499061954));
#39189=CARTESIAN_POINT('Ctrl Pts',(-0.249377465954066,2.30413776387588,
11.9854240648956));
#39190=CARTESIAN_POINT('Ctrl Pts',(-0.248958647495949,2.30464805879873,
11.985382947382));
#39191=CARTESIAN_POINT('Ctrl Pts',(-0.248802371927658,2.30483802346548,
11.9853676422378));
#39192=CARTESIAN_POINT('Ctrl Pts',(-0.24850656088635,2.30519676600037,11.985338741978));
#39193=CARTESIAN_POINT('Ctrl Pts',(-0.24836707203216,2.30536557917783,11.9853251437229));
#39194=CARTESIAN_POINT('Ctrl Pts',(-0.248048663944691,2.30575012634821,
11.9852941704474));
#39195=CARTESIAN_POINT('Ctrl Pts',(-0.247869635591606,2.30596576883105,
11.9852768035529));
#39196=CARTESIAN_POINT('Ctrl Pts',(-0.247334580884248,2.30660854270363,
11.9852250423686));
#39197=CARTESIAN_POINT('Ctrl Pts',(-0.246977727825137,2.30703498928574,
11.9851907081387));
#39198=CARTESIAN_POINT('Ctrl Pts',(-0.244462830659138,2.31002458643005,
11.9849500375422));
#39199=CARTESIAN_POINT('Ctrl Pts',(-0.24226593212391,2.31255498759519,11.9847464834603));
#39200=CARTESIAN_POINT('Ctrl Pts',(-0.223224836657174,2.3338077888887,11.9830335220682));
#39201=CARTESIAN_POINT('Ctrl Pts',(-0.204276648897697,2.35053310299692,
11.9816581951961));
#39202=CARTESIAN_POINT('Ctrl Pts',(-0.177410987497878,2.36915180801182,
11.9798239717321));
#39203=CARTESIAN_POINT('Ctrl Pts',(-0.171103661643706,2.3732048405163,11.9794010476863));
#39204=CARTESIAN_POINT('Ctrl Pts',(-0.157445147313083,2.38132305914348,
11.9784929139338));
#39205=CARTESIAN_POINT('Ctrl Pts',(-0.150064969971981,2.38532810505858,
11.9780066503481));
#39206=CARTESIAN_POINT('Ctrl Pts',(-0.138639245049303,2.39096258331196,
11.9772541433389));
#39207=CARTESIAN_POINT('Ctrl Pts',(-0.134702900288916,2.39280572252739,
11.9769949698291));
#39208=CARTESIAN_POINT('Ctrl Pts',(-0.129147863052701,2.39527106805049,
11.9766287446207));
#39209=CARTESIAN_POINT('Ctrl Pts',(-0.127559494214819,2.39596072275757,
11.976523976498));
#39210=CARTESIAN_POINT('Ctrl Pts',(-0.124795705033128,2.39713435222583,
11.9763415507626));
#39211=CARTESIAN_POINT('Ctrl Pts',(-0.123622826445872,2.39762423956485,
11.9762640947415));
#39212=CARTESIAN_POINT('Ctrl Pts',(-0.122050622481403,2.39827002009293,
11.9761602049899));
#39213=CARTESIAN_POINT('Ctrl Pts',(-0.121653828529178,2.39843207826192,
11.9761339799187));
#39214=CARTESIAN_POINT('Ctrl Pts',(-0.120916895736116,2.3987313416272,11.9760852639237));
#39215=CARTESIAN_POINT('Ctrl Pts',(-0.120576843290157,2.39886875883114,
11.9760627801999));
#39216=CARTESIAN_POINT('Ctrl Pts',(-0.119872197041766,2.39915211218997,
11.9760161813597));
#39217=CARTESIAN_POINT('Ctrl Pts',(-0.119507569749674,2.39929796294278,
11.9759920634093));
#39218=CARTESIAN_POINT('Ctrl Pts',(-0.118679023955847,2.39962762540449,
11.9759372485525));
#39219=CARTESIAN_POINT('Ctrl Pts',(-0.118214944108632,2.39981102651099,
11.9759065378809));
#39220=CARTESIAN_POINT('Ctrl Pts',(-0.11684074205851,2.40035041480111,11.9758155744021));
#39221=CARTESIAN_POINT('Ctrl Pts',(-0.115929430559339,2.4007033384791,11.9757552188162));
#39222=CARTESIAN_POINT('Ctrl Pts',(-0.109744237766218,2.40306638271131,
11.9753453398858));
#39223=CARTESIAN_POINT('Ctrl Pts',(-0.104420227298461,2.40494169881607,
11.9749913361187));
#39224=CARTESIAN_POINT('Ctrl Pts',(-0.0974708942640044,2.40718618789567,
11.9745273348628));
#39225=CARTESIAN_POINT('Ctrl Pts',(-0.095887912713916,2.40768398933973,
11.9744215150012));
#39226=CARTESIAN_POINT('Ctrl Pts',(-0.0914388700455854,2.40904541519539,
11.9741237455252));
#39227=CARTESIAN_POINT('Ctrl Pts',(-0.0885645721769404,2.40988135027313,
11.9739309561341));
#39228=CARTESIAN_POINT('Ctrl Pts',(-0.0820986371681164,2.41166453804147,
11.9734963474253));
#39229=CARTESIAN_POINT('Ctrl Pts',(-0.078501463073567,2.4125899697296,11.9732539345335));
#39230=CARTESIAN_POINT('Ctrl Pts',(-0.0721577895715706,2.41410558018112,
11.9728254524368));
#39231=CARTESIAN_POINT('Ctrl Pts',(-0.0694180200938113,2.41472241732074,
11.9726400777879));
#39232=CARTESIAN_POINT('Ctrl Pts',(-0.0497333249290104,2.41888472719661,
11.9713062976586));
#39233=CARTESIAN_POINT('Ctrl Pts',(-0.0325357846113654,2.42109535475346,
11.9701288366965));
#39234=CARTESIAN_POINT('Ctrl Pts',(-0.0129550453979711,2.42202266975356,
11.9688060154347));
#39235=CARTESIAN_POINT('Ctrl Pts',(-0.0106635950950383,2.42210669188842,
11.968651522797));
#39236=CARTESIAN_POINT('Ctrl Pts',(-0.00554141373540266,2.42223979072454,
11.9683070914584));
#39237=CARTESIAN_POINT('Ctrl Pts',(-0.00271051037756672,2.42227603640808,
11.9681173549484));
#39238=CARTESIAN_POINT('Ctrl Pts',(0.00803423608660622,2.4222720173494,
11.9674003142077));
#39239=CARTESIAN_POINT('Ctrl Pts',(0.0159457664539845,2.42197756729501,
11.9668786904721));
#39240=CARTESIAN_POINT('Ctrl Pts',(0.0276290591701246,2.42111096898884,
11.9661249527688));
#39241=CARTESIAN_POINT('Ctrl Pts',(0.0314140744901395,2.42076280706022,
11.9658833633901));
#39242=CARTESIAN_POINT('Ctrl Pts',(0.0357254596148987,2.42028917388723,
11.9656118155341));
#39243=CARTESIAN_POINT('Ctrl Pts',(0.0362585317030203,2.42022926515651,
11.9655783042387));
#39244=CARTESIAN_POINT('Ctrl Pts',(0.0370620921066239,2.42013692564997,
11.9655278874057));
#39245=CARTESIAN_POINT('Ctrl Pts',(0.0373326895944099,2.4201054828098,11.9655109264933));
#39246=CARTESIAN_POINT('Ctrl Pts',(0.0378200001968005,2.42004823205267,
11.9654804128906));
#39247=CARTESIAN_POINT('Ctrl Pts',(0.0380367264602394,2.42002254716826,
11.9654668532796));
#39248=CARTESIAN_POINT('Ctrl Pts',(0.0384704854097021,2.41997069422731,
11.9654397369456));
#39249=CARTESIAN_POINT('Ctrl Pts',(0.038687516599473,2.41994452561657,11.9654261803138));
#39250=CARTESIAN_POINT('Ctrl Pts',(0.0393017456622678,2.41986983060792,
11.9653878438923));
#39251=CARTESIAN_POINT('Ctrl Pts',(0.0396988817924841,2.41982078502464,
11.9653630935129));
#39252=CARTESIAN_POINT('Ctrl Pts',(0.0413596164800909,2.41961254632039,
11.9652597415022));
#39253=CARTESIAN_POINT('Ctrl Pts',(0.0426223791567534,2.41944660048657,
11.965181516215));
#39254=CARTESIAN_POINT('Ctrl Pts',(0.0656285555145804,2.41628439778233,
11.9637623600202));
#39255=CARTESIAN_POINT('Ctrl Pts',(0.0870146435547348,2.41108150852532,
11.9625391361374));
#39256=CARTESIAN_POINT('Ctrl Pts',(0.118644368864585,2.39986550952689,11.9606632941634));
#39257=CARTESIAN_POINT('Ctrl Pts',(0.129362706452983,2.39539987749009,11.9600154592711));
#39258=CARTESIAN_POINT('Ctrl Pts',(0.149846322273975,2.38553664431393,11.9587220616112));
#39259=CARTESIAN_POINT('Ctrl Pts',(0.159618264070581,2.38019113242853,11.9580783635133));
#39260=CARTESIAN_POINT('Ctrl Pts',(0.172112886572602,2.37249020127256,11.9572064947208));
#39261=CARTESIAN_POINT('Ctrl Pts',(0.175101251650892,2.37057957370505,11.9569941250499));
#39262=CARTESIAN_POINT('Ctrl Pts',(0.179298777869239,2.36779720318224,11.9566900088476));
#39263=CARTESIAN_POINT('Ctrl Pts',(0.180534430457346,2.36696575263963,11.9565997545202));
#39264=CARTESIAN_POINT('Ctrl Pts',(0.18269063448116,2.36549306242653,11.956440952947));
#39265=CARTESIAN_POINT('Ctrl Pts',(0.183613689926892,2.36485552088893,11.9563725457064));
#39266=CARTESIAN_POINT('Ctrl Pts',(0.184960819494214,2.36391465039563,11.9562720776961));
#39267=CARTESIAN_POINT('Ctrl Pts',(0.185387523140706,2.36361508625291,11.9562401607777));
#39268=CARTESIAN_POINT('Ctrl Pts',(0.186138175792319,2.36308537216911,11.9561838467203));
#39269=CARTESIAN_POINT('Ctrl Pts',(0.186462430353594,2.36285565544799,11.9561594662344));
#39270=CARTESIAN_POINT('Ctrl Pts',(0.187088670521513,2.36241025647235,11.9561122730182));
#39271=CARTESIAN_POINT('Ctrl Pts',(0.187390710258606,2.36219465106362,11.9560894632697));
#39272=CARTESIAN_POINT('Ctrl Pts',(0.188106955742959,2.36168150283269,11.9560352582659));
#39273=CARTESIAN_POINT('Ctrl Pts',(0.188520827984663,2.36138349820688,11.9560038452117));
#39274=CARTESIAN_POINT('Ctrl Pts',(0.189758048427826,2.36048818277634,11.9559096642018));
#39275=CARTESIAN_POINT('Ctrl Pts',(0.190579272037186,2.35988795920743,11.9558467834665));
#39276=CARTESIAN_POINT('Ctrl Pts',(0.198611418216968,2.35395880594021,11.9552281264419));
#39277=CARTESIAN_POINT('Ctrl Pts',(0.205599182870998,2.34833550035663,11.9546608298194));
#39278=CARTESIAN_POINT('Ctrl Pts',(0.215792649082532,2.33940705662627,11.9537867181084));
#39279=CARTESIAN_POINT('Ctrl Pts',(0.219177335534874,2.33631229050391,11.9534881547959));
#39280=CARTESIAN_POINT('Ctrl Pts',(0.240198806576647,2.31625122664893,11.9515807817846));
#39281=CARTESIAN_POINT('Ctrl Pts',(0.255919977060544,2.2973950444249,11.9499025030514));
#39282=CARTESIAN_POINT('Ctrl Pts',(0.274221513907964,2.26953564094756,11.9476714303976));
#39283=CARTESIAN_POINT('Ctrl Pts',(0.278781701335296,2.26192764082981,11.9470852370471));
#39284=CARTESIAN_POINT('Ctrl Pts',(0.284876502130722,2.2507367822357,11.9462649820303));
#39285=CARTESIAN_POINT('Ctrl Pts',(0.286668896460554,2.2472995116246,11.9460185119031));
#39286=CARTESIAN_POINT('Ctrl Pts',(0.288639446878408,2.24334830220079,11.945742071343));
#39287=CARTESIAN_POINT('Ctrl Pts',(0.288878748693808,2.24286544229179,11.9457084045001));
#39288=CARTESIAN_POINT('Ctrl Pts',(0.289237420356777,2.2421371337116,11.9456578007575));
#39289=CARTESIAN_POINT('Ctrl Pts',(0.289357689908607,2.24189213299711,11.9456408078689));
#39290=CARTESIAN_POINT('Ctrl Pts',(0.289573588557877,2.24145091050229,11.9456102597804));
#39291=CARTESIAN_POINT('Ctrl Pts',(0.289669329322274,2.24125474478102,11.9455966975893));
#39292=CARTESIAN_POINT('Ctrl Pts',(0.289874623182387,2.2408330264342,11.9455675831521));
#39293=CARTESIAN_POINT('Ctrl Pts',(0.28998411203079,2.24060744386585,11.9455520349794));
#39294=CARTESIAN_POINT('Ctrl Pts',(0.290278236130656,2.23999964796404,11.9455102109881));
#39295=CARTESIAN_POINT('Ctrl Pts',(0.290462380528173,2.23961719558844,11.9454839658433));
#39296=CARTESIAN_POINT('Ctrl Pts',(0.291305975726576,2.2378562269276,11.9453634499451));
#39297=CARTESIAN_POINT('Ctrl Pts',(0.291956386253598,2.23647336567625,11.9452697327507));
#39298=CARTESIAN_POINT('Ctrl Pts',(0.304726851911641,2.2088124524726,11.9434124367505));
#39299=CARTESIAN_POINT('Ctrl Pts',(0.313265033822044,2.18102005787011,11.9418480231226));
#39300=CARTESIAN_POINT('Ctrl Pts',(0.319877595125289,2.14093683388401,11.9395615871811));
#39301=CARTESIAN_POINT('Ctrl Pts',(0.321150507915636,2.12932269053951,11.9388969874046));
#39302=CARTESIAN_POINT('Ctrl Pts',(0.322233993380862,2.10958648611679,11.9377420710263));
#39303=CARTESIAN_POINT('Ctrl Pts',(0.322373073651035,2.10149394643532,11.9372613957773));
#39304=CARTESIAN_POINT('Ctrl Pts',(0.322173910703158,2.09176324702142,11.9366715175432));
#39305=CARTESIAN_POINT('Ctrl Pts',(0.32212775328657,2.09012157682071,11.9365715954554));
#39306=CARTESIAN_POINT('Ctrl Pts',(0.322047378265076,2.08787443243656,11.9364342451967));
#39307=CARTESIAN_POINT('Ctrl Pts',(0.322023996115217,2.08726857611234,11.9363971567013));
#39308=CARTESIAN_POINT('Ctrl Pts',(0.321983755255769,2.08629704494426,11.9363375897542));
#39309=CARTESIAN_POINT('Ctrl Pts',(0.321967982872494,2.08593132454236,11.9363151453895));
#39310=CARTESIAN_POINT('Ctrl Pts',(0.321933864762426,2.08517033656856,11.9362683989866));
#39311=CARTESIAN_POINT('Ctrl Pts',(0.321915414108091,2.08477507452373,11.9362440936967));
#39312=CARTESIAN_POINT('Ctrl Pts',(0.32187139489396,2.08386793737798,11.9361882547772));
#39313=CARTESIAN_POINT('Ctrl Pts',(0.321845333184344,2.08335608825896,11.9361567057334));
#39314=CARTESIAN_POINT('Ctrl Pts',(0.321772795567957,2.0819953788594,11.9360727220935));
#39315=CARTESIAN_POINT('Ctrl Pts',(0.321724181835174,2.0811466408737,11.9360202205443));
#39316=CARTESIAN_POINT('Ctrl Pts',(0.321374123720412,2.07543125128269,11.9356658759686));
#39317=CARTESIAN_POINT('Ctrl Pts',(0.320965637089675,2.07057201302788,11.9353606890644));
#39318=CARTESIAN_POINT('Ctrl Pts',(0.317382656091595,2.03707452902304,11.9332282390498));
#39319=CARTESIAN_POINT('Ctrl Pts',(0.310490344103112,2.00897009183596,11.9312768499659));
#39320=CARTESIAN_POINT('Ctrl Pts',(0.293935448393333,1.96682886709923,11.928219449767));
#39321=CARTESIAN_POINT('Ctrl Pts',(0.286743730421849,1.95197712001772,11.9271176273678));
#39322=CARTESIAN_POINT('Ctrl Pts',(0.277838680573019,1.93669567842793,11.9260022555656));
#39323=CARTESIAN_POINT('Ctrl Pts',(0.277224811596123,1.935655733864,11.9259264530588));
#39324=CARTESIAN_POINT('Ctrl Pts',(0.276411782096375,1.93429591357351,11.9258274934217));
#39325=CARTESIAN_POINT('Ctrl Pts',(0.27621789595906,1.93397291939105,11.9258039996525));
#39326=CARTESIAN_POINT('Ctrl Pts',(0.275900799351741,1.93344676227582,11.9257657485936));
#39327=CARTESIAN_POINT('Ctrl Pts',(0.275777930468778,1.93324339549339,11.9257509689941));
#39328=CARTESIAN_POINT('Ctrl Pts',(0.275540149903792,1.93285081387444,11.9257224481303));
#39329=CARTESIAN_POINT('Ctrl Pts',(0.275425268459795,1.93266158203951,11.9257087049925));
#39330=CARTESIAN_POINT('Ctrl Pts',(0.275158244064802,1.93222276140732,11.9256768452976));
#39331=CARTESIAN_POINT('Ctrl Pts',(0.275005955934355,1.93197326025641,11.9256587383154));
#39332=CARTESIAN_POINT('Ctrl Pts',(0.274511638028437,1.93116586708348,11.9256001668896));
#39333=CARTESIAN_POINT('Ctrl Pts',(0.274168245624862,1.93060880495312,11.925559791547));
#39334=CARTESIAN_POINT('Ctrl Pts',(0.270822938636907,1.92521876355081,11.9251694378927));
#39335=CARTESIAN_POINT('Ctrl Pts',(0.267695012077192,1.92046466943811,11.9248275714058));
#39336=CARTESIAN_POINT('Ctrl Pts',(0.263723836559744,1.91476367782538,11.9244174082025));
#39337=CARTESIAN_POINT('Ctrl Pts',(0.262999016781653,1.91373600917549,11.9243434634037));
#39338=CARTESIAN_POINT('Ctrl Pts',(0.259908487766431,1.90940818233584,11.9240319053703));
#39339=CARTESIAN_POINT('Ctrl Pts',(0.257486461069764,1.90614854232988,11.923796862455));
#39340=CARTESIAN_POINT('Ctrl Pts',(0.241403616829571,1.88533719064967,11.9222876757143));
#39341=CARTESIAN_POINT('Ctrl Pts',(0.226018265692793,1.86919343733556,11.9210727650098));
#39342=CARTESIAN_POINT('Ctrl Pts',(0.203039153480014,1.8496012106097,11.919360444021));
#39343=CARTESIAN_POINT('Ctrl Pts',(0.196797310161656,1.84466637698704,11.9189045709676));
#39344=CARTESIAN_POINT('Ctrl Pts',(0.18346821157641,1.834907634253,11.9179415332678));
#39345=CARTESIAN_POINT('Ctrl Pts',(0.176358382874251,1.8301254954577,11.9174334940673));
#39346=CARTESIAN_POINT('Ctrl Pts',(0.168091796792566,1.82503157355596,11.9168452059578));
#39347=CARTESIAN_POINT('Ctrl Pts',(0.167113432252009,1.82443587243894,11.9167756205313));
#39348=CARTESIAN_POINT('Ctrl Pts',(0.165352478042518,1.82337649948574,11.9166504341912));
#39349=CARTESIAN_POINT('Ctrl Pts',(0.164571058276077,1.8229108991988,11.9165949041077));
#39350=CARTESIAN_POINT('Ctrl Pts',(0.16337790477558,1.82220679948755,11.9165101429544));
#39351=CARTESIAN_POINT('Ctrl Pts',(0.162967592202825,1.82196589074799,11.916480999531));
#39352=CARTESIAN_POINT('Ctrl Pts',(0.1622509499628,1.82154725663906,11.9164301064376));
#39353=CARTESIAN_POINT('Ctrl Pts',(0.161944857281851,1.82136912545912,11.916408371524));
#39354=CARTESIAN_POINT('Ctrl Pts',(0.161310069617872,1.82100110903089,11.9163633018003));
#39355=CARTESIAN_POINT('Ctrl Pts',(0.160981331649354,1.82081129933216,11.9163399642999));
#39356=CARTESIAN_POINT('Ctrl Pts',(0.160182699637211,1.82035205747829,11.9162832748212));
#39357=CARTESIAN_POINT('Ctrl Pts',(0.159712461410356,1.8200832290051,11.9162499011231));
#39358=CARTESIAN_POINT('Ctrl Pts',(0.157950626792031,1.81908189822436,11.9161248785518));
#39359=CARTESIAN_POINT('Ctrl Pts',(0.156654666138279,1.81835714838134,11.9160329514677));
#39360=CARTESIAN_POINT('Ctrl Pts',(0.133439502823702,1.80558416115297,11.9143867113656));
#39361=CARTESIAN_POINT('Ctrl Pts',(0.110200969260311,1.79612169339898,11.9127363379));
#39362=CARTESIAN_POINT('Ctrl Pts',(0.0707623468615258,1.78518663572277,
11.9099726590372));
#39363=CARTESIAN_POINT('Ctrl Pts',(0.0551221973562432,1.78207494965335,
11.9088882984734));
#39364=CARTESIAN_POINT('Ctrl Pts',(0.0315516128561676,1.779177831656,11.9073169586769));
#39365=CARTESIAN_POINT('Ctrl Pts',(0.0237545825445637,1.77850643877727,
11.9068074961154));
#39366=CARTESIAN_POINT('Ctrl Pts',(0.0142754796270235,1.778037013981,11.9062065198696));
#39367=CARTESIAN_POINT('Ctrl Pts',(0.0126101110209586,1.77796748755945,
11.9061016240386));
#39368=CARTESIAN_POINT('Ctrl Pts',(0.0105217368608655,1.77789652688921,
11.9059710106224));
#39369=CARTESIAN_POINT('Ctrl Pts',(0.0100992070245002,1.77788300206456,
11.9059446317987));
#39370=CARTESIAN_POINT('Ctrl Pts',(0.00942886095272575,1.77786286513284,
11.9059028583119));
#39371=CARTESIAN_POINT('Ctrl Pts',(0.00918106346136307,1.77785570755638,
11.9058874331075));
#39372=CARTESIAN_POINT('Ctrl Pts',(0.00871468133577316,1.77784277477254,
11.9058584327669));
#39373=CARTESIAN_POINT('Ctrl Pts',(0.00849610084225586,1.7778369361521,
11.9058448542011));
#39374=CARTESIAN_POINT('Ctrl Pts',(0.00800045058094651,1.77782420135971,
11.9058140931454));
#39375=CARTESIAN_POINT('Ctrl Pts',(0.00772337830367184,1.77781744015548,
11.9057969183637));
#39376=CARTESIAN_POINT('Ctrl Pts',(0.00700960772429537,1.77780094378876,
11.9057527271239));
#39377=CARTESIAN_POINT('Ctrl Pts',(0.00657289594078645,1.77779173898219,
11.9057257403628));
#39378=CARTESIAN_POINT('Ctrl Pts',(0.00400707394892082,1.77774287649343,
11.9055674776781));
#39379=CARTESIAN_POINT('Ctrl Pts',(0.00187756722605931,1.77772343304744,
11.9054373134188));
#39380=CARTESIAN_POINT('Ctrl Pts',(-0.00065529111074268,1.77772541392767,
11.9052837398627));
#39381=CARTESIAN_POINT('Ctrl Pts',(-0.00105854100558473,1.77772648615029,
11.9052593273473));
#39382=CARTESIAN_POINT('Ctrl Pts',(-0.0366183193238867,1.77788778151695,
11.9031097860917));
#39383=CARTESIAN_POINT('Ctrl Pts',(-0.0715175642871153,1.78379852313034,
11.9012563065549));
#39384=CARTESIAN_POINT('Ctrl Pts',(-0.116042493295097,1.7991059675031,11.898551640593));
#39385=CARTESIAN_POINT('Ctrl Pts',(-0.127083108591905,1.80360007727022,
11.897853004082));
#39386=CARTESIAN_POINT('Ctrl Pts',(-0.139739951603399,1.80958943099496,
11.8970066206193));
#39387=CARTESIAN_POINT('Ctrl Pts',(-0.14162224708126,1.81050269176417,11.8968795397269));
#39388=CARTESIAN_POINT('Ctrl Pts',(-0.144093078184212,1.8117313650917,11.8967110762267));
#39389=CARTESIAN_POINT('Ctrl Pts',(-0.144689744782218,1.81203038563627,
11.8966702672072));
#39390=CARTESIAN_POINT('Ctrl Pts',(-0.145664783290114,1.81252282332818,
11.8966033683572));
#39391=CARTESIAN_POINT('Ctrl Pts',(-0.146043711151618,1.8127151402728,11.8965773171863));
#39392=CARTESIAN_POINT('Ctrl Pts',(-0.146775110598325,1.8130881678518,11.8965269319488));
#39393=CARTESIAN_POINT('Ctrl Pts',(-0.147127631751823,1.81326878005585,
11.8965026013804));
#39394=CARTESIAN_POINT('Ctrl Pts',(-0.147937782849754,1.81368574377397,
11.8964465798531));
#39395=CARTESIAN_POINT('Ctrl Pts',(-0.148395180061732,1.81392254293234,
11.8964148731453));
#39396=CARTESIAN_POINT('Ctrl Pts',(-0.149613656567506,1.81455706906073,
11.8963301993365));
#39397=CARTESIAN_POINT('Ctrl Pts',(-0.150373713274924,1.81495674119924,
11.8962771635227));
#39398=CARTESIAN_POINT('Ctrl Pts',(-0.155575117868523,1.81771846815806,
11.8959127037637));
#39399=CARTESIAN_POINT('Ctrl Pts',(-0.159962018908159,1.82018107924266,
11.8955977164679));
#39400=CARTESIAN_POINT('Ctrl Pts',(-0.174994238743154,1.82908852910586,
11.8944908398537));
#39401=CARTESIAN_POINT('Ctrl Pts',(-0.185321587955848,1.83604573378236,
11.8936806876661));
#39402=CARTESIAN_POINT('Ctrl Pts',(-0.200867946695899,1.84788170905821,
11.8923831625068));
#39403=CARTESIAN_POINT('Ctrl Pts',(-0.20637206961328,1.85236695200649,11.8919070608736));
#39404=CARTESIAN_POINT('Ctrl Pts',(-0.221380114951674,1.86544492897593,
11.8905648244737));
#39405=CARTESIAN_POINT('Ctrl Pts',(-0.230526544731307,1.8744279470857,11.8896938002725));
#39406=CARTESIAN_POINT('Ctrl Pts',(-0.245737109347077,1.89126085027975,
11.8881718151932));
#39407=CARTESIAN_POINT('Ctrl Pts',(-0.252020209061949,1.89889155219584,
11.8875170386819));
#39408=CARTESIAN_POINT('Ctrl Pts',(-0.260202234508694,1.90981542739261,
11.8866391297362));
#39409=CARTESIAN_POINT('Ctrl Pts',(-0.262408250939913,1.91287093380066,
11.8863996301579));
#39410=CARTESIAN_POINT('Ctrl Pts',(-0.264865990412456,1.91640405958182,
11.8861301793369));
#39411=CARTESIAN_POINT('Ctrl Pts',(-0.265170604581527,1.91684429386207,
11.8860967359273));
#39412=CARTESIAN_POINT('Ctrl Pts',(-0.265628443912795,1.91750950847004,
11.8860464006907));
#39413=CARTESIAN_POINT('Ctrl Pts',(-0.265782481415698,1.91773392447248,
11.8860294537558));
#39414=CARTESIAN_POINT('Ctrl Pts',(-0.266059503015643,1.91813861294209,
11.8859989552017));
#39415=CARTESIAN_POINT('Ctrl Pts',(-0.266182588033365,1.91831881474309,
11.8859853966925));
#39416=CARTESIAN_POINT('Ctrl Pts',(-0.266447006046569,1.91870677968211,
11.8859562533954));
#39417=CARTESIAN_POINT('Ctrl Pts',(-0.26658827868847,1.91891458249941,11.8859406727577));
#39418=CARTESIAN_POINT('Ctrl Pts',(-0.266968811070454,1.91947573116585,
11.8858986769967));
#39419=CARTESIAN_POINT('Ctrl Pts',(-0.267207613336945,1.91982938890535,
11.8858722929777));
#39420=CARTESIAN_POINT('Ctrl Pts',(-0.268310350832387,1.92146951900206,
11.8857503142456));
#39421=CARTESIAN_POINT('Ctrl Pts',(-0.269165721194187,1.92276176549964,
11.8856552895133));
#39422=CARTESIAN_POINT('Ctrl Pts',(-0.28737175625935,1.95070224543244,11.8836227082783));
#39423=CARTESIAN_POINT('Ctrl Pts',(-0.300696424273517,1.97977187474693,
11.8819234881039));
#39424=CARTESIAN_POINT('Ctrl Pts',(-0.313957892892305,2.02554999157407,
11.8792231192045));
#39425=CARTESIAN_POINT('Ctrl Pts',(-0.317238355945099,2.04107556579118,
11.8783059865185));
#39426=CARTESIAN_POINT('Ctrl Pts',(-0.319697177946093,2.05924365070786,
11.8772003247134));
#39427=CARTESIAN_POINT('Ctrl Pts',(-0.320002281765058,2.06171286477267,
11.877049409315));
#39428=CARTESIAN_POINT('Ctrl Pts',(-0.320357813053041,2.0648922619779,11.876854181309));
#39429=CARTESIAN_POINT('Ctrl Pts',(-0.320434525303831,2.06559946753773,
11.8768106984734));
#39430=CARTESIAN_POINT('Ctrl Pts',(-0.320554346822314,2.06673928197126,
11.8767405218595));
#39431=CARTESIAN_POINT('Ctrl Pts',(-0.320598923534733,2.06717173693439,
11.8767138743448));
#39432=CARTESIAN_POINT('Ctrl Pts',(-0.320682150337311,2.06799548956898,
11.8766630731254));
#39433=CARTESIAN_POINT('Ctrl Pts',(-0.320720959654002,2.06838677065958,
11.8766389244815));
#39434=CARTESIAN_POINT('Ctrl Pts',(-0.320807797281842,2.06927890001303,
11.8765838232452));
#39435=CARTESIAN_POINT('Ctrl Pts',(-0.320855368868727,2.06977979078873,
11.8765528563386));
#39436=CARTESIAN_POINT('Ctrl Pts',(-0.320996839248251,2.07130735806691,
11.8764583238351));
#39437=CARTESIAN_POINT('Ctrl Pts',(-0.321086983976121,2.07233436807111,
11.8763946403649));
#39438=CARTESIAN_POINT('Ctrl Pts',(-0.321706261765551,2.07980088929458,
11.8759307027241));
#39439=CARTESIAN_POINT('Ctrl Pts',(-0.322046527493159,2.08625418908253,
11.8755245499221));
#39440=CARTESIAN_POINT('Ctrl Pts',(-0.322248915265885,2.0952027048059,11.8749536251292));
#39441=CARTESIAN_POINT('Ctrl Pts',(-0.322276363226365,2.09769292396946,
11.8747939240554));
#39442=CARTESIAN_POINT('Ctrl Pts',(-0.322270555415569,2.10791201595138,
11.8741351782895));
#39443=CARTESIAN_POINT('Ctrl Pts',(-0.321988134303093,2.11563770899795,
11.8736291397252));
#39444=CARTESIAN_POINT('Ctrl Pts',(-0.319228571217128,2.15363251957197,
11.8711043324824));
#39445=CARTESIAN_POINT('Ctrl Pts',(-0.312759663303515,2.18345402603753,
11.8689914748367));
#39446=CARTESIAN_POINT('Ctrl Pts',(-0.300887051948024,2.21551082881476,
11.8667907638231));
#39447=CARTESIAN_POINT('Ctrl Pts',(-0.299496599585889,2.21906955794002,
11.8665477661154));
#39448=CARTESIAN_POINT('Ctrl Pts',(-0.297820304106974,2.22314457004338,
11.8662717236344));
#39449=CARTESIAN_POINT('Ctrl Pts',(-0.297596008258828,2.22368562790708,
11.8662351175877));
#39450=CARTESIAN_POINT('Ctrl Pts',(-0.297261395007878,2.22448661932958,
11.8661809959303));
#39451=CARTESIAN_POINT('Ctrl Pts',(-0.297152210597528,2.22474702037566,
11.8661634121434));
#39452=CARTESIAN_POINT('Ctrl Pts',(-0.296957647339344,2.22520934219326,
11.8661322136254));
#39453=CARTESIAN_POINT('Ctrl Pts',(-0.296872404712535,2.22541131929409,
11.8661185906067));
#39454=CARTESIAN_POINT('Ctrl Pts',(-0.296691548199762,2.22583862987168,
11.8660897838495));
#39455=CARTESIAN_POINT('Ctrl Pts',(-0.29659588393765,2.2260639408132,11.8660746032867));
#39456=CARTESIAN_POINT('Ctrl Pts',(-0.296339774721068,2.22666523060811,
11.8660341130841));
#39457=CARTESIAN_POINT('Ctrl Pts',(-0.296178870294943,2.22704101511689,
11.8660088315012));
#39458=CARTESIAN_POINT('Ctrl Pts',(-0.295419290077363,2.2288056912485,11.8658902148768));
#39459=CARTESIAN_POINT('Ctrl Pts',(-0.294811544391363,2.23019069303091,
11.8657974254289));
#39460=CARTESIAN_POINT('Ctrl Pts',(-0.289818244037389,2.24135572833373,
11.8650514974071));
#39461=CARTESIAN_POINT('Ctrl Pts',(-0.284956528384057,2.25091681558778,
11.8644256341339));
#39462=CARTESIAN_POINT('Ctrl Pts',(-0.265242888201808,2.28532265671748,
11.8621581376671));
#39463=CARTESIAN_POINT('Ctrl Pts',(-0.247544435414865,2.30837503945137,
11.8605954716918));
#39464=CARTESIAN_POINT('Ctrl Pts',(-0.220045814899674,2.33566324066035,
11.8583413584187));
#39465=CARTESIAN_POINT('Ctrl Pts',(-0.212774722407434,2.34224824413426,
11.857759612165));
#39466=CARTESIAN_POINT('Ctrl Pts',(-0.20441278130814,2.34915391581625,11.8571001647116));
#39467=CARTESIAN_POINT('Ctrl Pts',(-0.203607056224353,2.34981278098728,
11.8570367193307));
#39468=CARTESIAN_POINT('Ctrl Pts',(-0.202397177231539,2.35079239316756,
11.8569415871785));
#39469=CARTESIAN_POINT('Ctrl Pts',(-0.201995416286347,2.35111609589277,
11.8569100194504));
#39470=CARTESIAN_POINT('Ctrl Pts',(-0.201302132478617,2.35167194114552,
11.8568555836928));
#39471=CARTESIAN_POINT('Ctrl Pts',(-0.20101098023509,2.3519045460555,11.856832734255));
#39472=CARTESIAN_POINT('Ctrl Pts',(-0.200409235424575,2.35238357945124,
11.8567855329958));
#39473=CARTESIAN_POINT('Ctrl Pts',(-0.200098590349256,2.35262994073968,
11.8567611785416));
#39474=CARTESIAN_POINT('Ctrl Pts',(-0.199374434279252,2.35320206890304,
11.8567044341658));
#39475=CARTESIAN_POINT('Ctrl Pts',(-0.19896057903664,2.35352739639951,11.8566720268184));
#39476=CARTESIAN_POINT('Ctrl Pts',(-0.197638999398129,2.35456104814156,
11.8565686080163));
#39477=CARTESIAN_POINT('Ctrl Pts',(-0.196728283014751,2.3552655165136,11.8564974439261));
#39478=CARTESIAN_POINT('Ctrl Pts',(-0.176932844179349,2.37040906841153,
11.8549527444143));
#39479=CARTESIAN_POINT('Ctrl Pts',(-0.156515893223953,2.38271651318578,
11.8533929135579));
#39480=CARTESIAN_POINT('Ctrl Pts',(-0.113880288591816,2.40237402684906,
11.8502296219761));
#39481=CARTESIAN_POINT('Ctrl Pts',(-0.0918373759162351,2.40978183189838,
11.848638928633));
#39482=CARTESIAN_POINT('Ctrl Pts',(-0.0655494903571434,2.41556034238662,
11.846907275142));
#39483=CARTESIAN_POINT('Ctrl Pts',(-0.0618956947351822,2.41629731474561,
11.8466703110782));
#39484=CARTESIAN_POINT('Ctrl Pts',(-0.0576578814998444,2.41707583066751,
11.8464003970775));
#39485=CARTESIAN_POINT('Ctrl Pts',(-0.0570857268370138,2.41717933964332,
11.8463640589082));
#39486=CARTESIAN_POINT('Ctrl Pts',(-0.0562361318703206,2.41733066720835,
11.8463102567767));
#39487=CARTESIAN_POINT('Ctrl Pts',(-0.055958908008866,2.41737967089047,
11.8462927257952));
#39488=CARTESIAN_POINT('Ctrl Pts',(-0.055465785993254,2.41746617178284,
11.8462615863096));
#39489=CARTESIAN_POINT('Ctrl Pts',(-0.0552499138917325,2.41750381203751,
11.8462479696333));
#39490=CARTESIAN_POINT('Ctrl Pts',(-0.0547923474488468,2.41758311421874,
11.8462191396645));
#39491=CARTESIAN_POINT('Ctrl Pts',(-0.0545506445750195,2.41762472031194,
11.8462039296216));
#39492=CARTESIAN_POINT('Ctrl Pts',(-0.0539038505679594,2.41773529765177,
11.8461632779111));
#39493=CARTESIAN_POINT('Ctrl Pts',(-0.0534986729228843,2.41780377039904,
11.8461378646954));
#39494=CARTESIAN_POINT('Ctrl Pts',(-0.0515792134044037,2.41812437344344,
11.8460177184478));
#39495=CARTESIAN_POINT('Ctrl Pts',(-0.0500632410114724,2.41836646235672,
11.8459235482739));
#39496=CARTESIAN_POINT('Ctrl Pts',(-0.0376624745739469,2.42025599935117,
11.8451586826571));
#39497=CARTESIAN_POINT('Ctrl Pts',(-0.0267002706111915,2.4213557501579,
11.8445167428276));
#39498=CARTESIAN_POINT('Ctrl Pts',(0.0135194310577731,2.42331769512947,
11.842217052745));
#39499=CARTESIAN_POINT('Ctrl Pts',(0.0427983435519015,2.42075773510434,
11.8406367004223));
#39500=CARTESIAN_POINT('Ctrl Pts',(0.0802973369684861,2.4122467786152,11.8383934724666));
#39501=CARTESIAN_POINT('Ctrl Pts',(0.0891717756257766,2.40982911904033,
11.8378470192701));
#39502=CARTESIAN_POINT('Ctrl Pts',(0.0990138853554707,2.40668994128337,
11.83721875536));
#39503=CARTESIAN_POINT('Ctrl Pts',(0.100095767115053,2.40633854953513,11.8371493901617));
#39504=CARTESIAN_POINT('Ctrl Pts',(0.101667709352083,2.40581877146511,11.8370481535422));
#39505=CARTESIAN_POINT('Ctrl Pts',(0.10215926827498,2.40565491654134,11.8370164316362));
#39506=CARTESIAN_POINT('Ctrl Pts',(0.103026369990979,2.40536355382041,11.8369603601126));
#39507=CARTESIAN_POINT('Ctrl Pts',(0.10340207749022,2.40523653661353,11.8369360267526));
#39508=CARTESIAN_POINT('Ctrl Pts',(0.10417863280432,2.40497240460708,11.8368856525873));
#39509=CARTESIAN_POINT('Ctrl Pts',(0.104579446438932,2.40483519233284,11.8368596085937));
#39510=CARTESIAN_POINT('Ctrl Pts',(0.105605491691137,2.40448167999215,11.8367928257547));
#39511=CARTESIAN_POINT('Ctrl Pts',(0.106230327678378,2.40426424501917,11.8367520493369));
#39512=CARTESIAN_POINT('Ctrl Pts',(0.108783064134468,2.4033671033407,11.8365850164294));
#39513=CARTESIAN_POINT('Ctrl Pts',(0.11070511296696,2.40267099643893,11.8364582158546));
#39514=CARTESIAN_POINT('Ctrl Pts',(0.12337020740203,2.39794731305084,11.8356156708809));
#39515=CARTESIAN_POINT('Ctrl Pts',(0.133897036181778,2.39336724464954,11.8348814183693));
#39516=CARTESIAN_POINT('Ctrl Pts',(0.173384447266412,2.37361830053667,11.8319919691008));
#39517=CARTESIAN_POINT('Ctrl Pts',(0.20021401765059,2.35464295234354,11.8297132051395));
#39518=CARTESIAN_POINT('Ctrl Pts',(0.223820563282745,2.33187398884641,11.8275827498975));
#39519=CARTESIAN_POINT('Ctrl Pts',(0.223910487995763,2.33178715369351,11.8275746325986));
#39520=CARTESIAN_POINT('Ctrl Pts',(0.224587525771665,2.33113261535554,11.8275135050623));
#39521=CARTESIAN_POINT('Ctrl Pts',(0.225172535203309,2.33056272905623,11.8274606134425));
#39522=CARTESIAN_POINT('Ctrl Pts',(0.228868849438541,2.3269344818775,11.8271259945453));
#39523=CARTESIAN_POINT('Ctrl Pts',(0.231920137138423,2.32381524516,11.8268478256322));
#39524=CARTESIAN_POINT('Ctrl Pts',(0.235318729695183,2.32019680333319,11.826536743448));
#39525=CARTESIAN_POINT('Ctrl Pts',(0.235728915309947,2.31975762840941,11.8264991768293));
#39526=CARTESIAN_POINT('Ctrl Pts',(0.236332876158374,2.31910734670439,11.8264438354462));
#39527=CARTESIAN_POINT('Ctrl Pts',(0.236527599090586,2.31889712790053,11.8264259885201));
#39528=CARTESIAN_POINT('Ctrl Pts',(0.236871632926425,2.31852472111335,11.8263944496167));
#39529=CARTESIAN_POINT('Ctrl Pts',(0.237021057964513,2.31836263944517,11.8263807488501));
#39530=CARTESIAN_POINT('Ctrl Pts',(0.237329638806674,2.31802723119061,11.8263524503036));
#39531=CARTESIAN_POINT('Ctrl Pts',(0.237488770718182,2.31785388401488,11.8263378543486));
#39532=CARTESIAN_POINT('Ctrl Pts',(0.237901403974315,2.31740340079807,11.8262999991705));
#39533=CARTESIAN_POINT('Ctrl Pts',(0.238154611878585,2.31712599461115,11.8262767624031));
#39534=CARTESIAN_POINT('Ctrl Pts',(0.238706149547586,2.31651962268942,11.8262261303214));
#39535=CARTESIAN_POINT('Ctrl Pts',(0.239004286038416,2.31619048106282,11.8261987495092));
#39536=CARTESIAN_POINT('Ctrl Pts',(0.239872085081427,2.31522844488519,11.8261190140058));
#39537=CARTESIAN_POINT('Ctrl Pts',(0.2404399261004,2.31459390173835,11.8260667926926));
#39538=CARTESIAN_POINT('Ctrl Pts',(0.246385238683807,2.30789699140745,11.8255194472551));
#39539=CARTESIAN_POINT('Ctrl Pts',(0.251535254983926,2.30163552543278,11.8250402261378));
#39540=CARTESIAN_POINT('Ctrl Pts',(0.269277213457459,2.27832533865867,11.8233426880013));
#39541=CARTESIAN_POINT('Ctrl Pts',(0.280416999083914,2.26023913398309,11.8221814407824));
#39542=CARTESIAN_POINT('Ctrl Pts',(0.298542592863542,2.22304784971495,11.8198526846149));
#39543=CARTESIAN_POINT('Ctrl Pts',(0.305659081035013,2.20411914012657,11.8186927081922));
#39544=CARTESIAN_POINT('Ctrl Pts',(0.31129948776745,2.18339956135352,11.8173884658584));
#39545=CARTESIAN_POINT('Ctrl Pts',(0.311632613360392,2.18214604148449,11.8173094466799));
#39546=CARTESIAN_POINT('Ctrl Pts',(0.312086506964273,2.18039557993601,11.8171989323084));
#39547=CARTESIAN_POINT('Ctrl Pts',(0.312213675894898,2.17990029838397,11.8171676441869));
#39548=CARTESIAN_POINT('Ctrl Pts',(0.312431186227086,2.17904471819236,11.8171135619049));
#39549=CARTESIAN_POINT('Ctrl Pts',(0.312522084726933,2.17868456111227,11.8170907857792));
#39550=CARTESIAN_POINT('Ctrl Pts',(0.312708885920893,2.17793898917356,11.8170436149003));
#39551=CARTESIAN_POINT('Ctrl Pts',(0.312804699175932,2.17755355271382,11.8170192173035));
#39552=CARTESIAN_POINT('Ctrl Pts',(0.313026880080136,2.17665265579953,11.8169621637914));
#39553=CARTESIAN_POINT('Ctrl Pts',(0.313152687137656,2.1761370594843,11.8169294898667));
#39554=CARTESIAN_POINT('Ctrl Pts',(0.313552818524207,2.17447942750916,11.8168243737746));
#39555=CARTESIAN_POINT('Ctrl Pts',(0.313822171094595,2.17333621204769,11.8167517718033));
#39556=CARTESIAN_POINT('Ctrl Pts',(0.317929441702056,2.15546662800753,11.8156151982127));
#39557=CARTESIAN_POINT('Ctrl Pts',(0.320430964654827,2.13846426944246,11.814507810578));
#39558=CARTESIAN_POINT('Ctrl Pts',(0.32340940612798,2.09359540284013,11.8115214745401));
#39559=CARTESIAN_POINT('Ctrl Pts',(0.321651678455091,2.06572533584755,11.8095952147709));
#39560=CARTESIAN_POINT('Ctrl Pts',(0.316251564346348,2.03798120625939,11.8077558457193));
#39561=CARTESIAN_POINT('Ctrl Pts',(0.316163671503912,2.03753468519169,11.807726266824));
#39562=CARTESIAN_POINT('Ctrl Pts',(0.315918033270298,2.03630057254475,11.807644585584));
#39563=CARTESIAN_POINT('Ctrl Pts',(0.315758287728039,2.03551337689361,11.8075925630766));
#39564=CARTESIAN_POINT('Ctrl Pts',(0.31470885956459,2.03043939853587,11.8072577891008));
#39565=CARTESIAN_POINT('Ctrl Pts',(0.313734789617186,2.02617026301319,11.8069786223044));
#39566=CARTESIAN_POINT('Ctrl Pts',(0.312528233197793,2.02133844065882,11.8066665375241));
#39567=CARTESIAN_POINT('Ctrl Pts',(0.312380864642385,2.02075523435039,11.8066289332662));
#39568=CARTESIAN_POINT('Ctrl Pts',(0.312160855341345,2.01989470557334,11.8065735468188));
#39569=CARTESIAN_POINT('Ctrl Pts',(0.312089477168177,2.01961706620777,11.8065556923005));
#39570=CARTESIAN_POINT('Ctrl Pts',(0.311962548595352,2.01912607030098,11.8065241446454));
#39571=CARTESIAN_POINT('Ctrl Pts',(0.311907149646376,2.0189126752709,11.8065104427027));
#39572=CARTESIAN_POINT('Ctrl Pts',(0.311792190058654,2.01847171548664,11.806482148169));
#39573=CARTESIAN_POINT('Ctrl Pts',(0.311732599388707,2.01824415961858,11.8064675573899));
#39574=CARTESIAN_POINT('Ctrl Pts',(0.311577572073877,2.0176547984642,11.8064297946059));
#39575=CARTESIAN_POINT('Ctrl Pts',(0.311481754019993,2.01729309248063,11.8064066447906));
#39576=CARTESIAN_POINT('Ctrl Pts',(0.311271150555932,2.01650363721059,11.8063561737966));
#39577=CARTESIAN_POINT('Ctrl Pts',(0.311156112707261,2.01607595518661,11.8063288671162));
#39578=CARTESIAN_POINT('Ctrl Pts',(0.310818159188337,2.01482977534973,11.8062494012246));
#39579=CARTESIAN_POINT('Ctrl Pts',(0.310592890925302,2.01401191133708,11.8061973743052));
#39580=CARTESIAN_POINT('Ctrl Pts',(0.302752942807692,1.98598081934197,11.804418264597));
#39581=CARTESIAN_POINT('Ctrl Pts',(0.291593767699802,1.95988076927474,11.8028850860857));
#39582=CARTESIAN_POINT('Ctrl Pts',(0.266333502687802,1.9173015023525,11.8001038637217));
#39583=CARTESIAN_POINT('Ctrl Pts',(0.253719553825934,1.90015390823077,11.7988873460262));
#39584=CARTESIAN_POINT('Ctrl Pts',(0.238642380658758,1.88340664937096,11.7975187104103));
#39585=CARTESIAN_POINT('Ctrl Pts',(0.237766813883331,1.88244585151826,11.7974395171488));
#39586=CARTESIAN_POINT('Ctrl Pts',(0.236538432970812,1.88111416828081,11.7973287980994));
#39587=CARTESIAN_POINT('Ctrl Pts',(0.236190503537246,1.8807387776333,11.7972974803986));
#39588=CARTESIAN_POINT('Ctrl Pts',(0.23558844562702,1.88009229667204,11.7972433607571));
#39589=CARTESIAN_POINT('Ctrl Pts',(0.235334739117352,1.87982081329375,11.7972205769101));
#39590=CARTESIAN_POINT('Ctrl Pts',(0.234808935959189,1.87926011483875,11.7971734030118));
#39591=CARTESIAN_POINT('Ctrl Pts',(0.23453677325662,1.8789709627776,11.7971490101395));
#39592=CARTESIAN_POINT('Ctrl Pts',(0.233899929719419,1.87829686588267,11.7970919900868));
#39593=CARTESIAN_POINT('Ctrl Pts',(0.233534832652152,1.8779123174668,11.7970593449601));
#39594=CARTESIAN_POINT('Ctrl Pts',(0.232359734299669,1.87668071488045,11.7969544130597));
#39595=CARTESIAN_POINT('Ctrl Pts',(0.231546067791806,1.87583718492553,11.7968819672682));
#39596=CARTESIAN_POINT('Ctrl Pts',(0.219098745128709,1.86307309727659,11.7957768387381));
#39597=CARTESIAN_POINT('Ctrl Pts',(0.206564651470505,1.8520695603545,11.7947033443389));
#39598=CARTESIAN_POINT('Ctrl Pts',(0.170885980811952,1.82533793779371,11.791746987975));
#39599=CARTESIAN_POINT('Ctrl Pts',(0.146453590161215,1.81156893742319,11.7898124704495));
#39600=CARTESIAN_POINT('Ctrl Pts',(0.115038519631861,1.79889756380337,11.7876034564957));
#39601=CARTESIAN_POINT('Ctrl Pts',(0.109462644358897,1.79682599253988,11.7872217612272));
#39602=CARTESIAN_POINT('Ctrl Pts',(0.10326791928281,1.79471772442695,11.7868114405864));
#39603=CARTESIAN_POINT('Ctrl Pts',(0.102703090586885,1.79452724159198,11.786774152309));
#39604=CARTESIAN_POINT('Ctrl Pts',(0.101861516421708,1.7942460271544,11.7867187824942));
#39605=CARTESIAN_POINT('Ctrl Pts',(0.101585175188119,1.7941541031463,11.78670063131));
#39606=CARTESIAN_POINT('Ctrl Pts',(0.101110845955794,1.7939970328614,11.7866695277055));
#39607=CARTESIAN_POINT('Ctrl Pts',(0.100912919327229,1.79393170405783,11.7866565644709));
#39608=CARTESIAN_POINT('Ctrl Pts',(0.100516045488607,1.79380113641609,11.7866306025802));
#39609=CARTESIAN_POINT('Ctrl Pts',(0.100317098555393,1.7937358995926,11.7866176041135));
#39610=CARTESIAN_POINT('Ctrl Pts',(0.0998472197775074,1.79358232829294,
11.7865869410838));
#39611=CARTESIAN_POINT('Ctrl Pts',(0.0995762333188271,1.79349415896071,
11.7865692863477));
#39612=CARTESIAN_POINT('Ctrl Pts',(0.098733663440106,1.79322125210116,11.7865144824297));
#39613=CARTESIAN_POINT('Ctrl Pts',(0.0981616760392877,1.79303775178442,
11.7864774059885));
#39614=CARTESIAN_POINT('Ctrl Pts',(0.0968318748762844,1.79261523292338,
11.7863914970572));
#39615=CARTESIAN_POINT('Ctrl Pts',(0.0960736797804176,1.79237741450469,
11.7863427332254));
#39616=CARTESIAN_POINT('Ctrl Pts',(0.0935165471388722,1.79158571053427,
11.7861789778073));
#39617=CARTESIAN_POINT('Ctrl Pts',(0.0917136001434671,1.79104476948785,
11.7860646978029));
#39618=CARTESIAN_POINT('Ctrl Pts',(0.0840643965085473,1.78882262823844,
11.7855844197877));
#39619=CARTESIAN_POINT('Ctrl Pts',(0.0781755466227434,1.78729123246203,
11.7852259073712));
#39620=CARTESIAN_POINT('Ctrl Pts',(0.061770190224892,1.78351748904971,11.7842491674188));
#39621=CARTESIAN_POINT('Ctrl Pts',(0.051179219797018,1.78163315037415,11.7836431389335));
#39622=CARTESIAN_POINT('Ctrl Pts',(0.0168969983911632,1.77728905566019,
11.781706868318));
#39623=CARTESIAN_POINT('Ctrl Pts',(-0.00697599470007906,1.77692245346771,
11.7803910358026));
#39624=CARTESIAN_POINT('Ctrl Pts',(-0.038065382725545,1.77989474012361,
11.7785546517917));
#39625=CARTESIAN_POINT('Ctrl Pts',(-0.0454325132410477,1.78085704743446,
11.7781109326985));
#39626=CARTESIAN_POINT('Ctrl Pts',(-0.0537124806884222,1.78223109277357,
11.7776002559405));
#39627=CARTESIAN_POINT('Ctrl Pts',(-0.0546648261846304,1.78239353638826,
11.7775413398889));
#39628=CARTESIAN_POINT('Ctrl Pts',(-0.0561059094728479,1.78264601861147,
11.7774519122617));
#39629=CARTESIAN_POINT('Ctrl Pts',(-0.0565951989304509,1.78273291057127,
11.7774215006994));
#39630=CARTESIAN_POINT('Ctrl Pts',(-0.057446215786213,1.78288607227839,
11.7773685213464));
#39631=CARTESIAN_POINT('Ctrl Pts',(-0.0578080353158415,1.78295183029343,
11.7773459698734));
#39632=CARTESIAN_POINT('Ctrl Pts',(-0.0585628878815867,1.7830903542677,
11.7772988653871));
#39633=CARTESIAN_POINT('Ctrl Pts',(-0.0589558994954324,1.78316323239302,
11.7772743088354));
#39634=CARTESIAN_POINT('Ctrl Pts',(-0.0598850971739494,1.78333732695134,
11.7772161741735));
#39635=CARTESIAN_POINT('Ctrl Pts',(-0.0604211624921362,1.78343917411797,
11.7771825760081));
#39636=CARTESIAN_POINT('Ctrl Pts',(-0.0621912347783861,1.78378013046192,
11.7770714373212));
#39637=CARTESIAN_POINT('Ctrl Pts',(-0.063424089835754,1.78402509540998,
11.7769937101678));
#39638=CARTESIAN_POINT('Ctrl Pts',(-0.0785772970635241,1.78712825387335,
11.776034357707));
#39639=CARTESIAN_POINT('Ctrl Pts',(-0.0922933029898179,1.79089651047776,
11.7751233558813));
#39640=CARTESIAN_POINT('Ctrl Pts',(-0.11851376680257,1.80000126898148,11.773296165906));
#39641=CARTESIAN_POINT('Ctrl Pts',(-0.131019190881346,1.80524811571201,
11.772384093323));
#39642=CARTESIAN_POINT('Ctrl Pts',(-0.155959698262365,1.81761379658061,
11.7705008748386));
#39643=CARTESIAN_POINT('Ctrl Pts',(-0.168327112664878,1.82480658549107,
11.7695312717921));
#39644=CARTESIAN_POINT('Ctrl Pts',(-0.182065793034183,1.83407065982949,
11.768438366233));
#39645=CARTESIAN_POINT('Ctrl Pts',(-0.183941373147152,1.83536451734087,
11.7682888238722));
#39646=CARTESIAN_POINT('Ctrl Pts',(-0.186390828142627,1.83709288296392,
11.7680932274148));
#39647=CARTESIAN_POINT('Ctrl Pts',(-0.18697715500017,1.83750954964256,11.7680463846979));
#39648=CARTESIAN_POINT('Ctrl Pts',(-0.188428525437206,1.83854828042607,
11.7679303848923));
#39649=CARTESIAN_POINT('Ctrl Pts',(-0.189291894849796,1.83917268266337,
11.7678613388378));
#39650=CARTESIAN_POINT('Ctrl Pts',(-0.193657545165101,1.84236308311626,
11.767512055546));
#39651=CARTESIAN_POINT('Ctrl Pts',(-0.197111021480385,1.84499553816574,
11.7672352562673));
#39652=CARTESIAN_POINT('Ctrl Pts',(-0.20098033209129,1.84807056151212,11.7669255446263));
#39653=CARTESIAN_POINT('Ctrl Pts',(-0.201449177002585,1.84844530423166,
11.7668880240045));
#39654=CARTESIAN_POINT('Ctrl Pts',(-0.202140192272888,1.84900079618438,
11.7668327376979));
#39655=CARTESIAN_POINT('Ctrl Pts',(-0.202363169561291,1.84918053254417,
11.766814900055));
#39656=CARTESIAN_POINT('Ctrl Pts',(-0.202757338060085,1.84949912959089,
11.7667833718495));
#39657=CARTESIAN_POINT('Ctrl Pts',(-0.202928626597585,1.84963786883531,
11.7667696725172));
#39658=CARTESIAN_POINT('Ctrl Pts',(-0.203258333536368,1.84990548351178,
11.7667433061486));
#39659=CARTESIAN_POINT('Ctrl Pts',(-0.203416771180086,1.85003433329219,
11.766730637323));
#39660=CARTESIAN_POINT('Ctrl Pts',(-0.203844311905702,1.85038270745885,
11.7666964539154));
#39661=CARTESIAN_POINT('Ctrl Pts',(-0.204113183772749,1.85060251716441,
11.7666749600339));
#39662=CARTESIAN_POINT('Ctrl Pts',(-0.205134483944484,1.85144021433353,
11.7665933268893));
#39663=CARTESIAN_POINT('Ctrl Pts',(-0.205884476050621,1.85206108386853,
11.7665334014878));
#39664=CARTESIAN_POINT('Ctrl Pts',(-0.207750237339644,1.8536199294317,11.7663843463566));
#39665=CARTESIAN_POINT('Ctrl Pts',(-0.208862490711725,1.85456210471595,
11.7662955083583));
#39666=CARTESIAN_POINT('Ctrl Pts',(-0.213245148173981,1.85832596468861,
11.7659453578196));
#39667=CARTESIAN_POINT('Ctrl Pts',(-0.216465227154571,1.86120585867247,
11.7656878701537));
#39668=CARTESIAN_POINT('Ctrl Pts',(-0.224695530106086,1.8688700166897,11.7650261651648));
#39669=CARTESIAN_POINT('Ctrl Pts',(-0.229611266189895,1.87375272880925,
11.7646273251012));
#39670=CARTESIAN_POINT('Ctrl Pts',(-0.256251182606515,1.90197704973941,
11.7624192516564));
#39671=CARTESIAN_POINT('Ctrl Pts',(-0.274573409335034,1.92828140074248,
11.7606982614548));
#39672=CARTESIAN_POINT('Ctrl Pts',(-0.291305496533585,1.96202995618514,
11.7584660192234));
#39673=CARTESIAN_POINT('Ctrl Pts',(-0.293734421229658,1.96727958471352,
11.7581188801863));
#39674=CARTESIAN_POINT('Ctrl Pts',(-0.296409970276014,1.97349594964596,
11.7577068708082));
#39675=CARTESIAN_POINT('Ctrl Pts',(-0.296795106928273,1.97440219068517,
11.7576467845135));
#39676=CARTESIAN_POINT('Ctrl Pts',(-0.297369766324003,1.97577178942146,
11.7575559376356));
#39677=CARTESIAN_POINT('Ctrl Pts',(-0.29756237498149,1.97623385269775,11.7575252818974));
#39678=CARTESIAN_POINT('Ctrl Pts',(-0.297904230286483,1.97705936565765,
11.7574705004382));
#39679=CARTESIAN_POINT('Ctrl Pts',(-0.298053890669067,1.9774226438124,11.7574463887941));
#39680=CARTESIAN_POINT('Ctrl Pts',(-0.298368281932675,1.97818976157715,
11.7573954638254));
#39681=CARTESIAN_POINT('Ctrl Pts',(-0.298532857968454,1.97859366343433,
11.7573686453212));
#39682=CARTESIAN_POINT('Ctrl Pts',(-0.298966045346289,1.97966299693225,
11.7572976277554));
#39683=CARTESIAN_POINT('Ctrl Pts',(-0.299233253788373,1.98032899101605,
11.7572533814351));
#39684=CARTESIAN_POINT('Ctrl Pts',(-0.30043965629483,1.98336514961971,11.7570515934221));
#39685=CARTESIAN_POINT('Ctrl Pts',(-0.301352908470266,1.98574546243783,
11.7568931818498));
#39686=CARTESIAN_POINT('Ctrl Pts',(-0.305211968187628,1.99617202435961,
11.7561981954884));
#39687=CARTESIAN_POINT('Ctrl Pts',(-0.30786422930257,2.00432247852731,11.755651979041));
#39688=CARTESIAN_POINT('Ctrl Pts',(-0.318225927603125,2.04108352142416,
11.7531738206257));
#39689=CARTESIAN_POINT('Ctrl Pts',(-0.322291789681375,2.07056820816242,
11.7511303604084));
#39690=CARTESIAN_POINT('Ctrl Pts',(-0.322274947886789,2.10018327456701,
11.7491602604485));
#39691=CARTESIAN_POINT('',(-0.322274998490625,2.09996880917294,11.4996790403846));
#39692=CARTESIAN_POINT('Ctrl Pts',(-0.322274947619657,2.10018374369947,
11.7491602292402));
#39693=CARTESIAN_POINT('Ctrl Pts',(-0.322268950934441,2.11070155421152,
11.748460547305));
#39694=CARTESIAN_POINT('Ctrl Pts',(-0.321748061778375,2.12121429561999,
11.7477736286716));
#39695=CARTESIAN_POINT('Ctrl Pts',(-0.320667537867109,2.1321516176864,11.7470842989936));
#39696=CARTESIAN_POINT('Ctrl Pts',(-0.320620324781466,2.13261906965548,
11.7470548864868));
#39697=CARTESIAN_POINT('Ctrl Pts',(-0.320542098304985,2.13337700070024,
11.7470072778706));
#39698=CARTESIAN_POINT('Ctrl Pts',(-0.320511712109824,2.13366754169137,
11.7469890471902));
#39699=CARTESIAN_POINT('Ctrl Pts',(-0.32045782597811,2.13417609508444,11.7469571711405));
#39700=CARTESIAN_POINT('Ctrl Pts',(-0.320434498569135,2.13439412498187,
11.746943516111));
#39701=CARTESIAN_POINT('Ctrl Pts',(-0.320388722059018,2.13481788666074,
11.7469169979818));
#39702=CARTESIAN_POINT('Ctrl Pts',(-0.320366297251527,2.13502362117741,
11.7469041334929));
#39703=CARTESIAN_POINT('Ctrl Pts',(-0.320321291777004,2.13543286021143,
11.746878563936));
#39704=CARTESIAN_POINT('Ctrl Pts',(-0.320298715366229,2.13563636462625,
11.7468658586436));
#39705=CARTESIAN_POINT('Ctrl Pts',(-0.320245123767606,2.13611527569325,
11.7468359818308));
#39706=CARTESIAN_POINT('Ctrl Pts',(-0.320213947170666,2.13639066465521,
11.7468188194791));
#39707=CARTESIAN_POINT('Ctrl Pts',(-0.32012094981732,2.13720275502851,11.746768261156));
#39708=CARTESIAN_POINT('Ctrl Pts',(-0.320058134319823,2.13773934497758,
11.7467349209991));
#39709=CARTESIAN_POINT('Ctrl Pts',(-0.319501534579595,2.14239264178265,
11.7464463517458));
#39710=CARTESIAN_POINT('Ctrl Pts',(-0.318929669392683,2.14649985599115,
11.7461954222511));
#39711=CARTESIAN_POINT('Ctrl Pts',(-0.318222174302826,2.15095049448819,
11.7459265114914));
#39712=CARTESIAN_POINT('Ctrl Pts',(-0.318165087024727,2.15130577460117,
11.7459050660666));
#39713=CARTESIAN_POINT('Ctrl Pts',(-0.317946762045513,2.15265013197692,
11.7458239943743));
#39714=CARTESIAN_POINT('Ctrl Pts',(-0.317781504700217,2.15363856084549,
11.7457645436688));
#39715=CARTESIAN_POINT('Ctrl Pts',(-0.317405010814399,2.15582759849676,
11.7456331960615));
#39716=CARTESIAN_POINT('Ctrl Pts',(-0.317191566513112,2.15702781649517,
11.7455613909783));
#39717=CARTESIAN_POINT('Ctrl Pts',(-0.316441384880153,2.16111160639411,
11.7453177030334));
#39718=CARTESIAN_POINT('Ctrl Pts',(-0.315872083083141,2.16398911280353,
11.7451470707396));
#39719=CARTESIAN_POINT('Ctrl Pts',(-0.314939078590981,2.16838858669777,
11.7448872981295));
#39720=CARTESIAN_POINT('Ctrl Pts',(-0.31460345648086,2.16991628780983,11.7447972996535));
#39721=CARTESIAN_POINT('Ctrl Pts',(-0.310992465654227,2.1858003061269,11.7438631629755));
#39722=CARTESIAN_POINT('Ctrl Pts',(-0.306747789749089,2.19991917240016,
11.7430458268146));
#39723=CARTESIAN_POINT('Ctrl Pts',(-0.29284195021286,2.23680027423194,11.7408404606812));
#39724=CARTESIAN_POINT('Ctrl Pts',(-0.281507658437494,2.25882033261991,
11.739441533447));
#39725=CARTESIAN_POINT('Ctrl Pts',(-0.267130699610873,2.28028781170197,
11.7378704155822));
#39726=CARTESIAN_POINT('Ctrl Pts',(-0.266483815291574,2.28124260497022,
11.7378000935766));
#39727=CARTESIAN_POINT('Ctrl Pts',(-0.265534020539039,2.28262841250604,
11.7376973687041));
#39728=CARTESIAN_POINT('Ctrl Pts',(-0.265235151128824,2.28306219631199,
11.7376651193121));
#39729=CARTESIAN_POINT('Ctrl Pts',(-0.264709443973943,2.28382122602114,
11.7376085228084));
#39730=CARTESIAN_POINT('Ctrl Pts',(-0.264483066385325,2.28414679051792,
11.7375841932761));
#39731=CARTESIAN_POINT('Ctrl Pts',(-0.264042835826657,2.28477742089377,
11.7375369607276));
#39732=CARTESIAN_POINT('Ctrl Pts',(-0.263829053483098,2.28508253553466,
11.7375140604373));
#39733=CARTESIAN_POINT('Ctrl Pts',(-0.263318173917205,2.28580898983719,
11.7374594216567));
#39734=CARTESIAN_POINT('Ctrl Pts',(-0.263020594466208,2.28622998765269,
11.7374276646958));
#39735=CARTESIAN_POINT('Ctrl Pts',(-0.262120104481805,2.28749748402103,
11.7373317735963));
#39736=CARTESIAN_POINT('Ctrl Pts',(-0.261514112647027,2.28834177585879,
11.7372675209018));
#39737=CARTESIAN_POINT('Ctrl Pts',(-0.255181905203886,2.29707457739523,
11.7365989576935));
#39738=CARTESIAN_POINT('Ctrl Pts',(-0.249105237759864,2.30470159072167,
11.7359809991665));
#39739=CARTESIAN_POINT('Ctrl Pts',(-0.225254265144905,2.33200037509071,
11.733634866946));
#39740=CARTESIAN_POINT('Ctrl Pts',(-0.205421566774034,2.34973034338367,
11.7318229293518));
#39741=CARTESIAN_POINT('Ctrl Pts',(-0.176093504824484,2.37006806653454,
11.7294241289772));
#39742=CARTESIAN_POINT('Ctrl Pts',(-0.16831806673017,2.37498133766676,11.728812308266));
#39743=CARTESIAN_POINT('Ctrl Pts',(-0.158445115785468,2.38064409159899,
11.728073489801));
#39744=CARTESIAN_POINT('Ctrl Pts',(-0.156536478559515,2.38171313827169,
11.7279323641213));
#39745=CARTESIAN_POINT('Ctrl Pts',(-0.151857160786773,2.38427182910921,
11.7275907649438));
#39746=CARTESIAN_POINT('Ctrl Pts',(-0.149075193117343,2.38574054442383,
11.7273913794451));
#39747=CARTESIAN_POINT('Ctrl Pts',(-0.145817358688473,2.38739995460051,
11.7271625476154));
#39748=CARTESIAN_POINT('Ctrl Pts',(-0.145362122280678,2.38763047372248,
11.7271306763015));
#39749=CARTESIAN_POINT('Ctrl Pts',(-0.14471174805151,2.38795786681495,11.7270852946028));
#39750=CARTESIAN_POINT('Ctrl Pts',(-0.144517059551175,2.38805562411468,
11.7270717289667));
#39751=CARTESIAN_POINT('Ctrl Pts',(-0.144136419260573,2.38824626879369,
11.7270452443816));
#39752=CARTESIAN_POINT('Ctrl Pts',(-0.143950476235573,2.38833917393108,
11.7270323243075));
#39753=CARTESIAN_POINT('Ctrl Pts',(-0.143579924284762,2.38852386984925,
11.7270066121948));
#39754=CARTESIAN_POINT('Ctrl Pts',(-0.14339531745632,2.38861566323159,11.7269938199907));
#39755=CARTESIAN_POINT('Ctrl Pts',(-0.142957397485407,2.38883288945286,
11.7269635156129));
#39756=CARTESIAN_POINT('Ctrl Pts',(-0.14270400664981,2.38895816654491,11.7269460132635));
#39757=CARTESIAN_POINT('Ctrl Pts',(-0.141814477718846,2.38939649653379,
11.7268846839697));
#39758=CARTESIAN_POINT('Ctrl Pts',(-0.141177465730696,2.3897077863797,11.7268409666856));
#39759=CARTESIAN_POINT('Ctrl Pts',(-0.132776010820972,2.39377905027203,
11.72626697445));
#39760=CARTESIAN_POINT('Ctrl Pts',(-0.12486384559136,2.39722827971215,11.7257554464584));
#39761=CARTESIAN_POINT('Ctrl Pts',(-0.100692277647183,2.40662968978287,
11.7242509166264));
#39762=CARTESIAN_POINT('Ctrl Pts',(-0.0840822762275282,2.4115942188867,
11.7232924980548));
#39763=CARTESIAN_POINT('Ctrl Pts',(-0.0650240110179947,2.41565454490743,
11.7222020774622));
#39764=CARTESIAN_POINT('Ctrl Pts',(-0.0628905397562314,2.41608652876088,
11.7220801607051));
#39765=CARTESIAN_POINT('Ctrl Pts',(-0.0582041225921994,2.41698610566029,
11.7218124464915));
#39766=CARTESIAN_POINT('Ctrl Pts',(-0.055649583104193,2.4174445380996,11.7216665749756));
#39767=CARTESIAN_POINT('Ctrl Pts',(-0.0438989422912002,2.41940708623251,
11.7209950487034));
#39768=CARTESIAN_POINT('Ctrl Pts',(-0.03464628805122,2.42054270025812,11.7204646265548));
#39769=CARTESIAN_POINT('Ctrl Pts',(-0.0168046720244086,2.4219509146117,
11.7194257772018));
#39770=CARTESIAN_POINT('Ctrl Pts',(-0.00822857072006633,2.42228412916206,
11.7189193783453));
#39771=CARTESIAN_POINT('Ctrl Pts',(0.00290545431056951,2.42227203386079,
11.7182481671951));
#39772=CARTESIAN_POINT('Ctrl Pts',(0.00546062730743365,2.42223886550676,
11.7180931992389));
#39773=CARTESIAN_POINT('Ctrl Pts',(0.00873305095507294,2.42215745412284,
11.7178934545744));
#39774=CARTESIAN_POINT('Ctrl Pts',(0.00945095526919228,2.42213719260161,
11.7178495559387));
#39775=CARTESIAN_POINT('Ctrl Pts',(0.0106048421228915,2.42210076573501,
11.7177788692149));
#39776=CARTESIAN_POINT('Ctrl Pts',(0.0110408728203206,2.42208611439789,
11.7177521286204));
#39777=CARTESIAN_POINT('Ctrl Pts',(0.0118694936856635,2.42205658678744,
11.7177012549395));
#39778=CARTESIAN_POINT('Ctrl Pts',(0.012262089337997,2.42204187792339,11.717677127146));
#39779=CARTESIAN_POINT('Ctrl Pts',(0.0131546354110652,2.42200680358947,
11.7176222185132));
#39780=CARTESIAN_POINT('Ctrl Pts',(0.01365456638542,2.42198599162546,11.7175914237283));
#39781=CARTESIAN_POINT('Ctrl Pts',(0.0151370828808383,2.42192081602623,
11.7174999853565));
#39782=CARTESIAN_POINT('Ctrl Pts',(0.0161195093675584,2.42187311856155,
11.7174392373843));
#39783=CARTESIAN_POINT('Ctrl Pts',(0.0228562296136296,2.4215151265364,11.7170215999422));
#39784=CARTESIAN_POINT('Ctrl Pts',(0.0286012035467558,2.42105505455501,
11.7166600356854));
#39785=CARTESIAN_POINT('Ctrl Pts',(0.0346851291765129,2.42040325320505,
11.7162710444655));
#39786=CARTESIAN_POINT('Ctrl Pts',(0.0350397218225903,2.42036466837551,
11.7162483507436));
#39787=CARTESIAN_POINT('Ctrl Pts',(0.0581351308789641,2.41781274958896,
11.7147688263816));
#39788=CARTESIAN_POINT('Ctrl Pts',(0.0805401078380058,2.41288591071856,
11.7132359547607));
#39789=CARTESIAN_POINT('Ctrl Pts',(0.112884892985624,2.40206685704193,11.7109280549968));
#39790=CARTESIAN_POINT('Ctrl Pts',(0.12334569696915,2.39794838604962,11.7101671199623));
#39791=CARTESIAN_POINT('Ctrl Pts',(0.140384051959473,2.390188816883,11.7089216570347));
#39792=CARTESIAN_POINT('Ctrl Pts',(0.14708811074073,2.38684897848462,11.7084300481458));
#39793=CARTESIAN_POINT('Ctrl Pts',(0.155584474927382,2.38223995030405,11.7078103327022));
#39794=CARTESIAN_POINT('Ctrl Pts',(0.157488226382901,2.38118210740182,11.707671700506));
#39795=CARTESIAN_POINT('Ctrl Pts',(0.160149977319933,2.37966755769964,11.7074783438169));
#39796=CARTESIAN_POINT('Ctrl Pts',(0.160916994962477,2.37922693072113,11.7074226814974));
#39797=CARTESIAN_POINT('Ctrl Pts',(0.162249992586815,2.37845384959776,11.7073260567755));
#39798=CARTESIAN_POINT('Ctrl Pts',(0.162816784752807,2.3781228165235,11.7072850068874));
#39799=CARTESIAN_POINT('Ctrl Pts',(0.163636710600072,2.3776405761058,11.7072256791768));
#39800=CARTESIAN_POINT('Ctrl Pts',(0.163890649679756,2.37749075210822,11.7072073125257));
#39801=CARTESIAN_POINT('Ctrl Pts',(0.164322599988114,2.37723510175401,11.7071760844932));
#39802=CARTESIAN_POINT('Ctrl Pts',(0.164500715115238,2.37712945213184,11.707163211541));
#39803=CARTESIAN_POINT('Ctrl Pts',(0.164854920191167,2.37691889232597,11.7071376200604));
#39804=CARTESIAN_POINT('Ctrl Pts',(0.165031011709835,2.37681398594164,11.7071249013171));
#39805=CARTESIAN_POINT('Ctrl Pts',(0.165445707132117,2.37656639511478,11.7070949577055));
#39806=CARTESIAN_POINT('Ctrl Pts',(0.165684227181443,2.37642356950858,11.7070777421086));
#39807=CARTESIAN_POINT('Ctrl Pts',(0.166388590629643,2.37600055805358,11.7070269233886));
#39808=CARTESIAN_POINT('Ctrl Pts',(0.166853913217789,2.37571950020205,11.7069933768954));
#39809=CARTESIAN_POINT('Ctrl Pts',(0.170940563622235,2.37323700268524,11.7066989650441));
#39810=CARTESIAN_POINT('Ctrl Pts',(0.174519061167846,2.37096538048701,11.7064425934264));
#39811=CARTESIAN_POINT('Ctrl Pts',(0.178291119749714,2.36846514597378,11.7061727343928));
#39812=CARTESIAN_POINT('Ctrl Pts',(0.178530115806142,2.36830627226308,11.7061556378921));
#39813=CARTESIAN_POINT('Ctrl Pts',(0.179349488072056,2.36776001131051,11.7060970289044));
#39814=CARTESIAN_POINT('Ctrl Pts',(0.179928822076298,2.36737105589566,11.706055597448));
#39815=CARTESIAN_POINT('Ctrl Pts',(0.1809209483708,2.36670027348489,11.7059846499838));
#39816=CARTESIAN_POINT('Ctrl Pts',(0.181334354337716,2.36641936374597,11.7059550886397));
#39817=CARTESIAN_POINT('Ctrl Pts',(0.20432198646598,2.3507209530597,11.7043113027594));
#39818=CARTESIAN_POINT('Ctrl Pts',(0.224845996088185,2.33249324098366,11.7028347083803));
#39819=CARTESIAN_POINT('Ctrl Pts',(0.253235129311885,2.2999597358024,11.7003881792259));
#39820=CARTESIAN_POINT('Ctrl Pts',(0.262751652325356,2.28727892894038,11.6994717987528));
#39821=CARTESIAN_POINT('Ctrl Pts',(0.272639364276537,2.27185789585365,11.6983670340386));
#39822=CARTESIAN_POINT('Ctrl Pts',(0.2739572844014,2.26974912403018,11.6982161944951));
#39823=CARTESIAN_POINT('Ctrl Pts',(0.275620572735821,2.26701790728419,11.6980210511169));
#39824=CARTESIAN_POINT('Ctrl Pts',(0.275988490002778,2.26640923905249,11.6979775761631));
#39825=CARTESIAN_POINT('Ctrl Pts',(0.276578034813643,2.2654265857227,11.6979074092183));
#39826=CARTESIAN_POINT('Ctrl Pts',(0.276800927155291,2.26505335903363,11.6978807634678));
#39827=CARTESIAN_POINT('Ctrl Pts',(0.277223988937843,2.26434168733287,11.6978299636048));
#39828=CARTESIAN_POINT('Ctrl Pts',(0.277424295614608,2.26400332447419,11.6978058145487));
#39829=CARTESIAN_POINT('Ctrl Pts',(0.2778795276969,2.26323111505557,11.6977507095799));
#39830=CARTESIAN_POINT('Ctrl Pts',(0.278134056780807,2.26279703710267,11.6977197393458));
#39831=CARTESIAN_POINT('Ctrl Pts',(0.278907102504429,2.26147156789141,11.6976251868385));
#39832=CARTESIAN_POINT('Ctrl Pts',(0.279422354428512,2.26057828891466,11.6975614866189));
#39833=CARTESIAN_POINT('Ctrl Pts',(0.283137595973581,2.25406524301752,11.6970971748517));
#39834=CARTESIAN_POINT('Ctrl Pts',(0.286171876346258,2.24835310842052,11.6966906539616));
#39835=CARTESIAN_POINT('Ctrl Pts',(0.289295402289979,2.24202006941801,11.6962402302613));
#39836=CARTESIAN_POINT('Ctrl Pts',(0.28955720579601,2.24148552741459,11.6962022146931));
#39837=CARTESIAN_POINT('Ctrl Pts',(0.300755763059905,2.2184594044522,11.6945647492212));
#39838=CARTESIAN_POINT('Ctrl Pts',(0.30903713488611,2.19477500640232,11.6928747755306));
#39839=CARTESIAN_POINT('Ctrl Pts',(0.318245997667544,2.15362288023519,11.690023326279));
#39840=CARTESIAN_POINT('Ctrl Pts',(0.320650823101592,2.13659397024029,11.6888694836161));
#39841=CARTESIAN_POINT('Ctrl Pts',(0.321761238601345,2.11823125455351,11.6877027000368));
#39842=CARTESIAN_POINT('Ctrl Pts',(0.321828150896782,2.11700925363514,11.6876254247287));
#39843=CARTESIAN_POINT('Ctrl Pts',(0.321916456563464,2.11520873667219,11.6875121425098));
#39844=CARTESIAN_POINT('Ctrl Pts',(0.321943253939489,2.11463051374857,11.6874758502839));
#39845=CARTESIAN_POINT('Ctrl Pts',(0.321983193150699,2.1137154148654,11.6874185558428));
#39846=CARTESIAN_POINT('Ctrl Pts',(0.321997364350109,2.11337858850869,11.6873974975083));
#39847=CARTESIAN_POINT('Ctrl Pts',(0.322023170284944,2.11274141924462,11.6873577200725));
#39848=CARTESIAN_POINT('Ctrl Pts',(0.32203491341676,2.11244108143029,11.6873389949679));
#39849=CARTESIAN_POINT('Ctrl Pts',(0.322054481797711,2.11192200840681,11.6873066752643));
#39850=CARTESIAN_POINT('Ctrl Pts',(0.322062504400508,2.11170328119804,11.6872930695223));
#39851=CARTESIAN_POINT('Ctrl Pts',(0.322077625910719,2.11127921654863,11.6872667166317));
#39852=CARTESIAN_POINT('Ctrl Pts',(0.322084751272772,2.11107388081874,11.6872539679933));
#39853=CARTESIAN_POINT('Ctrl Pts',(0.322101120369138,2.11058877878363,11.6872238768023));
#39854=CARTESIAN_POINT('Ctrl Pts',(0.32211019599974,2.11030900642974,11.6872065437466));
#39855=CARTESIAN_POINT('Ctrl Pts',(0.322140476100427,2.10933646902387,11.6871463643265));
#39856=CARTESIAN_POINT('Ctrl Pts',(0.322159810468988,2.10864364134049,11.687103622272));
#39857=CARTESIAN_POINT('Ctrl Pts',(0.322369371893727,2.10015188148049,11.686581272501));
#39858=CARTESIAN_POINT('Ctrl Pts',(0.322278610382905,2.09234783307556,11.6861169808051));
#39859=CARTESIAN_POINT('Ctrl Pts',(0.32043795575391,2.05398724855068,11.683878934921));
#39860=CARTESIAN_POINT('Ctrl Pts',(0.31462527586319,2.02378356191423,11.682240403367));
#39861=CARTESIAN_POINT('Ctrl Pts',(0.301062831114946,1.98449037510482,11.6798431320755));
#39862=CARTESIAN_POINT('Ctrl Pts',(0.296960989024225,1.97432011298298,11.6791982728875));
#39863=CARTESIAN_POINT('Ctrl Pts',(0.291513079344913,1.9625763849461,11.6784152688151));
#39864=CARTESIAN_POINT('Ctrl Pts',(0.290660089526937,1.96078133212326,11.6782945035354));
#39865=CARTESIAN_POINT('Ctrl Pts',(0.28950418149779,1.95840574535073,11.678133197943));
#39866=CARTESIAN_POINT('Ctrl Pts',(0.28921600617323,1.95781805382669,11.6780931712929));
#39867=CARTESIAN_POINT('Ctrl Pts',(0.28873905529866,1.95685283190517,11.6780272298284));
#39868=CARTESIAN_POINT('Ctrl Pts',(0.288551323903355,1.95647478528402,11.678001351547));
#39869=CARTESIAN_POINT('Ctrl Pts',(0.288185470061826,1.95574166132243,11.6779510675016));
#39870=CARTESIAN_POINT('Ctrl Pts',(0.288007432640619,1.95538654220896,11.6779266647511));
#39871=CARTESIAN_POINT('Ctrl Pts',(0.287593904419605,1.95456549821941,11.6778701389721));
#39872=CARTESIAN_POINT('Ctrl Pts',(0.287357937644618,1.95409981550732,11.6778379992714));
#39873=CARTESIAN_POINT('Ctrl Pts',(0.286720033599365,1.95284845634464,11.6777514205894));
#39874=CARTESIAN_POINT('Ctrl Pts',(0.286316001005212,1.95206385833427,11.6776969079228));
#39875=CARTESIAN_POINT('Ctrl Pts',(0.283379961551483,1.94641939447648,11.6773030775343));
#39876=CARTESIAN_POINT('Ctrl Pts',(0.280727719342338,1.94162340249499,11.6769595180058));
#39877=CARTESIAN_POINT('Ctrl Pts',(0.277042167560516,1.93534258713933,11.6764971866976));
#39878=CARTESIAN_POINT('Ctrl Pts',(0.276116687236431,1.93379530380112,11.676382267651));
#39879=CARTESIAN_POINT('Ctrl Pts',(0.262420202890649,1.91132670479636,11.6746984319663));
#39880=CARTESIAN_POINT('Ctrl Pts',(0.24731789982308,1.89192441556278,11.6730434488863));
#39881=CARTESIAN_POINT('Ctrl Pts',(0.217081169941339,1.86107229301274,11.6701217793369));
#39882=CARTESIAN_POINT('Ctrl Pts',(0.20285671410034,1.8488824526282,11.6688643320497));
#39883=CARTESIAN_POINT('Ctrl Pts',(0.187161846662895,1.83764149556746,11.6676506485025));
#39884=CARTESIAN_POINT('Ctrl Pts',(0.186668962397552,1.83729057842244,11.6676127006088));
#39885=CARTESIAN_POINT('Ctrl Pts',(0.185780924304916,1.83666208595334,11.6675446329519));
#39886=CARTESIAN_POINT('Ctrl Pts',(0.185386130893913,1.83638400790271,11.6675144796184));
#39887=CARTESIAN_POINT('Ctrl Pts',(0.18477809496137,1.83595777105278,11.6674682061021));
#39888=CARTESIAN_POINT('Ctrl Pts',(0.184565298064352,1.83580898236971,11.6674520428669));
#39889=CARTESIAN_POINT('Ctrl Pts',(0.184175330853926,1.83553701640646,11.6674224800742));
#39890=CARTESIAN_POINT('Ctrl Pts',(0.183998217371865,1.83541376038978,11.6674090751256));
#39891=CARTESIAN_POINT('Ctrl Pts',(0.183638304127025,1.83516382734951,11.667381878982));
#39892=CARTESIAN_POINT('Ctrl Pts',(0.183455497818968,1.83503716221414,11.6673680886082));
#39893=CARTESIAN_POINT('Ctrl Pts',(0.182927915287885,1.83467241193609,11.6673283552339));
#39894=CARTESIAN_POINT('Ctrl Pts',(0.182582804056972,1.83443480866878,11.6673024452228));
#39895=CARTESIAN_POINT('Ctrl Pts',(0.181055744554309,1.83338783775543,11.667188150788));
#39896=CARTESIAN_POINT('Ctrl Pts',(0.179868847435537,1.83258566681254,11.6671002487598));
#39897=CARTESIAN_POINT('Ctrl Pts',(0.155924426925709,1.81663424572912,11.6653447127623));
#39898=CARTESIAN_POINT('Ctrl Pts',(0.131331797775004,1.80443091233002,11.6638565571037));
#39899=CARTESIAN_POINT('Ctrl Pts',(0.0845123520095106,1.78821209982904,
11.6610761676898));
#39900=CARTESIAN_POINT('Ctrl Pts',(0.0628439018776408,1.78313338422472,
11.6598071939064));
#39901=CARTESIAN_POINT('Ctrl Pts',(0.0396895936633786,1.78017625556617,
11.6583877067298));
#39902=CARTESIAN_POINT('Ctrl Pts',(0.0385510293995014,1.78003701866026,
11.6583177636331));
#39903=CARTESIAN_POINT('Ctrl Pts',(0.0368897058276257,1.77984284876052,
11.6582154908786));
#39904=CARTESIAN_POINT('Ctrl Pts',(0.0363675081555351,1.77978311064028,
11.65818331278));
#39905=CARTESIAN_POINT('Ctrl Pts',(0.0354512776032882,1.77968056625419,
11.6581267988061));
#39906=CARTESIAN_POINT('Ctrl Pts',(0.0350573065073592,1.779637208813,11.6581024803519));
#39907=CARTESIAN_POINT('Ctrl Pts',(0.0342925254220064,1.77955447050031,
11.6580552378965));
#39908=CARTESIAN_POINT('Ctrl Pts',(0.0339217249089475,1.77951500619601,
11.6580323165633));
#39909=CARTESIAN_POINT('Ctrl Pts',(0.033036831818815,1.77942237993539,11.6579775775109));
#39910=CARTESIAN_POINT('Ctrl Pts',(0.0325226794131003,1.77936981105682,
11.6579457411649));
#39911=CARTESIAN_POINT('Ctrl Pts',(0.0309691866045579,1.77921475121073,
11.6578494535648));
#39912=CARTESIAN_POINT('Ctrl Pts',(0.0299294799287948,1.77911607620548,
11.6577848823937));
#39913=CARTESIAN_POINT('Ctrl Pts',(0.0189897186077547,1.77813145191743,
11.6571040810206));
#39914=CARTESIAN_POINT('Ctrl Pts',(0.00905519104353847,1.77769899141529,
11.6564736520581));
#39915=CARTESIAN_POINT('Ctrl Pts',(-0.0291243773725897,1.77780355582412,
11.6540006821517));
#39916=CARTESIAN_POINT('Ctrl Pts',(-0.0572313375997836,1.781593186946,11.6520610039077));
#39917=CARTESIAN_POINT('Ctrl Pts',(-0.095309661136734,1.79193632518954,
11.6494213132625));
#39918=CARTESIAN_POINT('Ctrl Pts',(-0.105981618639087,1.79544275905365,
11.648682253378));
#39919=CARTESIAN_POINT('Ctrl Pts',(-0.117404642485375,1.79986940506027,
11.6479072777536));
#39920=CARTESIAN_POINT('Ctrl Pts',(-0.118357654597363,1.80024394958659,
11.6478427491901));
#39921=CARTESIAN_POINT('Ctrl Pts',(-0.119998940673424,1.80089804134049,
11.6477318569634));
#39922=CARTESIAN_POINT('Ctrl Pts',(-0.120688056501404,1.8011754352792,11.6476853705573));
#39923=CARTESIAN_POINT('Ctrl Pts',(-0.121664519046595,1.80157242538911,
11.6476196106227));
#39924=CARTESIAN_POINT('Ctrl Pts',(-0.121952654504553,1.80169005624313,
11.6476002197867));
#39925=CARTESIAN_POINT('Ctrl Pts',(-0.122447672051414,1.80189298346252,
11.6475669303474));
#39926=CARTESIAN_POINT('Ctrl Pts',(-0.122654636146046,1.80197807810044,
11.6475530194641));
#39927=CARTESIAN_POINT('Ctrl Pts',(-0.123051171011972,1.8021415990362,11.6475263808877));
#39928=CARTESIAN_POINT('Ctrl Pts',(-0.123240755231485,1.80221999065973,
11.6475136510959));
#39929=CARTESIAN_POINT('Ctrl Pts',(-0.123687730851597,1.80240531163081,
11.6474836528119));
#39930=CARTESIAN_POINT('Ctrl Pts',(-0.123945059139253,1.80251239416557,
11.6474663936746));
#39931=CARTESIAN_POINT('Ctrl Pts',(-0.1247064102858,1.8028303760903,11.6474153616381));
#39932=CARTESIAN_POINT('Ctrl Pts',(-0.125210039325594,1.80304222488139,
11.6473816460411));
#39933=CARTESIAN_POINT('Ctrl Pts',(-0.129686196226932,1.80493850746372,
11.6470823395953));
#39934=CARTESIAN_POINT('Ctrl Pts',(-0.133625294777522,1.80670138272974,
11.6468214085531));
#39935=CARTESIAN_POINT('Ctrl Pts',(-0.137735783309624,1.8086409733795,11.6465505269026));
#39936=CARTESIAN_POINT('Ctrl Pts',(-0.137943433484373,1.80873922757041,
11.646536846544));
#39937=CARTESIAN_POINT('Ctrl Pts',(-0.138269322529276,1.80889385573213,
11.6465153821158));
#39938=CARTESIAN_POINT('Ctrl Pts',(-0.138387632000905,1.80895007972428,
11.6465075909386));
#39939=CARTESIAN_POINT('Ctrl Pts',(-0.14978567381247,1.81437527118008,11.6457570929036));
#39940=CARTESIAN_POINT('Ctrl Pts',(-0.160744853738672,1.82039602086603,
11.6450457422108));
#39941=CARTESIAN_POINT('Ctrl Pts',(-0.1803598637424,1.83270762170132,11.6437428903569));
#39942=CARTESIAN_POINT('Ctrl Pts',(-0.189105176985062,1.83882164713838,
11.6431499147818));
#39943=CARTESIAN_POINT('Ctrl Pts',(-0.207285848164231,1.85292479024039,
11.641859869132));
#39944=CARTESIAN_POINT('Ctrl Pts',(-0.216596969026116,1.86104539360262,
11.6411620353827));
#39945=CARTESIAN_POINT('Ctrl Pts',(-0.231558581895466,1.87568860245673,
11.6399469375239));
#39946=CARTESIAN_POINT('Ctrl Pts',(-0.237455090466544,1.88194028174133,
11.6394399111003));
#39947=CARTESIAN_POINT('Ctrl Pts',(-0.244775943077742,1.89035154944457,
11.6387677002613));
#39948=CARTESIAN_POINT('Ctrl Pts',(-0.24643426610853,1.89230337741389,11.6386123838274));
#39949=CARTESIAN_POINT('Ctrl Pts',(-0.248527944533823,1.89482799156527,
11.6384122511904));
#39950=CARTESIAN_POINT('Ctrl Pts',(-0.24898492027092,1.89538279220981,11.6383683172778));
#39951=CARTESIAN_POINT('Ctrl Pts',(-0.249716361827222,1.89627689205044,
11.6382975872743));
#39952=CARTESIAN_POINT('Ctrl Pts',(-0.24999200290181,1.89661523026778,11.638270838782));
#39953=CARTESIAN_POINT('Ctrl Pts',(-0.250514462846134,1.89725919538126,
11.6382199588735));
#39954=CARTESIAN_POINT('Ctrl Pts',(-0.250761411971926,1.8975647159801,11.6381958327699));
#39955=CARTESIAN_POINT('Ctrl Pts',(-0.251321482938759,1.89826022213501,
11.638140940097));
#39956=CARTESIAN_POINT('Ctrl Pts',(-0.251634256268489,1.8986504859026,11.6381101596129));
#39957=CARTESIAN_POINT('Ctrl Pts',(-0.252558775573924,1.89980957606703,
11.6380188020629));
#39958=CARTESIAN_POINT('Ctrl Pts',(-0.253167911413419,1.90058046848366,
11.6379581208862));
#39959=CARTESIAN_POINT('Ctrl Pts',(-0.257312961672676,1.90587584124378,
11.6375418156726));
#39960=CARTESIAN_POINT('Ctrl Pts',(-0.260730734192278,1.91049109083251,
11.6371815505319));
#39961=CARTESIAN_POINT('Ctrl Pts',(-0.264222551135567,1.91547970325174,
11.6367944717464));
#39962=CARTESIAN_POINT('Ctrl Pts',(-0.264421408764202,1.91576478342534,
11.6367723596792));
#39963=CARTESIAN_POINT('Ctrl Pts',(-0.28272655300698,1.94209752888334,11.6347306119083));
#39964=CARTESIAN_POINT('Ctrl Pts',(-0.296885704238967,1.97067267719311,
11.6325556830131));
#39965=CARTESIAN_POINT('Ctrl Pts',(-0.310277277508958,2.01208645353341,
11.6296389571148));
#39966=CARTESIAN_POINT('Ctrl Pts',(-0.313292024768791,2.02352155528033,
11.6288592359749));
#39967=CARTESIAN_POINT('Ctrl Pts',(-0.315993252829298,2.0366597811229,11.6280104143363));
#39968=CARTESIAN_POINT('Ctrl Pts',(-0.316302843572848,2.03822435303421,
11.6279100823872));
#39969=CARTESIAN_POINT('Ctrl Pts',(-0.316678608463224,2.04020026790976,
11.6277843724921));
#39970=CARTESIAN_POINT('Ctrl Pts',(-0.316755610246725,2.04060949235659,
11.6277583911777));
#39971=CARTESIAN_POINT('Ctrl Pts',(-0.316876929331963,2.041261187991,11.6277171027624));
#39972=CARTESIAN_POINT('Ctrl Pts',(-0.316921761645495,2.04150356100089,
11.627701766315));
#39973=CARTESIAN_POINT('Ctrl Pts',(-0.317005883351596,2.04196127619565,
11.6276728403506));
#39974=CARTESIAN_POINT('Ctrl Pts',(-0.317045231087765,2.04217660520874,
11.6276592476182));
#39975=CARTESIAN_POINT('Ctrl Pts',(-0.31713430998197,2.04266691059038,11.6276283315031));
#39976=CARTESIAN_POINT('Ctrl Pts',(-0.317183902820995,2.04294191116372,
11.6276110161344));
#39977=CARTESIAN_POINT('Ctrl Pts',(-0.317333738537926,2.04377900739939,
11.6275583828218));
#39978=CARTESIAN_POINT('Ctrl Pts',(-0.317432846067931,2.04434130910205,
11.6275231294424));
#39979=CARTESIAN_POINT('Ctrl Pts',(-0.318130166857817,2.04836011434741,
11.6272718800847));
#39980=CARTESIAN_POINT('Ctrl Pts',(-0.318673433607352,2.05182608577884,
11.6270589358217));
#39981=CARTESIAN_POINT('Ctrl Pts',(-0.321220880109221,2.07001513449006,
11.625957721768));
#39982=CARTESIAN_POINT('Ctrl Pts',(-0.322261887838054,2.08485656652799,
11.6251144298139));
#39983=CARTESIAN_POINT('Ctrl Pts',(-0.322294982549349,2.12272268958028,
11.6229888485315));
#39984=CARTESIAN_POINT('Ctrl Pts',(-0.319852072557969,2.14566145757631,
11.6217211217113));
#39985=CARTESIAN_POINT('Ctrl Pts',(-0.313016431727294,2.17725826061194,
11.6198362669214));
#39986=CARTESIAN_POINT('Ctrl Pts',(-0.310650298176335,2.18628147024724,
11.6192822798217));
#39987=CARTESIAN_POINT('Ctrl Pts',(-0.307559310124833,2.19627953963459,
11.6186458637341));
#39988=CARTESIAN_POINT('Ctrl Pts',(-0.307216315599347,2.19736844649967,
11.6185762479169));
#39989=CARTESIAN_POINT('Ctrl Pts',(-0.306709015321908,2.19894960748956,
11.6184747126471));
#39990=CARTESIAN_POINT('Ctrl Pts',(-0.306549292307643,2.19944333201769,
11.6184429439665));
#39991=CARTESIAN_POINT('Ctrl Pts',(-0.306265354802826,2.20031383485516,
11.6183868179411));
#39992=CARTESIAN_POINT('Ctrl Pts',(-0.306141635424202,2.20069077451988,
11.6183624769552));
#39993=CARTESIAN_POINT('Ctrl Pts',(-0.30588445925753,2.20146946548055,11.6183121144855));
#39994=CARTESIAN_POINT('Ctrl Pts',(-0.305750906308165,2.20187118399819,
11.6182860898666));
#39995=CARTESIAN_POINT('Ctrl Pts',(-0.305407058006443,2.20289868988323,
11.6182194136248));
#39996=CARTESIAN_POINT('Ctrl Pts',(-0.305195631343805,2.20352409409471,
11.6181787246628));
#39997=CARTESIAN_POINT('Ctrl Pts',(-0.304325377490146,2.20607248549372,
11.6180124908964));
#39998=CARTESIAN_POINT('Ctrl Pts',(-0.303650296585401,2.20798983583043,
11.6178864085445));
#39999=CARTESIAN_POINT('Ctrl Pts',(-0.29502677676077,2.2317618259758,11.6163103068185));
#40000=CARTESIAN_POINT('Ctrl Pts',(-0.284755217455978,2.2526958973546,11.6147786317867));
#40001=CARTESIAN_POINT('Ctrl Pts',(-0.258910288675556,2.29353508859649,
11.611519191112));
#40002=CARTESIAN_POINT('Ctrl Pts',(-0.243066944424643,2.31309394962098,
11.6097970847404));
#40003=CARTESIAN_POINT('Ctrl Pts',(-0.224088639080887,2.33161932514816,
11.6081207007523));
#40004=CARTESIAN_POINT('Ctrl Pts',(-0.223056294069078,2.33261367071816,
11.6080305880336));
#40005=CARTESIAN_POINT('Ctrl Pts',(-0.221713556015596,2.33388982520161,
11.6079148042989));
#40006=CARTESIAN_POINT('Ctrl Pts',(-0.221409220103028,2.33417794198435,
11.607888655069));
#40007=CARTESIAN_POINT('Ctrl Pts',(-0.220942504697662,2.33461806135229,
11.6078486979615));
#40008=CARTESIAN_POINT('Ctrl Pts',(-0.220780529890952,2.33477048944992,
11.6078348572157));
#40009=CARTESIAN_POINT('Ctrl Pts',(-0.220461103724958,2.33507046588285,
11.6078076145963));
#40010=CARTESIAN_POINT('Ctrl Pts',(-0.220303662892221,2.33521802291246,
11.6077942120939));
#40011=CARTESIAN_POINT('Ctrl Pts',(-0.219952558918515,2.33554642357472,
11.6077643791886));
#40012=CARTESIAN_POINT('Ctrl Pts',(-0.219758821403285,2.33572718606536,
11.6077479550864));
#40013=CARTESIAN_POINT('Ctrl Pts',(-0.219198219044171,2.33624895188041,
11.6077005376548));
#40014=CARTESIAN_POINT('Ctrl Pts',(-0.218830779799195,2.3365893410896,11.6076695914653));
#40015=CARTESIAN_POINT('Ctrl Pts',(-0.216331132347251,2.33889416503876,
11.6074599561811));
#40016=CARTESIAN_POINT('Ctrl Pts',(-0.214173206739673,2.34083068708095,
11.6072833535722));
#40017=CARTESIAN_POINT('Ctrl Pts',(-0.207319556266128,2.3468161590465,11.6067349178555));
#40018=CARTESIAN_POINT('Ctrl Pts',(-0.202532722904973,2.35075909029097,
11.6063698025944));
#40019=CARTESIAN_POINT('Ctrl Pts',(-0.186347204485524,2.36332508720379,
11.6051819168795));
#40020=CARTESIAN_POINT('Ctrl Pts',(-0.174488478988628,2.37132859515005,
11.6043843633477));
#40021=CARTESIAN_POINT('Ctrl Pts',(-0.139037686017919,2.39196591710504,
11.6020915844994));
#40022=CARTESIAN_POINT('Ctrl Pts',(-0.114359331173322,2.40248513261884,
11.6005929856368));
#40023=CARTESIAN_POINT('Ctrl Pts',(-0.0871190585330053,2.41028058063091,
11.5988756565194));
#40024=CARTESIAN_POINT('Ctrl Pts',(-0.0855675125816673,2.41071203665191,
11.5987776775778));
#40025=CARTESIAN_POINT('Ctrl Pts',(-0.0834116565349521,2.41129416783258,
11.5986412886999));
#40026=CARTESIAN_POINT('Ctrl Pts',(-0.0828100275586342,2.41145475225085,
11.5986032003335));
#40027=CARTESIAN_POINT('Ctrl Pts',(-0.0818466672458766,2.41170889991738,
11.5985421672329));
#40028=CARTESIAN_POINT('Ctrl Pts',(-0.0814852299654972,2.4118035800348,
11.5985192587074));
#40029=CARTESIAN_POINT('Ctrl Pts',(-0.0807404149639149,2.41199730416301,
11.5984720303252));
#40030=CARTESIAN_POINT('Ctrl Pts',(-0.0803570178420062,2.41209627055588,
11.5984477080009));
#40031=CARTESIAN_POINT('Ctrl Pts',(-0.0794666862001406,2.41232434272856,
11.59839119963));
#40032=CARTESIAN_POINT('Ctrl Pts',(-0.0789596188527971,2.41245292103281,
11.5983589966031));
#40033=CARTESIAN_POINT('Ctrl Pts',(-0.0773525119523605,2.41285627708525,
11.5982568671196));
#40034=CARTESIAN_POINT('Ctrl Pts',(-0.0762513433221206,2.41312648212169,
11.5981867933586));
#40035=CARTESIAN_POINT('Ctrl Pts',(-0.0566201591266331,2.41783389305874,
11.5969357698892));
#40036=CARTESIAN_POINT('Ctrl Pts',(-0.0377375416710892,2.42062418627174,
11.5957008039333));
#40037=CARTESIAN_POINT('Ctrl Pts',(0.00944724371809469,2.4233699406826,
11.5925464508341));
#40038=CARTESIAN_POINT('Ctrl Pts',(0.0377087274903272,2.42130269127191,
11.5905907828801));
#40039=CARTESIAN_POINT('Ctrl Pts',(0.0687343848253874,2.41487899055468,
11.5885559794927));
#40040=CARTESIAN_POINT('Ctrl Pts',(0.0721177987617064,2.41412134575814,
11.5883358096784));
#40041=CARTESIAN_POINT('Ctrl Pts',(0.0760415652003278,2.4131759563471,11.5880830174059));
#40042=CARTESIAN_POINT('Ctrl Pts',(0.0765942892986817,2.41304123391435,
11.5880474666515));
#40043=CARTESIAN_POINT('Ctrl Pts',(0.0774175684257859,2.41283825465783,
11.5879946050238));
#40044=CARTESIAN_POINT('Ctrl Pts',(0.077688392470774,2.41277110984718,11.5879772304781));
#40045=CARTESIAN_POINT('Ctrl Pts',(0.0781714807961838,2.41265067265336,
11.5879462649079));
#40046=CARTESIAN_POINT('Ctrl Pts',(0.078383777808129,2.41259751582194,11.5879326660541));
#40047=CARTESIAN_POINT('Ctrl Pts',(0.0788353064461566,2.4124839691251,11.5879037627345));
#40048=CARTESIAN_POINT('Ctrl Pts',(0.0790745222186617,2.41242352094474,
11.5878884617445));
#40049=CARTESIAN_POINT('Ctrl Pts',(0.0797183508833321,2.41226004304615,
11.5878473114441));
#40050=CARTESIAN_POINT('Ctrl Pts',(0.0801228351073641,2.41215650121335,
11.5878214918196));
#40051=CARTESIAN_POINT('Ctrl Pts',(0.0820834626654473,2.41165054835129,
11.5876964931322));
#40052=CARTESIAN_POINT('Ctrl Pts',(0.0836368171896738,2.41123727635507,
11.5875979336032));
#40053=CARTESIAN_POINT('Ctrl Pts',(0.0967538331240418,2.40764218182421,
11.5867691762146));
#40054=CARTESIAN_POINT('Ctrl Pts',(0.108136080432116,2.40382836196836,11.5860730393524));
#40055=CARTESIAN_POINT('Ctrl Pts',(0.148902322741741,2.38758653384137,11.5835769229432));
#40056=CARTESIAN_POINT('Ctrl Pts',(0.176607206007824,2.37145512475177,11.5818555216293));
#40057=CARTESIAN_POINT('Ctrl Pts',(0.205965880738581,2.34793561198496,11.5796257127626));
#40058=CARTESIAN_POINT('Ctrl Pts',(0.210341472724196,2.34423445762416,11.5792817185573));
#40059=CARTESIAN_POINT('Ctrl Pts',(0.215348367164173,2.33976492752099,11.578873115035));
#40060=CARTESIAN_POINT('Ctrl Pts',(0.216077854672554,2.33910771714033,11.5788131992865));
#40061=CARTESIAN_POINT('Ctrl Pts',(0.217174263682004,2.33811082465448,11.5787225604055));
#40062=CARTESIAN_POINT('Ctrl Pts',(0.217543421257456,2.33777360132404,11.5786919414006));
#40063=CARTESIAN_POINT('Ctrl Pts',(0.218195274434962,2.33717534840772,11.5786376946601));
#40064=CARTESIAN_POINT('Ctrl Pts',(0.218478290782697,2.33691466846252,11.5786140818322));
#40065=CARTESIAN_POINT('Ctrl Pts',(0.219073065837619,2.3363648625266,11.5785643303538));
#40066=CARTESIAN_POINT('Ctrl Pts',(0.219384720351546,2.33607562535388,11.5785381869753));
#40067=CARTESIAN_POINT('Ctrl Pts',(0.220020489162074,2.33548324127708,11.5784847025341));
#40068=CARTESIAN_POINT('Ctrl Pts',(0.220344551396197,2.33518004005514,11.578457359168));
#40069=CARTESIAN_POINT('Ctrl Pts',(0.221141664138062,2.3344311464515,11.5783898995624));
#40070=CARTESIAN_POINT('Ctrl Pts',(0.221613993117354,2.33398469199712,11.5783497505026));
#40071=CARTESIAN_POINT('Ctrl Pts',(0.222915662144452,2.33274685237931,11.5782386160428));
#40072=CARTESIAN_POINT('Ctrl Pts',(0.223742129140374,2.33195247210348,11.5781675009021));
#40073=CARTESIAN_POINT('Ctrl Pts',(0.230716527319223,2.32517688937974,11.5775626303178));
#40074=CARTESIAN_POINT('Ctrl Pts',(0.236627135946422,2.31895735543262,11.5770184066137));
#40075=CARTESIAN_POINT('Ctrl Pts',(0.247531626405735,2.30652516356812,11.5759498409434));
#40076=CARTESIAN_POINT('Ctrl Pts',(0.252557095316357,2.30034831564823,11.5754272606583));
#40077=CARTESIAN_POINT('Ctrl Pts',(0.276693574097054,2.26832904843085,11.5727633715538));
#40078=CARTESIAN_POINT('Ctrl Pts',(0.292090245387561,2.23991862778065,11.570519664294));
#40079=CARTESIAN_POINT('Ctrl Pts',(0.303541696016864,2.20828609953411,11.5683918240097));
#40080=CARTESIAN_POINT('Ctrl Pts',(0.304044076873539,2.2068673949384,11.5682971658994));
#40081=CARTESIAN_POINT('Ctrl Pts',(0.304676227865976,2.20504167811461,11.5681763906884));
#40082=CARTESIAN_POINT('Ctrl Pts',(0.30481514215586,2.20463788551612,11.5681497439328));
#40083=CARTESIAN_POINT('Ctrl Pts',(0.305033741165144,2.20399833798408,11.5681076436178));
#40084=CARTESIAN_POINT('Ctrl Pts',(0.305113955461257,2.20376276661909,11.5680921587004));
#40085=CARTESIAN_POINT('Ctrl Pts',(0.305257069817226,2.20334087102509,11.568064466332));
#40086=CARTESIAN_POINT('Ctrl Pts',(0.305320071738619,2.20315458347293,11.5680522528696));
#40087=CARTESIAN_POINT('Ctrl Pts',(0.305467628496894,2.202716960059,11.568023594162));
#40088=CARTESIAN_POINT('Ctrl Pts',(0.305552043537183,2.20246557780416,11.5680071573199));
#40089=CARTESIAN_POINT('Ctrl Pts',(0.305795315547532,2.20173815637049,11.5679596671004));
#40090=CARTESIAN_POINT('Ctrl Pts',(0.305953371893711,2.20126184724465,11.5679286610876));
#40091=CARTESIAN_POINT('Ctrl Pts',(0.30702350579876,2.19801157701477,11.5677176820938));
#40092=CARTESIAN_POINT('Ctrl Pts',(0.307898995649087,2.19522558617688,11.5675398263198));
#40093=CARTESIAN_POINT('Ctrl Pts',(0.310527683880753,2.18644499578954,11.5669874879647));
#40094=CARTESIAN_POINT('Ctrl Pts',(0.312144665352545,2.18041080946064,11.5666198148879));
#40095=CARTESIAN_POINT('Ctrl Pts',(0.31708200760208,2.15958187472932,11.5653793042261));
#40096=CARTESIAN_POINT('Ctrl Pts',(0.319533689838805,2.14460136218606,11.5645352961534));
#40097=CARTESIAN_POINT('Ctrl Pts',(0.323292097284807,2.10371903122009,11.5622403722068));
#40098=CARTESIAN_POINT('Ctrl Pts',(0.322546407736126,2.07774769941953,11.5607834369839));
#40099=CARTESIAN_POINT('Ctrl Pts',(0.318474713637766,2.05063012017575,11.5591205728399));
#40100=CARTESIAN_POINT('Ctrl Pts',(0.318236139905476,2.04911495905617,11.5590272239508));
#40101=CARTESIAN_POINT('Ctrl Pts',(0.317897486116887,2.04705979366299,11.5588999911668));
#40102=CARTESIAN_POINT('Ctrl Pts',(0.317806825743077,2.04651824019661,11.5588664062252));
#40103=CARTESIAN_POINT('Ctrl Pts',(0.317650805832134,2.0456006724566,11.5588094030532));
#40104=CARTESIAN_POINT('Ctrl Pts',(0.317586161337876,2.04522453644538,11.5587860075707));
#40105=CARTESIAN_POINT('Ctrl Pts',(0.317455010129089,2.04446946620519,11.5587389852895));
#40106=CARTESIAN_POINT('Ctrl Pts',(0.317388492704829,2.04409053446726,11.558715358184));
#40107=CARTESIAN_POINT('Ctrl Pts',(0.31723637356626,2.04323297325173,11.5586618215789));
#40108=CARTESIAN_POINT('Ctrl Pts',(0.317150367029671,2.04275441739204,11.5586318992426));
#40109=CARTESIAN_POINT('Ctrl Pts',(0.31696853166609,2.04175564086098,11.558569351326));
#40110=CARTESIAN_POINT('Ctrl Pts',(0.316872504423855,2.04123545820077,11.5585367194967));
#40111=CARTESIAN_POINT('Ctrl Pts',(0.316618362073062,2.03987749758475,11.5584513861567));
#40112=CARTESIAN_POINT('Ctrl Pts',(0.316458203175623,2.03904011057298,11.5583986195659));
#40113=CARTESIAN_POINT('Ctrl Pts',(0.315974804409917,2.03656592237408,11.5582422765026));
#40114=CARTESIAN_POINT('Ctrl Pts',(0.315642178415896,2.03493100383112,11.5581384012001));
#40115=CARTESIAN_POINT('Ctrl Pts',(0.313530248452106,2.02494790629779,11.5575005943022));
#40116=CARTESIAN_POINT('Ctrl Pts',(0.311432701718048,2.01667123090506,11.5569565562979));
#40117=CARTESIAN_POINT('Ctrl Pts',(0.304929189452833,1.9947107353093,11.5554707995222));
#40118=CARTESIAN_POINT('Ctrl Pts',(0.299932643241671,1.98122301314241,11.5545124166085));
#40119=CARTESIAN_POINT('Ctrl Pts',(0.283893636129505,1.9454621464165,11.5518682411617));
#40120=CARTESIAN_POINT('Ctrl Pts',(0.271149457431684,1.92405761597038,11.5501650061831));
#40121=CARTESIAN_POINT('Ctrl Pts',(0.255214831423693,1.90320425899285,11.5485063981178));
#40122=CARTESIAN_POINT('Ctrl Pts',(0.254349157280599,1.90208668508119,11.548417534166));
#40123=CARTESIAN_POINT('Ctrl Pts',(0.253218712646049,1.90064696403551,11.5483031258811));
#40124=CARTESIAN_POINT('Ctrl Pts',(0.252960648693245,1.90031960637124,11.5482771170198));
#40125=CARTESIAN_POINT('Ctrl Pts',(0.252564193232096,1.89981869919597,11.5482373280888));
#40126=CARTESIAN_POINT('Ctrl Pts',(0.252426257595767,1.89964479200313,11.5482235155826));
#40127=CARTESIAN_POINT('Ctrl Pts',(0.252153858988122,1.89930208372765,11.5481962995014));
#40128=CARTESIAN_POINT('Ctrl Pts',(0.252019406935512,1.89913327620762,11.5481828953562));
#40129=CARTESIAN_POINT('Ctrl Pts',(0.251719059114187,1.89875695916607,11.5481530175509));
#40130=CARTESIAN_POINT('Ctrl Pts',(0.251553076701583,1.89854952020756,11.5481365502864));
#40131=CARTESIAN_POINT('Ctrl Pts',(0.251071361494426,1.89794901324016,11.548088886064));
#40132=CARTESIAN_POINT('Ctrl Pts',(0.250754960778373,1.89755647832917,11.54805773701));
#40133=CARTESIAN_POINT('Ctrl Pts',(0.248567924711413,1.89485617860846,11.5478434992577));
#40134=CARTESIAN_POINT('Ctrl Pts',(0.246666301272548,1.89257353596184,11.5476626032494));
#40135=CARTESIAN_POINT('Ctrl Pts',(0.240611127960411,1.88550617459855,11.5471019945483));
#40136=CARTESIAN_POINT('Ctrl Pts',(0.236347680480554,1.88081719731685,11.5467292597696));
#40137=CARTESIAN_POINT('Ctrl Pts',(0.219573710074085,1.86342808979586,11.5453301450097));
#40138=CARTESIAN_POINT('Ctrl Pts',(0.206155180735637,1.85164740602974,11.5443449852298));
#40139=CARTESIAN_POINT('Ctrl Pts',(0.17311150715471,1.82716991228453,11.5420418936996));
#40140=CARTESIAN_POINT('Ctrl Pts',(0.15294755859425,1.81537628546624,11.5407175853775));
#40141=CARTESIAN_POINT('Ctrl Pts',(0.130432206526646,1.80529588454672,11.5392201027296));
#40142=CARTESIAN_POINT('Ctrl Pts',(0.129170369982013,1.80474063674281,11.5391361449978));
#40143=CARTESIAN_POINT('Ctrl Pts',(0.127423279541293,1.80398520488836,11.5390198405335));
#40144=CARTESIAN_POINT('Ctrl Pts',(0.126941028366662,1.80377807912628,11.5389877306425));
#40145=CARTESIAN_POINT('Ctrl Pts',(0.126113320886006,1.80342497311812,11.5389326075727));
#40146=CARTESIAN_POINT('Ctrl Pts',(0.125768110707689,1.80327841567898,11.5389096140782));
#40147=CARTESIAN_POINT('Ctrl Pts',(0.125065802000194,1.80298169944869,11.5388628279137));
#40148=CARTESIAN_POINT('Ctrl Pts',(0.124708687029687,1.80283158130509,11.5388390339072));
#40149=CARTESIAN_POINT('Ctrl Pts',(0.123886507433871,1.80248770995678,11.5387842441287));
#40150=CARTESIAN_POINT('Ctrl Pts',(0.12342125830539,1.802294403068,11.5387532332825));
#40151=CARTESIAN_POINT('Ctrl Pts',(0.122444131166048,1.80189109961964,11.5386880885259));
#40152=CARTESIAN_POINT('Ctrl Pts',(0.121932162256249,1.80168132887061,11.5386539470785));
#40153=CARTESIAN_POINT('Ctrl Pts',(0.120576076219173,1.80112976925892,11.5385634902513));
#40154=CARTESIAN_POINT('Ctrl Pts',(0.119731050689025,1.80079024004354,11.5385070987075));
#40155=CARTESIAN_POINT('Ctrl Pts',(0.117188031169288,1.79978095875797,11.5383373141451));
#40156=CARTESIAN_POINT('Ctrl Pts',(0.115485796994084,1.79912205490355,11.5382235577248));
#40157=CARTESIAN_POINT('Ctrl Pts',(0.109411809852674,1.79683006346992,11.5378172217022));
#40158=CARTESIAN_POINT('Ctrl Pts',(0.105010457466901,1.7952775775871,11.5375219911797));
#40159=CARTESIAN_POINT('Ctrl Pts',(0.09047246689367,1.79050197058509,11.5365438819269));
#40160=CARTESIAN_POINT('Ctrl Pts',(0.0802106378386884,1.78768523418066,
11.5358485710002));
#40161=CARTESIAN_POINT('Ctrl Pts',(0.0385498039188777,1.77843867658274,
11.5330128265004));
#40162=CARTESIAN_POINT('Ctrl Pts',(0.00641209109946308,1.77619976194548,
11.5307763411033));
#40163=CARTESIAN_POINT('Ctrl Pts',(-0.0270412416340491,1.7788578899055,
11.5286534656157));
#40164=CARTESIAN_POINT('Ctrl Pts',(-0.0285548445712876,1.77898893369204,
11.5285579044613));
#40165=CARTESIAN_POINT('Ctrl Pts',(-0.0304891801006262,1.77917019325197,
11.5284364544719));
#40166=CARTESIAN_POINT('Ctrl Pts',(-0.030910785612659,1.77921053892174,
11.5284100243671));
#40167=CARTESIAN_POINT('Ctrl Pts',(-0.0315816542997596,1.77927607276519,
11.5283680347349));
#40168=CARTESIAN_POINT('Ctrl Pts',(-0.0318309679062435,1.77930072049908,
11.5283524448505));
#40169=CARTESIAN_POINT('Ctrl Pts',(-0.0322974772923847,1.77934739008711,
11.5283233011713));
#40170=CARTESIAN_POINT('Ctrl Pts',(-0.0325146777762391,1.77936934174519,
11.5283097435552));
#40171=CARTESIAN_POINT('Ctrl Pts',(-0.0330036834853458,1.77941926576802,
11.5282792451786));
#40172=CARTESIAN_POINT('Ctrl Pts',(-0.0332754749191719,1.77944736305164,
11.5282623116014));
#40173=CARTESIAN_POINT('Ctrl Pts',(-0.0340847077635674,1.77953206031344,
11.5282119448954));
#40174=CARTESIAN_POINT('Ctrl Pts',(-0.034622046298193,1.77958966684823,
11.5281785684253));
#40175=CARTESIAN_POINT('Ctrl Pts',(-0.0390589036127109,1.78007662133725,
11.5279035146523));
#40176=CARTESIAN_POINT('Ctrl Pts',(-0.0429506406741204,1.78057581178246,
11.527665694334));
#40177=CARTESIAN_POINT('Ctrl Pts',(-0.0555676082576323,1.78242896119883,
11.5269030683628));
#40178=CARTESIAN_POINT('Ctrl Pts',(-0.0642470442662829,1.78407047211645,
11.5263914977357));
#40179=CARTESIAN_POINT('Ctrl Pts',(-0.0874190444930373,1.78944757111988,
11.5250352567948));
#40180=CARTESIAN_POINT('Ctrl Pts',(-0.101736753244368,1.79383898697891,
11.5242068343924));
#40181=CARTESIAN_POINT('Ctrl Pts',(-0.123807947510714,1.80232858946436,
11.5228814082342));
#40182=CARTESIAN_POINT('Ctrl Pts',(-0.131788075182596,1.80577462666305,
11.5223917619239));
#40183=CARTESIAN_POINT('Ctrl Pts',(-0.152379927611386,1.81567272188714,
11.5210844163471));
#40184=CARTESIAN_POINT('Ctrl Pts',(-0.164721228471299,1.82264016020916,
11.5202550805417));
#40185=CARTESIAN_POINT('Ctrl Pts',(-0.177594807922572,1.83107105123723,
11.5193200036892));
#40186=CARTESIAN_POINT('Ctrl Pts',(-0.178622185018869,1.83175233414479,
11.519244878741));
#40187=CARTESIAN_POINT('Ctrl Pts',(-0.180060992451828,1.83271837897171,
11.5191389520845));
#40188=CARTESIAN_POINT('Ctrl Pts',(-0.180475715992405,1.8329982361953,11.5191083353731));
#40189=CARTESIAN_POINT('Ctrl Pts',(-0.18119484628816,1.83348594939298,11.5190550986719));
#40190=CARTESIAN_POINT('Ctrl Pts',(-0.181499552062431,1.83369336453694,
11.5190324953979));
#40191=CARTESIAN_POINT('Ctrl Pts',(-0.182126812189448,1.83412192107684,
11.5189858693268));
#40192=CARTESIAN_POINT('Ctrl Pts',(-0.182449321087705,1.83434312769534,
11.5189618440763));
#40193=CARTESIAN_POINT('Ctrl Pts',(-0.183204797520332,1.83486332835797,
11.5189054418962));
#40194=CARTESIAN_POINT('Ctrl Pts',(-0.183637436077162,1.83516279613761,
11.5188730469564));
#40195=CARTESIAN_POINT('Ctrl Pts',(-0.184548922504466,1.83579702464247,
11.5188045950571));
#40196=CARTESIAN_POINT('Ctrl Pts',(-0.185027596833968,1.83613203038645,
11.5187685287924));
#40197=CARTESIAN_POINT('Ctrl Pts',(-0.18631111447421,1.83703552482912,11.518671501027));
#40198=CARTESIAN_POINT('Ctrl Pts',(-0.187114261084638,1.83760640281702,
11.5186104478904));
#40199=CARTESIAN_POINT('Ctrl Pts',(-0.189565136793502,1.83936546406545,
11.518423089598));
#40200=CARTESIAN_POINT('Ctrl Pts',(-0.191204235688836,1.84056553359353,
11.5182963264613));
#40201=CARTESIAN_POINT('Ctrl Pts',(-0.19715353969909,1.84500833325495,11.5178307830151));
#40202=CARTESIAN_POINT('Ctrl Pts',(-0.201393303248048,1.84834348781353,
11.5174884248549));
#40203=CARTESIAN_POINT('Ctrl Pts',(-0.210134151579303,1.85558174706168,
11.5167596100325));
#40204=CARTESIAN_POINT('Ctrl Pts',(-0.214614703007654,1.85950641088499,
11.5163724123246));
#40205=CARTESIAN_POINT('Ctrl Pts',(-0.2310119738557,1.87469261431733,11.5149038770566));
#40206=CARTESIAN_POINT('Ctrl Pts',(-0.242171708430901,1.88673319717696,
11.5137961238617));
#40207=CARTESIAN_POINT('Ctrl Pts',(-0.264590190256713,1.91496072656484,
11.5113568924354));
#40208=CARTESIAN_POINT('Ctrl Pts',(-0.275382114609853,1.93144026323942,
11.510029418704));
#40209=CARTESIAN_POINT('Ctrl Pts',(-0.285139433592585,1.94980688134202,
11.5087184598918));
#40210=CARTESIAN_POINT('Ctrl Pts',(-0.285667777237769,1.95081424122439,
11.5086470714868));
#40211=CARTESIAN_POINT('Ctrl Pts',(-0.286366672148987,1.95216410771361,
11.5085521173304));
#40212=CARTESIAN_POINT('Ctrl Pts',(-0.286541954849484,1.9525041353785,11.508528258278));
#40213=CARTESIAN_POINT('Ctrl Pts',(-0.286814829203746,1.9530358015649,11.508491046378));
#40214=CARTESIAN_POINT('Ctrl Pts',(-0.286912834453933,1.9532272256203,11.5084776674048));
#40215=CARTESIAN_POINT('Ctrl Pts',(-0.28710025662649,1.95359420406155,11.5084520552274));
#40216=CARTESIAN_POINT('Ctrl Pts',(-0.287189703530052,1.95376974107267,
11.5084398201949));
#40217=CARTESIAN_POINT('Ctrl Pts',(-0.287400769416072,1.95418489252018,
11.5084109217064));
#40218=CARTESIAN_POINT('Ctrl Pts',(-0.287522249568002,1.95442457681697,
11.5083942671111));
#40219=CARTESIAN_POINT('Ctrl Pts',(-0.287877300741607,1.9551272824667,11.5083455254019));
#40220=CARTESIAN_POINT('Ctrl Pts',(-0.288110055483813,1.95559071876869,
11.5083134895959));
#40221=CARTESIAN_POINT('Ctrl Pts',(-0.289820138716054,1.9590162446977,11.5080774869168));
#40222=CARTESIAN_POINT('Ctrl Pts',(-0.291252941172031,1.96200051305261,
11.5078762524734));
#40223=CARTESIAN_POINT('Ctrl Pts',(-0.295849678470874,1.97196534042078,
11.5072169495189));
#40224=CARTESIAN_POINT('Ctrl Pts',(-0.298810795011803,1.97903705817536,
11.5067693345922));
#40225=CARTESIAN_POINT('Ctrl Pts',(-0.307023728810907,2.0007990766942,11.5054332065256));
#40226=CARTESIAN_POINT('Ctrl Pts',(-0.311464204206702,2.01577118909666,
11.5045687718015));
#40227=CARTESIAN_POINT('Ctrl Pts',(-0.31976848465604,2.0536619885797,11.5023974765617));
#40228=CARTESIAN_POINT('Ctrl Pts',(-0.322272754439886,2.07678245867823,
11.5010822755746));
#40229=CARTESIAN_POINT('Ctrl Pts',(-0.322274998490625,2.09996880917294,
11.4996790403846));
#40230=CARTESIAN_POINT('',(-0.322274977094782,2.09987849461815,11.2490951747016));
#40231=CARTESIAN_POINT('Ctrl Pts',(-0.322274998502865,2.0999689359024,11.499679032715));
#40232=CARTESIAN_POINT('Ctrl Pts',(-0.322275099486767,2.1010165950739,11.4996156284931));
#40233=CARTESIAN_POINT('Ctrl Pts',(-0.322270091837628,2.10206424137144,
11.4995520677508));
#40234=CARTESIAN_POINT('Ctrl Pts',(-0.322250763173066,2.10406590582397,
11.4994303174676));
#40235=CARTESIAN_POINT('Ctrl Pts',(-0.322237313678586,2.10501992015537,
11.4993721557721));
#40236=CARTESIAN_POINT('Ctrl Pts',(-0.322211300242446,2.10642304140411,
11.4992864120943));
#40237=CARTESIAN_POINT('Ctrl Pts',(-0.322202033181655,2.1068722103572,11.499258933258));
#40238=CARTESIAN_POINT('Ctrl Pts',(-0.322183414761047,2.10769155343982,
11.4992087521226));
#40239=CARTESIAN_POINT('Ctrl Pts',(-0.322174364562626,2.108061734197,11.4991860592853));
#40240=CARTESIAN_POINT('Ctrl Pts',(-0.322155452750297,2.10878431390489,
11.4991417225374));
#40241=CARTESIAN_POINT('Ctrl Pts',(-0.322145650852467,2.10913671400454,
11.4991200805285));
#40242=CARTESIAN_POINT('Ctrl Pts',(-0.322121913947223,2.10994253304504,
11.4990705486242));
#40243=CARTESIAN_POINT('Ctrl Pts',(-0.322107599802702,2.11039593932095,
11.4990426468884));
#40244=CARTESIAN_POINT('Ctrl Pts',(-0.322066224517841,2.11162428097165,
11.4989669700515));
#40245=CARTESIAN_POINT('Ctrl Pts',(-0.322037323927901,2.11239914770598,
11.4989191373895));
#40246=CARTESIAN_POINT('Ctrl Pts',(-0.321900227497391,2.11575015473037,
11.4987118670454));
#40247=CARTESIAN_POINT('Ctrl Pts',(-0.321763916376092,2.11832499204841,
11.4985515505396));
#40248=CARTESIAN_POINT('Ctrl Pts',(-0.319263892784774,2.15679780651772,
11.4961397562275));
#40249=CARTESIAN_POINT('Ctrl Pts',(-0.310935952237075,2.19204820152477,
11.4936741023558));
#40250=CARTESIAN_POINT('Ctrl Pts',(-0.292507500731267,2.23576630667989,
11.4904977398617));
#40251=CARTESIAN_POINT('Ctrl Pts',(-0.287482295100116,2.2461065314714,11.4897406225045));
#40252=CARTESIAN_POINT('Ctrl Pts',(-0.281153711068542,2.25753169482296,
11.4889142598651));
#40253=CARTESIAN_POINT('Ctrl Pts',(-0.280382358983871,2.25890052589766,
11.4888154316593));
#40254=CARTESIAN_POINT('Ctrl Pts',(-0.279395006402081,2.26062309182209,
11.4886913419045));
#40255=CARTESIAN_POINT('Ctrl Pts',(-0.279188309941846,2.26098209473509,
11.4886654954915));
#40256=CARTESIAN_POINT('Ctrl Pts',(-0.278857764268774,2.26155365501622,
11.4886243717364));
#40257=CARTESIAN_POINT('Ctrl Pts',(-0.278734363776928,2.26176646930969,
11.4886090654487));
#40258=CARTESIAN_POINT('Ctrl Pts',(-0.278500655260794,2.26216845747054,
11.4885801642548));
#40259=CARTESIAN_POINT('Ctrl Pts',(-0.278390399007472,2.26235765864237,
11.4885665662065));
#40260=CARTESIAN_POINT('Ctrl Pts',(-0.278138603285059,2.262788732787,11.4885355950427));
#40261=CARTESIAN_POINT('Ctrl Pts',(-0.277996941361132,2.26303053319867,
11.488518230049));
#40262=CARTESIAN_POINT('Ctrl Pts',(-0.277573327529032,2.2637514351171,11.4884664796885));
#40263=CARTESIAN_POINT('Ctrl Pts',(-0.27729044935753,2.26422999532499,11.4884321543444));
#40264=CARTESIAN_POINT('Ctrl Pts',(-0.275295345043811,2.26758537037305,
11.4881916679761));
#40265=CARTESIAN_POINT('Ctrl Pts',(-0.273539542368667,2.27043621757659,
11.4879882844259));
#40266=CARTESIAN_POINT('Ctrl Pts',(-0.263757127463278,2.28577893642419,
11.4868959496517));
#40267=CARTESIAN_POINT('Ctrl Pts',(-0.25491804438629,2.29773348066788,11.4860525721841));
#40268=CARTESIAN_POINT('Ctrl Pts',(-0.225675311325338,2.33204705575656,
11.483521013414));
#40269=CARTESIAN_POINT('Ctrl Pts',(-0.202928302829027,2.35218072922635,
11.481859864261));
#40270=CARTESIAN_POINT('Ctrl Pts',(-0.176096250597378,2.36991670446061,
11.4799250680259));
#40271=CARTESIAN_POINT('Ctrl Pts',(-0.174473134938694,2.37096870992292,
11.4798081929933));
#40272=CARTESIAN_POINT('Ctrl Pts',(-0.172038542058987,2.37251572226197,
11.4796330839575));
#40273=CARTESIAN_POINT('Ctrl Pts',(-0.171234165914402,2.37302186584085,
11.4795752607826));
#40274=CARTESIAN_POINT('Ctrl Pts',(-0.169943980107026,2.37382575463158,
11.4794825605243));
#40275=CARTESIAN_POINT('Ctrl Pts',(-0.169459595047152,2.37412578483988,
11.4794477675519));
#40276=CARTESIAN_POINT('Ctrl Pts',(-0.168535344675143,2.3746948836423,11.479381397671));
#40277=CARTESIAN_POINT('Ctrl Pts',(-0.168095623858632,2.37496418446539,
11.479349829408));
#40278=CARTESIAN_POINT('Ctrl Pts',(-0.167322805386222,2.37543493961424,
11.4792943604496));
#40279=CARTESIAN_POINT('Ctrl Pts',(-0.166989984642264,2.37563684838867,
11.4792704764686));
#40280=CARTESIAN_POINT('Ctrl Pts',(-0.166338962227335,2.37603018524685,
11.479223765414));
#40281=CARTESIAN_POINT('Ctrl Pts',(-0.166020793780224,2.37622166742142,
11.4792009403648));
#40282=CARTESIAN_POINT('Ctrl Pts',(-0.16526406560645,2.37667530664248,11.4791466617775));
#40283=CARTESIAN_POINT('Ctrl Pts',(-0.16482521298458,2.37693697089098,11.4791151903267));
#40284=CARTESIAN_POINT('Ctrl Pts',(-0.163272195535001,2.37785795265877,
11.4790038405145));
#40285=CARTESIAN_POINT('Ctrl Pts',(-0.162154693317995,2.3785115923028,11.4789237561517));
#40286=CARTESIAN_POINT('Ctrl Pts',(-0.144001112821963,2.38898353272403,
11.4776233458485));
#40287=CARTESIAN_POINT('Ctrl Pts',(-0.126108816074974,2.39722737567277,
11.4763454014616));
#40288=CARTESIAN_POINT('Ctrl Pts',(-0.0982467335899388,2.40709410472849,
11.4743685632446));
#40289=CARTESIAN_POINT('Ctrl Pts',(-0.088766373968394,2.4099673030876,11.4736988387156));
#40290=CARTESIAN_POINT('Ctrl Pts',(-0.0714363988427003,2.41435911294969,
11.4724890071636));
#40291=CARTESIAN_POINT('Ctrl Pts',(-0.0636334050071042,2.41603102103039,
11.4719494526071));
#40292=CARTESIAN_POINT('Ctrl Pts',(-0.0443777946816995,2.419414658434,11.470640203911));
#40293=CARTESIAN_POINT('Ctrl Pts',(-0.0328783151121363,2.42080241689272,
11.469877166965));
#40294=CARTESIAN_POINT('Ctrl Pts',(-0.020289506899484,2.42163736500157,
11.4690788757297));
#40295=CARTESIAN_POINT('Ctrl Pts',(-0.019250756896274,2.42170120777318,
11.4690132811013));
#40296=CARTESIAN_POINT('Ctrl Pts',(-0.0174604423789802,2.4218025400341,
11.4689007223165));
#40297=CARTESIAN_POINT('Ctrl Pts',(-0.0167090295677126,2.4218424306681,
11.4688536305295));
#40298=CARTESIAN_POINT('Ctrl Pts',(-0.0156450045574491,2.42189518066471,
11.468787166297));
#40299=CARTESIAN_POINT('Ctrl Pts',(-0.0153325101002077,2.42191021673564,
11.4687676731249));
#40300=CARTESIAN_POINT('Ctrl Pts',(-0.0147961569684847,2.42193524127602,
11.4687342623279));
#40301=CARTESIAN_POINT('Ctrl Pts',(-0.0145723092897989,2.42194545134163,
11.4687203321926));
#40302=CARTESIAN_POINT('Ctrl Pts',(-0.0141438508557647,2.42196454626536,
11.4686936958779));
#40303=CARTESIAN_POINT('Ctrl Pts',(-0.0139392425620056,2.42197346953789,
11.4686809875242));
#40304=CARTESIAN_POINT('Ctrl Pts',(-0.0134575333082109,2.42199401755607,
11.4686510954841));
#40305=CARTESIAN_POINT('Ctrl Pts',(-0.0131804250432202,2.42200547967644,
11.46863392099));
#40306=CARTESIAN_POINT('Ctrl Pts',(-0.0123627202737596,2.42203824535184,
11.468583303329));
#40307=CARTESIAN_POINT('Ctrl Pts',(-0.0118220811168599,2.42205854550056,
11.4685499161619));
#40308=CARTESIAN_POINT('Ctrl Pts',(-0.00711694632201651,2.42222335197574,
11.4682600229133));
#40309=CARTESIAN_POINT('Ctrl Pts',(-0.00294982476750907,2.42228844537827,
11.4680078600452));
#40310=CARTESIAN_POINT('Ctrl Pts',(0.0348191690993515,2.42214574517247,
11.4657544547342));
#40311=CARTESIAN_POINT('Ctrl Pts',(0.0681982705008702,2.41676484451376,
11.4639737192927));
#40312=CARTESIAN_POINT('Ctrl Pts',(0.109349437952026,2.40331109514354,11.4614842261548));
#40313=CARTESIAN_POINT('Ctrl Pts',(0.118411268170538,2.39988942290897,11.4609179314254));
#40314=CARTESIAN_POINT('Ctrl Pts',(0.129566858940363,2.39509264252856,11.4601906293601));
#40315=CARTESIAN_POINT('Ctrl Pts',(0.131817648449671,2.39409411020995,11.4600423146492));
#40316=CARTESIAN_POINT('Ctrl Pts',(0.135089797935967,2.39259735585401,11.4598242933062));
#40317=CARTESIAN_POINT('Ctrl Pts',(0.13612035074755,2.39211935269724,11.4597552762567));
#40318=CARTESIAN_POINT('Ctrl Pts',(0.137732722919111,2.39136109844096,11.4596467320565));
#40319=CARTESIAN_POINT('Ctrl Pts',(0.138316270542451,2.39108452714142,11.4596073317756));
#40320=CARTESIAN_POINT('Ctrl Pts',(0.139413540868271,2.3905604333434,11.4595330249397));
#40321=CARTESIAN_POINT('Ctrl Pts',(0.139927446235233,2.39031329729384,11.4594981318693));
#40322=CARTESIAN_POINT('Ctrl Pts',(0.140800361237079,2.38989065798852,11.459438705858));
#40323=CARTESIAN_POINT('Ctrl Pts',(0.141159706592269,2.38971584793727,11.4594141970884));
#40324=CARTESIAN_POINT('Ctrl Pts',(0.141875440732306,2.38936601836966,11.4593652902418));
#40325=CARTESIAN_POINT('Ctrl Pts',(0.14223183307106,2.38919100769059,11.4593408925058));
#40326=CARTESIAN_POINT('Ctrl Pts',(0.14302225731945,2.38880104591987,11.459286681423));
#40327=CARTESIAN_POINT('Ctrl Pts',(0.143456129273519,2.38858577439461,11.4592568569069));
#40328=CARTESIAN_POINT('Ctrl Pts',(0.144934102996692,2.38784830077549,11.459155028864));
#40329=CARTESIAN_POINT('Ctrl Pts',(0.14597584252845,2.38732140855043,11.4590828610627));
#40330=CARTESIAN_POINT('Ctrl Pts',(0.156555869938985,2.38189783899782,11.4583458390003));
#40331=CARTESIAN_POINT('Ctrl Pts',(0.165845996589991,2.37653425400956,11.4576644588148));
#40332=CARTESIAN_POINT('Ctrl Pts',(0.191418932790986,2.3600172712934,11.4556862858127));
#40333=CARTESIAN_POINT('Ctrl Pts',(0.206967948304152,2.34781905697087,11.4543547210414));
#40334=CARTESIAN_POINT('Ctrl Pts',(0.224239975295333,2.33150363854518,11.4527470631791));
#40335=CARTESIAN_POINT('Ctrl Pts',(0.227124799251591,2.3286740633799,11.4524738420395));
#40336=CARTESIAN_POINT('Ctrl Pts',(0.232897783138565,2.32279459709926,11.4519183112049));
#40337=CARTESIAN_POINT('Ctrl Pts',(0.235781107814682,2.31974093962852,11.4516361155775));
#40338=CARTESIAN_POINT('Ctrl Pts',(0.245801185449163,2.30870455873079,11.4506405023665));
#40339=CARTESIAN_POINT('Ctrl Pts',(0.252599707040138,2.30042269000668,11.4499368973252));
#40340=CARTESIAN_POINT('Ctrl Pts',(0.259873551972031,2.29060219656546,11.4491640796824));
#40341=CARTESIAN_POINT('Ctrl Pts',(0.260764673861288,2.28938121720207,11.4490690322456));
#40342=CARTESIAN_POINT('Ctrl Pts',(0.261885802040222,2.28782217480185,11.4489490262113));
#40343=CARTESIAN_POINT('Ctrl Pts',(0.262123781509663,2.28748990860582,11.4489235280372));
#40344=CARTESIAN_POINT('Ctrl Pts',(0.262503270459444,2.28695793251417,11.4488828294243));
#40345=CARTESIAN_POINT('Ctrl Pts',(0.262645184616516,2.28675851394405,11.4488676010649));
#40346=CARTESIAN_POINT('Ctrl Pts',(0.26291378186107,2.28638016792461,11.4488387626131));
#40347=CARTESIAN_POINT('Ctrl Pts',(0.263040508499757,2.28620127436881,11.4488251495694));
#40348=CARTESIAN_POINT('Ctrl Pts',(0.263330057784839,2.28579164685265,11.4487940302376));
#40349=CARTESIAN_POINT('Ctrl Pts',(0.263492759516144,2.28556082845583,11.4487765323604));
#40350=CARTESIAN_POINT('Ctrl Pts',(0.263992073592508,2.28485049080302,11.4487227968521));
#40351=CARTESIAN_POINT('Ctrl Pts',(0.264327684286568,2.28437026387744,11.4486866278184));
#40352=CARTESIAN_POINT('Ctrl Pts',(0.266843949689678,2.28074873476982,11.4484150402188));
#40353=CARTESIAN_POINT('Ctrl Pts',(0.268969963243728,2.27756959371364,11.4481832570298));
#40354=CARTESIAN_POINT('Ctrl Pts',(0.271353787627852,2.27386384363646,11.4479197001052));
#40355=CARTESIAN_POINT('Ctrl Pts',(0.271667253712895,2.27337363540563,11.4478849674402));
#40356=CARTESIAN_POINT('Ctrl Pts',(0.288269994341243,2.24725415373155,11.4460411581386));
#40357=CARTESIAN_POINT('Ctrl Pts',(0.30085862087886,2.21944874733956,11.4444151023456));
#40358=CARTESIAN_POINT('Ctrl Pts',(0.31146520517992,2.18310588371104,11.4422597171165));
#40359=CARTESIAN_POINT('Ctrl Pts',(0.313310588607304,2.17585266633669,11.4418289820176));
#40360=CARTESIAN_POINT('Ctrl Pts',(0.316128907222517,2.16290451368283,11.4410535042307));
#40361=CARTESIAN_POINT('Ctrl Pts',(0.31720432306609,2.15723526241841,11.4407118033176));
#40362=CARTESIAN_POINT('Ctrl Pts',(0.318468392006984,2.14943295465982,11.4402371406345));
#40363=CARTESIAN_POINT('Ctrl Pts',(0.318788873850223,2.14732216489365,11.4401082940329));
#40364=CARTESIAN_POINT('Ctrl Pts',(0.319231747721815,2.14419628688937,11.4399167817488));
#40365=CARTESIAN_POINT('Ctrl Pts',(0.319370324105763,2.14318352199022,11.4398546242671));
#40366=CARTESIAN_POINT('Ctrl Pts',(0.319582514386165,2.14157585158959,11.4397557762692));
#40367=CARTESIAN_POINT('Ctrl Pts',(0.319659291547239,2.14098136474885,11.439719185386));
#40368=CARTESIAN_POINT('Ctrl Pts',(0.319801633734589,2.13985446582775,11.4396497495591));
#40369=CARTESIAN_POINT('Ctrl Pts',(0.319867528948603,2.13932209689917,11.4396169151304));
#40370=CARTESIAN_POINT('Ctrl Pts',(0.31996140237849,2.13854783917416,11.4395691152713));
#40371=CARTESIAN_POINT('Ctrl Pts',(0.319990436357057,2.13830607727909,11.4395541831574));
#40372=CARTESIAN_POINT('Ctrl Pts',(0.320064618999412,2.13768239892331,11.4395156452872));
#40373=CARTESIAN_POINT('Ctrl Pts',(0.320109357994325,2.13730043493417,11.4394920266442));
#40374=CARTESIAN_POINT('Ctrl Pts',(0.320210661597778,2.13642193802021,11.4394376664272));
#40375=CARTESIAN_POINT('Ctrl Pts',(0.320266755062864,2.13592535270603,11.4394069100561));
#40376=CARTESIAN_POINT('Ctrl Pts',(0.32042950410366,2.13445388649695,11.4393156887068));
#40377=CARTESIAN_POINT('Ctrl Pts',(0.320532864331179,2.13347865356412,11.4392551200791));
#40378=CARTESIAN_POINT('Ctrl Pts',(0.321207458607547,2.12682398969673,11.4388410488103));
#40379=CARTESIAN_POINT('Ctrl Pts',(0.321632135590966,2.12113103200114,11.4384829612592));
#40380=CARTESIAN_POINT('Ctrl Pts',(0.323401327081103,2.08422180573654,11.4361344265199));
#40381=CARTESIAN_POINT('Ctrl Pts',(0.320350390423041,2.05296599248663,11.4339977024744));
#40382=CARTESIAN_POINT('Ctrl Pts',(0.309558844462763,2.00931922038741,11.4309785531798));
#40383=CARTESIAN_POINT('Ctrl Pts',(0.305414583016254,1.99621312605224,11.4300710101978));
#40384=CARTESIAN_POINT('Ctrl Pts',(0.300171775123826,1.98270270036126,11.4291612766139));
#40385=CARTESIAN_POINT('Ctrl Pts',(0.299894839063215,1.98199645507691,11.429113798996));
#40386=CARTESIAN_POINT('Ctrl Pts',(0.299499789011998,1.98099936751194,11.429046886384));
#40387=CARTESIAN_POINT('Ctrl Pts',(0.299383742588535,1.98070771681925,11.4290273284594));
#40388=CARTESIAN_POINT('Ctrl Pts',(0.299184050149406,1.98020797163346,11.4289938407599));
#40389=CARTESIAN_POINT('Ctrl Pts',(0.29910061282879,1.97999979445627,11.4289798983277));
#40390=CARTESIAN_POINT('Ctrl Pts',(0.298940646929157,1.97960188085142,11.4289532629432));
#40391=CARTESIAN_POINT('Ctrl Pts',(0.298864155086619,1.97941213043648,11.4289405677695));
#40392=CARTESIAN_POINT('Ctrl Pts',(0.298683862137945,1.97896610982035,11.4289107413907));
#40393=CARTESIAN_POINT('Ctrl Pts',(0.2985799116175,1.97870989960647,11.428893619277));
#40394=CARTESIAN_POINT('Ctrl Pts',(0.298272832111733,1.97795581789813,11.4288432573979));
#40395=CARTESIAN_POINT('Ctrl Pts',(0.298068785393743,1.97745831752176,11.4288100728361));
#40396=CARTESIAN_POINT('Ctrl Pts',(0.296306614940954,1.97319229100682,11.4285258539455));
#40397=CARTESIAN_POINT('Ctrl Pts',(0.294678251095913,1.96945293103433,11.4282789774995));
#40398=CARTESIAN_POINT('Ctrl Pts',(0.292524022787654,1.96475183592434,11.4279702517209));
#40399=CARTESIAN_POINT('Ctrl Pts',(0.292063731776089,1.96376070157079,11.4279052569048));
#40400=CARTESIAN_POINT('Ctrl Pts',(0.291549097490608,1.96266714601046,11.4278336293091));
#40401=CARTESIAN_POINT('Ctrl Pts',(0.291499736042787,1.96256240354417,11.4278267695566));
#40402=CARTESIAN_POINT('Ctrl Pts',(0.291262961256112,1.96206068094208,11.4277939149084));
#40403=CARTESIAN_POINT('Ctrl Pts',(0.291074792508294,1.96166405560422,11.4277679543356));
#40404=CARTESIAN_POINT('Ctrl Pts',(0.280057161954155,1.93856291004629,11.4262565256465));
#40405=CARTESIAN_POINT('Ctrl Pts',(0.26660633350777,1.91720146391741,11.4248884855704));
#40406=CARTESIAN_POINT('Ctrl Pts',(0.239618237195677,1.88375551133249,11.4224661705895));
#40407=CARTESIAN_POINT('Ctrl Pts',(0.227301585258933,1.87084407132313,11.4214422151618));
#40408=CARTESIAN_POINT('Ctrl Pts',(0.212675172725801,1.85785644170849,11.4202636956892));
#40409=CARTESIAN_POINT('Ctrl Pts',(0.211358525140154,1.85670633879562,11.4201579346938));
#40410=CARTESIAN_POINT('Ctrl Pts',(0.209363430169687,1.85499202431341,11.4199981328109));
#40411=CARTESIAN_POINT('Ctrl Pts',(0.20869190239758,1.85441978114678,11.4199444219011));
#40412=CARTESIAN_POINT('Ctrl Pts',(0.2076045101523,1.8535008395092,11.4198575680532));
#40413=CARTESIAN_POINT('Ctrl Pts',(0.207190103872449,1.85315241623636,11.419824495693));
#40414=CARTESIAN_POINT('Ctrl Pts',(0.206394984843502,1.85248731126307,11.4197610918534));
#40415=CARTESIAN_POINT('Ctrl Pts',(0.206014416009136,1.85217045929425,11.419730767429));
#40416=CARTESIAN_POINT('Ctrl Pts',(0.205335787486942,1.85160809369365,11.4196767325492));
#40417=CARTESIAN_POINT('Ctrl Pts',(0.205038013334749,1.85136223571826,11.4196530361506));
#40418=CARTESIAN_POINT('Ctrl Pts',(0.20444782292304,1.85087672475632,11.4196060959728));
#40419=CARTESIAN_POINT('Ctrl Pts',(0.204155425333689,1.85063704992314,11.4195828531303));
#40420=CARTESIAN_POINT('Ctrl Pts',(0.203447407510393,1.85005877612463,11.4195266026581));
#40421=CARTESIAN_POINT('Ctrl Pts',(0.203031363903342,1.84972069945555,11.419493574015));
#40422=CARTESIAN_POINT('Ctrl Pts',(0.201487768961774,1.848472757312,11.41937112307));
#40423=CARTESIAN_POINT('Ctrl Pts',(0.200354942296662,1.84756947125457,11.4192814370363));
#40424=CARTESIAN_POINT('Ctrl Pts',(0.181275877559256,1.83256566414207,11.4177737993979));
#40425=CARTESIAN_POINT('Ctrl Pts',(0.161891611982213,1.82040604046788,11.4162769405174));
#40426=CARTESIAN_POINT('Ctrl Pts',(0.125092269501113,1.80243987375647,11.41351982038));
#40427=CARTESIAN_POINT('Ctrl Pts',(0.108151860438058,1.79587288790738,11.4122808171936));
#40428=CARTESIAN_POINT('Ctrl Pts',(0.0846397711225724,1.7889729609589,11.4106593261453));
#40429=CARTESIAN_POINT('Ctrl Pts',(0.078478514648324,1.7873614803117,11.4102433906528));
#40430=CARTESIAN_POINT('Ctrl Pts',(0.06934940390309,1.78526068437766,11.4096440118448));
#40431=CARTESIAN_POINT('Ctrl Pts',(0.0664162700588182,1.78462869933861,
11.4094539725711));
#40432=CARTESIAN_POINT('Ctrl Pts',(0.062979010804003,1.78393817795183,11.4092345664235));
#40433=CARTESIAN_POINT('Ctrl Pts',(0.0624831720564446,1.78383978052845,
11.4092029960339));
#40434=CARTESIAN_POINT('Ctrl Pts',(0.0617261136775131,1.78369139555529,
11.4091549175691));
#40435=CARTESIAN_POINT('Ctrl Pts',(0.0614650631572211,1.78364056459812,
11.4091383615193));
#40436=CARTESIAN_POINT('Ctrl Pts',(0.0609920549182021,1.78354906945807,
11.4091084039986));
#40437=CARTESIAN_POINT('Ctrl Pts',(0.0607801200964875,1.78350829520217,
11.4090949962657));
#40438=CARTESIAN_POINT('Ctrl Pts',(0.0603503060075456,1.78342605069282,
11.4090678350604));
#40439=CARTESIAN_POINT('Ctrl Pts',(0.0601324258355243,1.78338459263799,
11.409054082332));
#40440=CARTESIAN_POINT('Ctrl Pts',(0.0595058004750214,1.78326602905287,
11.4090145742024));
#40441=CARTESIAN_POINT('Ctrl Pts',(0.0590969466601207,1.7831894895333,11.4089888512012));
#40442=CARTESIAN_POINT('Ctrl Pts',(0.0573056209852522,1.78285773258151,
11.4088763856765));
#40443=CARTESIAN_POINT('Ctrl Pts',(0.0559216089114385,1.78261076608365,
11.4087901068411));
#40444=CARTESIAN_POINT('Ctrl Pts',(0.0290012912009832,1.77798859707933,
11.4071230451104));
#40445=CARTESIAN_POINT('Ctrl Pts',(0.0030263258399031,1.77669868232371,
11.4057041329939));
#40446=CARTESIAN_POINT('Ctrl Pts',(-0.0464229641918105,1.78020991766549,
11.4029276692986));
#40447=CARTESIAN_POINT('Ctrl Pts',(-0.0697593588392407,1.78447793757808,
11.4015823151899));
#40448=CARTESIAN_POINT('Ctrl Pts',(-0.0935197057024527,1.79159026387387,
11.4000741097969));
#40449=CARTESIAN_POINT('Ctrl Pts',(-0.0946206878970762,1.79192626522192,
11.4000039201711));
#40450=CARTESIAN_POINT('Ctrl Pts',(-0.0962224496205946,1.79242449239783,
11.399901353231));
#40451=CARTESIAN_POINT('Ctrl Pts',(-0.0967246778120061,1.79258206073052,
11.3998691287208));
#40452=CARTESIAN_POINT('Ctrl Pts',(-0.0976045129501196,1.79286046840959,
11.3998125610325));
#40453=CARTESIAN_POINT('Ctrl Pts',(-0.0979822881245507,1.79298077580482,
11.3997882353785));
#40454=CARTESIAN_POINT('Ctrl Pts',(-0.0987147319342856,1.79321552156216,
11.3997409994211));
#40455=CARTESIAN_POINT('Ctrl Pts',(-0.099069426142199,1.79332987867535,
11.3997180918234));
#40456=CARTESIAN_POINT('Ctrl Pts',(-0.100011515011491,1.79363542294212,
11.3996571595791));
#40457=CARTESIAN_POINT('Ctrl Pts',(-0.100598557546721,1.7938276834497,11.399619099606));
#40458=CARTESIAN_POINT('Ctrl Pts',(-0.102685099663265,1.7945176892436,11.3994834942132));
#40459=CARTESIAN_POINT('Ctrl Pts',(-0.104181468755356,1.79502476608227,
11.3993856410926));
#40460=CARTESIAN_POINT('Ctrl Pts',(-0.12899374249744,1.80363685690961,11.3977528514854));
#40461=CARTESIAN_POINT('Ctrl Pts',(-0.15130124512736,1.81438147232735,11.3961246305909));
#40462=CARTESIAN_POINT('Ctrl Pts',(-0.181975728002518,1.83376545720852,
11.393674846602));
#40463=CARTESIAN_POINT('Ctrl Pts',(-0.191449045639193,1.84049419208442,
11.3928860442356));
#40464=CARTESIAN_POINT('Ctrl Pts',(-0.208370023553719,1.85394473579229,
11.3914354188375));
#40465=CARTESIAN_POINT('Ctrl Pts',(-0.215908032359701,1.86053180516414,
11.3907719916862));
#40466=CARTESIAN_POINT('Ctrl Pts',(-0.225865789374535,1.87008649868474,
11.3898841502351));
#40467=CARTESIAN_POINT('Ctrl Pts',(-0.228557198741824,1.87276183652576,
11.3896429557711));
#40468=CARTESIAN_POINT('Ctrl Pts',(-0.231574433270721,1.87586891110053,
11.3893718040988));
#40469=CARTESIAN_POINT('Ctrl Pts',(-0.231947037657232,1.87625453102284,
11.389338305572));
#40470=CARTESIAN_POINT('Ctrl Pts',(-0.232507455706521,1.87683742954081,
11.3892879040854));
#40471=CARTESIAN_POINT('Ctrl Pts',(-0.232695982221152,1.87703401678166,
11.389270945801));
#40472=CARTESIAN_POINT('Ctrl Pts',(-0.233035115930447,1.87738854926842,
11.389240435029));
#40473=CARTESIAN_POINT('Ctrl Pts',(-0.233185811563569,1.87754640812089,
11.3892268756263));
#40474=CARTESIAN_POINT('Ctrl Pts',(-0.233509580011898,1.87788625719874,
11.3891977395314));
#40475=CARTESIAN_POINT('Ctrl Pts',(-0.233682599952229,1.87806829613795,
11.3891821669704));
#40476=CARTESIAN_POINT('Ctrl Pts',(-0.234148642674469,1.87855978148246,
11.3891402139529));
#40477=CARTESIAN_POINT('Ctrl Pts',(-0.234441266027767,1.87886960853007,
11.3891138644934));
#40478=CARTESIAN_POINT('Ctrl Pts',(-0.235791390892575,1.88030480125339,
11.3889922512655));
#40479=CARTESIAN_POINT('Ctrl Pts',(-0.236841432429995,1.88143720243551,
11.3888975533506));
#40480=CARTESIAN_POINT('Ctrl Pts',(-0.259372643302606,1.9060886997761,11.3868619276317));
#40481=CARTESIAN_POINT('Ctrl Pts',(-0.277261718287582,1.9326605253831,11.3851601879815));
#40482=CARTESIAN_POINT('Ctrl Pts',(-0.298528101470506,1.97731458201701,
11.3823575257023));
#40483=CARTESIAN_POINT('Ctrl Pts',(-0.304778660268125,1.99378997435736,
11.3813365373181));
#40484=CARTESIAN_POINT('Ctrl Pts',(-0.30996516036343,2.01177278597578,11.3801982217841));
#40485=CARTESIAN_POINT('Ctrl Pts',(-0.310271334769157,2.01285563297686,
11.3801295974769));
#40486=CARTESIAN_POINT('Ctrl Pts',(-0.310711089494955,2.01444261310416,
11.3800289000181));
#40487=CARTESIAN_POINT('Ctrl Pts',(-0.310849129633137,2.01494551047207,
11.3799969718492));
#40488=CARTESIAN_POINT('Ctrl Pts',(-0.31108976779386,2.0158305958635,11.3799407463367));
#40489=CARTESIAN_POINT('Ctrl Pts',(-0.311192883929079,2.01621264290853,
11.3799164658603));
#40490=CARTESIAN_POINT('Ctrl Pts',(-0.311392120010616,2.01695625736643,
11.3798691851972));
#40491=CARTESIAN_POINT('Ctrl Pts',(-0.311488314563644,2.01731780431216,
11.3798461874716));
#40492=CARTESIAN_POINT('Ctrl Pts',(-0.311743586295423,2.01828401045264,
11.3797847013309));
#40493=CARTESIAN_POINT('Ctrl Pts',(-0.311901533189148,2.01888896419416,
11.3797461763876));
#40494=CARTESIAN_POINT('Ctrl Pts',(-0.312463938284782,2.02106897137341,
11.3796072459193));
#40495=CARTESIAN_POINT('Ctrl Pts',(-0.312858229029909,2.0226466007139,11.3795065125137));
#40496=CARTESIAN_POINT('Ctrl Pts',(-0.319266889452423,2.04913962117935,
11.3778115051525));
#40497=CARTESIAN_POINT('Ctrl Pts',(-0.322298473416595,2.07467656809684,
11.3761160603101));
#40498=CARTESIAN_POINT('Ctrl Pts',(-0.322253346302143,2.12364577356137,
11.3728067123969));
#40499=CARTESIAN_POINT('Ctrl Pts',(-0.319694501316975,2.14692529899204,
11.3712117409314));
#40500=CARTESIAN_POINT('Ctrl Pts',(-0.314359649194358,2.17099921377188,
11.3696549685826));
#40501=CARTESIAN_POINT('Ctrl Pts',(-0.314069674331122,2.17227113670679,
11.3695730133649));
#40502=CARTESIAN_POINT('Ctrl Pts',(-0.313679796577574,2.17393459291369,
11.3694662490481));
#40503=CARTESIAN_POINT('Ctrl Pts',(-0.313586874787494,2.1743277254833,11.3694410476469));
#40504=CARTESIAN_POINT('Ctrl Pts',(-0.313442351362779,2.17493407850222,
11.369402226484));
#40505=CARTESIAN_POINT('Ctrl Pts',(-0.313391271220161,2.17514742093047,
11.3693885767228));
#40506=CARTESIAN_POINT('Ctrl Pts',(-0.313288962954833,2.17557280530305,
11.3693613791507));
#40507=CARTESIAN_POINT('Ctrl Pts',(-0.313237737731742,2.17578484592476,
11.3693478313569));
#40508=CARTESIAN_POINT('Ctrl Pts',(-0.31312238908277,2.17626020276741,11.3693174804528));
#40509=CARTESIAN_POINT('Ctrl Pts',(-0.313058148939225,2.1765234895641,11.3693006842261));
#40510=CARTESIAN_POINT('Ctrl Pts',(-0.312867386664942,2.17730106392869,
11.3692511206979));
#40511=CARTESIAN_POINT('Ctrl Pts',(-0.312739928028976,2.17781512416576,
11.3692184073775));
#40512=CARTESIAN_POINT('Ctrl Pts',(-0.311735517035027,2.18182373706968,
11.3689637117584));
#40513=CARTESIAN_POINT('Ctrl Pts',(-0.310801242347256,2.18530385064392,
11.3687449750859));
#40514=CARTESIAN_POINT('Ctrl Pts',(-0.307295983124388,2.1975375743701,11.367982111548));
#40515=CARTESIAN_POINT('Ctrl Pts',(-0.304411744969148,2.20619754121014,
11.3674531122003));
#40516=CARTESIAN_POINT('Ctrl Pts',(-0.291928334298789,2.23896789179042,
11.3654534256326));
#40517=CARTESIAN_POINT('Ctrl Pts',(-0.279799623035608,2.26200765349055,
11.3640441005038));
#40518=CARTESIAN_POINT('Ctrl Pts',(-0.261908755108897,2.28787033300837,
11.3622303962566));
#40519=CARTESIAN_POINT('Ctrl Pts',(-0.258662816353377,2.29231484830051,
11.3619098155108));
#40520=CARTESIAN_POINT('Ctrl Pts',(-0.254253890372147,2.29803812845045,
11.3614836535988));
#40521=CARTESIAN_POINT('Ctrl Pts',(-0.253192075065908,2.29939386663975,
11.3613816908475));
#40522=CARTESIAN_POINT('Ctrl Pts',(-0.248909954603756,2.30477196992698,
11.3609730305071));
#40523=CARTESIAN_POINT('Ctrl Pts',(-0.245604389998335,2.30872518817796,
11.3606631854897));
#40524=CARTESIAN_POINT('Ctrl Pts',(-0.241634750866392,2.31324767682501,
11.3602967438195));
#40525=CARTESIAN_POINT('Ctrl Pts',(-0.241061270838694,2.31389574137006,
11.3602439384914));
#40526=CARTESIAN_POINT('Ctrl Pts',(-0.240141007125877,2.31492728917213,
11.360159409913));
#40527=CARTESIAN_POINT('Ctrl Pts',(-0.239795895994813,2.3153122643823,11.36012775688));
#40528=CARTESIAN_POINT('Ctrl Pts',(-0.239184544853084,2.31599094025439,
11.3600717655193));
#40529=CARTESIAN_POINT('Ctrl Pts',(-0.23891868589476,2.31628498398328,11.3600474432997));
#40530=CARTESIAN_POINT('Ctrl Pts',(-0.23836726707907,2.31689260357345,11.3599970514745));
#40531=CARTESIAN_POINT('Ctrl Pts',(-0.238081629523655,2.31720610760345,
11.3599709786015));
#40532=CARTESIAN_POINT('Ctrl Pts',(-0.237347416437861,2.31800876134596,
11.3599040369711));
#40533=CARTESIAN_POINT('Ctrl Pts',(-0.23689794883459,2.31849708908991,11.3598631302928));
#40534=CARTESIAN_POINT('Ctrl Pts',(-0.235046242546941,2.32049646033625,
11.3596949006925));
#40535=CARTESIAN_POINT('Ctrl Pts',(-0.233631054122086,2.32199539497185,
11.3595670238161));
#40536=CARTESIAN_POINT('Ctrl Pts',(-0.22413656197855,2.3318603950268,11.3587135207124));
#40537=CARTESIAN_POINT('Ctrl Pts',(-0.215624758982773,2.33979647510923,
11.357968864963));
#40538=CARTESIAN_POINT('Ctrl Pts',(-0.181055528946665,2.36869617858792,
11.3550181370014));
#40539=CARTESIAN_POINT('Ctrl Pts',(-0.152232497679068,2.38601319419522,
11.3526824613742));
#40540=CARTESIAN_POINT('Ctrl Pts',(-0.117208616749167,2.40023739173137,
11.3502400099718));
#40541=CARTESIAN_POINT('Ctrl Pts',(-0.113118033792052,2.40180236311669,
11.3499607862732));
#40542=CARTESIAN_POINT('Ctrl Pts',(-0.108430467011868,2.40348702003269,
11.3496486443292));
#40543=CARTESIAN_POINT('Ctrl Pts',(-0.107863778379305,2.4036888915195,11.3496110379291));
#40544=CARTESIAN_POINT('Ctrl Pts',(-0.107026203868007,2.40398462048627,
11.3495556489169));
#40545=CARTESIAN_POINT('Ctrl Pts',(-0.106755756827718,2.40407970368351,
11.3495377939667));
#40546=CARTESIAN_POINT('Ctrl Pts',(-0.106277095754183,2.40424727303559,
11.3495062458134));
#40547=CARTESIAN_POINT('Ctrl Pts',(-0.106068933964605,2.40431990648054,
11.3494925438038));
#40548=CARTESIAN_POINT('Ctrl Pts',(-0.105633923129305,2.40447119330934,
11.3494639469764));
#40549=CARTESIAN_POINT('Ctrl Pts',(-0.105407061199591,2.40454980663443,
11.3494490545828));
#40550=CARTESIAN_POINT('Ctrl Pts',(-0.104813468497689,2.40475475861509,
11.3494101427263));
#40551=CARTESIAN_POINT('Ctrl Pts',(-0.104446595726837,2.40488068932269,
11.3493861475778));
#40552=CARTESIAN_POINT('Ctrl Pts',(-0.102842839134792,2.40542795133668,
11.3492814889179));
#40553=CARTESIAN_POINT('Ctrl Pts',(-0.101603604243687,2.4058424279928,11.3492012266636));
#40554=CARTESIAN_POINT('Ctrl Pts',(-0.0924298191168617,2.40884879544283,
11.3486113104357));
#40555=CARTESIAN_POINT('Ctrl Pts',(-0.0843990020981954,2.41113933395943,
11.348118284486));
#40556=CARTESIAN_POINT('Ctrl Pts',(-0.0608749879572826,2.41687073066331,
11.3467171688794));
#40557=CARTESIAN_POINT('Ctrl Pts',(-0.0452051845918544,2.41948298976214,
11.3458361389578));
#40558=CARTESIAN_POINT('Ctrl Pts',(-0.00452228508986718,2.42321063729027,
11.3435515659846));
#40559=CARTESIAN_POINT('Ctrl Pts',(0.02053775698261,2.42258876656911,11.3421403900052));
#40560=CARTESIAN_POINT('Ctrl Pts',(0.0467323080080221,2.41887213776658,
11.3405353959467));
#40561=CARTESIAN_POINT('Ctrl Pts',(0.0481904201930731,2.41865503627687,
11.340445654233));
#40562=CARTESIAN_POINT('Ctrl Pts',(0.050180546179098,2.41834475028077,11.3403226053533));
#40563=CARTESIAN_POINT('Ctrl Pts',(0.0507139069303691,2.41826021882167,
11.3402895724247));
#40564=CARTESIAN_POINT('Ctrl Pts',(0.0516213770467913,2.418114056295,11.3402332743332));
#40565=CARTESIAN_POINT('Ctrl Pts',(0.0519955959776072,2.41805310465016,
11.3402100307555));
#40566=CARTESIAN_POINT('Ctrl Pts',(0.0527192841295516,2.41793392116256,
11.340165027124));
#40567=CARTESIAN_POINT('Ctrl Pts',(0.0530687667862062,2.41787577311767,
11.3401432697593));
#40568=CARTESIAN_POINT('Ctrl Pts',(0.053898022902754,2.41773639315297,11.3400915857229));
#40569=CARTESIAN_POINT('Ctrl Pts',(0.0543777086429537,2.4176546508479,11.3400616428753));
#40570=CARTESIAN_POINT('Ctrl Pts',(0.0557929840800038,2.41741017684335,
11.339973161816));
#40571=CARTESIAN_POINT('Ctrl Pts',(0.0567280356482728,2.41724439691957,
11.3399145267954));
#40572=CARTESIAN_POINT('Ctrl Pts',(0.0640509930196899,2.41591266314197,
11.3394539141401));
#40573=CARTESIAN_POINT('Ctrl Pts',(0.0704026703108798,2.41455809409364,
11.3390459532616));
#40574=CARTESIAN_POINT('Ctrl Pts',(0.0829432737469404,2.41148481926685,
11.3382227377634));
#40575=CARTESIAN_POINT('Ctrl Pts',(0.0891303931241315,2.40977111455441,
11.3378078056179));
#40576=CARTESIAN_POINT('Ctrl Pts',(0.12618682374267,2.39830516734182,11.3352699337926));
#40577=CARTESIAN_POINT('Ctrl Pts',(0.155488028036088,2.38413396138863,11.3330145199447));
#40578=CARTESIAN_POINT('Ctrl Pts',(0.18246282617565,2.36564752262211,11.3308858038243));
#40579=CARTESIAN_POINT('Ctrl Pts',(0.182740533754245,2.3654565624283,11.3308638849336));
#40580=CARTESIAN_POINT('Ctrl Pts',(0.183379332606582,2.36501582739628,11.3308134584491));
#40581=CARTESIAN_POINT('Ctrl Pts',(0.183740214838645,2.36476574901755,11.3307849651146));
#40582=CARTESIAN_POINT('Ctrl Pts',(0.18811028475716,2.36172421019724,11.3304398719187));
#40583=CARTESIAN_POINT('Ctrl Pts',(0.192056286464393,2.35884248242849,11.3301276894277));
#40584=CARTESIAN_POINT('Ctrl Pts',(0.196384680129769,2.35552798891617,11.3297859787899));
#40585=CARTESIAN_POINT('Ctrl Pts',(0.196832965692875,2.35518283511489,11.3297505972382));
#40586=CARTESIAN_POINT('Ctrl Pts',(0.197504640355259,2.35466286168595,11.3296976007998));
#40587=CARTESIAN_POINT('Ctrl Pts',(0.197728708399935,2.35448892698888,11.3296799241469));
#40588=CARTESIAN_POINT('Ctrl Pts',(0.198115442409466,2.35418790237786,11.3296494200222));
#40589=CARTESIAN_POINT('Ctrl Pts',(0.198278215942483,2.35406095197721,11.3296365826508));
#40590=CARTESIAN_POINT('Ctrl Pts',(0.19861284832173,2.35379944788421,11.3296101948599));
#40591=CARTESIAN_POINT('Ctrl Pts',(0.198784692216103,2.35366487617642,11.3295966458465));
#40592=CARTESIAN_POINT('Ctrl Pts',(0.199189694368833,2.35334705292501,11.3295647177061));
#40593=CARTESIAN_POINT('Ctrl Pts',(0.199422737410001,2.3531636533433,11.3295463491652));
#40594=CARTESIAN_POINT('Ctrl Pts',(0.19991584763242,2.35277448341472,11.3295074882116));
#40595=CARTESIAN_POINT('Ctrl Pts',(0.200175851280654,2.35256863258638,11.3294870015374));
#40596=CARTESIAN_POINT('Ctrl Pts',(0.200878252913607,2.35201075922419,11.3294316651193));
#40597=CARTESIAN_POINT('Ctrl Pts',(0.201320045589448,2.35165797128934,11.3293968690411));
#40598=CARTESIAN_POINT('Ctrl Pts',(0.213573677646391,2.34182007065545,11.3284319410117));
#40599=CARTESIAN_POINT('Ctrl Pts',(0.224704873299075,2.33151353625263,11.327559757136));
#40600=CARTESIAN_POINT('Ctrl Pts',(0.255400806295196,2.29878333129684,11.3250249098442));
#40601=CARTESIAN_POINT('Ctrl Pts',(0.272633249537323,2.27440028916025,11.3234068039666));
#40602=CARTESIAN_POINT('Ctrl Pts',(0.288898485470596,2.24293818888046,11.3213070850102));
#40603=CARTESIAN_POINT('Ctrl Pts',(0.291381042673278,2.23780690307811,11.3209649033049));
#40604=CARTESIAN_POINT('Ctrl Pts',(0.294129493499249,2.23171931354814,11.320558263061));
#40605=CARTESIAN_POINT('Ctrl Pts',(0.29452877257205,2.23082407500769,11.3204984463579));
#40606=CARTESIAN_POINT('Ctrl Pts',(0.295125393567224,2.22946979317445,11.3204079282924));
#40607=CARTESIAN_POINT('Ctrl Pts',(0.2953257649204,2.22901208409517,11.3203773306423));
#40608=CARTESIAN_POINT('Ctrl Pts',(0.295681751970442,2.22819372629069,11.3203226139489));
#40609=CARTESIAN_POINT('Ctrl Pts',(0.295837774596875,2.22783325478138,11.3202985088563));
#40610=CARTESIAN_POINT('Ctrl Pts',(0.296165862624206,2.22707142925538,11.320247557236));
#40611=CARTESIAN_POINT('Ctrl Pts',(0.296337771929277,2.22667000924429,11.320220705448));
#40612=CARTESIAN_POINT('Ctrl Pts',(0.296790962609327,2.22560580615584,11.3201495063654));
#40613=CARTESIAN_POINT('Ctrl Pts',(0.297070838473189,2.22494243051109,11.3201051113781));
#40614=CARTESIAN_POINT('Ctrl Pts',(0.29834088854247,2.22190370216548,11.3199016879763));
#40615=CARTESIAN_POINT('Ctrl Pts',(0.299304789493341,2.21951753321753,11.3197417723334));
#40616=CARTESIAN_POINT('Ctrl Pts',(0.303269873599306,2.20935295435963,11.3190596490866));
#40617=CARTESIAN_POINT('Ctrl Pts',(0.305996968363029,2.20147176797048,11.3185283850568));
#40618=CARTESIAN_POINT('Ctrl Pts',(0.312511922447542,2.17998048936091,11.3170724314153));
#40619=CARTESIAN_POINT('Ctrl Pts',(0.315715518841181,2.16621342556584,11.3161314727547));
#40620=CARTESIAN_POINT('Ctrl Pts',(0.321555727886701,2.13069027157465,11.3137039684498));
#40621=CARTESIAN_POINT('Ctrl Pts',(0.32289747059995,2.10879225398944,11.3122056014617));
#40622=CARTESIAN_POINT('Ctrl Pts',(0.321981298021614,2.08622647382615,11.3107459870959));
#40623=CARTESIAN_POINT('Ctrl Pts',(0.321950599739869,2.08552665748753,11.3107008095637));
#40624=CARTESIAN_POINT('Ctrl Pts',(0.321740343714891,2.08106578262378,11.3104134188027));
#40625=CARTESIAN_POINT('Ctrl Pts',(0.321497155651959,2.07730781352421,11.3101739698107));
#40626=CARTESIAN_POINT('Ctrl Pts',(0.321140290116267,2.07297353486125,11.3099015304684));
#40627=CARTESIAN_POINT('Ctrl Pts',(0.32109085533509,2.07239242157138,11.3098650811168));
#40628=CARTESIAN_POINT('Ctrl Pts',(0.321015188402491,2.07153064997296,11.3098111463397));
#40629=CARTESIAN_POINT('Ctrl Pts',(0.320990165425847,2.07124989082816,11.3097935934159));
#40630=CARTESIAN_POINT('Ctrl Pts',(0.320945481107521,2.07075586124075,11.3097627401829));
#40631=CARTESIAN_POINT('Ctrl Pts',(0.320925975516493,2.07054257759177,11.3097494310759));
#40632=CARTESIAN_POINT('Ctrl Pts',(0.320885628894405,2.07010620471909,11.3097222234596));
#40633=CARTESIAN_POINT('Ctrl Pts',(0.320864767894126,2.06988311848417,11.309708326134));
#40634=CARTESIAN_POINT('Ctrl Pts',(0.320808399800986,2.0692870282428,11.3096712238331));
#40635=CARTESIAN_POINT('Ctrl Pts',(0.320772474693204,2.06891406267128,11.3096480424899));
#40636=CARTESIAN_POINT('Ctrl Pts',(0.320692650090385,2.06810021783746,11.3095975292078));
#40637=CARTESIAN_POINT('Ctrl Pts',(0.320648491632602,2.06765936390213,11.3095702117091));
#40638=CARTESIAN_POINT('Ctrl Pts',(0.320517087765459,2.06637422876746,11.3094907064822));
#40639=CARTESIAN_POINT('Ctrl Pts',(0.320427415167719,2.06553019166484,11.3094386512038));
#40640=CARTESIAN_POINT('Ctrl Pts',(0.317235386036507,2.03657477832187,11.3076580867215));
#40641=CARTESIAN_POINT('Ctrl Pts',(0.310448791682766,2.00898789033902,11.3061237860713));
#40642=CARTESIAN_POINT('Ctrl Pts',(0.292419750605674,1.96287986451402,11.3033424926663));
#40643=CARTESIAN_POINT('Ctrl Pts',(0.282763374647675,1.94393618872499,11.3021272706346));
#40644=CARTESIAN_POINT('Ctrl Pts',(0.27061562193278,1.92498557071362,11.3007601152078));
#40645=CARTESIAN_POINT('Ctrl Pts',(0.269907521962876,1.92389550033283,11.3006809240588));
#40646=CARTESIAN_POINT('Ctrl Pts',(0.26891144580463,1.92238223087507,11.300570207493));
#40647=CARTESIAN_POINT('Ctrl Pts',(0.268629020101468,1.92195537877203,11.3005388901509));
#40648=CARTESIAN_POINT('Ctrl Pts',(0.268139806322849,1.92121980545952,11.3004847709626));
#40649=CARTESIAN_POINT('Ctrl Pts',(0.267933498366403,1.92091076485157,11.3004619872092));
#40650=CARTESIAN_POINT('Ctrl Pts',(0.267505610792991,1.92027220164292,11.3004148133478));
#40651=CARTESIAN_POINT('Ctrl Pts',(0.267283955767604,1.91994273051322,11.3003904204184));
#40652=CARTESIAN_POINT('Ctrl Pts',(0.26676488889663,1.91917425277872,11.3003333999611));
#40653=CARTESIAN_POINT('Ctrl Pts',(0.266467002007438,1.91873556983795,11.300300754486));
#40654=CARTESIAN_POINT('Ctrl Pts',(0.265507225842488,1.91732963478781,11.3001958203587));
#40655=CARTESIAN_POINT('Ctrl Pts',(0.264841147969225,1.91636526585228,11.3001233726792));
#40656=CARTESIAN_POINT('Ctrl Pts',(0.254625774337976,1.90174630475253,11.2990178787223));
#40657=CARTESIAN_POINT('Ctrl Pts',(0.244038487195102,1.88885107144398,11.2979439910343));
#40658=CARTESIAN_POINT('Ctrl Pts',(0.229809403740695,1.87402666052507,11.2965813541071));
#40659=CARTESIAN_POINT('Ctrl Pts',(0.227064745038438,1.87126890808962,11.2963218932464));
#40660=CARTESIAN_POINT('Ctrl Pts',(0.203516933220354,1.84845035945618,11.2941254875298));
#40661=CARTESIAN_POINT('Ctrl Pts',(0.180152157028259,1.83122188011563,11.2921222987019));
#40662=CARTESIAN_POINT('Ctrl Pts',(0.153511652218545,1.81663183568528,11.2902016840408));
#40663=CARTESIAN_POINT('Ctrl Pts',(0.152215280648293,1.81593336618361,11.2901090847738));
#40664=CARTESIAN_POINT('Ctrl Pts',(0.150539974389725,1.81504549300565,11.2899905675948));
#40665=CARTESIAN_POINT('Ctrl Pts',(0.150165417586754,1.81484793125153,11.2899641436437));
#40666=CARTESIAN_POINT('Ctrl Pts',(0.149570832201879,1.81453581080391,11.2899223151025));
#40667=CARTESIAN_POINT('Ctrl Pts',(0.14935106053848,1.81442076777894,11.289906879834));
#40668=CARTESIAN_POINT('Ctrl Pts',(0.148941164310051,1.81420680356039,11.2898781392636));
#40669=CARTESIAN_POINT('Ctrl Pts',(0.148751075399112,1.81410781905559,11.2898648300061));
#40670=CARTESIAN_POINT('Ctrl Pts',(0.148322240818617,1.8138850566243,11.2898348477393));
#40671=CARTESIAN_POINT('Ctrl Pts',(0.148083439378098,1.813761388126,11.2898181817485));
#40672=CARTESIAN_POINT('Ctrl Pts',(0.147583922668493,1.81350349499057,11.2897833824373));
#40673=CARTESIAN_POINT('Ctrl Pts',(0.147323178253634,1.81336932689661,11.2897652526915));
#40674=CARTESIAN_POINT('Ctrl Pts',(0.146641821407566,1.81301990472017,11.2897179685363));
#40675=CARTESIAN_POINT('Ctrl Pts',(0.146220916192554,1.8128052184545,11.289688849441));
#40676=CARTESIAN_POINT('Ctrl Pts',(0.144972528190746,1.81217192345535,11.2896027466521));
#40677=CARTESIAN_POINT('Ctrl Pts',(0.144143700632759,1.81175595549363,11.2895459233637));
#40678=CARTESIAN_POINT('Ctrl Pts',(0.141232883023147,1.81031078338081,11.2893475171262));
#40679=CARTESIAN_POINT('Ctrl Pts',(0.139141518589621,1.80930048509612,11.2892070296331));
#40680=CARTESIAN_POINT('Ctrl Pts',(0.132667334532932,1.80625880850857,11.2887778936299));
#40681=CARTESIAN_POINT('Ctrl Pts',(0.128249455929038,1.80430321065738,11.2884931142327));
#40682=CARTESIAN_POINT('Ctrl Pts',(0.116223922539828,1.7993002958613,11.2877351292652));
#40683=CARTESIAN_POINT('Ctrl Pts',(0.108541091946679,1.79644249644365,11.2872689956764));
#40684=CARTESIAN_POINT('Ctrl Pts',(0.077182039404477,1.78612086063972,11.2854084415905));
#40685=CARTESIAN_POINT('Ctrl Pts',(0.0527907366784927,1.7811108512324,11.2840486745648));
#40686=CARTESIAN_POINT('Ctrl Pts',(0.0186781773322447,1.77812873778148,
11.2820530226371));
#40687=CARTESIAN_POINT('Ctrl Pts',(0.00925949832198398,1.77772027806431,
11.2814933064693));
#40688=CARTESIAN_POINT('Ctrl Pts',(-0.00130767159243636,1.77772561986267,
11.2808506894171));
#40689=CARTESIAN_POINT('Ctrl Pts',(-0.00245240735778875,1.77773229801436,
11.2807808852584));
#40690=CARTESIAN_POINT('Ctrl Pts',(-0.00411653486913456,1.77775087332754,
11.2806791256132));
#40691=CARTESIAN_POINT('Ctrl Pts',(-0.0046359807307583,1.77775792767212,
11.2806473218467));
#40692=CARTESIAN_POINT('Ctrl Pts',(-0.00555217478502938,1.77777258582359,
11.2805911549076));
#40693=CARTESIAN_POINT('Ctrl Pts',(-0.00594893121706805,1.77777966652181,
11.2805668081702));
#40694=CARTESIAN_POINT('Ctrl Pts',(-0.0067686959336765,1.77779581101593,
11.2805164543174));
#40695=CARTESIAN_POINT('Ctrl Pts',(-0.00719170127821379,1.77780497509501,
11.2804904441068));
#40696=CARTESIAN_POINT('Ctrl Pts',(-0.00827362898359217,1.77783054592782,
11.2804238471732));
#40697=CARTESIAN_POINT('Ctrl Pts',(-0.00893251893961792,1.77784814113712,
11.2803832232845));
#40698=CARTESIAN_POINT('Ctrl Pts',(-0.0116146488198333,1.77792800037926,
11.2802175819054));
#40699=CARTESIAN_POINT('Ctrl Pts',(-0.0136373005621482,1.77800730328181,
11.2800920316862));
#40700=CARTESIAN_POINT('Ctrl Pts',(-0.0466842568565628,1.77961492217671,
11.2780299958882));
#40701=CARTESIAN_POINT('Ctrl Pts',(-0.0773217963492715,1.78560148169534,
11.2759393477898));
#40702=CARTESIAN_POINT('Ctrl Pts',(-0.111101254718751,1.79744383609631,
11.2735195361634));
#40703=CARTESIAN_POINT('Ctrl Pts',(-0.115546893373469,1.79911357955727,
11.2731991765968));
#40704=CARTESIAN_POINT('Ctrl Pts',(-0.127451296333696,1.80388753756222,
11.2723384685707));
#40705=CARTESIAN_POINT('Ctrl Pts',(-0.134833341961031,1.80717511998225,
11.271801601766));
#40706=CARTESIAN_POINT('Ctrl Pts',(-0.1470422208551,1.81317205438604,11.2709166706874));
#40707=CARTESIAN_POINT('Ctrl Pts',(-0.151936917833623,1.81573451278306,
11.2705627521864));
#40708=CARTESIAN_POINT('Ctrl Pts',(-0.157274657684916,1.81870620391343,
11.2701797304175));
#40709=CARTESIAN_POINT('Ctrl Pts',(-0.15778487669942,1.8189920813138,11.2701431487217));
#40710=CARTESIAN_POINT('Ctrl Pts',(-0.158545568256638,1.81942102429236,
11.270088657122));
#40711=CARTESIAN_POINT('Ctrl Pts',(-0.158796628013536,1.81956303782116,
11.2700706805443));
#40712=CARTESIAN_POINT('Ctrl Pts',(-0.159228129668902,1.8198078846927,11.2700397978916));
#40713=CARTESIAN_POINT('Ctrl Pts',(-0.159408662858292,1.81991055542109,
11.2700268813413));
#40714=CARTESIAN_POINT('Ctrl Pts',(-0.159778028335868,1.82012108943712,
11.2700004633603));
#40715=CARTESIAN_POINT('Ctrl Pts',(-0.159966850332798,1.82022896913444,
11.2699869631153));
#40716=CARTESIAN_POINT('Ctrl Pts',(-0.16041277516867,1.82048433846677,11.2699550917747));
#40717=CARTESIAN_POINT('Ctrl Pts',(-0.160669784799948,1.8206319922867,11.269936731338));
#40718=CARTESIAN_POINT('Ctrl Pts',(-0.161210346190913,1.82094354125368,
11.2698981318075));
#40719=CARTESIAN_POINT('Ctrl Pts',(-0.161493852808435,1.8211075146327,11.2698778977728));
#40720=CARTESIAN_POINT('Ctrl Pts',(-0.162257378338485,1.8215506739812,11.2698234305137));
#40721=CARTESIAN_POINT('Ctrl Pts',(-0.162736929102377,1.82183067044949,
11.2697892487911));
#40722=CARTESIAN_POINT('Ctrl Pts',(-0.164212992263351,1.82269762651548,
11.2696841151418));
#40723=CARTESIAN_POINT('Ctrl Pts',(-0.165207083623808,1.82328871945569,
11.2696134203523));
#40724=CARTESIAN_POINT('Ctrl Pts',(-0.1688890343888,1.82550494518646,11.2693519060697));
#40725=CARTESIAN_POINT('Ctrl Pts',(-0.171556367827907,1.82716405051337,
11.2691631080574));
#40726=CARTESIAN_POINT('Ctrl Pts',(-0.18077973775653,1.83308982525626,11.268511008555));
#40727=CARTESIAN_POINT('Ctrl Pts',(-0.187204730967481,1.83755617556832,
11.2680580651307));
#40728=CARTESIAN_POINT('Ctrl Pts',(-0.216191211510735,1.85931294985773,
11.2659899158481));
#40729=CARTESIAN_POINT('Ctrl Pts',(-0.236564245898053,1.87930483769415,
11.2644522131718));
#40730=CARTESIAN_POINT('Ctrl Pts',(-0.260074077646783,1.90942600154758,
11.2622288005819));
#40731=CARTESIAN_POINT('Ctrl Pts',(-0.265741114708693,1.91741137636493,
11.2616480809618));
#40732=CARTESIAN_POINT('Ctrl Pts',(-0.271598532797114,1.92651658605029,
11.2609897426253));
#40733=CARTESIAN_POINT('Ctrl Pts',(-0.272157136290327,1.9273942322524,11.2609263262336));
#40734=CARTESIAN_POINT('Ctrl Pts',(-0.272986333648588,1.92871105307256,
11.2608312304881));
#40735=CARTESIAN_POINT('Ctrl Pts',(-0.273260142264864,1.9291482035713,11.2607996700504));
#40736=CARTESIAN_POINT('Ctrl Pts',(-0.273729938942078,1.92990227807647,
11.2607452435183));
#40737=CARTESIAN_POINT('Ctrl Pts',(-0.273926429608413,1.93021888904562,
11.260722396001));
#40738=CARTESIAN_POINT('Ctrl Pts',(-0.274330862200261,1.93087309238842,
11.2606751955851));
#40739=CARTESIAN_POINT('Ctrl Pts',(-0.274538731037759,1.9312107290383,11.2606508400483));
#40740=CARTESIAN_POINT('Ctrl Pts',(-0.275021188533818,1.93199762289192,
11.2605940878111));
#40741=CARTESIAN_POINT('Ctrl Pts',(-0.275295299750861,1.93244717016309,
11.2605616736701));
#40742=CARTESIAN_POINT('Ctrl Pts',(-0.276165615009344,1.93388240384989,
11.2604582118271));
#40743=CARTESIAN_POINT('Ctrl Pts',(-0.276757631206685,1.9348706077713,11.26038701131));
#40744=CARTESIAN_POINT('Ctrl Pts',(-0.289584037343805,1.95654340768279,
11.2588261757985));
#40745=CARTESIAN_POINT('Ctrl Pts',(-0.299469411161466,1.97852439614754,
11.2572482081739));
#40746=CARTESIAN_POINT('Ctrl Pts',(-0.313383815465663,2.02182035364275,
11.2541829465012));
#40747=CARTESIAN_POINT('Ctrl Pts',(-0.317892374598418,2.04285112077207,
11.2527138231252));
#40748=CARTESIAN_POINT('Ctrl Pts',(-0.320430100751893,2.06553829594953,
11.2512321995997));
#40749=CARTESIAN_POINT('Ctrl Pts',(-0.320573929873987,2.06690295894055,
11.251143486109));
#40750=CARTESIAN_POINT('Ctrl Pts',(-0.321084753464039,2.0720658367076,11.2508095024859));
#40751=CARTESIAN_POINT('Ctrl Pts',(-0.321393014763523,2.0758697363302,11.2505667861608));
#40752=CARTESIAN_POINT('Ctrl Pts',(-0.321670576091457,2.08026275306692,
11.2502910292397));
#40753=CARTESIAN_POINT('Ctrl Pts',(-0.321705903848731,2.08084719651897,
11.2502544355313));
#40754=CARTESIAN_POINT('Ctrl Pts',(-0.321755905452735,2.0817135941602,11.2502003285863));
#40755=CARTESIAN_POINT('Ctrl Pts',(-0.321771801624668,2.08199547243258,
11.250182747227));
#40756=CARTESIAN_POINT('Ctrl Pts',(-0.32179894351493,2.08248828402835,11.250152048515));
#40757=CARTESIAN_POINT('Ctrl Pts',(-0.321810352264769,2.0826992075374,11.2501389219625));
#40758=CARTESIAN_POINT('Ctrl Pts',(-0.321832392049017,2.08311424190376,
11.2501131175547));
#40759=CARTESIAN_POINT('Ctrl Pts',(-0.321843036248721,2.0833183508837,11.2501004389825));
#40760=CARTESIAN_POINT('Ctrl Pts',(-0.321865672053124,2.08376049317069,
11.2500729997118));
#40761=CARTESIAN_POINT('Ctrl Pts',(-0.321877593802975,2.08399853016888,
11.2500582429597));
#40762=CARTESIAN_POINT('Ctrl Pts',(-0.321905926134909,2.08457707681381,
11.2500224146935));
#40763=CARTESIAN_POINT('Ctrl Pts',(-0.321922060554809,2.08491760062065,
11.2500013586024));
#40764=CARTESIAN_POINT('Ctrl Pts',(-0.321964557838471,2.08584567117974,
11.2499440572337));
#40765=CARTESIAN_POINT('Ctrl Pts',(-0.321989852871072,2.08643326903229,
11.2499078706804));
#40766=CARTESIAN_POINT('Ctrl Pts',(-0.322186188854554,2.09130441040243,
11.2496086350079));
#40767=CARTESIAN_POINT('Ctrl Pts',(-0.322273360650711,2.09559111682564,
11.249350095042));
#40768=CARTESIAN_POINT('Ctrl Pts',(-0.322274977094782,2.09987849461815,
11.2490951747016));
#40769=CARTESIAN_POINT('',(-0.32227491802331,2.10022986532739,10.9995935809957));
#40770=CARTESIAN_POINT('Ctrl Pts',(-0.322274976960673,2.09987813943263,
11.2490951958204));
#40771=CARTESIAN_POINT('Ctrl Pts',(-0.322285613871733,2.12800873443155,
11.2474225961834));
#40772=CARTESIAN_POINT('Ctrl Pts',(-0.318613164737115,2.15602501186304,
11.245905465835));
#40773=CARTESIAN_POINT('Ctrl Pts',(-0.308097884298559,2.19536871258844,
11.243599559658));
#40774=CARTESIAN_POINT('Ctrl Pts',(-0.304140198034284,2.20732283407027,
11.2428754933141));
#40775=CARTESIAN_POINT('Ctrl Pts',(-0.297415342162845,2.22424563838345,
11.2417949778934));
#40776=CARTESIAN_POINT('Ctrl Pts',(-0.295199879667812,2.22942136407662,
11.2414567578009));
#40777=CARTESIAN_POINT('Ctrl Pts',(-0.292467475953579,2.23536909277436,
11.2410580357785));
#40778=CARTESIAN_POINT('Ctrl Pts',(-0.292081288333471,2.23620035516626,
11.2410020785454));
#40779=CARTESIAN_POINT('Ctrl Pts',(-0.291487600522268,2.23746412066347,
11.2409166497411));
#40780=CARTESIAN_POINT('Ctrl Pts',(-0.291282669932361,2.23789783145908,
11.2408872671398));
#40781=CARTESIAN_POINT('Ctrl Pts',(-0.290925065218167,2.23865030462103,
11.240836176833));
#40782=CARTESIAN_POINT('Ctrl Pts',(-0.290772833214783,2.23896927720312,
11.240814484499));
#40783=CARTESIAN_POINT('Ctrl Pts',(-0.290454859202993,2.23963272009415,
11.2407692921755));
#40784=CARTESIAN_POINT('Ctrl Pts',(-0.290289028477201,2.23997714706095,
11.2407457891262));
#40785=CARTESIAN_POINT('Ctrl Pts',(-0.289882535188768,2.24081759611114,
11.2406883368147));
#40786=CARTESIAN_POINT('Ctrl Pts',(-0.289641212488931,2.24131329592043,
11.24065436459));
#40787=CARTESIAN_POINT('Ctrl Pts',(-0.288717148140621,2.24319910099912,
11.2405247907533));
#40788=CARTESIAN_POINT('Ctrl Pts',(-0.288025669814612,2.24458488009068,
11.240428884289));
#40789=CARTESIAN_POINT('Ctrl Pts',(-0.287063662926605,2.24647853101494,
11.2402968671713));
#40790=CARTESIAN_POINT('Ctrl Pts',(-0.286801714679353,2.24699075845509,
11.2402610597552));
#40791=CARTESIAN_POINT('Ctrl Pts',(-0.270637040716542,2.27839230563341,
11.238059927211));
#40792=CARTESIAN_POINT('Ctrl Pts',(-0.249847768579935,2.30650188632565,
11.2356952319962));
#40793=CARTESIAN_POINT('Ctrl Pts',(-0.218019421384603,2.33753606109702,
11.2327050717952));
#40794=CARTESIAN_POINT('Ctrl Pts',(-0.210748303738176,2.34401030651234,
11.2320569718964));
#40795=CARTESIAN_POINT('Ctrl Pts',(-0.200532469710946,2.3523086792004,11.2312033860424));
#40796=CARTESIAN_POINT('Ctrl Pts',(-0.197835609615366,2.35442880086486,
11.2309831051006));
#40797=CARTESIAN_POINT('Ctrl Pts',(-0.194123838752605,2.35725207755928,
11.2306872882039));
#40798=CARTESIAN_POINT('Ctrl Pts',(-0.193138086907931,2.35799297602575,
11.230609418173));
#40799=CARTESIAN_POINT('Ctrl Pts',(-0.191680793684819,2.35907525501481,
11.2304953416608));
#40800=CARTESIAN_POINT('Ctrl Pts',(-0.191212554997324,2.35942103471458,
11.2304588452868));
#40801=CARTESIAN_POINT('Ctrl Pts',(-0.190470584742774,2.35996585643628,
11.2304012647322));
#40802=CARTESIAN_POINT('Ctrl Pts',(-0.190197474824839,2.36016573705552,
11.2303801237182));
#40803=CARTESIAN_POINT('Ctrl Pts',(-0.189680464266221,2.36054287172317,
11.230340204892));
#40804=CARTESIAN_POINT('Ctrl Pts',(-0.189436629036298,2.36072021423578,
11.230321420994));
#40805=CARTESIAN_POINT('Ctrl Pts',(-0.18901509188959,2.36102589662939,11.2302890222007));
#40806=CARTESIAN_POINT('Ctrl Pts',(-0.188837507538888,2.36115439766695,
11.2302753960522));
#40807=CARTESIAN_POINT('Ctrl Pts',(-0.188493372383148,2.36140288125228,
11.2302490345981));
#40808=CARTESIAN_POINT('Ctrl Pts',(-0.188326838302245,2.36152288568124,
11.2302362977434));
#40809=CARTESIAN_POINT('Ctrl Pts',(-0.187933542788105,2.36180572387793,
11.2302062645911));
#40810=CARTESIAN_POINT('Ctrl Pts',(-0.187706683766943,2.36196842258318,
11.2301889777015));
#40811=CARTESIAN_POINT('Ctrl Pts',(-0.186919367530656,2.36253152210366,
11.2301291094583));
#40812=CARTESIAN_POINT('Ctrl Pts',(-0.186357833207874,2.36293042440687,
11.230086630991));
#40813=CARTESIAN_POINT('Ctrl Pts',(-0.179585403879764,2.36770882202297,
11.2295769141881));
#40814=CARTESIAN_POINT('Ctrl Pts',(-0.173222161193793,2.37186951886729,
11.2291242070256));
#40815=CARTESIAN_POINT('Ctrl Pts',(-0.159017811271356,2.38045579372389,
11.2281558457846));
#40816=CARTESIAN_POINT('Ctrl Pts',(-0.151126467388971,2.3847857556229,11.2276442947439));
#40817=CARTESIAN_POINT('Ctrl Pts',(-0.133822548380917,2.39335824994293,
11.2265568819979));
#40818=CARTESIAN_POINT('Ctrl Pts',(-0.124366724062661,2.39749026890407,
11.2259831164714));
#40819=CARTESIAN_POINT('Ctrl Pts',(-0.0927006455418031,2.40955360643537,
11.2240850941368));
#40820=CARTESIAN_POINT('Ctrl Pts',(-0.0698220287320776,2.41550195275426,
11.2227440935401));
#40821=CARTESIAN_POINT('Ctrl Pts',(-0.0453623845872847,2.41906857302622,
11.2212409750878));
#40822=CARTESIAN_POINT('Ctrl Pts',(-0.044222644669577,2.41922853549308,
11.2211707976746));
#40823=CARTESIAN_POINT('Ctrl Pts',(-0.0425604781814816,2.41945274821947,
11.2210682453056));
#40824=CARTESIAN_POINT('Ctrl Pts',(-0.042038703434711,2.4195218303283,11.2210360230923));
#40825=CARTESIAN_POINT('Ctrl Pts',(-0.0411236032885894,2.4196407077668,
11.2209794580633));
#40826=CARTESIAN_POINT('Ctrl Pts',(-0.0407303498345634,2.41969105619203,
11.2209551327666));
#40827=CARTESIAN_POINT('Ctrl Pts',(-0.0399672512741995,2.41978732517869,
11.2209078964919));
#40828=CARTESIAN_POINT('Ctrl Pts',(-0.039597417263531,2.41983333013243,
11.2208849882177));
#40829=CARTESIAN_POINT('Ctrl Pts',(-0.0387153032508349,2.41994150592843,
11.2208303113702));
#40830=CARTESIAN_POINT('Ctrl Pts',(-0.0382029532823698,2.42000308791809,
11.220798524267));
#40831=CARTESIAN_POINT('Ctrl Pts',(-0.0366564009198007,2.42018520890683,
11.2207024826953));
#40832=CARTESIAN_POINT('Ctrl Pts',(-0.0356217676849437,2.42030196589673,
11.2206381091554));
#40833=CARTESIAN_POINT('Ctrl Pts',(-0.0248233406750721,2.4214675865628,
11.2199649375776));
#40834=CARTESIAN_POINT('Ctrl Pts',(-0.0150179880984472,2.42207457782395,
11.2193422854927));
#40835=CARTESIAN_POINT('Ctrl Pts',(0.010961889585408,2.42249390725853,11.2176601383133));
#40836=CARTESIAN_POINT('Ctrl Pts',(0.0271197255087503,2.42153832634082,
11.216579705673));
#40837=CARTESIAN_POINT('Ctrl Pts',(0.0585276572852727,2.41729625747436,
11.214438504025));
#40838=CARTESIAN_POINT('Ctrl Pts',(0.0737493797053583,2.41410740569524,
11.2133816388565));
#40839=CARTESIAN_POINT('Ctrl Pts',(0.0946027756135815,2.40813863009649,
11.2119469449604));
#40840=CARTESIAN_POINT('Ctrl Pts',(0.100473973942773,2.40627453598039,11.2115446908144));
#40841=CARTESIAN_POINT('Ctrl Pts',(0.108216262023889,2.4035697383151,11.2110196280893));
#40842=CARTESIAN_POINT('Ctrl Pts',(0.110137620995487,2.40287794623495,11.2108897771829));
#40843=CARTESIAN_POINT('Ctrl Pts',(0.112843366527661,2.40187457998704,11.2107076830228));
#40844=CARTESIAN_POINT('Ctrl Pts',(0.113633258633955,2.40157813246455,11.2106546171051));
#40845=CARTESIAN_POINT('Ctrl Pts',(0.114834374047575,2.40112196325454,11.2105740765876));
#40846=CARTESIAN_POINT('Ctrl Pts',(0.115246441315336,2.40096449622298,11.2105464728183));
#40847=CARTESIAN_POINT('Ctrl Pts',(0.116006850408579,2.40067212345244,11.2104955863505));
#40848=CARTESIAN_POINT('Ctrl Pts',(0.116355282739889,2.40053745747411,11.210472289592));
#40849=CARTESIAN_POINT('Ctrl Pts',(0.116922409217856,2.40031713406066,11.2104344045713));
#40850=CARTESIAN_POINT('Ctrl Pts',(0.11714124400075,2.40023184331866,11.2104197942876));
#40851=CARTESIAN_POINT('Ctrl Pts',(0.117560109263007,2.40006806312464,11.2103918452568));
#40852=CARTESIAN_POINT('Ctrl Pts',(0.117760153850822,2.39998961309109,11.2103785042327));
#40853=CARTESIAN_POINT('Ctrl Pts',(0.118224723989199,2.39980688969554,11.2103475381091));
#40854=CARTESIAN_POINT('Ctrl Pts',(0.118489190888015,2.39970246598156,11.2103299221318));
#40855=CARTESIAN_POINT('Ctrl Pts',(0.119322112804953,2.39937231520747,11.2102744790684));
#40856=CARTESIAN_POINT('Ctrl Pts',(0.119890067899432,2.39914531811557,11.2102367282776));
#40857=CARTESIAN_POINT('Ctrl Pts',(0.124574211061576,2.3972577032683,11.2099258094942));
#40858=CARTESIAN_POINT('Ctrl Pts',(0.128656583540053,2.3955137298424,11.2096575566237));
#40859=CARTESIAN_POINT('Ctrl Pts',(0.133385808904091,2.39337683086763,11.209348540669));
#40860=CARTESIAN_POINT('Ctrl Pts',(0.134068675389736,2.39306540090211,11.209303963966));
#40861=CARTESIAN_POINT('Ctrl Pts',(0.147305370410249,2.38697269040325,11.2084406076175));
#40862=CARTESIAN_POINT('Ctrl Pts',(0.159476800673317,2.38039154855982,11.2076589334872));
#40863=CARTESIAN_POINT('Ctrl Pts',(0.183658203039899,2.36523091259455,11.206058624942));
#40864=CARTESIAN_POINT('Ctrl Pts',(0.195577010718693,2.35656850234787,11.2052424318784));
#40865=CARTESIAN_POINT('Ctrl Pts',(0.219781571794237,2.33630723684455,11.2034504378983));
#40866=CARTESIAN_POINT('Ctrl Pts',(0.231831313928422,2.32449758894549,11.2024708155577));
#40867=CARTESIAN_POINT('Ctrl Pts',(0.243672787482944,2.31091733967566,11.2013753224514));
#40868=CARTESIAN_POINT('Ctrl Pts',(0.244438845653017,2.31002905088213,11.2013038063654));
#40869=CARTESIAN_POINT('Ctrl Pts',(0.245544253451992,2.30873302707068,11.2011996581206));
#40870=CARTESIAN_POINT('Ctrl Pts',(0.245887478845685,2.30832859797681,11.2011671855499));
#40871=CARTESIAN_POINT('Ctrl Pts',(0.2464859151481,2.30761990984583,11.2011103300268));
#40872=CARTESIAN_POINT('Ctrl Pts',(0.246741565746916,2.30731602220104,11.2010859651509));
#40873=CARTESIAN_POINT('Ctrl Pts',(0.247235302823283,2.3067269181715,11.2010387609057));
#40874=CARTESIAN_POINT('Ctrl Pts',(0.247473459189251,2.30644176092525,11.2010159244417));
#40875=CARTESIAN_POINT('Ctrl Pts',(0.248038414911546,2.30576292701271,11.2009615910351));
#40876=CARTESIAN_POINT('Ctrl Pts',(0.248364770165664,2.30536888357394,11.2009300760952));
#40877=CARTESIAN_POINT('Ctrl Pts',(0.249516236996881,2.30397183611664,11.2008184260229));
#40878=CARTESIAN_POINT('Ctrl Pts',(0.250336213842704,2.30296463340585,11.2007380834278));
#40879=CARTESIAN_POINT('Ctrl Pts',(0.264110365233951,2.28583496744804,11.1993741383148));
#40880=CARTESIAN_POINT('Ctrl Pts',(0.275486518072593,2.26851054009212,11.1980264471711));
#40881=CARTESIAN_POINT('Ctrl Pts',(0.298206251272945,2.22538733023949,11.1947590847124));
#40882=CARTESIAN_POINT('Ctrl Pts',(0.307989310832357,2.19895275257214,11.1928164904636));
#40883=CARTESIAN_POINT('Ctrl Pts',(0.31450507181521,2.17035150983895,11.1909550176108));
#40884=CARTESIAN_POINT('Ctrl Pts',(0.314778738451621,2.1691167206544,11.1908751275911));
#40885=CARTESIAN_POINT('Ctrl Pts',(0.315170035809796,2.16730063740992,11.190758356452));
#40886=CARTESIAN_POINT('Ctrl Pts',(0.31529333847217,2.16672059649205,11.1907211696297));
#40887=CARTESIAN_POINT('Ctrl Pts',(0.315485408764238,2.16580463544437,11.1906626220033));
#40888=CARTESIAN_POINT('Ctrl Pts',(0.315555241745524,2.16546894377188,11.1906412019184));
#40889=CARTESIAN_POINT('Ctrl Pts',(0.315686078668222,2.16483492944696,11.1906008170881));
#40890=CARTESIAN_POINT('Ctrl Pts',(0.315747195736611,2.16453663089756,11.1905818459469));
#40891=CARTESIAN_POINT('Ctrl Pts',(0.315851708661636,2.16402282472951,11.1905492204608));
#40892=CARTESIAN_POINT('Ctrl Pts',(0.315895306875682,2.16380735886874,11.1905355544618));
#40893=CARTESIAN_POINT('Ctrl Pts',(0.315979044848403,2.16339132967506,11.1905091979407));
#40894=CARTESIAN_POINT('Ctrl Pts',(0.316019214090229,2.16319077296282,11.1904965057144));
#40895=CARTESIAN_POINT('Ctrl Pts',(0.316113197175031,2.1627192039169,11.1904666940577));
#40896=CARTESIAN_POINT('Ctrl Pts',(0.316166853583983,2.16244815981532,11.1904495836958));
#40897=CARTESIAN_POINT('Ctrl Pts',(0.316323760870393,2.16165016038049,11.1903992791347));
#40898=CARTESIAN_POINT('Ctrl Pts',(0.316426044030888,2.16112301231846,11.1903661399613));
#40899=CARTESIAN_POINT('Ctrl Pts',(0.317291007385889,2.15660479260114,11.1900828652619));
#40900=CARTESIAN_POINT('Ctrl Pts',(0.317979504687194,2.15259966007758,11.1898368576505));
#40901=CARTESIAN_POINT('Ctrl Pts',(0.321896462525297,2.12691313595252,11.1882854398066));
#40902=CARTESIAN_POINT('Ctrl Pts',(0.322981878540907,2.10496044507895,11.1870762052888));
#40903=CARTESIAN_POINT('Ctrl Pts',(0.321076436946661,2.06874910247598,11.1850472913117));
#40904=CARTESIAN_POINT('Ctrl Pts',(0.319368744020788,2.05449989656714,11.1842405294662));
#40905=CARTESIAN_POINT('Ctrl Pts',(0.315142780545402,2.03203812379401,11.1829133508353));
#40906=CARTESIAN_POINT('Ctrl Pts',(0.313235813604235,2.02373011712177,11.1824102444439));
#40907=CARTESIAN_POINT('Ctrl Pts',(0.310565814597484,2.0139022717199,11.181796198236));
#40908=CARTESIAN_POINT('Ctrl Pts',(0.310117175908395,2.01230005097512,11.1816954866114));
#40909=CARTESIAN_POINT('Ctrl Pts',(0.309312491112667,2.00950968698331,11.1815190010501));
#40910=CARTESIAN_POINT('Ctrl Pts',(0.308961952652534,2.00831998225319,11.181443406533));
#40911=CARTESIAN_POINT('Ctrl Pts',(0.308448177452069,2.00661267773816,11.1813344126332));
#40912=CARTESIAN_POINT('Ctrl Pts',(0.30829048404227,2.00609341036949,11.1813011945935));
#40913=CARTESIAN_POINT('Ctrl Pts',(0.308014519554895,2.00519287621554,11.181243467265));
#40914=CARTESIAN_POINT('Ctrl Pts',(0.307896849927373,2.00481142516353,11.1812189777286));
#40915=CARTESIAN_POINT('Ctrl Pts',(0.307669215582214,2.00407833848334,11.1811718408395));
#40916=CARTESIAN_POINT('Ctrl Pts',(0.307559355927551,2.00372667064669,11.1811491969664));
#40917=CARTESIAN_POINT('Ctrl Pts',(0.307299091623264,2.00289853991067,11.1810957980815));
#40918=CARTESIAN_POINT('Ctrl Pts',(0.307148181830025,2.0024222378921,11.1810650265071));
#40919=CARTESIAN_POINT('Ctrl Pts',(0.306699044088186,2.0010160334167,11.180974002785));
#40920=CARTESIAN_POINT('Ctrl Pts',(0.306397698388591,2.00008713959804,11.1809136481302));
#40921=CARTESIAN_POINT('Ctrl Pts',(0.303679116966014,1.99183512242224,11.1803754276997));
#40922=CARTESIAN_POINT('Ctrl Pts',(0.301004157866724,1.98460014184695,11.1798890747005));
#40923=CARTESIAN_POINT('Ctrl Pts',(0.296756684033871,1.97426765330199,11.1791724056787));
#40924=CARTESIAN_POINT('Ctrl Pts',(0.2953894403431,1.97108828732678,11.1789487811933));
#40925=CARTESIAN_POINT('Ctrl Pts',(0.282900253255653,1.94328857258051,11.1769661304825));
#40926=CARTESIAN_POINT('Ctrl Pts',(0.268774979054459,1.92013708425124,11.1751115548118));
#40927=CARTESIAN_POINT('Ctrl Pts',(0.247787912721925,1.89382900540209,11.1728595445137));
#40928=CARTESIAN_POINT('Ctrl Pts',(0.243484203653094,1.88876368386816,11.1724189725811));
#40929=CARTESIAN_POINT('Ctrl Pts',(0.235436107571636,1.87986442529763,11.1716370361573));
#40930=CARTESIAN_POINT('Ctrl Pts',(0.231746855031262,1.87598385035512,11.1712931624396));
#40931=CARTESIAN_POINT('Ctrl Pts',(0.227487563396585,1.87172158370865,11.1709139301591));
#40932=CARTESIAN_POINT('Ctrl Pts',(0.227011255874286,1.87124791461094,11.1708717639116));
#40933=CARTESIAN_POINT('Ctrl Pts',(0.226267118919601,1.87051251287593,11.1708062690723));
#40934=CARTESIAN_POINT('Ctrl Pts',(0.226000311769296,1.87024975531191,11.1707828620879));
#40935=CARTESIAN_POINT('Ctrl Pts',(0.225553056226599,1.86981082117102,11.1707437521506));
#40936=CARTESIAN_POINT('Ctrl Pts',(0.22537285879264,1.86963439114361,11.1707280294873));
#40937=CARTESIAN_POINT('Ctrl Pts',(0.225020911832249,1.86929061057975,11.1706973889708));
#40938=CARTESIAN_POINT('Ctrl Pts',(0.224849182308022,1.86912323992053,11.1706824695363));
#40939=CARTESIAN_POINT('Ctrl Pts',(0.224524020966735,1.86880703876358,11.1706542798342));
#40940=CARTESIAN_POINT('Ctrl Pts',(0.224370629137461,1.86865817045535,11.1706410066135));
#40941=CARTESIAN_POINT('Ctrl Pts',(0.224016326330692,1.8683149998818,11.1706104057283));
#40942=CARTESIAN_POINT('Ctrl Pts',(0.223815310910442,1.86812080656957,11.1705930866693));
#40943=CARTESIAN_POINT('Ctrl Pts',(0.223202671170461,1.86753049759624,11.1705404311935));
#40944=CARTESIAN_POINT('Ctrl Pts',(0.22279024321544,1.86713521196774,11.1705051594211));
#40945=CARTESIAN_POINT('Ctrl Pts',(0.219833462812496,1.86431637404737,11.1702535236381));
#40946=CARTESIAN_POINT('Ctrl Pts',(0.217250551001605,1.86193336340606,11.1700402219281));
#40947=CARTESIAN_POINT('Ctrl Pts',(0.196989426977284,1.8438447673167,11.1684118011165));
#40948=CARTESIAN_POINT('Ctrl Pts',(0.177667599327041,1.83008357075567,11.1671135651346));
#40949=CARTESIAN_POINT('Ctrl Pts',(0.145559128197653,1.81217072971679,11.1650540867161));
#40950=CARTESIAN_POINT('Ctrl Pts',(0.133728251883271,1.8064870230169,11.1643141049457));
#40951=CARTESIAN_POINT('Ctrl Pts',(0.113642965582844,1.79830480511951,11.1630551781468));
#40952=CARTESIAN_POINT('Ctrl Pts',(0.105575822666422,1.79538804882416,11.1625490226636));
#40953=CARTESIAN_POINT('Ctrl Pts',(0.0949687400073146,1.79202494829385,
11.1618781984801));
#40954=CARTESIAN_POINT('Ctrl Pts',(0.0925259912391918,1.791282273883,11.1617233649469));
#40955=CARTESIAN_POINT('Ctrl Pts',(0.0893853738948245,1.79036804745345,
11.1615237699575));
#40956=CARTESIAN_POINT('Ctrl Pts',(0.0886953543514017,1.79016968320151,
11.1614798849497));
#40957=CARTESIAN_POINT('Ctrl Pts',(0.0875850338067536,1.78985450547714,
11.1614092149451));
#40958=CARTESIAN_POINT('Ctrl Pts',(0.0871651457482567,1.78973623594837,
11.1613824774016));
#40959=CARTESIAN_POINT('Ctrl Pts',(0.0863666376024173,1.78951306969385,
11.1613316061232));
#40960=CARTESIAN_POINT('Ctrl Pts',(0.085988062998148,1.78940801201361,11.1613074776737));
#40961=CARTESIAN_POINT('Ctrl Pts',(0.0851268238044925,1.78917070609547,
11.1612525628597));
#40962=CARTESIAN_POINT('Ctrl Pts',(0.0846440422280816,1.78903888958421,
11.1612217625379));
#40963=CARTESIAN_POINT('Ctrl Pts',(0.0832110993756456,1.78865122959978,
11.1611302928646));
#40964=CARTESIAN_POINT('Ctrl Pts',(0.0822600776489263,1.78839861444494,
11.1610695190216));
#40965=CARTESIAN_POINT('Ctrl Pts',(0.0757240228596573,1.78669448217,11.1606513642812));
#40966=CARTESIAN_POINT('Ctrl Pts',(0.0701023438682621,1.78538892331602,
11.1602892954836));
#40967=CARTESIAN_POINT('Ctrl Pts',(0.0633030533443531,1.78400116014501,
11.1598481107241));
#40968=CARTESIAN_POINT('Ctrl Pts',(0.0621559262149118,1.78377352398619,
11.1597735672833));
#40969=CARTESIAN_POINT('Ctrl Pts',(0.0305142368402735,1.77767336127625,
11.1577143530949));
#40970=CARTESIAN_POINT('Ctrl Pts',(-0.000665465190473068,1.77623402889956,
11.1555837734216));
#40971=CARTESIAN_POINT('Ctrl Pts',(-0.0431443463476149,1.7804139342069,
11.1527247989634));
#40972=CARTESIAN_POINT('Ctrl Pts',(-0.0546605162650784,1.78218090287316,
11.1519570922089));
#40973=CARTESIAN_POINT('Ctrl Pts',(-0.0670786734378294,1.78478147759472,
11.1511542696831));
#40974=CARTESIAN_POINT('Ctrl Pts',(-0.0680993544880657,1.78500040748456,
11.1510884720872));
#40975=CARTESIAN_POINT('Ctrl Pts',(-0.0698557039191077,1.78538606959842,
11.1509755963115));
#40976=CARTESIAN_POINT('Ctrl Pts',(-0.0705918766489096,1.78555043083012,
11.1509283895594));
#40977=CARTESIAN_POINT('Ctrl Pts',(-0.0716328708023237,1.78578668787489,
11.1508617916843));
#40978=CARTESIAN_POINT('Ctrl Pts',(-0.0719381676920451,1.78585644407832,
11.15084227918));
#40979=CARTESIAN_POINT('Ctrl Pts',(-0.0724617971480981,1.78597688967753,
11.1508088454324));
#40980=CARTESIAN_POINT('Ctrl Pts',(-0.0726801789829622,1.78602736194589,
11.150794911635));
#40981=CARTESIAN_POINT('Ctrl Pts',(-0.0730979400746548,1.78612437383693,
11.1507682756381));
#40982=CARTESIAN_POINT('Ctrl Pts',(-0.0732973273698071,1.78617087556532,
11.1507555712502));
#40983=CARTESIAN_POINT('Ctrl Pts',(-0.0737664575355801,1.78628075904453,
11.1507256989386));
#40984=CARTESIAN_POINT('Ctrl Pts',(-0.0740361637636604,1.78634429885698,
11.150708540177));
#40985=CARTESIAN_POINT('Ctrl Pts',(-0.0748312611590856,1.78653269771403,
11.1506579993924));
#40986=CARTESIAN_POINT('Ctrl Pts',(-0.0753564241334326,1.78665853035246,
11.1506246731293));
#40987=CARTESIAN_POINT('Ctrl Pts',(-0.0799049534559692,1.78776048571096,
11.1503364944292));
#40988=CARTESIAN_POINT('Ctrl Pts',(-0.0839097086400566,1.7888127885025,
11.1500859287721));
#40989=CARTESIAN_POINT('Ctrl Pts',(-0.0882443117006682,1.79004153473639,
11.1498170730391));
#40990=CARTESIAN_POINT('Ctrl Pts',(-0.0885951571941766,1.79014163419365,
11.1497953285321));
#40991=CARTESIAN_POINT('Ctrl Pts',(-0.089197947030021,1.79031472319032,
11.1497579969354));
#40992=CARTESIAN_POINT('Ctrl Pts',(-0.0894499728793633,1.79038742470663,
11.1497423969871));
#40993=CARTESIAN_POINT('Ctrl Pts',(-0.117807831053197,1.7986052887049,11.1479880083282));
#40994=CARTESIAN_POINT('Ctrl Pts',(-0.144676856635989,1.81054096151597,
11.1464158822174));
#40995=CARTESIAN_POINT('Ctrl Pts',(-0.182302251693312,1.83382091072605,
11.143902255676));
#40996=CARTESIAN_POINT('Ctrl Pts',(-0.194470363975291,1.84257698301877,
11.1430331014031));
#40997=CARTESIAN_POINT('Ctrl Pts',(-0.20720562916949,1.85316093801789,11.1420339906839));
#40998=CARTESIAN_POINT('Ctrl Pts',(-0.208418884574288,1.85418449256799,
11.1419378612906));
#40999=CARTESIAN_POINT('Ctrl Pts',(-0.210531607811743,1.85599376239595,
11.1417687670302));
#41000=CARTESIAN_POINT('Ctrl Pts',(-0.211434368456021,1.8567755981547,11.1416959616922));
#41001=CARTESIAN_POINT('Ctrl Pts',(-0.212734734273322,1.85791449031987,
11.1415902790221));
#41002=CARTESIAN_POINT('Ctrl Pts',(-0.213135837161863,1.85826755270484,
11.1415575680086));
#41003=CARTESIAN_POINT('Ctrl Pts',(-0.213833978093957,1.85888516500358,
11.1415004346921));
#41004=CARTESIAN_POINT('Ctrl Pts',(-0.214131408721481,1.85914927104221,
11.1414760309989));
#41005=CARTESIAN_POINT('Ctrl Pts',(-0.214704923779828,1.85966043066521,
11.1414288526659));
#41006=CARTESIAN_POINT('Ctrl Pts',(-0.214981072798249,1.85990741115131,
11.1414060811192));
#41007=CARTESIAN_POINT('Ctrl Pts',(-0.215634589475266,1.86049393088982,
11.1413520603655));
#41008=CARTESIAN_POINT('Ctrl Pts',(-0.216011581135442,1.8608338859089,11.1413207936436));
#41009=CARTESIAN_POINT('Ctrl Pts',(-0.217332760792655,1.86203094145216,
11.1412108510957));
#41010=CARTESIAN_POINT('Ctrl Pts',(-0.218272654015633,1.86289274542222,
11.1411319760462));
#41011=CARTESIAN_POINT('Ctrl Pts',(-0.231831284114687,1.87547382062437,
11.1399844216267));
#41012=CARTESIAN_POINT('Ctrl Pts',(-0.243493797013867,1.88817850576825,
11.1388720569459));
#41013=CARTESIAN_POINT('Ctrl Pts',(-0.266656452250681,1.91786489637708,
11.1363697114697));
#41014=CARTESIAN_POINT('Ctrl Pts',(-0.27766703046908,1.93513702317913,11.1349713234374));
#41015=CARTESIAN_POINT('Ctrl Pts',(-0.290871241177242,1.96097234106822,
11.1330287542691));
#41016=CARTESIAN_POINT('Ctrl Pts',(-0.294469114255374,1.96876459170062,
11.1324610320473));
#41017=CARTESIAN_POINT('Ctrl Pts',(-0.299380234701648,1.98062345002478,
11.131632784031));
#41018=CARTESIAN_POINT('Ctrl Pts',(-0.30093056188646,1.98458731913911,11.1313617357899));
#41019=CARTESIAN_POINT('Ctrl Pts',(-0.302592309191356,1.98909746158374,
11.1310607566978));
#41020=CARTESIAN_POINT('Ctrl Pts',(-0.302781288963815,1.98961444989041,
11.1310263652634));
#41021=CARTESIAN_POINT('Ctrl Pts',(-0.303062795549528,1.99039072409714,
11.1309748918061));
#41022=CARTESIAN_POINT('Ctrl Pts',(-0.30315631496482,1.99064964513751,11.1309577508931));
#41023=CARTESIAN_POINT('Ctrl Pts',(-0.303316468447645,1.99109483607576,
11.1309283266668));
#41024=CARTESIAN_POINT('Ctrl Pts',(-0.303383262730744,1.99128104739011,
11.1309160337373));
#41025=CARTESIAN_POINT('Ctrl Pts',(-0.303521293162504,1.99166697096075,
11.1308905865732));
#41026=CARTESIAN_POINT('Ctrl Pts',(-0.303592503478052,1.99186669145726,
11.1308774339137));
#41027=CARTESIAN_POINT('Ctrl Pts',(-0.303786591998069,1.99241274614059,
11.1308415182288));
#41028=CARTESIAN_POINT('Ctrl Pts',(-0.303909075496294,1.99275922181843,
11.1308187788229));
#41029=CARTESIAN_POINT('Ctrl Pts',(-0.304372682610936,1.99407782527937,
11.1307324229937));
#41030=CARTESIAN_POINT('Ctrl Pts',(-0.304709741401117,1.99505139076526,
11.1306690456774));
#41031=CARTESIAN_POINT('Ctrl Pts',(-0.310970101904116,2.0134183306045,11.1294802755612));
#41032=CARTESIAN_POINT('Ctrl Pts',(-0.315400836322276,2.03128815683696,
11.1284388282697));
#41033=CARTESIAN_POINT('Ctrl Pts',(-0.320928806882402,2.06608821077844,
11.1264630025729));
#41034=CARTESIAN_POINT('Ctrl Pts',(-0.32226302998602,2.08291697756033,11.1255295197136));
#41035=CARTESIAN_POINT('Ctrl Pts',(-0.322279117997924,2.10572423217828,
11.1242264343365));
#41036=CARTESIAN_POINT('Ctrl Pts',(-0.322118451696256,2.11167452734151,
11.1238831533318));
#41037=CARTESIAN_POINT('Ctrl Pts',(-0.321647698777409,2.12027344737234,
11.1233800252546));
#41038=CARTESIAN_POINT('Ctrl Pts',(-0.32146936504506,2.12292818301118,11.1232237255624));
#41039=CARTESIAN_POINT('Ctrl Pts',(-0.32075409603904,2.1319110928246,11.1226911743545));
#41040=CARTESIAN_POINT('Ctrl Pts',(-0.320063017265102,2.1382251811988,11.1223106207509));
#41041=CARTESIAN_POINT('Ctrl Pts',(-0.319044223611113,2.14553033222982,
11.1218616849225));
#41042=CARTESIAN_POINT('Ctrl Pts',(-0.318897694264697,2.14654555109881,
11.121799100939));
#41043=CARTESIAN_POINT('Ctrl Pts',(-0.318672223507138,2.14805665093449,
11.1217056530564));
#41044=CARTESIAN_POINT('Ctrl Pts',(-0.31859696480177,2.14855308176226,11.1216749058185));
#41045=CARTESIAN_POINT('Ctrl Pts',(-0.318460721454884,2.149437829895,11.1216200221086));
#41046=CARTESIAN_POINT('Ctrl Pts',(-0.318400185796314,2.1498262161617,11.1215958999131));
#41047=CARTESIAN_POINT('Ctrl Pts',(-0.318271112559775,2.15064448670135,
11.1215450158031));
#41048=CARTESIAN_POINT('Ctrl Pts',(-0.318202414281175,2.15107434449849,
11.121518248835));
#41049=CARTESIAN_POINT('Ctrl Pts',(-0.318018756444221,2.15220877137954,
11.1214475123212));
#41050=CARTESIAN_POINT('Ctrl Pts',(-0.317902326837207,2.15291309703346,
11.1214034961857));
#41051=CARTESIAN_POINT('Ctrl Pts',(-0.317365517759242,2.15609471886882,
11.1212042144911));
#41052=CARTESIAN_POINT('Ctrl Pts',(-0.316918523890522,2.15856737989268,
11.1210481052854));
#41053=CARTESIAN_POINT('Ctrl Pts',(-0.314833793246507,2.16937598269823,
11.1203601355605));
#41054=CARTESIAN_POINT('Ctrl Pts',(-0.312895858390997,2.17764988373085,
11.1198187847556));
#41055=CARTESIAN_POINT('Ctrl Pts',(-0.306831272443274,2.19959687304708,
11.118342079836));
#41056=CARTESIAN_POINT('Ctrl Pts',(-0.302119352988017,2.21308752254531,
11.1173902852623));
#41057=CARTESIAN_POINT('Ctrl Pts',(-0.286749788100479,2.24919526734346,
11.1147432845072));
#41058=CARTESIAN_POINT('Ctrl Pts',(-0.274332596453154,2.27095759539256,
11.113029537657));
#41059=CARTESIAN_POINT('Ctrl Pts',(-0.258680684119955,2.29221735861426,
11.1113609142009));
#41060=CARTESIAN_POINT('Ctrl Pts',(-0.257827572545595,2.29336016214196,
11.1112712594194));
#41061=CARTESIAN_POINT('Ctrl Pts',(-0.256714457306904,2.29483079319912,
11.1111559798661));
#41062=CARTESIAN_POINT('Ctrl Pts',(-0.256461379224928,2.29516380694108,
11.1111298819214));
#41063=CARTESIAN_POINT('Ctrl Pts',(-0.256072829916008,2.29567302011369,
11.1110899862565));
#41064=CARTESIAN_POINT('Ctrl Pts',(-0.255937824764592,2.29584957206252,
11.1110761558261));
#41065=CARTESIAN_POINT('Ctrl Pts',(-0.255671380674219,2.29619726627702,
11.1110489229284));
#41066=CARTESIAN_POINT('Ctrl Pts',(-0.25553995325328,2.2963684151851,11.1110355198537));
#41067=CARTESIAN_POINT('Ctrl Pts',(-0.25524660623941,2.29674962762791,11.1110056706771));
#41068=CARTESIAN_POINT('Ctrl Pts',(-0.255084599612639,2.2969596227914,11.1109892309105));
#41069=CARTESIAN_POINT('Ctrl Pts',(-0.254615165849222,2.29756655844655,
11.1109417239758));
#41070=CARTESIAN_POINT('Ctrl Pts',(-0.254307068377375,2.2979629831009,11.1109107042241));
#41071=CARTESIAN_POINT('Ctrl Pts',(-0.252197798673163,2.30066390020984,
11.1106994150509));
#41072=CARTESIAN_POINT('Ctrl Pts',(-0.250366178895085,2.3029445944537,11.1105212699617));
#41073=CARTESIAN_POINT('Ctrl Pts',(-0.244520805746983,2.31002352155858,
11.1099680631264));
#41074=CARTESIAN_POINT('Ctrl Pts',(-0.240398061280094,2.31473026535673,
11.1095998306152));
#41075=CARTESIAN_POINT('Ctrl Pts',(-0.225764312132883,2.33048675150322,
11.1083537559461));
#41076=CARTESIAN_POINT('Ctrl Pts',(-0.214607462332204,2.3409094563838,11.1075050890333));
#41077=CARTESIAN_POINT('Ctrl Pts',(-0.182738411805528,2.36670379927038,
11.1052131722153));
#41078=CARTESIAN_POINT('Ctrl Pts',(-0.160857040059098,2.38044428517751,
11.1037637547439));
#41079=CARTESIAN_POINT('Ctrl Pts',(-0.136162617065269,2.39210162444621,
11.1021081069975));
#41080=CARTESIAN_POINT('Ctrl Pts',(-0.134744754261485,2.39275837879598,
11.1020130196591));
#41081=CARTESIAN_POINT('Ctrl Pts',(-0.132818375103367,2.39363371928278,
11.1018837746176));
#41082=CARTESIAN_POINT('Ctrl Pts',(-0.132313973312393,2.39386135221428,
11.101849928158));
#41083=CARTESIAN_POINT('Ctrl Pts',(-0.131459630790511,2.39424426530894,
11.1017925904391));
#41084=CARTESIAN_POINT('Ctrl Pts',(-0.131109993854174,2.39440022368247,
11.1017691224852));
#41085=CARTESIAN_POINT('Ctrl Pts',(-0.130437166088818,2.39469890761734,
11.1017239561701));
#41086=CARTESIAN_POINT('Ctrl Pts',(-0.130114016632863,2.39484172554479,
11.1017022610099));
#41087=CARTESIAN_POINT('Ctrl Pts',(-0.129352654250365,2.39517671897671,
11.1016511396702));
#41088=CARTESIAN_POINT('Ctrl Pts',(-0.128914247759272,2.39536845008942,
11.1016216983517));
#41089=CARTESIAN_POINT('Ctrl Pts',(-0.127639979228913,2.39592235665005,
11.101536109849));
#41090=CARTESIAN_POINT('Ctrl Pts',(-0.126803011665821,2.39628196311635,
11.1014798751963));
#41091=CARTESIAN_POINT('Ctrl Pts',(-0.120904922981518,2.39878653090654,
11.1010834480923));
#41092=CARTESIAN_POINT('Ctrl Pts',(-0.115791439402396,2.40080513293414,
11.100738994105));
#41093=CARTESIAN_POINT('Ctrl Pts',(-0.0994712558807518,2.40676990086376,
11.0996363197452));
#41094=CARTESIAN_POINT('Ctrl Pts',(-0.0880977061581307,2.41022740422566,
11.0988625954484));
#41095=CARTESIAN_POINT('Ctrl Pts',(-0.0449963585995469,2.42076841611452,
11.095917465657));
#41096=CARTESIAN_POINT('Ctrl Pts',(-0.0124488653819679,2.42366955683189,
11.0936472027799));
#41097=CARTESIAN_POINT('Ctrl Pts',(0.0214561711553594,2.42156335563747,
11.0914990887251));
#41098=CARTESIAN_POINT('Ctrl Pts',(0.0229303290677825,2.4214615982928,11.0914061658428));
#41099=CARTESIAN_POINT('Ctrl Pts',(0.0248265762976301,2.42131759449503,
11.0912872934295));
#41100=CARTESIAN_POINT('Ctrl Pts',(0.0252493235984321,2.4212846511825,11.0912608341821));
#41101=CARTESIAN_POINT('Ctrl Pts',(0.0259194047849398,2.42123110322143,
11.091218962582));
#41102=CARTESIAN_POINT('Ctrl Pts',(0.026166780128673,2.42121104719477,11.0912035194437));
#41103=CARTESIAN_POINT('Ctrl Pts',(0.0266102105352606,2.42117458029343,
11.0911758636298));
#41104=CARTESIAN_POINT('Ctrl Pts',(0.0268062723042598,2.42115827577202,
11.0911636450406));
#41105=CARTESIAN_POINT('Ctrl Pts',(0.0272674612588645,2.42111949797235,
11.0911349256308));
#41106=CARTESIAN_POINT('Ctrl Pts',(0.0275325752427082,2.42109687591636,
11.0911184333299));
#41107=CARTESIAN_POINT('Ctrl Pts',(0.0283018649697433,2.4210302730123,11.0910706257092));
#41108=CARTESIAN_POINT('Ctrl Pts',(0.0288059684242431,2.42098543260172,
11.0910393587396));
#41109=CARTESIAN_POINT('Ctrl Pts',(0.0323107292670041,2.42066535838381,
11.0908223848903));
#41110=CARTESIAN_POINT('Ctrl Pts',(0.0353076301967922,2.42034922837953,
11.0906389351467));
#41111=CARTESIAN_POINT('Ctrl Pts',(0.0446266766786995,2.41923383023239,
11.0900737592643));
#41112=CARTESIAN_POINT('Ctrl Pts',(0.0509301623547187,2.41828903274906,
11.0896990414985));
#41113=CARTESIAN_POINT('Ctrl Pts',(0.0727402495397434,2.41435541333712,
11.0884162132588));
#41114=CARTESIAN_POINT('Ctrl Pts',(0.0880526634141122,2.41041466362918,
11.087539050788));
#41115=CARTESIAN_POINT('Ctrl Pts',(0.126801261285647,2.39734285721421,11.0852523562657));
#41116=CARTESIAN_POINT('Ctrl Pts',(0.149564247831897,2.38656869013924,11.0838353556271));
#41117=CARTESIAN_POINT('Ctrl Pts',(0.172103804205766,2.37247689678683,11.0822228713464));
#41118=CARTESIAN_POINT('Ctrl Pts',(0.173356886600899,2.3716813730417,11.082132519326));
#41119=CARTESIAN_POINT('Ctrl Pts',(0.175059611923363,2.37058381547612,11.0820087616163));
#41120=CARTESIAN_POINT('Ctrl Pts',(0.175514068538771,2.37028925369628,11.0819756342714));
#41121=CARTESIAN_POINT('Ctrl Pts',(0.176285778108725,2.36978629346281,11.0819192156953));
#41122=CARTESIAN_POINT('Ctrl Pts',(0.176603410390046,2.36957847677515,11.0818959462469));
#41123=CARTESIAN_POINT('Ctrl Pts',(0.177243009337119,2.36915839200497,11.0818489929649));
#41124=CARTESIAN_POINT('Ctrl Pts',(0.177564963603618,2.3689461062072,11.0818253084913));
#41125=CARTESIAN_POINT('Ctrl Pts',(0.178295694490519,2.36846240280061,11.0817714391224));
#41126=CARTESIAN_POINT('Ctrl Pts',(0.178704233102021,2.36819062895356,11.0817412408593));
#41127=CARTESIAN_POINT('Ctrl Pts',(0.179557545754608,2.36762016073199,11.081677995748));
#41128=CARTESIAN_POINT('Ctrl Pts',(0.1800021984696,2.36732128835576,11.0816449422332));
#41129=CARTESIAN_POINT('Ctrl Pts',(0.181165921206137,2.36653487460004,11.0815581800709));
#41130=CARTESIAN_POINT('Ctrl Pts',(0.181883765084588,2.36604553437236,11.0815044033373));
#41131=CARTESIAN_POINT('Ctrl Pts',(0.18401015692187,2.36458338597921,11.0813443345965));
#41132=CARTESIAN_POINT('Ctrl Pts',(0.185412925159595,2.36360226286643,11.0812377265307));
#41133=CARTESIAN_POINT('Ctrl Pts',(0.200764104832932,2.35268219260395,11.0800597461879));
#41134=CARTESIAN_POINT('Ctrl Pts',(0.213904514039949,2.34165928001635,11.0789456286619));
#41135=CARTESIAN_POINT('Ctrl Pts',(0.246240300319671,2.30982207801136,11.075917236271));
#41136=CARTESIAN_POINT('Ctrl Pts',(0.263679868442746,2.2874366970557,11.0739587115042));
#41137=CARTESIAN_POINT('Ctrl Pts',(0.279718055797393,2.26009630305539,11.0719233937438));
#41138=CARTESIAN_POINT('Ctrl Pts',(0.281411632792724,2.25710032551796,11.0717048798757));
#41139=CARTESIAN_POINT('Ctrl Pts',(0.283328344537239,2.25357912285398,11.0714537815786));
#41140=CARTESIAN_POINT('Ctrl Pts',(0.283598395506784,2.25307987415876,11.0714183124619));
#41141=CARTESIAN_POINT('Ctrl Pts',(0.28399910708349,2.25233437073984,11.0713655484525));
#41142=CARTESIAN_POINT('Ctrl Pts',(0.284130767607277,2.25208865912102,11.0713481902297));
#41143=CARTESIAN_POINT('Ctrl Pts',(0.284365210050861,2.25164976366982,11.0713172427194));
#41144=CARTESIAN_POINT('Ctrl Pts',(0.284468113929106,2.25145664616336,11.0713036456383));
#41145=CARTESIAN_POINT('Ctrl Pts',(0.284686704167322,2.25104541387169,11.0712747342533));
#41146=CARTESIAN_POINT('Ctrl Pts',(0.284802336260141,2.25082727154951,11.0712594234496));
#41147=CARTESIAN_POINT('Ctrl Pts',(0.285113172787784,2.25023924004627,11.0712182193114));
#41148=CARTESIAN_POINT('Ctrl Pts',(0.285307908893267,2.24986910180032,11.0711923557973));
#41149=CARTESIAN_POINT('Ctrl Pts',(0.286251249457965,2.24806757604753,11.071066820996));
#41150=CARTESIAN_POINT('Ctrl Pts',(0.286989822621137,2.24663092054597,11.0709677756827));
#41151=CARTESIAN_POINT('Ctrl Pts',(0.291186723640849,2.23831400680171,11.0704001595333));
#41152=CARTESIAN_POINT('Ctrl Pts',(0.294408667973479,2.23131652476751,11.0699452060125));
#41153=CARTESIAN_POINT('Ctrl Pts',(0.303225123611616,2.21020858436422,11.0686195744459));
#41154=CARTESIAN_POINT('Ctrl Pts',(0.308077472363713,2.19581095917314,11.0677748511331));
#41155=CARTESIAN_POINT('Ctrl Pts',(0.314869487164515,2.16969776225745,11.0662665723314));
#41156=CARTESIAN_POINT('Ctrl Pts',(0.317211239260883,2.1581169896719,11.0656057025822));
#41157=CARTESIAN_POINT('Ctrl Pts',(0.320996684282201,2.13211842079167,11.0641039172204));
#41158=CARTESIAN_POINT('Ctrl Pts',(0.322114557332758,2.11768027433914,11.0632573188632));
#41159=CARTESIAN_POINT('Ctrl Pts',(0.322271302044505,2.10197901312523,11.0623032319578));
#41160=CARTESIAN_POINT('Ctrl Pts',(0.322276526654214,2.10074088812983,11.0622277801365));
#41161=CARTESIAN_POINT('Ctrl Pts',(0.322273843065144,2.0990015220015,11.0621214676756));
#41162=CARTESIAN_POINT('Ctrl Pts',(0.322271900252881,2.09850027162237,11.0620907938385));
#41163=CARTESIAN_POINT('Ctrl Pts',(0.322266497944401,2.0976301958884,11.062037485386));
#41164=CARTESIAN_POINT('Ctrl Pts',(0.322263574667099,2.09726136716151,11.0620148675977));
#41165=CARTESIAN_POINT('Ctrl Pts',(0.32225624989628,2.09650174838609,11.0619682435209));
#41166=CARTESIAN_POINT('Ctrl Pts',(0.322251770710347,2.09611095982051,11.0619442348352));
#41167=CARTESIAN_POINT('Ctrl Pts',(0.32223959754566,2.09519438803488,11.0618878700318));
#41168=CARTESIAN_POINT('Ctrl Pts',(0.322231327556487,2.0946686147481,11.0618554959246));
#41169=CARTESIAN_POINT('Ctrl Pts',(0.322211171522466,2.09355975953625,11.0617871304216));
#41170=CARTESIAN_POINT('Ctrl Pts',(0.322198989441538,2.09297668548288,11.0617511298493));
#41171=CARTESIAN_POINT('Ctrl Pts',(0.322162028490324,2.0914111154573,11.0616543271295));
#41172=CARTESIAN_POINT('Ctrl Pts',(0.322134338011105,2.09042870027305,11.0615934338998));
#41173=CARTESIAN_POINT('Ctrl Pts',(0.322035864637907,2.08742322411333,11.0614066837301));
#41174=CARTESIAN_POINT('Ctrl Pts',(0.321950515038195,2.08540072021513,11.0612803722761));
#41175=CARTESIAN_POINT('Ctrl Pts',(0.32029236528087,2.05329223099935,11.0592646618716));
#41176=CARTESIAN_POINT('Ctrl Pts',(0.314527605761694,2.02357761218143,11.0572323069601));
#41177=CARTESIAN_POINT('Ctrl Pts',(0.299903426465526,1.9810939538075,11.0541958279302));
#41178=CARTESIAN_POINT('Ctrl Pts',(0.294119812161654,1.96743176257577,11.0532013403303));
#41179=CARTESIAN_POINT('Ctrl Pts',(0.285910411790693,1.95124688877837,11.0520369663987));
#41180=CARTESIAN_POINT('Ctrl Pts',(0.2843589592489,1.94830215524334,11.0518257401204));
#41181=CARTESIAN_POINT('Ctrl Pts',(0.282495867423631,1.9448949761208,11.05158253724));
#41182=CARTESIAN_POINT('Ctrl Pts',(0.282228381032615,1.9444087904327,11.051547862261));
#41183=CARTESIAN_POINT('Ctrl Pts',(0.281824021988285,1.94367829750742,11.0514958092828));
#41184=CARTESIAN_POINT('Ctrl Pts',(0.281688086219814,1.94343347700394,11.0514783718401));
#41185=CARTESIAN_POINT('Ctrl Pts',(0.281445290663683,1.942997541639,11.0514473365238));
#41186=CARTESIAN_POINT('Ctrl Pts',(0.281338555273559,1.94280635863426,11.051433730683));
#41187=CARTESIAN_POINT('Ctrl Pts',(0.281111425655288,1.94240049945948,11.0514048577014));
#41188=CARTESIAN_POINT('Ctrl Pts',(0.280990980664248,1.94218585300777,11.0513895939443));
#41189=CARTESIAN_POINT('Ctrl Pts',(0.280666881642268,1.94160981959497,11.0513486478316));
#41190=CARTESIAN_POINT('Ctrl Pts',(0.280462774706148,1.94124868596375,11.0513229946538));
#41191=CARTESIAN_POINT('Ctrl Pts',(0.279479200947461,1.93951623153267,11.0512000074647));
#41192=CARTESIAN_POINT('Ctrl Pts',(0.278690353321097,1.93815022116898,11.0511032691406));
#41193=CARTESIAN_POINT('Ctrl Pts',(0.27203104218852,1.92681166241834,11.0503017892195));
#41194=CARTESIAN_POINT('Ctrl Pts',(0.26563667952492,1.91715496782149,11.0496287843113));
#41195=CARTESIAN_POINT('Ctrl Pts',(0.240250574813183,1.88296961864961,11.047202714715));
#41196=CARTESIAN_POINT('Ctrl Pts',(0.218270933963974,1.86087572183108,11.0455293532236));
#41197=CARTESIAN_POINT('Ctrl Pts',(0.192520298191899,1.84154588523502,11.0436320462348));
#41198=CARTESIAN_POINT('Ctrl Pts',(0.191563664544495,1.84083604218772,11.0435616702048));
#41199=CARTESIAN_POINT('Ctrl Pts',(0.185877920286694,1.83666577631576,11.0431439745677));
#41200=CARTESIAN_POINT('Ctrl Pts',(0.181059318987063,1.83332973372031,11.0427923298735));
#41201=CARTESIAN_POINT('Ctrl Pts',(0.175324772006733,1.82958665453525,11.0423754421814));
#41202=CARTESIAN_POINT('Ctrl Pts',(0.174494388865769,1.82905007601985,11.0423151144478));
#41203=CARTESIAN_POINT('Ctrl Pts',(0.17323913449647,1.82824711710714,11.0422239731899));
#41204=CARTESIAN_POINT('Ctrl Pts',(0.172816083772021,1.82797789011392,11.0421932655301));
#41205=CARTESIAN_POINT('Ctrl Pts',(0.172060362746374,1.82749942817451,11.042138426083));
#41206=CARTESIAN_POINT('Ctrl Pts',(0.171727934110242,1.82728981185572,11.0421143084859));
#41207=CARTESIAN_POINT('Ctrl Pts',(0.171033590667704,1.82685375941754,11.0420639447801));
#41208=CARTESIAN_POINT('Ctrl Pts',(0.170671607888851,1.82662743345599,11.0420376946634));
#41209=CARTESIAN_POINT('Ctrl Pts',(0.169722914018998,1.82603689123126,11.0419689128574));
#41210=CARTESIAN_POINT('Ctrl Pts',(0.169135482410123,1.8256738417734,11.0419263382903));
#41211=CARTESIAN_POINT('Ctrl Pts',(0.16784948556733,1.82488475993528,11.0418331656254));
#41212=CARTESIAN_POINT('Ctrl Pts',(0.167150457094497,1.82445949518378,11.0417825396755));
#41213=CARTESIAN_POINT('Ctrl Pts',(0.165099279114955,1.82322230727891,11.041634040344));
#41214=CARTESIAN_POINT('Ctrl Pts',(0.16374279454102,1.82241765141529,11.0415359027395));
#41215=CARTESIAN_POINT('Ctrl Pts',(0.159070777691876,1.81969241076672,11.0411980978001));
#41216=CARTESIAN_POINT('Ctrl Pts',(0.155727032314647,1.81782107401212,11.0409566725901));
#41217=CARTESIAN_POINT('Ctrl Pts',(0.145708991078284,1.81244674342985,11.0402341163603));
#41218=CARTESIAN_POINT('Ctrl Pts',(0.138944662149605,1.80911797607926,11.0397471622313));
#41219=CARTESIAN_POINT('Ctrl Pts',(0.100930842397006,1.79203974173737,11.0370166351006));
#41220=CARTESIAN_POINT('Ctrl Pts',(0.0677721683802175,1.78308830305369,
11.0346271685664));
#41221=CARTESIAN_POINT('Ctrl Pts',(0.0302654281520986,1.77912926837845,
11.0322030515938));
#41222=CARTESIAN_POINT('Ctrl Pts',(0.0266947533513148,1.77881249191683,
11.031975301615));
#41223=CARTESIAN_POINT('Ctrl Pts',(0.0225460814464715,1.7785141057799,11.0317147648449));
#41224=CARTESIAN_POINT('Ctrl Pts',(0.0219726903407202,1.77847440714246,
11.0316788461748));
#41225=CARTESIAN_POINT('Ctrl Pts',(0.0211196163049158,1.77841763739252,
11.0316255448654));
#41226=CARTESIAN_POINT('Ctrl Pts',(0.0208400163266329,1.7783993969937,11.0316080969997));
#41227=CARTESIAN_POINT('Ctrl Pts',(0.0203418600286957,1.77836755091128,
11.0315770501018));
#41228=CARTESIAN_POINT('Ctrl Pts',(0.0201233137717307,1.77835380334885,
11.0315634430796));
#41229=CARTESIAN_POINT('Ctrl Pts',(0.0196591910234741,1.7783250827866,11.0315345750139));
#41230=CARTESIAN_POINT('Ctrl Pts',(0.0194136120554594,1.77831016829269,
11.031519317339));
#41231=CARTESIAN_POINT('Ctrl Pts',(0.0187543718336034,1.77827088899131,
11.0314784045715));
#41232=CARTESIAN_POINT('Ctrl Pts',(0.0183406785079819,1.77824704065116,
11.0314527785743));
#41233=CARTESIAN_POINT('Ctrl Pts',(0.0163568486976606,1.77813651658437,
11.0313301166423));
#41234=CARTESIAN_POINT('Ctrl Pts',(0.0147861031163011,1.77806053387875,
11.0312336725858));
#41235=CARTESIAN_POINT('Ctrl Pts',(0.00171869788088448,1.77752425629725,
11.0304364904961));
#41236=CARTESIAN_POINT('Ctrl Pts',(-0.00979585634195999,1.77766839654384,
11.0297671310321));
#41237=CARTESIAN_POINT('Ctrl Pts',(-0.0245016404735278,1.77864151713911,
11.0289271936185));
#41238=CARTESIAN_POINT('Ctrl Pts',(-0.0277206975157908,1.77890317892308,
11.0287442636428));
#41239=CARTESIAN_POINT('Ctrl Pts',(-0.0335646388919616,1.7794667439872,
11.0284130544401));
#41240=CARTESIAN_POINT('Ctrl Pts',(-0.0361907565463395,1.7797526228393,
11.0282645440845));
#41241=CARTESIAN_POINT('Ctrl Pts',(-0.0410439982808445,1.78034140703195,
11.0279902596633));
#41242=CARTESIAN_POINT('Ctrl Pts',(-0.0432720300804582,1.78063538493908,
11.0278644086016));
#41243=CARTESIAN_POINT('Ctrl Pts',(-0.0648293316889683,1.78370950079021,
11.0266460526296));
#41244=CARTESIAN_POINT('Ctrl Pts',(-0.0838698940767816,1.78821754088196,
11.025561537711));
#41245=CARTESIAN_POINT('Ctrl Pts',(-0.104098591739613,1.79499520404949,
11.0243222163564));
#41246=CARTESIAN_POINT('Ctrl Pts',(-0.105807482652546,1.79558380659809,
11.0242168449933));
#41247=CARTESIAN_POINT('Ctrl Pts',(-0.109291999942323,1.79681688321899,
11.0240005220917));
#41248=CARTESIAN_POINT('Ctrl Pts',(-0.111067088979279,1.79746265503595,
11.0238895375877));
#41249=CARTESIAN_POINT('Ctrl Pts',(-0.119097215571865,1.80046418653697,
11.0233837073748));
#41250=CARTESIAN_POINT('Ctrl Pts',(-0.125283358621095,1.80299845029202,
11.0229835779295));
#41251=CARTESIAN_POINT('Ctrl Pts',(-0.132336707711849,1.80614756152015,
11.0225134808532));
#41252=CARTESIAN_POINT('Ctrl Pts',(-0.133285418125911,1.80657665893172,
11.0224499562903));
#41253=CARTESIAN_POINT('Ctrl Pts',(-0.134691306536387,1.80722076100732,
11.0223553757741));
#41254=CARTESIAN_POINT('Ctrl Pts',(-0.135150091809499,1.80743225823597,
11.0223244406983));
#41255=CARTESIAN_POINT('Ctrl Pts',(-0.135965301887799,1.80781039184513,
11.0222693462241));
#41256=CARTESIAN_POINT('Ctrl Pts',(-0.136321923188993,1.80797660421292,
11.0222452015121));
#41257=CARTESIAN_POINT('Ctrl Pts',(-0.137010098445047,1.80829888098698,
11.0221985255289));
#41258=CARTESIAN_POINT('Ctrl Pts',(-0.13734169251422,1.80845485871835,11.0221759972878));
#41259=CARTESIAN_POINT('Ctrl Pts',(-0.138241775466249,1.80888012291063,
11.0221147436299));
#41260=CARTESIAN_POINT('Ctrl Pts',(-0.138809740948873,1.80915050777191,
11.0220759801544));
#41261=CARTESIAN_POINT('Ctrl Pts',(-0.141003111879503,1.81020256897181,
11.0219258485607));
#41262=CARTESIAN_POINT('Ctrl Pts',(-0.142622711880395,1.81099621034718,
11.021814064774));
#41263=CARTESIAN_POINT('Ctrl Pts',(-0.146634782764315,1.81300415627534,
11.0215348055511));
#41264=CARTESIAN_POINT('Ctrl Pts',(-0.149018877871526,1.81423480413325,
11.0213667623699));
#41265=CARTESIAN_POINT('Ctrl Pts',(-0.158327768679603,1.8191881364948,11.0207021861747));
#41266=CARTESIAN_POINT('Ctrl Pts',(-0.165130277988696,1.82313367952103,
11.0201978958739));
#41267=CARTESIAN_POINT('Ctrl Pts',(-0.177771575930151,1.83109747659912,
11.0192244968837));
#41268=CARTESIAN_POINT('Ctrl Pts',(-0.183635541835949,1.83506740854312,
11.0187571505113));
#41269=CARTESIAN_POINT('Ctrl Pts',(-0.211803155702295,1.85552169293917,
11.0164367826161));
#41270=CARTESIAN_POINT('Ctrl Pts',(-0.232044528409271,1.87464356862274,
11.0145160745419));
#41271=CARTESIAN_POINT('Ctrl Pts',(-0.252350114430097,1.8995014730939,11.0124423923362));
#41272=CARTESIAN_POINT('Ctrl Pts',(-0.255043477133289,1.9029389206495,11.0121639983922));
#41273=CARTESIAN_POINT('Ctrl Pts',(-0.258027329705992,1.90691081327303,
11.011852690093));
#41274=CARTESIAN_POINT('Ctrl Pts',(-0.258387009880774,1.9073923935957,11.0118151149746));
#41275=CARTESIAN_POINT('Ctrl Pts',(-0.258916184969184,1.90810506283431,
11.0117597634147));
#41276=CARTESIAN_POINT('Ctrl Pts',(-0.259086719712887,1.9083353725416,11.0117419147737));
#41277=CARTESIAN_POINT('Ctrl Pts',(-0.259387899072206,1.90874325622439,
11.0117103738938));
#41278=CARTESIAN_POINT('Ctrl Pts',(-0.25951866883508,1.90892073699119,11.0116966728617));
#41279=CARTESIAN_POINT('Ctrl Pts',(-0.259791507792974,1.90929183087134,
11.0116680740764));
#41280=CARTESIAN_POINT('Ctrl Pts',(-0.259933542396538,1.90948546818722,
11.0116531787552));
#41281=CARTESIAN_POINT('Ctrl Pts',(-0.260304551421007,1.90999245606685,
11.0116142508483));
#41282=CARTESIAN_POINT('Ctrl Pts',(-0.260533177362328,1.91030606298766,
11.011590242614));
#41283=CARTESIAN_POINT('Ctrl Pts',(-0.26153023281012,1.91167892985865,11.0114854504282));
#41284=CARTESIAN_POINT('Ctrl Pts',(-0.262292786927755,1.9127424709231,11.0114050690028));
#41285=CARTESIAN_POINT('Ctrl Pts',(-0.267883344341346,1.92064082668769,
11.0108137674166));
#41286=CARTESIAN_POINT('Ctrl Pts',(-0.272450451507057,1.92765738291489,
11.0103195579266));
#41287=CARTESIAN_POINT('Ctrl Pts',(-0.2912016926338,1.95907752358079,11.0082024002778));
#41288=CARTESIAN_POINT('Ctrl Pts',(-0.302418854024023,1.985105968262,11.0066814454124));
#41289=CARTESIAN_POINT('Ctrl Pts',(-0.310711320300946,2.01441583205885,
11.0049312656844));
#41290=CARTESIAN_POINT('Ctrl Pts',(-0.311297573753096,2.01657341751796,
11.0048022975496));
#41291=CARTESIAN_POINT('Ctrl Pts',(-0.312508079197259,2.02121894326585,
11.0045241528572));
#41292=CARTESIAN_POINT('Ctrl Pts',(-0.313125170536016,2.02370857468679,
11.0043748069752));
#41293=CARTESIAN_POINT('Ctrl Pts',(-0.314135560411626,2.02800389326498,
11.0041164630363));
#41294=CARTESIAN_POINT('Ctrl Pts',(-0.314543170787361,2.02980610266152,
11.0040078640121));
#41295=CARTESIAN_POINT('Ctrl Pts',(-0.316343626074911,2.03809738625001,
11.0035071287701));
#41296=CARTESIAN_POINT('Ctrl Pts',(-0.317551230152649,2.04462464494493,
11.0031097627783));
#41297=CARTESIAN_POINT('Ctrl Pts',(-0.31871381437623,2.0522112997722,11.0026426526187));
#41298=CARTESIAN_POINT('Ctrl Pts',(-0.318866238879339,2.05323915091653,
11.002579258297));
#41299=CARTESIAN_POINT('Ctrl Pts',(-0.319085316794538,2.05476736777779,
11.0024848345324));
#41300=CARTESIAN_POINT('Ctrl Pts',(-0.319155770787228,2.05526718899678,
11.0024539253791));
#41301=CARTESIAN_POINT('Ctrl Pts',(-0.319279044924097,2.05615684931865,
11.0023988600579));
#41302=CARTESIAN_POINT('Ctrl Pts',(-0.319332326163335,2.05654662436303,
11.0023747185198));
#41303=CARTESIAN_POINT('Ctrl Pts',(-0.319433861995732,2.057299675252,11.0023280444873));
#41304=CARTESIAN_POINT('Ctrl Pts',(-0.319482210925086,2.05766293794149,
11.0023055150149));
#41305=CARTESIAN_POINT('Ctrl Pts',(-0.319585361997866,2.05844818778289,
11.0022567823775));
#41306=CARTESIAN_POINT('Ctrl Pts',(-0.319639948113751,2.05887020217776,
11.0022305724271));
#41307=CARTESIAN_POINT('Ctrl Pts',(-0.319770202014971,2.05989313822431,
11.0021669928502));
#41308=CARTESIAN_POINT('Ctrl Pts',(-0.319845011704316,2.06049416577215,
11.0021295961878));
#41309=CARTESIAN_POINT('Ctrl Pts',(-0.320043362362268,2.06212523167554,
11.0020279980808));
#41310=CARTESIAN_POINT('Ctrl Pts',(-0.320163623885117,2.06315565486961,
11.0019636933928));
#41311=CARTESIAN_POINT('Ctrl Pts',(-0.321617301848811,2.07615589485294,
11.0011508482936));
#41312=CARTESIAN_POINT('Ctrl Pts',(-0.322283506226235,2.08818906550373,
11.0003813438037));
#41313=CARTESIAN_POINT('Ctrl Pts',(-0.32227491802331,2.10022986532739,10.9995935809957));
#41314=CARTESIAN_POINT('',(-0.322274874088783,2.09970506445917,10.749346402247));
#41315=CARTESIAN_POINT('Ctrl Pts',(-0.322274918312996,2.1002294588239,10.9995936075909));
#41316=CARTESIAN_POINT('Ctrl Pts',(-0.322254316620498,2.12916453594962,
10.9977005467693));
#41317=CARTESIAN_POINT('Ctrl Pts',(-0.318337387949409,2.15796166008248,
10.9957002776856));
#41318=CARTESIAN_POINT('Ctrl Pts',(-0.3089462136507,2.19194228602188,10.9933681639819));
#41319=CARTESIAN_POINT('Ctrl Pts',(-0.307082988721927,2.19798569347298,
10.9929552751647));
#41320=CARTESIAN_POINT('Ctrl Pts',(-0.3040875609404,2.20677407166114,10.9923613634342));
#41321=CARTESIAN_POINT('Ctrl Pts',(-0.303093442514989,2.20956419913827,
10.9921737956288));
#41322=CARTESIAN_POINT('Ctrl Pts',(-0.301885355354942,2.21281250649253,
10.9919569134209));
#41323=CARTESIAN_POINT('Ctrl Pts',(-0.301708643818288,2.2132842603914,10.9919254524363));
#41324=CARTESIAN_POINT('Ctrl Pts',(-0.301437080941571,2.21400408936757,
10.9918775061136));
#41325=CARTESIAN_POINT('Ctrl Pts',(-0.301343028918333,2.21425246204196,
10.9918609732035));
#41326=CARTESIAN_POINT('Ctrl Pts',(-0.301178787374538,2.21468457763812,
10.9918322284167));
#41327=CARTESIAN_POINT('Ctrl Pts',(-0.301108736863945,2.21486837204954,
10.9918200082126));
#41328=CARTESIAN_POINT('Ctrl Pts',(-0.300949785464969,2.21528427486162,
10.9917923690978));
#41329=CARTESIAN_POINT('Ctrl Pts',(-0.300860784485301,2.2155163441322,10.9917769563335));
#41330=CARTESIAN_POINT('Ctrl Pts',(-0.300618636409769,2.21614556491955,
10.9917351923026));
#41331=CARTESIAN_POINT('Ctrl Pts',(-0.300464970138649,2.21654251812908,
10.991708872271));
#41332=CARTESIAN_POINT('Ctrl Pts',(-0.299768965779487,2.21832992120043,
10.9915904769586));
#41333=CARTESIAN_POINT('Ctrl Pts',(-0.299217748024084,2.21971692681167,
10.991498927462));
#41334=CARTESIAN_POINT('Ctrl Pts',(-0.286543749729241,2.25097352823701,
10.9894420916439));
#41335=CARTESIAN_POINT('Ctrl Pts',(-0.270014895549163,2.27886618433466,
10.9877223439953));
#41336=CARTESIAN_POINT('Ctrl Pts',(-0.24636705480681,2.30782408624367,10.9856019524841));
#41337=CARTESIAN_POINT('Ctrl Pts',(-0.243022451321976,2.31172543971965,
10.9853085200821));
#41338=CARTESIAN_POINT('Ctrl Pts',(-0.234031854218152,2.32171881209846,
10.984533264499));
#41339=CARTESIAN_POINT('Ctrl Pts',(-0.228241429859492,2.32767514960056,
10.9840470198535));
#41340=CARTESIAN_POINT('Ctrl Pts',(-0.220203271341155,2.33532851329367,
10.9833839950791));
#41341=CARTESIAN_POINT('Ctrl Pts',(-0.218153818122197,2.33722963723058,
10.9832159359588));
#41342=CARTESIAN_POINT('Ctrl Pts',(-0.214699020833591,2.34035176385765,
10.9829340984594));
#41343=CARTESIAN_POINT('Ctrl Pts',(-0.213307339321934,2.34158770395463,
10.9828209521063));
#41344=CARTESIAN_POINT('Ctrl Pts',(-0.211424555353486,2.34323083632394,
10.9826683581312));
#41345=CARTESIAN_POINT('Ctrl Pts',(-0.210942817587459,2.34364874316177,
10.9826293564194));
#41346=CARTESIAN_POINT('Ctrl Pts',(-0.210182117332645,2.34430470250415,
10.9825678338617));
#41347=CARTESIAN_POINT('Ctrl Pts',(-0.209903981748576,2.34454371502128,
10.9825453527292));
#41348=CARTESIAN_POINT('Ctrl Pts',(-0.209327089228582,2.34503775144521,
10.9824987511044));
#41349=CARTESIAN_POINT('Ctrl Pts',(-0.209028272924962,2.34529270481218,
10.9824746277635));
#41350=CARTESIAN_POINT('Ctrl Pts',(-0.20834822011093,2.34587078833507,10.9824197613047));
#41351=CARTESIAN_POINT('Ctrl Pts',(-0.2079666972623,2.34619357872461,10.9823890043224));
#41352=CARTESIAN_POINT('Ctrl Pts',(-0.206834232999903,2.34714719813158,
10.9822977795223));
#41353=CARTESIAN_POINT('Ctrl Pts',(-0.206081166134593,2.34777548388713,
10.9822372080432));
#41354=CARTESIAN_POINT('Ctrl Pts',(-0.200924954385384,2.35203755761678,
10.9818230803444));
#41355=CARTESIAN_POINT('Ctrl Pts',(-0.196429034515186,2.35555702966356,
10.9814649377996));
#41356=CARTESIAN_POINT('Ctrl Pts',(-0.190873433857037,2.35967279716054,
10.981025498682));
#41357=CARTESIAN_POINT('Ctrl Pts',(-0.189900617704411,2.36038506998423,
10.9809486642239));
#41358=CARTESIAN_POINT('Ctrl Pts',(-0.186218527130038,2.36304939925105,
10.9806582703352));
#41359=CARTESIAN_POINT('Ctrl Pts',(-0.183483036271274,2.36496471541736,
10.9804433860462));
#41360=CARTESIAN_POINT('Ctrl Pts',(-0.167480955484765,2.3758022991545,10.9791912758487));
#41361=CARTESIAN_POINT('Ctrl Pts',(-0.153596232881644,2.38376904641042,
10.9781225019774));
#41362=CARTESIAN_POINT('Ctrl Pts',(-0.127084837253748,2.39646320816438,
10.976136632348));
#41363=CARTESIAN_POINT('Ctrl Pts',(-0.114640459262448,2.40149389703811,
10.9752251475055));
#41364=CARTESIAN_POINT('Ctrl Pts',(-0.0923493499580106,2.40892478214824,
10.9736590598583));
#41365=CARTESIAN_POINT('Ctrl Pts',(-0.0826344512289054,2.41166410603651,
10.9729978027781));
#41366=CARTESIAN_POINT('Ctrl Pts',(-0.0713828064349738,2.41427345614789,
10.9722677230855));
#41367=CARTESIAN_POINT('Ctrl Pts',(-0.0699572672683585,2.41459385124713,
10.9721758755418));
#41368=CARTESIAN_POINT('Ctrl Pts',(-0.0681349771411878,2.41499041825054,
10.9720593378102));
#41369=CARTESIAN_POINT('Ctrl Pts',(-0.0677402239639423,2.41507554770442,
10.9720341449901));
#41370=CARTESIAN_POINT('Ctrl Pts',(-0.0671070212604436,2.41521085434428,
10.9719938192418));
#41371=CARTESIAN_POINT('Ctrl Pts',(-0.0668686746399742,2.41526150312358,
10.9719786592792));
#41372=CARTESIAN_POINT('Ctrl Pts',(-0.0664155347493087,2.41535725858015,
10.9719498743019));
#41373=CARTESIAN_POINT('Ctrl Pts',(-0.0662007546369079,2.4154024157818,
10.9719362465048));
#41374=CARTESIAN_POINT('Ctrl Pts',(-0.0657121539662772,2.41550462227561,
10.9719052804098));
#41375=CARTESIAN_POINT('Ctrl Pts',(-0.0654383055761518,2.4155615344444,
10.9718879500929));
#41376=CARTESIAN_POINT('Ctrl Pts',(-0.0645890026122627,2.41573688656978,
10.9718342802672));
#41377=CARTESIAN_POINT('Ctrl Pts',(-0.064013293893507,2.41585411033732,
10.9717980102496));
#41378=CARTESIAN_POINT('Ctrl Pts',(-0.0596521447409737,2.41672969844215,
10.9715240700566));
#41379=CARTESIAN_POINT('Ctrl Pts',(-0.0558534718073047,2.41742160158631,
10.9712901062092));
#41380=CARTESIAN_POINT('Ctrl Pts',(-0.022133890849511,2.4229392807607,10.9692469362343));
#41381=CARTESIAN_POINT('Ctrl Pts',(0.00832014880910999,2.42359083319733,
10.9676232160316));
#41382=CARTESIAN_POINT('Ctrl Pts',(0.0497949703326796,2.41861087059711,
10.9652492598846));
#41383=CARTESIAN_POINT('Ctrl Pts',(0.0610878232946712,2.41663964773347,
10.9645874688396));
#41384=CARTESIAN_POINT('Ctrl Pts',(0.0757319884901491,2.41327080868357,
10.9636950022801));
#41385=CARTESIAN_POINT('Ctrl Pts',(0.0791992448934196,2.41241224648511,
10.9634811622914));
#41386=CARTESIAN_POINT('Ctrl Pts',(0.0840984811542229,2.41111229888031,
10.9631750862183));
#41387=CARTESIAN_POINT('Ctrl Pts',(0.0855428338205187,2.41071826549557,
10.9630843645337));
#41388=CARTESIAN_POINT('Ctrl Pts',(0.0877428747093789,2.41010157061525,
10.9629454121138));
#41389=CARTESIAN_POINT('Ctrl Pts',(0.0885005919638206,2.4098861748532,10.9628974164195));
#41390=CARTESIAN_POINT('Ctrl Pts',(0.0898781615628398,2.40948910952578,
10.9628099012137));
#41391=CARTESIAN_POINT('Ctrl Pts',(0.0904982736319636,2.40930834987281,
10.9627704114327));
#41392=CARTESIAN_POINT('Ctrl Pts',(0.0915278360996699,2.40900487625663,
10.9627046878403));
#41393=CARTESIAN_POINT('Ctrl Pts',(0.0919375952288033,2.4088832091782,10.962678488258));
#41394=CARTESIAN_POINT('Ctrl Pts',(0.0927235219460625,2.40864814670382,
10.9626281557183));
#41395=CARTESIAN_POINT('Ctrl Pts',(0.0930997268350522,2.40853487784504,
10.9626040269384));
#41396=CARTESIAN_POINT('Ctrl Pts',(0.0939547066874318,2.40827575191144,
10.9625491090141));
#41397=CARTESIAN_POINT('Ctrl Pts',(0.0944333500400041,2.40812946714165,
10.9625183059064));
#41398=CARTESIAN_POINT('Ctrl Pts',(0.0958522123211437,2.40769221260033,
10.9624268204824));
#41399=CARTESIAN_POINT('Ctrl Pts',(0.0967914348802043,2.40739805204516,
10.9623660336209));
#41400=CARTESIAN_POINT('Ctrl Pts',(0.103231934263653,2.40534847132313,10.9619476182942));
#41401=CARTESIAN_POINT('Ctrl Pts',(0.108686211086973,2.40344986693634,10.9615852953156));
#41402=CARTESIAN_POINT('Ctrl Pts',(0.115180196672241,2.40099180393797,10.9611438379382));
#41403=CARTESIAN_POINT('Ctrl Pts',(0.116271846229873,2.40057179086019,10.9610692824062));
#41404=CARTESIAN_POINT('Ctrl Pts',(0.143171311263054,2.39005372836305,10.9592235711181));
#41405=CARTESIAN_POINT('Ctrl Pts',(0.16756828748977,2.37667583573062,10.9573390505891));
#41406=CARTESIAN_POINT('Ctrl Pts',(0.202882739244931,2.35091059781883,10.9543912104484));
#41407=CARTESIAN_POINT('Ctrl Pts',(0.215097910206543,2.34052144286568,10.9533245559022));
#41408=CARTESIAN_POINT('Ctrl Pts',(0.227027262906564,2.32873645301858,10.9522719553081));
#41409=CARTESIAN_POINT('Ctrl Pts',(0.227561287297254,2.32820517871654,10.9522248124474));
#41410=CARTESIAN_POINT('Ctrl Pts',(0.228314563999211,2.3274505077033,10.9521582888395));
#41411=CARTESIAN_POINT('Ctrl Pts',(0.228535355924007,2.32722866166774,10.952138787075));
#41412=CARTESIAN_POINT('Ctrl Pts',(0.228913682197164,2.32684741997869,10.9521053660784));
#41413=CARTESIAN_POINT('Ctrl Pts',(0.229071373813674,2.32668818131585,10.9520914343164));
#41414=CARTESIAN_POINT('Ctrl Pts',(0.229372836325212,2.32638312550459,10.9520647981472));
#41415=CARTESIAN_POINT('Ctrl Pts',(0.22951663414784,2.32623733601492,10.9520520915594));
#41416=CARTESIAN_POINT('Ctrl Pts',(0.22985478371803,2.32589384870671,10.9520222083011));
#41417=CARTESIAN_POINT('Ctrl Pts',(0.230049019887142,2.3256960365888,10.9520050408094));
#41418=CARTESIAN_POINT('Ctrl Pts',(0.230621243873135,2.32511177161235,10.9519544573711));
#41419=CARTESIAN_POINT('Ctrl Pts',(0.230998517266899,2.32472461563995,10.9519210973174));
#41420=CARTESIAN_POINT('Ctrl Pts',(0.234267124511223,2.32135345947039,10.9516319681619));
#41421=CARTESIAN_POINT('Ctrl Pts',(0.23710163858998,2.31831458173548,10.9513805170775));
#41422=CARTESIAN_POINT('Ctrl Pts',(0.240112276858187,2.31495905310643,10.9511115257517));
#41423=CARTESIAN_POINT('Ctrl Pts',(0.240347375534513,2.31469615526651,10.9510905074132));
#41424=CARTESIAN_POINT('Ctrl Pts',(0.240667576049242,2.31433690766734,10.9510618621699));
#41425=CARTESIAN_POINT('Ctrl Pts',(0.240753051632117,2.31424089310806,10.9510542136806));
#41426=CARTESIAN_POINT('Ctrl Pts',(0.26291036367739,2.28932162143064,10.949071063481));
#41427=CARTESIAN_POINT('Ctrl Pts',(0.281014620332351,2.26123268985443,10.94730844595));
#41428=CARTESIAN_POINT('Ctrl Pts',(0.298453417663256,2.22198838381815,10.9448383265381));
#41429=CARTESIAN_POINT('Ctrl Pts',(0.301995551289514,2.21293480116184,10.9442697073108));
#41430=CARTESIAN_POINT('Ctrl Pts',(0.305893015935163,2.20147097981928,10.9435440885228));
#41431=CARTESIAN_POINT('Ctrl Pts',(0.306637690292235,2.19919790002815,10.9433999543898));
#41432=CARTESIAN_POINT('Ctrl Pts',(0.307691347324556,2.19585638559832,10.943187609609));
#41433=CARTESIAN_POINT('Ctrl Pts',(0.308020223203044,2.19479427160036,10.943120047172));
#41434=CARTESIAN_POINT('Ctrl Pts',(0.308601785342841,2.19288111649883,10.9429982177161));
#41435=CARTESIAN_POINT('Ctrl Pts',(0.308856464905853,2.19203068933758,10.942944016205));
#41436=CARTESIAN_POINT('Ctrl Pts',(0.309240909085793,2.19072738121578,10.9428608758231));
#41437=CARTESIAN_POINT('Ctrl Pts',(0.309373201238093,2.19027524525831,10.9428320195204));
#41438=CARTESIAN_POINT('Ctrl Pts',(0.309612821181782,2.18944958148121,10.9427792981806));
#41439=CARTESIAN_POINT('Ctrl Pts',(0.309720465742506,2.18907614588346,10.9427554435234));
#41440=CARTESIAN_POINT('Ctrl Pts',(0.309950777308237,2.18827169474433,10.9427040350708));
#41441=CARTESIAN_POINT('Ctrl Pts',(0.310073221206371,2.18784061665591,10.9426764740658));
#41442=CARTESIAN_POINT('Ctrl Pts',(0.310398684274769,2.18668562564395,10.94260259423));
#41443=CARTESIAN_POINT('Ctrl Pts',(0.310600069066699,2.18596125856009,10.9425562223569));
#41444=CARTESIAN_POINT('Ctrl Pts',(0.311499074570377,2.18268319194556,10.9423461965308));
#41445=CARTESIAN_POINT('Ctrl Pts',(0.312167732363441,2.18012171919535,10.9421816062565));
#41446=CARTESIAN_POINT('Ctrl Pts',(0.312960646702323,2.17692352681353,10.94197545816));
#41447=CARTESIAN_POINT('Ctrl Pts',(0.313114653077911,2.17629422900715,10.9419348642213));
#41448=CARTESIAN_POINT('Ctrl Pts',(0.313504607476084,2.17467973619252,10.9418306382932));
#41449=CARTESIAN_POINT('Ctrl Pts',(0.313737808262352,2.17369389076172,10.9417669190733));
#41450=CARTESIAN_POINT('Ctrl Pts',(0.31405875518752,2.17230796401215,10.9416772313852));
#41451=CARTESIAN_POINT('Ctrl Pts',(0.314150394484256,2.17190878258199,10.9416513863601));
#41452=CARTESIAN_POINT('Ctrl Pts',(0.314280578138682,2.17133670309884,10.9416143286759));
#41453=CARTESIAN_POINT('Ctrl Pts',(0.3143197415451,2.17116394507767,10.9416031355049));
#41454=CARTESIAN_POINT('Ctrl Pts',(0.321651449884091,2.13869811527477,10.9394991892384));
#41455=CARTESIAN_POINT('Ctrl Pts',(0.323923122566275,2.10547854432306,10.9372318975712));
#41456=CARTESIAN_POINT('Ctrl Pts',(0.320074875582644,2.06053197107727,10.9342072271989));
#41457=CARTESIAN_POINT('Ctrl Pts',(0.318380185112872,2.04862124594854,10.9334134189066));
#41458=CARTESIAN_POINT('Ctrl Pts',(0.315708264437853,2.03525390527992,10.932550648803));
#41459=CARTESIAN_POINT('Ctrl Pts',(0.31538103641162,2.03367830563291,10.9324494087023));
#41460=CARTESIAN_POINT('Ctrl Pts',(0.314954016971755,2.0316968721015,10.9323227214565));
#41461=CARTESIAN_POINT('Ctrl Pts',(0.314865227085134,2.03128872825598,10.9322966596325));
#41462=CARTESIAN_POINT('Ctrl Pts',(0.314722717788588,2.03063972730411,10.9322552729572));
#41463=CARTESIAN_POINT('Ctrl Pts',(0.314669515175312,2.03039875905561,10.932239918519));
#41464=CARTESIAN_POINT('Ctrl Pts',(0.314568608398194,2.02994420703047,10.9322109776543));
#41465=CARTESIAN_POINT('Ctrl Pts',(0.314520963842863,2.02973061248421,10.9321973879688));
#41466=CARTESIAN_POINT('Ctrl Pts',(0.314412091095358,2.0292448558908,10.9321665041076));
#41467=CARTESIAN_POINT('Ctrl Pts',(0.314350727184671,2.0289727252054,10.9321492178825));
#41468=CARTESIAN_POINT('Ctrl Pts',(0.314163213885511,2.0281461624335,10.9320967594241));
#41469=CARTESIAN_POINT('Ctrl Pts',(0.314035949611341,2.02759198044919,10.9320616511268));
#41470=CARTESIAN_POINT('Ctrl Pts',(0.313123686387054,2.02366710813565,10.9318134344212));
#41471=CARTESIAN_POINT('Ctrl Pts',(0.312285865082099,2.02030875721253,10.9316032953075));
#41472=CARTESIAN_POINT('Ctrl Pts',(0.30412240492641,1.98969474568462,10.9297029302322));
#41473=CARTESIAN_POINT('Ctrl Pts',(0.293299188776839,1.96349445808206,10.9281790672865));
#41474=CARTESIAN_POINT('Ctrl Pts',(0.27064135323254,1.92419331536507,10.9256178589639));
#41475=CARTESIAN_POINT('Ctrl Pts',(0.26091500242289,1.91005796651308,10.9246307799976));
#41476=CARTESIAN_POINT('Ctrl Pts',(0.249032498569792,1.89543479785534,10.9234951732656));
#41477=CARTESIAN_POINT('Ctrl Pts',(0.247942173707335,1.89411462996041,10.9233915672007));
#41478=CARTESIAN_POINT('Ctrl Pts',(0.246282758382411,1.89213770531581,10.9232347427594));
#41479=CARTESIAN_POINT('Ctrl Pts',(0.24572143520289,1.89147444548307,10.9231818397407));
#41480=CARTESIAN_POINT('Ctrl Pts',(0.24480964222259,1.89040586409597,10.9230961358285));
#41481=CARTESIAN_POINT('Ctrl Pts',(0.244460829260343,1.88999912932942,10.9230634029898));
#41482=CARTESIAN_POINT('Ctrl Pts',(0.243790300620451,1.88922119119517,10.923000581946));
#41483=CARTESIAN_POINT('Ctrl Pts',(0.243468747166803,1.88884984947532,10.9229705004899));
#41484=CARTESIAN_POINT('Ctrl Pts',(0.242893253357124,1.88818831052414,10.9229167413469));
#41485=CARTESIAN_POINT('Ctrl Pts',(0.242639638238097,1.88789783056598,10.9228930772035));
#41486=CARTESIAN_POINT('Ctrl Pts',(0.242135290452497,1.88732226048309,10.9228460710658));
#41487=CARTESIAN_POINT('Ctrl Pts',(0.241884574095973,1.88703715680657,10.9228227297723));
#41488=CARTESIAN_POINT('Ctrl Pts',(0.241274795363934,1.88634620906036,10.9227660227479));
#41489=CARTESIAN_POINT('Ctrl Pts',(0.240915212987752,1.88594082732541,10.9227326352689));
#41490=CARTESIAN_POINT('Ctrl Pts',(0.23956552476436,1.88442694030493,10.9226075090879));
#41491=CARTESIAN_POINT('Ctrl Pts',(0.238568788506461,1.88332439511175,10.9225154915827));
#41492=CARTESIAN_POINT('Ctrl Pts',(0.220630299820272,1.86375547317653,10.9208661447417));
#41493=CARTESIAN_POINT('Ctrl Pts',(0.201602972975033,1.84732444533936,10.9192123540315));
#41494=CARTESIAN_POINT('Ctrl Pts',(0.16777896148828,1.82438874823419,10.916452550539));
#41495=CARTESIAN_POINT('Ctrl Pts',(0.15405209957324,1.81648752694927,10.9153756496069));
#41496=CARTESIAN_POINT('Ctrl Pts',(0.134071172587125,1.80686773202247,10.9139079826725));
#41497=CARTESIAN_POINT('Ctrl Pts',(0.128261309521345,1.80427943318373,10.9134925004579));
#41498=CARTESIAN_POINT('Ctrl Pts',(0.119566489977303,1.80071039373603,10.9128909615369));
#41499=CARTESIAN_POINT('Ctrl Pts',(0.116738381563927,1.79959599559338,10.912698398922));
#41500=CARTESIAN_POINT('Ctrl Pts',(0.113420286245595,1.79834245973328,10.9124764183916));
#41501=CARTESIAN_POINT('Ctrl Pts',(0.112945339238842,1.79816431078419,10.9124447380932));
#41502=CARTESIAN_POINT('Ctrl Pts',(0.112220391474482,1.79789433919556,10.9123965269131));
#41503=CARTESIAN_POINT('Ctrl Pts',(0.111970696998275,1.79780170488944,10.9123799476507));
#41504=CARTESIAN_POINT('Ctrl Pts',(0.111536325250548,1.79764116931983,10.9123511519816));
#41505=CARTESIAN_POINT('Ctrl Pts',(0.111351701107732,1.79757312784446,10.9123389271494));
#41506=CARTESIAN_POINT('Ctrl Pts',(0.110934228695462,1.79741970646472,10.9123113169187));
#41507=CARTESIAN_POINT('Ctrl Pts',(0.110701344600727,1.79733442640971,10.9122959375879));
#41508=CARTESIAN_POINT('Ctrl Pts',(0.110070780717832,1.79710434474412,10.9122543572663));
#41509=CARTESIAN_POINT('Ctrl Pts',(0.109672912008038,1.79696005689472,10.9122281870433));
#41510=CARTESIAN_POINT('Ctrl Pts',(0.107891537478405,1.79631800578265,10.9121113047588));
#41511=CARTESIAN_POINT('Ctrl Pts',(0.106504890900473,1.79582892004842,10.9120211022404));
#41512=CARTESIAN_POINT('Ctrl Pts',(0.0743400643474861,1.78473095328814,
10.9099457077039));
#41513=CARTESIAN_POINT('Ctrl Pts',(0.0421281686983365,1.77883479836709,
10.9082110626206));
#41514=CARTESIAN_POINT('Ctrl Pts',(-0.00711923318000085,1.77737109440469,
10.9054145130027));
#41515=CARTESIAN_POINT('Ctrl Pts',(-0.0238236530241909,1.77817332683375,
10.9044439802448));
#41516=CARTESIAN_POINT('Ctrl Pts',(-0.0416961499783715,1.7804310060269,
10.9033497841008));
#41517=CARTESIAN_POINT('Ctrl Pts',(-0.043001996829613,1.78060410300044,
10.9032695245635));
#41518=CARTESIAN_POINT('Ctrl Pts',(-0.044857634027944,1.78086166379507,
10.9031550172557));
#41519=CARTESIAN_POINT('Ctrl Pts',(-0.0454083356291735,1.78093955429183,
10.9031209773756));
#41520=CARTESIAN_POINT('Ctrl Pts',(-0.046356353356507,1.78107614477175,
10.9030622789614));
#41521=CARTESIAN_POINT('Ctrl Pts',(-0.0467537677345155,1.78113416280443,
10.9030376420575));
#41522=CARTESIAN_POINT('Ctrl Pts',(-0.0475126636617733,1.78124640233266,
10.9029905377392));
#41523=CARTESIAN_POINT('Ctrl Pts',(-0.0478741637130052,1.78130049626462,
10.9029680743997));
#41524=CARTESIAN_POINT('Ctrl Pts',(-0.04871808646623,1.78142824696226,10.9029155744689));
#41525=CARTESIAN_POINT('Ctrl Pts',(-0.0492004344679933,1.78150238458278,
10.9028855226772));
#41526=CARTESIAN_POINT('Ctrl Pts',(-0.0508566626605956,1.78176080152828,
10.9027821779457));
#41527=CARTESIAN_POINT('Ctrl Pts',(-0.0520296802832212,1.78195047572764,
10.9027087141035));
#41528=CARTESIAN_POINT('Ctrl Pts',(-0.0646036709469267,1.78405508309663,
10.9019182780645));
#41529=CARTESIAN_POINT('Ctrl Pts',(-0.0758934435529317,1.78657543915536,
10.9011820395239));
#41530=CARTESIAN_POINT('Ctrl Pts',(-0.106434539356613,1.79514047041579,
10.8991140943432));
#41531=CARTESIAN_POINT('Ctrl Pts',(-0.12529113690889,1.80239354146713,10.8977487760819));
#41532=CARTESIAN_POINT('Ctrl Pts',(-0.159478555645247,1.81937163159771,
10.8951675838473));
#41533=CARTESIAN_POINT('Ctrl Pts',(-0.174914761135057,1.82872397092471,
10.893956884432));
#41534=CARTESIAN_POINT('Ctrl Pts',(-0.190466743979409,1.84002874482821,
10.8927444072567));
#41535=CARTESIAN_POINT('Ctrl Pts',(-0.191439617028282,1.84074432075764,
10.8926685992253));
#41536=CARTESIAN_POINT('Ctrl Pts',(-0.192710679276106,1.84169027962395,
10.8925696334761));
#41537=CARTESIAN_POINT('Ctrl Pts',(-0.193012503042593,1.84191572845193,
10.8925461390678));
#41538=CARTESIAN_POINT('Ctrl Pts',(-0.193504043646303,1.84228423181158,
10.8925078872289));
#41539=CARTESIAN_POINT('Ctrl Pts',(-0.193693997730832,1.84242696700869,
10.8924931074868));
#41540=CARTESIAN_POINT('Ctrl Pts',(-0.194060625142903,1.84270309290592,
10.8924645865368));
#41541=CARTESIAN_POINT('Ctrl Pts',(-0.194237318433028,1.84283645522895,
10.8924508434548));
#41542=CARTESIAN_POINT('Ctrl Pts',(-0.194646996931876,1.84314633027963,
10.8924189841531));
#41543=CARTESIAN_POINT('Ctrl Pts',(-0.194879880320359,1.84332297860666,
10.8924008775076));
#41544=CARTESIAN_POINT('Ctrl Pts',(-0.195633331826957,1.84389610840547,
10.8923423082637));
#41545=CARTESIAN_POINT('Ctrl Pts',(-0.196152937086307,1.84429386182243,
10.8923019347568));
#41546=CARTESIAN_POINT('Ctrl Pts',(-0.201177682031358,1.8481645902218,10.8919116441347));
#41547=CARTESIAN_POINT('Ctrl Pts',(-0.205591674108126,1.85175494646884,
10.8915698359808));
#41548=CARTESIAN_POINT('Ctrl Pts',(-0.210099706711998,1.855624566939,10.8912191013189));
#41549=CARTESIAN_POINT('Ctrl Pts',(-0.210290602584344,1.855788817804,10.8912042460605));
#41550=CARTESIAN_POINT('Ctrl Pts',(-0.234795515099827,1.87692340327459,
10.8892968729428));
#41551=CARTESIAN_POINT('Ctrl Pts',(-0.255841720139801,1.90141089006542,
10.8875866634696));
#41552=CARTESIAN_POINT('Ctrl Pts',(-0.278955740211868,1.93821740473511,
10.8850841948291));
#41553=CARTESIAN_POINT('Ctrl Pts',(-0.284477639338235,1.94813709026265,
10.8844174875965));
#41554=CARTESIAN_POINT('Ctrl Pts',(-0.29035718954039,1.96015008023005,10.8836087549886));
#41555=CARTESIAN_POINT('Ctrl Pts',(-0.291232431988367,1.96198200174203,
10.883485405026));
#41556=CARTESIAN_POINT('Ctrl Pts',(-0.292369123367405,1.96442010930197,
10.8833211663119));
#41557=CARTESIAN_POINT('Ctrl Pts',(-0.292646115816498,1.96501903116504,
10.8832808153461));
#41558=CARTESIAN_POINT('Ctrl Pts',(-0.293097759542932,1.96600351446988,
10.8832144771566));
#41559=CARTESIAN_POINT('Ctrl Pts',(-0.293273495054448,1.96638857878403,
10.8831885273421));
#41560=CARTESIAN_POINT('Ctrl Pts',(-0.293612485267293,1.9671352509777,10.8831382026958));
#41561=CARTESIAN_POINT('Ctrl Pts',(-0.293775831879298,1.96749681649491,
10.8831138310801));
#41562=CARTESIAN_POINT('Ctrl Pts',(-0.294151348364753,1.96833212491591,
10.8830575199645));
#41563=CARTESIAN_POINT('Ctrl Pts',(-0.294363041740745,1.9688060796909,10.8830255641853));
#41564=CARTESIAN_POINT('Ctrl Pts',(-0.295037021186503,1.97032487839287,
10.8829231444916));
#41565=CARTESIAN_POINT('Ctrl Pts',(-0.295494892439676,1.9713716612771,10.8828525297723));
#41566=CARTESIAN_POINT('Ctrl Pts',(-0.299649797587623,1.98100985401166,
10.8822020801297));
#41567=CARTESIAN_POINT('Ctrl Pts',(-0.302976406617867,1.98975516428787,
10.88160973112));
#41568=CARTESIAN_POINT('Ctrl Pts',(-0.315418084558816,2.02730284350263,
10.8790539498074));
#41569=CARTESIAN_POINT('Ctrl Pts',(-0.32083960404873,2.05716510600591,10.876972307672));
#41570=CARTESIAN_POINT('Ctrl Pts',(-0.322193647604366,2.0915969622432,10.8746763502237));
#41571=CARTESIAN_POINT('Ctrl Pts',(-0.322276631350591,2.09586077190173,
10.8743942202839));
#41572=CARTESIAN_POINT('Ctrl Pts',(-0.322274825622189,2.10051169824796,
10.8740896644046));
#41573=CARTESIAN_POINT('Ctrl Pts',(-0.322273979979023,2.10089827381881,
10.8740643744063));
#41574=CARTESIAN_POINT('Ctrl Pts',(-0.322268744481638,2.10221146871072,
10.8739785481545));
#41575=CARTESIAN_POINT('Ctrl Pts',(-0.322261053749342,2.10313807832468,
10.8739181294848));
#41576=CARTESIAN_POINT('Ctrl Pts',(-0.32223793987718,2.1049705677535,10.8737989397274));
#41577=CARTESIAN_POINT('Ctrl Pts',(-0.322222693036883,2.10587644173465,
10.8737401624225));
#41578=CARTESIAN_POINT('Ctrl Pts',(-0.322200901706047,2.10691168030863,
10.873673163529));
#41579=CARTESIAN_POINT('Ctrl Pts',(-0.322198099238625,2.10704111013993,
10.8736647901252));
#41580=CARTESIAN_POINT('Ctrl Pts',(-0.322187161584062,2.10753257392999,
10.8736330068673));
#41581=CARTESIAN_POINT('Ctrl Pts',(-0.32217849415639,2.10789459720923,10.8736096188517));
#41582=CARTESIAN_POINT('Ctrl Pts',(-0.322063063684964,2.11239864417594,
10.8733189489061));
#41583=CARTESIAN_POINT('Ctrl Pts',(-0.321877034748086,2.11653849738668,
10.8730550180787));
#41584=CARTESIAN_POINT('Ctrl Pts',(-0.321576555715706,2.12121287806403,
10.8727615263765));
#41585=CARTESIAN_POINT('Ctrl Pts',(-0.321540550165263,2.12175182730689,
10.8727277552361));
#41586=CARTESIAN_POINT('Ctrl Pts',(-0.321484022016173,2.12256714445417,
10.8726767721292));
#41587=CARTESIAN_POINT('Ctrl Pts',(-0.321464497884594,2.12284357725347,
10.8726595047004));
#41588=CARTESIAN_POINT('Ctrl Pts',(-0.321429928709937,2.12332420363556,
10.8726295146196));
#41589=CARTESIAN_POINT('Ctrl Pts',(-0.32141504563002,2.12352840812515,10.8726167828399));
#41590=CARTESIAN_POINT('Ctrl Pts',(-0.321383462720451,2.1239561213365,10.8725901371635));
#41591=CARTESIAN_POINT('Ctrl Pts',(-0.321366724336315,2.12417962674193,
10.872576225528));
#41592=CARTESIAN_POINT('Ctrl Pts',(-0.321326042531581,2.12471534064146,
10.872542910239));
#41593=CARTESIAN_POINT('Ctrl Pts',(-0.321301877147555,2.12502753314797,
10.8725235191398));
#41594=CARTESIAN_POINT('Ctrl Pts',(-0.321217966831608,2.12609141650644,
10.8724575178563));
#41595=CARTESIAN_POINT('Ctrl Pts',(-0.321156038134715,2.12684293998963,
10.8724110297553));
#41596=CARTESIAN_POINT('Ctrl Pts',(-0.319379622969743,2.14751361592085,
10.8711359180619));
#41597=CARTESIAN_POINT('Ctrl Pts',(-0.315817567634234,2.16723409805002,
10.8700087077598));
#41598=CARTESIAN_POINT('Ctrl Pts',(-0.304441948982124,2.20806140802929,
10.8676358545664));
#41599=CARTESIAN_POINT('Ctrl Pts',(-0.296205064151348,2.2289365695121,10.8663957408124));
#41600=CARTESIAN_POINT('Ctrl Pts',(-0.28505537167474,2.25035870644512,10.8649801648288));
#41601=CARTESIAN_POINT('Ctrl Pts',(-0.284225684101026,2.25192124886153,
10.8648760763473));
#41602=CARTESIAN_POINT('Ctrl Pts',(-0.280309857622231,2.259151520405,10.8643903783157));
#41603=CARTESIAN_POINT('Ctrl Pts',(-0.277066956436572,2.26473225398132,
10.8640037869734));
#41604=CARTESIAN_POINT('Ctrl Pts',(-0.273114567388822,2.27108673484803,
10.8635483235887));
#41605=CARTESIAN_POINT('Ctrl Pts',(-0.272566059816848,2.27195924156083,
10.8634854448175));
#41606=CARTESIAN_POINT('Ctrl Pts',(-0.271743593836216,2.27325370967893,
10.8633916418055));
#41607=CARTESIAN_POINT('Ctrl Pts',(-0.271472813460144,2.27367769072633,
10.8633608355396));
#41608=CARTESIAN_POINT('Ctrl Pts',(-0.270988629768869,2.27443191440212,
10.8633058857192));
#41609=CARTESIAN_POINT('Ctrl Pts',(-0.270775612263447,2.27476240450159,
10.8632817565698));
#41610=CARTESIAN_POINT('Ctrl Pts',(-0.270325770988583,2.27545752250566,
10.8632308981058));
#41611=CARTESIAN_POINT('Ctrl Pts',(-0.270088813242093,2.27582206238958,
10.8632041638177));
#41612=CARTESIAN_POINT('Ctrl Pts',(-0.269462129081457,2.27678190770583,
10.8631336055275));
#41613=CARTESIAN_POINT('Ctrl Pts',(-0.26907116920142,2.27737640145416,10.8630897353578));
#41614=CARTESIAN_POINT('Ctrl Pts',(-0.267303381510711,2.28004520622942,
10.86289202697));
#41615=CARTESIAN_POINT('Ctrl Pts',(-0.265904543063711,2.28210477059075,
10.8627373613536));
#41616=CARTESIAN_POINT('Ctrl Pts',(-0.255415098375652,2.29717021427896,
10.861590199882));
#41617=CARTESIAN_POINT('Ctrl Pts',(-0.24540022877856,2.30950312357756,10.8605616978375));
#41618=CARTESIAN_POINT('Ctrl Pts',(-0.21267000601413,2.34422817888678,10.8573888244243));
#41619=CARTESIAN_POINT('Ctrl Pts',(-0.187505946093624,2.36404054256763,
10.8551661494065));
#41620=CARTESIAN_POINT('Ctrl Pts',(-0.158550648780054,2.38057992092367,
10.8530572512341));
#41621=CARTESIAN_POINT('Ctrl Pts',(-0.157250372257713,2.38131071946006,
10.8529634465478));
#41622=CARTESIAN_POINT('Ctrl Pts',(-0.155572626892992,2.38223840008126,
10.8528436067625));
#41623=CARTESIAN_POINT('Ctrl Pts',(-0.155199804278868,2.3824435828189,10.852817051861));
#41624=CARTESIAN_POINT('Ctrl Pts',(-0.154608606444273,2.38276742422637,
10.8527750635793));
#41625=CARTESIAN_POINT('Ctrl Pts',(-0.154390500164541,2.38288656887558,
10.852759599122));
#41626=CARTESIAN_POINT('Ctrl Pts',(-0.153999528060085,2.3830995578787,10.8527319247046));
#41627=CARTESIAN_POINT('Ctrl Pts',(-0.15382671539677,2.38319349558986,10.8527197087809));
#41628=CARTESIAN_POINT('Ctrl Pts',(-0.153420334544091,2.38341391483853,
10.8526910205767));
#41629=CARTESIAN_POINT('Ctrl Pts',(-0.153186696262187,2.38354026568587,
10.852674556756));
#41630=CARTESIAN_POINT('Ctrl Pts',(-0.152509362044669,2.38390548433638,
10.8526269122443));
#41631=CARTESIAN_POINT('Ctrl Pts',(-0.152065259194466,2.38414360190195,
10.8525957793959));
#41632=CARTESIAN_POINT('Ctrl Pts',(-0.149004317073925,2.38577557588487,
10.8523819141305));
#41633=CARTESIAN_POINT('Ctrl Pts',(-0.146368800705609,2.38713436221885,
10.8522013657055));
#41634=CARTESIAN_POINT('Ctrl Pts',(-0.138051505692683,2.39127820287519,
10.8516415861598));
#41635=CARTESIAN_POINT('Ctrl Pts',(-0.132305952769972,2.3939325697275,10.8512693190619));
#41636=CARTESIAN_POINT('Ctrl Pts',(-0.112118376941293,2.40254693496245,
10.8499982120266));
#41637=CARTESIAN_POINT('Ctrl Pts',(-0.0973234851078491,2.40762539220445,
10.8491298564629));
#41638=CARTESIAN_POINT('Ctrl Pts',(-0.0668949738773259,2.41565387959206,
10.8473703637616));
#41639=CARTESIAN_POINT('Ctrl Pts',(-0.0512956472830773,2.4185608467032,
10.8464811473232));
#41640=CARTESIAN_POINT('Ctrl Pts',(-0.0322804170163812,2.42067109467057,
10.8453688679589));
#41641=CARTESIAN_POINT('Ctrl Pts',(-0.0290087619299157,2.42098359302477,
10.8451765541134));
#41642=CARTESIAN_POINT('Ctrl Pts',(-0.0245484507849553,2.42134088020315,
10.8449127816755));
#41643=CARTESIAN_POINT('Ctrl Pts',(-0.023363421891669,2.42142921178927,
10.8448425499225));
#41644=CARTESIAN_POINT('Ctrl Pts',(-0.0164123305417085,2.42190870054511,
10.8444296412595));
#41645=CARTESIAN_POINT('Ctrl Pts',(-0.0106373668911117,2.42215123167219,
10.8440827533912));
#41646=CARTESIAN_POINT('Ctrl Pts',(-0.00387491567942501,2.42225320762339,
10.8436710160015));
#41647=CARTESIAN_POINT('Ctrl Pts',(-0.0028905090694996,2.42226354078405,
10.8436109432667));
#41648=CARTESIAN_POINT('Ctrl Pts',(-0.00140553397426754,2.42227232374715,
10.8435201129249));
#41649=CARTESIAN_POINT('Ctrl Pts',(-0.000904984925018192,2.4222741180687,
10.8434894601056));
#41650=CARTESIAN_POINT('Ctrl Pts',(-1.1542251554175E-5,2.42227523928697,
10.8434346819036));
#41651=CARTESIAN_POINT('Ctrl Pts',(0.000381350629554541,2.42227501386274,
10.8434105705915));
#41652=CARTESIAN_POINT('Ctrl Pts',(0.00121041202159171,2.42227302210117,
10.8433596442969));
#41653=CARTESIAN_POINT('Ctrl Pts',(0.00164657900812938,2.42227108875305,
10.8433328241308));
#41654=CARTESIAN_POINT('Ctrl Pts',(0.00280044562657512,2.42226363160241,
10.8432617975017));
#41655=CARTESIAN_POINT('Ctrl Pts',(0.0035181300406506,2.42225659573851,
10.8432175437585));
#41656=CARTESIAN_POINT('Ctrl Pts',(0.00678621880943238,2.42221363832007,
10.8430156744027));
#41657=CARTESIAN_POINT('Ctrl Pts',(0.00933610820792382,2.42214983775739,
10.842857188052));
#41658=CARTESIAN_POINT('Ctrl Pts',(0.0204498601225729,2.42173970387509,
10.8421619773793));
#41659=CARTESIAN_POINT('Ctrl Pts',(0.0289980645457899,2.42108211381585,
10.8416156066078));
#41660=CARTESIAN_POINT('Ctrl Pts',(0.0518506750052404,2.41840411832439,
10.840122660526));
#41661=CARTESIAN_POINT('Ctrl Pts',(0.0660614457994081,2.41576175021939,
10.8391592651973));
#41662=CARTESIAN_POINT('Ctrl Pts',(0.100061661172676,2.40704366481283,10.8367908423604));
#41663=CARTESIAN_POINT('Ctrl Pts',(0.11953833727544,2.39999803835101,10.8353782450734));
#41664=CARTESIAN_POINT('Ctrl Pts',(0.142793934344817,2.38895821323529,10.8337078052743));
#41665=CARTESIAN_POINT('Ctrl Pts',(0.147329061408764,2.38667248130582,10.8333830738473));
#41666=CARTESIAN_POINT('Ctrl Pts',(0.152368685614037,2.38398127130485,10.8330249437837));
#41667=CARTESIAN_POINT('Ctrl Pts',(0.152927913338762,2.38368051069083,10.8329852419164));
#41668=CARTESIAN_POINT('Ctrl Pts',(0.153740130145165,2.38324058919787,10.8329276394043));
#41669=CARTESIAN_POINT('Ctrl Pts',(0.153993822444982,2.38310274042573,10.83290965607));
#41670=CARTESIAN_POINT('Ctrl Pts',(0.154441187509682,2.38285887642632,10.8328779595415));
#41671=CARTESIAN_POINT('Ctrl Pts',(0.15463493685416,2.38275300295109,10.8328642372649));
#41672=CARTESIAN_POINT('Ctrl Pts',(0.155038322735569,2.3825320358852,10.8328356784643));
#41673=CARTESIAN_POINT('Ctrl Pts',(0.155247939552821,2.38241690828205,10.8328208442059));
#41674=CARTESIAN_POINT('Ctrl Pts',(0.155786759878913,2.38212019144365,10.832782728005));
#41675=CARTESIAN_POINT('Ctrl Pts',(0.156115775298288,2.38193825863157,10.8327594681153));
#41676=CARTESIAN_POINT('Ctrl Pts',(0.157500660487726,2.38116930312701,10.8326616217875));
#41677=CARTESIAN_POINT('Ctrl Pts',(0.158553561158957,2.38057691178591,10.8325873752561));
#41678=CARTESIAN_POINT('Ctrl Pts',(0.166009405698405,2.37632667238095,10.8320624640645));
#41679=CARTESIAN_POINT('Ctrl Pts',(0.172289033519813,2.37245561244307,10.8316248037739));
#41680=CARTESIAN_POINT('Ctrl Pts',(0.187890154103074,2.36208299841643,10.8305344728968));
#41681=CARTESIAN_POINT('Ctrl Pts',(0.197010994941928,2.35529768771181,10.8298939995265));
#41682=CARTESIAN_POINT('Ctrl Pts',(0.227028489085056,2.33039792720633,10.8277088209117));
#41683=CARTESIAN_POINT('Ctrl Pts',(0.245940977411665,2.31009047109807,10.8261815815243));
#41684=CARTESIAN_POINT('Ctrl Pts',(0.263275708302855,2.28588074828818,10.8244000716234));
#41685=CARTESIAN_POINT('Ctrl Pts',(0.264503637797201,2.28412923838518,10.8242714611924));
#41686=CARTESIAN_POINT('Ctrl Pts',(0.266893076745795,2.28064773092194,10.824016275425));
#41687=CARTESIAN_POINT('Ctrl Pts',(0.268055424469995,2.27891843448501,10.8238897397952));
#41688=CARTESIAN_POINT('Ctrl Pts',(0.269581618897993,2.27659956379977,10.8237203050365));
#41689=CARTESIAN_POINT('Ctrl Pts',(0.269960468991074,2.2760198862409,10.8236779691838));
#41690=CARTESIAN_POINT('Ctrl Pts',(0.270548379797402,2.27511396276046,10.8236118356599));
#41691=CARTESIAN_POINT('Ctrl Pts',(0.270758727020435,2.27478855084024,10.8235880860411));
#41692=CARTESIAN_POINT('Ctrl Pts',(0.271159266944028,2.27416644847412,10.8235426937839));
#41693=CARTESIAN_POINT('Ctrl Pts',(0.271349560984522,2.27386982364876,10.8235210549582));
#41694=CARTESIAN_POINT('Ctrl Pts',(0.271792334550795,2.27317714372988,10.8234705344156));
#41695=CARTESIAN_POINT('Ctrl Pts',(0.2720444350845,2.27278084837991,10.823441638686));
#41696=CARTESIAN_POINT('Ctrl Pts',(0.272751531107803,2.27166392814386,10.8233602205534));
#41697=CARTESIAN_POINT('Ctrl Pts',(0.273204533208145,2.27094205146664,10.8233076245379));
#41698=CARTESIAN_POINT('Ctrl Pts',(0.275961294149326,2.26651009509438,10.8229848557913));
#41699=CARTESIAN_POINT('Ctrl Pts',(0.278192213177379,2.26275545196488,10.8227120211129));
#41700=CARTESIAN_POINT('Ctrl Pts',(0.284577792356043,2.2514934472642,10.8218949441144));
#41701=CARTESIAN_POINT('Ctrl Pts',(0.288509454058563,2.24386471994284,10.8213430165293));
#41702=CARTESIAN_POINT('Ctrl Pts',(0.302868305213806,2.21304162077153,10.819119239426));
#41703=CARTESIAN_POINT('Ctrl Pts',(0.3108389087555,2.1888060638396,10.8173752510299));
#41704=CARTESIAN_POINT('Ctrl Pts',(0.31716280067314,2.15754049933757,10.8152396653128));
#41705=CARTESIAN_POINT('Ctrl Pts',(0.318255514282371,2.15115259386374,10.8148097021576));
#41706=CARTESIAN_POINT('Ctrl Pts',(0.319219968588202,2.14427196206787,10.8143561049554));
#41707=CARTESIAN_POINT('Ctrl Pts',(0.319283969726922,2.14380800898004,10.8143255657953));
#41708=CARTESIAN_POINT('Ctrl Pts',(0.320114209472132,2.13769101344285,10.8139235465938));
#41709=CARTESIAN_POINT('Ctrl Pts',(0.320731287520682,2.13201828848829,10.8135577436096));
#41710=CARTESIAN_POINT('Ctrl Pts',(0.321250974254636,2.12567909643771,10.8131589439058));
#41711=CARTESIAN_POINT('Ctrl Pts',(0.321302490496047,2.12502626764627,10.8131179921234));
#41712=CARTESIAN_POINT('Ctrl Pts',(0.321374130021455,2.1240817289397,10.8130589162377));
#41713=CARTESIAN_POINT('Ctrl Pts',(0.321395846311586,2.1237901469322,10.8130407034126));
#41714=CARTESIAN_POINT('Ctrl Pts',(0.321433308186684,2.12327773668905,10.8130087399866));
#41715=CARTESIAN_POINT('Ctrl Pts',(0.321449223072885,2.12305692139539,10.8129949798098));
#41716=CARTESIAN_POINT('Ctrl Pts',(0.32148174423954,2.12259911908549,10.8129664808602));
#41717=CARTESIAN_POINT('Ctrl Pts',(0.321498315987564,2.12236213050614,10.8129517440802));
#41718=CARTESIAN_POINT('Ctrl Pts',(0.321539958544361,2.12175699528843,10.8129141553932));
#41719=CARTESIAN_POINT('Ctrl Pts',(0.321564659237252,2.12138882225719,10.8128913243839));
#41720=CARTESIAN_POINT('Ctrl Pts',(0.321663347109478,2.11987902239117,10.8127978540849));
#41721=CARTESIAN_POINT('Ctrl Pts',(0.321731888698102,2.11873702996835,10.8127275173552));
#41722=CARTESIAN_POINT('Ctrl Pts',(0.322162733150101,2.11085718583566,10.812244542223));
#41723=CARTESIAN_POINT('Ctrl Pts',(0.322319460272764,2.10410922070286,10.811842803961));
#41724=CARTESIAN_POINT('Ctrl Pts',(0.322170215683179,2.08588560106358,10.8107780117959));
#41725=CARTESIAN_POINT('Ctrl Pts',(0.321463384350314,2.07442279251201,10.8101296455797));
#41726=CARTESIAN_POINT('Ctrl Pts',(0.318151064318214,2.04574598094925,10.8085108981325));
#41727=CARTESIAN_POINT('Ctrl Pts',(0.314760745307126,2.02866101804574,10.807548186357));
#41728=CARTESIAN_POINT('Ctrl Pts',(0.308293931901818,2.00589683634375,10.8061938089964));
#41729=CARTESIAN_POINT('Ctrl Pts',(0.306403266848392,1.99991211037764,10.8058309528896));
#41730=CARTESIAN_POINT('Ctrl Pts',(0.303769500211715,1.99235119368304,10.8053615327717));
#41731=CARTESIAN_POINT('Ctrl Pts',(0.303186653246037,1.99072041408497,10.8052596251761));
#41732=CARTESIAN_POINT('Ctrl Pts',(0.300375677576086,1.98305105078815,10.8047770948787));
#41733=CARTESIAN_POINT('Ctrl Pts',(0.297980236284294,1.97707573723689,10.8043914992427));
#41734=CARTESIAN_POINT('Ctrl Pts',(0.294995983397775,1.97023249289481,10.8039371122638));
#41735=CARTESIAN_POINT('Ctrl Pts',(0.294579819742053,1.96929052871632,10.8038742817928));
#41736=CARTESIAN_POINT('Ctrl Pts',(0.293953711182385,1.96789154368097,10.8037805369586));
#41737=CARTESIAN_POINT('Ctrl Pts',(0.293747196819757,1.96743298711633,10.8037497403544));
#41738=CARTESIAN_POINT('Ctrl Pts',(0.293377320838695,1.96661680080161,10.8036948013628));
#41739=CARTESIAN_POINT('Ctrl Pts',(0.293214376166809,1.96625898229106,10.8036706733594));
#41740=CARTESIAN_POINT('Ctrl Pts',(0.292869827375283,1.96550602633493,10.8036198107353));
#41741=CARTESIAN_POINT('Ctrl Pts',(0.292688077572445,1.96511095677171,10.8035930711282));
#41742=CARTESIAN_POINT('Ctrl Pts',(0.292206683881702,1.96407010504709,10.8035224838292));
#41743=CARTESIAN_POINT('Ctrl Pts',(0.291905700070021,1.96342494846904,10.8034785899013));
#41744=CARTESIAN_POINT('Ctrl Pts',(0.290563828504156,1.96057335619494,10.8032839470755));
#41745=CARTESIAN_POINT('Ctrl Pts',(0.289500065727184,1.95837783063611,10.803132406664));
#41746=CARTESIAN_POINT('Ctrl Pts',(0.285336166523421,1.95002684542292,10.802549412836));
#41747=CARTESIAN_POINT('Ctrl Pts',(0.282063980205399,1.94395970263495,10.8021119786927));
#41748=CARTESIAN_POINT('Ctrl Pts',(0.274779318427399,1.9314316915685,10.8011784549952));
#41749=CARTESIAN_POINT('Ctrl Pts',(0.270727600632003,1.92499856860512,10.8006812427713));
#41750=CARTESIAN_POINT('Ctrl Pts',(0.256201855459062,1.90364863809213,10.7989713365855));
#41751=CARTESIAN_POINT('Ctrl Pts',(0.244692238546218,1.88947951314088,10.7977307628302));
#41752=CARTESIAN_POINT('Ctrl Pts',(0.221115940790994,1.86501680838258,10.7954398317263));
#41753=CARTESIAN_POINT('Ctrl Pts',(0.209365082551467,1.85448878692668,10.7943902494897));
#41754=CARTESIAN_POINT('Ctrl Pts',(0.196176144150561,1.84431091437637,10.7933426458307));
#41755=CARTESIAN_POINT('Ctrl Pts',(0.195460253945488,1.84376323992363,10.7932861654675));
#41756=CARTESIAN_POINT('Ctrl Pts',(0.194492881862838,1.84302958859923,10.79321036955));
#41757=CARTESIAN_POINT('Ctrl Pts',(0.194243422120287,1.84284097061193,10.7931908705696));
#41758=CARTESIAN_POINT('Ctrl Pts',(0.193822531167957,1.84252369433805,10.7931580510286));
#41759=CARTESIAN_POINT('Ctrl Pts',(0.193651246138516,1.8423948439272,10.7931447169323));
#41760=CARTESIAN_POINT('Ctrl Pts',(0.193322141882042,1.84214778658587,10.7931191395962));
#41761=CARTESIAN_POINT('Ctrl Pts',(0.193164343881372,1.84202955448821,10.7931068946283));
#41762=CARTESIAN_POINT('Ctrl Pts',(0.192790079310927,1.8417496680869,10.7930778964225));
#41763=CARTESIAN_POINT('Ctrl Pts',(0.192573518154887,1.84158814129249,10.7930611522335));
#41764=CARTESIAN_POINT('Ctrl Pts',(0.191943536556329,1.84111948771465,10.7930125440126));
#41765=CARTESIAN_POINT('Ctrl Pts',(0.191529580269318,1.84081307757253,10.7929807301094));
#41766=CARTESIAN_POINT('Ctrl Pts',(0.188488287307231,1.83857317962341,10.7927479062483));
#41767=CARTESIAN_POINT('Ctrl Pts',(0.185832343635391,1.83667860149329,10.792549548796));
#41768=CARTESIAN_POINT('Ctrl Pts',(0.177133834337808,1.83067082608023,10.7919142072025));
#41769=CARTESIAN_POINT('Ctrl Pts',(0.170979667262602,1.82672254280494,10.7914866064025));
#41770=CARTESIAN_POINT('Ctrl Pts',(0.150500920550196,1.81454706264683,10.7901155524729));
#41771=CARTESIAN_POINT('Ctrl Pts',(0.135677266190528,1.80721057699218,10.7892015917685));
#41772=CARTESIAN_POINT('Ctrl Pts',(0.098848311992101,1.79238378771678,10.7869781129733));
#41773=CARTESIAN_POINT('Ctrl Pts',(0.0764728904200744,1.78607263948,10.785660325576));
#41774=CARTESIAN_POINT('Ctrl Pts',(0.0521666338831035,1.78197173393901,
10.7841649158761));
#41775=CARTESIAN_POINT('Ctrl Pts',(0.0507157585877637,1.78173714099231,
10.7840754443978));
#41776=CARTESIAN_POINT('Ctrl Pts',(0.0487303563231147,1.78143004084754,
10.7839527095283));
#41777=CARTESIAN_POINT('Ctrl Pts',(0.0481971612349797,1.78134893669549,
10.7839197185659));
#41778=CARTESIAN_POINT('Ctrl Pts',(0.0472889729973594,1.78121312406217,
10.7838634740113));
#41779=CARTESIAN_POINT('Ctrl Pts',(0.0469140810878628,1.78115773769614,
10.783840241917));
#41780=CARTESIAN_POINT('Ctrl Pts',(0.0461884616525597,1.78105184246282,
10.7837952461277));
#41781=CARTESIAN_POINT('Ctrl Pts',(0.0458377466165753,1.7810012505201,10.783773485095));
#41782=CARTESIAN_POINT('Ctrl Pts',(0.0450047784740421,1.78088249381383,
10.7837217699005));
#41783=CARTESIAN_POINT('Ctrl Pts',(0.0445224539117189,1.78081484380767,
10.7836917995057));
#41784=CARTESIAN_POINT('Ctrl Pts',(0.0435239257859611,1.7806770993354,10.7836297009935));
#41785=CARTESIAN_POINT('Ctrl Pts',(0.0430077022223628,1.78060716265214,
10.7835975679744));
#41786=CARTESIAN_POINT('Ctrl Pts',(0.0400986429325167,1.78022023107301,
10.7834163238579));
#41787=CARTESIAN_POINT('Ctrl Pts',(0.0377025264427915,1.77992888169953,
10.7832664050089));
#41788=CARTESIAN_POINT('Ctrl Pts',(0.0243791632026217,1.77846054556863,
10.7824291016603));
#41789=CARTESIAN_POINT('Ctrl Pts',(0.0134016727939297,1.77781633631662,
10.7817250760602));
#41790=CARTESIAN_POINT('Ctrl Pts',(-0.0153453844068379,1.7776010274237,
10.77984378476));
#41791=CARTESIAN_POINT('Ctrl Pts',(-0.0330835211050536,1.7789362295998,
10.7786438881372));
#41792=CARTESIAN_POINT('Ctrl Pts',(-0.0648422002494271,1.7839872358441,
10.7764679307087));
#41793=CARTESIAN_POINT('Ctrl Pts',(-0.0788983628367126,1.7872002450973,
10.775495491016));
#41794=CARTESIAN_POINT('Ctrl Pts',(-0.0981707844038029,1.79298797823714,
10.7741848989983));
#41795=CARTESIAN_POINT('Ctrl Pts',(-0.103603952139945,1.7947785794191,10.7738181481725));
#41796=CARTESIAN_POINT('Ctrl Pts',(-0.109603861005411,1.79693466221395,
10.7734183992851));
#41797=CARTESIAN_POINT('Ctrl Pts',(-0.110220075302332,1.79715822558155,
10.7733774061805));
#41798=CARTESIAN_POINT('Ctrl Pts',(-0.111110274720616,1.79748426811576,
10.773318281662));
#41799=CARTESIAN_POINT('Ctrl Pts',(-0.111384804077562,1.79758524075671,
10.7733000613232));
#41800=CARTESIAN_POINT('Ctrl Pts',(-0.11186689015307,1.79776329883086,10.7732680891249));
#41801=CARTESIAN_POINT('Ctrl Pts',(-0.112074505271714,1.79784022452448,
10.7732543276733));
#41802=CARTESIAN_POINT('Ctrl Pts',(-0.112504677296678,1.79800011651413,
10.7732258305171));
#41803=CARTESIAN_POINT('Ctrl Pts',(-0.112727221386195,1.79808311475088,
10.7732110967968));
#41804=CARTESIAN_POINT('Ctrl Pts',(-0.113177731384221,1.79825170085499,
10.7731812880924));
#41805=CARTESIAN_POINT('Ctrl Pts',(-0.113405692488535,1.79833730122814,
10.7731662138721));
#41806=CARTESIAN_POINT('Ctrl Pts',(-0.113964366481706,1.79854780848473,
10.7731292928594));
#41807=CARTESIAN_POINT('Ctrl Pts',(-0.114294972239522,1.79867300167344,
10.7731074631));
#41808=CARTESIAN_POINT('Ctrl Pts',(-0.117197162756775,1.79977746143001,
10.7729159935531));
#41809=CARTESIAN_POINT('Ctrl Pts',(-0.119756414988149,1.80078912134339,
10.7727482593783));
#41810=CARTESIAN_POINT('Ctrl Pts',(-0.127698422202196,1.80404678858108,
10.7722302834361));
#41811=CARTESIAN_POINT('Ctrl Pts',(-0.133033630854286,1.80640631422611,
10.7718860012415));
#41812=CARTESIAN_POINT('Ctrl Pts',(-0.145807976095883,1.81247562911149,
10.7710638616066));
#41813=CARTESIAN_POINT('Ctrl Pts',(-0.153173438418639,1.81633092851107,
10.7705916484649));
#41814=CARTESIAN_POINT('Ctrl Pts',(-0.167248980172034,1.82440676164033,
10.7696778047332));
#41815=CARTESIAN_POINT('Ctrl Pts',(-0.173968550279033,1.82859845044054,
10.7692360983364));
#41816=CARTESIAN_POINT('Ctrl Pts',(-0.193904732327327,1.84207960883757,
10.7678905955094));
#41817=CARTESIAN_POINT('Ctrl Pts',(-0.206582853771419,1.85211808789723,
10.7669846279726));
#41818=CARTESIAN_POINT('Ctrl Pts',(-0.22567209497134,1.86971830563562,10.7654739439579));
#41819=CARTESIAN_POINT('Ctrl Pts',(-0.232581221058186,1.87669863558606,
10.7648915233247));
#41820=CARTESIAN_POINT('Ctrl Pts',(-0.239858432389519,1.88475550647357,
10.7642313472801));
#41821=CARTESIAN_POINT('Ctrl Pts',(-0.240552536525814,1.88553150181668,
10.764167882888));
#41822=CARTESIAN_POINT('Ctrl Pts',(-0.24158501751995,1.88669711391323,10.7640727268612));
#41823=CARTESIAN_POINT('Ctrl Pts',(-0.241926243234808,1.88708420741413,
10.7640411543528));
#41824=CARTESIAN_POINT('Ctrl Pts',(-0.242512304681486,1.88775227540928,
10.7639867125459));
#41825=CARTESIAN_POINT('Ctrl Pts',(-0.24275758616245,1.88803285897444,10.7639638618486));
#41826=CARTESIAN_POINT('Ctrl Pts',(-0.243262798702852,1.88861281122461,
10.763916660035));
#41827=CARTESIAN_POINT('Ctrl Pts',(-0.243522665041562,1.88891223526701,
10.7638923062895));
#41828=CARTESIAN_POINT('Ctrl Pts',(-0.244126240357445,1.88961028676714,
10.7638355670627));
#41829=CARTESIAN_POINT('Ctrl Pts',(-0.244469525864673,1.89000927738701,
10.7638031641654));
#41830=CARTESIAN_POINT('Ctrl Pts',(-0.245185987935276,1.89084613812682,
10.7637352584002));
#41831=CARTESIAN_POINT('Ctrl Pts',(-0.245558972192081,1.89128416977776,
10.7636997477658));
#41832=CARTESIAN_POINT('Ctrl Pts',(-0.246553615560689,1.89245863286658,
10.763604621645));
#41833=CARTESIAN_POINT('Ctrl Pts',(-0.247173143968474,1.89319685378121,
10.7635449191471));
#41834=CARTESIAN_POINT('Ctrl Pts',(-0.251699643887626,1.89863996102266,
10.7631053579098));
#41835=CARTESIAN_POINT('Ctrl Pts',(-0.255475071885383,1.90345215488008,
10.7627202152829));
#41836=CARTESIAN_POINT('Ctrl Pts',(-0.266748429169294,1.91869523109058,
10.7615097313423));
#41837=CARTESIAN_POINT('Ctrl Pts',(-0.273760717666368,1.92946804588284,
10.7606669029885));
#41838=CARTESIAN_POINT('Ctrl Pts',(-0.282428943559775,1.94470338840907,
10.7594961165116));
#41839=CARTESIAN_POINT('Ctrl Pts',(-0.284657654187898,1.94882737080095,
10.7591812800396));
#41840=CARTESIAN_POINT('Ctrl Pts',(-0.288995875197006,1.95729110644638,
10.7585402058681));
#41841=CARTESIAN_POINT('Ctrl Pts',(-0.291099489825572,1.96163262545429,
10.7582139804731));
#41842=CARTESIAN_POINT('Ctrl Pts',(-0.301787756297035,1.98501503467603,
10.7564742353186));
#41843=CARTESIAN_POINT('Ctrl Pts',(-0.308604591443418,2.00481175290639,
10.7550579039448));
#41844=CARTESIAN_POINT('Ctrl Pts',(-0.313744243975711,2.02633016006292,
10.7536620709368));
#41845=CARTESIAN_POINT('Ctrl Pts',(-0.314023811025219,2.02753109515205,
10.753584641336));
#41846=CARTESIAN_POINT('Ctrl Pts',(-0.314383842334844,2.0291188927553,10.7534829174762));
#41847=CARTESIAN_POINT('Ctrl Pts',(-0.314470492790375,2.02950432031956,
10.7534582750149));
#41848=CARTESIAN_POINT('Ctrl Pts',(-0.314603767138215,2.03010226995748,
10.7534201239611));
#41849=CARTESIAN_POINT('Ctrl Pts',(-0.314650884507248,2.03031467986631,
10.7534065870088));
#41850=CARTESIAN_POINT('Ctrl Pts',(-0.314744419923687,2.03073837608001,
10.7533796157682));
#41851=CARTESIAN_POINT('Ctrl Pts',(-0.314790840000343,2.03094965986041,
10.7533661814998));
#41852=CARTESIAN_POINT('Ctrl Pts',(-0.314895436098572,2.03142803291989,
10.7533357993947));
#41853=CARTESIAN_POINT('Ctrl Pts',(-0.314953484940393,2.03169514899971,
10.7533188589836));
#41854=CARTESIAN_POINT('Ctrl Pts',(-0.315073269849817,2.03224974754472,
10.7532837367297));
#41855=CARTESIAN_POINT('Ctrl Pts',(-0.315134952510768,2.0325372414641,10.7532655579586));
#41856=CARTESIAN_POINT('Ctrl Pts',(-0.315295126749975,2.03328880355613,
10.7532181074321));
#41857=CARTESIAN_POINT('Ctrl Pts',(-0.315392987693711,2.03375300758843,
10.7531888713319));
#41858=CARTESIAN_POINT('Ctrl Pts',(-0.315680163968844,2.03513029022962,
10.7531023368503));
#41859=CARTESIAN_POINT('Ctrl Pts',(-0.315866543726185,2.03604398564295,
10.7530452008022));
#41860=CARTESIAN_POINT('Ctrl Pts',(-0.320169775754063,2.05761758049861,
10.7517022603504));
#41861=CARTESIAN_POINT('Ctrl Pts',(-0.322255586913252,2.07863376685202,
10.7505244445363));
#41862=CARTESIAN_POINT('Ctrl Pts',(-0.322274865121244,2.09970515074319,
10.7493463817436));
#41863=CARTESIAN_POINT('',(-0.322378175270278,2.10028753889625,10.4993773449273));
#41864=CARTESIAN_POINT('Ctrl Pts',(-0.322274865041499,2.09970506359358,
10.749346386616));
#41865=CARTESIAN_POINT('Ctrl Pts',(-0.322298947962674,2.12602029631154,
10.747875149744));
#41866=CARTESIAN_POINT('Ctrl Pts',(-0.319100146337298,2.15223683286578,
10.7464067880084));
#41867=CARTESIAN_POINT('Ctrl Pts',(-0.312294610467603,2.17960409921395,
10.7447097168287));
#41868=CARTESIAN_POINT('Ctrl Pts',(-0.311823167679749,2.18143124833739,
10.7445956620758));
#41869=CARTESIAN_POINT('Ctrl Pts',(-0.311094630812034,2.18415567252314,
10.744424429838));
#41870=CARTESIAN_POINT('Ctrl Pts',(-0.310849635013528,2.18505616333527,
10.7443676417984));
#41871=CARTESIAN_POINT('Ctrl Pts',(-0.310450663350225,2.18649784874588,
10.7442764120228));
#41872=CARTESIAN_POINT('Ctrl Pts',(-0.31029917412897,2.18703973081777,10.7442420508823));
#41873=CARTESIAN_POINT('Ctrl Pts',(-0.310005712233462,2.18807895042629,
10.7441760158872));
#41874=CARTESIAN_POINT('Ctrl Pts',(-0.309863959764702,2.18857634875961,
10.7441443492701));
#41875=CARTESIAN_POINT('Ctrl Pts',(-0.309611814493428,2.18945309408581,
10.7440884241138));
#41876=CARTESIAN_POINT('Ctrl Pts',(-0.309501920051702,2.18983258427484,
10.7440641818648));
#41877=CARTESIAN_POINT('Ctrl Pts',(-0.309286221045972,2.19057234725597,
10.7440168550992));
#41878=CARTESIAN_POINT('Ctrl Pts',(-0.30918048407323,2.19093263925974,10.7439937728217));
#41879=CARTESIAN_POINT('Ctrl Pts',(-0.308895022809321,2.19189907628478,
10.7439317701755));
#41880=CARTESIAN_POINT('Ctrl Pts',(-0.308714144787251,2.19250487629064,
10.7438928121462));
#41881=CARTESIAN_POINT('Ctrl Pts',(-0.308048997736904,2.19470891996789,
10.7437507342567));
#41882=CARTESIAN_POINT('Ctrl Pts',(-0.307554096759057,2.19630390400352,
10.7436472667847));
#41883=CARTESIAN_POINT('Ctrl Pts',(-0.298907164508607,2.22342494795731,
10.7418765848048));
#41884=CARTESIAN_POINT('Ctrl Pts',(-0.287617053967074,2.24783445387442,
10.7400979402577));
#41885=CARTESIAN_POINT('Ctrl Pts',(-0.271109525969361,2.27429921569771,
10.7379882550481));
#41886=CARTESIAN_POINT('Ctrl Pts',(-0.268701074259604,2.27798967495513,
10.7376898907732));
#41887=CARTESIAN_POINT('Ctrl Pts',(-0.263954048790093,2.28494747437011,
10.7371203814653));
#41888=CARTESIAN_POINT('Ctrl Pts',(-0.261628532548203,2.28822279319848,
10.7368492118639));
#41889=CARTESIAN_POINT('Ctrl Pts',(-0.253165820068518,2.29968192028348,
10.7358912199109));
#41890=CARTESIAN_POINT('Ctrl Pts',(-0.246700451731211,2.30761677042343,
10.735210522179));
#41891=CARTESIAN_POINT('Ctrl Pts',(-0.237627904264332,2.31772782629353,
10.7343326017391));
#41892=CARTESIAN_POINT('Ctrl Pts',(-0.235348762854026,2.32018943914594,
10.7341179940958));
#41893=CARTESIAN_POINT('Ctrl Pts',(-0.232056064482261,2.32363620601565,
10.7338168096945));
#41894=CARTESIAN_POINT('Ctrl Pts',(-0.231073905433615,2.32465088494316,
10.7337280582832));
#41895=CARTESIAN_POINT('Ctrl Pts',(-0.229878412548336,2.32586982576314,
10.7336213716394));
#41896=CARTESIAN_POINT('Ctrl Pts',(-0.229671447282492,2.32608027125522,
10.7336029500902));
#41897=CARTESIAN_POINT('Ctrl Pts',(-0.22930944242504,2.32644735328804,10.7335708133176));
#41898=CARTESIAN_POINT('Ctrl Pts',(-0.229154531159029,2.32660411524599,
10.7335570881019));
#41899=CARTESIAN_POINT('Ctrl Pts',(-0.22884277404062,2.32691895024804,10.7335295206109));
#41900=CARTESIAN_POINT('Ctrl Pts',(-0.228685924671178,2.32707702012919,
10.7335156785938));
#41901=CARTESIAN_POINT('Ctrl Pts',(-0.228383273736942,2.32738139449964,
10.7334890228318));
#41902=CARTESIAN_POINT('Ctrl Pts',(-0.228237495679712,2.32752772106683,
10.7334762072742));
#41903=CARTESIAN_POINT('Ctrl Pts',(-0.227890852872223,2.32787499979183,
10.7334457894489));
#41904=CARTESIAN_POINT('Ctrl Pts',(-0.227689862447762,2.32807582706836,
10.7334281971804));
#41905=CARTESIAN_POINT('Ctrl Pts',(-0.227086533149923,2.32867707427269,
10.7333755215595));
#41906=CARTESIAN_POINT('Ctrl Pts',(-0.226683398982979,2.32907669997849,
10.7333405008279));
#41907=CARTESIAN_POINT('Ctrl Pts',(-0.222759111821345,2.33294633098297,
10.733001274239));
#41908=CARTESIAN_POINT('Ctrl Pts',(-0.219159377203399,2.33633617777352,
10.7327031976152));
#41909=CARTESIAN_POINT('Ctrl Pts',(-0.204157909887012,2.34982528945459,
10.7315061892919));
#41910=CARTESIAN_POINT('Ctrl Pts',(-0.192124151046473,2.35919400674232,
10.7306483123578));
#41911=CARTESIAN_POINT('Ctrl Pts',(-0.170176457118849,2.3739094618392,10.7291689120569));
#41912=CARTESIAN_POINT('Ctrl Pts',(-0.160562881928018,2.37965331498035,
10.7285461873567));
#41913=CARTESIAN_POINT('Ctrl Pts',(-0.138568829296287,2.39128552974201,
10.7271421017815));
#41914=CARTESIAN_POINT('Ctrl Pts',(-0.126073159891165,2.39690753071808,
10.7263574913742));
#41915=CARTESIAN_POINT('Ctrl Pts',(-0.109638873987785,2.40307662867029,
10.7253171200076));
#41916=CARTESIAN_POINT('Ctrl Pts',(-0.105994959828447,2.40437015643307,
10.7250859917346));
#41917=CARTESIAN_POINT('Ctrl Pts',(-0.100055025677356,2.40635913080523,
10.7247080451412));
#41918=CARTESIAN_POINT('Ctrl Pts',(-0.0977729069876538,2.40709507220141,
10.7245625600458));
#41919=CARTESIAN_POINT('Ctrl Pts',(-0.0948072288030243,2.40801504079811,
10.7243730687199));
#41920=CARTESIAN_POINT('Ctrl Pts',(-0.0941309386358112,2.40822239109148,
10.7243298286319));
#41921=CARTESIAN_POINT('Ctrl Pts',(-0.0930387630393945,2.4085533218532,
10.7242599498034));
#41922=CARTESIAN_POINT('Ctrl Pts',(-0.0926232985535299,2.40867829275266,
10.7242333566144));
#41923=CARTESIAN_POINT('Ctrl Pts',(-0.0918306228589753,2.40891498361228,
10.7241825968639));
#41924=CARTESIAN_POINT('Ctrl Pts',(-0.0914534566807141,2.40902685264199,
10.7241584352265));
#41925=CARTESIAN_POINT('Ctrl Pts',(-0.0905918456461861,2.40928069446871,
10.7241032175996));
#41926=CARTESIAN_POINT('Ctrl Pts',(-0.0901072710311573,2.40942221990563,
10.7240721470738));
#41927=CARTESIAN_POINT('Ctrl Pts',(-0.0886239874656251,2.40985164963416,
10.7239769905544));
#41928=CARTESIAN_POINT('Ctrl Pts',(-0.0876242238987311,2.41013585939218,
10.7239127843964));
#41929=CARTESIAN_POINT('Ctrl Pts',(-0.0802244784532333,2.41220079992454,
10.7234370328298));
#41930=CARTESIAN_POINT('Ctrl Pts',(-0.0737725856011363,2.41378798805052,
10.7230192456786));
#41931=CARTESIAN_POINT('Ctrl Pts',(-0.0654651764833456,2.41556127321382,
10.7224769617545));
#41932=CARTESIAN_POINT('Ctrl Pts',(-0.0636504578355044,2.41593231154828,
10.7223582434674));
#41933=CARTESIAN_POINT('Ctrl Pts',(-0.0599144870418084,2.41666267528131,
10.722113304814));
#41934=CARTESIAN_POINT('Ctrl Pts',(-0.0579929644795718,2.41702020675858,
10.7219870373087));
#41935=CARTESIAN_POINT('Ctrl Pts',(-0.0407613136134358,2.42006453921861,
10.7208521619613));
#41936=CARTESIAN_POINT('Ctrl Pts',(-0.0252803082319925,2.42165758931989,
10.7198131369327));
#41937=CARTESIAN_POINT('Ctrl Pts',(0.00553072171022078,2.422589818381,10.7177309124917));
#41938=CARTESIAN_POINT('Ctrl Pts',(0.02082175660266,2.42196469037408,10.716690841117));
#41939=CARTESIAN_POINT('Ctrl Pts',(0.0451900359692089,2.41922461576825,
10.715066236458));
#41940=CARTESIAN_POINT('Ctrl Pts',(0.0543214520439307,2.41779822476334,
10.7144653013709));
#41941=CARTESIAN_POINT('Ctrl Pts',(0.0641483601666872,2.41582713286592,
10.7138359049116));
#41942=CARTESIAN_POINT('Ctrl Pts',(0.0649162972986963,2.41567018285206,
10.7137868362696));
#41943=CARTESIAN_POINT('Ctrl Pts',(0.0659257224586744,2.41546003847582,
10.7137224974864));
#41944=CARTESIAN_POINT('Ctrl Pts',(0.066167724158927,2.41540936739016,10.7137070848949));
#41945=CARTESIAN_POINT('Ctrl Pts',(0.0666446111939686,2.41530894226107,
10.7136767371661));
#41946=CARTESIAN_POINT('Ctrl Pts',(0.0668794996752409,2.41525920414016,
10.7136618011274));
#41947=CARTESIAN_POINT('Ctrl Pts',(0.0673299694455499,2.4151632901314,10.7136331792871));
#41948=CARTESIAN_POINT('Ctrl Pts',(0.0675455582484216,2.41511715566297,
10.7136194912026));
#41949=CARTESIAN_POINT('Ctrl Pts',(0.0680413648033316,2.41501052439887,
10.7135880342486));
#41950=CARTESIAN_POINT('Ctrl Pts',(0.0683215501142049,2.41494987473862,
10.7135702742098));
#41951=CARTESIAN_POINT('Ctrl Pts',(0.069189430855253,2.41476079832211,10.7135153124763));
#41952=CARTESIAN_POINT('Ctrl Pts',(0.0697768521861863,2.41463109893208,
10.7134781835308));
#41953=CARTESIAN_POINT('Ctrl Pts',(0.0746372189181442,2.41354367544523,
10.7131715437163));
#41954=CARTESIAN_POINT('Ctrl Pts',(0.0788908541853553,2.41250054176492,
10.7129068178719));
#41955=CARTESIAN_POINT('Ctrl Pts',(0.083301800030047,2.41132301602692,10.7126348525201));
#41956=CARTESIAN_POINT('Ctrl Pts',(0.0834814016268824,2.41127490386966,
10.7126237832735));
#41957=CARTESIAN_POINT('Ctrl Pts',(0.0961816200177723,2.40786095286697,
10.7118413478027));
#41958=CARTESIAN_POINT('Ctrl Pts',(0.108489056587662,2.40374242506058,10.7111039683175));
#41959=CARTESIAN_POINT('Ctrl Pts',(0.136685402817694,2.39237345193751,10.7093949101415));
#41960=CARTESIAN_POINT('Ctrl Pts',(0.152298840695882,2.38455261435712,10.7084317662239));
#41961=CARTESIAN_POINT('Ctrl Pts',(0.173493095747547,2.37169000430709,10.7070191853711));
#41962=CARTESIAN_POINT('Ctrl Pts',(0.179650255244757,2.36765853034723,10.7065952825656));
#41963=CARTESIAN_POINT('Ctrl Pts',(0.192441241305427,2.35864318358707,10.7056789730607));
#41964=CARTESIAN_POINT('Ctrl Pts',(0.19903128990327,2.35360689100153,10.705185030678));
#41965=CARTESIAN_POINT('Ctrl Pts',(0.206293111102138,2.34759970432696,10.7046119130088));
#41966=CARTESIAN_POINT('Ctrl Pts',(0.20716295721725,2.34687237669808,10.7045427759468));
#41967=CARTESIAN_POINT('Ctrl Pts',(0.208433989094991,2.34579814701021,10.7044410261721));
#41968=CARTESIAN_POINT('Ctrl Pts',(0.208838192253594,2.34545481526066,10.7044085598966));
#41969=CARTESIAN_POINT('Ctrl Pts',(0.209543567714831,2.3448526629359,10.7043517116932));
#41970=CARTESIAN_POINT('Ctrl Pts',(0.209845113349675,2.34459427981546,10.7043273478277));
#41971=CARTESIAN_POINT('Ctrl Pts',(0.210427878719988,2.34409305917469,10.704280142839));
#41972=CARTESIAN_POINT('Ctrl Pts',(0.210709157720643,2.3438502912254,10.7042573046161));
#41973=CARTESIAN_POINT('Ctrl Pts',(0.211376847838965,2.34327199944299,10.7042029627682));
#41974=CARTESIAN_POINT('Ctrl Pts',(0.211762879955846,2.3429360413428,10.7041714411327));
#41975=CARTESIAN_POINT('Ctrl Pts',(0.213126273336623,2.34174378116023,10.7040597447862));
#41976=CARTESIAN_POINT('Ctrl Pts',(0.214099244157049,2.34088249767896,10.7039793623865));
#41977=CARTESIAN_POINT('Ctrl Pts',(0.230671677884107,2.3260326854551,10.7025985633957));
#41978=CARTESIAN_POINT('Ctrl Pts',(0.244872459941179,2.31056440479508,10.7012322714636));
#41979=CARTESIAN_POINT('Ctrl Pts',(0.267782336255844,2.28013266425698,10.698677420583));
#41980=CARTESIAN_POINT('Ctrl Pts',(0.276984782086083,2.26563385157707,10.69750693796));
#41981=CARTESIAN_POINT('Ctrl Pts',(0.290155500838176,2.2406888498499,10.6956207521332));
#41982=CARTESIAN_POINT('Ctrl Pts',(0.294814341998062,2.2306450388883,10.6948927521361));
#41983=CARTESIAN_POINT('Ctrl Pts',(0.299520623389033,2.21895765766375,10.6940958083928));
#41984=CARTESIAN_POINT('Ctrl Pts',(0.300083396109276,2.21753077790015,10.6939993442869));
#41985=CARTESIAN_POINT('Ctrl Pts',(0.300783776247607,2.21571717201296,10.6938778374951));
#41986=CARTESIAN_POINT('Ctrl Pts',(0.300930849044591,2.2153341582108,10.6938522386131));
#41987=CARTESIAN_POINT('Ctrl Pts',(0.301165289484826,2.21472011610684,10.6938112993711));
#41988=CARTESIAN_POINT('Ctrl Pts',(0.301253123042089,2.21448926800543,10.6937959310524));
#41989=CARTESIAN_POINT('Ctrl Pts',(0.301418266577142,2.21405372451225,10.6937669786296));
#41990=CARTESIAN_POINT('Ctrl Pts',(0.301495632846599,2.21384905303181,10.6937533912328));
#41991=CARTESIAN_POINT('Ctrl Pts',(0.301671034769556,2.21338359680543,10.6937225319647));
#41992=CARTESIAN_POINT('Ctrl Pts',(0.301768940556282,2.21312276411232,10.6937052679955));
#41993=CARTESIAN_POINT('Ctrl Pts',(0.302065003905849,2.21233089647643,10.6936529428578));
#41994=CARTESIAN_POINT('Ctrl Pts',(0.302262100223842,2.21179946183977,10.6936179451481));
#41995=CARTESIAN_POINT('Ctrl Pts',(0.303640443295218,2.20805272009653,10.6933720182825));
#41996=CARTESIAN_POINT('Ctrl Pts',(0.304771819561358,2.20481912710627,10.6931639969605));
#41997=CARTESIAN_POINT('Ctrl Pts',(0.308988971208575,2.19212002273206,10.6923611950681));
#41998=CARTESIAN_POINT('Ctrl Pts',(0.311687299820541,2.1825308818715,10.6917853491847));
#41999=CARTESIAN_POINT('Ctrl Pts',(0.318786142613836,2.15193153154589,10.6899988111078));
#42000=CARTESIAN_POINT('Ctrl Pts',(0.32153568657827,2.13059965247486,10.6888241535609));
#42001=CARTESIAN_POINT('Ctrl Pts',(0.322550512340565,2.09487949536509,10.6867893455161));
#42002=CARTESIAN_POINT('Ctrl Pts',(0.322007000756692,2.08059723941255,10.6859586247012));
#42003=CARTESIAN_POINT('Ctrl Pts',(0.320357601281125,2.06486359599118,10.6850037512694));
#42004=CARTESIAN_POINT('Ctrl Pts',(0.320185589843294,2.06332920079406,10.6849102190718));
#42005=CARTESIAN_POINT('Ctrl Pts',(0.319865379692897,2.06064706297677,10.6847459802128));
#42006=CARTESIAN_POINT('Ctrl Pts',(0.319722011447954,2.05949876397645,10.6846754259583));
#42007=CARTESIAN_POINT('Ctrl Pts',(0.319503506014869,2.05782216241935,10.684572053971));
#42008=CARTESIAN_POINT('Ctrl Pts',(0.319433235232706,2.05729322580515,10.6845393899724));
#42009=CARTESIAN_POINT('Ctrl Pts',(0.319308305521555,2.05637042556133,10.6844823115127));
#42010=CARTESIAN_POINT('Ctrl Pts',(0.319254230489449,2.05597648295462,10.6844579155562));
#42011=CARTESIAN_POINT('Ctrl Pts',(0.319148337154954,2.05521549459697,10.6844107324549));
#42012=CARTESIAN_POINT('Ctrl Pts',(0.319096614363009,2.05484843598226,10.6843879483665));
#42013=CARTESIAN_POINT('Ctrl Pts',(0.318972449709663,2.05397815263709,10.6843338670379));
#42014=CARTESIAN_POINT('Ctrl Pts',(0.31889945025578,2.05347500961513,10.6843025521895));
#42015=CARTESIAN_POINT('Ctrl Pts',(0.318638513152496,2.05170599078855,10.6841922794232));
#42016=CARTESIAN_POINT('Ctrl Pts',(0.318444228085861,2.05044107636091,10.6841131207015));
#42017=CARTESIAN_POINT('Ctrl Pts',(0.315454607189546,2.03172059443509,10.682936914757));
#42018=CARTESIAN_POINT('Ctrl Pts',(0.311235719264727,2.01452588216347,10.6817937398494));
#42019=CARTESIAN_POINT('Ctrl Pts',(0.297965061485477,1.97485311257546,10.6790100413986));
#42020=CARTESIAN_POINT('Ctrl Pts',(0.287748941994135,1.95287628132012,10.6773465842651));
#42021=CARTESIAN_POINT('Ctrl Pts',(0.271159156558394,1.92566307328497,10.6752430291027));
#42022=CARTESIAN_POINT('Ctrl Pts',(0.266909354062832,1.91922369921736,10.6747423755288));
#42023=CARTESIAN_POINT('Ctrl Pts',(0.261712726710623,1.91193309486013,10.6741775670027));
#42024=CARTESIAN_POINT('Ctrl Pts',(0.260987420186091,1.91092784775599,10.6740997371059));
#42025=CARTESIAN_POINT('Ctrl Pts',(0.260031860263166,1.90961945448595,10.6739985257031));
#42026=CARTESIAN_POINT('Ctrl Pts',(0.259806857078832,1.90931251357122,10.6739747885978));
#42027=CARTESIAN_POINT('Ctrl Pts',(0.259438954608668,1.90881249477511,10.6739361314559));
#42028=CARTESIAN_POINT('Ctrl Pts',(0.259296383063203,1.90861917793623,10.6739211886853));
#42029=CARTESIAN_POINT('Ctrl Pts',(0.259022558868092,1.90824875954998,10.6738925622388));
#42030=CARTESIAN_POINT('Ctrl Pts',(0.258891341066005,1.90807163383708,10.6738788762628));
#42031=CARTESIAN_POINT('Ctrl Pts',(0.258589193275903,1.90766465016238,10.6738474354345));
#42032=CARTESIAN_POINT('Ctrl Pts',(0.258418137997655,1.90743488469717,10.6738296893832));
#42033=CARTESIAN_POINT('Ctrl Pts',(0.257887573750776,1.90672419846363,10.6737748107936));
#42034=CARTESIAN_POINT('Ctrl Pts',(0.25752702431116,1.90624405062624,10.6737377506899));
#42035=CARTESIAN_POINT('Ctrl Pts',(0.254545119754088,1.90229604168079,10.6734331351089));
#42036=CARTESIAN_POINT('Ctrl Pts',(0.251855031601444,1.89888033237553,10.6731702945455));
#42037=CARTESIAN_POINT('Ctrl Pts',(0.248965139386178,1.895359882096,10.6728989071326));
#42038=CARTESIAN_POINT('Ctrl Pts',(0.248833628196177,1.89519999032107,10.6728865801924));
#42039=CARTESIAN_POINT('Ctrl Pts',(0.247035462461752,1.89301806292881,10.6727183470089));
#42040=CARTESIAN_POINT('Ctrl Pts',(0.245344313343016,1.89101624302113,10.6725638084742));
#42041=CARTESIAN_POINT('Ctrl Pts',(0.225994854707848,1.86867086841682,10.6708336974255));
#42042=CARTESIAN_POINT('Ctrl Pts',(0.205875823633146,1.85059615837575,10.6693780503921));
#42043=CARTESIAN_POINT('Ctrl Pts',(0.171515019078687,1.82675064351744,10.6670012313608));
#42044=CARTESIAN_POINT('Ctrl Pts',(0.158718311161655,1.8191245379348,10.6661372540693));
#42045=CARTESIAN_POINT('Ctrl Pts',(0.143310313993249,1.81133231217202,10.6650954261186));
#42046=CARTESIAN_POINT('Ctrl Pts',(0.141167095034946,1.81027818360029,10.6649505077027));
#42047=CARTESIAN_POINT('Ctrl Pts',(0.138375351502392,1.80894341388019,10.6647616653035));
#42048=CARTESIAN_POINT('Ctrl Pts',(0.137737306751037,1.80864092850298,10.6647185011272));
#42049=CARTESIAN_POINT('Ctrl Pts',(0.136705890871401,1.80815609820774,10.6646487154176));
#42050=CARTESIAN_POINT('Ctrl Pts',(0.136313134433313,1.80797244480987,10.6646221392139));
#42051=CARTESIAN_POINT('Ctrl Pts',(0.135563242327533,1.80762363676797,10.6645713922998));
#42052=CARTESIAN_POINT('Ctrl Pts',(0.135206172209959,1.80745834238302,10.6645472264705));
#42053=CARTESIAN_POINT('Ctrl Pts',(0.134389815687101,1.80708224969276,10.6644919718286));
#42054=CARTESIAN_POINT('Ctrl Pts',(0.13393033521952,1.80687187731503,10.664460868409));
#42055=CARTESIAN_POINT('Ctrl Pts',(0.132521872648275,1.80623101800445,10.6643655133251));
#42056=CARTESIAN_POINT('Ctrl Pts',(0.131571302829227,1.80580405552783,10.6643011407628));
#42057=CARTESIAN_POINT('Ctrl Pts',(0.124491868373924,1.80266539616593,10.6638215685955));
#42058=CARTESIAN_POINT('Ctrl Pts',(0.118282214609934,1.80014103520548,10.6634000141291));
#42059=CARTESIAN_POINT('Ctrl Pts',(0.110169026472496,1.79713407427764,10.6628474968132));
#42060=CARTESIAN_POINT('Ctrl Pts',(0.108333221760304,1.79647257757789,10.6627223678306));
#42061=CARTESIAN_POINT('Ctrl Pts',(0.0784607091494834,1.78601412567791,
10.660684477829));
#42062=CARTESIAN_POINT('Ctrl Pts',(0.0492102102441535,1.78012347961877,
10.6586444317073));
#42063=CARTESIAN_POINT('Ctrl Pts',(0.00835778947718865,1.77763742442317,
10.6559062865581));
#42064=CARTESIAN_POINT('Ctrl Pts',(-0.00288948366096541,1.77754195451658,
10.6551662377923));
#42065=CARTESIAN_POINT('Ctrl Pts',(-0.0151435571886671,1.77807936038324,
10.6543902989268));
#42066=CARTESIAN_POINT('Ctrl Pts',(-0.016167020799385,1.77812913608182,
10.6543257256139));
#42067=CARTESIAN_POINT('Ctrl Pts',(-0.0179324322385133,1.77822343790756,
10.6542147633768));
#42068=CARTESIAN_POINT('Ctrl Pts',(-0.018674488473154,1.77826565066146,
10.6541682515068));
#42069=CARTESIAN_POINT('Ctrl Pts',(-0.0197271244150919,1.77832918520907,
10.6541024619283));
#42070=CARTESIAN_POINT('Ctrl Pts',(-0.0200378223479627,1.77834839001886,
10.6540830667695));
#42071=CARTESIAN_POINT('Ctrl Pts',(-0.0205718335789742,1.77838217498306,
10.6540497722085));
#42072=CARTESIAN_POINT('Ctrl Pts',(-0.0207951599992192,1.77839653760077,
10.6540358605166));
#42073=CARTESIAN_POINT('Ctrl Pts',(-0.0212231723529629,1.77842451172198,
10.6540092220555));
#42074=CARTESIAN_POINT('Ctrl Pts',(-0.0214278599319772,1.77843808601562,
10.6539964931844));
#42075=CARTESIAN_POINT('Ctrl Pts',(-0.0219105658856927,1.7784705606347,
10.6539664994505));
#42076=CARTESIAN_POINT('Ctrl Pts',(-0.0221885735159514,1.77848962616631,
10.6539492439355));
#42077=CARTESIAN_POINT('Ctrl Pts',(-0.0230113653269691,1.77854712482837,
10.6538982296592));
#42078=CARTESIAN_POINT('Ctrl Pts',(-0.0235560804115875,1.77858658245765,
10.653864528144));
#42079=CARTESIAN_POINT('Ctrl Pts',(-0.0283969981610894,1.77894961745865,
10.6535656363785));
#42080=CARTESIAN_POINT('Ctrl Pts',(-0.0326866629084256,1.77935795018307,
10.6533050917391));
#42081=CARTESIAN_POINT('Ctrl Pts',(-0.0371999536787768,1.77987909469105,
10.6530343071208));
#42082=CARTESIAN_POINT('Ctrl Pts',(-0.0374327802155412,1.77990623633773,
10.6530203475944));
#42083=CARTESIAN_POINT('Ctrl Pts',(-0.0377932934974776,1.77994866172931,
10.6529987466642));
#42084=CARTESIAN_POINT('Ctrl Pts',(-0.0379210005963382,1.77996376786914,
10.6529910975941));
#42085=CARTESIAN_POINT('Ctrl Pts',(-0.0394341395470693,1.78014367156438,
10.6529005000365));
#42086=CARTESIAN_POINT('Ctrl Pts',(-0.0408185170970988,1.78031739023526,
10.6528179351177));
#42087=CARTESIAN_POINT('Ctrl Pts',(-0.0739911911105266,1.78469906512859,
10.6508463323331));
#42088=CARTESIAN_POINT('Ctrl Pts',(-0.104978714780698,1.79361893231556,
10.6491381366845));
#42089=CARTESIAN_POINT('Ctrl Pts',(-0.144449100312507,1.81168743387289,
10.6466386064222));
#42090=CARTESIAN_POINT('Ctrl Pts',(-0.154499215229547,1.81694589126024,
10.6459724841665));
#42091=CARTESIAN_POINT('Ctrl Pts',(-0.165996547881922,1.82375655838926,
10.645164440796));
#42092=CARTESIAN_POINT('Ctrl Pts',(-0.1677325133804,1.82480716469213,10.6450411597027));
#42093=CARTESIAN_POINT('Ctrl Pts',(-0.170019579463829,1.82622097692943,
10.644876999074));
#42094=CARTESIAN_POINT('Ctrl Pts',(-0.170579677278318,1.82656959831804,
10.6448366566744));
#42095=CARTESIAN_POINT('Ctrl Pts',(-0.17149733033233,1.82714468954034,10.6447703289663));
#42096=CARTESIAN_POINT('Ctrl Pts',(-0.17185551879193,1.82737014944213,10.6447443810438));
#42097=CARTESIAN_POINT('Ctrl Pts',(-0.172548627551553,1.82780833190964,
10.644694057495));
#42098=CARTESIAN_POINT('Ctrl Pts',(-0.172883601350699,1.82802096876871,
10.6446696850796));
#42099=CARTESIAN_POINT('Ctrl Pts',(-0.173655975585981,1.82851326496984,
10.6446133683992));
#42100=CARTESIAN_POINT('Ctrl Pts',(-0.174093093761888,1.82879336318327,
10.6445814078448));
#42101=CARTESIAN_POINT('Ctrl Pts',(-0.175490378955381,1.8296934908691,10.6444789576728));
#42102=CARTESIAN_POINT('Ctrl Pts',(-0.17644791700731,1.83031756728649,10.6444083171237));
#42103=CARTESIAN_POINT('Ctrl Pts',(-0.185221654035153,1.83610259026258,
10.643757018908));
#42104=CARTESIAN_POINT('Ctrl Pts',(-0.192811980867188,1.84159641133959,
10.6431638111054));
#42105=CARTESIAN_POINT('Ctrl Pts',(-0.206178374068528,1.85218801574152,
10.6420618352222));
#42106=CARTESIAN_POINT('Ctrl Pts',(-0.212031769976707,1.8571773977429,10.641557348302));
#42107=CARTESIAN_POINT('Ctrl Pts',(-0.23299369306225,1.87638140299186,10.6396701529999));
#42108=CARTESIAN_POINT('Ctrl Pts',(-0.246898036763436,1.89183513913508,
10.6382508834874));
#42109=CARTESIAN_POINT('Ctrl Pts',(-0.266099788641974,1.9178293326402,10.636086655363));
#42110=CARTESIAN_POINT('Ctrl Pts',(-0.272473526524003,1.92750800428579,
10.6353232116672));
#42111=CARTESIAN_POINT('Ctrl Pts',(-0.279108542127127,1.93887245111991,
10.6344905536046));
#42112=CARTESIAN_POINT('Ctrl Pts',(-0.279894101009923,1.94024093841722,
10.6343912988104));
#42113=CARTESIAN_POINT('Ctrl Pts',(-0.280873484909639,1.94197647892662,
10.6342667492149));
#42114=CARTESIAN_POINT('Ctrl Pts',(-0.281076677249562,1.94233818075179,
10.6342408643287));
#42115=CARTESIAN_POINT('Ctrl Pts',(-0.281399310538288,1.94291510499665,
10.6341996936114));
#42116=CARTESIAN_POINT('Ctrl Pts',(-0.281519203475698,1.94313007208193,
10.6341843787205));
#42117=CARTESIAN_POINT('Ctrl Pts',(-0.281745284159368,1.94353652687675,
10.6341554704877));
#42118=CARTESIAN_POINT('Ctrl Pts',(-0.281851522159065,1.94372798387184,
10.6341418739827));
#42119=CARTESIAN_POINT('Ctrl Pts',(-0.282093176684477,1.94416453003825,
10.6341109186484));
#42120=CARTESIAN_POINT('Ctrl Pts',(-0.282228468728226,1.94440968709176,
10.6340935679099));
#42121=CARTESIAN_POINT('Ctrl Pts',(-0.282640045704719,1.94515779168168,
10.6340407219673));
#42122=CARTESIAN_POINT('Ctrl Pts',(-0.282915308897297,1.94566130453969,
10.634005292096));
#42123=CARTESIAN_POINT('Ctrl Pts',(-0.284891237555549,1.94929873249034,
10.6337503187314));
#42124=CARTESIAN_POINT('Ctrl Pts',(-0.286541217937032,1.95246009946763,
10.6335339297426));
#42125=CARTESIAN_POINT('Ctrl Pts',(-0.295789101613459,1.97091968191431,
10.6322965619018));
#42126=CARTESIAN_POINT('Ctrl Pts',(-0.302214540346773,1.98677705091995,
10.6313355261449));
#42127=CARTESIAN_POINT('Ctrl Pts',(-0.312263334152678,2.01864078124881,
10.629465696369));
#42128=CARTESIAN_POINT('Ctrl Pts',(-0.31598328516405,2.03456111486351,10.6285587985491));
#42129=CARTESIAN_POINT('Ctrl Pts',(-0.32037303737777,2.06291573048987,10.6269135315642));
#42130=CARTESIAN_POINT('Ctrl Pts',(-0.321559891740573,2.07523492808655,
10.6261893231636));
#42131=CARTESIAN_POINT('Ctrl Pts',(-0.322118447795861,2.08973037114639,
10.6253127410583));
#42132=CARTESIAN_POINT('Ctrl Pts',(-0.322179563960661,2.09187055286401,
10.6251827124183));
#42133=CARTESIAN_POINT('Ctrl Pts',(-0.32223186003238,2.09468424722614,10.6250109183032));
#42134=CARTESIAN_POINT('Ctrl Pts',(-0.322242261255481,2.09535738246266,
10.6249697555244));
#42135=CARTESIAN_POINT('Ctrl Pts',(-0.322255803055986,2.09645673960136,
10.6249024234368));
#42136=CARTESIAN_POINT('Ctrl Pts',(-0.322260207395294,2.09688294621664,
10.6248762937635));
#42137=CARTESIAN_POINT('Ctrl Pts',(-0.322267069478345,2.09770477124514,
10.624825859299));
#42138=CARTESIAN_POINT('Ctrl Pts',(-0.32226964426969,2.09810038812739,10.6248015582207));
#42139=CARTESIAN_POINT('Ctrl Pts',(-0.322273880357315,2.0990080855648,10.6247457500752));
#42140=CARTESIAN_POINT('Ctrl Pts',(-0.322275049623255,2.09952016637256,
10.6247142276505));
#42141=CARTESIAN_POINT('Ctrl Pts',(-0.322274887805991,2.10113743837012,
10.6246145509417));
#42142=CARTESIAN_POINT('Ctrl Pts',(-0.322269092092557,2.10224261220303,
10.624546257021));
#42143=CARTESIAN_POINT('Ctrl Pts',(-0.322101872276328,2.11833947907641,
10.6235488922284));
#42144=CARTESIAN_POINT('Ctrl Pts',(-0.320900231448132,2.13329980047741,
10.62258695804));
#42145=CARTESIAN_POINT('Ctrl Pts',(-0.316133179799011,2.16486808434016,
10.6204814041765));
#42146=CARTESIAN_POINT('Ctrl Pts',(-0.312287957371054,2.18138922386094,
10.6193332870512));
#42147=CARTESIAN_POINT('Ctrl Pts',(-0.303289733818903,2.2097283377801,10.617322755468));
#42148=CARTESIAN_POINT('Ctrl Pts',(-0.298693116954973,2.22168582585911,
10.6164613590884));
#42149=CARTESIAN_POINT('Ctrl Pts',(-0.293053731852387,2.23409464896252,
10.6155728443954));
#42150=CARTESIAN_POINT('Ctrl Pts',(-0.292707376819011,2.23484901265895,
10.6155188532204));
#42151=CARTESIAN_POINT('Ctrl Pts',(-0.29021861512046,2.24021478501449,10.6151350270138));
#42152=CARTESIAN_POINT('Ctrl Pts',(-0.287970100311195,2.24477658321316,
10.6148098210626));
#42153=CARTESIAN_POINT('Ctrl Pts',(-0.285320173614871,2.24984651363281,
10.6144512190946));
#42154=CARTESIAN_POINT('Ctrl Pts',(-0.285024265203572,2.25040860141961,
10.6144115017946));
#42155=CARTESIAN_POINT('Ctrl Pts',(-0.284591419897391,2.25122494084432,
10.6143538810633));
#42156=CARTESIAN_POINT('Ctrl Pts',(-0.284455802464262,2.25147988466644,
10.6143358948691));
#42157=CARTESIAN_POINT('Ctrl Pts',(-0.284215886085028,2.25192943912444,
10.6143041950273));
#42158=CARTESIAN_POINT('Ctrl Pts',(-0.284111729658993,2.25212412513184,
10.6142904722913));
#42159=CARTESIAN_POINT('Ctrl Pts',(-0.283894350902737,2.25252944087545,
10.6142619142993));
#42160=CARTESIAN_POINT('Ctrl Pts',(-0.283781094439752,2.25274005122342,
10.6142470813055));
#42161=CARTESIAN_POINT('Ctrl Pts',(-0.283485564342004,2.25328815204493,
10.6142084952888));
#42162=CARTESIAN_POINT('Ctrl Pts',(-0.283302921747109,2.25362544477016,
10.614184765834));
#42163=CARTESIAN_POINT('Ctrl Pts',(-0.282514127177264,2.25507594986013,
10.6140827833769));
#42164=CARTESIAN_POINT('Ctrl Pts',(-0.28190200207261,2.25618592648598,10.6140049066545));
#42165=CARTESIAN_POINT('Ctrl Pts',(-0.270885211488913,2.27588708081191,
10.6126250639713));
#42166=CARTESIAN_POINT('Ctrl Pts',(-0.258666983423515,2.2934082683905,10.6114342541627));
#42167=CARTESIAN_POINT('Ctrl Pts',(-0.230280174730862,2.32656366791077,
10.6089940764318));
#42168=CARTESIAN_POINT('Ctrl Pts',(-0.214031094273961,2.3419723542264,10.6077488458138));
#42169=CARTESIAN_POINT('Ctrl Pts',(-0.195078654313094,2.3565305939115,10.6063361835187));
#42170=CARTESIAN_POINT('Ctrl Pts',(-0.193830089353779,2.35747528681586,
10.6062433144724));
#42171=CARTESIAN_POINT('Ctrl Pts',(-0.188672568959996,2.36131880978429,
10.6058604076998));
#42172=CARTESIAN_POINT('Ctrl Pts',(-0.184705237869046,2.36413789928119,
10.6055675176712));
#42173=CARTESIAN_POINT('Ctrl Pts',(-0.179972230122461,2.36734227841042,
10.6052194089959));
#42174=CARTESIAN_POINT('Ctrl Pts',(-0.179266829279648,2.36781579740422,
10.6051675612142));
#42175=CARTESIAN_POINT('Ctrl Pts',(-0.178133045596116,2.36857039337862,
10.6050842774087));
#42176=CARTESIAN_POINT('Ctrl Pts',(-0.177705847259194,2.36885324989294,
10.6050529083604));
#42177=CARTESIAN_POINT('Ctrl Pts',(-0.176947551250084,2.36935273580443,
10.6049972463795));
#42178=CARTESIAN_POINT('Ctrl Pts',(-0.176616724968369,2.36956977693718,
10.6049729689409));
#42179=CARTESIAN_POINT('Ctrl Pts',(-0.175928790754885,2.37001929149389,
10.6049224985648));
#42180=CARTESIAN_POINT('Ctrl Pts',(-0.175571619964615,2.37025166688767,
10.604896302027));
#42181=CARTESIAN_POINT('Ctrl Pts',(-0.174649415671359,2.37084905339973,
10.60482868164));
#42182=CARTESIAN_POINT('Ctrl Pts',(-0.174083700411648,2.37121300367405,
10.604787218368));
#42183=CARTESIAN_POINT('Ctrl Pts',(-0.171716491882821,2.37272547833394,
10.6046137871584));
#42184=CARTESIAN_POINT('Ctrl Pts',(-0.169904772413769,2.37385782456362,
10.6044812212612));
#42185=CARTESIAN_POINT('Ctrl Pts',(-0.157566280887133,2.38139996513841,
10.6035793654261));
#42186=CARTESIAN_POINT('Ctrl Pts',(-0.146691831263112,2.38721858357531,
10.6027886524027));
#42187=CARTESIAN_POINT('Ctrl Pts',(-0.120714326350644,2.39925780171569,
10.6009084360497));
#42188=CARTESIAN_POINT('Ctrl Pts',(-0.105418495876552,2.40498202632303,
10.5998069942132));
#42189=CARTESIAN_POINT('Ctrl Pts',(-0.0706824252419293,2.41505490133353,
10.5973595269109));
#42190=CARTESIAN_POINT('Ctrl Pts',(-0.0511353081470509,2.41881181000973,
10.5960171592826));
#42191=CARTESIAN_POINT('Ctrl Pts',(-0.0301904195768933,2.42085994815445,
10.594690072508));
#42192=CARTESIAN_POINT('Ctrl Pts',(-0.0290154878773678,2.42096833072649,
10.5946160029913));
#42193=CARTESIAN_POINT('Ctrl Pts',(-0.0274533135494249,2.42110378668643,
10.594518043206));
#42194=CARTESIAN_POINT('Ctrl Pts',(-0.0270665983569622,2.42113661501977,
10.5944938358132));
#42195=CARTESIAN_POINT('Ctrl Pts',(-0.0264643920446245,2.42118664092582,
10.594456206358));
#42196=CARTESIAN_POINT('Ctrl Pts',(-0.0262489429777537,2.42120432025226,
10.5944427571859));
#42197=CARTESIAN_POINT('Ctrl Pts',(-0.0258373323102506,2.42123767931074,
10.5944170886015));
#42198=CARTESIAN_POINT('Ctrl Pts',(-0.0256411754988713,2.42125339604306,
10.5944048672057));
#42199=CARTESIAN_POINT('Ctrl Pts',(-0.0251792841491755,2.42128997856143,
10.5943761156927));
#42200=CARTESIAN_POINT('Ctrl Pts',(-0.0249135384118099,2.42131069431207,
10.5943595941566));
#42201=CARTESIAN_POINT('Ctrl Pts',(-0.0241409223233759,2.42136995798687,
10.5943116188553));
#42202=CARTESIAN_POINT('Ctrl Pts',(-0.0236339831433821,2.42140763661781,
10.5942802139651));
#42203=CARTESIAN_POINT('Ctrl Pts',(-0.0200708746813913,2.42166399172676,
10.5940599811173));
#42204=CARTESIAN_POINT('Ctrl Pts',(-0.017011680900007,2.4218402833017,10.5938734883344));
#42205=CARTESIAN_POINT('Ctrl Pts',(-0.00765904737650977,2.42224551019416,
10.5933099911903));
#42206=CARTESIAN_POINT('Ctrl Pts',(-0.00136071564873546,2.42233366108226,
10.5929396977314));
#42207=CARTESIAN_POINT('Ctrl Pts',(0.0336364142372838,2.42179751739353,
10.5909134702201));
#42208=CARTESIAN_POINT('Ctrl Pts',(0.0621499220440724,2.41752587772587,
10.5893682522793));
#42209=CARTESIAN_POINT('Ctrl Pts',(0.095190739864799,2.40794855632652,10.5873889479673));
#42210=CARTESIAN_POINT('Ctrl Pts',(0.100615844160285,2.40621893677704,10.5870580450734));
#42211=CARTESIAN_POINT('Ctrl Pts',(0.112766068418738,2.4019874858033,10.5863006353681));
#42212=CARTESIAN_POINT('Ctrl Pts',(0.119458951637307,2.39940303035856,10.5858718325772));
#42213=CARTESIAN_POINT('Ctrl Pts',(0.127037746239446,2.39618189693642,10.5853707473604));
#42214=CARTESIAN_POINT('Ctrl Pts',(0.12801374092245,2.39576136856441,10.5853059182461));
#42215=CARTESIAN_POINT('Ctrl Pts',(0.12945447431168,2.39513213011022,10.5852097691087));
#42216=CARTESIAN_POINT('Ctrl Pts',(0.129920833710825,2.3949271301625,10.5851785759291));
#42217=CARTESIAN_POINT('Ctrl Pts',(0.130747017803886,2.39456162037406,10.5851231900771));
#42218=CARTESIAN_POINT('Ctrl Pts',(0.131107038721515,2.39440155444136,10.5850990126554));
#42219=CARTESIAN_POINT('Ctrl Pts',(0.131860726772466,2.39406480671901,10.5850483092035));
#42220=CARTESIAN_POINT('Ctrl Pts',(0.132254334155832,2.39388799381697,10.5850217787077));
#42221=CARTESIAN_POINT('Ctrl Pts',(0.133282653787309,2.3934235767643,10.5849523322017));
#42222=CARTESIAN_POINT('Ctrl Pts',(0.133916787902301,2.39313470471352,10.5849093726236));
#42223=CARTESIAN_POINT('Ctrl Pts',(0.136641973021836,2.39188259140979,10.5847241725702));
#42224=CARTESIAN_POINT('Ctrl Pts',(0.138723564965764,2.39089903410002,10.5845812320817));
#42225=CARTESIAN_POINT('Ctrl Pts',(0.153393941048295,2.38377397492711,10.5835631032709));
#42226=CARTESIAN_POINT('Ctrl Pts',(0.165579396523631,2.37684063854556,10.5826600642274));
#42227=CARTESIAN_POINT('Ctrl Pts',(0.201385022007874,2.35325639864308,10.5798267934464));
#42228=CARTESIAN_POINT('Ctrl Pts',(0.223250001140489,2.33420923502168,10.5778247748898));
#42229=CARTESIAN_POINT('Ctrl Pts',(0.242545427619116,2.31220991204856,10.5759144852643));
#42230=CARTESIAN_POINT('Ctrl Pts',(0.242804994717016,2.31191287307241,10.5758887599422));
#42231=CARTESIAN_POINT('Ctrl Pts',(0.246848734076133,2.30726818401922,10.5754875684628));
#42232=CARTESIAN_POINT('Ctrl Pts',(0.250516448660152,2.30281991238011,10.5751178834493));
#42233=CARTESIAN_POINT('Ctrl Pts',(0.25446721754494,2.29775753388324,10.5747152442235));
#42234=CARTESIAN_POINT('Ctrl Pts',(0.25486972589158,2.29723851006993,10.5746741697713));
#42235=CARTESIAN_POINT('Ctrl Pts',(0.255449341274268,2.29648637450622,10.5746149495273));
#42236=CARTESIAN_POINT('Ctrl Pts',(0.255627718487173,2.29625425056984,10.5745967144107));
#42237=CARTESIAN_POINT('Ctrl Pts',(0.255940473772509,2.29584610935328,10.5745647249529));
#42238=CARTESIAN_POINT('Ctrl Pts',(0.256074986949946,2.29567019630872,10.5745509609879));
#42239=CARTESIAN_POINT('Ctrl Pts',(0.256353339706178,2.29530539473941,10.5745224673296));
#42240=CARTESIAN_POINT('Ctrl Pts',(0.256497151634962,2.29511648622516,10.5745077396035));
#42241=CARTESIAN_POINT('Ctrl Pts',(0.256863539178482,2.29463410167027,10.5744702012048));
#42242=CARTESIAN_POINT('Ctrl Pts',(0.257085821427088,2.29434040165818,10.5744474113197));
#42243=CARTESIAN_POINT('Ctrl Pts',(0.257991893972917,2.29313893927685,10.5743544467344));
#42244=CARTESIAN_POINT('Ctrl Pts',(0.258671394440155,2.29222792983773,10.5742845703029));
#42245=CARTESIAN_POINT('Ctrl Pts',(0.263310484633149,2.28593913735411,10.5738062662536));
#42246=CARTESIAN_POINT('Ctrl Pts',(0.267107221845943,2.28044256921731,10.5734085171922));
#42247=CARTESIAN_POINT('Ctrl Pts',(0.274541894537162,2.2689298065942,10.5726074331073));
#42248=CARTESIAN_POINT('Ctrl Pts',(0.278159303437135,2.26290470701461,10.5722050891743));
#42249=CARTESIAN_POINT('Ctrl Pts',(0.291810712716592,2.23838455480655,10.5706148842395));
#42250=CARTESIAN_POINT('Ctrl Pts',(0.300219878349783,2.21904548873031,10.569461277327));
#42251=CARTESIAN_POINT('Ctrl Pts',(0.311284802758755,2.18477681716413,10.5674062770849));
#42252=CARTESIAN_POINT('Ctrl Pts',(0.314886195136794,2.17022769700975,10.5665314504221));
#42253=CARTESIAN_POINT('Ctrl Pts',(0.317677709120912,2.15425496251369,10.565546258926));
#42254=CARTESIAN_POINT('Ctrl Pts',(0.317885075620312,2.15302646942378,10.5654703384502));
#42255=CARTESIAN_POINT('Ctrl Pts',(0.318166089919634,2.15130075490805,10.5653634730838));
#42256=CARTESIAN_POINT('Ctrl Pts',(0.318245707636989,2.15080450565649,10.5653327176017));
#42257=CARTESIAN_POINT('Ctrl Pts',(0.318381794601162,2.14994341586929,10.565279306535));
#42258=CARTESIAN_POINT('Ctrl Pts',(0.318438798537131,2.14957865978964,10.5652566679368));
#42259=CARTESIAN_POINT('Ctrl Pts',(0.318556050739551,2.14881984305812,10.5652095429882));
#42260=CARTESIAN_POINT('Ctrl Pts',(0.318616194840782,2.14842576712818,10.5651850533784));
#42261=CARTESIAN_POINT('Ctrl Pts',(0.318756017143791,2.14749808672523,10.5651273645859));
#42262=CARTESIAN_POINT('Ctrl Pts',(0.318835086673455,2.14696439298249,10.565094146193));
#42263=CARTESIAN_POINT('Ctrl Pts',(0.319084133879111,2.14525378604073,10.5649875760334));
#42264=CARTESIAN_POINT('Ctrl Pts',(0.319248936517816,2.144076139984,10.5649140608115));
#42265=CARTESIAN_POINT('Ctrl Pts',(0.319619739695642,2.14131521275585,10.5647413505592));
#42266=CARTESIAN_POINT('Ctrl Pts',(0.319820497828673,2.13973127016687,10.5646419915434));
#42267=CARTESIAN_POINT('Ctrl Pts',(0.321799984932654,2.12312518055891,10.5635973333809));
#42268=CARTESIAN_POINT('Ctrl Pts',(0.322530461533653,2.10799925431078,10.562618927519));
#42269=CARTESIAN_POINT('Ctrl Pts',(0.321708972110891,2.07082628030248,10.5601524719535));
#42270=CARTESIAN_POINT('Ctrl Pts',(0.318958807320579,2.04888302401824,10.5586401747953));
#42271=CARTESIAN_POINT('Ctrl Pts',(0.313075447295526,2.02344018879822,10.5568965820186));
#42272=CARTESIAN_POINT('Ctrl Pts',(0.312086665109935,2.01950431042533,10.5566273229405));
#42273=CARTESIAN_POINT('Ctrl Pts',(0.310772070619766,2.0146605641952,10.5562973093378));
#42274=CARTESIAN_POINT('Ctrl Pts',(0.310516205919494,2.01373421838026,10.5562342575917));
#42275=CARTESIAN_POINT('Ctrl Pts',(0.31007843366465,2.01217647056235,10.5561283486323));
#42276=CARTESIAN_POINT('Ctrl Pts',(0.309898733082624,2.01154445979593,10.5560854122902));
#42277=CARTESIAN_POINT('Ctrl Pts',(0.309582155672909,2.01044385661525,10.5560107043556));
#42278=CARTESIAN_POINT('Ctrl Pts',(0.309446145197896,2.00997501926407,10.5559788999947));
#42279=CARTESIAN_POINT('Ctrl Pts',(0.309213486176365,2.00917978493676,10.5559249897273));
#42280=CARTESIAN_POINT('Ctrl Pts',(0.309117385196703,2.0088532300715,10.5559028622814));
#42281=CARTESIAN_POINT('Ctrl Pts',(0.308986956979781,2.00841260878144,10.555873020056));
#42282=CARTESIAN_POINT('Ctrl Pts',(0.308953083959704,2.00829840936104,10.5558652869088));
#42283=CARTESIAN_POINT('Ctrl Pts',(0.308563903481817,2.00698899051464,10.5557766332601));
#42284=CARTESIAN_POINT('Ctrl Pts',(0.308201720128999,2.00579580570652,10.5556959942204));
#42285=CARTESIAN_POINT('Ctrl Pts',(0.306670808935692,2.00085568214609,10.5553628113027));
#42286=CARTESIAN_POINT('Ctrl Pts',(0.305440544302357,1.99712795249222,10.5551130357275));
#42287=CARTESIAN_POINT('Ctrl Pts',(0.303947183381552,1.99286628043021,10.554830121659));
#42288=CARTESIAN_POINT('Ctrl Pts',(0.303750417245472,1.99230966528624,10.5547932226244));
#42289=CARTESIAN_POINT('Ctrl Pts',(0.303456971511172,1.99148676433291,10.5547387517394));
#42290=CARTESIAN_POINT('Ctrl Pts',(0.30336146995417,1.99122006424714,10.554721110437));
#42291=CARTESIAN_POINT('Ctrl Pts',(0.303191399953817,1.99074708823794,10.5546898474431));
#42292=CARTESIAN_POINT('Ctrl Pts',(0.303116972585147,1.99054076253522,10.5546762173379));
#42293=CARTESIAN_POINT('Ctrl Pts',(0.302959213473314,1.99010482147521,10.5546474350154));
#42294=CARTESIAN_POINT('Ctrl Pts',(0.302875831530322,1.98987522546161,10.5546322858942));
#42295=CARTESIAN_POINT('Ctrl Pts',(0.302655786487334,1.98927146163625,10.5545924732672));
#42296=CARTESIAN_POINT('Ctrl Pts',(0.302518690019417,1.98889745054488,10.5545678356814));
#42297=CARTESIAN_POINT('Ctrl Pts',(0.301892668864792,1.98719936021826,10.5544560852029));
#42298=CARTESIAN_POINT('Ctrl Pts',(0.30139573267332,1.98587822141475,10.5543694443169));
#42299=CARTESIAN_POINT('Ctrl Pts',(0.300046290324357,1.98236093844937,10.5541394808833));
#42300=CARTESIAN_POINT('Ctrl Pts',(0.299178340854831,1.98017076224843,10.5539970189566));
#42301=CARTESIAN_POINT('Ctrl Pts',(0.294929597163461,1.96978354019558,10.5533239896147));
#42302=CARTESIAN_POINT('Ctrl Pts',(0.291235219924701,1.96171816118037,10.5528091740582));
#42303=CARTESIAN_POINT('Ctrl Pts',(0.279803782528578,1.93925861825843,10.5513703368679));
#42304=CARTESIAN_POINT('Ctrl Pts',(0.27129888416226,1.92528621808786,10.5504678513984));
#42305=CARTESIAN_POINT('Ctrl Pts',(0.24911055958682,1.89438818792162,10.5483326841923));
#42306=CARTESIAN_POINT('Ctrl Pts',(0.234703613114626,1.87808494617109,10.5470916570029));
#42307=CARTESIAN_POINT('Ctrl Pts',(0.217792534424859,1.86245135971162,10.5456931832354));
#42308=CARTESIAN_POINT('Ctrl Pts',(0.216810342469333,1.86155457674852,10.5456121670436));
#42309=CARTESIAN_POINT('Ctrl Pts',(0.215438789395028,1.86031777120266,10.5454993079632));
#42310=CARTESIAN_POINT('Ctrl Pts',(0.215054109500165,1.85997255832002,10.5454676839457));
#42311=CARTESIAN_POINT('Ctrl Pts',(0.214390468380293,1.85937988082783,10.5454131769422));
#42312=CARTESIAN_POINT('Ctrl Pts',(0.214111904214357,1.85913197149775,10.5453903126606));
#42313=CARTESIAN_POINT('Ctrl Pts',(0.21353637839345,1.85862156720664,10.5453431048006));
#42314=CARTESIAN_POINT('Ctrl Pts',(0.213239361619447,1.85835913555627,10.5453187586313));
#42315=CARTESIAN_POINT('Ctrl Pts',(0.212547360771013,1.85774998187117,10.5452620746047));
#42316=CARTESIAN_POINT('Ctrl Pts',(0.212152011984379,1.85740367756311,10.5452297194353));
#42317=CARTESIAN_POINT('Ctrl Pts',(0.21091961347521,1.85632947908972,10.5451289495501));
#42318=CARTESIAN_POINT('Ctrl Pts',(0.210079658207441,1.85560494426572,10.5450603959269));
#42319=CARTESIAN_POINT('Ctrl Pts',(0.202601837551441,1.84922170495013,10.5444511773602));
#42320=CARTESIAN_POINT('Ctrl Pts',(0.19574109711567,1.84383080405913,10.5438996492481));
#42321=CARTESIAN_POINT('Ctrl Pts',(0.182445252792877,1.834229665401,10.5428428548966));
#42322=CARTESIAN_POINT('Ctrl Pts',(0.17606154320618,1.82995841072312,10.5423403043375));
#42323=CARTESIAN_POINT('Ctrl Pts',(0.154077303472251,1.81636012076571,10.5406277681789));
#42324=CARTESIAN_POINT('Ctrl Pts',(0.137842674218888,1.8081255148071,10.5393904728125));
#42325=CARTESIAN_POINT('Ctrl Pts',(0.106504061008595,1.79543021926908,10.5371108478022));
#42326=CARTESIAN_POINT('Ctrl Pts',(0.0915954623321869,1.79061953914345,
10.5360690606917));
#42327=CARTESIAN_POINT('Ctrl Pts',(0.075517958927093,1.78669658828385,10.5350283790326));
#42328=CARTESIAN_POINT('Ctrl Pts',(0.0746403921908587,1.78648636104104,
10.5349718332031));
#42329=CARTESIAN_POINT('Ctrl Pts',(0.0734573570829739,1.78620820562718,
10.5348959628036));
#42330=CARTESIAN_POINT('Ctrl Pts',(0.0731526667984573,1.78613703489003,
10.5348764543548));
#42331=CARTESIAN_POINT('Ctrl Pts',(0.0726390404861891,1.78601784862661,
10.5348436227112));
#42332=CARTESIAN_POINT('Ctrl Pts',(0.0724301601614801,1.78596959783579,
10.5348302859608));
#42333=CARTESIAN_POINT('Ctrl Pts',(0.0720290773354552,1.7858773702539,10.534804706592));
#42334=CARTESIAN_POINT('Ctrl Pts',(0.0718368840411786,1.78583336174587,
10.5347924622396));
#42335=CARTESIAN_POINT('Ctrl Pts',(0.071439914866234,1.78574284688465,10.534767198483));
#42336=CARTESIAN_POINT('Ctrl Pts',(0.0712351345868771,1.78569636444793,
10.5347541805086));
#42337=CARTESIAN_POINT('Ctrl Pts',(0.0707724429555244,1.78559181494002,
10.5347247996032));
#42338=CARTESIAN_POINT('Ctrl Pts',(0.0705145048948518,1.78553386491512,
10.5347084434182));
#42339=CARTESIAN_POINT('Ctrl Pts',(0.0693220148394745,1.78526749340417,
10.5346329305535));
#42340=CARTESIAN_POINT('Ctrl Pts',(0.068386595416225,1.78506291728116,10.5345739927676));
#42341=CARTESIAN_POINT('Ctrl Pts',(0.0591054079231446,1.78307642386444,
10.533992025009));
#42342=CARTESIAN_POINT('Ctrl Pts',(0.0506920417893542,1.78162231783749,
10.5334869485133));
#42343=CARTESIAN_POINT('Ctrl Pts',(0.0278578942360343,1.77860416692022,
10.5321524706262));
#42344=CARTESIAN_POINT('Ctrl Pts',(0.013372957283202,1.77767630779857,10.531344018866));
#42345=CARTESIAN_POINT('Ctrl Pts',(-0.0275380678385514,1.77781925070106,
10.5290573279285));
#42346=CARTESIAN_POINT('Ctrl Pts',(-0.0538341553457881,1.78115771537185,
10.5275746766322));
#42347=CARTESIAN_POINT('Ctrl Pts',(-0.0809851227926357,1.78806223254299,
10.5258766317182));
#42348=CARTESIAN_POINT('Ctrl Pts',(-0.0825403888697342,1.78847015401542,
10.5257788067047));
#42349=CARTESIAN_POINT('Ctrl Pts',(-0.0846932386512311,1.78905206515365,
10.5256425980039));
#42350=CARTESIAN_POINT('Ctrl Pts',(-0.0852934866823589,1.7892161780603,
10.5256045347661));
#42351=CARTESIAN_POINT('Ctrl Pts',(-0.0862532940489387,1.7894815876104,
10.5255435317106));
#42352=CARTESIAN_POINT('Ctrl Pts',(-0.0866131611832705,1.78958177328774,
10.5255206280355));
#42353=CARTESIAN_POINT('Ctrl Pts',(-0.087354164912857,1.78978945485657,
10.5254734019636));
#42354=CARTESIAN_POINT('Ctrl Pts',(-0.08773527906754,1.78989702798817,10.5254490770859));
#42355=CARTESIAN_POINT('Ctrl Pts',(-0.0886196317688793,1.79014840581414,
10.5253925497597));
#42356=CARTESIAN_POINT('Ctrl Pts',(-0.0891227191391028,1.79029273421104,
10.525360330295));
#42357=CARTESIAN_POINT('Ctrl Pts',(-0.0901741305228367,1.79059714271747,
10.5252928627609));
#42358=CARTESIAN_POINT('Ctrl Pts',(-0.0907223845407319,1.7907574562796,
10.5252576071557));
#42359=CARTESIAN_POINT('Ctrl Pts',(-0.0944597070016526,1.79186107132695,
10.5250167625057));
#42360=CARTESIAN_POINT('Ctrl Pts',(-0.0976343366093973,1.79285220073833,
10.5248096142726));
#42361=CARTESIAN_POINT('Ctrl Pts',(-0.106445393299578,1.79575344237772,
10.5242272700972));
#42362=CARTESIAN_POINT('Ctrl Pts',(-0.112044860295305,1.79777073045438,
10.523848611848));
#42363=CARTESIAN_POINT('Ctrl Pts',(-0.129604033082161,1.80465171211856,
10.5226332916566));
#42364=CARTESIAN_POINT('Ctrl Pts',(-0.141327994616978,1.81007905776409,
10.5217793971582));
#42365=CARTESIAN_POINT('Ctrl Pts',(-0.161938767634362,1.82116811827667,
10.5202083379808));
#42366=CARTESIAN_POINT('Ctrl Pts',(-0.170934887300376,1.82659071321151,
10.5194964845861));
#42367=CARTESIAN_POINT('Ctrl Pts',(-0.191661696099379,1.84050762106991,
10.5178086440866));
#42368=CARTESIAN_POINT('Ctrl Pts',(-0.203117712482278,1.84937324099307,
10.5168361074261));
#42369=CARTESIAN_POINT('Ctrl Pts',(-0.216977054017489,1.86167537853919,
10.5156411938572));
#42370=CARTESIAN_POINT('Ctrl Pts',(-0.219963097604545,1.86442855296617,
10.515382606792));
#42371=CARTESIAN_POINT('Ctrl Pts',(-0.223284232364362,1.86760891701959,
10.5150944976478));
#42372=CARTESIAN_POINT('Ctrl Pts',(-0.22367107175575,1.86798121726714,10.5150609313825));
#42373=CARTESIAN_POINT('Ctrl Pts',(-0.224255567306875,1.86854656518548,
10.5150102049987));
#42374=CARTESIAN_POINT('Ctrl Pts',(-0.224453906178619,1.86873890089742,
10.514992990197));
#42375=CARTESIAN_POINT('Ctrl Pts',(-0.22479864712963,1.86907406878476,10.5149630659779));
#42376=CARTESIAN_POINT('Ctrl Pts',(-0.224945160625977,1.86921678533643,
10.5149503475301));
#42377=CARTESIAN_POINT('Ctrl Pts',(-0.225252079722071,1.86951632047462,
10.514923703264));
#42378=CARTESIAN_POINT('Ctrl Pts',(-0.2254124574173,1.86967316702536,10.5149097797504));
#42379=CARTESIAN_POINT('Ctrl Pts',(-0.225732110340787,1.86998643556904,
10.5148820265226));
#42380=CARTESIAN_POINT('Ctrl Pts',(-0.225891387297782,1.87014285608982,
10.5148681966655));
#42381=CARTESIAN_POINT('Ctrl Pts',(-0.226266301135242,1.87051181236128,
10.5148356406512));
#42382=CARTESIAN_POINT('Ctrl Pts',(-0.226481801758825,1.87072448720158,
10.51481692539));
#42383=CARTESIAN_POINT('Ctrl Pts',(-0.227791668892591,1.87202082732957,
10.5147031543778));
#42384=CARTESIAN_POINT('Ctrl Pts',(-0.228878580045845,1.87311204658134,
10.5146086850561));
#42385=CARTESIAN_POINT('Ctrl Pts',(-0.238322141041879,1.88272996201918,
10.5137868732515));
#42386=CARTESIAN_POINT('Ctrl Pts',(-0.246207834619344,1.89170817784276,
10.5130934479709));
#42387=CARTESIAN_POINT('Ctrl Pts',(-0.258428329101278,1.90728844259288,
10.5119666122913));
#42388=CARTESIAN_POINT('Ctrl Pts',(-0.263051139700552,1.91364804661381,
10.5115257644934));
#42389=CARTESIAN_POINT('Ctrl Pts',(-0.272793876415334,1.92813714314506,
10.5105489647993));
#42390=CARTESIAN_POINT('Ctrl Pts',(-0.277792130959398,1.93633916329057,
10.5100140008736));
#42391=CARTESIAN_POINT('Ctrl Pts',(-0.29193191614421,1.9620613018615,10.5083603983596));
#42392=CARTESIAN_POINT('Ctrl Pts',(-0.299834191301724,1.98020596888851,
10.507223475659));
#42393=CARTESIAN_POINT('Ctrl Pts',(-0.30643168634884,2.00018780500769,10.5059453785795));
#42394=CARTESIAN_POINT('Ctrl Pts',(-0.306830285453337,2.0014199385275,10.5058664820753));
#42395=CARTESIAN_POINT('Ctrl Pts',(-0.307375796135252,2.00314156359891,
10.5057561119614));
#42396=CARTESIAN_POINT('Ctrl Pts',(-0.307528989687556,2.003629064294,10.5057248447093));
#42397=CARTESIAN_POINT('Ctrl Pts',(-0.30779150984991,2.00447147023506,10.5056707887805));
#42398=CARTESIAN_POINT('Ctrl Pts',(-0.307901383990714,2.00482620492242,
10.5056480180975));
#42399=CARTESIAN_POINT('Ctrl Pts',(-0.308127513809282,2.00556076745532,
10.5056008493205));
#42400=CARTESIAN_POINT('Ctrl Pts',(-0.308243680835297,2.00594062177102,
10.5055764483671));
#42401=CARTESIAN_POINT('Ctrl Pts',(-0.308513512481653,2.00682881207109,
10.5055193711379));
#42402=CARTESIAN_POINT('Ctrl Pts',(-0.308666623148082,2.00733731391317,
10.505486676808));
#42403=CARTESIAN_POINT('Ctrl Pts',(-0.308984852165373,2.00840373753051,
10.5054180745856));
#42404=CARTESIAN_POINT('Ctrl Pts',(-0.309149717700978,2.00896173219829,
10.5053821585542));
#42405=CARTESIAN_POINT('Ctrl Pts',(-0.309588072645398,2.01046028618344,
10.5052856453655));
#42406=CARTESIAN_POINT('Ctrl Pts',(-0.309858784942062,2.01140164541683,
10.5052249578356));
#42407=CARTESIAN_POINT('Ctrl Pts',(-0.310673289159565,2.01428335237103,
10.5050389893905));
#42408=CARTESIAN_POINT('Ctrl Pts',(-0.31120316940756,2.0162275502832,10.5049132583973));
#42409=CARTESIAN_POINT('Ctrl Pts',(-0.313069312008367,2.02333681113125,
10.5044524816794));
#42410=CARTESIAN_POINT('Ctrl Pts',(-0.314295436241986,2.02852964265951,
10.5041139380964));
#42411=CARTESIAN_POINT('Ctrl Pts',(-0.319988664784006,2.0556331378746,10.5023360342051));
#42412=CARTESIAN_POINT('Ctrl Pts',(-0.32229453126736,2.07793112920496,10.500830560742));
#42413=CARTESIAN_POINT('Ctrl Pts',(-0.322274875394328,2.10028339825448,
10.4993179956939));
#42414=CARTESIAN_POINT('',(-0.322700899340442,2.0998332352938,10.3743773449273));
#42415=CARTESIAN_POINT('Ctrl Pts',(-0.322700899340442,2.0998332352938,10.3743773449273));
#42416=CARTESIAN_POINT('Ctrl Pts',(-0.322760860387383,2.0903049967056,10.3749677204787));
#42417=CARTESIAN_POINT('Ctrl Pts',(-0.318052407360913,1.97393915136881,
10.3821815438711));
#42418=CARTESIAN_POINT('Ctrl Pts',(-0.176976240170584,1.76251740973093,
10.3960188151044));
#42419=CARTESIAN_POINT('Ctrl Pts',(0.187960967754062,1.7685097845779,10.4158891586272));
#42420=CARTESIAN_POINT('Ctrl Pts',(0.38046957633948,2.07859930375687,10.43575950215));
#42421=CARTESIAN_POINT('Ctrl Pts',(0.223949144889084,2.4083210482972,10.4556298456727));
#42422=CARTESIAN_POINT('Ctrl Pts',(-0.138014139074013,2.45520020514535,
10.4755001891955));
#42423=CARTESIAN_POINT('Ctrl Pts',(-0.310736422666012,2.2504699430552,10.4900826889471));
#42424=CARTESIAN_POINT('Ctrl Pts',(-0.322577931129815,2.12189942032013,
10.4980417408576));
#42425=CARTESIAN_POINT('Ctrl Pts',(-0.322378175270278,2.10028753889625,
10.4993773449273));
#42426=CARTESIAN_POINT('',(-0.322274890758155,2.1002653522546,10.1245441658164));
#42427=CARTESIAN_POINT('Ctrl Pts',(-0.322274949351636,2.09981931961724,
10.3741325730749));
#42428=CARTESIAN_POINT('Ctrl Pts',(-0.32228888357138,2.12467342881166,10.3726881081679));
#42429=CARTESIAN_POINT('Ctrl Pts',(-0.319427720275429,2.14944844835512,
10.3713381024607));
#42430=CARTESIAN_POINT('Ctrl Pts',(-0.310180543568759,2.18884054883889,
10.3690438376053));
#42431=CARTESIAN_POINT('Ctrl Pts',(-0.305516975523145,2.203749193326,10.3681401976533));
#42432=CARTESIAN_POINT('Ctrl Pts',(-0.298888071275734,2.22055361361139,
10.3670506232369));
#42433=CARTESIAN_POINT('Ctrl Pts',(-0.297957186028004,2.22283634510533,
10.366901076289));
#42434=CARTESIAN_POINT('Ctrl Pts',(-0.29672498390221,2.22576152928336,10.3667073754916));
#42435=CARTESIAN_POINT('Ctrl Pts',(-0.296447590535905,2.22641401968239,
10.3666640354162));
#42436=CARTESIAN_POINT('Ctrl Pts',(-0.29599684421038,2.22746463192364,10.3665940339328));
#42437=CARTESIAN_POINT('Ctrl Pts',(-0.295824834774944,2.22786333055801,
10.366567418369));
#42438=CARTESIAN_POINT('Ctrl Pts',(-0.295495483213476,2.22862250863517,
10.3665166416145));
#42439=CARTESIAN_POINT('Ctrl Pts',(-0.295338285794573,2.22898305031636,
10.3664924854043));
#42440=CARTESIAN_POINT('Ctrl Pts',(-0.29497810100415,2.22980504495677,10.36643731608));
#42441=CARTESIAN_POINT('Ctrl Pts',(-0.294774690477397,2.2302663103707,10.3664062885217));
#42442=CARTESIAN_POINT('Ctrl Pts',(-0.294150004752996,2.23167392827167,
10.3663113910337));
#42443=CARTESIAN_POINT('Ctrl Pts',(-0.293725251432721,2.23261872157932,
10.3662474018934));
#42444=CARTESIAN_POINT('Ctrl Pts',(-0.290574359519416,2.23953796292447,
10.3657765898293));
#42445=CARTESIAN_POINT('Ctrl Pts',(-0.287670902185649,2.24542951321801,
10.3653636698464));
#42446=CARTESIAN_POINT('Ctrl Pts',(-0.269898940067852,2.27887384299062,
10.3629467531254));
#42447=CARTESIAN_POINT('Ctrl Pts',(-0.251259525838447,2.30422824573741,
10.360799342436));
#42448=CARTESIAN_POINT('Ctrl Pts',(-0.225064991562881,2.33074370695163,
10.3583024557819));
#42449=CARTESIAN_POINT('Ctrl Pts',(-0.22074620877351,2.33487874920317,10.3579051320033));
#42450=CARTESIAN_POINT('Ctrl Pts',(-0.212752015246372,2.34211744153673,
10.3571984501881));
#42451=CARTESIAN_POINT('Ctrl Pts',(-0.209117384443732,2.34526353261613,
10.35688720574));
#42452=CARTESIAN_POINT('Ctrl Pts',(-0.204199881916846,2.34933123481119,
10.3564807132202));
#42453=CARTESIAN_POINT('Ctrl Pts',(-0.202978858835254,2.35032626614653,
10.3563809404691));
#42454=CARTESIAN_POINT('Ctrl Pts',(-0.200943097520943,2.35196055122853,
10.3562165741361));
#42455=CARTESIAN_POINT('Ctrl Pts',(-0.200132500537109,2.35260488933306,
10.3561516403509));
#42456=CARTESIAN_POINT('Ctrl Pts',(-0.199039747335734,2.35346494967293,
10.356064807213));
#42457=CARTESIAN_POINT('Ctrl Pts',(-0.198760331187157,2.35368411949004,
10.3560426653862));
#42458=CARTESIAN_POINT('Ctrl Pts',(-0.198319477644181,2.35402874288414,
10.3560078280483));
#42459=CARTESIAN_POINT('Ctrl Pts',(-0.198158283219286,2.3541545046158,10.3559951105071));
#42460=CARTESIAN_POINT('Ctrl Pts',(-0.197823646432666,2.35441507186388,
10.3559687516828));
#42461=CARTESIAN_POINT('Ctrl Pts',(-0.197650187280385,2.35454985238201,
10.355955112282));
#42462=CARTESIAN_POINT('Ctrl Pts',(-0.197254415426059,2.3548567249601,10.3559240458154));
#42463=CARTESIAN_POINT('Ctrl Pts',(-0.197032015560026,2.3550287033027,10.355906626919));
#42464=CARTESIAN_POINT('Ctrl Pts',(-0.196338277321527,2.35556371110128,
10.3558524107671));
#42465=CARTESIAN_POINT('Ctrl Pts',(-0.195866155124501,2.35592572919409,
10.3558156850643));
#42466=CARTESIAN_POINT('Ctrl Pts',(-0.19218798343589,2.35872997081875,10.355530868397));
#42467=CARTESIAN_POINT('Ctrl Pts',(-0.188937202371077,2.36111330103821,
10.3552868210233));
#42468=CARTESIAN_POINT('Ctrl Pts',(-0.176407953253459,2.36994264559564,
10.354371411469));
#42469=CARTESIAN_POINT('Ctrl Pts',(-0.166836817887374,2.37596072621874,
10.353723361673));
#42470=CARTESIAN_POINT('Ctrl Pts',(-0.150673855232,2.38497457981584,10.3526774425168));
#42471=CARTESIAN_POINT('Ctrl Pts',(-0.144263074596166,2.38827294512693,
10.3522742943601));
#42472=CARTESIAN_POINT('Ctrl Pts',(-0.123884236810992,2.3979077095669,10.3510142095415));
#42473=CARTESIAN_POINT('Ctrl Pts',(-0.109571847785605,2.40346380995871,
10.3501588139026));
#42474=CARTESIAN_POINT('Ctrl Pts',(-0.0838887909432318,2.41137930242907,
10.3486126514736));
#42475=CARTESIAN_POINT('Ctrl Pts',(-0.0726849642575297,2.41418346665747,
10.3479348745162));
#42476=CARTESIAN_POINT('Ctrl Pts',(-0.0593414268293379,2.4167711802308,
10.3471130954248));
#42477=CARTESIAN_POINT('Ctrl Pts',(-0.0573234940589404,2.41714255830781,
10.3469884457075));
#42478=CARTESIAN_POINT('Ctrl Pts',(-0.0546494956259246,2.41760832354531,
10.3468227339911));
#42479=CARTESIAN_POINT('Ctrl Pts',(-0.0539964580017836,2.41771999790753,
10.3467822221186));
#42480=CARTESIAN_POINT('Ctrl Pts',(-0.0529250745727525,2.41789981403068,
10.3467156870208));
#42481=CARTESIAN_POINT('Ctrl Pts',(-0.0525069282532875,2.41796914592765,
10.3466897016421));
#42482=CARTESIAN_POINT('Ctrl Pts',(-0.0516973453375493,2.41810174054077,
10.3466393561319));
#42483=CARTESIAN_POINT('Ctrl Pts',(-0.051305926177642,2.4181651061742,10.3466149993161));
#42484=CARTESIAN_POINT('Ctrl Pts',(-0.0504032445082699,2.41830952943369,
10.346558791696));
#42485=CARTESIAN_POINT('Ctrl Pts',(-0.0498919026602835,2.41839007778071,
10.3465269248019));
#42486=CARTESIAN_POINT('Ctrl Pts',(-0.0482589475640513,2.41864327614353,
10.3464250714086));
#42487=CARTESIAN_POINT('Ctrl Pts',(-0.0471366248648717,2.41881123254212,
10.3463549364466));
#42488=CARTESIAN_POINT('Ctrl Pts',(-0.036996373656594,2.42027401329828,
10.3457200401463));
#42489=CARTESIAN_POINT('Ctrl Pts',(-0.027929024218799,2.42119171500596,
10.3451434158459));
#42490=CARTESIAN_POINT('Ctrl Pts',(0.00616481034600214,2.4231877736036,
10.3429390215637));
#42491=CARTESIAN_POINT('Ctrl Pts',(0.0312478486247287,2.42173211827196,
10.3412357634632));
#42492=CARTESIAN_POINT('Ctrl Pts',(0.0640096514840762,2.4159615054665,10.3389915977708));
#42493=CARTESIAN_POINT('Ctrl Pts',(0.0720576291801567,2.41422383712596,
10.3384396590112));
#42494=CARTESIAN_POINT('Ctrl Pts',(0.0851627889161504,2.41086419116731,
10.3375478688154));
#42495=CARTESIAN_POINT('Ctrl Pts',(0.0902620665210687,2.40942206140203,
10.3372026676597));
#42496=CARTESIAN_POINT('Ctrl Pts',(0.0972998478321883,2.40724289181015,
10.3367308506347));
#42497=CARTESIAN_POINT('Ctrl Pts',(0.0992700618918268,2.40661198651308,
10.336599277179));
#42498=CARTESIAN_POINT('Ctrl Pts',(0.102042765033955,2.40569457833011,10.3364149692848));
#42499=CARTESIAN_POINT('Ctrl Pts',(0.102850355345233,2.40542381301977,10.3363613901504));
#42500=CARTESIAN_POINT('Ctrl Pts',(0.104077455316809,2.40500697733076,10.3362801463517));
#42501=CARTESIAN_POINT('Ctrl Pts',(0.104497744595358,2.40486323869189,10.3362523498254));
#42502=CARTESIAN_POINT('Ctrl Pts',(0.10527292751445,2.40459633529156,10.3362011389486));
#42503=CARTESIAN_POINT('Ctrl Pts',(0.105627904785272,2.40447341833829,10.3361777102524));
#42504=CARTESIAN_POINT('Ctrl Pts',(0.106204906794605,2.40427249099568,10.3361396647962));
#42505=CARTESIAN_POINT('Ctrl Pts',(0.106427061142112,2.40419485804575,10.336125025662));
#42506=CARTESIAN_POINT('Ctrl Pts',(0.106857155987072,2.40404403042252,10.3360967016149));
#42507=CARTESIAN_POINT('Ctrl Pts',(0.107065105764317,2.40397086595448,10.3360830150157));
#42508=CARTESIAN_POINT('Ctrl Pts',(0.107543155856651,2.4038021187272,10.3360515694152));
#42509=CARTESIAN_POINT('Ctrl Pts',(0.107813204678027,2.40370638882533,10.3360338192235));
#42510=CARTESIAN_POINT('Ctrl Pts',(0.108533359442728,2.40345001880399,10.3359865184103));
#42511=CARTESIAN_POINT('Ctrl Pts',(0.108983238487022,2.40328873661888,10.3359570058469));
#42512=CARTESIAN_POINT('Ctrl Pts',(0.112049193641018,2.40218188522832,10.3357561118189));
#42513=CARTESIAN_POINT('Ctrl Pts',(0.114653393363298,2.4012034431985,10.3355866471551));
#42514=CARTESIAN_POINT('Ctrl Pts',(0.146073802186834,2.38893168298727,10.3335525475035));
#42515=CARTESIAN_POINT('Ctrl Pts',(0.173135203120958,2.37357619847468,10.3318963168215));
#42516=CARTESIAN_POINT('Ctrl Pts',(0.209717493048685,2.34518415853004,10.329268612545));
#42517=CARTESIAN_POINT('Ctrl Pts',(0.221152153919479,2.33492196932802,10.3283790017032));
#42518=CARTESIAN_POINT('Ctrl Pts',(0.233507469593503,2.32212923514616,10.3273061448079));
#42519=CARTESIAN_POINT('Ctrl Pts',(0.235183386320996,2.32035405545381,10.3271580378102));
#42520=CARTESIAN_POINT('Ctrl Pts',(0.237318084299341,2.31804082566691,10.3269659451595));
#42521=CARTESIAN_POINT('Ctrl Pts',(0.237795518183092,2.31752003657717,10.3269227566169));
#42522=CARTESIAN_POINT('Ctrl Pts',(0.238563232468572,2.31667705878603,10.326852941018));
#42523=CARTESIAN_POINT('Ctrl Pts',(0.238854583624589,2.31635584477576,10.3268263593625));
#42524=CARTESIAN_POINT('Ctrl Pts',(0.239409031984174,2.31574208174269,10.326775608335));
#42525=CARTESIAN_POINT('Ctrl Pts',(0.239672243716308,2.31544963685297,10.326751443858));
#42526=CARTESIAN_POINT('Ctrl Pts',(0.240272186324793,2.31478060273538,10.3266962011299));
#42527=CARTESIAN_POINT('Ctrl Pts',(0.240608567968258,2.31440370297245,10.3266651082944));
#42528=CARTESIAN_POINT('Ctrl Pts',(0.241635529617899,2.31324758038979,10.3265698171269));
#42529=CARTESIAN_POINT('Ctrl Pts',(0.242323215649973,2.31246580626568,10.3265054981333));
#42530=CARTESIAN_POINT('Ctrl Pts',(0.247396682743893,2.30664152290583,10.3260271590527));
#42531=CARTESIAN_POINT('Ctrl Pts',(0.251628174194777,2.30146733928063,10.3256068207285));
#42532=CARTESIAN_POINT('Ctrl Pts',(0.256946929484487,2.29453451538598,10.3250488904696));
#42533=CARTESIAN_POINT('Ctrl Pts',(0.258182660862609,2.29289146060889,10.3249170402512));
#42534=CARTESIAN_POINT('Ctrl Pts',(0.274202255765956,2.27116172203337,10.3231781984959));
#42535=CARTESIAN_POINT('Ctrl Pts',(0.286619670091613,2.24943898557834,10.3214847050039));
#42536=CARTESIAN_POINT('Ctrl Pts',(0.299703202609065,2.21878414318467,10.3192344285879));
#42537=CARTESIAN_POINT('Ctrl Pts',(0.302696397552957,2.21093505487075,10.318670453852));
#42538=CARTESIAN_POINT('Ctrl Pts',(0.307887253472908,2.19554160296507,10.3175975708367));
#42539=CARTESIAN_POINT('Ctrl Pts',(0.310122591076253,2.18801568214007,10.3170878336785));
#42540=CARTESIAN_POINT('Ctrl Pts',(0.312289642975818,2.1796056098065,10.3165398846622));
#42541=CARTESIAN_POINT('Ctrl Pts',(0.312495052782837,2.17879540751088,10.3164873172727));
#42542=CARTESIAN_POINT('Ctrl Pts',(0.312803334240926,2.17755927853038,10.3164074603327));
#42543=CARTESIAN_POINT('Ctrl Pts',(0.312908491284998,2.17713393342408,10.3163800442021));
#42544=CARTESIAN_POINT('Ctrl Pts',(0.313101115162584,2.17634792097324,10.3163294973434));
#42545=CARTESIAN_POINT('Ctrl Pts',(0.313188826877085,2.17598731522856,10.3163063527586));
#42546=CARTESIAN_POINT('Ctrl Pts',(0.313330929731969,2.17539866748338,10.3162686465582));
#42547=CARTESIAN_POINT('Ctrl Pts',(0.313385694975512,2.17517071750707,10.3162540633385));
#42548=CARTESIAN_POINT('Ctrl Pts',(0.313491543304857,2.17472801768963,10.316225777102));
#42549=CARTESIAN_POINT('Ctrl Pts',(0.313542654336369,2.17451327575281,10.3162120725404));
#42550=CARTESIAN_POINT('Ctrl Pts',(0.313660037091126,2.17401783528397,10.3161804915533));
#42551=CARTESIAN_POINT('Ctrl Pts',(0.313726152871029,2.17373709930849,10.316162624188));
#42552=CARTESIAN_POINT('Ctrl Pts',(0.313936242456229,2.17283963466513,10.3161055925557));
#42553=CARTESIAN_POINT('Ctrl Pts',(0.314078776384394,2.17222256535615,10.3160665109579));
#42554=CARTESIAN_POINT('Ctrl Pts',(0.315336291067836,2.16670430241477,10.3157181588576));
#42555=CARTESIAN_POINT('Ctrl Pts',(0.316338360191054,2.16177773979604,10.3154152068479));
#42556=CARTESIAN_POINT('Ctrl Pts',(0.323019288146932,2.12448445034314,10.3131685268737));
#42557=CARTESIAN_POINT('Ctrl Pts',(0.323833741487077,2.09144019812893,10.3114227468492));
#42558=CARTESIAN_POINT('Ctrl Pts',(0.318164550493345,2.04741487200693,10.3088687628231));
#42559=CARTESIAN_POINT('Ctrl Pts',(0.316081937562729,2.03607784908025,10.3081922643318));
#42560=CARTESIAN_POINT('Ctrl Pts',(0.312919456651998,2.02288457336635,10.3073719923769));
#42561=CARTESIAN_POINT('Ctrl Pts',(0.312422767184617,2.02089633623996,10.3072474924329));
#42562=CARTESIAN_POINT('Ctrl Pts',(0.311740538841501,2.01827209412849,10.3070819503873));
#42563=CARTESIAN_POINT('Ctrl Pts',(0.31157194583778,2.01763170080743,10.307041456983));
#42564=CARTESIAN_POINT('Ctrl Pts',(0.311292226117584,2.01658234490789,10.306974944488));
#42565=CARTESIAN_POINT('Ctrl Pts',(0.311182263805687,2.01617307167528,10.3069489631936));
#42566=CARTESIAN_POINT('Ctrl Pts',(0.310967846889535,2.01538126051426,10.3068986201016));
#42567=CARTESIAN_POINT('Ctrl Pts',(0.310863492837383,2.01499869595132,10.3068742616084));
#42568=CARTESIAN_POINT('Ctrl Pts',(0.310621243925306,2.0141170181182,10.3068180422084));
#42569=CARTESIAN_POINT('Ctrl Pts',(0.310482851962785,2.01361804362786,10.3067861651902));
#42570=CARTESIAN_POINT('Ctrl Pts',(0.310037090084867,2.01202575253903,10.3066842473918));
#42571=CARTESIAN_POINT('Ctrl Pts',(0.309725145734263,2.01093373538995,10.3066140578834));
#42572=CARTESIAN_POINT('Ctrl Pts',(0.306851162286687,2.00107054325669,10.3059774121687));
#42573=CARTESIAN_POINT('Ctrl Pts',(0.303923167713101,1.99241118079135,10.3053990206713));
#42574=CARTESIAN_POINT('Ctrl Pts',(0.289621201534053,1.95538105461509,10.3028364944962));
#42575=CARTESIAN_POINT('Ctrl Pts',(0.274612318745951,1.92858657832475,10.3007294914701));
#42576=CARTESIAN_POINT('Ctrl Pts',(0.250061221206791,1.89646073636747,10.2980365885471));
#42577=CARTESIAN_POINT('Ctrl Pts',(0.243701609858709,1.88888767586324,10.2973892404031));
#42578=CARTESIAN_POINT('Ctrl Pts',(0.23635656803126,1.88091631897174,10.2967041988586));
#42579=CARTESIAN_POINT('Ctrl Pts',(0.235706703685719,1.88021729723407,10.2966440952859));
#42580=CARTESIAN_POINT('Ctrl Pts',(0.234723635409272,1.87916924259015,10.2965539481341));
#42581=CARTESIAN_POINT('Ctrl Pts',(0.234392744231831,1.87881806154996,10.2965237361173));
#42582=CARTESIAN_POINT('Ctrl Pts',(0.233784848633584,1.87817578663082,10.2964684733158));
#42583=CARTESIAN_POINT('Ctrl Pts',(0.233508086819422,1.8778844659156,10.296443404363));
#42584=CARTESIAN_POINT('Ctrl Pts',(0.233064229844219,1.87741900657247,10.2964033465404));
#42585=CARTESIAN_POINT('Ctrl Pts',(0.232897483811156,1.87724453788197,10.2963883307694));
#42586=CARTESIAN_POINT('Ctrl Pts',(0.232579100267325,1.87691215704683,10.2963597228517));
#42587=CARTESIAN_POINT('Ctrl Pts',(0.232427499064008,1.87675421340187,10.2963461281565));
#42588=CARTESIAN_POINT('Ctrl Pts',(0.232081820906305,1.87639480712275,10.2963151915413));
#42589=CARTESIAN_POINT('Ctrl Pts',(0.231887642858669,1.87619344297423,10.2962978576754));
#42590=CARTESIAN_POINT('Ctrl Pts',(0.23129529204231,1.87558076905126,10.2962451132226));
#42591=CARTESIAN_POINT('Ctrl Pts',(0.230896282584455,1.87517026433067,10.2962097676011));
#42592=CARTESIAN_POINT('Ctrl Pts',(0.228023468230252,1.8722303995527,10.2959565764503));
#42593=CARTESIAN_POINT('Ctrl Pts',(0.225509133083264,1.86974074100718,10.2957418360165));
#42594=CARTESIAN_POINT('Ctrl Pts',(0.200808359003068,1.84607519642265,10.2936912834566));
#42595=CARTESIAN_POINT('Ctrl Pts',(0.175744145554674,1.82812429515202,10.2920497191915));
#42596=CARTESIAN_POINT('Ctrl Pts',(0.138360804401912,1.80871248818975,10.2896557637877));
#42597=CARTESIAN_POINT('Ctrl Pts',(0.127932185399244,1.80398404516596,10.2889946999428));
#42598=CARTESIAN_POINT('Ctrl Pts',(0.112213942916123,1.79784320445093,10.2879924354602));
#42599=CARTESIAN_POINT('Ctrl Pts',(0.107104065019908,1.79599438829222,10.2876657978369));
#42600=CARTESIAN_POINT('Ctrl Pts',(0.101088566561202,1.79398839540164,10.287279488529));
#42601=CARTESIAN_POINT('Ctrl Pts',(0.100225811631146,1.79370473870034,10.2872240415869));
#42602=CARTESIAN_POINT('Ctrl Pts',(0.0989072417658184,1.7932773866257,10.2871392330804));
#42603=CARTESIAN_POINT('Ctrl Pts',(0.0984522821738875,1.79313105051226,
10.2871099584991));
#42604=CARTESIAN_POINT('Ctrl Pts',(0.0976604894913164,1.79287831533009,
10.2870589883422));
#42605=CARTESIAN_POINT('Ctrl Pts',(0.0973238029757818,1.79277145677051,
10.2870373079109));
#42606=CARTESIAN_POINT('Ctrl Pts',(0.0966215736010932,1.79254985131148,
10.2869920742734));
#42607=CARTESIAN_POINT('Ctrl Pts',(0.0962560006242379,1.79243520234657,
10.286968517891));
#42608=CARTESIAN_POINT('Ctrl Pts',(0.0953609181330605,1.79215624369425,
10.2869108209865));
#42609=CARTESIAN_POINT('Ctrl Pts',(0.0948311888292194,1.79199264842748,
10.2868766570994));
#42610=CARTESIAN_POINT('Ctrl Pts',(0.0928002307785471,1.79137116767388,
10.2867456050262));
#42611=CARTESIAN_POINT('Ctrl Pts',(0.0912961058345109,1.79092289004995,
10.2866484030595));
#42612=CARTESIAN_POINT('Ctrl Pts',(0.0892799708107033,1.79033801796338,
10.2865179063589));
#42613=CARTESIAN_POINT('Ctrl Pts',(0.0887707933898943,1.79019166805533,
10.2864849316899));
#42614=CARTESIAN_POINT('Ctrl Pts',(0.0551558524363579,1.78061959431953,
10.284306825811));
#42615=CARTESIAN_POINT('Ctrl Pts',(0.020760017249443,1.77655946288935,10.2819664939808));
#42616=CARTESIAN_POINT('Ctrl Pts',(-0.0250630580282221,1.77849670661605,
10.2788795165502));
#42617=CARTESIAN_POINT('Ctrl Pts',(-0.036480735185802,1.77959130892716,
10.2781164839686));
#42618=CARTESIAN_POINT('Ctrl Pts',(-0.0515216636897675,1.78184794640111,
10.2771383104572));
#42619=CARTESIAN_POINT('Ctrl Pts',(-0.0552168129024151,1.78246839899426,
10.2769002159862));
#42620=CARTESIAN_POINT('Ctrl Pts',(-0.0594260976411399,1.78325088737467,
10.2766321758607));
#42621=CARTESIAN_POINT('Ctrl Pts',(-0.0599514607852521,1.78334990322238,
10.2765987785384));
#42622=CARTESIAN_POINT('Ctrl Pts',(-0.0607437887374191,1.78350127684038,
10.2765484987052));
#42623=CARTESIAN_POINT('Ctrl Pts',(-0.061010934330028,1.78355266547918,
10.2765315612672));
#42624=CARTESIAN_POINT('Ctrl Pts',(-0.0614922493452293,1.78364588431146,
10.2765010729285));
#42625=CARTESIAN_POINT('Ctrl Pts',(-0.0617064408349523,1.78368759366248,
10.2764875151588));
#42626=CARTESIAN_POINT('Ctrl Pts',(-0.0621672939050994,1.78377782116313,
10.2764583657971));
#42627=CARTESIAN_POINT('Ctrl Pts',(-0.0624139403753086,1.78382641023058,
10.2764427783713));
#42628=CARTESIAN_POINT('Ctrl Pts',(-0.0630795790524016,1.78395834952927,
10.2764007466804));
#42629=CARTESIAN_POINT('Ctrl Pts',(-0.0634984646465469,1.78404224472533,
10.2763743336099));
#42630=CARTESIAN_POINT('Ctrl Pts',(-0.0654404843702239,1.78443521412597,
10.2762520468699));
#42631=CARTESIAN_POINT('Ctrl Pts',(-0.0669615699209405,1.78475447749471,
10.2761567466713));
#42632=CARTESIAN_POINT('Ctrl Pts',(-0.0994897466986224,1.79182793597579,
10.2741279229893));
#42633=CARTESIAN_POINT('Ctrl Pts',(-0.129338973517293,1.80311542309378,
10.2724317403689));
#42634=CARTESIAN_POINT('Ctrl Pts',(-0.17094618758953,1.82633696985537,10.2697324499497));
#42635=CARTESIAN_POINT('Ctrl Pts',(-0.184237619829957,1.83510293895639,
10.2688124043368));
#42636=CARTESIAN_POINT('Ctrl Pts',(-0.198800815478983,1.84633560430254,
10.2677032683209));
#42637=CARTESIAN_POINT('Ctrl Pts',(-0.200756944743664,1.84788090417787,
10.2675520596688));
#42638=CARTESIAN_POINT('Ctrl Pts',(-0.203248338926103,1.84989643127474,
10.2673565045241));
#42639=CARTESIAN_POINT('Ctrl Pts',(-0.203800280530339,1.85034598339245,
10.267312991252));
#42640=CARTESIAN_POINT('Ctrl Pts',(-0.204686984609724,1.85107309695564,
10.2672427772997));
#42641=CARTESIAN_POINT('Ctrl Pts',(-0.205022684764122,1.8513495154699,10.2672161229725));
#42642=CARTESIAN_POINT('Ctrl Pts',(-0.205660839807665,1.85187714901132,
10.2671653165093));
#42643=CARTESIAN_POINT('Ctrl Pts',(-0.205963396675659,1.85212823992881,
10.2671411694511));
#42644=CARTESIAN_POINT('Ctrl Pts',(-0.206651925693984,1.85270177885855,
10.2670860825993));
#42645=CARTESIAN_POINT('Ctrl Pts',(-0.207037603344304,1.85302457739761,
10.2670551285189));
#42646=CARTESIAN_POINT('Ctrl Pts',(-0.208210768992602,1.85401115463935,
10.2669606731019));
#42647=CARTESIAN_POINT('Ctrl Pts',(-0.208995826325596,1.8546778018495,10.2668970541735));
#42648=CARTESIAN_POINT('Ctrl Pts',(-0.214665828100839,1.8595395675113,10.2664345553281));
#42649=CARTESIAN_POINT('Ctrl Pts',(-0.21942696528653,1.86387623032181,10.2660298178779));
#42650=CARTESIAN_POINT('Ctrl Pts',(-0.225299385120587,1.86955616526625,
10.2655087580452));
#42651=CARTESIAN_POINT('Ctrl Pts',(-0.226534264798849,1.87076998322098,
10.265397908653));
#42652=CARTESIAN_POINT('Ctrl Pts',(-0.229836476142383,1.87406861668662,
10.265098007707));
#42653=CARTESIAN_POINT('Ctrl Pts',(-0.231885162902036,1.87617179331546,
10.264908210074));
#42654=CARTESIAN_POINT('Ctrl Pts',(-0.253919368813548,1.89941927591674,
10.2628256590534));
#42655=CARTESIAN_POINT('Ctrl Pts',(-0.270981027425314,1.92314833595424,
10.2608192281397));
#42656=CARTESIAN_POINT('Ctrl Pts',(-0.287089866249677,1.95347963865494,
10.2585345788915));
#42657=CARTESIAN_POINT('Ctrl Pts',(-0.289441649321907,1.95818200128935,
10.258188066369));
#42658=CARTESIAN_POINT('Ctrl Pts',(-0.293981129700156,1.96784247263212,
10.257494468844));
#42659=CARTESIAN_POINT('Ctrl Pts',(-0.296161017229568,1.97280260529715,
10.2571477893164));
#42660=CARTESIAN_POINT('Ctrl Pts',(-0.298434240647232,1.97835085647988,
10.2567722005812));
#42661=CARTESIAN_POINT('Ctrl Pts',(-0.298652070592939,1.9788866198442,10.2567360564568));
#42662=CARTESIAN_POINT('Ctrl Pts',(-0.298973558686569,1.97968347686127,
10.2566824859202));
#42663=CARTESIAN_POINT('Ctrl Pts',(-0.299078318099037,1.97994412060046,
10.256664993321));
#42664=CARTESIAN_POINT('Ctrl Pts',(-0.299256576842517,1.98038931359871,
10.2566351662712));
#42665=CARTESIAN_POINT('Ctrl Pts',(-0.299330246356087,1.98057379390534,
10.2566228214587));
#42666=CARTESIAN_POINT('Ctrl Pts',(-0.299481390866339,1.98095330249226,
10.256597456956));
#42667=CARTESIAN_POINT('Ctrl Pts',(-0.299558845753334,1.98114833785637,
10.2565844385071));
#42668=CARTESIAN_POINT('Ctrl Pts',(-0.299745277471662,1.9816191224415,10.2565530541385));
#42669=CARTESIAN_POINT('Ctrl Pts',(-0.299854064609073,1.98189494728363,
10.2565346997336));
#42670=CARTESIAN_POINT('Ctrl Pts',(-0.300252222039868,1.98290855351865,
10.2564673710249));
#42671=CARTESIAN_POINT('Ctrl Pts',(-0.300539254413513,1.98364725930728,
10.2564185366112));
#42672=CARTESIAN_POINT('Ctrl Pts',(-0.305770102730545,1.99725786341734,
10.2555229342964));
#42673=CARTESIAN_POINT('Ctrl Pts',(-0.309886240042588,2.01043478888042,
10.2547241392142));
#42674=CARTESIAN_POINT('Ctrl Pts',(-0.315669846875002,2.03421408591075,
10.2533358784551));
#42675=CARTESIAN_POINT('Ctrl Pts',(-0.317676512083658,2.04471090220126,
10.252740725704));
#42676=CARTESIAN_POINT('Ctrl Pts',(-0.321225274298717,2.07004240427519,
10.2513105902921));
#42677=CARTESIAN_POINT('Ctrl Pts',(-0.322266549859838,2.08492145256059,
10.2504748489422));
#42678=CARTESIAN_POINT('Ctrl Pts',(-0.322276716835356,2.10295423647165,
10.2494303352084));
#42679=CARTESIAN_POINT('Ctrl Pts',(-0.322232712885111,2.10608996056174,
10.2492475951044));
#42680=CARTESIAN_POINT('Ctrl Pts',(-0.321916774282351,2.1171233663404,10.2485999739315));
#42681=CARTESIAN_POINT('Ctrl Pts',(-0.321400168572899,2.1250106968606,10.2481285768766));
#42682=CARTESIAN_POINT('Ctrl Pts',(-0.320484300312303,2.13394336119121,
10.2475823036084));
#42683=CARTESIAN_POINT('Ctrl Pts',(-0.320368928388166,2.13501554218857,
10.2475165327137));
#42684=CARTESIAN_POINT('Ctrl Pts',(-0.3201905497065,2.13659852962666,10.2474191219767));
#42685=CARTESIAN_POINT('Ctrl Pts',(-0.32013169620365,2.13710980427196,10.247387613064));
#42686=CARTESIAN_POINT('Ctrl Pts',(-0.320025387588235,2.13801425739179,
10.2473317890992));
#42687=CARTESIAN_POINT('Ctrl Pts',(-0.31997843183043,2.13840749441407,10.2473074898431));
#42688=CARTESIAN_POINT('Ctrl Pts',(-0.319879569557385,2.13922266342354,
10.2472570593305));
#42689=CARTESIAN_POINT('Ctrl Pts',(-0.319827552811289,2.13964458104508,
10.2472309246392));
#42690=CARTESIAN_POINT('Ctrl Pts',(-0.319691629977039,2.14072939753612,
10.2471636434788));
#42691=CARTESIAN_POINT('Ctrl Pts',(-0.319606497098098,2.14139213817831,
10.24712245834));
#42692=CARTESIAN_POINT('Ctrl Pts',(-0.319245440845404,2.1441353441082,10.2469516444635));
#42693=CARTESIAN_POINT('Ctrl Pts',(-0.318951264403229,2.14621331735357,
10.246821440134));
#42694=CARTESIAN_POINT('Ctrl Pts',(-0.316842833626621,2.16012610043917,
10.2459440636011));
#42695=CARTESIAN_POINT('Ctrl Pts',(-0.314390777516254,2.1718533805654,10.2451766990906));
#42696=CARTESIAN_POINT('Ctrl Pts',(-0.302037930123091,2.21795183181976,
10.2420470090228));
#42697=CARTESIAN_POINT('Ctrl Pts',(-0.287103176946999,2.25070114578868,
10.239534197368));
#42698=CARTESIAN_POINT('Ctrl Pts',(-0.266030208539513,2.28191416455311,
10.2371437585563));
#42699=CARTESIAN_POINT('Ctrl Pts',(-0.264945674874943,2.28349012210745,
10.237023172216));
#42700=CARTESIAN_POINT('Ctrl Pts',(-0.263605782795067,2.28540049507824,
10.2368772223337));
#42701=CARTESIAN_POINT('Ctrl Pts',(-0.263363749535825,2.28574414589281,
10.2368509768337));
#42702=CARTESIAN_POINT('Ctrl Pts',(-0.262963952131915,2.28630944559922,
10.2368078195395));
#42703=CARTESIAN_POINT('Ctrl Pts',(-0.262806579345573,2.28653136866038,
10.2367908811256));
#42704=CARTESIAN_POINT('Ctrl Pts',(-0.262522472564793,2.28693093548578,
10.2367603917376));
#42705=CARTESIAN_POINT('Ctrl Pts',(-0.262395839468559,2.28710864938224,
10.2367468338922));
#42706=CARTESIAN_POINT('Ctrl Pts',(-0.262122941521863,2.28749080602003,
10.2367176851553));
#42707=CARTESIAN_POINT('Ctrl Pts',(-0.261976618393266,2.287695205667,10.2367020984283));
#42708=CARTESIAN_POINT('Ctrl Pts',(-0.261574473839645,2.28825557739459,
10.2366593762261));
#42709=CARTESIAN_POINT('Ctrl Pts',(-0.261318163849062,2.28861120070823,
10.236632274472));
#42710=CARTESIAN_POINT('Ctrl Pts',(-0.2599716316571,2.29047146472033,10.2364905547087));
#42711=CARTESIAN_POINT('Ctrl Pts',(-0.258869108857966,2.2919672185651,10.2363767739299));
#42712=CARTESIAN_POINT('Ctrl Pts',(-0.247465091304613,2.30716171801238,
10.2352217418688));
#42713=CARTESIAN_POINT('Ctrl Pts',(-0.236097727779618,2.32002949904546,
10.2342495618533));
#42714=CARTESIAN_POINT('Ctrl Pts',(-0.208483600994742,2.34667040192605,
10.2320971245937));
#42715=CARTESIAN_POINT('Ctrl Pts',(-0.191790570564711,2.35986155516685,
10.2309252112259));
#42716=CARTESIAN_POINT('Ctrl Pts',(-0.172080245809586,2.37249651712578,
10.2295676575219));
#42717=CARTESIAN_POINT('Ctrl Pts',(-0.170226295930851,2.37365849288642,
10.2294402483126));
#42718=CARTESIAN_POINT('Ctrl Pts',(-0.16669107266537,2.37582439317333,10.2291976941318));
#42719=CARTESIAN_POINT('Ctrl Pts',(-0.165012197320453,2.37683205032779,
10.229082672291));
#42720=CARTESIAN_POINT('Ctrl Pts',(-0.157549501012761,2.38121913695622,
10.228571924948));
#42721=CARTESIAN_POINT('Ctrl Pts',(-0.151670646041347,2.38443286290163,
10.2281709271541));
#42722=CARTESIAN_POINT('Ctrl Pts',(-0.144766875374731,2.38793195898004,
10.2276998915251));
#42723=CARTESIAN_POINT('Ctrl Pts',(-0.143835245869158,2.38839847990868,
10.2276363262004));
#42724=CARTESIAN_POINT('Ctrl Pts',(-0.14244844965183,2.38908453809908,10.2275416966308));
#42725=CARTESIAN_POINT('Ctrl Pts',(-0.141994996024861,2.38930753891918,
10.2275107534478));
#42726=CARTESIAN_POINT('Ctrl Pts',(-0.14118753056389,2.38970228107067,10.2274556498518));
#42727=CARTESIAN_POINT('Ctrl Pts',(-0.140833724373961,2.38987444268348,
10.2274315041428));
#42728=CARTESIAN_POINT('Ctrl Pts',(-0.140089375947592,2.39023495718478,
10.2273807030773));
#42729=CARTESIAN_POINT('Ctrl Pts',(-0.139698767369983,2.39042317059391,
10.2273540429306));
#42730=CARTESIAN_POINT('Ctrl Pts',(-0.138670980821531,2.39091585278389,
10.2272838890154));
#42731=CARTESIAN_POINT('Ctrl Pts',(-0.138033182441832,2.39121901527077,
10.2272403500317));
#42732=CARTESIAN_POINT('Ctrl Pts',(-0.135188967272487,2.39255950348518,
10.2270461661523));
#42733=CARTESIAN_POINT('Ctrl Pts',(-0.132971863918247,2.39357384562058,
10.2268947296445));
#42734=CARTESIAN_POINT('Ctrl Pts',(-0.116746815116286,2.40077543070837,
10.2257857568515));
#42735=CARTESIAN_POINT('Ctrl Pts',(-0.102327240609211,2.40598152330111,
10.2247947645774));
#42736=CARTESIAN_POINT('Ctrl Pts',(-0.0563260178287632,2.41897372077274,
10.2216220048773));
#42737=CARTESIAN_POINT('Ctrl Pts',(-0.0239046922849002,2.42302527443662,
10.2193519646799));
#42738=CARTESIAN_POINT('Ctrl Pts',(0.0100509583545428,2.4221216198764,10.2172040174813));
#42739=CARTESIAN_POINT('Ctrl Pts',(0.0115280616561617,2.42207214059716,
10.2171110777308));
#42740=CARTESIAN_POINT('Ctrl Pts',(0.013428515059428,2.42199538883481,10.2169921868044));
#42741=CARTESIAN_POINT('Ctrl Pts',(0.01385219329443,2.42197744050387,10.21696572572));
#42742=CARTESIAN_POINT('Ctrl Pts',(0.0145237866074252,2.42194766165806,
10.216923851879));
#42743=CARTESIAN_POINT('Ctrl Pts',(0.0147717236872081,2.42193638098981,
10.2169084083311));
#42744=CARTESIAN_POINT('Ctrl Pts',(0.0152161732483076,2.42191564485549,
10.2168807521608));
#42745=CARTESIAN_POINT('Ctrl Pts',(0.0154126886648717,2.42190629593017,
10.2168685336239));
#42746=CARTESIAN_POINT('Ctrl Pts',(0.0158749520332594,2.42188388017218,
10.2168398148181));
#42747=CARTESIAN_POINT('Ctrl Pts',(0.0161406920627803,2.42187066420803,
10.2168233230679));
#42748=CARTESIAN_POINT('Ctrl Pts',(0.0169118072180625,2.42183135721213,
10.2167755186033));
#42749=CARTESIAN_POINT('Ctrl Pts',(0.0174171405580597,2.42180440477317,
10.2167442542293));
#42750=CARTESIAN_POINT('Ctrl Pts',(0.0209300547234772,2.42160874119018,
10.2165273411002));
#42751=CARTESIAN_POINT('Ctrl Pts',(0.0239353317044781,2.42139905269883,
10.2163439480406));
#42752=CARTESIAN_POINT('Ctrl Pts',(0.0332869399459402,2.42061465364066,
10.2157788349526));
#42753=CARTESIAN_POINT('Ctrl Pts',(0.0396197786009589,2.41989382740721,
10.2154041244397));
#42754=CARTESIAN_POINT('Ctrl Pts',(0.0615536735255772,2.41673578941638,
10.2141213986409));
#42755=CARTESIAN_POINT('Ctrl Pts',(0.0769944377059781,2.41334060814226,
10.2132443265186));
#42756=CARTESIAN_POINT('Ctrl Pts',(0.116177662349037,2.40165201901112,10.2109578937159));
#42757=CARTESIAN_POINT('Ctrl Pts',(0.139305755559593,2.39169305825259,10.2095410773283));
#42758=CARTESIAN_POINT('Ctrl Pts',(0.162332192302773,2.37840914221612,10.2079285586656));
#42759=CARTESIAN_POINT('Ctrl Pts',(0.163616299877506,2.37765643775332,10.2078379538772));
#42760=CARTESIAN_POINT('Ctrl Pts',(0.165360992359369,2.37661744670995,10.2077139027223));
#42761=CARTESIAN_POINT('Ctrl Pts',(0.165826151011712,2.37633884499538,10.2076807364101));
#42762=CARTESIAN_POINT('Ctrl Pts',(0.166615896668097,2.37586312333279,10.2076242680939));
#42763=CARTESIAN_POINT('Ctrl Pts',(0.166940843494051,2.37566660045956,10.2076009879542));
#42764=CARTESIAN_POINT('Ctrl Pts',(0.167568120305008,2.37528571716469,10.2075559590203));
#42765=CARTESIAN_POINT('Ctrl Pts',(0.167870495444122,2.37510143179418,10.2075342130002));
#42766=CARTESIAN_POINT('Ctrl Pts',(0.168578162750681,2.37466853612653,10.2074832251134));
#42767=CARTESIAN_POINT('Ctrl Pts',(0.168983208882309,2.37441952701345,10.2074539686122));
#42768=CARTESIAN_POINT('Ctrl Pts',(0.170160508556535,2.37369216676697,10.2073687194778));
#42769=CARTESIAN_POINT('Ctrl Pts',(0.170931287748707,2.37321144863153,10.2073126396266));
#42770=CARTESIAN_POINT('Ctrl Pts',(0.172667580331227,2.37211833742271,10.2071857018617));
#42771=CARTESIAN_POINT('Ctrl Pts',(0.173631884057074,2.3715040545623,10.2071147742441));
#42772=CARTESIAN_POINT('Ctrl Pts',(0.181769531307242,2.3662591088262,10.2065125499472));
#42773=CARTESIAN_POINT('Ctrl Pts',(0.188758910962429,2.36135058227448,10.2059708815105));
#42774=CARTESIAN_POINT('Ctrl Pts',(0.201861163279412,2.35134914339914,10.2049059746637));
#42775=CARTESIAN_POINT('Ctrl Pts',(0.207996722431496,2.34629589797771,10.204384435751));
#42776=CARTESIAN_POINT('Ctrl Pts',(0.238026839225436,2.31964012652625,10.2017172461518));
#42777=CARTESIAN_POINT('Ctrl Pts',(0.258772052938662,2.29477041105743,10.1994682660753));
#42778=CARTESIAN_POINT('Ctrl Pts',(0.276261903006829,2.26596016100563,10.1973366749835));
#42779=CARTESIAN_POINT('Ctrl Pts',(0.277029407627232,2.26467580760319,10.1972425764988));
#42780=CARTESIAN_POINT('Ctrl Pts',(0.278003958552199,2.26301888288995,10.1971224145955));
#42781=CARTESIAN_POINT('Ctrl Pts',(0.278219232702047,2.2626512087537,10.197095827993));
#42782=CARTESIAN_POINT('Ctrl Pts',(0.278558981842014,2.26206829141269,10.1970538010444));
#42783=CARTESIAN_POINT('Ctrl Pts',(0.278683936995338,2.26185333085257,10.1970383295244));
#42784=CARTESIAN_POINT('Ctrl Pts',(0.27890728954147,2.261468071608,10.1970106489211));
#42785=CARTESIAN_POINT('Ctrl Pts',(0.279005779096378,2.26129782868756,10.1969984338577));
#42786=CARTESIAN_POINT('Ctrl Pts',(0.27923683638241,2.26089759259308,10.196969755885));
#42787=CARTESIAN_POINT('Ctrl Pts',(0.279369275633034,2.26066752605488,10.196953301416));
#42788=CARTESIAN_POINT('Ctrl Pts',(0.279751933616068,2.2600008889506,10.1969057104104));
#42789=CARTESIAN_POINT('Ctrl Pts',(0.280001415769493,2.25956389316541,10.1968746215505));
#42790=CARTESIAN_POINT('Ctrl Pts',(0.281706097630932,2.25656164372482,10.1966617631));
#42791=CARTESIAN_POINT('Ctrl Pts',(0.28312710826658,2.2539769975604,10.1964821540814));
#42792=CARTESIAN_POINT('Ctrl Pts',(0.287472416019746,2.24580979767593,10.1959247874246));
#42793=CARTESIAN_POINT('Ctrl Pts',(0.290268730264669,2.24016048723107,10.1955539482835));
#42794=CARTESIAN_POINT('Ctrl Pts',(0.299371105407499,2.22032847871433,10.1942899559377));
#42795=CARTESIAN_POINT('Ctrl Pts',(0.304817709053173,2.20577442773385,10.1934269641108));
#42796=CARTESIAN_POINT('Ctrl Pts',(0.309985007400795,2.18819481770798,10.1924025607434));
#42797=CARTESIAN_POINT('Ctrl Pts',(0.310740271305906,2.18549569791799,10.192245790965));
#42798=CARTESIAN_POINT('Ctrl Pts',(0.317335580343344,2.16068293176026,10.1908071293027));
#42799=CARTESIAN_POINT('Ctrl Pts',(0.320840369902876,2.13801994083312,10.1895048771523));
#42800=CARTESIAN_POINT('Ctrl Pts',(0.321981601457013,2.11381610238357,10.1880338495369));
#42801=CARTESIAN_POINT('Ctrl Pts',(0.322037195550189,2.11245315039475,10.1879507702548));
#42802=CARTESIAN_POINT('Ctrl Pts',(0.322102113908958,2.11056772596927,10.1878354936258));
#42803=CARTESIAN_POINT('Ctrl Pts',(0.322118823364463,2.11004550874783,10.1878035276797));
#42804=CARTESIAN_POINT('Ctrl Pts',(0.322145326270901,2.10914901971396,10.1877485873219));
#42805=CARTESIAN_POINT('Ctrl Pts',(0.322155737615082,2.10877476607529,10.1877256323026));
#42806=CARTESIAN_POINT('Ctrl Pts',(0.32217580818246,2.10800504438436,10.1876783810458));
#42807=CARTESIAN_POINT('Ctrl Pts',(0.322185391472247,2.1076095751076,10.1876540824681));
#42808=CARTESIAN_POINT('Ctrl Pts',(0.322205665476916,2.1067041016306,10.1875983978331));
#42809=CARTESIAN_POINT('Ctrl Pts',(0.32221587345273,2.1061940886673,10.1875669967084));
#42810=CARTESIAN_POINT('Ctrl Pts',(0.322243841858294,2.10460858072232,10.1874692636264));
#42811=CARTESIAN_POINT('Ctrl Pts',(0.322257428620327,2.10353302787113,10.1874028011198));
#42812=CARTESIAN_POINT('Ctrl Pts',(0.322276367159658,2.10104944880743,10.1872489452351));
#42813=CARTESIAN_POINT('Ctrl Pts',(0.322277876209116,2.09964142322781,10.1871614325446));
#42814=CARTESIAN_POINT('Ctrl Pts',(0.322203230711669,2.08602390545062,10.1863122317901));
#42815=CARTESIAN_POINT('Ctrl Pts',(0.321442523306059,2.07382952204161,10.1855291560603));
#42816=CARTESIAN_POINT('Ctrl Pts',(0.317925889171002,2.04444164648694,10.1835863912151));
#42817=CARTESIAN_POINT('Ctrl Pts',(0.314465551617781,2.02737136985831,10.1824099858604));
#42818=CARTESIAN_POINT('Ctrl Pts',(0.304390135563161,1.99244868612957,10.1799509659343));
#42819=CARTESIAN_POINT('Ctrl Pts',(0.29753656184219,1.97472902765568,10.1786732057549));
#42820=CARTESIAN_POINT('Ctrl Pts',(0.289049496588848,1.9574811205319,10.1774614717579));
#42821=CARTESIAN_POINT('Ctrl Pts',(0.288935056620201,1.95724925380214,10.1774451886932));
#42822=CARTESIAN_POINT('Ctrl Pts',(0.288402527519514,1.95617356089962,10.1773696781551));
#42823=CARTESIAN_POINT('Ctrl Pts',(0.287981014348883,1.95533142051241,10.1773106510515));
#42824=CARTESIAN_POINT('Ctrl Pts',(0.287396055339469,1.95417541979105,10.1772297597578));
#42825=CARTESIAN_POINT('Ctrl Pts',(0.287235780315555,1.95385997356241,10.1772077002351));
#42826=CARTESIAN_POINT('Ctrl Pts',(0.286979856702142,1.95335832348388,10.1771726421203));
#42827=CARTESIAN_POINT('Ctrl Pts',(0.28688454621999,1.95317194891642,10.1771596222539));
#42828=CARTESIAN_POINT('Ctrl Pts',(0.286698331466266,1.95280868941753,10.1771342554664));
#42829=CARTESIAN_POINT('Ctrl Pts',(0.286607445316277,1.95263179628577,10.1771219074995));
#42830=CARTESIAN_POINT('Ctrl Pts',(0.286387115623111,1.95220393994474,10.1770920522105));
#42831=CARTESIAN_POINT('Ctrl Pts',(0.286257505534049,1.95195306187,10.1770745554682));
#42832=CARTESIAN_POINT('Ctrl Pts',(0.285858014603468,1.95118227844976,10.1770208268521));
#42833=CARTESIAN_POINT('Ctrl Pts',(0.285587043966299,1.9506629346352,10.1769846635502));
#42834=CARTESIAN_POINT('Ctrl Pts',(0.282616016091493,1.94500630660084,10.1765911645923));
#42835=CARTESIAN_POINT('Ctrl Pts',(0.279778868587143,1.93994172134119,10.1762423376253));
#42836=CARTESIAN_POINT('Ctrl Pts',(0.273367816919066,1.92918931030657,10.1755033435574));
#42837=CARTESIAN_POINT('Ctrl Pts',(0.269749793022916,1.92353098117248,10.1751154440138));
#42838=CARTESIAN_POINT('Ctrl Pts',(0.250806165353673,1.89585016570161,10.1732018665211));
#42839=CARTESIAN_POINT('Ctrl Pts',(0.23295011912224,1.87568945784308,10.1717467469305));
#42840=CARTESIAN_POINT('Ctrl Pts',(0.209949120621521,1.85546581051673,10.1699752498973));
#42841=CARTESIAN_POINT('Ctrl Pts',(0.207052551073976,1.85300841581856,10.1697539697653));
#42842=CARTESIAN_POINT('Ctrl Pts',(0.198211181805984,1.84577240263181,10.1690827987541));
#42843=CARTESIAN_POINT('Ctrl Pts',(0.192139863679668,1.84115332287285,10.1686274646284));
#42844=CARTESIAN_POINT('Ctrl Pts',(0.185115652869838,1.8361926493763,10.1681042798604));
#42845=CARTESIAN_POINT('Ctrl Pts',(0.184317991449631,1.83563472017691,10.1680449198895));
#42846=CARTESIAN_POINT('Ctrl Pts',(0.183107765355365,1.83479635989196,10.1679549316943));
#42847=CARTESIAN_POINT('Ctrl Pts',(0.18269705222233,1.83451325538768,10.167924405277));
#42848=CARTESIAN_POINT('Ctrl Pts',(0.181982023188761,1.83402283095983,10.1678712819083));
#42849=CARTESIAN_POINT('Ctrl Pts',(0.181678005380304,1.83381507635911,10.1678487014972));
#42850=CARTESIAN_POINT('Ctrl Pts',(0.181043536555791,1.83338309698869,10.1678015910343));
#42851=CARTESIAN_POINT('Ctrl Pts',(0.180713023645052,1.83315896458229,10.1677770575382));
#42852=CARTESIAN_POINT('Ctrl Pts',(0.179940682784765,1.83263730619594,10.1677197452475));
#42853=CARTESIAN_POINT('Ctrl Pts',(0.179498533056314,1.83234026080785,10.1676869483947));
#42854=CARTESIAN_POINT('Ctrl Pts',(0.178062439832272,1.83138062225204,10.167580466456));
#42855=CARTESIAN_POINT('Ctrl Pts',(0.17706555713016,1.830722464737,10.1675066149567));
#42856=CARTESIAN_POINT('Ctrl Pts',(0.174723142355374,1.82919459760054,10.1673332224154));
#42857=CARTESIAN_POINT('Ctrl Pts',(0.173374747444346,1.8283293552063,10.1672335167237));
#42858=CARTESIAN_POINT('Ctrl Pts',(0.168710575844485,1.82538530097995,10.1668889623726));
#42859=CARTESIAN_POINT('Ctrl Pts',(0.165363523589845,1.82335691907918,10.1666422763839));
#42860=CARTESIAN_POINT('Ctrl Pts',(0.15533981381169,1.81752925441043,10.1659049287698));
#42861=CARTESIAN_POINT('Ctrl Pts',(0.148563710120675,1.81390737749328,10.1654082401108));
#42862=CARTESIAN_POINT('Ctrl Pts',(0.130514708312829,1.80507425221755,10.1640903474292));
#42863=CARTESIAN_POINT('Ctrl Pts',(0.119059145155823,1.80026651421094,10.1632585227543));
#42864=CARTESIAN_POINT('Ctrl Pts',(0.0973078349957262,1.79258184458971,
10.1617004316635));
#42865=CARTESIAN_POINT('Ctrl Pts',(0.0870900312954191,1.7895325031056,10.1609769460985));
#42866=CARTESIAN_POINT('Ctrl Pts',(0.0632446307792649,1.78368629242499,
10.1593271839626));
#42867=CARTESIAN_POINT('Ctrl Pts',(0.0495476097231807,1.78125342099902,
10.1584075849549));
#42868=CARTESIAN_POINT('Ctrl Pts',(0.0348937968962166,1.7796184860574,10.1574809326854));
#42869=CARTESIAN_POINT('Ctrl Pts',(0.0340525205807042,1.77952797716765,
10.1574279335444));
#42870=CARTESIAN_POINT('Ctrl Pts',(0.0329079980250895,1.7794094012341,10.1573561112264));
#42871=CARTESIAN_POINT('Ctrl Pts',(0.0326050637718685,1.77937845024172,
10.1573371279083));
#42872=CARTESIAN_POINT('Ctrl Pts',(0.0320911049542223,1.77932667467969,
10.1573049666544));
#42873=CARTESIAN_POINT('Ctrl Pts',(0.0318801036735994,1.77930562901804,
10.1572917762466));
#42874=CARTESIAN_POINT('Ctrl Pts',(0.0314722135044432,1.77926535182979,
10.1572663031904));
#42875=CARTESIAN_POINT('Ctrl Pts',(0.0312753291881682,1.77924609348583,
10.1572540191428));
#42876=CARTESIAN_POINT('Ctrl Pts',(0.0308044471122331,1.7792004715839,10.1572246671725));
#42877=CARTESIAN_POINT('Ctrl Pts',(0.0305304334143919,1.77917427779125,
10.1572076089586));
#42878=CARTESIAN_POINT('Ctrl Pts',(0.0297085218762604,1.77909677132138,
10.1571565079363));
#42879=CARTESIAN_POINT('Ctrl Pts',(0.0291605222703362,1.77904651053473,
10.1571225242911));
#42880=CARTESIAN_POINT('Ctrl Pts',(0.024378692687874,1.77862028442435,10.1568267248375));
#42881=CARTESIAN_POINT('Ctrl Pts',(0.0201376909896521,1.77832668760928,
10.1565694454976));
#42882=CARTESIAN_POINT('Ctrl Pts',(0.00731995009551853,1.77769385517253,
10.1558037977783));
#42883=CARTESIAN_POINT('Ctrl Pts',(-0.00126615595632977,1.77761319421737,
10.1553069807815));
#42884=CARTESIAN_POINT('Ctrl Pts',(-0.0126959361606186,1.77796254975445,
10.1546552530361));
#42885=CARTESIAN_POINT('Ctrl Pts',(-0.0155447750850952,1.77808748610062,
10.154493614807));
#42886=CARTESIAN_POINT('Ctrl Pts',(-0.0207295372943453,1.77838385360752,
10.1542003455146));
#42887=CARTESIAN_POINT('Ctrl Pts',(-0.0230659477176856,1.77854297086814,
10.1540685251049));
#42888=CARTESIAN_POINT('Ctrl Pts',(-0.043670795470961,1.78017203082368,
10.1529075143096));
#42889=CARTESIAN_POINT('Ctrl Pts',(-0.0617840496531189,1.78317231238318,
10.1518952230683));
#42890=CARTESIAN_POINT('Ctrl Pts',(-0.0855973286917739,1.78923756164319,
10.1504892536515));
#42891=CARTESIAN_POINT('Ctrl Pts',(-0.0916043077933855,1.79095495408075,
10.150128191693));
#42892=CARTESIAN_POINT('Ctrl Pts',(-0.0992687234499406,1.79338930160738,
10.1496569403565));
#42893=CARTESIAN_POINT('Ctrl Pts',(-0.100975485081835,1.79394714335067,
10.1495513175315));
#42894=CARTESIAN_POINT('Ctrl Pts',(-0.108824841347796,1.79658545023754,
10.1490622486057));
#42895=CARTESIAN_POINT('Ctrl Pts',(-0.114908076181694,1.79883665540829,
10.1486737839291));
#42896=CARTESIAN_POINT('Ctrl Pts',(-0.121875645928436,1.80165696292966,
10.1482162954444));
#42897=CARTESIAN_POINT('Ctrl Pts',(-0.122830460859628,1.80204879814811,
10.1481533261168));
#42898=CARTESIAN_POINT('Ctrl Pts',(-0.124248128650533,1.80263855069187,
10.1480594140394));
#42899=CARTESIAN_POINT('Ctrl Pts',(-0.124712433090793,1.8028329795623,10.1480285896695));
#42900=CARTESIAN_POINT('Ctrl Pts',(-0.125538633007392,1.80318123058497,
10.1479736195501));
#42901=CARTESIAN_POINT('Ctrl Pts',(-0.125900706848187,1.80333462914022,
10.1479494882453));
#42902=CARTESIAN_POINT('Ctrl Pts',(-0.126599727730764,1.80363229104882,
10.1479028202342));
#42903=CARTESIAN_POINT('Ctrl Pts',(-0.126936711359007,1.80377646737967,
10.1478802865232));
#42904=CARTESIAN_POINT('Ctrl Pts',(-0.127665055410159,1.80408955586728,
10.1478315046946));
#42905=CARTESIAN_POINT('Ctrl Pts',(-0.128056327755394,1.80425867005318,
10.1478052497084));
#42906=CARTESIAN_POINT('Ctrl Pts',(-0.129591659113807,1.80492588305837,
10.1477020331109));
#42907=CARTESIAN_POINT('Ctrl Pts',(-0.130733145177707,1.805429843191,10.1476248712256));
#42908=CARTESIAN_POINT('Ctrl Pts',(-0.133415914618493,1.80663293700132,
10.1474425116309));
#42909=CARTESIAN_POINT('Ctrl Pts',(-0.134954662744456,1.8073376027681,10.1473371251291));
#42910=CARTESIAN_POINT('Ctrl Pts',(-0.140305131230139,1.8098390049233,10.1469678719691));
#42911=CARTESIAN_POINT('Ctrl Pts',(-0.144086972472864,1.81169829244366,
10.146701861441));
#42912=CARTESIAN_POINT('Ctrl Pts',(-0.159119056548183,1.81945824904999,
10.1456238283261));
#42913=CARTESIAN_POINT('Ctrl Pts',(-0.170051302617941,1.82594701594472,
10.1447918851835));
#42914=CARTESIAN_POINT('Ctrl Pts',(-0.202157140040345,1.84766522436195,
10.1422066529196));
#42915=CARTESIAN_POINT('Ctrl Pts',(-0.221891288400186,1.86483077169538,
10.1404065459565));
#42916=CARTESIAN_POINT('Ctrl Pts',(-0.243181659338713,1.88844216379355,
10.1383357323394));
#42917=CARTESIAN_POINT('Ctrl Pts',(-0.246906541402382,1.89280152645085,
10.1379681039967));
#42918=CARTESIAN_POINT('Ctrl Pts',(-0.250926024741231,1.89776811346674,
10.1375674905578));
#42919=CARTESIAN_POINT('Ctrl Pts',(-0.251337092179029,1.89827922284463,
10.1375264730715));
#42920=CARTESIAN_POINT('Ctrl Pts',(-0.251929268592681,1.89902013818866,
10.1374673198599));
#42921=CARTESIAN_POINT('Ctrl Pts',(-0.252111626093049,1.89924893719411,
10.13744909509));
#42922=CARTESIAN_POINT('Ctrl Pts',(-0.252431441275568,1.89965132367063,
10.1374171177172));
#42923=CARTESIAN_POINT('Ctrl Pts',(-0.252569031887072,1.89982480477289,
10.1374033555128));
#42924=CARTESIAN_POINT('Ctrl Pts',(-0.252853827547614,1.90018465044015,
10.1373748594096));
#42925=CARTESIAN_POINT('Ctrl Pts',(-0.253001005139948,1.90037103560792,
10.1373601274899));
#42926=CARTESIAN_POINT('Ctrl Pts',(-0.25338079451323,1.90085309410642,10.1373220969849));
#42927=CARTESIAN_POINT('Ctrl Pts',(-0.253613095671186,1.90114901342301,
10.1372988207149));
#42928=CARTESIAN_POINT('Ctrl Pts',(-0.254586176694237,1.90239306196783,
10.1372012545747));
#42929=CARTESIAN_POINT('Ctrl Pts',(-0.255322174348429,1.90334494485143,
10.1371273016437));
#42930=CARTESIAN_POINT('Ctrl Pts',(-0.26047015059009,1.91008056205998,10.1366087357031));
#42931=CARTESIAN_POINT('Ctrl Pts',(-0.264690904509269,1.9160085985615,10.136176777103));
#42932=CARTESIAN_POINT('Ctrl Pts',(-0.282832977836315,1.94340729504158,
10.1342631611438));
#42933=CARTESIAN_POINT('Ctrl Pts',(-0.294368688616418,1.96634720330998,
10.1328759772448));
#42934=CARTESIAN_POINT('Ctrl Pts',(-0.303860509652376,1.99259717453918,
10.1312917150564));
#42935=CARTESIAN_POINT('Ctrl Pts',(-0.304627078778883,1.99479107038169,
10.1311593926873));
#42936=CARTESIAN_POINT('Ctrl Pts',(-0.307026183798727,2.00190335025002,
10.1307303534473));
#42937=CARTESIAN_POINT('Ctrl Pts',(-0.308563790076345,2.0068527279617,10.130431667043));
#42938=CARTESIAN_POINT('Ctrl Pts',(-0.312570459064317,2.02094016733407,
10.1295782427468));
#42939=CARTESIAN_POINT('Ctrl Pts',(-0.314757085133555,2.03015231006502,
10.1290161858076));
#42940=CARTESIAN_POINT('Ctrl Pts',(-0.316750433080215,2.04057229495527,
10.1283710347541));
#42941=CARTESIAN_POINT('Ctrl Pts',(-0.316959754494367,2.04169903121609,
10.1283011542116));
#42942=CARTESIAN_POINT('Ctrl Pts',(-0.317255262062329,2.04333833362079,
10.1281993035841));
#42943=CARTESIAN_POINT('Ctrl Pts',(-0.317346226628274,2.04385003844255,
10.1281674856041));
#42944=CARTESIAN_POINT('Ctrl Pts',(-0.317504466997128,2.04475285926548,
10.1281113020831));
#42945=CARTESIAN_POINT('Ctrl Pts',(-0.317572259066667,2.04514388464785,
10.1280869530082));
#42946=CARTESIAN_POINT('Ctrl Pts',(-0.317701194322453,2.04589583420773,
10.128040099773));
#42947=CARTESIAN_POINT('Ctrl Pts',(-0.317762445199514,2.04625673950106,
10.128017599076));
#42948=CARTESIAN_POINT('Ctrl Pts',(-0.31789177382186,2.04702672613575,10.1279695660028));
#42949=CARTESIAN_POINT('Ctrl Pts',(-0.317959677070191,2.04743583575896,
10.1279440281244));
#42950=CARTESIAN_POINT('Ctrl Pts',(-0.318120470596281,2.04841631167379,
10.1278827827648));
#42951=CARTESIAN_POINT('Ctrl Pts',(-0.318212611229245,2.04898779791655,
10.127847051547));
#42952=CARTESIAN_POINT('Ctrl Pts',(-0.318455392460631,2.05051986214893,
10.127751170967));
#42953=CARTESIAN_POINT('Ctrl Pts',(-0.318603225545463,2.05148087317603,
10.1276909327731));
#42954=CARTESIAN_POINT('Ctrl Pts',(-0.321109153307386,2.06827647272606,
10.1266364395165));
#42955=CARTESIAN_POINT('Ctrl Pts',(-0.322288067930669,2.08426144891936,
10.1256045749165));
#42956=CARTESIAN_POINT('Ctrl Pts',(-0.322274890758155,2.1002653522546,10.1245441658164));
#42957=CARTESIAN_POINT('',(-0.322274855599701,2.09970609858236,9.87441280121724));
#42958=CARTESIAN_POINT('Ctrl Pts',(-0.32227489106725,2.10026497658775,10.1245441907079));
#42959=CARTESIAN_POINT('Ctrl Pts',(-0.322257938840951,2.12088293733043,
10.1231780574279));
#42960=CARTESIAN_POINT('Ctrl Pts',(-0.320262365543633,2.14145188343667,
10.1217683869481));
#42961=CARTESIAN_POINT('Ctrl Pts',(-0.314416419040088,2.17142809675683,
10.1197192579556));
#42962=CARTESIAN_POINT('Ctrl Pts',(-0.312067804907137,2.1810763657603,10.1190613622444));
#42963=CARTESIAN_POINT('Ctrl Pts',(-0.308215404461165,2.19422691146406,
10.1181798669604));
#42964=CARTESIAN_POINT('Ctrl Pts',(-0.307089664032326,2.19783346940103,
10.117939751909));
#42965=CARTESIAN_POINT('Ctrl Pts',(-0.30573213545481,2.20192803298355,10.117669683351));
#42966=CARTESIAN_POINT('Ctrl Pts',(-0.305562294710364,2.20243606112507,
10.1176362198667));
#42967=CARTESIAN_POINT('Ctrl Pts',(-0.30530421929072,2.20320166390911,10.1175858604995));
#42968=CARTESIAN_POINT('Ctrl Pts',(-0.30521692463703,2.20345955087256,10.1175689094299));
#42969=CARTESIAN_POINT('Ctrl Pts',(-0.305059069943524,2.20392394861108,
10.1175384064259));
#42970=CARTESIAN_POINT('Ctrl Pts',(-0.304988627112674,2.2041304978505,10.1175248475924));
#42971=CARTESIAN_POINT('Ctrl Pts',(-0.304836638538316,2.2045746744916,10.1174957069249));
#42972=CARTESIAN_POINT('Ctrl Pts',(-0.304755024970108,2.20481227741475,
10.1174801292341));
#42973=CARTESIAN_POINT('Ctrl Pts',(-0.304534102242949,2.20545301379606,
10.1174381490695));
#42974=CARTESIAN_POINT('Ctrl Pts',(-0.304394269865006,2.20585596830555,
10.1174117776608));
#42975=CARTESIAN_POINT('Ctrl Pts',(-0.303743346225721,2.20771977789344,
10.1172899324101));
#42976=CARTESIAN_POINT('Ctrl Pts',(-0.303222524836559,2.2091772484648,10.1171950270397));
#42977=CARTESIAN_POINT('Ctrl Pts',(-0.291885997197875,2.24019449508783,
10.1151821921667));
#42978=CARTESIAN_POINT('Ctrl Pts',(-0.276806062846409,2.26802116132223,
10.1134980411939));
#42979=CARTESIAN_POINT('Ctrl Pts',(-0.253686308562861,2.29888302171432,
10.1113150609373));
#42980=CARTESIAN_POINT('Ctrl Pts',(-0.249260761820422,2.30440221290151,
10.110911066259));
#42981=CARTESIAN_POINT('Ctrl Pts',(-0.237701694976071,2.31788362479289,
10.1098820233748));
#42982=CARTESIAN_POINT('Ctrl Pts',(-0.230347476959078,2.32564434936758,
10.1092499782684));
#42983=CARTESIAN_POINT('Ctrl Pts',(-0.221719771297361,2.33388688615347,
10.1085249330278));
#42984=CARTESIAN_POINT('Ctrl Pts',(-0.22081258398833,2.33474355195118,10.1084488915513));
#42985=CARTESIAN_POINT('Ctrl Pts',(-0.219588472391922,2.3358861177505,10.1083465367667));
#42986=CARTESIAN_POINT('Ctrl Pts',(-0.219275913257072,2.33617669575412,
10.1083204237822));
#42987=CARTESIAN_POINT('Ctrl Pts',(-0.218693804263142,2.33671571553767,
10.1082718310615));
#42988=CARTESIAN_POINT('Ctrl Pts',(-0.218424405603673,2.33696432018454,
10.1082493583156));
#42989=CARTESIAN_POINT('Ctrl Pts',(-0.217865231186964,2.33747856998585,
10.108202745465));
#42990=CARTESIAN_POINT('Ctrl Pts',(-0.217575392501089,2.3377441455399,10.1081786024608));
#42991=CARTESIAN_POINT('Ctrl Pts',(-0.216914028386872,2.33834792284827,
10.1081235525712));
#42992=CARTESIAN_POINT('Ctrl Pts',(-0.216542197232684,2.33868578686254,
10.1080926314698));
#42993=CARTESIAN_POINT('Ctrl Pts',(-0.215407693083005,2.33971181997201,
10.1079983741018));
#42994=CARTESIAN_POINT('Ctrl Pts',(-0.214642523986204,2.34039720824363,
10.107934920965));
#42995=CARTESIAN_POINT('Ctrl Pts',(-0.209099607407693,2.34531462816244,
10.1074760967494));
#42996=CARTESIAN_POINT('Ctrl Pts',(-0.204200641510692,2.34940729985432,
10.1070749724205));
#42997=CARTESIAN_POINT('Ctrl Pts',(-0.197848672282886,2.35440118381033,
10.1065597818018));
#42998=CARTESIAN_POINT('Ctrl Pts',(-0.196505417293216,2.3554401696114,10.1064511048776));
#42999=CARTESIAN_POINT('Ctrl Pts',(-0.190261421843346,2.36019140031748,
10.1059471673028));
#43000=CARTESIAN_POINT('Ctrl Pts',(-0.185263543514597,2.36377335980565,
10.105547253633));
#43001=CARTESIAN_POINT('Ctrl Pts',(-0.169603270706567,2.37433230840627,
10.1043052506307));
#43002=CARTESIAN_POINT('Ctrl Pts',(-0.158627726238927,2.3808214479617,10.1034494648409));
#43003=CARTESIAN_POINT('Ctrl Pts',(-0.137297717399238,2.39178231562937,
10.1018281959589));
#43004=CARTESIAN_POINT('Ctrl Pts',(-0.127035467839363,2.39639430087592,
10.1010651243515));
#43005=CARTESIAN_POINT('Ctrl Pts',(-0.105972115751367,2.40456508181908,
10.0995531464768));
#43006=CARTESIAN_POINT('Ctrl Pts',(-0.0951804873906182,2.40810827966795,
10.0988055092198));
#43007=CARTESIAN_POINT('Ctrl Pts',(-0.0827165842986341,2.41148287085239,
10.0979885942502));
#43008=CARTESIAN_POINT('Ctrl Pts',(-0.081206913461176,2.4118798640383,10.0978904135174));
#43009=CARTESIAN_POINT('Ctrl Pts',(-0.0792939039620157,2.41236808935681,
10.0977670220605));
#43010=CARTESIAN_POINT('Ctrl Pts',(-0.0788932270376829,2.41246952681196,
10.0977412343538));
#43011=CARTESIAN_POINT('Ctrl Pts',(-0.0782539623965361,2.41263005838896,
10.0977001822613));
#43012=CARTESIAN_POINT('Ctrl Pts',(-0.0780155020060391,2.41268965043116,
10.0976848891038));
#43013=CARTESIAN_POINT('Ctrl Pts',(-0.0775644227889487,2.41280182850157,
10.0976559986108));
#43014=CARTESIAN_POINT('Ctrl Pts',(-0.0773518202869763,2.41285447015362,
10.097642398165));
#43015=CARTESIAN_POINT('Ctrl Pts',(-0.076866722751274,2.41297405849796,
10.0976114026443));
#43016=CARTESIAN_POINT('Ctrl Pts',(-0.0765941943045591,2.41304086595759,
10.0975940157387));
#43017=CARTESIAN_POINT('Ctrl Pts',(-0.0757612032789912,2.41324391196034,
10.0975409518931));
#43018=CARTESIAN_POINT('Ctrl Pts',(-0.0752004580343544,2.41337900284813,
10.097505341078));
#43019=CARTESIAN_POINT('Ctrl Pts',(-0.0711124136956874,2.41435226189732,
10.0972465071859));
#43020=CARTESIAN_POINT('Ctrl Pts',(-0.0675713803009467,2.41513240263841,
10.0970265470143));
#43021=CARTESIAN_POINT('Ctrl Pts',(-0.0398524872201292,2.42075053288999,
10.0953323217932));
#43022=CARTESIAN_POINT('Ctrl Pts',(-0.01520152465871,2.42285969969594,10.0939840630197));
#43023=CARTESIAN_POINT('Ctrl Pts',(0.0222284425364871,2.42176149852903,
10.0918834827467));
#43024=CARTESIAN_POINT('Ctrl Pts',(0.0349709647895566,2.42062682508333,
10.091159828552));
#43025=CARTESIAN_POINT('Ctrl Pts',(0.0541172346379056,2.41776684339642,
10.0900325041495));
#43026=CARTESIAN_POINT('Ctrl Pts',(0.060591126940391,2.41659619159425,10.089644391292));
#43027=CARTESIAN_POINT('Ctrl Pts',(0.070529094835069,2.41448316461107,10.0890353207473));
#43028=CARTESIAN_POINT('Ctrl Pts',(0.0740210384586993,2.41367961095249,
10.0888187505667));
#43029=CARTESIAN_POINT('Ctrl Pts',(0.0782778912461906,2.41262500168678,
10.0885513625044));
#43030=CARTESIAN_POINT('Ctrl Pts',(0.079056298122792,2.41242906658376,10.0885023291108));
#43031=CARTESIAN_POINT('Ctrl Pts',(0.0802011898678842,2.41213632990032,
10.0884300027874));
#43032=CARTESIAN_POINT('Ctrl Pts',(0.0805682531630738,2.41204178547141,
10.0884067828422));
#43033=CARTESIAN_POINT('Ctrl Pts',(0.0812791306576516,2.41185734692955,
10.0883617523849));
#43034=CARTESIAN_POINT('Ctrl Pts',(0.0816229647808132,2.41176753123623,
10.0883399444388));
#43035=CARTESIAN_POINT('Ctrl Pts',(0.082330285709921,2.41158151591081,10.0882950245047));
#43036=CARTESIAN_POINT('Ctrl Pts',(0.0826937540325095,2.41148524851829,
10.0882719103474));
#43037=CARTESIAN_POINT('Ctrl Pts',(0.0835676497070665,2.41125215309455,
10.0882162606517));
#43038=CARTESIAN_POINT('Ctrl Pts',(0.0840779093554974,2.4111147055937,10.0881837050567));
#43039=CARTESIAN_POINT('Ctrl Pts',(0.0856408400567726,2.41068957661684,
10.0880837946781));
#43040=CARTESIAN_POINT('Ctrl Pts',(0.0866923817143451,2.41039780509801,
10.0880163071685));
#43041=CARTESIAN_POINT('Ctrl Pts',(0.0991974009266791,2.40685953340229,
10.0872105065631));
#43042=CARTESIAN_POINT('Ctrl Pts',(0.11046261599593,2.40298654826912,10.0864517047593));
#43043=CARTESIAN_POINT('Ctrl Pts',(0.145614598909193,2.38868000602228,10.083974147244));
#43044=CARTESIAN_POINT('Ctrl Pts',(0.168461385669334,2.37597139833511,10.0821865246162));
#43045=CARTESIAN_POINT('Ctrl Pts',(0.198709220412049,2.35397785761062,10.079683643709));
#43046=CARTESIAN_POINT('Ctrl Pts',(0.207534718826404,2.34681877113475,10.0789356189322));
#43047=CARTESIAN_POINT('Ctrl Pts',(0.217123610877008,2.33816160703279,10.0781183174426));
#43048=CARTESIAN_POINT('Ctrl Pts',(0.218274934662435,2.33710686746058,10.0780201100507));
#43049=CARTESIAN_POINT('Ctrl Pts',(0.21972132695564,2.33576234849268,10.0778966898337));
#43050=CARTESIAN_POINT('Ctrl Pts',(0.220023539461164,2.33548033585304,10.0778708997022));
#43051=CARTESIAN_POINT('Ctrl Pts',(0.220504597472854,2.33502969713769,10.0778298446499));
#43052=CARTESIAN_POINT('Ctrl Pts',(0.220683792803222,2.33486144774793,10.0778145509501));
#43053=CARTESIAN_POINT('Ctrl Pts',(0.221022296633268,2.33454289157154,10.0777856600161));
#43054=CARTESIAN_POINT('Ctrl Pts',(0.221181643081175,2.33439262863835,10.0777720596704));
#43055=CARTESIAN_POINT('Ctrl Pts',(0.221544775322975,2.33404949664125,10.0777410651604));
#43056=CARTESIAN_POINT('Ctrl Pts',(0.221748462158523,2.33385652413968,10.0777236791637));
#43057=CARTESIAN_POINT('Ctrl Pts',(0.222370035760419,2.33326610429487,10.0776706207997));
#43058=CARTESIAN_POINT('Ctrl Pts',(0.222787110817126,2.33286779829533,10.0776350145374));
#43059=CARTESIAN_POINT('Ctrl Pts',(0.225817231897343,2.32995844563729,10.0773762784198));
#43060=CARTESIAN_POINT('Ctrl Pts',(0.228388957410542,2.32740447611739,10.0771564087011));
#43061=CARTESIAN_POINT('Ctrl Pts',(0.252283850739779,2.30286018615077,10.0751044007694));
#43062=CARTESIAN_POINT('Ctrl Pts',(0.270415585602447,2.27797584412988,10.0734648398319));
#43063=CARTESIAN_POINT('Ctrl Pts',(0.290098639794037,2.24083261814496,10.07107543535));
#43064=CARTESIAN_POINT('Ctrl Pts',(0.294896447858766,2.23048791291838,10.0704170032287));
#43065=CARTESIAN_POINT('Ctrl Pts',(0.300463205362311,2.21660085570194,10.069528388724));
#43066=CARTESIAN_POINT('Ctrl Pts',(0.301735221928695,2.21326849373299,10.0693148477026));
#43067=CARTESIAN_POINT('Ctrl Pts',(0.303461710412642,2.20850991946455,10.0690091700895));
#43068=CARTESIAN_POINT('Ctrl Pts',(0.303961988309701,2.2071005222001,10.0689185433705));
#43069=CARTESIAN_POINT('Ctrl Pts',(0.304710566600814,2.20494410801539,10.0687797231434));
#43070=CARTESIAN_POINT('Ctrl Pts',(0.304965974502683,2.20419956614008,10.0687317641293));
#43071=CARTESIAN_POINT('Ctrl Pts',(0.305426453901111,2.20284102260284,10.0686441991254));
#43072=CARTESIAN_POINT('Ctrl Pts',(0.305632408491317,2.20222732287784,10.0686046224626));
#43073=CARTESIAN_POINT('Ctrl Pts',(0.305971105406613,2.20120790732546,10.068538846021));
#43074=CARTESIAN_POINT('Ctrl Pts',(0.306104893788574,2.20080253888099,10.0685126808088));
#43075=CARTESIAN_POINT('Ctrl Pts',(0.306360305359024,2.20002346411796,10.0684623756392));
#43076=CARTESIAN_POINT('Ctrl Pts',(0.306482051215201,2.19964979856769,10.068438239776));
#43077=CARTESIAN_POINT('Ctrl Pts',(0.306757585183341,2.19879884116886,10.0683832556798));
#43078=CARTESIAN_POINT('Ctrl Pts',(0.306910943129306,2.19832141204627,10.0683523933568));
#43079=CARTESIAN_POINT('Ctrl Pts',(0.307363350304337,2.1969016201845,10.0682605728334));
#43080=CARTESIAN_POINT('Ctrl Pts',(0.307659175984739,2.19595824353433,10.0681995089459));
#43081=CARTESIAN_POINT('Ctrl Pts',(0.309678354745062,2.18941383427287,10.0677755034296));
#43082=CARTESIAN_POINT('Ctrl Pts',(0.311252901154919,2.1837683794723,10.0674077242376));
#43083=CARTESIAN_POINT('Ctrl Pts',(0.312961178244143,2.17692785680348,10.0669592815705));
#43084=CARTESIAN_POINT('Ctrl Pts',(0.313243345746615,2.17577071021195,10.0668833282047));
#43085=CARTESIAN_POINT('Ctrl Pts',(0.320891644032214,2.14363263204022,10.0647711886882));
#43086=CARTESIAN_POINT('Ctrl Pts',(0.3236306162865,2.11173451208725,10.0625809613985));
#43087=CARTESIAN_POINT('Ctrl Pts',(0.321114975689018,2.07134975382454,10.0598775156433));
#43088=CARTESIAN_POINT('Ctrl Pts',(0.320232533196219,2.06276005330485,10.059308253438));
#43089=CARTESIAN_POINT('Ctrl Pts',(0.318509799473951,2.05075680522363,10.05852968785));
#43090=CARTESIAN_POINT('Ctrl Pts',(0.317957157957463,2.04730623594852,10.0583078698918));
#43091=CARTESIAN_POINT('Ctrl Pts',(0.317256915639011,2.04334753819743,10.0580562149974));
#43092=CARTESIAN_POINT('Ctrl Pts',(0.317164086560611,2.04283012896168,10.0580233790373));
#43093=CARTESIAN_POINT('Ctrl Pts',(0.317021627833639,2.04204712162714,10.0579737745547));
#43094=CARTESIAN_POINT('Ctrl Pts',(0.316972930028647,2.04178135817173,10.0579569532872));
#43095=CARTESIAN_POINT('Ctrl Pts',(0.316888114847453,2.04132174871779,10.0579278893369));
#43096=CARTESIAN_POINT('Ctrl Pts',(0.31685215384638,2.04112787494252,10.0579156377147));
#43097=CARTESIAN_POINT('Ctrl Pts',(0.316776733186256,2.04072333618625,10.0578900905857));
#43098=CARTESIAN_POINT('Ctrl Pts',(0.316737241427864,2.04051267820464,10.0578767969841));
#43099=CARTESIAN_POINT('Ctrl Pts',(0.31663961497295,2.03999476992276,10.0578441378509));
#43100=CARTESIAN_POINT('Ctrl Pts',(0.316581243038617,2.03968756376258,10.05782478591));
#43101=CARTESIAN_POINT('Ctrl Pts',(0.316352932096357,2.03849544797276,10.0577497679926));
#43102=CARTESIAN_POINT('Ctrl Pts',(0.316179727128979,2.03761115673253,10.0576942866655));
#43103=CARTESIAN_POINT('Ctrl Pts',(0.312891692424119,2.02118965111645,10.0566668710805));
#43104=CARTESIAN_POINT('Ctrl Pts',(0.308638297132342,2.00589987146619,10.0557578937949));
#43105=CARTESIAN_POINT('Ctrl Pts',(0.296240964791316,1.97141144097039,10.0536919400521));
#43106=CARTESIAN_POINT('Ctrl Pts',(0.287327840234406,1.95256718710399,10.0525485720161));
#43107=CARTESIAN_POINT('Ctrl Pts',(0.270390434237204,1.92421695238188,10.050653856929));
#43108=CARTESIAN_POINT('Ctrl Pts',(0.263528127440062,1.91408727580639,10.0499375451591));
#43109=CARTESIAN_POINT('Ctrl Pts',(0.255252176139032,1.90325273054783,10.049113611773));
#43110=CARTESIAN_POINT('Ctrl Pts',(0.254389440072215,1.90213849757197,10.0490281673853));
#43111=CARTESIAN_POINT('Ctrl Pts',(0.252855227652787,1.9001836671427,10.0488769834624));
#43112=CARTESIAN_POINT('Ctrl Pts',(0.252186793683828,1.89934070149784,10.0488113648431));
#43113=CARTESIAN_POINT('Ctrl Pts',(0.251194974773575,1.89810269719179,10.0487143599643));
#43114=CARTESIAN_POINT('Ctrl Pts',(0.250874847083431,1.89770504868175,10.0486831044575));
#43115=CARTESIAN_POINT('Ctrl Pts',(0.250318364242457,1.89701716267315,10.0486288660998));
#43116=CARTESIAN_POINT('Ctrl Pts',(0.250082445113057,1.89672657239415,10.048605900858));
#43117=CARTESIAN_POINT('Ctrl Pts',(0.24961213210839,1.89614932857523,10.0485601759538));
#43118=CARTESIAN_POINT('Ctrl Pts',(0.24937774934492,1.89586266665327,10.0485374167606));
#43119=CARTESIAN_POINT('Ctrl Pts',(0.248821359932251,1.89518456263703,10.0484834557578));
#43120=CARTESIAN_POINT('Ctrl Pts',(0.248498923536025,1.8947934758896,10.0484522365249));
#43121=CARTESIAN_POINT('Ctrl Pts',(0.247364916840373,1.89342461853874,10.0483426192306));
#43122=CARTESIAN_POINT('Ctrl Pts',(0.246548495519373,1.89245089835831,10.0482640234958));
#43123=CARTESIAN_POINT('Ctrl Pts',(0.234871704821368,1.87869047620885,10.0471443863688));
#43124=CARTESIAN_POINT('Ctrl Pts',(0.223036685775311,1.86676814607881,10.0460619688402));
#43125=CARTESIAN_POINT('Ctrl Pts',(0.194469139846209,1.84216067223422,10.0435594611397));
#43126=CARTESIAN_POINT('Ctrl Pts',(0.177315769270858,1.83007706165624,10.0421266493883));
#43127=CARTESIAN_POINT('Ctrl Pts',(0.148177984968654,1.81353428856733,10.039883571533));
#43128=CARTESIAN_POINT('Ctrl Pts',(0.136886513768707,1.80797006349781,10.0390560840142));
#43129=CARTESIAN_POINT('Ctrl Pts',(0.124659281116331,1.80281029815124,10.0382236044869));
#43130=CARTESIAN_POINT('Ctrl Pts',(0.12402034133007,1.80254309520393,10.0381802818811));
#43131=CARTESIAN_POINT('Ctrl Pts',(0.123101140871952,1.80216216457543,10.0381182185526));
#43132=CARTESIAN_POINT('Ctrl Pts',(0.122821579338308,1.80204677087669,10.038099377624));
#43133=CARTESIAN_POINT('Ctrl Pts',(0.122336342135631,1.80184728008658,10.0380667360205));
#43134=CARTESIAN_POINT('Ctrl Pts',(0.122130741510867,1.80176300199657,10.0380529242923));
#43135=CARTESIAN_POINT('Ctrl Pts',(0.121733206233193,1.80160052768474,10.0380262555862));
#43136=CARTESIAN_POINT('Ctrl Pts',(0.121541283793706,1.80152230416289,10.0380133969313));
#43137=CARTESIAN_POINT('Ctrl Pts',(0.121083594931224,1.80133627452097,10.0379827711138));
#43138=CARTESIAN_POINT('Ctrl Pts',(0.12081775924943,1.80122863770115,10.0379650142728));
#43139=CARTESIAN_POINT('Ctrl Pts',(0.119871906633108,1.800847130967,10.0379019448621));
#43140=CARTESIAN_POINT('Ctrl Pts',(0.119191092694471,1.80057522397447,10.0378567503022));
#43141=CARTESIAN_POINT('Ctrl Pts',(0.109104809388386,1.79658676431529,10.0371900931612));
#43142=CARTESIAN_POINT('Ctrl Pts',(0.0995293102140311,1.79331218692966,
10.0365944258341));
#43143=CARTESIAN_POINT('Ctrl Pts',(0.0640982872391286,1.78303059544257,
10.0344702615992));
#43144=CARTESIAN_POINT('Ctrl Pts',(0.0375515841675513,1.77880186724202,
10.0330215100762));
#43145=CARTESIAN_POINT('Ctrl Pts',(0.00305160629579006,1.77764653690111,
10.0310410290353));
#43146=CARTESIAN_POINT('Ctrl Pts',(-0.00468940555814354,1.7776662218976,
10.030591126381));
#43147=CARTESIAN_POINT('Ctrl Pts',(-0.0185481650303265,1.77820079400813,
10.0297701632972));
#43148=CARTESIAN_POINT('Ctrl Pts',(-0.0246661630684275,1.77861186061775,
10.0294023306781));
#43149=CARTESIAN_POINT('Ctrl Pts',(-0.0317006599856948,1.77928654402572,
10.0289719121467));
#43150=CARTESIAN_POINT('Ctrl Pts',(-0.0326324956545053,1.77938001795773,
10.0289147450226));
#43151=CARTESIAN_POINT('Ctrl Pts',(-0.0340451421202877,1.77952794497241,
10.0288278470609));
#43152=CARTESIAN_POINT('Ctrl Pts',(-0.0345262650427791,1.77957942205013,
10.0287982099866));
#43153=CARTESIAN_POINT('Ctrl Pts',(-0.0353591133794374,1.77967042909022,
10.0287468348102));
#43154=CARTESIAN_POINT('Ctrl Pts',(-0.0357108939321741,1.77970945541402,
10.0287251126152));
#43155=CARTESIAN_POINT('Ctrl Pts',(-0.0364405615694661,1.77979162135027,
10.0286800097669));
#43156=CARTESIAN_POINT('Ctrl Pts',(-0.0368184378454589,1.77983485055728,
10.0286566263195));
#43157=CARTESIAN_POINT('Ctrl Pts',(-0.0377369484826849,1.77994157617379,
10.0285997245305));
#43158=CARTESIAN_POINT('Ctrl Pts',(-0.0382774987910083,1.78000577345302,
10.0285661841251));
#43159=CARTESIAN_POINT('Ctrl Pts',(-0.0403094183755431,1.78025231220636,
10.0284399041278));
#43160=CARTESIAN_POINT('Ctrl Pts',(-0.041799651003758,1.78044371057293,
10.0283468790925));
#43161=CARTESIAN_POINT('Ctrl Pts',(-0.0682995418918661,1.78403576837955,
10.026685214084));
#43162=CARTESIAN_POINT('Ctrl Pts',(-0.0928202254584118,1.7903516388729,
10.0250186242543));
#43163=CARTESIAN_POINT('Ctrl Pts',(-0.130982357759135,1.80512535971778,
10.0222545370275));
#43164=CARTESIAN_POINT('Ctrl Pts',(-0.145183608765201,1.8118521525183,10.0211863666889));
#43165=CARTESIAN_POINT('Ctrl Pts',(-0.164360709565477,1.8227149293279,10.0197281524638));
#43166=CARTESIAN_POINT('Ctrl Pts',(-0.169789601093856,1.82600555492843,
10.0193136117893));
#43167=CARTESIAN_POINT('Ctrl Pts',(-0.177618913456452,1.83107329735673,
10.0187169725749));
#43168=CARTESIAN_POINT('Ctrl Pts',(-0.180097254258496,1.832726674774,10.0185282949015));
#43169=CARTESIAN_POINT('Ctrl Pts',(-0.182968213115632,1.83470005054465,
10.018310278956));
#43170=CARTESIAN_POINT('Ctrl Pts',(-0.183383339477102,1.83498682862508,
10.0182787686229));
#43171=CARTESIAN_POINT('Ctrl Pts',(-0.184016087661491,1.83542614314818,
10.0182307626915));
#43172=CARTESIAN_POINT('Ctrl Pts',(-0.184234194730501,1.83557797417591,
10.0182142193399));
#43173=CARTESIAN_POINT('Ctrl Pts',(-0.184629083903442,1.83585359442723,
10.0181842751113));
#43174=CARTESIAN_POINT('Ctrl Pts',(-0.184805928771692,1.83597729095465,
10.0181708680005));
#43175=CARTESIAN_POINT('Ctrl Pts',(-0.18516437036028,1.83622854433962,10.0181436994989));
#43176=CARTESIAN_POINT('Ctrl Pts',(-0.185345958793273,1.83635611057367,
10.0181299388684));
#43177=CARTESIAN_POINT('Ctrl Pts',(-0.185868051887956,1.83672368799987,
10.0180903834698));
#43178=CARTESIAN_POINT('Ctrl Pts',(-0.186208224727613,1.83696417312192,
10.018064621225));
#43179=CARTESIAN_POINT('Ctrl Pts',(-0.187698832711067,1.83802229894201,
10.0179517740247));
#43180=CARTESIAN_POINT('Ctrl Pts',(-0.188844378291509,1.83884684835942,
10.0178651566286));
#43181=CARTESIAN_POINT('Ctrl Pts',(-0.210017328042146,1.85429904328435,
10.0162654589097));
#43182=CARTESIAN_POINT('Ctrl Pts',(-0.228299263844469,1.87118540841104,
10.0149008792548));
#43183=CARTESIAN_POINT('Ctrl Pts',(-0.260594661000986,1.90878193117505,
10.0121278900786));
#43184=CARTESIAN_POINT('Ctrl Pts',(-0.274504581900125,1.92935153722198,
10.0107256188471));
#43185=CARTESIAN_POINT('Ctrl Pts',(-0.28645522827859,1.95233176310571,10.009150554318));
#43186=CARTESIAN_POINT('Ctrl Pts',(-0.286981889916914,1.95335791599553,
10.009080225143));
#43187=CARTESIAN_POINT('Ctrl Pts',(-0.287741048973956,1.95485682283767,
10.0089774917182));
#43188=CARTESIAN_POINT('Ctrl Pts',(-0.287977917823889,1.95532736270456,
10.0089452409794));
#43189=CARTESIAN_POINT('Ctrl Pts',(-0.288391061362612,1.95615310711098,
10.0088886429157));
#43190=CARTESIAN_POINT('Ctrl Pts',(-0.288567836625784,1.95650806109568,
10.0088643131732));
#43191=CARTESIAN_POINT('Ctrl Pts',(-0.288909421908162,1.9571971276497,10.0088170808077));
#43192=CARTESIAN_POINT('Ctrl Pts',(-0.289074308655236,1.95753120168791,
10.0087941809118));
#43193=CARTESIAN_POINT('Ctrl Pts',(-0.28951076963833,1.95841938452501,10.0087332961776));
#43194=CARTESIAN_POINT('Ctrl Pts',(-0.289781331302907,1.95897398667369,
10.0086952761154));
#43195=CARTESIAN_POINT('Ctrl Pts',(-0.290737243225128,1.9609477979679,10.0085599536462));
#43196=CARTESIAN_POINT('Ctrl Pts',(-0.291413765317225,1.96237123581862,
10.008462345224));
#43197=CARTESIAN_POINT('Ctrl Pts',(-0.302478602737599,1.98609961421407,
10.006834753535));
#43198=CARTESIAN_POINT('Ctrl Pts',(-0.310287119609825,2.0095123061569,10.0052121268332));
#43199=CARTESIAN_POINT('Ctrl Pts',(-0.318653451112574,2.04923482588306,
10.0024717411476));
#43200=CARTESIAN_POINT('Ctrl Pts',(-0.320780473736779,2.06511389630568,
10.001382024296));
#43201=CARTESIAN_POINT('Ctrl Pts',(-0.322090856425951,2.08740249954927,
9.99990349791909));
#43202=CARTESIAN_POINT('Ctrl Pts',(-0.322276135752653,2.09372942164882,
9.99948967543666));
#43203=CARTESIAN_POINT('Ctrl Pts',(-0.322274427660535,2.1032036216054,9.99888259274212));
#43204=CARTESIAN_POINT('Ctrl Pts',(-0.3222278084343,2.10634911052634,9.99868311965728));
#43205=CARTESIAN_POINT('Ctrl Pts',(-0.322119078848428,2.11003852156452,
9.99845198836603));
#43206=CARTESIAN_POINT('Ctrl Pts',(-0.322101635213386,2.110583452961,9.99841792256334));
#43207=CARTESIAN_POINT('Ctrl Pts',(-0.322073210953433,2.11140612405797,
9.99836660649659));
#43208=CARTESIAN_POINT('Ctrl Pts',(-0.32206325386039,2.11168389464756,9.99834929923402));
#43209=CARTESIAN_POINT('Ctrl Pts',(-0.322044818626816,2.11218024084605,
9.9983184079959));
#43210=CARTESIAN_POINT('Ctrl Pts',(-0.322036477318266,2.11239882046523,
9.99830481633854));
#43211=CARTESIAN_POINT('Ctrl Pts',(-0.322018227529482,2.11286460140716,
9.99827587925237));
#43212=CARTESIAN_POINT('Ctrl Pts',(-0.322008256967211,2.11311179913358,
9.99826053739987));
#43213=CARTESIAN_POINT('Ctrl Pts',(-0.321980571357155,2.11377911857146,
9.99821916287334));
#43214=CARTESIAN_POINT('Ctrl Pts',(-0.321962318626598,2.11419921932475,
9.99819316044732));
#43215=CARTESIAN_POINT('Ctrl Pts',(-0.321868808545783,2.11625848123244,
9.99806591283297));
#43216=CARTESIAN_POINT('Ctrl Pts',(-0.321781853616707,2.11789712482943,
9.99796531443234));
#43217=CARTESIAN_POINT('Ctrl Pts',(-0.321211848651136,2.12728334796018,
9.9973924903088));
#43218=CARTESIAN_POINT('Ctrl Pts',(-0.32046147700495,2.13501279660081,9.99693407346861));
#43219=CARTESIAN_POINT('Ctrl Pts',(-0.317373799432371,2.15810681107936,
9.99558448835812));
#43220=CARTESIAN_POINT('Ctrl Pts',(-0.314204109480535,2.17333738151107,
9.99472060000492));
#43221=CARTESIAN_POINT('Ctrl Pts',(-0.303005055353753,2.2126565419427,9.99243493162794));
#43222=CARTESIAN_POINT('Ctrl Pts',(-0.293212390040804,2.23612420541474,
9.99100641944024));
#43223=CARTESIAN_POINT('Ctrl Pts',(-0.2799927778458,2.25958617438035,9.98937395786617));
#43224=CARTESIAN_POINT('Ctrl Pts',(-0.279202197387143,2.26096532400603,
9.98927723262625));
#43225=CARTESIAN_POINT('Ctrl Pts',(-0.278089489355844,2.26287355552748,
9.98914231194009));
#43226=CARTESIAN_POINT('Ctrl Pts',(-0.277775982250721,2.26340765850033,
9.98910442899438));
#43227=CARTESIAN_POINT('Ctrl Pts',(-0.277271204202263,2.26426196778395,
9.98904364143787));
#43228=CARTESIAN_POINT('Ctrl Pts',(-0.277080912458586,2.26458275331653,
9.98902077249597));
#43229=CARTESIAN_POINT('Ctrl Pts',(-0.276687281689178,2.26524370134464,
9.98897356253363));
#43230=CARTESIAN_POINT('Ctrl Pts',(-0.27648387129758,2.26558382044372,9.98894921893539));
#43231=CARTESIAN_POINT('Ctrl Pts',(-0.276009377259191,2.26637390192887,
9.98889255370635));
#43232=CARTESIAN_POINT('Ctrl Pts',(-0.275737820354292,2.26682357746763,
9.98886021479901));
#43233=CARTESIAN_POINT('Ctrl Pts',(-0.274870614785753,2.26825169509022,
9.98875722898129));
#43234=CARTESIAN_POINT('Ctrl Pts',(-0.274270853349249,2.26922761808348,
9.98868643123666));
#43235=CARTESIAN_POINT('Ctrl Pts',(-0.262187115022523,2.28865711950061,
9.98726841125085));
#43236=CARTESIAN_POINT('Ctrl Pts',(-0.248873077788396,2.30590152937929,
9.98584990813407));
#43237=CARTESIAN_POINT('Ctrl Pts',(-0.214830239536102,2.3418265075295,9.98252691750616));
#43238=CARTESIAN_POINT('Ctrl Pts',(-0.1932073726006,2.35942851485318,9.9806075647171));
#43239=CARTESIAN_POINT('Ctrl Pts',(-0.168344444614696,2.37481536929332,
9.97875874962293));
#43240=CARTESIAN_POINT('Ctrl Pts',(-0.167088357873659,2.37558087758689,
9.97866625120993));
#43241=CARTESIAN_POINT('Ctrl Pts',(-0.16546409441007,2.37655557896717,9.97854784476274));
#43242=CARTESIAN_POINT('Ctrl Pts',(-0.165100711778827,2.37677266803609,
9.97852143183302));
#43243=CARTESIAN_POINT('Ctrl Pts',(-0.164523730722105,2.37711582266043,
9.97847961673739));
#43244=CARTESIAN_POINT('Ctrl Pts',(-0.164310414269465,2.37724235770004,
9.9784641839265));
#43245=CARTESIAN_POINT('Ctrl Pts',(-0.163927606569691,2.37746883454628,
9.97843653708687));
#43246=CARTESIAN_POINT('Ctrl Pts',(-0.163758171114338,2.37756886665066,
9.97842431716883));
#43247=CARTESIAN_POINT('Ctrl Pts',(-0.163359199415934,2.37780392097325,
9.97839558246649));
#43248=CARTESIAN_POINT('Ctrl Pts',(-0.163129587683745,2.37793881370778,
9.97837907623125));
#43249=CARTESIAN_POINT('Ctrl Pts',(-0.162462209276824,2.37832977453201,
9.97833118872053));
#43250=CARTESIAN_POINT('Ctrl Pts',(-0.16202400248376,2.37858509554819,9.97829985604492));
#43251=CARTESIAN_POINT('Ctrl Pts',(-0.158957264853038,2.38036224546542,
9.97808133759348));
#43252=CARTESIAN_POINT('Ctrl Pts',(-0.156307825888829,2.38184794821856,
9.97789644576719));
#43253=CARTESIAN_POINT('Ctrl Pts',(-0.148045826866276,2.38632861178732,
9.97733058097489));
#43254=CARTESIAN_POINT('Ctrl Pts',(-0.14236503606082,2.38919517351615,9.97695654454989));
#43255=CARTESIAN_POINT('Ctrl Pts',(-0.12228275084459,2.39859350017305,9.97567319543483));
#43256=CARTESIAN_POINT('Ctrl Pts',(-0.10748807371349,2.40423268843545,9.97479491325108));
#43257=CARTESIAN_POINT('Ctrl Pts',(-0.0683187311445838,2.41594662720813,
9.97250877154913));
#43258=CARTESIAN_POINT('Ctrl Pts',(-0.0435470809002119,2.42030160167511,
9.97109339465884));
#43259=CARTESIAN_POINT('Ctrl Pts',(-0.0170441859333898,2.42182738383034,
9.96948302173576));
#43260=CARTESIAN_POINT('Ctrl Pts',(-0.0155649931259492,2.42190231458012,
9.96939286242818));
#43261=CARTESIAN_POINT('Ctrl Pts',(-0.0135447902681954,2.4219906940448,
9.9692693284925));
#43262=CARTESIAN_POINT('Ctrl Pts',(-0.0130041691089597,2.422012981066,9.96923623090867));
#43263=CARTESIAN_POINT('Ctrl Pts',(-0.0120843380306304,2.42204858077036,
9.96917985031591));
#43264=CARTESIAN_POINT('Ctrl Pts',(-0.0117051547589277,2.42206258545804,
9.96915658902747));
#43265=CARTESIAN_POINT('Ctrl Pts',(-0.0109719679962917,2.42208836831021,
9.96911157320205));
#43266=CARTESIAN_POINT('Ctrl Pts',(-0.0106179678933904,2.42210023259645,
9.96908982139554));
#43267=CARTESIAN_POINT('Ctrl Pts',(-0.00977827451479799,2.42212698907843,
9.96903818493204));
#43268=CARTESIAN_POINT('Ctrl Pts',(-0.0092925667307152,2.42214136639785,
9.9690082841862));
#43269=CARTESIAN_POINT('Ctrl Pts',(-0.00786082108146649,2.42218050642356,
9.96892004764882));
#43270=CARTESIAN_POINT('Ctrl Pts',(-0.0069147106419934,2.42220220044805,
9.96886161585609));
#43271=CARTESIAN_POINT('Ctrl Pts',(0.000430746176232562,2.42233826149321,
9.96840697726688));
#43272=CARTESIAN_POINT('Ctrl Pts',(0.00683172553678939,2.42226612979754,
9.9680049603652));
#43273=CARTESIAN_POINT('Ctrl Pts',(0.0164802454951995,2.42186982671293,
9.9673895424762));
#43274=CARTESIAN_POINT('Ctrl Pts',(0.0197322176373569,2.42168683875623,
9.9671805066665));
#43275=CARTESIAN_POINT('Ctrl Pts',(0.0309153723111586,2.42088735575775,
9.9664560929486));
#43276=CARTESIAN_POINT('Ctrl Pts',(0.0388257315951886,2.42002656552045,
9.9659339414994));
#43277=CARTESIAN_POINT('Ctrl Pts',(0.0743421798614234,2.41482556262928,
9.96354939349386));
#43278=CARTESIAN_POINT('Ctrl Pts',(0.101342683735276,2.40719937007033,9.96161364461138));
#43279=CARTESIAN_POINT('Ctrl Pts',(0.127994942158417,2.3957694955005,9.95972886991709));
#43280=CARTESIAN_POINT('Ctrl Pts',(0.128967281588405,2.39534681312629,9.95966016489659));
#43281=CARTESIAN_POINT('Ctrl Pts',(0.130431308069238,2.39470178256397,9.95955682089262));
#43282=CARTESIAN_POINT('Ctrl Pts',(0.130924542684925,2.39448298915511,9.95952202179467));
#43283=CARTESIAN_POINT('Ctrl Pts',(0.134921117966737,2.39269812688596,9.95924020977094));
#43284=CARTESIAN_POINT('Ctrl Pts',(0.138396974080169,2.39107075145244,9.95899609736042));
#43285=CARTESIAN_POINT('Ctrl Pts',(0.142369733439022,2.38912346597851,9.95871892385743));
#43286=CARTESIAN_POINT('Ctrl Pts',(0.142895649236577,2.38886390051554,9.95868226907393));
#43287=CARTESIAN_POINT('Ctrl Pts',(0.143673856950674,2.38847717114101,9.95862808930645));
#43288=CARTESIAN_POINT('Ctrl Pts',(0.143926691189009,2.38835111063675,9.9586104959348));
#43289=CARTESIAN_POINT('Ctrl Pts',(0.144375441830021,2.38812663099788,9.95857928668488));
#43290=CARTESIAN_POINT('Ctrl Pts',(0.144571423523204,2.38802834443051,9.95856566249799));
#43291=CARTESIAN_POINT('Ctrl Pts',(0.144985921345089,2.38781994043295,9.95853685987343));
#43292=CARTESIAN_POINT('Ctrl Pts',(0.145204411796217,2.38770977441683,9.95852168459812));
#43293=CARTESIAN_POINT('Ctrl Pts',(0.145787232609275,2.38741507479854,9.95848122335879));
#43294=CARTESIAN_POINT('Ctrl Pts',(0.146151339539563,2.38723009655759,9.95845596538122));
#43295=CARTESIAN_POINT('Ctrl Pts',(0.147829914123303,2.38637330752127,9.9583396085866));
#43296=CARTESIAN_POINT('Ctrl Pts',(0.149140134923043,2.38569314853776,9.9582490275766));
#43297=CARTESIAN_POINT('Ctrl Pts',(0.159581464332736,2.38018146177653,9.95752874655522));
#43298=CARTESIAN_POINT('Ctrl Pts',(0.168481143155382,2.37492189206595,9.95692440920953));
#43299=CARTESIAN_POINT('Ctrl Pts',(0.201372335738656,2.35328540411384,9.9546691702936));
#43300=CARTESIAN_POINT('Ctrl Pts',(0.223363077614642,2.33412261094557,9.95310233313227));
#43301=CARTESIAN_POINT('Ctrl Pts',(0.243895946659408,2.31066678998633,9.95129085454785));
#43302=CARTESIAN_POINT('Ctrl Pts',(0.245285482959955,2.30904726923819,9.95116632754694));
#43303=CARTESIAN_POINT('Ctrl Pts',(0.247781625529479,2.3060788327349,9.95093895117049));
#43304=CARTESIAN_POINT('Ctrl Pts',(0.248893562213517,2.30473449582485,9.95083629517814));
#43305=CARTESIAN_POINT('Ctrl Pts',(0.254058750345577,2.29838548908786,9.95035280385406));
#43306=CARTESIAN_POINT('Ctrl Pts',(0.257972088933788,2.29326935456872,9.94996699589042));
#43307=CARTESIAN_POINT('Ctrl Pts',(0.262330314866976,2.28720321143833,9.94951237937307));
#43308=CARTESIAN_POINT('Ctrl Pts',(0.262927260730678,2.28636386988115,9.94944953859246));
#43309=CARTESIAN_POINT('Ctrl Pts',(0.263809696536688,2.28511043351522,9.94935578133985));
#43310=CARTESIAN_POINT('Ctrl Pts',(0.264098261236531,2.28469850294542,9.94932498267308));
#43311=CARTESIAN_POINT('Ctrl Pts',(0.26461068953753,2.2839633474271,9.94927004136994));
#43312=CARTESIAN_POINT('Ctrl Pts',(0.264834928629913,2.28364038441891,9.94924591312216));
#43313=CARTESIAN_POINT('Ctrl Pts',(0.265305929811726,2.28295936250936,9.94919505138741));
#43314=CARTESIAN_POINT('Ctrl Pts',(0.265552559159887,2.2826012131498,9.94916831291676));
#43315=CARTESIAN_POINT('Ctrl Pts',(0.266192951426772,2.28166720918872,9.94909860728448));
#43316=CARTESIAN_POINT('Ctrl Pts',(0.266585569229281,2.28109057554214,9.94905559682116));
#43317=CARTESIAN_POINT('Ctrl Pts',(0.268303054001373,2.27855043399833,9.94886623262979));
#43318=CARTESIAN_POINT('Ctrl Pts',(0.269608095662722,2.27657366887186,9.94871913397827));
#43319=CARTESIAN_POINT('Ctrl Pts',(0.278847560161128,2.26223725939757,9.94765398310607));
#43320=CARTESIAN_POINT('Ctrl Pts',(0.285949539159132,2.24936412936613,9.94670522712979));
#43321=CARTESIAN_POINT('Ctrl Pts',(0.301082257611119,2.21686949364581,9.94433090147214));
#43322=CARTESIAN_POINT('Ctrl Pts',(0.308104539559079,2.19685293314543,9.94288294783857));
#43323=CARTESIAN_POINT('Ctrl Pts',(0.315430119668036,2.16678882704539,9.94080898680035));
#43324=CARTESIAN_POINT('Ctrl Pts',(0.317312540636782,2.15718123311942,9.94016140148789));
#43325=CARTESIAN_POINT('Ctrl Pts',(0.319260964792439,2.14410665541701,9.93931264677654));
#43326=CARTESIAN_POINT('Ctrl Pts',(0.319712706564265,2.14070317303685,9.93909466106959));
#43327=CARTESIAN_POINT('Ctrl Pts',(0.320175631422935,2.13672958433276,9.93884410324045));
#43328=CARTESIAN_POINT('Ctrl Pts',(0.320239777906501,2.13616603351734,9.93880866027399));
#43329=CARTESIAN_POINT('Ctrl Pts',(0.320333222918022,2.13532533908251,9.93875592753803));
#43330=CARTESIAN_POINT('Ctrl Pts',(0.320363649842978,2.13504832588064,9.93873857454801));
#43331=CARTESIAN_POINT('Ctrl Pts',(0.320417326081064,2.13455373571113,9.9387076328236));
#43332=CARTESIAN_POINT('Ctrl Pts',(0.320440713096714,2.13433617473823,9.93869403630715));
#43333=CARTESIAN_POINT('Ctrl Pts',(0.320490022249684,2.13387303123522,9.93866512231968));
#43334=CARTESIAN_POINT('Ctrl Pts',(0.320515883628373,2.13362744339926,9.93864980835655));
#43335=CARTESIAN_POINT('Ctrl Pts',(0.320584808286457,2.13296560988164,9.9386085868841));
#43336=CARTESIAN_POINT('Ctrl Pts',(0.320627343347362,2.13254930785193,9.93858270923863));
#43337=CARTESIAN_POINT('Ctrl Pts',(0.320826191888578,2.13056490762895,9.93845959640086));
#43338=CARTESIAN_POINT('Ctrl Pts',(0.320971816750039,2.12899572502474,9.93836295471556));
#43339=CARTESIAN_POINT('Ctrl Pts',(0.322096081983343,2.11583249258218,9.93755775061893));
#43340=CARTESIAN_POINT('Ctrl Pts',(0.32245780670679,2.10419293988358,9.93688127269676));
#43341=CARTESIAN_POINT('Ctrl Pts',(0.321679383321662,2.07049203399388,9.93496109997406));
#43342=CARTESIAN_POINT('Ctrl Pts',(0.318904246982666,2.04853656503831,9.93375421829145));
#43343=CARTESIAN_POINT('Ctrl Pts',(0.3129719385023,2.02301433285571,9.93226130685605));
#43344=CARTESIAN_POINT('Ctrl Pts',(0.311959850441387,2.01901063427327,9.93202455944491));
#43345=CARTESIAN_POINT('Ctrl Pts',(0.307852385798196,2.00398349729733,9.93112419992008));
#43346=CARTESIAN_POINT('Ctrl Pts',(0.304247572103815,1.99310926153087,9.93044816898485));
#43347=CARTESIAN_POINT('Ctrl Pts',(0.299634031006727,1.98133211799154,9.92967928593688));
#43348=CARTESIAN_POINT('Ctrl Pts',(0.299189610870233,1.98021604680129,9.92960605344678));
#43349=CARTESIAN_POINT('Ctrl Pts',(0.298558116737004,1.97865561832781,9.92950313737762));
#43350=CARTESIAN_POINT('Ctrl Pts',(0.298376265985279,1.97820914678989,9.92947363027879));
#43351=CARTESIAN_POINT('Ctrl Pts',(0.298041504438547,1.97739250567677,9.9294195470382));
#43352=CARTESIAN_POINT('Ctrl Pts',(0.29788890383604,1.97702220931696,9.9293949814364));
#43353=CARTESIAN_POINT('Ctrl Pts',(0.297578944887952,1.97627403369104,9.92934526138899));
#43354=CARTESIAN_POINT('Ctrl Pts',(0.297421556106704,1.97589616790638,9.92932010594664));
#43355=CARTESIAN_POINT('Ctrl Pts',(0.297105031377695,1.9751403020841,9.92926969683701));
#43356=CARTESIAN_POINT('Ctrl Pts',(0.296945892911048,1.97476230394019,9.92924444312115));
#43357=CARTESIAN_POINT('Ctrl Pts',(0.29636080066708,1.97337993184939,9.92915192319876));
#43358=CARTESIAN_POINT('Ctrl Pts',(0.295930472863308,1.97237742748832,9.92908450814562));
#43359=CARTESIAN_POINT('Ctrl Pts',(0.292615373881578,1.96476139892518,9.92856989439813));
#43360=CARTESIAN_POINT('Ctrl Pts',(0.289514524806766,1.95824470859934,9.92811531981475));
#43361=CARTESIAN_POINT('Ctrl Pts',(0.280801322774155,1.94141381685969,9.92690191945861));
#43362=CARTESIAN_POINT('Ctrl Pts',(0.274839909389009,1.93129334741991,9.92613164837258));
#43363=CARTESIAN_POINT('Ctrl Pts',(0.260209445633106,1.90929662481274,9.92436918699135));
#43364=CARTESIAN_POINT('Ctrl Pts',(0.251252856615057,1.89764214254737,9.923371464577));
#43365=CARTESIAN_POINT('Ctrl Pts',(0.233272338496599,1.8772874060257,9.92153798110756));
#43366=CARTESIAN_POINT('Ctrl Pts',(0.224474209971092,1.86842222459683,9.92070216614003));
#43367=CARTESIAN_POINT('Ctrl Pts',(0.215048630320779,1.85996813753457,9.91988317028396));
#43368=CARTESIAN_POINT('Ctrl Pts',(0.214913754662031,1.85984736841161,9.91987146593201));
#43369=CARTESIAN_POINT('Ctrl Pts',(0.211508350184048,1.8568032988135,9.91957633107998));
#43370=CARTESIAN_POINT('Ctrl Pts',(0.208178370920202,1.85394677753,9.91929661495904));
#43371=CARTESIAN_POINT('Ctrl Pts',(0.204326190093038,1.85077651414553,9.91898397836417));
#43372=CARTESIAN_POINT('Ctrl Pts',(0.203860396397636,1.85039535931021,9.91894635344377));
#43373=CARTESIAN_POINT('Ctrl Pts',(0.20317111825768,1.8498345456569,9.91889094225948));
#43374=CARTESIAN_POINT('Ctrl Pts',(0.202948460844892,1.84965387943292,9.91887308357512));
#43375=CARTESIAN_POINT('Ctrl Pts',(0.202554168861857,1.84933481910675,9.91884153111645));
#43376=CARTESIAN_POINT('Ctrl Pts',(0.202382633184889,1.84919630381134,9.91882782852744));
#43377=CARTESIAN_POINT('Ctrl Pts',(0.202024023594359,1.84890733354367,9.91879923285478));
#43378=CARTESIAN_POINT('Ctrl Pts',(0.201836924106067,1.8487569118847,9.91878434219066));
#43379=CARTESIAN_POINT('Ctrl Pts',(0.201347183744103,1.84836407733003,9.91874543981633));
#43380=CARTESIAN_POINT('Ctrl Pts',(0.201044271995156,1.84812200040232,9.91872145239876));
#43381=CARTESIAN_POINT('Ctrl Pts',(0.199743205868219,1.84708607425493,9.9186187362274));
#43382=CARTESIAN_POINT('Ctrl Pts',(0.198740763297477,1.84629759311834,9.9185403878987));
#43383=CARTESIAN_POINT('Ctrl Pts',(0.196105743028156,1.84425019422551,9.91833642652194));
#43384=CARTESIAN_POINT('Ctrl Pts',(0.19446569281328,1.84300093305569,9.91821145293172));
#43385=CARTESIAN_POINT('Ctrl Pts',(0.188257270686234,1.8383653090094,9.91774525227942));
#43386=CARTESIAN_POINT('Ctrl Pts',(0.183611283871766,1.83508413412942,9.91741021433531));
#43387=CARTESIAN_POINT('Ctrl Pts',(0.161238713334929,1.82015526854867,9.91584871759364));
#43388=CARTESIAN_POINT('Ctrl Pts',(0.142476617277192,1.81015254588702,9.91468602094042));
#43389=CARTESIAN_POINT('Ctrl Pts',(0.103897293103256,1.79424265276844,9.9123386514134));
#43390=CARTESIAN_POINT('Ctrl Pts',(0.0842274701162847,1.78825050759077,
9.91116056863902));
#43391=CARTESIAN_POINT('Ctrl Pts',(0.0628509912032709,1.783910433408,9.90983574671813));
#43392=CARTESIAN_POINT('Ctrl Pts',(0.061577117259003,1.78365980376095,9.909756650878));
#43393=CARTESIAN_POINT('Ctrl Pts',(0.059799250334402,1.78332116114134,9.90964604636691));
#43394=CARTESIAN_POINT('Ctrl Pts',(0.0592964977090335,1.78322663831044,
9.90961474521436));
#43395=CARTESIAN_POINT('Ctrl Pts',(0.0584282511968487,1.78306553815482,
9.90956064647477));
#43396=CARTESIAN_POINT('Ctrl Pts',(0.058062862257227,1.78299839485006,9.90953786694847));
#43397=CARTESIAN_POINT('Ctrl Pts',(0.0573066411346103,1.7828607841615,9.90949069474523));
#43398=CARTESIAN_POINT('Ctrl Pts',(0.0569157933064921,1.78279040712664,
9.90946629923456));
#43399=CARTESIAN_POINT('Ctrl Pts',(0.0561412495934787,1.78265241845381,
9.90941792477365));
#43400=CARTESIAN_POINT('Ctrl Pts',(0.0557575591850463,1.78258477980611,
9.90939394673067));
#43401=CARTESIAN_POINT('Ctrl Pts',(0.0545391516424456,1.7823722708823,9.90931775798246));
#43402=CARTESIAN_POINT('Ctrl Pts',(0.053703990584452,1.78222999710527,9.90926546484314));
#43403=CARTESIAN_POINT('Ctrl Pts',(0.0482173738705924,1.78131757238235,
9.90892145735028));
#43404=CARTESIAN_POINT('Ctrl Pts',(0.0435502627541095,1.78064631577146,
9.9086266223099));
#43405=CARTESIAN_POINT('Ctrl Pts',(0.029503215702636,1.77893961102169,9.90773201748767));
#43406=CARTESIAN_POINT('Ctrl Pts',(0.0200915086086435,1.77821355551467,
9.90712286250005));
#43407=CARTESIAN_POINT('Ctrl Pts',(-0.00320482895261495,1.77744239212582,
9.90559179177143));
#43408=CARTESIAN_POINT('Ctrl Pts',(-0.0170859994902055,1.77787937975245,
9.90465868507315));
#43409=CARTESIAN_POINT('Ctrl Pts',(-0.0528572907629566,1.78132444348676,
9.90222793680644));
#43410=CARTESIAN_POINT('Ctrl Pts',(-0.0745469458705863,1.78568969554585,
9.90072617269828));
#43411=CARTESIAN_POINT('Ctrl Pts',(-0.0968715275370533,1.79262596959161,
9.89925019946796));
#43412=CARTESIAN_POINT('Ctrl Pts',(-0.098118613909208,1.7930217838997,9.89916800148322));
#43413=CARTESIAN_POINT('Ctrl Pts',(-0.0997480071222414,1.79354988291193,
9.89906096753402));
#43414=CARTESIAN_POINT('Ctrl Pts',(-0.100132501498861,1.79367530080649,
9.89903573683006));
#43415=CARTESIAN_POINT('Ctrl Pts',(-0.100725279075145,1.79386989376178,
9.89899688053894));
#43416=CARTESIAN_POINT('Ctrl Pts',(-0.100933727654732,1.79393855778194,
9.89898322486533));
#43417=CARTESIAN_POINT('Ctrl Pts',(-0.101349215904362,1.79407589235037,
9.89895602207031));
#43418=CARTESIAN_POINT('Ctrl Pts',(-0.101556254570495,1.79414455969573,
9.89894247495338));
#43419=CARTESIAN_POINT('Ctrl Pts',(-0.102020208771163,1.79429895979606,
9.89891213515838));
#43420=CARTESIAN_POINT('Ctrl Pts',(-0.102277085407242,1.79438480603646,
9.89889534934122));
#43421=CARTESIAN_POINT('Ctrl Pts',(-0.102809300702446,1.79456341455317,
9.89886059632654));
#43422=CARTESIAN_POINT('Ctrl Pts',(-0.103084622906925,1.79465622560456,
9.8988426320253));
#43423=CARTESIAN_POINT('Ctrl Pts',(-0.104626507929913,1.79517831782669,
9.89874210264318));
#43424=CARTESIAN_POINT('Ctrl Pts',(-0.105890539280028,1.79561511548371,
9.89865997643893));
#43425=CARTESIAN_POINT('Ctrl Pts',(-0.109220987549227,1.79678923998765,
9.89844426130085));
#43426=CARTESIAN_POINT('Ctrl Pts',(-0.111282694445221,1.79753983467174,
9.89831140718745));
#43427=CARTESIAN_POINT('Ctrl Pts',(-0.120509233626228,1.80100600837233,
9.89771926082861));
#43428=CARTESIAN_POINT('Ctrl Pts',(-0.127584026453293,1.8039557181631,9.89727173367249));
#43429=CARTESIAN_POINT('Ctrl Pts',(-0.142415278774063,1.81076992881478,
9.89633416192085));
#43430=CARTESIAN_POINT('Ctrl Pts',(-0.150134572369021,1.81470056383909,
9.89584650502563));
#43431=CARTESIAN_POINT('Ctrl Pts',(-0.165343665065552,1.82323342688669,
9.89486932217386));
#43432=CARTESIAN_POINT('Ctrl Pts',(-0.172822088431143,1.82784050751257,
9.89438026524213));
#43433=CARTESIAN_POINT('Ctrl Pts',(-0.189464822290432,1.8390561320578,9.89325437129716));
#43434=CARTESIAN_POINT('Ctrl Pts',(-0.198488147396845,1.84585230217753,
9.89261587677547));
#43435=CARTESIAN_POINT('Ctrl Pts',(-0.209774029586698,1.85532084110524,
9.89176288373902));
#43436=CARTESIAN_POINT('Ctrl Pts',(-0.212376465921326,1.85757625966877,
9.89156217395371));
#43437=CARTESIAN_POINT('Ctrl Pts',(-0.220680320827547,1.86500919335534,
9.89090769484742));
#43438=CARTESIAN_POINT('Ctrl Pts',(-0.226232090747193,1.87034915733732,
9.89044802174623));
#43439=CARTESIAN_POINT('Ctrl Pts',(-0.232265822520867,1.87658398398682,
9.88992016073117));
#43440=CARTESIAN_POINT('Ctrl Pts',(-0.232941473464575,1.87728853098725,
9.88986063461622));
#43441=CARTESIAN_POINT('Ctrl Pts',(-0.233958021673845,1.87835824116803,
9.88977043670227));
#43442=CARTESIAN_POINT('Ctrl Pts',(-0.234301292147323,1.87872114954807,
9.88973986738567));
#43443=CARTESIAN_POINT('Ctrl Pts',(-0.234896251734726,1.87935308235259,
9.88968669018425));
#43444=CARTESIAN_POINT('Ctrl Pts',(-0.235148326565042,1.8796217436811,9.88966409892309));
#43445=CARTESIAN_POINT('Ctrl Pts',(-0.235672592724414,1.88018243011378,
9.88961698600386));
#43446=CARTESIAN_POINT('Ctrl Pts',(-0.235944703100051,1.88047452979455,
9.8895924609364));
#43447=CARTESIAN_POINT('Ctrl Pts',(-0.236483887368894,1.88105548327224,
9.88954372109935));
#43448=CARTESIAN_POINT('Ctrl Pts',(-0.236750976490736,1.88134432200661,
9.88951950704539));
#43449=CARTESIAN_POINT('Ctrl Pts',(-0.237372284102953,1.88201869696176,
9.88946301503901));
#43450=CARTESIAN_POINT('Ctrl Pts',(-0.237726092559501,1.8824046079401,9.88943071972559));
#43451=CARTESIAN_POINT('Ctrl Pts',(-0.238644874247811,1.88341167010896,
9.88934652547109));
#43452=CARTESIAN_POINT('Ctrl Pts',(-0.239208360415563,1.88403416720314,
9.8892945637996));
#43453=CARTESIAN_POINT('Ctrl Pts',(-0.24378790951703,1.88913321946703,9.88886958074356));
#43454=CARTESIAN_POINT('Ctrl Pts',(-0.247680147097211,1.89371892759231,
9.8884914187218));
#43455=CARTESIAN_POINT('Ctrl Pts',(-0.258288162271286,1.90695026083382,
9.88741045229816));
#43456=CARTESIAN_POINT('Ctrl Pts',(-0.264694543023223,1.91583232275206,
9.88669621031294));
#43457=CARTESIAN_POINT('Ctrl Pts',(-0.272807188855462,1.92838006764074,
9.88570425678538));
#43458=CARTESIAN_POINT('Ctrl Pts',(-0.274915416618389,1.93177789754889,
9.88543730002398));
#43459=CARTESIAN_POINT('Ctrl Pts',(-0.27920181128111,1.93898214507799,9.88487518992631));
#43460=CARTESIAN_POINT('Ctrl Pts',(-0.281366618228485,1.94279559185344,
9.88457985994763));
#43461=CARTESIAN_POINT('Ctrl Pts',(-0.294976223507685,1.96795197570047,
9.88264855050122));
#43462=CARTESIAN_POINT('Ctrl Pts',(-0.304062964015647,1.99048478518868,
9.88099028826353));
#43463=CARTESIAN_POINT('Ctrl Pts',(-0.31088806913972,2.01507956364011,9.879378855255));
#43464=CARTESIAN_POINT('Ctrl Pts',(-0.311228740860092,2.01633672822256,
9.8792970300292));
#43465=CARTESIAN_POINT('Ctrl Pts',(-0.311665015206745,2.01798623954543,
9.87919041012149));
#43466=CARTESIAN_POINT('Ctrl Pts',(-0.311767509279796,2.01837672654547,
9.87916522443983));
#43467=CARTESIAN_POINT('Ctrl Pts',(-0.311924551957967,2.01897964692479,
9.87912642212161));
#43468=CARTESIAN_POINT('Ctrl Pts',(-0.311979617453781,2.01919194334296,
9.87911277553228));
#43469=CARTESIAN_POINT('Ctrl Pts',(-0.31208902156242,2.01961551248133,9.87908558075673));
#43470=CARTESIAN_POINT('Ctrl Pts',(-0.312143362001146,2.01982678269834,
9.8790720325945));
#43471=CARTESIAN_POINT('Ctrl Pts',(-0.312264752969119,2.02030073291758,
9.87904167570545));
#43472=CARTESIAN_POINT('Ctrl Pts',(-0.312331686422183,2.02056344180222,
9.87902487387452));
#43473=CARTESIAN_POINT('Ctrl Pts',(-0.312469755638817,2.02110822563968,
9.87899008260698));
#43474=CARTESIAN_POINT('Ctrl Pts',(-0.312540841170675,2.02139031323937,
9.8789720960847));
#43475=CARTESIAN_POINT('Ctrl Pts',(-0.312725024878638,2.02212540566602,
9.87892529776407));
#43476=CARTESIAN_POINT('Ctrl Pts',(-0.312837521218514,2.02257856270861,
9.87889652029228));
#43477=CARTESIAN_POINT('Ctrl Pts',(-0.313166919160517,2.02391788193043,
9.87881167569745));
#43478=CARTESIAN_POINT('Ctrl Pts',(-0.313381045314108,2.02480473133156,
9.87875576342964));
#43479=CARTESIAN_POINT('Ctrl Pts',(-0.319337393109999,2.04994161834231,
9.87717827828858));
#43480=CARTESIAN_POINT('Ctrl Pts',(-0.32225212581812,2.07477878869423,9.87580752190471));
#43481=CARTESIAN_POINT('Ctrl Pts',(-0.322274865898728,2.09970600177385,
9.87441282464039));
#43482=CARTESIAN_POINT('',(-0.322274934653358,2.10025575292171,9.62425292903915));
#43483=CARTESIAN_POINT('Ctrl Pts',(-0.322274865987935,2.09970609957732,
9.87441281916821));
#43484=CARTESIAN_POINT('Ctrl Pts',(-0.322297305845905,2.12431240042638,
9.87303607716149));
#43485=CARTESIAN_POINT('Ctrl Pts',(-0.319501846540933,2.14883719023601,
9.87164199941798));
#43486=CARTESIAN_POINT('Ctrl Pts',(-0.313754231368156,2.17362174744587,
9.87009562371563));
#43487=CARTESIAN_POINT('Ctrl Pts',(-0.313561525540082,2.17443822323641,
9.87004453368211));
#43488=CARTESIAN_POINT('Ctrl Pts',(-0.313243454059054,2.17576270781824,
9.86996141168674));
#43489=CARTESIAN_POINT('Ctrl Pts',(-0.313120034411434,2.17627118362734,
9.86992944227753));
#43490=CARTESIAN_POINT('Ctrl Pts',(-0.312878946613936,2.17725399166109,
9.86986753602526));
#43491=CARTESIAN_POINT('Ctrl Pts',(-0.312761436680213,2.17772836151223,
9.86983760434906));
#43492=CARTESIAN_POINT('Ctrl Pts',(-0.31255681030874,2.17854643004297,9.86978589644286));
#43493=CARTESIAN_POINT('Ctrl Pts',(-0.312470204590151,2.1788902565887,9.86976413674167));
#43494=CARTESIAN_POINT('Ctrl Pts',(-0.312290031664546,2.17960059569219,
9.86971912476365));
#43495=CARTESIAN_POINT('Ctrl Pts',(-0.312196386258506,2.17996708771004,
9.86969586998628));
#43496=CARTESIAN_POINT('Ctrl Pts',(-0.311968290064461,2.1808532606959,9.86963956403524));
#43497=CARTESIAN_POINT('Ctrl Pts',(-0.311833186037185,2.1813727709448,9.86960649175923));
#43498=CARTESIAN_POINT('Ctrl Pts',(-0.311327472885493,2.18329761441702,
9.8694837181674));
#43499=CARTESIAN_POINT('Ctrl Pts',(-0.310948660734578,2.18470075688653,
9.8693937513264));
#43500=CARTESIAN_POINT('Ctrl Pts',(-0.304231966502203,2.20892733406003,
9.86783211893535));
#43501=CARTESIAN_POINT('Ctrl Pts',(-0.295407752386047,2.23098121234592,
9.86627500938244));
#43502=CARTESIAN_POINT('Ctrl Pts',(-0.281907377722443,2.25625018624662,
9.86434362167931));
#43503=CARTESIAN_POINT('Ctrl Pts',(-0.279463590524266,2.26058016997776,
9.86400734931183));
#43504=CARTESIAN_POINT('Ctrl Pts',(-0.274526895559133,2.2688729054334,9.8633542530397));
#43505=CARTESIAN_POINT('Ctrl Pts',(-0.272045833207488,2.27284137153076,
9.86303752074926));
#43506=CARTESIAN_POINT('Ctrl Pts',(-0.26305180116042,2.28655364383423,9.86193078240501));
#43507=CARTESIAN_POINT('Ctrl Pts',(-0.256094118617026,2.2959958126746,9.86114603027968));
#43508=CARTESIAN_POINT('Ctrl Pts',(-0.245460969945522,2.30888994205179,
9.86006169507488));
#43509=CARTESIAN_POINT('Ctrl Pts',(-0.242195669241725,2.31266725250173,
9.8597424072951));
#43510=CARTESIAN_POINT('Ctrl Pts',(-0.238531092191241,2.31671250655774,
9.85940008782886));
#43511=CARTESIAN_POINT('Ctrl Pts',(-0.238217726939383,2.31705692114904,
9.85937093955482));
#43512=CARTESIAN_POINT('Ctrl Pts',(-0.237707734013839,2.31761501127303,
9.85932370444822));
#43513=CARTESIAN_POINT('Ctrl Pts',(-0.237511563464139,2.31782910081931,
9.85930558377508));
#43514=CARTESIAN_POINT('Ctrl Pts',(-0.237131942192299,2.3182422757059,9.85927061143396));
#43515=CARTESIAN_POINT('Ctrl Pts',(-0.236948529544064,2.31844139548487,
9.85925375691608));
#43516=CARTESIAN_POINT('Ctrl Pts',(-0.236616886121135,2.31880053108729,
9.85922335745016));
#43517=CARTESIAN_POINT('Ctrl Pts',(-0.236468744204284,2.31896062709332,
9.85920980581612));
#43518=CARTESIAN_POINT('Ctrl Pts',(-0.236171173121815,2.31928155601092,
9.85918263998217));
#43519=CARTESIAN_POINT('Ctrl Pts',(-0.236021742819249,2.3194423859184,9.859169025997));
#43520=CARTESIAN_POINT('Ctrl Pts',(-0.235596331700964,2.31989931321491,
9.85913034704425));
#43521=CARTESIAN_POINT('Ctrl Pts',(-0.23531995597679,2.32019504487311,9.85910531234822));
#43522=CARTESIAN_POINT('Ctrl Pts',(-0.234145974951239,2.32144651081927,
9.85899936329186));
#43523=CARTESIAN_POINT('Ctrl Pts',(-0.233243082558528,2.32239730060512,
9.85891884917301));
#43524=CARTESIAN_POINT('Ctrl Pts',(-0.216653209305993,2.33965508587502,
9.85745647204684));
#43525=CARTESIAN_POINT('Ctrl Pts',(-0.199294803930529,2.35427367903028,
9.85619933181208));
#43526=CARTESIAN_POINT('Ctrl Pts',(-0.172947693847635,2.37209262161914,
9.85442150969516));
#43527=CARTESIAN_POINT('Ctrl Pts',(-0.16513445194697,2.3769041462864,9.85390879256252));
#43528=CARTESIAN_POINT('Ctrl Pts',(-0.146695956796233,2.38720063285064,
9.85271304547522));
#43529=CARTESIAN_POINT('Ctrl Pts',(-0.135950164127302,2.3924404561668,9.85202616048031));
#43530=CARTESIAN_POINT('Ctrl Pts',(-0.121149094371218,2.39866532500085,
9.85107616240516));
#43531=CARTESIAN_POINT('Ctrl Pts',(-0.117329187001707,2.40018650708016,
9.85083070045081));
#43532=CARTESIAN_POINT('Ctrl Pts',(-0.111128590942264,2.40251930660861,
9.850431246539));
#43533=CARTESIAN_POINT('Ctrl Pts',(-0.108765611497405,2.40337688738464,
9.85027878759168));
#43534=CARTESIAN_POINT('Ctrl Pts',(-0.105895087750046,2.40438082090678,
9.85009322709453));
#43535=CARTESIAN_POINT('Ctrl Pts',(-0.10539685915934,2.40455369940232,9.85006100707462));
#43536=CARTESIAN_POINT('Ctrl Pts',(-0.104433292487991,2.40488539618656,
9.84999866830571));
#43537=CARTESIAN_POINT('Ctrl Pts',(-0.103968010586591,2.40504437408048,
9.84996855493053));
#43538=CARTESIAN_POINT('Ctrl Pts',(-0.103166196521292,2.405316290966,9.84991664037546));
#43539=CARTESIAN_POINT('Ctrl Pts',(-0.102829837268975,2.40542974020141,
9.84989485610887));
#43540=CARTESIAN_POINT('Ctrl Pts',(-0.102135802974879,2.40566255177041,
9.84984989393903));
#43541=CARTESIAN_POINT('Ctrl Pts',(-0.101778104623577,2.40578184253071,
9.84982671370945));
#43542=CARTESIAN_POINT('Ctrl Pts',(-0.100914867664108,2.40606804560246,
9.84977075493809));
#43543=CARTESIAN_POINT('Ctrl Pts',(-0.100409124472092,2.4062343331044,9.84973795584884));
#43544=CARTESIAN_POINT('Ctrl Pts',(-0.098547393548133,2.40684135934776,
9.84961716120124));
#43545=CARTESIAN_POINT('Ctrl Pts',(-0.0971889126785451,2.4072743460314,
9.84952891097501));
#43546=CARTESIAN_POINT('Ctrl Pts',(-0.0746653382698697,2.41428894622515,
9.84806381705592));
#43547=CARTESIAN_POINT('Ctrl Pts',(-0.0528840396137501,2.41867753686474,
9.84661282817544));
#43548=CARTESIAN_POINT('Ctrl Pts',(-0.0136957691263339,2.42244357503113,
9.8439652832459));
#43549=CARTESIAN_POINT('Ctrl Pts',(0.00354165867539437,2.42271488028246,
9.84279015883714));
#43550=CARTESIAN_POINT('Ctrl Pts',(0.0305861848955652,2.4209726468715,9.84098619256883));
#43551=CARTESIAN_POINT('Ctrl Pts',(0.0404207035808147,2.41988304722363,
9.84033903892978));
#43552=CARTESIAN_POINT('Ctrl Pts',(0.0514736619476156,2.41814041739219,
9.83963276640123));
#43553=CARTESIAN_POINT('Ctrl Pts',(0.0527556133379823,2.41793035157104,
9.83955117641875));
#43554=CARTESIAN_POINT('Ctrl Pts',(0.0543201203553452,2.41766426151279,
9.83945203012769));
#43555=CARTESIAN_POINT('Ctrl Pts',(0.0546038921248988,2.4176156064872,9.83943406406591));
#43556=CARTESIAN_POINT('Ctrl Pts',(0.0551526201268768,2.41752076538734,
9.83939935693965));
#43557=CARTESIAN_POINT('Ctrl Pts',(0.0554175843488946,2.41747462781335,
9.83938261314604));
#43558=CARTESIAN_POINT('Ctrl Pts',(0.0558765676366583,2.41739411405798,
9.83935363553895));
#43559=CARTESIAN_POINT('Ctrl Pts',(0.056070612556328,2.4173598916968,9.8393413929505));
#43560=CARTESIAN_POINT('Ctrl Pts',(0.0564762599574232,2.4172879668102,9.83931581747479));
#43561=CARTESIAN_POINT('Ctrl Pts',(0.056687855455908,2.41725023067884,9.83930248657712));
#43562=CARTESIAN_POINT('Ctrl Pts',(0.0572753631028552,2.41714484749377,
9.83926549960808));
#43563=CARTESIAN_POINT('Ctrl Pts',(0.0576511945525295,2.41707674351907,
9.8392418696566));
#43564=CARTESIAN_POINT('Ctrl Pts',(0.0591417272083596,2.41680390811209,
9.83914827321261));
#43565=CARTESIAN_POINT('Ctrl Pts',(0.0602554833517576,2.4165939622104,9.83907860025547));
#43566=CARTESIAN_POINT('Ctrl Pts',(0.0798942418021805,2.41278461609167,
9.83785436160617));
#43567=CARTESIAN_POINT('Ctrl Pts',(0.0980720670802945,2.40757015995193,
9.83678772290392));
#43568=CARTESIAN_POINT('Ctrl Pts',(0.127938775151546,2.39608282335079,9.83499494080691));
#43569=CARTESIAN_POINT('Ctrl Pts',(0.13988712130818,2.39062855134709,9.8342659770238));
#43570=CARTESIAN_POINT('Ctrl Pts',(0.162598744044753,2.3785351045183,9.83280917768137));
#43571=CARTESIAN_POINT('Ctrl Pts',(0.173369665320538,2.37196151943526,9.83208367517406));
#43572=CARTESIAN_POINT('Ctrl Pts',(0.188351024389268,2.36156594038538,9.83100171622776));
#43573=CARTESIAN_POINT('Ctrl Pts',(0.192889763408983,2.35823706697396,9.83066358574443));
#43574=CARTESIAN_POINT('Ctrl Pts',(0.198061036653866,2.35423185455756,9.83026514598197));
#43575=CARTESIAN_POINT('Ctrl Pts',(0.198780866103344,2.35366942534805,9.83020937977084));
#43576=CARTESIAN_POINT('Ctrl Pts',(0.199804897234676,2.35286227690106,9.83012960699683));
#43577=CARTESIAN_POINT('Ctrl Pts',(0.200111065197759,2.35262004992052,9.83010569984734));
#43578=CARTESIAN_POINT('Ctrl Pts',(0.200728123989581,2.35213003374753,9.83005740228364));
#43579=CARTESIAN_POINT('Ctrl Pts',(0.201038997914169,2.35188222444881,9.83003301108998));
#43580=CARTESIAN_POINT('Ctrl Pts',(0.201638942873929,2.35140216753829,9.82998582495835));
#43581=CARTESIAN_POINT('Ctrl Pts',(0.201928073334578,2.35116999487173,9.82996303305393));
#43582=CARTESIAN_POINT('Ctrl Pts',(0.202613050362183,2.35061800897674,9.82990891401737));
#43583=CARTESIAN_POINT('Ctrl Pts',(0.203008540493409,2.35029775684678,9.82987756921893));
#43584=CARTESIAN_POINT('Ctrl Pts',(0.204398126183931,2.34916706579596,9.82976709084794));
#43585=CARTESIAN_POINT('Ctrl Pts',(0.20538813062054,2.34835163858689,9.82968775548488));
#43586=CARTESIAN_POINT('Ctrl Pts',(0.220184281651923,2.33601565760847,9.82849252063869));
#43587=CARTESIAN_POINT('Ctrl Pts',(0.233004963278584,2.32336740463764,9.82732882929094));
#43588=CARTESIAN_POINT('Ctrl Pts',(0.256627144583543,2.29580466365642,9.82491131665182));
#43589=CARTESIAN_POINT('Ctrl Pts',(0.267342925314749,2.28089959298636,9.82366061887386));
#43590=CARTESIAN_POINT('Ctrl Pts',(0.280263660576456,2.25925107628006,9.8219671747482));
#43591=CARTESIAN_POINT('Ctrl Pts',(0.283603572256919,2.25322417628279,9.82150802947032));
#43592=CARTESIAN_POINT('Ctrl Pts',(0.289488578222333,2.24175187647036,9.82066226873715));
#43593=CARTESIAN_POINT('Ctrl Pts',(0.292079610990846,2.23633320594882,9.82027407308481));
#43594=CARTESIAN_POINT('Ctrl Pts',(0.295128831444165,2.22946973712254,9.81979908925867));
#43595=CARTESIAN_POINT('Ctrl Pts',(0.295730152220973,2.22809026995562,9.81970445331327));
#43596=CARTESIAN_POINT('Ctrl Pts',(0.296486919263441,2.22632046036078,9.81958414378047));
#43597=CARTESIAN_POINT('Ctrl Pts',(0.296651282214774,2.22593398574326,9.81955793879455));
#43598=CARTESIAN_POINT('Ctrl Pts',(0.296911222348168,2.22531944309033,9.81951637741319));
#43599=CARTESIAN_POINT('Ctrl Pts',(0.297007292593845,2.22509158612718,9.81950099100123));
#43600=CARTESIAN_POINT('Ctrl Pts',(0.297187857639902,2.22466194588452,9.81947202343226));
#43601=CARTESIAN_POINT('Ctrl Pts',(0.297272408554982,2.22446018878566,9.81945843893898));
#43602=CARTESIAN_POINT('Ctrl Pts',(0.297463994149048,2.22400171437883,9.81942761135309));
#43603=CARTESIAN_POINT('Ctrl Pts',(0.297570901761335,2.22374494498902,9.81941037610029));
#43604=CARTESIAN_POINT('Ctrl Pts',(0.297893773244277,2.22296663826904,9.81935822271649));
#43605=CARTESIAN_POINT('Ctrl Pts',(0.298108700852122,2.22244466812636,9.81932336743259));
#43606=CARTESIAN_POINT('Ctrl Pts',(0.29960031731831,2.21879494196711,9.81908048013223));
#43607=CARTESIAN_POINT('Ctrl Pts',(0.300829187814022,2.21564769917812,9.81887527519133));
#43608=CARTESIAN_POINT('Ctrl Pts',(0.30239082270291,2.21145477342877,9.8186067395954));
#43609=CARTESIAN_POINT('Ctrl Pts',(0.302768012732389,2.21042602368287,9.81854123625238));
#43610=CARTESIAN_POINT('Ctrl Pts',(0.306011596891683,2.2014378912329,9.81797210545464));
#43611=CARTESIAN_POINT('Ctrl Pts',(0.308569024512462,2.1933698134325,9.81748281031494));
#43612=CARTESIAN_POINT('Ctrl Pts',(0.315262583000933,2.16895481292754,9.81604063135334));
#43613=CARTESIAN_POINT('Ctrl Pts',(0.318437097088449,2.15237476589654,9.81511055965198));
#43614=CARTESIAN_POINT('Ctrl Pts',(0.321787789347033,2.12224657356128,9.81340581455307));
#43615=CARTESIAN_POINT('Ctrl Pts',(0.322435947403746,2.10879221106583,9.81263954639161));
#43616=CARTESIAN_POINT('Ctrl Pts',(0.322133748893646,2.08790630496455,9.81141197503266));
#43617=CARTESIAN_POINT('Ctrl Pts',(0.321769214110453,2.08048156844214,9.81096826794861));
#43618=CARTESIAN_POINT('Ctrl Pts',(0.321053213688853,2.07194099058388,9.81044709169071));
#43619=CARTESIAN_POINT('Ctrl Pts',(0.320951999024646,2.07080602289462,9.81037761328371));
#43620=CARTESIAN_POINT('Ctrl Pts',(0.320794868993983,2.06914373957591,9.81027552622825));
#43621=CARTESIAN_POINT('Ctrl Pts',(0.320743667074442,2.06861597848335,9.81024306589319));
#43622=CARTESIAN_POINT('Ctrl Pts',(0.320651843407382,2.06769321086289,9.8101862245961));
#43623=CARTESIAN_POINT('Ctrl Pts',(0.320611793523599,2.06729814751118,9.81016186168329));
#43624=CARTESIAN_POINT('Ctrl Pts',(0.320532852972805,2.06653354119646,9.81011465599012));
#43625=CARTESIAN_POINT('Ctrl Pts',(0.320494053107751,2.06616398929387,9.81009181610536));
#43626=CARTESIAN_POINT('Ctrl Pts',(0.320400287332385,2.06528554339751,9.81003746628292));
#43627=CARTESIAN_POINT('Ctrl Pts',(0.320344748127649,2.06477671278701,9.8100059383226));
#43628=CARTESIAN_POINT('Ctrl Pts',(0.320143858098891,2.06297601035928,9.8098941982516));
#43629=CARTESIAN_POINT('Ctrl Pts',(0.319991904291529,2.06168490120324,9.80981377823887));
#43630=CARTESIAN_POINT('Ctrl Pts',(0.317213236251432,2.03924576441126,9.80841074147783));
#43631=CARTESIAN_POINT('Ctrl Pts',(0.312503683243919,2.01841299505657,9.80701984634121));
#43632=CARTESIAN_POINT('Ctrl Pts',(0.296868475033331,1.97144949488446,9.80369754655943));
#43633=CARTESIAN_POINT('Ctrl Pts',(0.284490267505094,1.94598192489157,9.80174706064239));
#43634=CARTESIAN_POINT('Ctrl Pts',(0.268255980660065,1.92139004441731,9.79988758999824));
#43635=CARTESIAN_POINT('Ctrl Pts',(0.267550278724164,1.92033465588822,9.79980786236898));
#43636=CARTESIAN_POINT('Ctrl Pts',(0.266620717420602,1.91896210538215,9.79970430083597));
#43637=CARTESIAN_POINT('Ctrl Pts',(0.266402508452238,1.9186411575366,9.79968009373914));
#43638=CARTESIAN_POINT('Ctrl Pts',(0.26604833992763,1.91812225502829,9.79964097181865));
#43639=CARTESIAN_POINT('Ctrl Pts',(0.265912738776006,1.91792405800933,9.79962603274411));
#43640=CARTESIAN_POINT('Ctrl Pts',(0.265652230018293,1.91754420559659,9.79959740882915));
#43641=CARTESIAN_POINT('Ctrl Pts',(0.265527357951223,1.91736252738076,9.79958372169801));
#43642=CARTESIAN_POINT('Ctrl Pts',(0.265239734521849,1.91694497827603,9.79955227202741));
#43643=CARTESIAN_POINT('Ctrl Pts',(0.26507685442797,1.91670919555067,9.79953451830532));
#43644=CARTESIAN_POINT('Ctrl Pts',(0.264571375157276,1.915979554558,9.79947959412768));
#43645=CARTESIAN_POINT('Ctrl Pts',(0.264227706227595,1.91548643364585,9.79944249627908));
#43646=CARTESIAN_POINT('Ctrl Pts',(0.261376327266272,1.91141937331919,9.79913668576985));
#43647=CARTESIAN_POINT('Ctrl Pts',(0.258797459936304,1.90789555829201,9.798872729477));
#43648=CARTESIAN_POINT('Ctrl Pts',(0.255529827265504,1.90361588813574,9.79855193963046));
#43649=CARTESIAN_POINT('Ctrl Pts',(0.254908188881738,1.90280966731294,9.79849149841036));
#43650=CARTESIAN_POINT('Ctrl Pts',(0.253633684977315,1.90117282485844,9.79836873641439));
#43651=CARTESIAN_POINT('Ctrl Pts',(0.252980534255685,1.90034244049195,9.7983064315288));
#43652=CARTESIAN_POINT('Ctrl Pts',(0.252068397777214,1.89919445633103,9.79822023632875));
#43653=CARTESIAN_POINT('Ctrl Pts',(0.251812878213565,1.8988741242535,9.7981961779597));
#43654=CARTESIAN_POINT('Ctrl Pts',(0.248949098441692,1.8952979593143,9.7979275075971));
#43655=CARTESIAN_POINT('Ctrl Pts',(0.246278371066991,1.89209245915756,9.79768589830229));
#43656=CARTESIAN_POINT('Ctrl Pts',(0.226995911383314,1.86984211116259,9.79599605017308));
#43657=CARTESIAN_POINT('Ctrl Pts',(0.208256714985489,1.85275707254662,9.79462396134834));
#43658=CARTESIAN_POINT('Ctrl Pts',(0.177201069282904,1.83050381469792,9.79243793321324));
#43659=CARTESIAN_POINT('Ctrl Pts',(0.166246492520114,1.82361176460769,9.79168210148426));
#43660=CARTESIAN_POINT('Ctrl Pts',(0.153631087115734,1.81669665282146,9.79081306423907));
#43661=CARTESIAN_POINT('Ctrl Pts',(0.152349034829988,1.81600516038142,9.79072477163155));
#43662=CARTESIAN_POINT('Ctrl Pts',(0.150085494271084,1.81480402703968,9.79056890617822));
#43663=CARTESIAN_POINT('Ctrl Pts',(0.14910598185343,1.81429069894181,9.79050146450662));
#43664=CARTESIAN_POINT('Ctrl Pts',(0.147659742344713,1.81354223835232,9.79040189028089));
#43665=CARTESIAN_POINT('Ctrl Pts',(0.147195047098176,1.81330317960921,9.79036989622024));
#43666=CARTESIAN_POINT('Ctrl Pts',(0.146377303071823,1.81288500997988,9.79031359479054));
#43667=CARTESIAN_POINT('Ctrl Pts',(0.146024500974872,1.81270541692957,9.79028930443455));
#43668=CARTESIAN_POINT('Ctrl Pts',(0.145337939969498,1.81235751608429,9.79024203438235));
#43669=CARTESIAN_POINT('Ctrl Pts',(0.145004217232303,1.81218913792076,9.79021905720225));
#43670=CARTESIAN_POINT('Ctrl Pts',(0.144113030328574,1.81174143741682,9.79015769700574));
#43671=CARTESIAN_POINT('Ctrl Pts',(0.143555049261279,1.81146315272417,9.79011927773544));
#43672=CARTESIAN_POINT('Ctrl Pts',(0.141548432629224,1.81046964418382,9.78998110774663));
#43673=CARTESIAN_POINT('Ctrl Pts',(0.140095249812797,1.80976370567053,9.7898810338229));
#43674=CARTESIAN_POINT('Ctrl Pts',(0.136621955895356,1.80810858450049,9.78964179041358));
#43675=CARTESIAN_POINT('Ctrl Pts',(0.134597192394109,1.80716941302022,9.78950227967538));
#43676=CARTESIAN_POINT('Ctrl Pts',(0.131862739252417,1.80593540906021,9.78931378259872));
#43677=CARTESIAN_POINT('Ctrl Pts',(0.131161478861849,1.80562195718072,9.789265434269));
#43678=CARTESIAN_POINT('Ctrl Pts',(0.129710176596205,1.80497946420575,9.7891653573722));
#43679=CARTESIAN_POINT('Ctrl Pts',(0.128959988174738,1.80465076962471,9.78911361757299));
#43680=CARTESIAN_POINT('Ctrl Pts',(0.0979021320076369,1.79118367829456,
9.78697117288976));
#43681=CARTESIAN_POINT('Ctrl Pts',(0.0657592857931973,1.78278227175213,
9.78470741414048));
#43682=CARTESIAN_POINT('Ctrl Pts',(0.0211334842549709,1.77820069796031,
9.78170098806605));
#43683=CARTESIAN_POINT('Ctrl Pts',(0.00929398069462249,1.77764134582955,
9.78091941939964));
#43684=CARTESIAN_POINT('Ctrl Pts',(-0.00414735685355448,1.77774773135416,
9.78006876629563));
#43685=CARTESIAN_POINT('Ctrl Pts',(-0.00574397429082147,1.77777223548279,
9.77996831396354));
#43686=CARTESIAN_POINT('Ctrl Pts',(-0.00775684790823911,1.77781809413138,
9.77984247446533));
#43687=CARTESIAN_POINT('Ctrl Pts',(-0.00817329750369071,1.777828389874,
9.77981648243746));
#43688=CARTESIAN_POINT('Ctrl Pts',(-0.00883616280807769,1.7778460637758,
9.77977518094625));
#43689=CARTESIAN_POINT('Ctrl Pts',(-0.00908259024036353,1.77785291720485,
9.77975984210432));
#43690=CARTESIAN_POINT('Ctrl Pts',(-0.00954780777627352,1.77786638967031,
9.77973091416207));
#43691=CARTESIAN_POINT('Ctrl Pts',(-0.00976659720525034,1.77787294879703,
9.77971732184053));
#43692=CARTESIAN_POINT('Ctrl Pts',(-0.010264619509705,1.77788838695266,
9.77968641004311));
#43693=CARTESIAN_POINT('Ctrl Pts',(-0.010543847128047,1.77789740615327,
9.77966909857274));
#43694=CARTESIAN_POINT('Ctrl Pts',(-0.0112668465988965,1.77792170057866,
9.77962432508355));
#43695=CARTESIAN_POINT('Ctrl Pts',(-0.0117106011090723,1.77793752994541,
9.77959689408986));
#43696=CARTESIAN_POINT('Ctrl Pts',(-0.014387501042807,1.7780385588006,9.7794317111711));
#43697=CARTESIAN_POINT('Ctrl Pts',(-0.0166198142580742,1.77814607002657,
9.77929518628514));
#43698=CARTESIAN_POINT('Ctrl Pts',(-0.0189881557188142,1.7782848395385,
9.77915147160512));
#43699=CARTESIAN_POINT('Ctrl Pts',(-0.0191254049468808,1.77829296959169,
9.77914314713557));
#43700=CARTESIAN_POINT('Ctrl Pts',(-0.0530559000650971,1.78032465637091,
9.77708617441784));
#43701=CARTESIAN_POINT('Ctrl Pts',(-0.0863249158435276,1.78766022651808,
9.7752929580443));
#43702=CARTESIAN_POINT('Ctrl Pts',(-0.13138131169467,1.80536190709868,9.77252575341611));
#43703=CARTESIAN_POINT('Ctrl Pts',(-0.144539335843734,1.81158892235489,
9.77167459192762));
#43704=CARTESIAN_POINT('Ctrl Pts',(-0.158283573633327,1.8192706995653,9.7707174952245));
#43705=CARTESIAN_POINT('Ctrl Pts',(-0.159332890610663,1.81986492595089,
9.7706439845545));
#43706=CARTESIAN_POINT('Ctrl Pts',(-0.160844171122918,1.82073199958781,
9.7705374634627));
#43707=CARTESIAN_POINT('Ctrl Pts',(-0.161308835825522,1.82100013814061,
9.77050462309901));
#43708=CARTESIAN_POINT('Ctrl Pts',(-0.162117156461919,1.8214692804964,9.77044733865349));
#43709=CARTESIAN_POINT('Ctrl Pts',(-0.162461114451169,1.82166976374192,
9.77042291347187));
#43710=CARTESIAN_POINT('Ctrl Pts',(-0.163123962618023,1.82205776625446,
9.77037574742084));
#43711=CARTESIAN_POINT('Ctrl Pts',(-0.163442903330892,1.82224519836975,
9.77035300974457));
#43712=CARTESIAN_POINT('Ctrl Pts',(-0.164196918533735,1.82269005944786,
9.77029915301651));
#43713=CARTESIAN_POINT('Ctrl Pts',(-0.164631710461629,1.82294796320757,
9.77026801670179));
#43714=CARTESIAN_POINT('Ctrl Pts',(-0.166150550320656,1.82385372510966,
9.77015896583892));
#43715=CARTESIAN_POINT('Ctrl Pts',(-0.167231384753808,1.82450692497236,
9.77008085630155));
#43716=CARTESIAN_POINT('Ctrl Pts',(-0.182106017075454,1.83361616473498,
9.76899879903645));
#43717=CARTESIAN_POINT('Ctrl Pts',(-0.195245558213547,1.84309150434982,
9.76795646474507));
#43718=CARTESIAN_POINT('Ctrl Pts',(-0.214244502983612,1.85909429095789,
9.76631072098358));
#43719=CARTESIAN_POINT('Ctrl Pts',(-0.2206441005582,1.86494163359599,9.76572923614095));
#43720=CARTESIAN_POINT('Ctrl Pts',(-0.238646699960941,1.88277435840428,
9.76401898430969));
#43721=CARTESIAN_POINT('Ctrl Pts',(-0.2495650155238,1.89541123703916,9.76288251820967));
#43722=CARTESIAN_POINT('Ctrl Pts',(-0.263119839030976,1.91380852466656,
9.7613722471434));
#43723=CARTESIAN_POINT('Ctrl Pts',(-0.2666396745088,1.91888509251695,9.76096928698511));
#43724=CARTESIAN_POINT('Ctrl Pts',(-0.271588654478606,1.9264801954585,9.76038973025778));
#43725=CARTESIAN_POINT('Ctrl Pts',(-0.273133105823263,1.92892157431099,
9.76020684904137));
#43726=CARTESIAN_POINT('Ctrl Pts',(-0.274906385955153,1.93180991419906,
9.75999475982114));
#43727=CARTESIAN_POINT('Ctrl Pts',(-0.275167194512037,1.93223694961925,
9.7599635112288));
#43728=CARTESIAN_POINT('Ctrl Pts',(-0.275564535202329,1.93289095561116,
9.75991582153778));
#43729=CARTESIAN_POINT('Ctrl Pts',(-0.275701782372438,1.93311748750783,
9.75989933364467));
#43730=CARTESIAN_POINT('Ctrl Pts',(-0.275940429603432,1.93351248216052,
9.75987063810736));
#43731=CARTESIAN_POINT('Ctrl Pts',(-0.276041954461068,1.93368086801554,
9.75985842223128));
#43732=CARTESIAN_POINT('Ctrl Pts',(-0.276255251691661,1.93403536922291,
9.75983274005259));
#43733=CARTESIAN_POINT('Ctrl Pts',(-0.276366989752446,1.93422150401203,
9.75981927603268));
#43734=CARTESIAN_POINT('Ctrl Pts',(-0.27668031325391,1.93474463975906,9.75978149279504));
#43735=CARTESIAN_POINT('Ctrl Pts',(-0.276881471829862,1.93508189792549,
9.75975720161944));
#43736=CARTESIAN_POINT('Ctrl Pts',(-0.277702491903747,1.93646413902228,
9.75965791607218));
#43737=CARTESIAN_POINT('Ctrl Pts',(-0.278317068317699,1.93751227299109,
9.75958326223036));
#43738=CARTESIAN_POINT('Ctrl Pts',(-0.288969533244621,1.95591736306462,
9.75828294139061));
#43739=CARTESIAN_POINT('Ctrl Pts',(-0.297373684356233,1.9741733270885,9.75715597044031));
#43740=CARTESIAN_POINT('Ctrl Pts',(-0.30940996989391,2.0084032019257,9.75512584973383));
#43741=CARTESIAN_POINT('Ctrl Pts',(-0.313628873807836,2.02409609566827,
9.75422387174479));
#43742=CARTESIAN_POINT('Ctrl Pts',(-0.318091344003069,2.04766202799877,
9.75284758579285));
#43743=CARTESIAN_POINT('Ctrl Pts',(-0.31925899291133,2.05533402496134,9.75239646562233));
#43744=CARTESIAN_POINT('Ctrl Pts',(-0.320844999060878,2.06907217242906,
9.75157762129026));
#43745=CARTESIAN_POINT('Ctrl Pts',(-0.321370705784315,2.07512217954957,
9.75121326509177));
#43746=CARTESIAN_POINT('Ctrl Pts',(-0.321779745936544,2.08211582770399,
9.75078656525539));
#43747=CARTESIAN_POINT('Ctrl Pts',(-0.321830240036878,2.08304874392122,
9.75072953358463));
#43748=CARTESIAN_POINT('Ctrl Pts',(-0.321900703160517,2.08446466577264,
9.75064279999281));
#43749=CARTESIAN_POINT('Ctrl Pts',(-0.321923643536548,2.084947524027,9.75061319129254));
#43750=CARTESIAN_POINT('Ctrl Pts',(-0.321963022232995,2.08581767970143,
9.75055977752707));
#43751=CARTESIAN_POINT('Ctrl Pts',(-0.321979848354056,2.08620495935959,
9.75053598466833));
#43752=CARTESIAN_POINT('Ctrl Pts',(-0.322014522698576,2.08703768771663,
9.75048478183374));
#43753=CARTESIAN_POINT('Ctrl Pts',(-0.322032145437325,2.08748314454919,
9.75045736483829));
#43754=CARTESIAN_POINT('Ctrl Pts',(-0.322077341531188,2.08868891949312,
9.75038307868663));
#43755=CARTESIAN_POINT('Ctrl Pts',(-0.322103146726464,2.08944929750828,
9.75033615420771));
#43756=CARTESIAN_POINT('Ctrl Pts',(-0.322206688439654,2.09285610738308,
9.75012555520162));
#43757=CARTESIAN_POINT('Ctrl Pts',(-0.322254502150832,2.09550328480943,
9.74996094611242));
#43758=CARTESIAN_POINT('Ctrl Pts',(-0.322273411130203,2.09879845286177,
9.74975478492523));
#43759=CARTESIAN_POINT('Ctrl Pts',(-0.322275175211994,2.0994462227569,9.74971419696014));
#43760=CARTESIAN_POINT('Ctrl Pts',(-0.322273302805116,2.10586638760011,
9.74931131846836));
#43761=CARTESIAN_POINT('Ctrl Pts',(-0.322116532944669,2.11163737770104,
9.74894430989695));
#43762=CARTESIAN_POINT('Ctrl Pts',(-0.321400676334139,2.12487623154211,
9.74809086439356));
#43763=CARTESIAN_POINT('Ctrl Pts',(-0.320736129714393,2.13233486589216,
9.74760156373966));
#43764=CARTESIAN_POINT('Ctrl Pts',(-0.316059594151767,2.16994792426403,
9.74509395513849));
#43765=CARTESIAN_POINT('Ctrl Pts',(-0.308052987212269,2.19944621280876,
9.74297782292642));
#43766=CARTESIAN_POINT('Ctrl Pts',(-0.294323019277409,2.23135378497443,
9.74073427392886));
#43767=CARTESIAN_POINT('Ctrl Pts',(-0.29253483335679,2.23528943906034,9.74045874355568));
#43768=CARTESIAN_POINT('Ctrl Pts',(-0.290431825866982,2.2396811688905,9.74015361694825));
#43769=CARTESIAN_POINT('Ctrl Pts',(-0.290194488546534,2.24017358255626,
9.74011943874484));
#43770=CARTESIAN_POINT('Ctrl Pts',(-0.289834215223509,2.24091621989981,
9.74006794595621));
#43771=CARTESIAN_POINT('Ctrl Pts',(-0.289712206985829,2.24116688871659,
9.74005057434575));
#43772=CARTESIAN_POINT('Ctrl Pts',(-0.289499843316978,2.24160176001176,
9.74002045369831));
#43773=CARTESIAN_POINT('Ctrl Pts',(-0.289409637228505,2.24178603456894,
9.74000769533899));
#43774=CARTESIAN_POINT('Ctrl Pts',(-0.2892206828405,2.24217110223605,9.73998104584695));
#43775=CARTESIAN_POINT('Ctrl Pts',(-0.28912190145218,2.24237187852504,9.7399671568904));
#43776=CARTESIAN_POINT('Ctrl Pts',(-0.288885262682978,2.24285159236075,
9.73993398660289));
#43777=CARTESIAN_POINT('Ctrl Pts',(-0.288747209818941,2.24313043442657,
9.73991471754587));
#43778=CARTESIAN_POINT('Ctrl Pts',(-0.288278395582984,2.24407391648643,
9.73984955767201));
#43779=CARTESIAN_POINT('Ctrl Pts',(-0.287945738362077,2.24473761970016,
9.73980378475377));
#43780=CARTESIAN_POINT('Ctrl Pts',(-0.287149164594124,2.24631329323574,
9.73969525668464));
#43781=CARTESIAN_POINT('Ctrl Pts',(-0.286683189442699,2.24722422171532,
9.7396326262312));
#43782=CARTESIAN_POINT('Ctrl Pts',(-0.28106100386613,2.25808704548987,9.73888691337876));
#43783=CARTESIAN_POINT('Ctrl Pts',(-0.275392728065583,2.26776681825872,
9.73823394896948));
#43784=CARTESIAN_POINT('Ctrl Pts',(-0.253634613879629,2.30083785970426,
9.73597506091713));
#43785=CARTESIAN_POINT('Ctrl Pts',(-0.234976438492165,2.32237926423071,
9.73443965479729));
#43786=CARTESIAN_POINT('Ctrl Pts',(-0.206384737560527,2.34771564530996,
9.73221703103888));
#43787=CARTESIAN_POINT('Ctrl Pts',(-0.198738179819942,2.35389132946558,
9.73163417717737));
#43788=CARTESIAN_POINT('Ctrl Pts',(-0.189982896015386,2.36032433467239,
9.73097353306597));
#43789=CARTESIAN_POINT('Ctrl Pts',(-0.189140753605194,2.36093684156681,
9.73091005647415));
#43790=CARTESIAN_POINT('Ctrl Pts',(-0.187876842277496,2.36184677597961,
9.73081488512686));
#43791=CARTESIAN_POINT('Ctrl Pts',(-0.187457297738772,2.36214729347195,
9.73078330955119));
#43792=CARTESIAN_POINT('Ctrl Pts',(-0.186733529275324,2.36266309898837,
9.73072886386259));
#43793=CARTESIAN_POINT('Ctrl Pts',(-0.186429649492779,2.36287887004074,
9.730706012357));
#43794=CARTESIAN_POINT('Ctrl Pts',(-0.185801741133313,2.36332308253775,
9.73065881018705));
#43795=CARTESIAN_POINT('Ctrl Pts',(-0.185477664043718,2.36355145407311,
9.73063445689574));
#43796=CARTESIAN_POINT('Ctrl Pts',(-0.184722395585458,2.36408159569706,
9.73057772097054));
#43797=CARTESIAN_POINT('Ctrl Pts',(-0.184290885682848,2.36438290804386,
9.73054532092668));
#43798=CARTESIAN_POINT('Ctrl Pts',(-0.182913530616396,2.36533966944501,
9.73044194838399));
#43799=CARTESIAN_POINT('Ctrl Pts',(-0.181964920019094,2.36599110453385,
9.73037082344262));
#43800=CARTESIAN_POINT('Ctrl Pts',(-0.16156198415252,2.37984209861582,9.72884245102156));
#43801=CARTESIAN_POINT('Ctrl Pts',(-0.140728943060134,2.3908759347482,9.72730094024204));
#43802=CARTESIAN_POINT('Ctrl Pts',(-0.0971380128821049,2.40817667079334,
9.72414230148877));
#43803=CARTESIAN_POINT('Ctrl Pts',(-0.0745139122299928,2.414414442158,9.7225362033182));
#43804=CARTESIAN_POINT('Ctrl Pts',(-0.0476865638607515,2.41874977041065,
9.72078726636761));
#43805=CARTESIAN_POINT('Ctrl Pts',(-0.0439496405399965,2.41928648058782,
9.72054720724879));
#43806=CARTESIAN_POINT('Ctrl Pts',(-0.0396248762496681,2.41983024472311,
9.72027414815069));
#43807=CARTESIAN_POINT('Ctrl Pts',(-0.0390455961610972,2.41990148122594,
9.72023767168754));
#43808=CARTESIAN_POINT('Ctrl Pts',(-0.0381861800249611,2.42000479805665,
9.72018370457097));
#43809=CARTESIAN_POINT('Ctrl Pts',(-0.0379061943391096,2.42003808454051,
9.72016614630204));
#43810=CARTESIAN_POINT('Ctrl Pts',(-0.0374084835451638,2.42009659327066,
9.72013497633107));
#43811=CARTESIAN_POINT('Ctrl Pts',(-0.0371907764593803,2.42012196084004,
9.7201213563972));
#43812=CARTESIAN_POINT('Ctrl Pts',(-0.0367296514535556,2.42017521509013,
9.72009253851741));
#43813=CARTESIAN_POINT('Ctrl Pts',(-0.0364862282470712,2.42020304621158,
9.72007734378288));
#43814=CARTESIAN_POINT('Ctrl Pts',(-0.0358355633737592,2.42027668657897,
9.72003677594483));
#43815=CARTESIAN_POINT('Ctrl Pts',(-0.0354282639708158,2.4203219968793,
9.72001143108791));
#43816=CARTESIAN_POINT('Ctrl Pts',(-0.0335066025968067,2.42053206334819,
9.71989208170253));
#43817=CARTESIAN_POINT('Ctrl Pts',(-0.0319911389339923,2.42068686174598,
9.71979863100221));
#43818=CARTESIAN_POINT('Ctrl Pts',(-0.0196668766053605,2.42185750006908,
9.71904369244579));
#43819=CARTESIAN_POINT('Ctrl Pts',(-0.00881290768415047,2.42233743589281,
9.71841017903219));
#43820=CARTESIAN_POINT('Ctrl Pts',(0.0297640250337196,2.42209255575652,
9.71620553632143));
#43821=CARTESIAN_POINT('Ctrl Pts',(0.0573435442426511,2.41834154859798,
9.71470519896699));
#43822=CARTESIAN_POINT('Ctrl Pts',(0.0865115727784765,2.41045634845394,
9.71295451375038));
#43823=CARTESIAN_POINT('Ctrl Pts',(0.0889116345882098,2.40977752876617,
9.71280930240391));
#43824=CARTESIAN_POINT('Ctrl Pts',(0.0930996700890285,2.4085403291196,9.71255369594664));
#43825=CARTESIAN_POINT('Ctrl Pts',(0.0948911200014029,2.40799408827722,
9.71244364299952));
#43826=CARTESIAN_POINT('Ctrl Pts',(0.103042272576261,2.40543080974689,9.71193944017563));
#43827=CARTESIAN_POINT('Ctrl Pts',(0.109342789235478,2.40323231052469,9.71154001766711));
#43828=CARTESIAN_POINT('Ctrl Pts',(0.116541694706376,2.40046679028313,9.71107068468672));
#43829=CARTESIAN_POINT('Ctrl Pts',(0.117511347641383,2.40008888983726,9.71100719336631));
#43830=CARTESIAN_POINT('Ctrl Pts',(0.11894885492292,2.39952061806226,9.71091265285657));
#43831=CARTESIAN_POINT('Ctrl Pts',(0.119418126202741,2.39933383013203,9.7108817243945));
#43832=CARTESIAN_POINT('Ctrl Pts',(0.120252158387223,2.39899957997237,9.71082663736028));
#43833=CARTESIAN_POINT('Ctrl Pts',(0.120617092814937,2.39885255116719,9.71080249345997));
#43834=CARTESIAN_POINT('Ctrl Pts',(0.121383752197806,2.39854203797431,9.7107516863605));
#43835=CARTESIAN_POINT('Ctrl Pts',(0.121785417924807,2.39837841026694,9.71072501835167));
#43836=CARTESIAN_POINT('Ctrl Pts',(0.122840736899737,2.3979460160531,9.71065482155169));
#43837=CARTESIAN_POINT('Ctrl Pts',(0.12349383581315,2.39767591039152,9.71061124744473));
#43838=CARTESIAN_POINT('Ctrl Pts',(0.126400980172652,2.39646237303852,9.71041669272082));
#43839=CARTESIAN_POINT('Ctrl Pts',(0.12864509346945,2.39549549203602,9.71026491676627));
#43840=CARTESIAN_POINT('Ctrl Pts',(0.144924368008203,2.38826094255759,9.70915197812451));
#43841=CARTESIAN_POINT('Ctrl Pts',(0.158504091427189,2.3810227274615,9.70815709961872));
#43842=CARTESIAN_POINT('Ctrl Pts',(0.193873218945202,2.35878916428168,9.70538365929412));
#43843=CARTESIAN_POINT('Ctrl Pts',(0.214418115340905,2.34204010927256,9.70355912743421));
#43844=CARTESIAN_POINT('Ctrl Pts',(0.234449587056449,2.32113580206036,9.70166030311343));
#43845=CARTESIAN_POINT('Ctrl Pts',(0.236188516074258,2.3192775351903,9.70149442044739));
#43846=CARTESIAN_POINT('Ctrl Pts',(0.237995550803001,2.31730004906291,9.70132110110298));
#43847=CARTESIAN_POINT('Ctrl Pts',(0.238085740899935,2.31720122813882,9.70131244814136));
#43848=CARTESIAN_POINT('Ctrl Pts',(0.238448427285877,2.31680333679867,9.70127764155284));
#43849=CARTESIAN_POINT('Ctrl Pts',(0.238720423042076,2.31650380816066,9.70125151578924));
#43850=CARTESIAN_POINT('Ctrl Pts',(0.241737083712688,2.31316918850029,9.70096151457338));
#43851=CARTESIAN_POINT('Ctrl Pts',(0.244424428647334,2.31008241985739,9.70070091239005));
#43852=CARTESIAN_POINT('Ctrl Pts',(0.247398026389371,2.30653252012041,9.70041076509293));
#43853=CARTESIAN_POINT('Ctrl Pts',(0.24774262048269,2.30611904166025,9.70037711362685));
#43854=CARTESIAN_POINT('Ctrl Pts',(0.248262749695936,2.30549174986433,9.70032628046412));
#43855=CARTESIAN_POINT('Ctrl Pts',(0.248439045929106,2.30527857318321,9.70030904376083));
#43856=CARTESIAN_POINT('Ctrl Pts',(0.24874526993362,2.30490731607397,9.70027909214027));
#43857=CARTESIAN_POINT('Ctrl Pts',(0.24887532167581,2.30474933884215,9.70026636815217));
#43858=CARTESIAN_POINT('Ctrl Pts',(0.249147580844303,2.30441797589654,9.70023972334232));
#43859=CARTESIAN_POINT('Ctrl Pts',(0.249289757723291,2.30424456566779,9.70022580480711));
#43860=CARTESIAN_POINT('Ctrl Pts',(0.249626410401491,2.3038330820903,9.7001928372904));
#43861=CARTESIAN_POINT('Ctrl Pts',(0.249820727446279,2.30359487779523,9.70017379991667));
#43862=CARTESIAN_POINT('Ctrl Pts',(0.250469294822435,2.30279750242345,9.70011022974829));
#43863=CARTESIAN_POINT('Ctrl Pts',(0.250922015132587,2.30223708112844,9.70006580711069));
#43864=CARTESIAN_POINT('Ctrl Pts',(0.251996452292413,2.30089787621244,9.69996024993827));
#43865=CARTESIAN_POINT('Ctrl Pts',(0.252616448016272,2.30011771257346,9.69989923473677));
#43866=CARTESIAN_POINT('Ctrl Pts',(0.259836386610023,2.29094557305619,9.69918730882531));
#43867=CARTESIAN_POINT('Ctrl Pts',(0.266019766997821,2.28223252866871,9.69856376919799));
#43868=CARTESIAN_POINT('Ctrl Pts',(0.282935060744857,2.25569579448488,9.69676391775409));
#43869=CARTESIAN_POINT('Ctrl Pts',(0.292387961617191,2.23712323255697,9.69562488934197));
#43870=CARTESIAN_POINT('Ctrl Pts',(0.306474581017473,2.20124115123914,9.69344298233561));
#43871=CARTESIAN_POINT('Ctrl Pts',(0.311585156899191,2.18420801882584,9.69241441053767));
#43872=CARTESIAN_POINT('Ctrl Pts',(0.315532591716083,2.1655896247659,9.69125831523383));
#43873=CARTESIAN_POINT('Ctrl Pts',(0.315790706479602,2.16433540968771,9.69118029717301));
#43874=CARTESIAN_POINT('Ctrl Pts',(0.316140874837186,2.16258099947833,9.69107096060646));
#43875=CARTESIAN_POINT('Ctrl Pts',(0.316239231772965,2.16208206279994,9.69103984338694));
#43876=CARTESIAN_POINT('Ctrl Pts',(0.316407246904658,2.16121900982434,9.69098597679048));
#43877=CARTESIAN_POINT('Ctrl Pts',(0.316477458722706,2.1608550012424,9.69096324511032));
#43878=CARTESIAN_POINT('Ctrl Pts',(0.316621674550341,2.16010032386752,9.69091609074094));
#43879=CARTESIAN_POINT('Ctrl Pts',(0.316695583922795,2.1597096377952,9.69089166507675));
#43880=CARTESIAN_POINT('Ctrl Pts',(0.316866959808635,2.1587944724058,9.69083441460974));
#43881=CARTESIAN_POINT('Ctrl Pts',(0.31696384724667,2.15826988705133,9.69080157142553));
#43882=CARTESIAN_POINT('Ctrl Pts',(0.317272539779687,2.15657495645995,9.69069536861242));
#43883=CARTESIAN_POINT('Ctrl Pts',(0.317479166862667,2.15540368890333,9.69062184449973));
#43884=CARTESIAN_POINT('Ctrl Pts',(0.320347110052166,2.13860368757796,9.68956527917788));
#43885=CARTESIAN_POINT('Ctrl Pts',(0.321857732102564,2.12280302647857,9.68854539866703));
#43886=CARTESIAN_POINT('Ctrl Pts',(0.322765895945265,2.08074538670313,9.6857623188952));
#43887=CARTESIAN_POINT('Ctrl Pts',(0.320131327700838,2.0545650565599,9.68395303870373));
#43888=CARTESIAN_POINT('Ctrl Pts',(0.313751729094932,2.0263213945268,9.68204242564132));
#43889=CARTESIAN_POINT('Ctrl Pts',(0.313113903708506,2.02365624738803,9.68186266548118));
#43890=CARTESIAN_POINT('Ctrl Pts',(0.311045257683612,2.01547488020574,9.68131310887575));
#43891=CARTESIAN_POINT('Ctrl Pts',(0.309501974975,2.00998785831035,9.68094771684389));
#43892=CARTESIAN_POINT('Ctrl Pts',(0.307619959387924,2.00391896756355,9.68054932246434));
#43893=CARTESIAN_POINT('Ctrl Pts',(0.307424145800625,2.00329426695134,9.68050838246976));
#43894=CARTESIAN_POINT('Ctrl Pts',(0.307138134588658,2.00239145848262,9.68044932045833));
#43895=CARTESIAN_POINT('Ctrl Pts',(0.30704946158886,2.00211287502759,9.68043110977744));
#43896=CARTESIAN_POINT('Ctrl Pts',(0.306892976049632,2.00162355014508,9.68039914885447));
#43897=CARTESIAN_POINT('Ctrl Pts',(0.306825325329854,2.0014127575592,9.6803853890412));
#43898=CARTESIAN_POINT('Ctrl Pts',(0.306694890901151,2.00100777216361,9.68035896930418));
#43899=CARTESIAN_POINT('Ctrl Pts',(0.306632140132289,2.0008135699033,9.68034630745979));
#43900=CARTESIAN_POINT('Ctrl Pts',(0.306464553154103,2.00029659757223,9.6803126200624));
#43901=CARTESIAN_POINT('Ctrl Pts',(0.306359391154507,1.99997393214978,9.68029161380569));
#43902=CARTESIAN_POINT('Ctrl Pts',(0.305965644879077,1.9987722581922,9.68021345285742));
#43903=CARTESIAN_POINT('Ctrl Pts',(0.305673782034734,1.99789431659462,9.68015648978955));
#43904=CARTESIAN_POINT('Ctrl Pts',(0.304942640766353,1.99572623129545,9.68001614052509));
#43905=CARTESIAN_POINT('Ctrl Pts',(0.30449894716187,1.99443758091691,9.67993300333779));
#43906=CARTESIAN_POINT('Ctrl Pts',(0.29459374035864,1.96625134973172,9.67811997973813));
#43907=CARTESIAN_POINT('Ctrl Pts',(0.281610634958944,1.94071974251957,9.67657783164741));
#43908=CARTESIAN_POINT('Ctrl Pts',(0.254054139738275,1.90070045060612,9.67384227256632));
#43909=CARTESIAN_POINT('Ctrl Pts',(0.241157391568482,1.88527518302982,9.67268848181439));
#43910=CARTESIAN_POINT('Ctrl Pts',(0.225990983968544,1.87023722719579,9.67139126148756));
#43911=CARTESIAN_POINT('Ctrl Pts',(0.225064822218721,1.86932992754876,9.67131227304987));
#43912=CARTESIAN_POINT('Ctrl Pts',(0.223765851833434,1.86807268257528,9.67120179482591));
#43913=CARTESIAN_POINT('Ctrl Pts',(0.223397638424758,1.86771799002923,9.67117051193214));
#43914=CARTESIAN_POINT('Ctrl Pts',(0.22276046617002,1.8671071312891,9.6711164362519));
#43915=CARTESIAN_POINT('Ctrl Pts',(0.22249190483519,1.86685055036391,9.67109366148995));
#43916=CARTESIAN_POINT('Ctrl Pts',(0.221935245502373,1.86632056106337,9.67104649113982));
#43917=CARTESIAN_POINT('Ctrl Pts',(0.221647084541177,1.86604721995639,9.67102209270401));
#43918=CARTESIAN_POINT('Ctrl Pts',(0.220972635679982,1.86540982189782,9.6709650332595));
#43919=CARTESIAN_POINT('Ctrl Pts',(0.220585953031272,1.86504618602526,9.67093235423016));
#43920=CARTESIAN_POINT('Ctrl Pts',(0.219340446031754,1.86388069772156,9.67082720546776));
#43921=CARTESIAN_POINT('Ctrl Pts',(0.218478141739201,1.86308259308897,9.67075457579111));
#43922=CARTESIAN_POINT('Ctrl Pts',(0.204884015400362,1.85063789719057,9.66961213293194));
#43923=CARTESIAN_POINT('Ctrl Pts',(0.191243584381455,1.84002955330688,9.66849840762894));
#43924=CARTESIAN_POINT('Ctrl Pts',(0.159422390758528,1.81914629676992,9.66597001102608));
#43925=CARTESIAN_POINT('Ctrl Pts',(0.140958016660451,1.80944010063729,9.66454536184561));
#43926=CARTESIAN_POINT('Ctrl Pts',(0.117050947254558,1.79969126141603,9.66281779162803));
#43927=CARTESIAN_POINT('Ctrl Pts',(0.112369380547921,1.79790831022279,9.66248496547189));
#43928=CARTESIAN_POINT('Ctrl Pts',(0.10569537890864,1.79554318209087,9.66201981266193));
#43929=CARTESIAN_POINT('Ctrl Pts',(0.103736105362701,1.79487004748534,9.66188437853778));
#43930=CARTESIAN_POINT('Ctrl Pts',(0.1008447564537,1.79390775489137,9.661686287607));
#43931=CARTESIAN_POINT('Ctrl Pts',(0.0999176731577746,1.79360387395548,
9.6616230380762));
#43932=CARTESIAN_POINT('Ctrl Pts',(0.0985425931815952,1.79316005279076,
9.6615296324339));
#43933=CARTESIAN_POINT('Ctrl Pts',(0.098095655878483,1.79301687639666,9.66149933680355));
#43934=CARTESIAN_POINT('Ctrl Pts',(0.0938207827218467,1.79165770959473,
9.66121018305601));
#43935=CARTESIAN_POINT('Ctrl Pts',(0.0899705219735288,1.79051233274813,
9.66095448269854));
#43936=CARTESIAN_POINT('Ctrl Pts',(0.0855269045845084,1.78928038771488,
9.66066557237252));
#43937=CARTESIAN_POINT('Ctrl Pts',(0.0849537231626,1.78912318548882,9.66062842346025));
#43938=CARTESIAN_POINT('Ctrl Pts',(0.0841088869527132,1.78889398955743,
9.6605738445402));
#43939=CARTESIAN_POINT('Ctrl Pts',(0.0838375718119742,1.78882076523002,
9.66055634353805));
#43940=CARTESIAN_POINT('Ctrl Pts',(0.0833540208688621,1.7886909396163,9.66052520049876));
#43941=CARTESIAN_POINT('Ctrl Pts',(0.0831418228972066,1.78863420040336,
9.66051155041395));
#43942=CARTESIAN_POINT('Ctrl Pts',(0.0827319949474164,1.78852506611443,
9.66048521933963));
#43943=CARTESIAN_POINT('Ctrl Pts',(0.0825343739693234,1.78847264238746,
9.66047253668263));
#43944=CARTESIAN_POINT('Ctrl Pts',(0.0819932171208717,1.78832963857264,
9.66043784587077));
#43945=CARTESIAN_POINT('Ctrl Pts',(0.0816495798421923,1.788239438093,9.66041585985452));
#43946=CARTESIAN_POINT('Ctrl Pts',(0.0803081056948663,1.78788968805235,
9.66033019643814));
#43947=CARTESIAN_POINT('Ctrl Pts',(0.0793091607788174,1.78763435568414,
9.66026676103446));
#43948=CARTESIAN_POINT('Ctrl Pts',(0.0767871373355638,1.78700259979855,
9.6601074605342));
#43949=CARTESIAN_POINT('Ctrl Pts',(0.0752624850015386,1.78663249120714,
9.66001194094924));
#43950=CARTESIAN_POINT('Ctrl Pts',(0.0690816467831274,1.78517980835601,
9.65962765012849));
#43951=CARTESIAN_POINT('Ctrl Pts',(0.064404110413597,1.78418970449458,9.6593435547836));
#43952=CARTESIAN_POINT('Ctrl Pts',(0.0461472220217545,1.78074777255789,
9.65825466628726));
#43953=CARTESIAN_POINT('Ctrl Pts',(0.0324371090219725,1.77906473163229,
9.65747915312179));
#43954=CARTESIAN_POINT('Ctrl Pts',(-0.00459485485672079,1.77691690260174,
9.65540346189885));
#43955=CARTESIAN_POINT('Ctrl Pts',(-0.0279253700752546,1.77809339996285,
9.65411083291383));
#43956=CARTESIAN_POINT('Ctrl Pts',(-0.0525708204126776,1.78203732300837,
9.65263860172436));
#43957=CARTESIAN_POINT('Ctrl Pts',(-0.0542149651854748,1.78231353109772,
9.65253990278948));
#43958=CARTESIAN_POINT('Ctrl Pts',(-0.0609871603706854,1.78350532880924,
9.65213126043745));
#43959=CARTESIAN_POINT('Ctrl Pts',(-0.0660945622508937,1.78453238722273,
9.65181807030848));
#43960=CARTESIAN_POINT('Ctrl Pts',(-0.0720215679705755,1.78587450998456,
9.65144801434797));
#43961=CARTESIAN_POINT('Ctrl Pts',(-0.0728677325276198,1.78606971591847,
9.6513950258484));
#43962=CARTESIAN_POINT('Ctrl Pts',(-0.0742172705369502,1.7863867977772,
9.65131025934326));
#43963=CARTESIAN_POINT('Ctrl Pts',(-0.0747211611001894,1.78650647226252,
9.65127855218297));
#43964=CARTESIAN_POINT('Ctrl Pts',(-0.0756103630484235,1.78671992421559,
9.65122249783128));
#43965=CARTESIAN_POINT('Ctrl Pts',(-0.0759957948580573,1.78681319943928,
9.6511981668653));
#43966=CARTESIAN_POINT('Ctrl Pts',(-0.0767927284878099,1.78700761664186,
9.65114778896317));
#43967=CARTESIAN_POINT('Ctrl Pts',(-0.0772042047549721,1.78710885925895,
9.65112173882189));
#43968=CARTESIAN_POINT('Ctrl Pts',(-0.0782580297563936,1.7873703553762,
9.65105492217032));
#43969=CARTESIAN_POINT('Ctrl Pts',(-0.0789000842249391,1.78753177662712,
9.65101411801351));
#43970=CARTESIAN_POINT('Ctrl Pts',(-0.0815261491698611,1.78820061513566,
9.65084683091554));
#43971=CARTESIAN_POINT('Ctrl Pts',(-0.083505764720183,1.78872495065035,
9.65071980180084));
#43972=CARTESIAN_POINT('Ctrl Pts',(-0.0965745684920587,1.79232008894459,
9.64987493425429));
#43973=CARTESIAN_POINT('Ctrl Pts',(-0.107496235180663,1.79596368469782,
9.64913847784199));
#43974=CARTESIAN_POINT('Ctrl Pts',(-0.129395424622546,1.80459713889712,
9.64759771418822));
#43975=CARTESIAN_POINT('Ctrl Pts',(-0.140335201254751,1.80963468491326,
9.64679301073633));
#43976=CARTESIAN_POINT('Ctrl Pts',(-0.160825555686133,1.82049895660885,
9.64522823538065));
#43977=CARTESIAN_POINT('Ctrl Pts',(-0.17040606698088,1.82623465177606,9.64447028875704));
#43978=CARTESIAN_POINT('Ctrl Pts',(-0.19150560710119,1.84040408036623,9.64276092390233));
#43979=CARTESIAN_POINT('Ctrl Pts',(-0.202802618122204,1.84913022313688,
9.64181587047063));
#43980=CARTESIAN_POINT('Ctrl Pts',(-0.214160064984539,1.85917339731651,
9.64086250368771));
#43981=CARTESIAN_POINT('Ctrl Pts',(-0.214831935488261,1.85977255457693,
9.64080609495576));
#43982=CARTESIAN_POINT('Ctrl Pts',(-0.215733708240548,1.86058354180188,
9.64073038054132));
#43983=CARTESIAN_POINT('Ctrl Pts',(-0.215965817402716,1.86079289508265,
9.64071089192738));
#43984=CARTESIAN_POINT('Ctrl Pts',(-0.216356540145974,1.86114634379626,
9.6406780856364));
#43985=CARTESIAN_POINT('Ctrl Pts',(-0.216515314616055,1.86129025976481,
9.64066475444523));
#43986=CARTESIAN_POINT('Ctrl Pts',(-0.216819916785194,1.86156691044629,
9.64063917932997));
#43987=CARTESIAN_POINT('Ctrl Pts',(-0.216965765125472,1.86169961965489,
9.64062693368429));
#43988=CARTESIAN_POINT('Ctrl Pts',(-0.217266714589235,1.86197396261683,
9.64060166565402));
#43989=CARTESIAN_POINT('Ctrl Pts',(-0.217421798549298,1.86211561367562,
9.64058864470244));
#43990=CARTESIAN_POINT('Ctrl Pts',(-0.217771890320768,1.86243600990774,
9.64055925059881));
#43991=CARTESIAN_POINT('Ctrl Pts',(-0.217966817056536,1.86261484404903,
9.64054288421044));
#43992=CARTESIAN_POINT('Ctrl Pts',(-0.218879440232389,1.86345419547722,
9.64046625697669));
#43993=CARTESIAN_POINT('Ctrl Pts',(-0.219594365894017,1.86411773801526,
9.64040622392944));
#43994=CARTESIAN_POINT('Ctrl Pts',(-0.227868223018751,1.87186715451755,
9.63971124320402));
#43995=CARTESIAN_POINT('Ctrl Pts',(-0.235085117380544,1.87931117101581,
9.63910287960286));
#43996=CARTESIAN_POINT('Ctrl Pts',(-0.246446218813147,1.89222094044135,
9.63811526922609));
#43997=CARTESIAN_POINT('Ctrl Pts',(-0.250796775581789,1.89749355473368,
9.63772882436611));
#43998=CARTESIAN_POINT('Ctrl Pts',(-0.267409485491206,1.91898450258699,
9.63620240134716));
#43999=CARTESIAN_POINT('Ctrl Pts',(-0.278292231497932,1.93620789944952,
9.63508166515518));
#44000=CARTESIAN_POINT('Ctrl Pts',(-0.289465650486568,1.95826040287656,
9.63365841333895));
#44001=CARTESIAN_POINT('Ctrl Pts',(-0.291370859629078,1.96221939135869,
9.63340349084786));
#44002=CARTESIAN_POINT('Ctrl Pts',(-0.293948058140469,1.96786745300775,
9.6330397951582));
#44003=CARTESIAN_POINT('Ctrl Pts',(-0.294687645890394,1.9695252436679,9.63293304483894));
#44004=CARTESIAN_POINT('Ctrl Pts',(-0.298025339558335,1.97717986953488,
9.63243997253386));
#44005=CARTESIAN_POINT('Ctrl Pts',(-0.300454513442979,1.9832482821958,9.63204856364141));
#44006=CARTESIAN_POINT('Ctrl Pts',(-0.303052461128865,1.99035762013918,
9.63158789255539));
#44007=CARTESIAN_POINT('Ctrl Pts',(-0.303402821716402,1.99133089954722,
9.6315247817099));
#44008=CARTESIAN_POINT('Ctrl Pts',(-0.303916853318795,1.99278071188368,
9.63143069921532));
#44009=CARTESIAN_POINT('Ctrl Pts',(-0.304084104740397,1.99325597574082,
9.63139984658037));
#44010=CARTESIAN_POINT('Ctrl Pts',(-0.304379924156572,1.99410291755908,
9.63134484474805));
#44011=CARTESIAN_POINT('Ctrl Pts',(-0.304508927864861,1.99447444315486,
9.631320710057));
#44012=CARTESIAN_POINT('Ctrl Pts',(-0.304778981913126,1.99525680693905,
9.63126987135502));
#44013=CARTESIAN_POINT('Ctrl Pts',(-0.304919882252861,1.99566769573825,
9.63124316243321));
#44014=CARTESIAN_POINT('Ctrl Pts',(-0.305288802220212,1.99675065839842,
9.63117274248554));
#44015=CARTESIAN_POINT('Ctrl Pts',(-0.305515432337938,1.99742320002702,
9.63112898561881));
#44016=CARTESIAN_POINT('Ctrl Pts',(-0.306521456895406,2.00044156275256,
9.63093249002478));
#44017=CARTESIAN_POINT('Ctrl Pts',(-0.307276051298396,2.00279550568328,
9.63077893630882));
#44018=CARTESIAN_POINT('Ctrl Pts',(-0.312616496928581,2.02013880424848,
9.62964504455104));
#44019=CARTESIAN_POINT('Ctrl Pts',(-0.316129707743057,2.03543404583506,
9.62862959870862));
#44020=CARTESIAN_POINT('Ctrl Pts',(-0.321031559363108,2.06724720442419,
9.62649063397092));
#44021=CARTESIAN_POINT('Ctrl Pts',(-0.322287987666894,2.08374034465902,
9.62536730016875));
#44022=CARTESIAN_POINT('Ctrl Pts',(-0.322274898786015,2.10025541625633,
9.62425288911819));
#44023=CARTESIAN_POINT('',(-0.322274974372014,2.0998714756124,9.37464719300612));
#44024=CARTESIAN_POINT('Ctrl Pts',(-0.32227489852238,2.1002557486849,9.62425286668644));
#44025=CARTESIAN_POINT('Ctrl Pts',(-0.322262200382935,2.11625697114477,
9.62317312952553));
#44026=CARTESIAN_POINT('Ctrl Pts',(-0.32105779650295,2.13223770964696,9.62210508086643));
#44027=CARTESIAN_POINT('Ctrl Pts',(-0.318559698462321,2.14880006876696,
9.62104974482184));
#44028=CARTESIAN_POINT('Ctrl Pts',(-0.318446288819205,2.14953472881498,
9.62100304252109));
#44029=CARTESIAN_POINT('Ctrl Pts',(-0.318267537075045,2.15066668100986,
9.62093126009712));
#44030=CARTESIAN_POINT('Ctrl Pts',(-0.318203991608626,2.15106424824529,
9.6209060819385));
#44031=CARTESIAN_POINT('Ctrl Pts',(-0.318097551833309,2.15172226614342,
9.62086446587441));
#44032=CARTESIAN_POINT('Ctrl Pts',(-0.318055082501554,2.15198278362567,
9.62084800425017));
#44033=CARTESIAN_POINT('Ctrl Pts',(-0.317978271682708,2.15245034230063,
9.62081848681461));
#44034=CARTESIAN_POINT('Ctrl Pts',(-0.317944047994441,2.15265740228388,
9.62080542433574));
#44035=CARTESIAN_POINT('Ctrl Pts',(-0.317877288140574,2.15305887450531,
9.62078011573428));
#44036=CARTESIAN_POINT('Ctrl Pts',(-0.317844775902008,2.15325329015126,
9.62076786828978));
#44037=CARTESIAN_POINT('Ctrl Pts',(-0.317776494501317,2.15365930693899,
9.62074230842603));
#44038=CARTESIAN_POINT('Ctrl Pts',(-0.317740692463515,2.15387090153504,
9.62072899795028));
#44039=CARTESIAN_POINT('Ctrl Pts',(-0.317652038852291,2.15439169268582,
9.62069626151754));
#44040=CARTESIAN_POINT('Ctrl Pts',(-0.31759894702101,2.15470084892705,9.62067684928027));
#44041=CARTESIAN_POINT('Ctrl Pts',(-0.317390446015414,2.15590442321913,
9.62060135579262));
#44042=CARTESIAN_POINT('Ctrl Pts',(-0.31723170734028,2.15679827164526,9.62054546216686));
#44043=CARTESIAN_POINT('Ctrl Pts',(-0.314185992258422,2.17353736242995,
9.6195017760887));
#44044=CARTESIAN_POINT('Ctrl Pts',(-0.310118498624611,2.1891473767991,9.61857899885584));
#44045=CARTESIAN_POINT('Ctrl Pts',(-0.303523922562006,2.20840871653887,
9.61743207485421));
#44046=CARTESIAN_POINT('Ctrl Pts',(-0.302068576776011,2.21240016502262,
9.61719397365354));
#44047=CARTESIAN_POINT('Ctrl Pts',(-0.299115915760111,2.22002618872931,
9.61673639628704));
#44048=CARTESIAN_POINT('Ctrl Pts',(-0.297630190971355,2.22366441101369,
9.61651690271767));
#44049=CARTESIAN_POINT('Ctrl Pts',(-0.29278406786216,2.23493792828201,9.6158308302073));
#44050=CARTESIAN_POINT('Ctrl Pts',(-0.289193613252246,2.24247036002145,
9.61536370601801));
#44051=CARTESIAN_POINT('Ctrl Pts',(-0.277972408313161,2.26383489276387,
9.61399617820118));
#44052=CARTESIAN_POINT('Ctrl Pts',(-0.269613145963772,2.27725457793182,
9.61308221121115));
#44053=CARTESIAN_POINT('Ctrl Pts',(-0.258841199852033,2.29201190703257,
9.61198032464317));
#44054=CARTESIAN_POINT('Ctrl Pts',(-0.257354390451935,2.29400014527333,
9.6118297288318));
#44055=CARTESIAN_POINT('Ctrl Pts',(-0.255412555826358,2.29653525689399,
9.61163485739529));
#44056=CARTESIAN_POINT('Ctrl Pts',(-0.254978459021187,2.29709811338156,
9.61159140779182));
#44057=CARTESIAN_POINT('Ctrl Pts',(-0.254275939551286,2.29800280576156,
9.6115212719459));
#44058=CARTESIAN_POINT('Ctrl Pts',(-0.2540086795961,2.29834554497405,9.61149463186924));
#44059=CARTESIAN_POINT('Ctrl Pts',(-0.253498295711054,2.29899734753555,
9.61144383636427));
#44060=CARTESIAN_POINT('Ctrl Pts',(-0.253255297658299,2.29930650882603,
9.61141968597809));
#44061=CARTESIAN_POINT('Ctrl Pts',(-0.252699948816612,2.3000104119233,9.61136456898333));
#44062=CARTESIAN_POINT('Ctrl Pts',(-0.252387238360407,2.30040486750044,
9.61133358803049));
#44063=CARTESIAN_POINT('Ctrl Pts',(-0.251430539233022,2.30160586499184,
9.61123897106904));
#44064=CARTESIAN_POINT('Ctrl Pts',(-0.250783603796875,2.30241004146305,
9.61117521687842));
#44065=CARTESIAN_POINT('Ctrl Pts',(-0.246043343329121,2.30824483490925,
9.61070969752524));
#44066=CARTESIAN_POINT('Ctrl Pts',(-0.241803108043954,2.31315366557734,
9.61030198837819));
#44067=CARTESIAN_POINT('Ctrl Pts',(-0.23702695959817,2.31835688745248,9.60985142922304));
#44068=CARTESIAN_POINT('Ctrl Pts',(-0.236634860480233,2.31878174666313,
9.60981450207376));
#44069=CARTESIAN_POINT('Ctrl Pts',(-0.219260692004582,2.33750618960886,
9.6081809467608));
#44070=CARTESIAN_POINT('Ctrl Pts',(-0.200213234783425,2.35376898319434,
9.60649414298764));
#44071=CARTESIAN_POINT('Ctrl Pts',(-0.169107449288632,2.37462694249824,
9.60396166265019));
#44072=CARTESIAN_POINT('Ctrl Pts',(-0.158333428910285,2.38097661047446,
9.60312056227439));
#44073=CARTESIAN_POINT('Ctrl Pts',(-0.143380544254812,2.38865515258379,
9.60202291003595));
#44074=CARTESIAN_POINT('Ctrl Pts',(-0.139504468742105,2.3905482486897,9.60174440643881));
#44075=CARTESIAN_POINT('Ctrl Pts',(-0.134270435620357,2.39297567453766,
9.60137742851918));
#44076=CARTESIAN_POINT('Ctrl Pts',(-0.132945349283149,2.39357934198294,
9.60128528981925));
#44077=CARTESIAN_POINT('Ctrl Pts',(-0.130726949434735,2.39457187467758,
9.60113236892195));
#44078=CARTESIAN_POINT('Ctrl Pts',(-0.129835896943699,2.39496570068809,
9.60107130256961));
#44079=CARTESIAN_POINT('Ctrl Pts',(-0.128701317121672,2.39546102310331,
9.60099401158509));
#44080=CARTESIAN_POINT('Ctrl Pts',(-0.128459444896338,2.39556626367063,
9.60097756129436));
#44081=CARTESIAN_POINT('Ctrl Pts',(-0.128024947095562,2.3957546830887,9.60094805849397));
#44082=CARTESIAN_POINT('Ctrl Pts',(-0.127832369349131,2.39583797084706,
9.60093499933557));
#44083=CARTESIAN_POINT('Ctrl Pts',(-0.12745873450257,2.39599913085923,9.60090969550594));
#44084=CARTESIAN_POINT('Ctrl Pts',(-0.127277687473913,2.39607702501623,
9.60089744951695));
#44085=CARTESIAN_POINT('Ctrl Pts',(-0.126899269591281,2.39623942529309,
9.60087188506872));
#44086=CARTESIAN_POINT('Ctrl Pts',(-0.126701886352943,2.39632390000818,
9.60085856856663));
#44087=CARTESIAN_POINT('Ctrl Pts',(-0.126215593575093,2.39653144551308,
9.60082580454638));
#44088=CARTESIAN_POINT('Ctrl Pts',(-0.125926587550521,2.39665429170909,
9.60080637079407));
#44089=CARTESIAN_POINT('Ctrl Pts',(-0.12479918848569,2.39713156462441,9.60073070716098));
#44090=CARTESIAN_POINT('Ctrl Pts',(-0.123959464514552,2.39748286563609,
9.60067466597537));
#44091=CARTESIAN_POINT('Ctrl Pts',(-0.109602727176092,2.40341770357699,
9.59972172271853));
#44092=CARTESIAN_POINT('Ctrl Pts',(-0.0957205202169412,2.4080791540464,
9.59887836496327));
#44093=CARTESIAN_POINT('Ctrl Pts',(-0.0647724982464628,2.41617572595831,
9.59706923663539));
#44094=CARTESIAN_POINT('Ctrl Pts',(-0.047649535788878,2.41920542803547,
9.5961120391964));
#44095=CARTESIAN_POINT('Ctrl Pts',(-0.0277172395205832,2.42109189847781,
9.59497935859231));
#44096=CARTESIAN_POINT('Ctrl Pts',(-0.0250658405173782,2.42130975075981,
9.59482835755838));
#44097=CARTESIAN_POINT('Ctrl Pts',(-0.0120856330054162,2.42221462852288,
9.59408668449346));
#44098=CARTESIAN_POINT('Ctrl Pts',(-0.0017313098922815,2.42243651090348,
9.5934872682096));
#44099=CARTESIAN_POINT('Ctrl Pts',(0.0141499249286719,2.42201181827835,
9.59254417541785));
#44100=CARTESIAN_POINT('Ctrl Pts',(0.0196797071634084,2.42172120682249,
9.59221142530428));
#44101=CARTESIAN_POINT('Ctrl Pts',(0.0261088941127144,2.42121695821156,
9.59181856411351));
#44102=CARTESIAN_POINT('Ctrl Pts',(0.027018456789112,2.42114173126566,9.59176284510302));
#44103=CARTESIAN_POINT('Ctrl Pts',(0.0284047419802902,2.42102114504787,
9.5916777058286));
#44104=CARTESIAN_POINT('Ctrl Pts',(0.0288817084638099,2.42097858471723,
9.59164837360437));
#44105=CARTESIAN_POINT('Ctrl Pts',(0.0297104511044625,2.42090277277109,
9.59159733939132));
#44106=CARTESIAN_POINT('Ctrl Pts',(0.0300622716399671,2.42087000529694,
9.59157565266798));
#44107=CARTESIAN_POINT('Ctrl Pts',(0.0307949967019486,2.4208005458817,9.59153044133358));
#44108=CARTESIAN_POINT('Ctrl Pts',(0.0311758910053264,2.4207637539965,9.59150691360876));
#44109=CARTESIAN_POINT('Ctrl Pts',(0.0321068169729162,2.42067215885965,
9.59144934806742));
#44110=CARTESIAN_POINT('Ctrl Pts',(0.0326567734245254,2.42061661888814,
9.59141528710243));
#44111=CARTESIAN_POINT('Ctrl Pts',(0.0347566106547962,2.42039909802098,
9.59128503011621));
#44112=CARTESIAN_POINT('Ctrl Pts',(0.0363054324183795,2.42022729339774,
9.59118852513341));
#44113=CARTESIAN_POINT('Ctrl Pts',(0.0639137852114066,2.41696194218873,
9.58946046070311));
#44114=CARTESIAN_POINT('Ctrl Pts',(0.0894947956353229,2.41070877779957,
9.58772234137034));
#44115=CARTESIAN_POINT('Ctrl Pts',(0.125759547124205,2.39698990098813,9.58510099455854));
#44116=CARTESIAN_POINT('Ctrl Pts',(0.137220981084427,2.39187134585129,9.58424942537694));
#44117=CARTESIAN_POINT('Ctrl Pts',(0.154585295669267,2.38286713023584,9.5829456135246));
#44118=CARTESIAN_POINT('Ctrl Pts',(0.16070867663877,2.37943364438964,9.5824831341886));
#44119=CARTESIAN_POINT('Ctrl Pts',(0.170394335078156,2.37357892060517,9.58175261457821));
#44120=CARTESIAN_POINT('Ctrl Pts',(0.174028602965502,2.37128159736772,9.58147875662744));
#44121=CARTESIAN_POINT('Ctrl Pts',(0.17807485841601,2.36860905195801,9.58117509203288));
#44122=CARTESIAN_POINT('Ctrl Pts',(0.178532916415187,2.36830481874274,9.58114073380981));
#44123=CARTESIAN_POINT('Ctrl Pts',(0.179174893619348,2.36787605800137,9.58109260830749));
#44124=CARTESIAN_POINT('Ctrl Pts',(0.179359462830936,2.36775251268208,9.58107877545264));
#44125=CARTESIAN_POINT('Ctrl Pts',(0.179729637470673,2.3675041739151,9.58105103891933));
#44126=CARTESIAN_POINT('Ctrl Pts',(0.179915241297113,2.36737937765932,9.58103713541177));
#44127=CARTESIAN_POINT('Ctrl Pts',(0.180270957688532,2.36713966306584,9.58101049569891));
#44128=CARTESIAN_POINT('Ctrl Pts',(0.180441090084959,2.36702477558911,9.5809977574241));
#44129=CARTESIAN_POINT('Ctrl Pts',(0.180842396925008,2.3667532213209,9.58096771726819));
#44130=CARTESIAN_POINT('Ctrl Pts',(0.181073478187405,2.3665964161596,9.58095042480586));
#44131=CARTESIAN_POINT('Ctrl Pts',(0.181874238109931,2.36605152185603,9.58089051905368));
#44132=CARTESIAN_POINT('Ctrl Pts',(0.182442880431044,2.36566190199324,9.58084800882122));
#44133=CARTESIAN_POINT('Ctrl Pts',(0.189277482867107,2.36094670496566,9.58033738346792));
#44134=CARTESIAN_POINT('Ctrl Pts',(0.19539009704611,2.35640179442417,9.5798838542713));
#44135=CARTESIAN_POINT('Ctrl Pts',(0.204583388007249,2.34904638882819,9.57919700659558));
#44136=CARTESIAN_POINT('Ctrl Pts',(0.207779810020162,2.34638591538527,9.57895725704352));
#44137=CARTESIAN_POINT('Ctrl Pts',(0.227227294108857,2.32955152005743,9.57748654493841));
#44138=CARTESIAN_POINT('Ctrl Pts',(0.242073486590309,2.31383789687348,9.57630693256959));
#44139=CARTESIAN_POINT('Ctrl Pts',(0.264664552003215,2.28453229202876,9.5742078271869));
#44140=CARTESIAN_POINT('Ctrl Pts',(0.273197779444786,2.27164606688306,9.57331323507061));
#44141=CARTESIAN_POINT('Ctrl Pts',(0.281976865919095,2.25606480793316,9.57223444345279));
#44142=CARTESIAN_POINT('Ctrl Pts',(0.283155031914784,2.25391687554846,9.57208582322332));
#44143=CARTESIAN_POINT('Ctrl Pts',(0.284641681938783,2.25113169407895,9.57189315725605));
#44144=CARTESIAN_POINT('Ctrl Pts',(0.28497273514287,2.25050653229922,9.57184991454794));
#44145=CARTESIAN_POINT('Ctrl Pts',(0.285503502177493,2.24949620097949,9.57178003250549));
#44146=CARTESIAN_POINT('Ctrl Pts',(0.285704502469419,2.24911170688011,9.57175343873018));
#44147=CARTESIAN_POINT('Ctrl Pts',(0.286086277894366,2.24837780155266,9.5717026785355));
#44148=CARTESIAN_POINT('Ctrl Pts',(0.286267190987562,2.24802846265149,9.57167851704167));
#44149=CARTESIAN_POINT('Ctrl Pts',(0.28667878307703,2.2472301116744,9.57162330068709));
#44150=CARTESIAN_POINT('Ctrl Pts',(0.286909047234248,2.24678088792719,9.5715922312924));
#44151=CARTESIAN_POINT('Ctrl Pts',(0.287610149502256,2.24540515000235,9.57149708159677));
#44152=CARTESIAN_POINT('Ctrl Pts',(0.288077558600378,2.24447690450115,9.57143288115675));
#44153=CARTESIAN_POINT('Ctrl Pts',(0.291498511127966,2.2376005002462,9.57095726035912));
#44154=CARTESIAN_POINT('Ctrl Pts',(0.294271866965297,2.2315649550397,9.57053960211202));
#44155=CARTESIAN_POINT('Ctrl Pts',(0.29769817705045,2.22345705565405,9.56997768814089));
#44156=CARTESIAN_POINT('Ctrl Pts',(0.298519620662459,2.22145733793528,9.56983903659537));
#44157=CARTESIAN_POINT('Ctrl Pts',(0.30461196548733,2.20619092602549,9.56878005247665));
#44158=CARTESIAN_POINT('Ctrl Pts',(0.309015694559345,2.19259687341035,9.56783327375727));
#44159=CARTESIAN_POINT('Ctrl Pts',(0.317052240468025,2.16070832568831,9.56562049512444));
#44160=CARTESIAN_POINT('Ctrl Pts',(0.320028753029072,2.14229940775301,9.56434813988974));
#44161=CARTESIAN_POINT('Ctrl Pts',(0.322002352563823,2.11557606543788,9.56257572151944));
#44162=CARTESIAN_POINT('Ctrl Pts',(0.322294072033266,2.10739498105171,9.56204346907199));
#44163=CARTESIAN_POINT('Ctrl Pts',(0.322271937457032,2.09835464559558,9.56147291617144));
#44164=CARTESIAN_POINT('Ctrl Pts',(0.322266428092087,2.09749835518705,9.56141904902585));
#44165=CARTESIAN_POINT('Ctrl Pts',(0.32225085192922,2.09600351792167,9.56132532983165));
#44166=CARTESIAN_POINT('Ctrl Pts',(0.322242299990887,2.09536496480488,9.56128539669779));
#44167=CARTESIAN_POINT('Ctrl Pts',(0.32222707184162,2.09443447573501,9.56122735829162));
#44168=CARTESIAN_POINT('Ctrl Pts',(0.322221896895899,2.09414252184006,9.56120916966992));
#44169=CARTESIAN_POINT('Ctrl Pts',(0.322212099423005,2.09362915592398,9.56117722586175));
#44170=CARTESIAN_POINT('Ctrl Pts',(0.322207645462111,2.09340774122246,9.56116346116637));
#44171=CARTESIAN_POINT('Ctrl Pts',(0.322198555549368,2.09297789993895,9.561136763985));
#44172=CARTESIAN_POINT('Ctrl Pts',(0.322193945597875,2.09276947387359,9.56112383004818));
#44173=CARTESIAN_POINT('Ctrl Pts',(0.322182406982745,2.09226972360657,9.56109284464231));
#44174=CARTESIAN_POINT('Ctrl Pts',(0.322175285414927,2.09197840342102,9.56107480405686));
#44175=CARTESIAN_POINT('Ctrl Pts',(0.322152374648972,2.09109049388134,9.56101988379818));
#44176=CARTESIAN_POINT('Ctrl Pts',(0.322135323297227,2.09049393410301,9.56098307440614));
#44177=CARTESIAN_POINT('Ctrl Pts',(0.321929495049367,2.08393118524587,9.5605790899159));
#44178=CARTESIAN_POINT('Ctrl Pts',(0.321576636889494,2.07797083062628,9.56022087105718));
#44179=CARTESIAN_POINT('Ctrl Pts',(0.320849482351277,2.06962607213052,9.55972727286096));
#44180=CARTESIAN_POINT('Ctrl Pts',(0.320613746052935,2.06723123117278,9.55958653631537));
#44181=CARTESIAN_POINT('Ctrl Pts',(0.317112316144761,2.03532958863653,9.55772145355924));
#44182=CARTESIAN_POINT('Ctrl Pts',(0.309811651127446,2.00640765961136,9.55612782221892));
#44183=CARTESIAN_POINT('Ctrl Pts',(0.294402274104891,1.96840795179206,9.55376650848369));
#44184=CARTESIAN_POINT('Ctrl Pts',(0.289602167492814,1.95815604146774,9.55310166458326));
#44185=CARTESIAN_POINT('Ctrl Pts',(0.283318703559918,1.94639077166714,9.55229512733951));
#44186=CARTESIAN_POINT('Ctrl Pts',(0.282347152558168,1.94461220135647,9.55217199681078));
#44187=CARTESIAN_POINT('Ctrl Pts',(0.281037339644572,1.9422672380458,9.55200800690835));
#44188=CARTESIAN_POINT('Ctrl Pts',(0.28071400674343,1.94169252425718,9.55196768325072));
#44189=CARTESIAN_POINT('Ctrl Pts',(0.280180290848348,1.9407506379302,9.55190137847451));
#44190=CARTESIAN_POINT('Ctrl Pts',(0.279970943418237,1.94038287830468,9.55187543469108));
#44191=CARTESIAN_POINT('Ctrl Pts',(0.279563896009068,1.93967108458481,9.55182511353908));
#44192=CARTESIAN_POINT('Ctrl Pts',(0.279366283698531,1.93932700102315,9.55180073936971));
#44193=CARTESIAN_POINT('Ctrl Pts',(0.278908566316841,1.93853341842758,9.55174441049451));
#44194=CARTESIAN_POINT('Ctrl Pts',(0.278648009691453,1.93808418230589,9.55171243947689));
#44195=CARTESIAN_POINT('Ctrl Pts',(0.277810078809478,1.9366474849296,9.55160992250343));
#44196=CARTESIAN_POINT('Ctrl Pts',(0.277228537538048,1.93566247540991,9.55153922533839));
#44197=CARTESIAN_POINT('Ctrl Pts',(0.271822131594927,1.92661551753557,9.55088606290102));
#44198=CARTESIAN_POINT('Ctrl Pts',(0.266652572284206,1.91876582547396,9.55029096810441));
#44199=CARTESIAN_POINT('Ctrl Pts',(0.2575564174807,1.90618711625269,9.54928780248056));
#44200=CARTESIAN_POINT('Ctrl Pts',(0.253824097440571,1.90132422772779,9.54888686715949));
#44201=CARTESIAN_POINT('Ctrl Pts',(0.23546340181205,1.878764235516,9.54696487238793));
#44202=CARTESIAN_POINT('Ctrl Pts',(0.219110156697215,1.86255764209322,9.5453904925347));
#44203=CARTESIAN_POINT('Ctrl Pts',(0.196200223475837,1.84425164395871,9.5434303131087));
#44204=CARTESIAN_POINT('Ctrl Pts',(0.191106881836289,1.84042357958275,9.54300847770785));
#44205=CARTESIAN_POINT('Ctrl Pts',(0.181618528278885,1.83372307855538,9.54225199652814));
#44206=CARTESIAN_POINT('Ctrl Pts',(0.177260359660562,1.83080218932308,9.54191522249682));
#44207=CARTESIAN_POINT('Ctrl Pts',(0.172272005362578,1.82763265094092,9.54154330565076));
#44208=CARTESIAN_POINT('Ctrl Pts',(0.171710369556634,1.82727822663,9.54150162166511));
#44209=CARTESIAN_POINT('Ctrl Pts',(0.170706536442728,1.82664908078055,9.54142746208543));
#44210=CARTESIAN_POINT('Ctrl Pts',(0.170264763597251,1.82637369112494,9.54139494368331));
#44211=CARTESIAN_POINT('Ctrl Pts',(0.169594624499057,1.82595819526466,9.54134579657827));
#44212=CARTESIAN_POINT('Ctrl Pts',(0.169366750303672,1.82581730307256,9.54132911620578));
#44213=CARTESIAN_POINT('Ctrl Pts',(0.168970518307262,1.825572999496,9.54130016731315));
#44214=CARTESIAN_POINT('Ctrl Pts',(0.168802241245001,1.8254694588682,9.54128789020965));
#44215=CARTESIAN_POINT('Ctrl Pts',(0.168452494093744,1.8252547031193,9.54126240946086));
#44216=CARTESIAN_POINT('Ctrl Pts',(0.168271009577188,1.82514351333658,9.54124920750826));
#44217=CARTESIAN_POINT('Ctrl Pts',(0.167772447948109,1.82483873937888,9.54121299468463));
#44218=CARTESIAN_POINT('Ctrl Pts',(0.167455144778372,1.82464552277536,9.54119000811692));
#44219=CARTESIAN_POINT('Ctrl Pts',(0.166232521407313,1.82390392111312,9.54110166719506));
#44220=CARTESIAN_POINT('Ctrl Pts',(0.165324822862846,1.82335944084633,9.54103656630801));
#44221=CARTESIAN_POINT('Ctrl Pts',(0.148991893445009,1.81367128148101,9.53987352616547));
#44222=CARTESIAN_POINT('Ctrl Pts',(0.132830145442655,1.80582475657567,9.53885537707198));
#44223=CARTESIAN_POINT('Ctrl Pts',(0.0872678167512609,1.788229920304,9.53611492919086));
#44224=CARTESIAN_POINT('Ctrl Pts',(0.0569913055994698,1.78130258358455,
9.53441383211136));
#44225=CARTESIAN_POINT('Ctrl Pts',(0.0241819768845004,1.77862720009411,
9.53242319043524));
#44226=CARTESIAN_POINT('Ctrl Pts',(0.0221700400539088,1.77848214114527,
9.53230063097016));
#44227=CARTESIAN_POINT('Ctrl Pts',(0.0194999424237518,1.77831481045842,
9.53213728876131));
#44228=CARTESIAN_POINT('Ctrl Pts',(0.0188428552820707,1.77827565258498,
9.53209703636636));
#44229=CARTESIAN_POINT('Ctrl Pts',(0.0177634174025764,1.77821464377222,
9.53203081877783));
#44230=CARTESIAN_POINT('Ctrl Pts',(0.0173411332415027,1.77819161046415,
9.53200489072639));
#44231=CARTESIAN_POINT('Ctrl Pts',(0.0165224530627962,1.7781485720087,9.53195457862853));
#44232=CARTESIAN_POINT('Ctrl Pts',(0.0161260628354912,1.77812846778499,
9.53193019773693));
#44233=CARTESIAN_POINT('Ctrl Pts',(0.0152102808405446,1.77808371684926,
9.53187382224672));
#44234=CARTESIAN_POINT('Ctrl Pts',(0.0146908655803926,1.778059594856,9.53184181125095));
#44235=CARTESIAN_POINT('Ctrl Pts',(0.0130251493995336,1.77798627740993,
9.53173903879166));
#44236=CARTESIAN_POINT('Ctrl Pts',(0.0118786529883231,1.77794194684527,
9.53166812505455));
#44237=CARTESIAN_POINT('Ctrl Pts',(0.0012295803227088,1.77758712937605,
9.53100777644001));
#44238=CARTESIAN_POINT('Ctrl Pts',(-0.00828123938175379,1.77769120185321,
9.53040540354889));
#44239=CARTESIAN_POINT('Ctrl Pts',(-0.0484849893704627,1.77991173552702,
9.52780206738453));
#44240=CARTESIAN_POINT('Ctrl Pts',(-0.0787944586706913,1.78599659003403,
9.52567840086594));
#44241=CARTESIAN_POINT('Ctrl Pts',(-0.116587095282174,1.79940711355527,
9.52301290550568));
#44242=CARTESIAN_POINT('Ctrl Pts',(-0.125261250160921,1.80291703217472,
9.52240163803254));
#44243=CARTESIAN_POINT('Ctrl Pts',(-0.134612679942308,1.8071835772769,9.52175229565125));
#44244=CARTESIAN_POINT('Ctrl Pts',(-0.135452470403925,1.80757110380903,
9.52169407098286));
#44245=CARTESIAN_POINT('Ctrl Pts',(-0.136911382833796,1.80825196111897,
9.52159309039891));
#44246=CARTESIAN_POINT('Ctrl Pts',(-0.137531254346956,1.80854365843481,
9.52155023862078));
#44247=CARTESIAN_POINT('Ctrl Pts',(-0.138422226582637,1.80896640490814,
9.52148872774822));
#44248=CARTESIAN_POINT('Ctrl Pts',(-0.138694075758991,1.80909585833935,
9.52146997088275));
#44249=CARTESIAN_POINT('Ctrl Pts',(-0.139166021526329,1.80932140885519,
9.52143742759432));
#44250=CARTESIAN_POINT('Ctrl Pts',(-0.13936620065474,1.80941733187669,9.5214236303044));
#44251=CARTESIAN_POINT('Ctrl Pts',(-0.139753411835051,1.80960337018746,
9.52139695403305));
#44252=CARTESIAN_POINT('Ctrl Pts',(-0.139940455423047,1.80969345914598,
9.52138407344192));
#44253=CARTESIAN_POINT('Ctrl Pts',(-0.140386897085345,1.80990901809716,
9.52135334238382));
#44254=CARTESIAN_POINT('Ctrl Pts',(-0.140646214732792,1.81003465562684,
9.52133550240228));
#44255=CARTESIAN_POINT('Ctrl Pts',(-0.141571868939122,1.81048466229307,
9.52127185677726));
#44256=CARTESIAN_POINT('Ctrl Pts',(-0.142237261285626,1.81081098504613,
9.52122617198096));
#44257=CARTESIAN_POINT('Ctrl Pts',(-0.1524949885873,1.81588556412855,9.52052282116987));
#44258=CARTESIAN_POINT('Ctrl Pts',(-0.161847251649668,1.82110708807086,
9.51989406040356));
#44259=CARTESIAN_POINT('Ctrl Pts',(-0.180688775895657,1.83289434623079,
9.51861791437396));
#44260=CARTESIAN_POINT('Ctrl Pts',(-0.190120169967184,1.83952311101595,
9.51797355961805));
#44261=CARTESIAN_POINT('Ctrl Pts',(-0.20757322411916,1.85324383430506,9.51673251120817));
#44262=CARTESIAN_POINT('Ctrl Pts',(-0.215636241772114,1.86025794772687,
9.5161365362948));
#44263=CARTESIAN_POINT('Ctrl Pts',(-0.232194561016728,1.87617451830043,
9.5148348278502));
#44264=CARTESIAN_POINT('Ctrl Pts',(-0.240558125970735,1.88518867777577,
9.51412700060318));
#44265=CARTESIAN_POINT('Ctrl Pts',(-0.251935142187424,1.89895054453304,
9.51306720596917));
#44266=CARTESIAN_POINT('Ctrl Pts',(-0.255372020243777,1.90333448473139,
9.51273249672363));
#44267=CARTESIAN_POINT('Ctrl Pts',(-0.259238560149989,1.90853882871748,
9.51233753616644));
#44268=CARTESIAN_POINT('Ctrl Pts',(-0.259780564072263,1.90927488450449,
9.51228173127294));
#44269=CARTESIAN_POINT('Ctrl Pts',(-0.260601899006011,1.91040027569842,
9.51219648760874));
#44270=CARTESIAN_POINT('Ctrl Pts',(-0.260883508380502,1.91078794892528,
9.51216713721252));
#44271=CARTESIAN_POINT('Ctrl Pts',(-0.261371298139543,1.91146261641315,
9.51211608277731));
#44272=CARTESIAN_POINT('Ctrl Pts',(-0.2615778735475,1.91174932518128,9.51209439404199));
#44273=CARTESIAN_POINT('Ctrl Pts',(-0.262007079546186,1.91234709643269,
9.51204918961638));
#44274=CARTESIAN_POINT('Ctrl Pts',(-0.262229628604596,1.91265821654128,
9.51202567083189));
#44275=CARTESIAN_POINT('Ctrl Pts',(-0.262772109619359,1.91341945707909,
9.51196814630246));
#44276=CARTESIAN_POINT('Ctrl Pts',(-0.263091438682812,1.91387000382471,
9.51193411747648));
#44277=CARTESIAN_POINT('Ctrl Pts',(-0.264305427773408,1.91559220730796,
9.51180410815769));
#44278=CARTESIAN_POINT('Ctrl Pts',(-0.265192027464228,1.91686949574299,
9.51170782019642));
#44279=CARTESIAN_POINT('Ctrl Pts',(-0.280043615311895,1.9385996040674,9.51007180700548));
#44280=CARTESIAN_POINT('Ctrl Pts',(-0.291611482455007,1.96058420260175,
9.50843811227095));
#44281=CARTESIAN_POINT('Ctrl Pts',(-0.306297162876582,1.99852606400774,
9.50569119760377));
#44282=CARTESIAN_POINT('Ctrl Pts',(-0.31093782209877,2.01378740786188,9.50460637168407));
#44283=CARTESIAN_POINT('Ctrl Pts',(-0.316270759515971,2.03751506230766,
9.50299628840218));
#44284=CARTESIAN_POINT('Ctrl Pts',(-0.317790333033185,2.04577000387048,
9.50245009064185));
#44285=CARTESIAN_POINT('Ctrl Pts',(-0.319172855946122,2.05537286202421,
9.50183767905432));
#44286=CARTESIAN_POINT('Ctrl Pts',(-0.319351712198856,2.05667128582541,
9.50175535679495));
#44287=CARTESIAN_POINT('Ctrl Pts',(-0.319573287332469,2.05835578749012,
9.50164921420182));
#44288=CARTESIAN_POINT('Ctrl Pts',(-0.319623233285,2.05874087785389,9.50162499366399));
#44289=CARTESIAN_POINT('Ctrl Pts',(-0.31970294684166,2.05936431250664,9.5015858553297));
#44290=CARTESIAN_POINT('Ctrl Pts',(-0.319733144027407,2.05960259997779,
9.5015709132452));
#44291=CARTESIAN_POINT('Ctrl Pts',(-0.319790544045989,2.06005964250263,
9.50154228726918));
#44292=CARTESIAN_POINT('Ctrl Pts',(-0.319817788744533,2.06027839100649,
9.50152860107921));
#44293=CARTESIAN_POINT('Ctrl Pts',(-0.319879922981636,2.06078147679054,
9.50149715861155));
#44294=CARTESIAN_POINT('Ctrl Pts',(-0.319914657957807,2.06106583358114,
9.50147941113791));
#44295=CARTESIAN_POINT('Ctrl Pts',(-0.320021037209972,2.06194645831825,
9.50142452409698));
#44296=CARTESIAN_POINT('Ctrl Pts',(-0.320091394492724,2.06254288482971,
9.50138745699609));
#44297=CARTESIAN_POINT('Ctrl Pts',(-0.320657979770469,2.06746408884773,
9.50108246417541));
#44298=CARTESIAN_POINT('Ctrl Pts',(-0.321068231883772,2.07179857236548,
9.50081926665511));
#44299=CARTESIAN_POINT('Ctrl Pts',(-0.321451662752336,2.07696339077266,
9.50051069023453));
#44300=CARTESIAN_POINT('Ctrl Pts',(-0.321509607149703,2.07778672946825,
9.50046165123315));
#44301=CARTESIAN_POINT('Ctrl Pts',(-0.321573059917299,2.07874065310821,
9.5004050012432));
#44302=CARTESIAN_POINT('Ctrl Pts',(-0.321581652130227,2.07887102207547,
9.50039726272073));
#44303=CARTESIAN_POINT('Ctrl Pts',(-0.321736937581211,2.08124919325417,
9.5002561629741));
#44304=CARTESIAN_POINT('Ctrl Pts',(-0.321860142625702,2.08349852052804,
9.50012377032853));
#44305=CARTESIAN_POINT('Ctrl Pts',(-0.322166486079966,2.09041946011863,
9.49971918120443));
#44306=CARTESIAN_POINT('Ctrl Pts',(-0.322271572270834,2.09509403845348,
9.49944978350821));
#44307=CARTESIAN_POINT('Ctrl Pts',(-0.322295821129269,2.12898474965668,
9.49751447770717));
#44308=CARTESIAN_POINT('Ctrl Pts',(-0.318344304100929,2.15806660197144,
9.49593615930897));
#44309=CARTESIAN_POINT('Ctrl Pts',(-0.308064308479255,2.19509124256648,
9.49369466283714));
#44310=CARTESIAN_POINT('Ctrl Pts',(-0.305221972556378,2.20385319172744,
9.49314742522801));
#44311=CARTESIAN_POINT('Ctrl Pts',(-0.301611485794939,2.21354726856676,
9.49251831265556));
#44312=CARTESIAN_POINT('Ctrl Pts',(-0.301208674467113,2.21461153928012,
9.49244892121089));
#44313=CARTESIAN_POINT('Ctrl Pts',(-0.300614231024252,2.216157342835,9.4923476533104));
#44314=CARTESIAN_POINT('Ctrl Pts',(-0.300427057488376,2.21664059033077,
9.49231592650116));
#44315=CARTESIAN_POINT('Ctrl Pts',(-0.300094580688692,2.2174928745377,9.49225984926668));
#44316=CARTESIAN_POINT('Ctrl Pts',(-0.299949759905136,2.21786209932152,
9.49223551510948));
#44317=CARTESIAN_POINT('Ctrl Pts',(-0.299648848407667,2.21862513529977,
9.49218514218138));
#44318=CARTESIAN_POINT('Ctrl Pts',(-0.299492662128992,2.21901890776298,
9.49215910022779));
#44319=CARTESIAN_POINT('Ctrl Pts',(-0.299090617066218,2.22002672999161,
9.49209232860986));
#44320=CARTESIAN_POINT('Ctrl Pts',(-0.298843644294399,2.22064033066911,
9.49205156139769));
#44321=CARTESIAN_POINT('Ctrl Pts',(-0.29782612466657,2.22314604720145,9.49188461277093));
#44322=CARTESIAN_POINT('Ctrl Pts',(-0.297039496269313,2.22503154330978,
9.49175788796263));
#44323=CARTESIAN_POINT('Ctrl Pts',(-0.291721305874853,2.23744539282073,
9.49091611247471));
#44324=CARTESIAN_POINT('Ctrl Pts',(-0.28664925714373,2.24773187516232,9.4901825900059));
#44325=CARTESIAN_POINT('Ctrl Pts',(-0.265070843387969,2.28618103841534,
9.48729720983177));
#44326=CARTESIAN_POINT('Ctrl Pts',(-0.244875425021176,2.31204127611886,
9.48502216988599));
#44327=CARTESIAN_POINT('Ctrl Pts',(-0.220630198403759,2.33491273083497,
9.48285635970915));
#44328=CARTESIAN_POINT('Ctrl Pts',(-0.220114274394814,2.33539622295301,
9.48281050526657));
#44329=CARTESIAN_POINT('Ctrl Pts',(-0.2195051110752,2.3359633393476,9.48275664122028));
#44330=CARTESIAN_POINT('Ctrl Pts',(-0.219413413235177,2.33604860812297,
9.48274854038928));
#44331=CARTESIAN_POINT('Ctrl Pts',(-0.219140485461509,2.33630210409827,
9.48272445118711));
#44332=CARTESIAN_POINT('Ctrl Pts',(-0.218959111167809,2.33647017656975,
9.48270847147154));
#44333=CARTESIAN_POINT('Ctrl Pts',(-0.215627015577904,2.33955077884497,
9.48241543249333));
#44334=CARTESIAN_POINT('Ctrl Pts',(-0.212418438501883,2.34240048871081,
9.48214194529387));
#44335=CARTESIAN_POINT('Ctrl Pts',(-0.208738697720301,2.34553946582924,
9.48183886514223));
#44336=CARTESIAN_POINT('Ctrl Pts',(-0.208322774560329,2.3458924456251,9.48180475678231));
#44337=CARTESIAN_POINT('Ctrl Pts',(-0.207693158063705,2.3464240355158,9.481753351407));
#44338=CARTESIAN_POINT('Ctrl Pts',(-0.207480128781689,2.34660342525712,
9.48173599763598));
#44339=CARTESIAN_POINT('Ctrl Pts',(-0.20710981411159,2.34691444386232,9.48170589936214));
#44340=CARTESIAN_POINT('Ctrl Pts',(-0.206952635569413,2.34704619875762,
9.48169314557047));
#44341=CARTESIAN_POINT('Ctrl Pts',(-0.206623663824097,2.34732142501102,
9.48166649682518));
#44342=CARTESIAN_POINT('Ctrl Pts',(-0.206451847027919,2.34746486736641,
9.48165260406219));
#44343=CARTESIAN_POINT('Ctrl Pts',(-0.206040567676928,2.34780750011874,
9.48161940930763));
#44344=CARTESIAN_POINT('Ctrl Pts',(-0.205800964678699,2.34800652326703,
9.48160011963735));
#44345=CARTESIAN_POINT('Ctrl Pts',(-0.204987795963277,2.34867998149149,
9.48153481818105));
#44346=CARTESIAN_POINT('Ctrl Pts',(-0.204412869735424,2.34915278124262,
9.48148892499236));
#44347=CARTESIAN_POINT('Ctrl Pts',(-0.203041149594618,2.3502728931802,9.48138006933562));
#44348=CARTESIAN_POINT('Ctrl Pts',(-0.202242885198979,2.35091840295332,
9.48131723257269));
#44349=CARTESIAN_POINT('Ctrl Pts',(-0.192638019970065,2.35860968166988,
9.48056708541994));
#44350=CARTESIAN_POINT('Ctrl Pts',(-0.183469446992151,2.36519312827681,
9.4799102636502));
#44351=CARTESIAN_POINT('Ctrl Pts',(-0.150732574404027,2.38618726204264,
9.47769176539477));
#44352=CARTESIAN_POINT('Ctrl Pts',(-0.125673234436649,2.39804326749506,
9.47619593879675));
#44353=CARTESIAN_POINT('Ctrl Pts',(-0.0969312426862239,2.40736345216879,
9.47444282374195));
#44354=CARTESIAN_POINT('Ctrl Pts',(-0.0944444202053473,2.40813667184715,
9.47429095523788));
#44355=CARTESIAN_POINT('Ctrl Pts',(-0.0903492962067929,2.40935572491413,
9.47404037460777));
#44356=CARTESIAN_POINT('Ctrl Pts',(-0.0887463955885584,2.40981936187511,
9.47394217016029));
#44357=CARTESIAN_POINT('Ctrl Pts',(-0.0809468024205457,2.4120098904307,
9.47346358417667));
#44358=CARTESIAN_POINT('Ctrl Pts',(-0.074703291433907,2.41356333650994,
9.47307820714079));
#44359=CARTESIAN_POINT('Ctrl Pts',(-0.0674116334440075,2.41514743761793,
9.47262405648245));
#44360=CARTESIAN_POINT('Ctrl Pts',(-0.0664044420915283,2.41536119893333,
9.47256123663149));
#44361=CARTESIAN_POINT('Ctrl Pts',(-0.0649038345853793,2.41567217294197,
9.47246750458945));
#44362=CARTESIAN_POINT('Ctrl Pts',(-0.0644111804744379,2.41577306461944,
9.47243671011018));
#44363=CARTESIAN_POINT('Ctrl Pts',(-0.0635329351061396,2.41595078155366,
9.47238177349971));
#44364=CARTESIAN_POINT('Ctrl Pts',(-0.0631474347631856,2.41602805522331,
9.47235764574796));
#44365=CARTESIAN_POINT('Ctrl Pts',(-0.0623352305389417,2.41618931637414,
9.47230678220697));
#44366=CARTESIAN_POINT('Ctrl Pts',(-0.0619084964279216,2.41627314590805,
9.47228004142842));
#44367=CARTESIAN_POINT('Ctrl Pts',(-0.0607826733403173,2.41649194174401,
9.47220944774119));
#44368=CARTESIAN_POINT('Ctrl Pts',(-0.0600833073939316,2.41662545495727,
9.47216554858119));
#44369=CARTESIAN_POINT('Ctrl Pts',(-0.0569319920771485,2.41721624338403,
9.47196752869842));
#44370=CARTESIAN_POINT('Ctrl Pts',(-0.0544752795231656,2.4176473518651,
9.47181257737375));
#44371=CARTESIAN_POINT('Ctrl Pts',(-0.0363047741705893,2.42061895547945,
9.47066198464658));
#44372=CARTESIAN_POINT('Ctrl Pts',(-0.0204293873655689,2.42202027165477,
9.46963010260825));
#44373=CARTESIAN_POINT('Ctrl Pts',(0.0272025572388639,2.42268801173638,
9.46646221583151));
#44374=CARTESIAN_POINT('Ctrl Pts',(0.0588125502753527,2.41844712554706,
9.46424933432333));
#44375=CARTESIAN_POINT('Ctrl Pts',(0.0907872115822737,2.40922690063284,
9.46214358143891));
#44376=CARTESIAN_POINT('Ctrl Pts',(0.0922782957813124,2.40878521697215,
9.46204574514148));
#44377=CARTESIAN_POINT('Ctrl Pts',(0.0941749682043113,2.40820842553216,
9.46192181083258));
#44378=CARTESIAN_POINT('Ctrl Pts',(0.0945835319307011,2.40808329019573,
9.46189514457338));
#44379=CARTESIAN_POINT('Ctrl Pts',(0.0952320866716068,2.40788323841827,
9.46185286438686));
#44380=CARTESIAN_POINT('Ctrl Pts',(0.0954722391649565,2.40780885364235,
9.46183721938858));
#44381=CARTESIAN_POINT('Ctrl Pts',(0.0959206728991603,2.40766938058988,
9.46180802633098));
#44382=CARTESIAN_POINT('Ctrl Pts',(0.0961289735175954,2.40760436227867,
9.46179447432058));
#44383=CARTESIAN_POINT('Ctrl Pts',(0.0965967844523198,2.40745781962584,
9.46176405727718));
#44384=CARTESIAN_POINT('Ctrl Pts',(0.0968562570680768,2.40737617845838,
9.46174719926272));
#44385=CARTESIAN_POINT('Ctrl Pts',(0.0976252456523518,2.40713315139647,
9.46169727519125));
#44386=CARTESIAN_POINT('Ctrl Pts',(0.0981344670417091,2.40697082542735,
9.46166426430943));
#44387=CARTESIAN_POINT('Ctrl Pts',(0.102205811956428,2.40566182485233,9.46140070656974));
#44388=CARTESIAN_POINT('Ctrl Pts',(0.105748305938762,2.40445439382104,9.46117366473429));
#44389=CARTESIAN_POINT('Ctrl Pts',(0.11967302340075,2.39943587488652,9.4602873098731));
#44390=CARTESIAN_POINT('Ctrl Pts',(0.129878047711789,2.39515286808206,9.45965114437382));
#44391=CARTESIAN_POINT('Ctrl Pts',(0.171195680681954,2.37525295759648,9.45705458427353));
#44392=CARTESIAN_POINT('Ctrl Pts',(0.199892245072711,2.35517684228811,9.45517087583014));
#44393=CARTESIAN_POINT('Ctrl Pts',(0.226249860016895,2.32951281873791,9.45294637928287));
#44394=CARTESIAN_POINT('Ctrl Pts',(0.227662262295686,2.32811187425039,9.45282552617872));
#44395=CARTESIAN_POINT('Ctrl Pts',(0.229539581208921,2.32621498191669,9.4526626165103));
#44396=CARTESIAN_POINT('Ctrl Pts',(0.230016050974719,2.32573048900844,9.45262106975628));
#44397=CARTESIAN_POINT('Ctrl Pts',(0.230759977926259,2.32496923420806,9.45255588597263));
#44398=CARTESIAN_POINT('Ctrl Pts',(0.231028479608154,2.32469349202982,9.45253229469513));
#44399=CARTESIAN_POINT('Ctrl Pts',(0.231564054188112,2.32414150011792,9.4524851075071));
#44400=CARTESIAN_POINT('Ctrl Pts',(0.231831128280468,2.32386525238491,9.45246151170434));
#44401=CARTESIAN_POINT('Ctrl Pts',(0.232430285327008,2.32324329303226,9.45240842974875));
#44402=CARTESIAN_POINT('Ctrl Pts',(0.232762091715507,2.32289731733995,9.45237893166911));
#44403=CARTESIAN_POINT('Ctrl Pts',(0.233451818763828,2.32217491699996,9.45231740043061));
#44404=CARTESIAN_POINT('Ctrl Pts',(0.233809603517261,2.32179836502128,9.45228536151397));
#44405=CARTESIAN_POINT('Ctrl Pts',(0.234736613914386,2.32081799367317,9.45220203451745));
#44406=CARTESIAN_POINT('Ctrl Pts',(0.235304417832037,2.32021284061087,9.45215068546844));
#44407=CARTESIAN_POINT('Ctrl Pts',(0.236965523145545,2.31842871093038,9.4519995444195));
#44408=CARTESIAN_POINT('Ctrl Pts',(0.238052333787264,2.31724375053362,9.45189947679271));
#44409=CARTESIAN_POINT('Ctrl Pts',(0.249396074304328,2.30468822158,9.45084238320692));
#44410=CARTESIAN_POINT('Ctrl Pts',(0.258837504200833,2.29261021409117,9.44985140995903));
#44411=CARTESIAN_POINT('Ctrl Pts',(0.285522077972278,2.25295104040815,9.44667864838775));
#44412=CARTESIAN_POINT('Ctrl Pts',(0.29947837682563,2.22340780757839,9.44440858188591));
#44413=CARTESIAN_POINT('Ctrl Pts',(0.309204540203415,2.19086204917898,9.44226061495914));
#44414=CARTESIAN_POINT('Ctrl Pts',(0.309617962356751,2.18944315092948,9.44216767718748));
#44415=CARTESIAN_POINT('Ctrl Pts',(0.310137437759879,2.18761349864264,9.44204878843287));
#44416=CARTESIAN_POINT('Ctrl Pts',(0.310252452458795,2.18720533924523,9.442022327564));
#44417=CARTESIAN_POINT('Ctrl Pts',(0.310433506412475,2.1865579304315,9.44198045398585));
#44418=CARTESIAN_POINT('Ctrl Pts',(0.310500074964,2.18631883150551,9.441965010486));
#44419=CARTESIAN_POINT('Ctrl Pts',(0.310618916401937,2.18589006406086,9.44193735435746));
#44420=CARTESIAN_POINT('Ctrl Pts',(0.310671291433447,2.18570042596438,9.44192513581439));
#44421=CARTESIAN_POINT('Ctrl Pts',(0.310794090368684,2.18525420698839,9.44189641693779));
#44422=CARTESIAN_POINT('Ctrl Pts',(0.31086437009975,2.18499758714826,9.441879925123));
#44423=CARTESIAN_POINT('Ctrl Pts',(0.311067396475096,2.18425263535107,9.44183212028819));
#44424=CARTESIAN_POINT('Ctrl Pts',(0.311199311587595,2.1837640745729,9.44180085560973));
#44425=CARTESIAN_POINT('Ctrl Pts',(0.312108478272817,2.18036509228744,9.44158393535985));
#44426=CARTESIAN_POINT('Ctrl Pts',(0.312846073117789,2.17744408551942,9.44140053565276));
#44427=CARTESIAN_POINT('Ctrl Pts',(0.315015877146681,2.16831379012124,9.44083541508428));
#44428=CARTESIAN_POINT('Ctrl Pts',(0.316305046895793,2.16207177501105,9.44046070360992));
#44429=CARTESIAN_POINT('Ctrl Pts',(0.32014164373459,2.14024611150429,9.43917796551637));
#44430=CARTESIAN_POINT('Ctrl Pts',(0.321728838115565,2.1245161456337,9.43830088263462));
#44431=CARTESIAN_POINT('Ctrl Pts',(0.322836863474844,2.0836385463757,9.43601427327013));
#44432=CARTESIAN_POINT('Ctrl Pts',(0.320582960966283,2.05855550003987,9.43459728529053));
#44433=CARTESIAN_POINT('Ctrl Pts',(0.315137863248776,2.03253511113195,9.43298470670581));
#44434=CARTESIAN_POINT('Ctrl Pts',(0.314823420287229,2.03108267266997,9.43289424516316));
#44435=CARTESIAN_POINT('Ctrl Pts',(0.314380636435146,2.02910370489382,9.43277036029786));
#44436=CARTESIAN_POINT('Ctrl Pts',(0.314260993004996,2.02857523192192,9.43273721605986));
#44437=CARTESIAN_POINT('Ctrl Pts',(0.314055254382719,2.02767699566307,9.4326807759214));
#44438=CARTESIAN_POINT('Ctrl Pts',(0.31396983723826,2.02730707693113,9.4326575018391));
#44439=CARTESIAN_POINT('Ctrl Pts',(0.313796419068784,2.026562057151,9.43261056586485));
#44440=CARTESIAN_POINT('Ctrl Pts',(0.313708398646986,2.02618696126954,9.43258690338136));
#44441=CARTESIAN_POINT('Ctrl Pts',(0.313506802792778,2.02533474185148,9.43253306990223));
#44442=CARTESIAN_POINT('Ctrl Pts',(0.313392810608187,2.02485771878232,9.43250288553058));
#44443=CARTESIAN_POINT('Ctrl Pts',(0.313152120291901,2.02386057684683,9.43243968130829));
#44444=CARTESIAN_POINT('Ctrl Pts',(0.313025214333634,2.02334051012926,9.432406654827));
#44445=CARTESIAN_POINT('Ctrl Pts',(0.312689207684199,2.02197828521762,9.43231998431469));
#44446=CARTESIAN_POINT('Ctrl Pts',(0.312478001501209,2.02113665532107,9.4322662723923));
#44447=CARTESIAN_POINT('Ctrl Pts',(0.311840726480372,2.01863994996806,9.43210644315864));
#44448=CARTESIAN_POINT('Ctrl Pts',(0.311404893538419,2.01698741943461,9.4320000109115));
#44449=CARTESIAN_POINT('Ctrl Pts',(0.306470169119154,1.99886252035095,9.43082545468942));
#44450=CARTESIAN_POINT('Ctrl Pts',(0.300682810569195,1.98277186472956,9.42971485070911));
#44451=CARTESIAN_POINT('Ctrl Pts',(0.282008898053794,1.94147443563514,9.42669058196201));
#44452=CARTESIAN_POINT('Ctrl Pts',(0.267034512776537,1.9173748725589,9.42473230165862));
#44453=CARTESIAN_POINT('Ctrl Pts',(0.246891477914125,1.89283339157701,9.42269284799245));
#44454=CARTESIAN_POINT('Ctrl Pts',(0.244628802431751,1.8901663587424,9.42247072202866));
#44455=CARTESIAN_POINT('Ctrl Pts',(0.241946991163536,1.88710764580198,9.42221592976329));
#44456=CARTESIAN_POINT('Ctrl Pts',(0.241569790856374,1.88667973099932,9.42218028324992));
#44457=CARTESIAN_POINT('Ctrl Pts',(0.24100619053917,1.88604376669373,9.42212730714452));
#44458=CARTESIAN_POINT('Ctrl Pts',(0.240820655556383,1.88583495731651,9.42210991347727));
#44459=CARTESIAN_POINT('Ctrl Pts',(0.240489250025858,1.8854629538826,9.42207892672944));
#44460=CARTESIAN_POINT('Ctrl Pts',(0.240343484819296,1.88529966734829,9.42206532577764));
#44461=CARTESIAN_POINT('Ctrl Pts',(0.240033176057989,1.8849527707626,9.42203643180461));
#44462=CARTESIAN_POINT('Ctrl Pts',(0.239868588604526,1.88476920152307,9.42202114223114));
#44463=CARTESIAN_POINT('Ctrl Pts',(0.239425264635291,1.88427588935616,9.42198005455102));
#44464=CARTESIAN_POINT('Ctrl Pts',(0.239146136577251,1.88396649652528,9.4219542859741));
#44465=CARTESIAN_POINT('Ctrl Pts',(0.237793620473765,1.88247316591569,9.42182990782071));
#44466=CARTESIAN_POINT('Ctrl Pts',(0.236712012123557,1.88129665514977,9.42173191036822));
#44467=CARTESIAN_POINT('Ctrl Pts',(0.227529407989373,1.87145628166384,9.42091170271394));
#44468=CARTESIAN_POINT('Ctrl Pts',(0.218963554547288,1.86323663352581,9.42022281539558));
#44469=CARTESIAN_POINT('Ctrl Pts',(0.198821073362664,1.84593888250069,9.41871180233112));
#44470=CARTESIAN_POINT('Ctrl Pts',(0.18703781605683,1.83714309216627,9.41789830998348));
#44471=CARTESIAN_POINT('Ctrl Pts',(0.155778876424557,1.81697906378041,9.41581277989258));
#44472=CARTESIAN_POINT('Ctrl Pts',(0.135639229480557,1.80679412843478,9.41452914505569));
#44473=CARTESIAN_POINT('Ctrl Pts',(0.11336835377941,1.79832046546932,9.4130821316533));
#44474=CARTESIAN_POINT('Ctrl Pts',(0.112129232337921,1.79785771502958,9.41300155739414));
#44475=CARTESIAN_POINT('Ctrl Pts',(0.110403131216121,1.79722518243057,9.41288921601863));
#44476=CARTESIAN_POINT('Ctrl Pts',(0.109918527972368,1.79704891691886,9.41285766513238));
#44477=CARTESIAN_POINT('Ctrl Pts',(0.109083057406742,1.79674729839173,9.41280325068625));
#44478=CARTESIAN_POINT('Ctrl Pts',(0.108732390868532,1.79662138898722,9.41278040568436));
#44479=CARTESIAN_POINT('Ctrl Pts',(0.108015550749706,1.79636540476403,9.41273369287286));
#44480=CARTESIAN_POINT('Ctrl Pts',(0.107649358753522,1.79623538358497,9.41270982332368));
#44481=CARTESIAN_POINT('Ctrl Pts',(0.106800564826833,1.79593573597684,9.41265448035606));
#44482=CARTESIAN_POINT('Ctrl Pts',(0.106317793387263,1.79576659600279,9.41262299085588));
#44483=CARTESIAN_POINT('Ctrl Pts',(0.105301927956455,1.79541339875124,9.41255670367256));
#44484=CARTESIAN_POINT('Ctrl Pts',(0.104768749897887,1.79522959013385,9.41252189785917));
#44485=CARTESIAN_POINT('Ctrl Pts',(0.103349038450332,1.79474432241685,9.4124291782461));
#44486=CARTESIAN_POINT('Ctrl Pts',(0.102461673952023,1.79444532766363,9.41237118311513));
#44487=CARTESIAN_POINT('Ctrl Pts',(0.0997739715087234,1.79355273895656,
9.4121953894337));
#44488=CARTESIAN_POINT('Ctrl Pts',(0.0979697118153263,1.79297116664532,
9.41207719644391));
#44489=CARTESIAN_POINT('Ctrl Pts',(0.0914725549219662,1.79094001950794,
9.41165087742117));
#44490=CARTESIAN_POINT('Ctrl Pts',(0.0867519833413467,1.78958191260499,
9.41133980380581));
#44491=CARTESIAN_POINT('Ctrl Pts',(0.0706636807584968,1.78534894397187,
9.4102747460098));
#44492=CARTESIAN_POINT('Ctrl Pts',(0.0591717367956374,1.78298691096113,
9.40950539815993));
#44493=CARTESIAN_POINT('Ctrl Pts',(0.0203670840984569,1.77719468697395,
9.40688799931844));
#44494=CARTESIAN_POINT('Ctrl Pts',(-0.00725039676497182,1.77663410797581,
9.40498327120166));
#44495=CARTESIAN_POINT('Ctrl Pts',(-0.0388485923793428,1.78004656984481,
9.40293121428378));
#44496=CARTESIAN_POINT('Ctrl Pts',(-0.0430848778315068,1.7805894361636,
9.40265905336652));
#44497=CARTESIAN_POINT('Ctrl Pts',(-0.0478482432475965,1.78129634764236,
9.40235730253564));
#44498=CARTESIAN_POINT('Ctrl Pts',(-0.0483869203337208,1.78137768697267,
9.40232324016933));
#44499=CARTESIAN_POINT('Ctrl Pts',(-0.0492004781585769,1.78150264360463,
9.40227189236619));
#44500=CARTESIAN_POINT('Ctrl Pts',(-0.049475509518873,1.78154525118762,
9.402254550351));
#44501=CARTESIAN_POINT('Ctrl Pts',(-0.049953076272882,1.78161986896095,
9.40222446681752));
#44502=CARTESIAN_POINT('Ctrl Pts',(-0.0501556363613433,1.78165171617976,
9.40221171603243));
#44503=CARTESIAN_POINT('Ctrl Pts',(-0.0505792805874181,1.78171873741091,
9.40218506775862));
#44504=CARTESIAN_POINT('Ctrl Pts',(-0.0508003583534382,1.78175394844311,
9.40217117247011));
#44505=CARTESIAN_POINT('Ctrl Pts',(-0.051329168524085,1.78183873705242,
9.40213796151166));
#44506=CARTESIAN_POINT('Ctrl Pts',(-0.0516368671089207,1.78188853095353,
9.40211865819435));
#44507=CARTESIAN_POINT('Ctrl Pts',(-0.052680400242128,1.78205895663339,
9.40205326288432));
#44508=CARTESIAN_POINT('Ctrl Pts',(-0.0534158952564986,1.78218169689788,
9.40200728995333));
#44509=CARTESIAN_POINT('Ctrl Pts',(-0.0551651785955241,1.78247986330419,
9.40189821700345));
#44510=CARTESIAN_POINT('Ctrl Pts',(-0.0561785729207752,1.7826575947867,
9.40183524336065));
#44511=CARTESIAN_POINT('Ctrl Pts',(-0.0683362612767503,1.78484990193908,
9.4010821379189));
#44512=CARTESIAN_POINT('Ctrl Pts',(-0.0793690778292553,1.78744594371111,
9.40042274331321));
#44513=CARTESIAN_POINT('Ctrl Pts',(-0.103783857631236,1.79456747285531,
9.39897224442632));
#44514=CARTESIAN_POINT('Ctrl Pts',(-0.117050853462566,1.79940185488798,
9.3981896980009));
#44515=CARTESIAN_POINT('Ctrl Pts',(-0.137175496261895,1.80827024032479,
9.39695840127328));
#44516=CARTESIAN_POINT('Ctrl Pts',(-0.144272810896659,1.81171417062702,
9.39651517237573));
#44517=CARTESIAN_POINT('Ctrl Pts',(-0.165247437901682,1.82286067219054,
9.3951635210907));
#44518=CARTESIAN_POINT('Ctrl Pts',(-0.178687505393542,1.83132995710408,
9.39423895899712));
#44519=CARTESIAN_POINT('Ctrl Pts',(-0.192461086576651,1.84150146812387,
9.39319873037454));
#44520=CARTESIAN_POINT('Ctrl Pts',(-0.193469495165107,1.84225532944671,
9.39312201184949));
#44521=CARTESIAN_POINT('Ctrl Pts',(-0.194876037157026,1.84331973067511,
9.3930142056253));
#44522=CARTESIAN_POINT('Ctrl Pts',(-0.195277906669753,1.8436253333872,9.39298331180776));
#44523=CARTESIAN_POINT('Ctrl Pts',(-0.195972859486507,1.8441563940636,9.39292972670439));
#44524=CARTESIAN_POINT('Ctrl Pts',(-0.196266276760142,1.84438141507566,
9.39290705267579));
#44525=CARTESIAN_POINT('Ctrl Pts',(-0.196855658686899,1.84483502372851,
9.39286140721108));
#44526=CARTESIAN_POINT('Ctrl Pts',(-0.197151614027167,1.84506362253037,
9.3928384353536));
#44527=CARTESIAN_POINT('Ctrl Pts',(-0.197851824429519,1.84560642040599,
9.39278396362928));
#44528=CARTESIAN_POINT('Ctrl Pts',(-0.198255729033612,1.84592106803343,
9.39275244598307));
#44529=CARTESIAN_POINT('Ctrl Pts',(-0.199513056502274,1.84690536813841,
9.39265403079365));
#44530=CARTESIAN_POINT('Ctrl Pts',(-0.200363842529508,1.84757836274847,
9.39258700010511));
#44531=CARTESIAN_POINT('Ctrl Pts',(-0.20232268092819,1.84914399951926,9.39243164766579));
#44532=CARTESIAN_POINT('Ctrl Pts',(-0.20342824541422,1.85003970503628,9.39234320338943));
#44533=CARTESIAN_POINT('Ctrl Pts',(-0.207105321188201,1.85305934868658,
9.39204645057628));
#44534=CARTESIAN_POINT('Ctrl Pts',(-0.209649719550282,1.85521582345928,
9.39183682780877));
#44535=CARTESIAN_POINT('Ctrl Pts',(-0.218631762472412,1.86307122461314,
9.39108111120357));
#44536=CARTESIAN_POINT('Ctrl Pts',(-0.224873807262726,1.86898735664733,
9.39052620619662));
#44537=CARTESIAN_POINT('Ctrl Pts',(-0.255963669111777,1.90090916743503,
9.38760383345891));
#44538=CARTESIAN_POINT('Ctrl Pts',(-0.276562679716115,1.93068619127209,
9.38507499716765));
#44539=CARTESIAN_POINT('Ctrl Pts',(-0.292548375144975,1.96479806122941,
9.38268785766659));
#44540=CARTESIAN_POINT('Ctrl Pts',(-0.293263636606715,1.96635660959003,
9.38257987957437));
#44541=CARTESIAN_POINT('Ctrl Pts',(-0.294148086025407,1.9683251142008,9.38244493308368));
#44542=CARTESIAN_POINT('Ctrl Pts',(-0.294328896721643,1.96872977251922,
9.38241726846352));
#44543=CARTESIAN_POINT('Ctrl Pts',(-0.294612465115776,1.96936793615425,
9.38237376104588));
#44544=CARTESIAN_POINT('Ctrl Pts',(-0.294715780474092,1.96960119077682,
9.38235788408284));
#44545=CARTESIAN_POINT('Ctrl Pts',(-0.294906837521714,1.97003392635536,
9.38232847643265));
#44546=CARTESIAN_POINT('Ctrl Pts',(-0.29499465325763,1.97023337229626,9.3823149412552));
#44547=CARTESIAN_POINT('Ctrl Pts',(-0.295189713156472,1.9706776110057,9.38228483496318));
#44548=CARTESIAN_POINT('Ctrl Pts',(-0.29529685487223,1.97092244752706,9.3822682702251));
#44549=CARTESIAN_POINT('Ctrl Pts',(-0.295608231753307,1.9716364119531,9.38222004667172));
#44550=CARTESIAN_POINT('Ctrl Pts',(-0.295811655621786,1.97210589605688,
9.38218843751308));
#44551=CARTESIAN_POINT('Ctrl Pts',(-0.297255906498752,1.97546097811683,
9.38196325766307));
#44552=CARTESIAN_POINT('Ctrl Pts',(-0.29845566091156,1.97836422330409,9.38177214325877));
#44553=CARTESIAN_POINT('Ctrl Pts',(-0.301100466440746,1.98503916327875,
9.38134022383136));
#44554=CARTESIAN_POINT('Ctrl Pts',(-0.30251747062057,1.9888214594421,9.38110085470681));
#44555=CARTESIAN_POINT('Ctrl Pts',(-0.316034006210467,2.02707385082697,
9.37872416390739));
#44556=CARTESIAN_POINT('Ctrl Pts',(-0.322260403908793,2.06333603087332,
9.37679719750188));
#44557=CARTESIAN_POINT('Ctrl Pts',(-0.322274974372014,2.0998714756124,9.37464719300612));
#44558=CARTESIAN_POINT('',(-0.322274999740166,2.09998705874836,9.12407167227341));
#44559=CARTESIAN_POINT('Ctrl Pts',(-0.322274974505127,2.09987180983054,
9.37464717333835));
#44560=CARTESIAN_POINT('Ctrl Pts',(-0.322277110580648,2.10524198514739,
9.37433115401095));
#44561=CARTESIAN_POINT('Ctrl Pts',(-0.322145019382397,2.11061118994016,
9.37401147726832));
#44562=CARTESIAN_POINT('Ctrl Pts',(-0.321766823267488,2.11823169941662,
9.37355134390472));
#44563=CARTESIAN_POINT('Ctrl Pts',(-0.32163105895509,2.12048767760956,9.37341432817286));
#44564=CARTESIAN_POINT('Ctrl Pts',(-0.321429283593712,2.12333989158731,
9.3732400323371));
#44565=CARTESIAN_POINT('Ctrl Pts',(-0.321385318859788,2.12393766289022,
9.37320344377587));
#44566=CARTESIAN_POINT('Ctrl Pts',(-0.321307485198678,2.12495705288305,
9.37314094605633));
#44567=CARTESIAN_POINT('Ctrl Pts',(-0.32127445325989,2.12537873545261,9.37311506318493));
#44568=CARTESIAN_POINT('Ctrl Pts',(-0.321211268653396,2.12616544804394,
9.37306671838576));
#44569=CARTESIAN_POINT('Ctrl Pts',(-0.32118132362295,2.12653049444167,9.37304426301192));
#44570=CARTESIAN_POINT('Ctrl Pts',(-0.321119286425513,2.12727126155572,
9.37299864931778));
#44571=CARTESIAN_POINT('Ctrl Pts',(-0.321087157013343,2.12764697850471,
9.37297548986086));
#44572=CARTESIAN_POINT('Ctrl Pts',(-0.321010827792065,2.12852147971539,
9.37292152825814));
#44573=CARTESIAN_POINT('Ctrl Pts',(-0.320966124852631,2.12902021808112,
9.37289071033703));
#44574=CARTESIAN_POINT('Ctrl Pts',(-0.320830008504175,2.1305000351093,9.37279914113781));
#44575=CARTESIAN_POINT('Ctrl Pts',(-0.320735258514318,2.13148079429874,
9.37273828502976));
#44576=CARTESIAN_POINT('Ctrl Pts',(-0.320052229261279,2.13822744832209,
9.37231848046731));
#44577=CARTESIAN_POINT('Ctrl Pts',(-0.31931303157068,2.14397667660772,9.37195480216073));
#44578=CARTESIAN_POINT('Ctrl Pts',(-0.318078404834808,2.15188630773486,
9.37144578736919));
#44579=CARTESIAN_POINT('Ctrl Pts',(-0.317715092194272,2.1540664439802,9.37130457379153));
#44580=CARTESIAN_POINT('Ctrl Pts',(-0.312059811832663,2.18597438814035,
9.36922432788522));
#44581=CARTESIAN_POINT('Ctrl Pts',(-0.302638045776677,2.2148150632461,9.36715138662394));
#44582=CARTESIAN_POINT('Ctrl Pts',(-0.285505590720188,2.24974577066783,
9.36454693329608));
#44583=CARTESIAN_POINT('Ctrl Pts',(-0.28134849063823,2.257417562983,9.36397002176843));
#44584=CARTESIAN_POINT('Ctrl Pts',(-0.274805698362227,2.26840283375879,
9.36314598112024));
#44585=CARTESIAN_POINT('Ctrl Pts',(-0.27266048537398,2.27185444367139,9.36288739037192));
#44586=CARTESIAN_POINT('Ctrl Pts',(-0.270154175255612,2.27572192236349,
9.36259882847387));
#44587=CARTESIAN_POINT('Ctrl Pts',(-0.269856744492273,2.27617834676693,
9.3625647926083));
#44588=CARTESIAN_POINT('Ctrl Pts',(-0.269407906376958,2.27686331093874,
9.36251374573381));
#44589=CARTESIAN_POINT('Ctrl Pts',(-0.26925736435615,2.27709241236131,9.36249667726692));
#44590=CARTESIAN_POINT('Ctrl Pts',(-0.268987466069528,2.27750201561849,
9.36246617096688));
#44591=CARTESIAN_POINT('Ctrl Pts',(-0.268868220545551,2.27768258899724,
9.36245272574479));
#44592=CARTESIAN_POINT('Ctrl Pts',(-0.268611264692764,2.27807084601557,
9.36242382424172));
#44593=CARTESIAN_POINT('Ctrl Pts',(-0.268473495734878,2.27827848947489,
9.36240837204354));
#44594=CARTESIAN_POINT('Ctrl Pts',(-0.268098152532454,2.2788427797568,9.36236639116611));
#44595=CARTESIAN_POINT('Ctrl Pts',(-0.267860106484653,2.27919911445519,
9.36233989427731));
#44596=CARTESIAN_POINT('Ctrl Pts',(-0.266775050728669,2.28081635777428,
9.3622196905617));
#44597=CARTESIAN_POINT('Ctrl Pts',(-0.265919825825667,2.28207176984814,
9.36212652928844));
#44598=CARTESIAN_POINT('Ctrl Pts',(-0.248693577698076,2.3069784252738,9.36028023902983));
#44599=CARTESIAN_POINT('Ctrl Pts',(-0.229234814593436,2.32834312362855,
9.35872408386193));
#44600=CARTESIAN_POINT('Ctrl Pts',(-0.19892321500865,2.35378604271672,9.35649757473676));
#44601=CARTESIAN_POINT('Ctrl Pts',(-0.190308300502816,2.36030852413816,
9.35588378359829));
#44602=CARTESIAN_POINT('Ctrl Pts',(-0.175806441413843,2.37018286786351,
9.35486312597605));
#44603=CARTESIAN_POINT('Ctrl Pts',(-0.170112634274441,2.37380352318409,
9.3544653750954));
#44604=CARTESIAN_POINT('Ctrl Pts',(-0.162248670009259,2.37846415295899,
9.35391757488902));
#44605=CARTESIAN_POINT('Ctrl Pts',(-0.160174142676971,2.3796625805373,9.35377321167319));
#44606=CARTESIAN_POINT('Ctrl Pts',(-0.157116423128887,2.3813838026871,9.35356055561746));
#44607=CARTESIAN_POINT('Ctrl Pts',(-0.156143545275065,2.38192482695242,
9.35349291322107));
#44608=CARTESIAN_POINT('Ctrl Pts',(-0.15438896528472,2.38288869339273,9.35337094434498));
#44609=CARTESIAN_POINT('Ctrl Pts',(-0.153608276845747,2.38331336486435,
9.35331668355144));
#44610=CARTESIAN_POINT('Ctrl Pts',(-0.152410915075227,2.3839582904387,9.35323347146609));
#44611=CARTESIAN_POINT('Ctrl Pts',(-0.151995494242797,2.38418087104711,
9.35320460296736));
#44612=CARTESIAN_POINT('Ctrl Pts',(-0.151236680990402,2.38458529992811,
9.35315187378738));
#44613=CARTESIAN_POINT('Ctrl Pts',(-0.15089344452434,2.38476744022029,9.35312802352166));
#44614=CARTESIAN_POINT('Ctrl Pts',(-0.150204743916452,2.38513130817347,
9.35308016961704));
#44615=CARTESIAN_POINT('Ctrl Pts',(-0.149859277337966,2.38531302982753,
9.35305616581531));
#44616=CARTESIAN_POINT('Ctrl Pts',(-0.148887392592978,2.38582200658525,
9.35298863855252));
#44617=CARTESIAN_POINT('Ctrl Pts',(-0.148260229683678,2.38614782788444,
9.35294506455187));
#44618=CARTESIAN_POINT('Ctrl Pts',(-0.145683615575148,2.38747567584247,
9.35276604959449));
#44619=CARTESIAN_POINT('Ctrl Pts',(-0.143725073987598,2.38845984603363,
9.35262998268297));
#44620=CARTESIAN_POINT('Ctrl Pts',(-0.124864338201729,2.39769762829194,
9.351319475839));
#44621=CARTESIAN_POINT('Ctrl Pts',(-0.107283152810747,2.40447509752426,
9.35009318879919));
#44622=CARTESIAN_POINT('Ctrl Pts',(-0.0816840372893737,2.41184980761404,
9.34831004619962));
#44623=CARTESIAN_POINT('Ctrl Pts',(-0.0740774855128724,2.41374369200601,
9.34778096715786));
#44624=CARTESIAN_POINT('Ctrl Pts',(-0.0640304026676524,2.41585945479017,
9.3470863270942));
#44625=CARTESIAN_POINT('Ctrl Pts',(-0.0616455279271145,2.41633355263805,
9.34692175412797));
#44626=CARTESIAN_POINT('Ctrl Pts',(-0.0511467547938183,2.41829740461938,
9.34619905433089));
#44627=CARTESIAN_POINT('Ctrl Pts',(-0.0429825161552331,2.41950233027117,
9.34564164454891));
#44628=CARTESIAN_POINT('Ctrl Pts',(-0.0232151527736135,2.42164821456,9.34431378262442));
#44629=CARTESIAN_POINT('Ctrl Pts',(-0.0115884289626762,2.42227673387109,
9.34355053978316));
#44630=CARTESIAN_POINT('Ctrl Pts',(0.000796610408746042,2.42227488464974,
9.34277315938522));
#44631=CARTESIAN_POINT('Ctrl Pts',(0.00154510788851761,2.42227216530802,
9.34272631735025));
#44632=CARTESIAN_POINT('Ctrl Pts',(0.00260577185346212,2.42226461648085,
9.34266014356296));
#44633=CARTESIAN_POINT('Ctrl Pts',(0.00291794397415571,2.42226194110915,
9.34264069250031));
#44634=CARTESIAN_POINT('Ctrl Pts',(0.0034540551022078,2.42225656747896,
9.34260733166719));
#44635=CARTESIAN_POINT('Ctrl Pts',(0.00367799566596483,2.42225408939062,
9.34259340948123));
#44636=CARTESIAN_POINT('Ctrl Pts',(0.00410686413504136,2.42224889649799,
9.34256677235448));
#44637=CARTESIAN_POINT('Ctrl Pts',(0.00431179173556544,2.4222462196517,
9.34255405527032));
#44638=CARTESIAN_POINT('Ctrl Pts',(0.00479459484181479,2.42223945245172,
9.34252411988373));
#44639=CARTESIAN_POINT('Ctrl Pts',(0.00507246841567341,2.42223519814198,
9.34250691083999));
#44640=CARTESIAN_POINT('Ctrl Pts',(0.00589345896592658,2.42222156636208,
9.34245612419612));
#44641=CARTESIAN_POINT('Ctrl Pts',(0.00643656157367349,2.42221117512068,
9.34242260312503));
#44642=CARTESIAN_POINT('Ctrl Pts',(0.0112052167570492,2.42210787419832,
9.34212891647229));
#44643=CARTESIAN_POINT('Ctrl Pts',(0.0154288322364225,2.42193321483216,
9.34187322029529));
#44644=CARTESIAN_POINT('Ctrl Pts',(0.0202676568975475,2.42163765805283,
9.34158411188367));
#44645=CARTESIAN_POINT('Ctrl Pts',(0.0208871768760164,2.42159802058992,
9.34154716917964));
#44646=CARTESIAN_POINT('Ctrl Pts',(0.0489588843387423,2.4197205081397,9.33987633651391));
#44647=CARTESIAN_POINT('Ctrl Pts',(0.0760663184928047,2.41437635317203,
9.33838983614043));
#44648=CARTESIAN_POINT('Ctrl Pts',(0.114438766109626,2.40154991075901,9.33610151151518));
#44649=CARTESIAN_POINT('Ctrl Pts',(0.126450573644565,2.39671329976524,9.33535792026808));
#44650=CARTESIAN_POINT('Ctrl Pts',(0.141530119954209,2.38955913625974,9.33436793047283));
#44651=CARTESIAN_POINT('Ctrl Pts',(0.144893302184801,2.38789094720827,9.33414339686622));
#44652=CARTESIAN_POINT('Ctrl Pts',(0.149605849919691,2.38544995787496,9.33382308503411));
#44653=CARTESIAN_POINT('Ctrl Pts',(0.150980020050386,2.38472552080329,9.33372898780577));
#44654=CARTESIAN_POINT('Ctrl Pts',(0.153061967409586,2.38360864688341,9.33358534115381));
#44655=CARTESIAN_POINT('Ctrl Pts',(0.153773605586826,2.38322342533855,9.3335360466421));
#44656=CARTESIAN_POINT('Ctrl Pts',(0.155084858688188,2.38250722346743,9.33344485464043));
#44657=CARTESIAN_POINT('Ctrl Pts',(0.155684885256794,2.3821770033096,9.33340298436084));
#44658=CARTESIAN_POINT('Ctrl Pts',(0.156655845992829,2.38163860259175,9.33333499924708));
#44659=CARTESIAN_POINT('Ctrl Pts',(0.157027430821572,2.38143159474443,9.333308926464));
#44660=CARTESIAN_POINT('Ctrl Pts',(0.157724586886115,2.38104140241247,9.33325990560218));
#44661=CARTESIAN_POINT('Ctrl Pts',(0.158050251863029,2.38085838613531,9.33323696359633));
#44662=CARTESIAN_POINT('Ctrl Pts',(0.158805913695828,2.38043199092002,9.33318363006048));
#44663=CARTESIAN_POINT('Ctrl Pts',(0.159235669688544,2.38018818899204,9.33315322333217));
#44664=CARTESIAN_POINT('Ctrl Pts',(0.160334974294744,2.37956120397614,9.33307525002431));
#44665=CARTESIAN_POINT('Ctrl Pts',(0.161003707975213,2.3791766049517,9.33302763237335));
#44666=CARTESIAN_POINT('Ctrl Pts',(0.164834904872025,2.37695488075905,9.33275376002236));
#44667=CARTESIAN_POINT('Ctrl Pts',(0.167967188033252,2.3750664897984,9.33252564966688));
#44668=CARTESIAN_POINT('Ctrl Pts',(0.199581485798853,2.3552655055645,9.3301790117144));
#44669=CARTESIAN_POINT('Ctrl Pts',(0.225118985712258,2.33305278134016,9.32787946287751));
#44670=CARTESIAN_POINT('Ctrl Pts',(0.249727178731369,2.30376189741836,9.32531120635085));
#44671=CARTESIAN_POINT('Ctrl Pts',(0.252626290725504,2.30015627534537,9.32500230544863));
#44672=CARTESIAN_POINT('Ctrl Pts',(0.259330263326419,2.29144074724498,9.32427466300522));
#44673=CARTESIAN_POINT('Ctrl Pts',(0.263063425431226,2.28627772485283,9.32385853116391));
#44674=CARTESIAN_POINT('Ctrl Pts',(0.268329168608988,2.27852076498167,9.32325863793406));
#44675=CARTESIAN_POINT('Ctrl Pts',(0.269982212895564,2.27601083083979,9.32306828179713));
#44676=CARTESIAN_POINT('Ctrl Pts',(0.27187220484289,2.27305182927692,9.3228485522375));
#44677=CARTESIAN_POINT('Ctrl Pts',(0.272143430851037,2.27262498207136,9.32281696794774));
#44678=CARTESIAN_POINT('Ctrl Pts',(0.272555781322148,2.2719726502916,9.32276887269659));
#44679=CARTESIAN_POINT('Ctrl Pts',(0.272697631673513,2.27174762898313,9.32275231370925));
#44680=CARTESIAN_POINT('Ctrl Pts',(0.272954070473797,2.27133971406746,9.32272235311133));
#44681=CARTESIAN_POINT('Ctrl Pts',(0.273068753353805,2.27115688168319,9.32270894523208));
#44682=CARTESIAN_POINT('Ctrl Pts',(0.273300901565202,2.2707859537716,9.32268178570573));
#44683=CARTESIAN_POINT('Ctrl Pts',(0.273418355906973,2.27059785302247,9.32266803479882));
#44684=CARTESIAN_POINT('Ctrl Pts',(0.273755482682205,2.27005670883943,9.3226285375639));
#44685=CARTESIAN_POINT('Ctrl Pts',(0.273974667166824,2.26970335964647,9.32260282360759));
#44686=CARTESIAN_POINT('Ctrl Pts',(0.274931233425394,2.26815458742115,9.32249044589305));
#44687=CARTESIAN_POINT('Ctrl Pts',(0.275661494025509,2.26695475214609,9.32240424493475));
#44688=CARTESIAN_POINT('Ctrl Pts',(0.28910761513023,2.24453370875449,9.32080859535926));
#44689=CARTESIAN_POINT('Ctrl Pts',(0.299348349226978,2.2219188359578,9.31944699385759));
#44690=CARTESIAN_POINT('Ctrl Pts',(0.31130192090492,2.18461831162818,9.3172556486139));
#44691=CARTESIAN_POINT('Ctrl Pts',(0.31477595047952,2.17060596694544,9.31644442352887));
#44692=CARTESIAN_POINT('Ctrl Pts',(0.318793607225193,2.14800667466691,9.3151119153959));
#44693=CARTESIAN_POINT('Ctrl Pts',(0.319952904256393,2.13954902072294,9.31460819945818));
#44694=CARTESIAN_POINT('Ctrl Pts',(0.320938248737837,2.12937141438724,9.31399182851701));
#44695=CARTESIAN_POINT('Ctrl Pts',(0.321088053155284,2.12768576239751,9.31388941400643));
#44696=CARTESIAN_POINT('Ctrl Pts',(0.321294071864631,2.12514034958045,9.31373423730632));
#44697=CARTESIAN_POINT('Ctrl Pts',(0.32136012743303,2.12428139753194,9.31368178253688));
#44698=CARTESIAN_POINT('Ctrl Pts',(0.321461454138795,2.12289089148367,9.3135967168224));
#44699=CARTESIAN_POINT('Ctrl Pts',(0.321498853002195,2.12235949290298,9.31356417255085));
#44700=CARTESIAN_POINT('Ctrl Pts',(0.321568019263655,2.12134064726148,9.31350170688179));
#44701=CARTESIAN_POINT('Ctrl Pts',(0.321599996324827,2.12085321554119,9.31347179213921));
#44702=CARTESIAN_POINT('Ctrl Pts',(0.321655217439827,2.11998112168741,9.3134182151589));
#44703=CARTESIAN_POINT('Ctrl Pts',(0.321678880027556,2.1195964862227,9.31339456610235));
#44704=CARTESIAN_POINT('Ctrl Pts',(0.321724533955342,2.11883201100172,9.31334752468675));
#44705=CARTESIAN_POINT('Ctrl Pts',(0.321746542642521,2.11845217284772,9.31332413290999));
#44706=CARTESIAN_POINT('Ctrl Pts',(0.321798431584484,2.11752831718236,9.31326719268379));
#44707=CARTESIAN_POINT('Ctrl Pts',(0.321827604926024,2.11698426257558,9.31323362210826));
#44708=CARTESIAN_POINT('Ctrl Pts',(0.321932207259695,2.114936419474,9.31310711364155));
#44709=CARTESIAN_POINT('Ctrl Pts',(0.321998476014577,2.11343220080957,9.31301388898242));
#44710=CARTESIAN_POINT('Ctrl Pts',(0.322995892387522,2.08650119072519,9.31133931193541));
#44711=CARTESIAN_POINT('Ctrl Pts',(0.320923013928696,2.06105837554091,9.3096582867879));
#44712=CARTESIAN_POINT('Ctrl Pts',(0.312800650625744,2.02088783306894,9.30688949054664));
#44713=CARTESIAN_POINT('Ctrl Pts',(0.308619650234542,2.00588876243242,9.30583131655575));
#44714=CARTESIAN_POINT('Ctrl Pts',(0.301243170409902,1.98531117428011,9.30438540503579));
#44715=CARTESIAN_POINT('Ctrl Pts',(0.298940280151752,1.97943593194171,9.30397344525857));
#44716=CARTESIAN_POINT('Ctrl Pts',(0.295308214869733,1.9709149283306,9.30338097911197));
#44717=CARTESIAN_POINT('Ctrl Pts',(0.294112853359124,1.96821408078086,9.30319394952822));
#44718=CARTESIAN_POINT('Ctrl Pts',(0.292670446725865,1.96507246898396,9.30297761729861));
#44719=CARTESIAN_POINT('Ctrl Pts',(0.292459338426577,1.96461549428365,9.30294618037436));
#44720=CARTESIAN_POINT('Ctrl Pts',(0.292135248125902,1.96391824913556,9.30289826311695));
#44721=CARTESIAN_POINT('Ctrl Pts',(0.29202303967483,1.96367762320072,9.30288173530024));
#44722=CARTESIAN_POINT('Ctrl Pts',(0.291827189591217,1.96325898302014,9.30285299609391));
#44723=CARTESIAN_POINT('Ctrl Pts',(0.291743682591993,1.96308090718334,9.30284077638791));
#44724=CARTESIAN_POINT('Ctrl Pts',(0.291554252313116,1.96267791368488,9.30281313404468));
#44725=CARTESIAN_POINT('Ctrl Pts',(0.291448231986424,1.96245304254624,9.30279771756275));
#44726=CARTESIAN_POINT('Ctrl Pts',(0.291159868875873,1.96184324919072,9.30275593309625));
#44727=CARTESIAN_POINT('Ctrl Pts',(0.290977022237704,1.96145856369801,9.30272959639889));
#44728=CARTESIAN_POINT('Ctrl Pts',(0.290148970578473,1.95972532166904,9.30261103170682));
#44729=CARTESIAN_POINT('Ctrl Pts',(0.289495136126377,1.95838087392306,9.30251933133136));
#44730=CARTESIAN_POINT('Ctrl Pts',(0.274543363257353,1.92817256513347,9.30046390739913));
#44731=CARTESIAN_POINT('Ctrl Pts',(0.256004967849526,1.90160390819619,9.2987453224863));
#44732=CARTESIAN_POINT('Ctrl Pts',(0.228363851595974,1.87246051648433,9.29646740760043));
#44733=CARTESIAN_POINT('Ctrl Pts',(0.222686951139093,1.86690178928056,9.2960121333234));
#44734=CARTESIAN_POINT('Ctrl Pts',(0.210496922445429,1.85581759715336,9.29505149672199));
#44735=CARTESIAN_POINT('Ctrl Pts',(0.203958018542915,1.85033000286046,9.29454529989065));
#44736=CARTESIAN_POINT('Ctrl Pts',(0.196305459717384,1.84440921654621,9.29395908257779));
#44737=CARTESIAN_POINT('Ctrl Pts',(0.195397731720319,1.84371459564046,9.29388964422535));
#44738=CARTESIAN_POINT('Ctrl Pts',(0.193969160340216,1.84263341099055,9.29378050587156));
#44739=CARTESIAN_POINT('Ctrl Pts',(0.193450806552801,1.84224356121355,9.2937409345204));
#44740=CARTESIAN_POINT('Ctrl Pts',(0.192576251440651,1.8415899393226,9.29367421808133));
#44741=CARTESIAN_POINT('Ctrl Pts',(0.192220674880557,1.84132533130668,9.29364710565782));
#44742=CARTESIAN_POINT('Ctrl Pts',(0.191523378647588,1.84080865877599,9.29359396249883));
#44743=CARTESIAN_POINT('Ctrl Pts',(0.191181704321476,1.84055653435846,9.29356793416731));
#44744=CARTESIAN_POINT('Ctrl Pts',(0.190529806795121,1.84007748061553,9.29351829529477));
#44745=CARTESIAN_POINT('Ctrl Pts',(0.190219673731412,1.8398504293987,9.29349468954556));
#44746=CARTESIAN_POINT('Ctrl Pts',(0.189504864235509,1.83932907251583,9.29344030307948));
#44747=CARTESIAN_POINT('Ctrl Pts',(0.189099907837803,1.83903515398505,9.29340950744909));
#44748=CARTESIAN_POINT('Ctrl Pts',(0.187896856629313,1.83816624651675,9.2933180642978));
#44749=CARTESIAN_POINT('Ctrl Pts',(0.187096817428827,1.83759397097636,9.29325731237546));
#44750=CARTESIAN_POINT('Ctrl Pts',(0.181590896754036,1.83369351497535,9.29283959599465));
#44751=CARTESIAN_POINT('Ctrl Pts',(0.17679934328509,1.83048862169564,9.29247795474948));
#44752=CARTESIAN_POINT('Ctrl Pts',(0.171618477234641,1.82722095947575,9.29208854592491));
#44753=CARTESIAN_POINT('Ctrl Pts',(0.171311956884023,1.8270283529292,9.29206551298342));
#44754=CARTESIAN_POINT('Ctrl Pts',(0.169470360494686,1.82587548247755,9.29192716524804));
#44755=CARTESIAN_POINT('Ctrl Pts',(0.167927562510964,1.82492766818028,9.29181141334538));
#44756=CARTESIAN_POINT('Ctrl Pts',(0.163353928201045,1.82217068447009,9.2914686968454));
#44757=CARTESIAN_POINT('Ctrl Pts',(0.160301333767252,1.82039829159432,9.29124050567791));
#44758=CARTESIAN_POINT('Ctrl Pts',(0.151297805332135,1.81536658448345,9.29056911605386));
#44759=CARTESIAN_POINT('Ctrl Pts',(0.145272546863271,1.81224474763069,9.29012184494769));
#44760=CARTESIAN_POINT('Ctrl Pts',(0.11770263215299,1.79904675553709,9.28808725386008));
#44761=CARTESIAN_POINT('Ctrl Pts',(0.0951824520950674,1.79118453603266,
9.28645078171237));
#44762=CARTESIAN_POINT('Ctrl Pts',(0.0642590882056443,1.78409643151518,
9.28435458792234));
#44763=CARTESIAN_POINT('Ctrl Pts',(0.056451393599643,1.78260819327844,9.28383831839708));
#44764=CARTESIAN_POINT('Ctrl Pts',(0.0473419126823514,1.78121868276833,
9.28325687548702));
#44765=CARTESIAN_POINT('Ctrl Pts',(0.0460866976093846,1.78103479603152,
9.28317721509758));
#44766=CARTESIAN_POINT('Ctrl Pts',(0.044450453554328,1.78080494988878,9.28307399803282));
#44767=CARTESIAN_POINT('Ctrl Pts',(0.0440704047874012,1.78075225566622,
9.28305006775));
#44768=CARTESIAN_POINT('Ctrl Pts',(0.043453312201162,1.78066781797097,9.28301128383923));
#44769=CARTESIAN_POINT('Ctrl Pts',(0.0432163269809917,1.78063565962394,
9.28299640672087));
#44770=CARTESIAN_POINT('Ctrl Pts',(0.0427604897811242,1.78057432024666,
9.28296782431492));
#44771=CARTESIAN_POINT('Ctrl Pts',(0.0425416442583363,1.78054510040347,
9.28295411689655));
#44772=CARTESIAN_POINT('Ctrl Pts',(0.0420365571953682,1.78047819035556,
9.28292251474028));
#44773=CARTESIAN_POINT('Ctrl Pts',(0.0417502940137508,1.78044065976626,
9.28290462910152));
#44774=CARTESIAN_POINT('Ctrl Pts',(0.0408343539197486,1.78032182704167,
9.28284748093711));
#44775=CARTESIAN_POINT('Ctrl Pts',(0.0402044820601876,1.780242000312,9.28280830155863));
#44776=CARTESIAN_POINT('Ctrl Pts',(0.0345371720173955,1.77954076511402,
9.28245682994647));
#44777=CARTESIAN_POINT('Ctrl Pts',(0.0294856040697999,1.77903653844019,
9.28215098169002));
#44778=CARTESIAN_POINT('Ctrl Pts',(0.0242906896697188,1.77864170172975,
9.28184214166569));
#44779=CARTESIAN_POINT('Ctrl Pts',(0.0241574755360709,1.77863166016607,
9.28183422585626));
#44780=CARTESIAN_POINT('Ctrl Pts',(0.00125812052171418,1.77691984593806,
9.2804741601245));
#44781=CARTESIAN_POINT('Ctrl Pts',(-0.0216270361881949,1.77764168175109,
9.27922222620605));
#44782=CARTESIAN_POINT('Ctrl Pts',(-0.0665934697885276,1.78387423876048,
9.27667621406895));
#44783=CARTESIAN_POINT('Ctrl Pts',(-0.0885502459302926,1.78930913974724,
9.27538821086509));
#44784=CARTESIAN_POINT('Ctrl Pts',(-0.110837505023448,1.7973821859204,9.27394672339378));
#44785=CARTESIAN_POINT('Ctrl Pts',(-0.111914926418665,1.79777898301173,
9.27387671241612));
#44786=CARTESIAN_POINT('Ctrl Pts',(-0.113482632557522,1.79836587690632,
9.27377435864941));
#44787=CARTESIAN_POINT('Ctrl Pts',(-0.113974617256266,1.79855143270735,
9.27374216776185));
#44788=CARTESIAN_POINT('Ctrl Pts',(-0.114836681755525,1.79887897903268,
9.27368563899117));
#44789=CARTESIAN_POINT('Ctrl Pts',(-0.115206958782272,1.79902045021149,
9.27366131855748));
#44790=CARTESIAN_POINT('Ctrl Pts',(-0.11592500622157,1.79929631268795,9.27361407791087));
#44791=CARTESIAN_POINT('Ctrl Pts',(-0.11627280644981,1.79943062513123,9.27359116037632));
#44792=CARTESIAN_POINT('Ctrl Pts',(-0.117101964863913,1.79975248156063,
9.27353643941066));
#44793=CARTESIAN_POINT('Ctrl Pts',(-0.11758310558766,1.79994057958566,9.27350461738098));
#44794=CARTESIAN_POINT('Ctrl Pts',(-0.119034705668059,1.80051209828081,
9.27340840133472));
#44795=CARTESIAN_POINT('Ctrl Pts',(-0.120003750037001,1.80089907327853,
9.27334388764747));
#44796=CARTESIAN_POINT('Ctrl Pts',(-0.130151262535391,1.8050085997919,9.27266531714067));
#44797=CARTESIAN_POINT('Ctrl Pts',(-0.139154444755825,1.80914731707223,
9.27203716281452));
#44798=CARTESIAN_POINT('Ctrl Pts',(-0.155749352561397,1.81772292380553,
9.27082741857528));
#44799=CARTESIAN_POINT('Ctrl Pts',(-0.163378220903477,1.8220688112014,9.27024920684198));
#44800=CARTESIAN_POINT('Ctrl Pts',(-0.178880907023782,1.83175912273989,
9.26903009468696));
#44801=CARTESIAN_POINT('Ctrl Pts',(-0.186714857630283,1.83715195210883,
9.26838854159852));
#44802=CARTESIAN_POINT('Ctrl Pts',(-0.20116444380182,1.84807124172975,9.26716316978081));
#44803=CARTESIAN_POINT('Ctrl Pts',(-0.207819720008185,1.85353255548032,
9.26658014512682));
#44804=CARTESIAN_POINT('Ctrl Pts',(-0.221790308664973,1.86596547196683,
9.26532475042865));
#44805=CARTESIAN_POINT('Ctrl Pts',(-0.229013250206423,1.87302848568942,
9.26465501754457));
#44806=CARTESIAN_POINT('Ctrl Pts',(-0.238491223189037,1.88321058212053,
9.26375996569211));
#44807=CARTESIAN_POINT('Ctrl Pts',(-0.241039655550134,1.88604766213267,
9.26351756214457));
#44808=CARTESIAN_POINT('Ctrl Pts',(-0.243888865830784,1.88933513594731,
9.26324519764691));
#44809=CARTESIAN_POINT('Ctrl Pts',(-0.244239452458768,1.88974169767854,
9.26321166011458));
#44810=CARTESIAN_POINT('Ctrl Pts',(-0.244766466172444,1.89035595186039,
9.26316121174955));
#44811=CARTESIAN_POINT('Ctrl Pts',(-0.244943646200372,1.89056299259612,
9.26314424543863));
#44812=CARTESIAN_POINT('Ctrl Pts',(-0.245260960192934,1.89093473795321,
9.26311385030455));
#44813=CARTESIAN_POINT('Ctrl Pts',(-0.245401190675574,1.89109935853284,
9.26310041431599));
#44814=CARTESIAN_POINT('Ctrl Pts',(-0.245703387916088,1.89145484073743,
9.26307145226073));
#44815=CARTESIAN_POINT('Ctrl Pts',(-0.245865297555767,1.8916457493975,9.26305593044334));
#44816=CARTESIAN_POINT('Ctrl Pts',(-0.246299976347489,1.89215949407944,
9.26301424581426));
#44817=CARTESIAN_POINT('Ctrl Pts',(-0.246572334323191,1.89248267975581,
9.26298811332896));
#44818=CARTESIAN_POINT('Ctrl Pts',(-0.247815404618548,1.89396363534135,
9.26286877265098));
#44819=CARTESIAN_POINT('Ctrl Pts',(-0.248778624072801,1.89512771114207,
9.26277610500984));
#44820=CARTESIAN_POINT('Ctrl Pts',(-0.270015356635874,1.9211634926797,9.26072754557983));
#44821=CARTESIAN_POINT('Ctrl Pts',(-0.286473783744934,1.94892260894471,
9.25901475177345));
#44822=CARTESIAN_POINT('Ctrl Pts',(-0.305082839575014,1.99471090782702,
9.2562125617498));
#44823=CARTESIAN_POINT('Ctrl Pts',(-0.3103000924616,2.01125850975935,9.25520671904228));
#44824=CARTESIAN_POINT('Ctrl Pts',(-0.314424179314365,2.0292893755722,9.25408214394024));
#44825=CARTESIAN_POINT('Ctrl Pts',(-0.314679958019772,2.0304364973001,9.254010488205));
#44826=CARTESIAN_POINT('Ctrl Pts',(-0.315042150364789,2.03210374870938,
9.25390617363479));
#44827=CARTESIAN_POINT('Ctrl Pts',(-0.315153564583383,2.03262279190371,
9.25387367511036));
#44828=CARTESIAN_POINT('Ctrl Pts',(-0.315346095010384,2.03353065558077,
9.25381678940207));
#44829=CARTESIAN_POINT('Ctrl Pts',(-0.315427776041648,2.0339193562005,9.25379242035267));
#44830=CARTESIAN_POINT('Ctrl Pts',(-0.315584445902157,2.03467182019226,
9.25374521913995));
#44831=CARTESIAN_POINT('Ctrl Pts',(-0.315659524916964,2.03503556434659,
9.25372238990259));
#44832=CARTESIAN_POINT('Ctrl Pts',(-0.315836445533802,2.03590026035484,
9.25366809119387));
#44833=CARTESIAN_POINT('Ctrl Pts',(-0.31593772409802,2.03640132519493,9.25363660377891));
#44834=CARTESIAN_POINT('Ctrl Pts',(-0.31629157978337,2.03817369335655,9.25352514380728));
#44835=CARTESIAN_POINT('Ctrl Pts',(-0.316537676513447,2.03944626432851,
9.25344496471372));
#44836=CARTESIAN_POINT('Ctrl Pts',(-0.320452522200097,2.06036622311442,
9.25212433245832));
#44837=CARTESIAN_POINT('Ctrl Pts',(-0.322292725957246,2.08030773341298,
9.25082424572997));
#44838=CARTESIAN_POINT('Ctrl Pts',(-0.322248784874179,2.12948008707199,
9.24753308221895));
#44839=CARTESIAN_POINT('Ctrl Pts',(-0.318256680675824,2.15853321851025,
9.2455081317289));
#44840=CARTESIAN_POINT('Ctrl Pts',(-0.309997251839141,2.1881203943083,9.2435648412986));
#44841=CARTESIAN_POINT('Ctrl Pts',(-0.309576898017133,2.18958596136027,
9.24346893800038));
#44842=CARTESIAN_POINT('Ctrl Pts',(-0.309026333950325,2.191455346539,9.24334711406544));
#44843=CARTESIAN_POINT('Ctrl Pts',(-0.308905714432217,2.19186193488804,
9.24332064814244));
#44844=CARTESIAN_POINT('Ctrl Pts',(-0.30871252674617,2.19250845521428,9.24327861443535));
#44845=CARTESIAN_POINT('Ctrl Pts',(-0.308640481175702,2.1927485408877,9.24326301618634));
#44846=CARTESIAN_POINT('Ctrl Pts',(-0.308505169495327,2.1931975518534,9.24323386505611));
#44847=CARTESIAN_POINT('Ctrl Pts',(-0.308441971702367,2.19340649532863,
9.24322030833382));
#44848=CARTESIAN_POINT('Ctrl Pts',(-0.308299244740658,2.19387665244126,
9.24318982250214));
#44849=CARTESIAN_POINT('Ctrl Pts',(-0.308219596048025,2.19413782871169,
9.24317290055075));
#44850=CARTESIAN_POINT('Ctrl Pts',(-0.307981589522417,2.19491473644723,
9.24312260207076));
#44851=CARTESIAN_POINT('Ctrl Pts',(-0.307822267502995,2.19543017509621,
9.24308928197094));
#44852=CARTESIAN_POINT('Ctrl Pts',(-0.306502231125542,2.19966305495287,
9.24281604676594));
#44853=CARTESIAN_POINT('Ctrl Pts',(-0.3052754526768,2.2033597770709,9.24257993180317));
#44854=CARTESIAN_POINT('Ctrl Pts',(-0.301042285194321,2.21538223427711,
9.24181752714214));
#44855=CARTESIAN_POINT('Ctrl Pts',(-0.297759730578613,2.22360698221587,
9.24130462433327));
#44856=CARTESIAN_POINT('Ctrl Pts',(-0.283921579933928,2.25451660009095,
9.23937372389428));
#44857=CARTESIAN_POINT('Ctrl Pts',(-0.271077768142592,2.27607885477031,
9.23801286452511));
#44858=CARTESIAN_POINT('Ctrl Pts',(-0.255107782884667,2.29693339589262,
9.23650286999729));
#44859=CARTESIAN_POINT('Ctrl Pts',(-0.254340758183702,2.29792302035118,
9.23643073288618));
#44860=CARTESIAN_POINT('Ctrl Pts',(-0.246382678805956,2.30806797561422,
9.2356860906442));
#44861=CARTESIAN_POINT('Ctrl Pts',(-0.238707075100769,2.31683079106351,
9.23499907576622));
#44862=CARTESIAN_POINT('Ctrl Pts',(-0.229743389893656,2.32601010366434,
9.23421919173987));
#44863=CARTESIAN_POINT('Ctrl Pts',(-0.228907163141345,2.32685700950455,
9.23414664156011));
#44864=CARTESIAN_POINT('Ctrl Pts',(-0.227721234991966,2.328044849197,9.23404403131291));
#44865=CARTESIAN_POINT('Ctrl Pts',(-0.227375413408941,2.32838965713123,
9.23401414294733));
#44866=CARTESIAN_POINT('Ctrl Pts',(-0.226769321475982,2.32899123156108,
9.23396181741621));
#44867=CARTESIAN_POINT('Ctrl Pts',(-0.226509394782134,2.32924834430848,
9.23393939556259));
#44868=CARTESIAN_POINT('Ctrl Pts',(-0.225963071653665,2.32978691676569,
9.23389230654042));
#44869=CARTESIAN_POINT('Ctrl Pts',(-0.225676585722401,2.33006828447712,
9.23386763538982));
#44870=CARTESIAN_POINT('Ctrl Pts',(-0.224992335713205,2.33073780221853,
9.23380876165914));
#44871=CARTESIAN_POINT('Ctrl Pts',(-0.224594092963673,2.33112545922501,
9.23377453761601));
#44872=CARTESIAN_POINT('Ctrl Pts',(-0.223250307337467,2.33242677281488,
9.23365919266835));
#44873=CARTESIAN_POINT('Ctrl Pts',(-0.22230018577673,2.33333566330262,9.23357786509292));
#44874=CARTESIAN_POINT('Ctrl Pts',(-0.209290035872313,2.34562964207,9.23246722311068));
#44875=CARTESIAN_POINT('Ctrl Pts',(-0.196376254490532,2.35607118160359,
9.23139752377565));
#44876=CARTESIAN_POINT('Ctrl Pts',(-0.164463256981946,2.37803619956201,
9.22882743055535));
#44877=CARTESIAN_POINT('Ctrl Pts',(-0.144962522255172,2.38868331363324,
9.22730782442123));
#44878=CARTESIAN_POINT('Ctrl Pts',(-0.113999883711374,2.40165446173952,
9.22506730081162));
#44879=CARTESIAN_POINT('Ctrl Pts',(-0.103246949205295,2.40550207786571,
9.22431916701531));
#44880=CARTESIAN_POINT('Ctrl Pts',(-0.0915930384696644,2.40898616956389,
9.22355554197668));
#44881=CARTESIAN_POINT('Ctrl Pts',(-0.0908739940220044,2.40919840703829,
9.22350861525267));
#44882=CARTESIAN_POINT('Ctrl Pts',(-0.0898761893278974,2.40948914370782,
9.2234437637663));
#44883=CARTESIAN_POINT('Ctrl Pts',(-0.0895980612295598,2.4095697771208,
9.22342571585984));
#44884=CARTESIAN_POINT('Ctrl Pts',(-0.0891199831508987,2.40970768070441,
9.22339474299419));
#44885=CARTESIAN_POINT('Ctrl Pts',(-0.0889200863736359,2.40976513219532,
9.22338180742166));
#44886=CARTESIAN_POINT('Ctrl Pts',(-0.0885069590612355,2.4098834345241,
9.2233551045819));
#44887=CARTESIAN_POINT('Ctrl Pts',(-0.0882937217555166,2.40994425868776,
9.22334133896922));
#44888=CARTESIAN_POINT('Ctrl Pts',(-0.0877921231587887,2.41008677585772,
9.22330899812379));
#44889=CARTESIAN_POINT('Ctrl Pts',(-0.0875037094745219,2.41016828703223,
9.22329043357298));
#44890=CARTESIAN_POINT('Ctrl Pts',(-0.0865630749125925,2.41043271176501,
9.22322998703071));
#44891=CARTESIAN_POINT('Ctrl Pts',(-0.0859103854186231,2.4106139729132,
9.22318820091608));
#44892=CARTESIAN_POINT('Ctrl Pts',(-0.0727909785173573,2.41421290288505,
9.22235133140243));
#44893=CARTESIAN_POINT('Ctrl Pts',(-0.0601285950861957,2.41687997430841,
9.22159878679526));
#44894=CARTESIAN_POINT('Ctrl Pts',(-0.0161271052058792,2.42341418340386,
9.2190661744642));
#44895=CARTESIAN_POINT('Ctrl Pts',(0.0155942167075223,2.42344045047705,
9.21736335468718));
#44896=CARTESIAN_POINT('Ctrl Pts',(0.0480562626852495,2.41867435727282,
9.21542358371179));
#44897=CARTESIAN_POINT('Ctrl Pts',(0.0492967514059602,2.41848482005429,
9.21534918727704));
#44898=CARTESIAN_POINT('Ctrl Pts',(0.0555863691839977,2.41748618786691,
9.21497054562902));
#44899=CARTESIAN_POINT('Ctrl Pts',(0.0606166144981682,2.41656428331611,
9.21466301516741));
#44900=CARTESIAN_POINT('Ctrl Pts',(0.0664677751013699,2.41534735725944,
9.2142990747713));
#44901=CARTESIAN_POINT('Ctrl Pts',(0.0673122413211632,2.41516818209175,
9.21424639724153));
#44902=CARTESIAN_POINT('Ctrl Pts',(0.0686606896333905,2.41487640748671,
9.2141620347003));
#44903=CARTESIAN_POINT('Ctrl Pts',(0.0691651426531609,2.41476598502623,
9.2141304194692));
#44904=CARTESIAN_POINT('Ctrl Pts',(0.0700562669078341,2.41456867637374,
9.21407447206174));
#44905=CARTESIAN_POINT('Ctrl Pts',(0.0704430482838862,2.41448228826889,
9.21405015591157));
#44906=CARTESIAN_POINT('Ctrl Pts',(0.07124366655539,2.41430191805765,9.21399975416798));
#44907=CARTESIAN_POINT('Ctrl Pts',(0.0716574789330507,2.41420783158476,
9.2139736652637));
#44908=CARTESIAN_POINT('Ctrl Pts',(0.0727191237618679,2.41396424430588,
9.21390663553585));
#44909=CARTESIAN_POINT('Ctrl Pts',(0.0733666792505109,2.41381355615783,
9.21386565659768));
#44910=CARTESIAN_POINT('Ctrl Pts',(0.0760294514117654,2.41318522855685,
9.21369675981475));
#44911=CARTESIAN_POINT('Ctrl Pts',(0.0780404721594917,2.41269018093233,
9.21356828247209));
#44912=CARTESIAN_POINT('Ctrl Pts',(0.0913977379148219,2.4092651781221,9.21270864357123));
#44913=CARTESIAN_POINT('Ctrl Pts',(0.102580401096877,2.40573796288231,9.21195815715932));
#44914=CARTESIAN_POINT('Ctrl Pts',(0.145276297111396,2.38966452237933,9.20896947933284));
#44915=CARTESIAN_POINT('Ctrl Pts',(0.17491814387827,2.37278914454418,9.20659769555844));
#44916=CARTESIAN_POINT('Ctrl Pts',(0.204382589033286,2.34920612274939,9.20416775590719));
#44917=CARTESIAN_POINT('Ctrl Pts',(0.207338889715483,2.34675194501224,9.20392336750097));
#44918=CARTESIAN_POINT('Ctrl Pts',(0.210686342041663,2.34387039843719,9.20364666092771));
#44919=CARTESIAN_POINT('Ctrl Pts',(0.211120929197663,2.34349426938561,9.2036107375397));
#44920=CARTESIAN_POINT('Ctrl Pts',(0.211766562770423,2.3429324546685,9.20355737251683));
#44921=CARTESIAN_POINT('Ctrl Pts',(0.211978373227364,2.34274765482736,9.20353986585437));
#44922=CARTESIAN_POINT('Ctrl Pts',(0.212352036702831,2.34242077987284,9.20350898310903));
#44923=CARTESIAN_POINT('Ctrl Pts',(0.212513989281265,2.34227881947637,9.20349559846286));
#44924=CARTESIAN_POINT('Ctrl Pts',(0.212829194895273,2.34200196508985,9.20346954927287));
#44925=CARTESIAN_POINT('Ctrl Pts',(0.212982461528205,2.34186708827177,9.20345688351602));
#44926=CARTESIAN_POINT('Ctrl Pts',(0.213399442329204,2.34149943554349,9.20342242575821));
#44927=CARTESIAN_POINT('Ctrl Pts',(0.213662904715161,2.34126637251329,9.20340065528547));
#44928=CARTESIAN_POINT('Ctrl Pts',(0.214680787731406,2.34036296202908,9.20331654718097));
#44929=CARTESIAN_POINT('Ctrl Pts',(0.215432449846251,2.33968949445776,9.20325444084433));
#44930=CARTESIAN_POINT('Ctrl Pts',(0.22020021859646,2.3353771644264,9.20286043248825));
#44931=CARTESIAN_POINT('Ctrl Pts',(0.224127435672611,2.3316407705738,9.20253556745034));
#44932=CARTESIAN_POINT('Ctrl Pts',(0.233038471009759,2.32272379101292,9.20179236723782));
#44933=CARTESIAN_POINT('Ctrl Pts',(0.237947013785835,2.31747194532052,9.20137826629825));
#44934=CARTESIAN_POINT('Ctrl Pts',(0.263631855131663,2.28807887105489,9.19915701602563));
#44935=CARTESIAN_POINT('Ctrl Pts',(0.280916417198049,2.26112561489226,9.19743824819553));
#44936=CARTESIAN_POINT('Ctrl Pts',(0.296375529083666,2.2267170770787,9.19520383593953));
#44937=CARTESIAN_POINT('Ctrl Pts',(0.298635507183917,2.22129509043419,9.19485140084271));
#44938=CARTESIAN_POINT('Ctrl Pts',(0.301101523517411,2.21489137038469,9.19443365753669));
#44939=CARTESIAN_POINT('Ctrl Pts',(0.301452808295963,2.21396648099165,9.19437328780386));
#44940=CARTESIAN_POINT('Ctrl Pts',(0.301975765990522,2.21257026243526,9.19428209534672));
#44941=CARTESIAN_POINT('Ctrl Pts',(0.30215060862232,2.21210012013807,9.19425137866463));
#44942=CARTESIAN_POINT('Ctrl Pts',(0.302460485357941,2.21126088658841,9.19419652913191));
#44943=CARTESIAN_POINT('Ctrl Pts',(0.302595943533375,2.21089195210824,9.19417241049113));
#44944=CARTESIAN_POINT('Ctrl Pts',(0.302880109608514,2.21011359846548,9.19412151288739));
#44945=CARTESIAN_POINT('Ctrl Pts',(0.303028662883704,2.20970412404022,9.19409472882898));
#44946=CARTESIAN_POINT('Ctrl Pts',(0.303418905909796,2.20862161182886,9.19402389911311));
#44947=CARTESIAN_POINT('Ctrl Pts',(0.303659185421062,2.20794807138638,9.19397980664445));
#44948=CARTESIAN_POINT('Ctrl Pts',(0.304737649454518,2.2048928761645,9.19377969725775));
#44949=CARTESIAN_POINT('Ctrl Pts',(0.305550051225639,2.20250227352422,9.19362282807738));
#44950=CARTESIAN_POINT('Ctrl Pts',(0.30898060578398,2.1920040623906,9.19293251834585));
#44951=CARTESIAN_POINT('Ctrl Pts',(0.31130455336543,2.1838046264506,9.19238953671076));
#44952=CARTESIAN_POINT('Ctrl Pts',(0.316659892285136,2.16158855380709,9.19090722490897));
#44953=CARTESIAN_POINT('Ctrl Pts',(0.319085226795173,2.14744659138467,9.18995131206832));
#44954=CARTESIAN_POINT('Ctrl Pts',(0.322873885072103,2.11085602244097,9.18746970081982));
#44955=CARTESIAN_POINT('Ctrl Pts',(0.322846002755955,2.08833879227044,9.18593206406742));
#44956=CARTESIAN_POINT('Ctrl Pts',(0.32010047891312,2.06245520685477,9.18425922995424));
#44957=CARTESIAN_POINT('Ctrl Pts',(0.31966478467034,2.05891038867476,9.18403233229352));
#44958=CARTESIAN_POINT('Ctrl Pts',(0.31909235015928,2.05481632979918,9.18377339520442));
#44959=CARTESIAN_POINT('Ctrl Pts',(0.319013005767058,2.05425949119423,9.18373824377928));
#44960=CARTESIAN_POINT('Ctrl Pts',(0.318892195623884,2.05342725309844,9.18368581034115));
#44961=CARTESIAN_POINT('Ctrl Pts',(0.318851830563197,2.05315169873217,9.18366846651512));
#44962=CARTESIAN_POINT('Ctrl Pts',(0.31877983185913,2.05266459912261,9.18363783801377));
#44963=CARTESIAN_POINT('Ctrl Pts',(0.318748344770384,2.05245303286674,9.18362454499482));
#44964=CARTESIAN_POINT('Ctrl Pts',(0.31868638253136,2.05203952751024,9.18359858378368));
#44965=CARTESIAN_POINT('Ctrl Pts',(0.31865592616886,2.05183758674664,9.18358591455372));
#44966=CARTESIAN_POINT('Ctrl Pts',(0.318572047551832,2.05128499250872,9.18355127128435));
#44967=CARTESIAN_POINT('Ctrl Pts',(0.318518238120746,2.05093439673691,9.18352931930948));
#44968=CARTESIAN_POINT('Ctrl Pts',(0.31830574446174,2.04956497395864,9.18344368049867));
#44969=CARTESIAN_POINT('Ctrl Pts',(0.318142747654755,2.04854680775884,9.18338023590473));
#44970=CARTESIAN_POINT('Ctrl Pts',(0.317060019534267,2.04198540971057,9.18297274715278));
#44971=CARTESIAN_POINT('Ctrl Pts',(0.316000271256853,2.03646586493018,9.18263626742063));
#44972=CARTESIAN_POINT('Ctrl Pts',(0.313226104936017,2.02381368238275,9.18187371911683));
#44973=CARTESIAN_POINT('Ctrl Pts',(0.311411453922295,2.01670614103382,9.1814518247345));
#44974=CARTESIAN_POINT('Ctrl Pts',(0.30051338523428,1.97938473070011,9.17924226706982));
#44975=CARTESIAN_POINT('Ctrl Pts',(0.287273816074932,1.95056723682215,9.17753734320381));
#44976=CARTESIAN_POINT('Ctrl Pts',(0.266890924238613,1.91926788465284,9.17532413514828));
#44977=CARTESIAN_POINT('Ctrl Pts',(0.263592940729428,1.91449092195419,9.17497578603572));
#44978=CARTESIAN_POINT('Ctrl Pts',(0.25958617221436,1.9090100354833,9.17456246634513));
#44979=CARTESIAN_POINT('Ctrl Pts',(0.259000771036862,1.9082169248358,9.17450231487037));
#44980=CARTESIAN_POINT('Ctrl Pts',(0.258112476162487,1.90702493397563,9.17441138851136));
#44981=CARTESIAN_POINT('Ctrl Pts',(0.257812272560361,1.90662404862386,9.17438071874684));
#44982=CARTESIAN_POINT('Ctrl Pts',(0.257274879907028,1.9059099018883,9.17432592163146));
#44983=CARTESIAN_POINT('Ctrl Pts',(0.257038049620511,1.90559637076099,9.17430180838818));
#44984=CARTESIAN_POINT('Ctrl Pts',(0.256537208318572,1.90493584008329,9.17425088977127));
#44985=CARTESIAN_POINT('Ctrl Pts',(0.256273065495231,1.9045889418825,9.17422407923752));
#44986=CARTESIAN_POINT('Ctrl Pts',(0.255572681322295,1.9036729913772,9.17415310513886));
#44987=CARTESIAN_POINT('Ctrl Pts',(0.255135245252128,1.90310485945585,9.17410889441892));
#44988=CARTESIAN_POINT('Ctrl Pts',(0.253137334292922,1.90052785591324,9.17390749607163));
#44989=CARTESIAN_POINT('Ctrl Pts',(0.251555039171011,1.89853608772178,9.1737494426714));
#44990=CARTESIAN_POINT('Ctrl Pts',(0.244547562709446,1.88992645955553,9.17305553378745));
#44991=CARTESIAN_POINT('Ctrl Pts',(0.238884020454427,1.88350795528189,9.17251005970223));
#44992=CARTESIAN_POINT('Ctrl Pts',(0.226727683386967,1.87078959278926,9.17136859285812));
#44993=CARTESIAN_POINT('Ctrl Pts',(0.220211533302147,1.86452237331555,9.17077197360049));
#44994=CARTESIAN_POINT('Ctrl Pts',(0.190948838587609,1.83865556592288,9.16816286969854));
#44995=CARTESIAN_POINT('Ctrl Pts',(0.165789524914751,1.82201390988374,9.16607658136737));
#44996=CARTESIAN_POINT('Ctrl Pts',(0.137323785113586,1.80844272097868,9.16408179344562));
#44997=CARTESIAN_POINT('Ctrl Pts',(0.135952221353923,1.80780064573863,9.16398654004472));
#44998=CARTESIAN_POINT('Ctrl Pts',(0.134194982601358,1.80699307474984,9.16386564652002));
#44999=CARTESIAN_POINT('Ctrl Pts',(0.133813469911855,1.80681864507642,9.1638394679706));
#45000=CARTESIAN_POINT('Ctrl Pts',(0.133207383923417,1.80654296877555,9.16379798968754));
#45001=CARTESIAN_POINT('Ctrl Pts',(0.132983034917777,1.80644123461934,9.16378265994439));
#45002=CARTESIAN_POINT('Ctrl Pts',(0.132560040236013,1.80625000625294,9.16375380203724));
#45003=CARTESIAN_POINT('Ctrl Pts',(0.132361421845507,1.80616045687946,9.16374027054313));
#45004=CARTESIAN_POINT('Ctrl Pts',(0.131971332015904,1.80598505619314,9.16371373129254));
#45005=CARTESIAN_POINT('Ctrl Pts',(0.131779868505301,1.80589919090025,9.16370072269295));
#45006=CARTESIAN_POINT('Ctrl Pts',(0.131186650982674,1.80563384731431,9.16366047109091));
#45007=CARTESIAN_POINT('Ctrl Pts',(0.13078461098561,1.80545500381467,9.16363326719018));
#45008=CARTESIAN_POINT('Ctrl Pts',(0.128663183824598,1.80451650790113,9.16349011394637));
#45009=CARTESIAN_POINT('Ctrl Pts',(0.126937495494548,1.80377106554039,9.1633750221242));
#45010=CARTESIAN_POINT('Ctrl Pts',(0.0995909339366301,1.79224108174669,
9.16157102601071));
#45011=CARTESIAN_POINT('Ctrl Pts',(0.072682332224846,1.7847988969068,9.16006252846432));
#45012=CARTESIAN_POINT('Ctrl Pts',(0.024363515506679,1.77796232442062,9.15731991706862));
#45013=CARTESIAN_POINT('Ctrl Pts',(0.00334423127245716,1.77705966082569,
9.15611655528472));
#45014=CARTESIAN_POINT('Ctrl Pts',(-0.018909361647475,1.77827760357419,
9.15476293823062));
#45015=CARTESIAN_POINT('Ctrl Pts',(-0.0202064611593273,1.77835646567975,
9.15468376974191));
#45016=CARTESIAN_POINT('Ctrl Pts',(-0.0220136586492022,1.77847731594518,
9.15457307981676));
#45017=CARTESIAN_POINT('Ctrl Pts',(-0.0225241993204483,1.77851267836952,
9.15454176632268));
#45018=CARTESIAN_POINT('Ctrl Pts',(-0.0234052618374122,1.77857581391439,
9.15448765199493));
#45019=CARTESIAN_POINT('Ctrl Pts',(-0.0237758249497694,1.7786030121041,
9.15446486924649));
#45020=CARTESIAN_POINT('Ctrl Pts',(-0.024542325788662,1.77866060378367,
9.15441769578054));
#45021=CARTESIAN_POINT('Ctrl Pts',(-0.0249382558878842,1.77869108834821,
9.15439330223868));
#45022=CARTESIAN_POINT('Ctrl Pts',(-0.02586281170737,1.77876399354865,9.15433627743853));
#45023=CARTESIAN_POINT('Ctrl Pts',(-0.0263913899086573,1.77880698730584,
9.15430362822502));
#45024=CARTESIAN_POINT('Ctrl Pts',(-0.0280881253106708,1.77894921385831,
9.1541986701978));
#45025=CARTESIAN_POINT('Ctrl Pts',(-0.0292558379016475,1.77905351543267,
9.15412620225493));
#45026=CARTESIAN_POINT('Ctrl Pts',(-0.0470739355504622,1.7807430991598,
9.15301676544352));
#45027=CARTESIAN_POINT('Ctrl Pts',(-0.0635739325559083,1.78361555330946,
9.15193863340219));
#45028=CARTESIAN_POINT('Ctrl Pts',(-0.106843161993814,1.79467024787076,
9.14897655377452));
#45029=CARTESIAN_POINT('Ctrl Pts',(-0.13289537377269,1.80507559073,9.14704138917412));
#45030=CARTESIAN_POINT('Ctrl Pts',(-0.158653774177087,1.81947791907748,
9.14511767977599));
#45031=CARTESIAN_POINT('Ctrl Pts',(-0.160023318368942,1.82025691124188,
9.1450154057203));
#45032=CARTESIAN_POINT('Ctrl Pts',(-0.165172319279618,1.82323583327889,
9.14463107016673));
#45033=CARTESIAN_POINT('Ctrl Pts',(-0.16891279146486,1.82550269105857,9.14435223373808));
#45034=CARTESIAN_POINT('Ctrl Pts',(-0.173110100509541,1.82816471016865,
9.14404077000811));
#45035=CARTESIAN_POINT('Ctrl Pts',(-0.173613132410826,1.828485705783,9.14400346599354));
#45036=CARTESIAN_POINT('Ctrl Pts',(-0.174355667562551,1.82896244093522,
9.14394843943619));
#45037=CARTESIAN_POINT('Ctrl Pts',(-0.174595856299142,1.8291171024231,9.14393064592648));
#45038=CARTESIAN_POINT('Ctrl Pts',(-0.175017808737747,1.82938959892126,
9.14389939811565));
#45039=CARTESIAN_POINT('Ctrl Pts',(-0.17519965958223,1.82950729800834,9.14388593470682));
#45040=CARTESIAN_POINT('Ctrl Pts',(-0.17555261033988,1.82973624312907,9.14385981102049));
#45041=CARTESIAN_POINT('Ctrl Pts',(-0.175723722743999,1.82984746800987,
9.14384714937398));
#45042=CARTESIAN_POINT('Ctrl Pts',(-0.176184476109127,1.8301475855677,9.14381306388029));
#45043=CARTESIAN_POINT('Ctrl Pts',(-0.176473919941158,1.83033678267132,
9.14379166048539));
#45044=CARTESIAN_POINT('Ctrl Pts',(-0.177570856838353,1.83105632609318,
9.14371057764903));
#45045=CARTESIAN_POINT('Ctrl Pts',(-0.178376278795038,1.83158984342593,
9.14365110866441));
#45046=CARTESIAN_POINT('Ctrl Pts',(-0.195424642986039,1.84299343314277,
9.14239345424319));
#45047=CARTESIAN_POINT('Ctrl Pts',(-0.210650655458016,1.85531710214423,
9.14129078237415));
#45048=CARTESIAN_POINT('Ctrl Pts',(-0.241265745106421,1.88508608544191,
9.13889961355804));
#45049=CARTESIAN_POINT('Ctrl Pts',(-0.256074983088156,1.90296534428046,
9.13761771849584));
#45050=CARTESIAN_POINT('Ctrl Pts',(-0.273000593140756,1.92856853107664,
9.13581399083593));
#45051=CARTESIAN_POINT('Ctrl Pts',(-0.276937822320651,1.93500454240386,
9.13536355167743));
#45052=CARTESIAN_POINT('Ctrl Pts',(-0.281122452668338,1.94241737469235,
9.13484563951005));
#45053=CARTESIAN_POINT('Ctrl Pts',(-0.281595642696187,1.94326451845423,
9.13478646631951));
#45054=CARTESIAN_POINT('Ctrl Pts',(-0.2823059005357,1.94454967934448,9.13469671394541));
#45055=CARTESIAN_POINT('Ctrl Pts',(-0.282545793580845,1.94498613547637,
9.13466623581234));
#45056=CARTESIAN_POINT('Ctrl Pts',(-0.28296119281772,1.9457460716037,9.13461317300681));
#45057=CARTESIAN_POINT('Ctrl Pts',(-0.283137158886007,1.94606930025932,
9.13459060478097));
#45058=CARTESIAN_POINT('Ctrl Pts',(-0.283502984159643,1.94674402721102,
9.13454349693796));
#45059=CARTESIAN_POINT('Ctrl Pts',(-0.283692744125307,1.94709557837874,
9.13451895383695));
#45060=CARTESIAN_POINT('Ctrl Pts',(-0.284139565542224,1.94792705917192,
9.13446090782268));
#45061=CARTESIAN_POINT('Ctrl Pts',(-0.284396064861843,1.94840728802505,
9.13442738502234));
#45062=CARTESIAN_POINT('Ctrl Pts',(-0.285237507572411,1.94999232466168,
9.13431674570738));
#45063=CARTESIAN_POINT('Ctrl Pts',(-0.285817234064097,1.95109987566199,
9.13423944486843));
#45064=CARTESIAN_POINT('Ctrl Pts',(-0.299013554261432,1.97667210717097,
9.13245472904365));
#45065=CARTESIAN_POINT('Ctrl Pts',(-0.308447821529095,2.00264424990726,
9.13062875611944));
#45066=CARTESIAN_POINT('Ctrl Pts',(-0.319128359725167,2.0502795604147,9.1273266524192));
#45067=CARTESIAN_POINT('Ctrl Pts',(-0.321717030553898,2.07148038515329,
9.12587722935952));
#45068=CARTESIAN_POINT('Ctrl Pts',(-0.322236906405087,2.09469047652434,
9.12440370653434));
#45069=CARTESIAN_POINT('Ctrl Pts',(-0.322262691384833,2.09659808113352,
9.12428345727989));
#45070=CARTESIAN_POINT('Ctrl Pts',(-0.322273624006796,2.09895613655316,
9.12413596567933));
#45071=CARTESIAN_POINT('Ctrl Pts',(-0.32227476794547,2.09940642361807,9.12410785308338));
#45072=CARTESIAN_POINT('Ctrl Pts',(-0.322274987464515,2.0999001627798,9.12407708571766));
#45073=CARTESIAN_POINT('Ctrl Pts',(-0.322274997995471,2.0999436107491,9.12407437874954));
#45074=CARTESIAN_POINT('Ctrl Pts',(-0.322274999740166,2.09998705874836,
9.12407167227341));
#45075=CARTESIAN_POINT('',(-0.322274883346534,2.1001520067383,8.8746518141229));
#45076=CARTESIAN_POINT('Ctrl Pts',(-0.3222749997412,2.09998708453407,9.12407167066716));
#45077=CARTESIAN_POINT('Ctrl Pts',(-0.322275006475149,2.10015511433518,
9.12406120370388));
#45078=CARTESIAN_POINT('Ctrl Pts',(-0.322274881796435,2.10032314458241,
9.12405074409919));
#45079=CARTESIAN_POINT('Ctrl Pts',(-0.322274305347323,2.10070137001345,
9.12402721693586));
#45080=CARTESIAN_POINT('Ctrl Pts',(-0.322273779350097,2.10091156537635,
9.12401415357674));
#45081=CARTESIAN_POINT('Ctrl Pts',(-0.322272318028823,2.10133139114295,
9.12398808538069));
#45082=CARTESIAN_POINT('Ctrl Pts',(-0.322271383815394,2.10154102055415,
9.12397508051068));
#45083=CARTESIAN_POINT('Ctrl Pts',(-0.322268314721346,2.10210599808351,
9.12394006173449));
#45084=CARTESIAN_POINT('Ctrl Pts',(-0.322265796640266,2.10246134515411,
9.12391806942701));
#45085=CARTESIAN_POINT('Ctrl Pts',(-0.322254373579189,2.10376827890683,
9.12383730285121));
#45086=CARTESIAN_POINT('Ctrl Pts',(-0.322241841434686,2.10471984101178,
9.12377872995073));
#45087=CARTESIAN_POINT('Ctrl Pts',(-0.322189763451291,2.10767872028998,
9.12359728136292));
#45088=CARTESIAN_POINT('Ctrl Pts',(-0.322135674229195,2.10968577667511,
9.12347518033166));
#45089=CARTESIAN_POINT('Ctrl Pts',(-0.320775593708641,2.14714916020973,
9.12121216451682));
#45090=CARTESIAN_POINT('Ctrl Pts',(-0.313642187258192,2.18215574250312,
9.11934376937572));
#45091=CARTESIAN_POINT('Ctrl Pts',(-0.296840065034912,2.22601073377984,
9.11664109221615));
#45092=CARTESIAN_POINT('Ctrl Pts',(-0.292168132095394,2.23649347269981,
9.11596741218478));
#45093=CARTESIAN_POINT('Ctrl Pts',(-0.286017448215895,2.24852397873105,
9.11515046246578));
#45094=CARTESIAN_POINT('Ctrl Pts',(-0.285069785752339,2.25033485921376,
9.11502629301877));
#45095=CARTESIAN_POINT('Ctrl Pts',(-0.283792683116517,2.25271976387082,
9.11486112543761));
#45096=CARTESIAN_POINT('Ctrl Pts',(-0.283478593857897,2.25330198981519,
9.11482067285366));
#45097=CARTESIAN_POINT('Ctrl Pts',(-0.28296043157443,2.25425546751951,9.11475421031527));
#45098=CARTESIAN_POINT('Ctrl Pts',(-0.282757414183987,2.25462729324968,
9.11472823804613));
#45099=CARTESIAN_POINT('Ctrl Pts',(-0.282362918369925,2.25534643622598,
9.11467790027765));
#45100=CARTESIAN_POINT('Ctrl Pts',(-0.282171530714198,2.25569380260841,
9.11465353805747));
#45101=CARTESIAN_POINT('Ctrl Pts',(-0.281728610304138,2.25649419882674,
9.11459729252982));
#45102=CARTESIAN_POINT('Ctrl Pts',(-0.28147662566395,2.25694697617399,9.11456539306317));
#45103=CARTESIAN_POINT('Ctrl Pts',(-0.280667922864831,2.25839187778283,
9.11446333236868));
#45104=CARTESIAN_POINT('Ctrl Pts',(-0.280107047500515,2.25938165440284,
9.11439302182294));
#45105=CARTESIAN_POINT('Ctrl Pts',(-0.274963639465519,2.26834721675459,
9.1137524774507));
#45106=CARTESIAN_POINT('Ctrl Pts',(-0.270047256484492,2.27612563647447,
9.11317014631783));
#45107=CARTESIAN_POINT('Ctrl Pts',(-0.248100795797389,2.30776467540335,
9.11068382794482));
#45108=CARTESIAN_POINT('Ctrl Pts',(-0.22819021214043,2.32945339730725,9.10866920339826));
#45109=CARTESIAN_POINT('Ctrl Pts',(-0.20071956032415,2.3522171736639,9.1062844085321));
#45110=CARTESIAN_POINT('Ctrl Pts',(-0.195689190118125,2.35613979483159,
9.10586206442916));
#45111=CARTESIAN_POINT('Ctrl Pts',(-0.18735542194903,2.36224943723577,9.10518908383455));
#45112=CARTESIAN_POINT('Ctrl Pts',(-0.18412242358853,2.36452931363229,9.10493421699836));
#45113=CARTESIAN_POINT('Ctrl Pts',(-0.179128041178886,2.36791535800599,
9.10455082618691));
#45114=CARTESIAN_POINT('Ctrl Pts',(-0.177396676352101,2.36906488799995,
9.10441976515729));
#45115=CARTESIAN_POINT('Ctrl Pts',(-0.175379766890807,2.37037607175871,
9.10426932463242));
#45116=CARTESIAN_POINT('Ctrl Pts',(-0.175105001037186,2.37055410074208,
9.10424887758286));
#45117=CARTESIAN_POINT('Ctrl Pts',(-0.174583330062121,2.37089097933189,
9.10421014776225));
#45118=CARTESIAN_POINT('Ctrl Pts',(-0.174336478495952,2.37104991069219,
9.10419185957968));
#45119=CARTESIAN_POINT('Ctrl Pts',(-0.173906165574756,2.37132612961839,
9.10416004706679));
#45120=CARTESIAN_POINT('Ctrl Pts',(-0.173722802175522,2.37144356880211,
9.10414651255123));
#45121=CARTESIAN_POINT('Ctrl Pts',(-0.173364690584578,2.37167241787107,
9.10412012119786));
#45122=CARTESIAN_POINT('Ctrl Pts',(-0.173189954364308,2.37178384477614,
9.10410726320088));
#45123=CARTESIAN_POINT('Ctrl Pts',(-0.172773179786678,2.37204905109484,
9.10407664054567));
#45124=CARTESIAN_POINT('Ctrl Pts',(-0.172531042928088,2.37220267647992,
9.10405888620415));
#45125=CARTESIAN_POINT('Ctrl Pts',(-0.171669159522273,2.37274789223841,
9.10399581920212));
#45126=CARTESIAN_POINT('Ctrl Pts',(-0.171048276206163,2.37313769473147,
9.10395062455782));
#45127=CARTESIAN_POINT('Ctrl Pts',(-0.161843376570682,2.37887301183097,
9.10328401466832));
#45128=CARTESIAN_POINT('Ctrl Pts',(-0.15301272663086,2.38381435482472,9.10268839078678));
#45129=CARTESIAN_POINT('Ctrl Pts',(-0.14079870778581,2.38991276445583,9.10190235699172));
#45130=CARTESIAN_POINT('Ctrl Pts',(-0.13760821335037,2.39144067643971,9.10170038046581));
#45131=CARTESIAN_POINT('Ctrl Pts',(-0.127819638621634,2.39593178741434,
9.10108899745989));
#45132=CARTESIAN_POINT('Ctrl Pts',(-0.121146308434953,2.39872572677038,
9.10068345075756));
#45133=CARTESIAN_POINT('Ctrl Pts',(-0.112373389731432,2.40205632643877,
9.10015850379826));
#45134=CARTESIAN_POINT('Ctrl Pts',(-0.110354698822169,2.40279967558499,
9.10003826576948));
#45135=CARTESIAN_POINT('Ctrl Pts',(-0.106004308987429,2.4043523503846,9.09978008297492));
#45136=CARTESIAN_POINT('Ctrl Pts',(-0.103670453392564,2.40515521258909,
9.09964214750342));
#45137=CARTESIAN_POINT('Ctrl Pts',(-0.0985766591353543,2.40684233054025,
9.09934196734812));
#45138=CARTESIAN_POINT('Ctrl Pts',(-0.0958135584986513,2.4077163228883,
9.09917968738911));
#45139=CARTESIAN_POINT('Ctrl Pts',(-0.0840697375560594,2.41125747899264,
9.09849119681587));
#45140=CARTESIAN_POINT('Ctrl Pts',(-0.0749871200052161,2.41356954157238,
9.09796160452972));
#45141=CARTESIAN_POINT('Ctrl Pts',(-0.054630931912622,2.41781631868772,
9.09676470484703));
#45142=CARTESIAN_POINT('Ctrl Pts',(-0.043329717323946,2.41955319344329,
9.09609343739053));
#45143=CARTESIAN_POINT('Ctrl Pts',(-0.0299318719113969,2.4208884803287,
9.09527933110038));
#45144=CARTESIAN_POINT('Ctrl Pts',(-0.02790093661394,2.42107144252262,9.09515544489651));
#45145=CARTESIAN_POINT('Ctrl Pts',(-0.0252096008689787,2.42128817054048,
9.09499059830643));
#45146=CARTESIAN_POINT('Ctrl Pts',(-0.0245506067106484,2.42133919805262,
9.09495018078039));
#45147=CARTESIAN_POINT('Ctrl Pts',(-0.0234691162626446,2.4214195942538,
9.0948837611441));
#45148=CARTESIAN_POINT('Ctrl Pts',(-0.0230467085712403,2.42145015820458,
9.09485779662383));
#45149=CARTESIAN_POINT('Ctrl Pts',(-0.0222285681444843,2.42150773508204,
9.09480746340354));
#45150=CARTESIAN_POINT('Ctrl Pts',(-0.0218328431805213,2.42153485023517,
9.09478309796098));
#45151=CARTESIAN_POINT('Ctrl Pts',(-0.0209197311695908,2.42159572338935,
9.09472682989403));
#45152=CARTESIAN_POINT('Ctrl Pts',(-0.0204023117249965,2.42162896344358,
9.09469491106923));
#45153=CARTESIAN_POINT('Ctrl Pts',(-0.0187476560859728,2.42173125289975,
9.09459272705157));
#45154=CARTESIAN_POINT('Ctrl Pts',(-0.0176101425610071,2.42179551974307,
9.09452231203086));
#45155=CARTESIAN_POINT('Ctrl Pts',(-0.00723308905086826,2.422326612463,
9.09387838328949));
#45156=CARTESIAN_POINT('Ctrl Pts',(0.00202135993366873,2.42240137786294,
9.09329263069196));
#45157=CARTESIAN_POINT('Ctrl Pts',(0.0352820480361989,2.4212380003023,9.09114317776906));
#45158=CARTESIAN_POINT('Ctrl Pts',(0.0591264892367729,2.41771436128919,
9.08951197234216));
#45159=CARTESIAN_POINT('Ctrl Pts',(0.0990626665044819,2.40715869967483,
9.08672231035184));
#45160=CARTESIAN_POINT('Ctrl Pts',(0.115392011659044,2.40140459384369,9.08556658588));
#45161=CARTESIAN_POINT('Ctrl Pts',(0.131601180017179,2.39418109189191,9.08445380821981));
#45162=CARTESIAN_POINT('Ctrl Pts',(0.132019144096375,2.39399376014938,9.08442513979912));
#45163=CARTESIAN_POINT('Ctrl Pts',(0.132698529429929,2.39368751827354,9.08437858321099));
#45164=CARTESIAN_POINT('Ctrl Pts',(0.132960191795416,2.39356914943806,9.08436066251124));
#45165=CARTESIAN_POINT('Ctrl Pts',(0.133462747505817,2.39334099736355,9.08432626398026));
#45166=CARTESIAN_POINT('Ctrl Pts',(0.133703664329392,2.39323126683924,9.08430978294207));
#45167=CARTESIAN_POINT('Ctrl Pts',(0.134139030605454,2.39303232221435,9.08428001641208));
#45168=CARTESIAN_POINT('Ctrl Pts',(0.134333525935228,2.39294321156973,9.08426672459544));
#45169=CARTESIAN_POINT('Ctrl Pts',(0.134756214771293,2.39274904152564,9.08423785127734));
#45170=CARTESIAN_POINT('Ctrl Pts',(0.134984373566294,2.3926439092611,9.08422227440706));
#45171=CARTESIAN_POINT('Ctrl Pts',(0.135592672475447,2.39236275119539,9.08418076628492));
#45172=CARTESIAN_POINT('Ctrl Pts',(0.135972594309035,2.39218625004805,9.08415486441848));
#45173=CARTESIAN_POINT('Ctrl Pts',(0.137719369223773,2.3913706020711,9.08403587420011));
#45174=CARTESIAN_POINT('Ctrl Pts',(0.139082095910216,2.39072258807412,9.08394332569059));
#45175=CARTESIAN_POINT('Ctrl Pts',(0.166571108161113,2.37741328275147,9.08208112357642));
#45176=CARTESIAN_POINT('Ctrl Pts',(0.190877437684557,2.36128624279729,9.0805121452953));
#45177=CARTESIAN_POINT('Ctrl Pts',(0.227557527627569,2.32906331637341,9.07776389390964));
#45178=CARTESIAN_POINT('Ctrl Pts',(0.24118225007744,2.31467040042247,9.0766274197742));
#45179=CARTESIAN_POINT('Ctrl Pts',(0.254387679546605,2.29786519301612,9.07533161800282));
#45180=CARTESIAN_POINT('Ctrl Pts',(0.255365055717651,2.29660217264241,9.07523442858076));
#45181=CARTESIAN_POINT('Ctrl Pts',(0.256697291505717,2.29485388737421,9.07510014863325));
#45182=CARTESIAN_POINT('Ctrl Pts',(0.25706025239857,2.29437480165977,9.07506337732801));
#45183=CARTESIAN_POINT('Ctrl Pts',(0.257668876498846,2.2935667695236,9.07500140023602));
#45184=CARTESIAN_POINT('Ctrl Pts',(0.257915256205702,2.293238362635,9.07497622259242));
#45185=CARTESIAN_POINT('Ctrl Pts',(0.258400155899498,2.29258944590693,9.07492649511849));
#45186=CARTESIAN_POINT('Ctrl Pts',(0.258638708799228,2.29226896148886,9.07490194663601));
#45187=CARTESIAN_POINT('Ctrl Pts',(0.259161535677316,2.29156383482329,9.07484795840206));
#45188=CARTESIAN_POINT('Ctrl Pts',(0.25944555018983,2.29117900216706,9.07481850861884));
#45189=CARTESIAN_POINT('Ctrl Pts',(0.260426299051021,2.28984390124101,9.07471638930528));
#45190=CARTESIAN_POINT('Ctrl Pts',(0.261118671341194,2.28889045368603,9.0746435509255));
#45191=CARTESIAN_POINT('Ctrl Pts',(0.267971646547206,2.27934371998573,9.07391507052987));
#45192=CARTESIAN_POINT('Ctrl Pts',(0.273710394512728,2.27045688936647,9.07324336960817));
#45193=CARTESIAN_POINT('Ctrl Pts',(0.293156612953367,2.23682166995211,9.07072030861133));
#45194=CARTESIAN_POINT('Ctrl Pts',(0.304026197468064,2.21058305501842,9.06877500196839));
#45195=CARTESIAN_POINT('Ctrl Pts',(0.313509350448234,2.17512729855535,9.06632464026598));
#45196=CARTESIAN_POINT('Ctrl Pts',(0.315367144530446,2.16690150444282,9.06576913197874));
#45197=CARTESIAN_POINT('Ctrl Pts',(0.317527982219409,2.15521833912484,9.06500651763709));
#45198=CARTESIAN_POINT('Ctrl Pts',(0.318101083291201,2.15181493667886,9.06478748479683));
#45199=CARTESIAN_POINT('Ctrl Pts',(0.318675110532792,2.14803630899597,9.0645482402996));
#45200=CARTESIAN_POINT('Ctrl Pts',(0.318730156582255,2.14766970047466,9.0645250693411));
#45201=CARTESIAN_POINT('Ctrl Pts',(0.318832180235634,2.14698214219073,9.06448169098019));
#45202=CARTESIAN_POINT('Ctrl Pts',(0.318879306040537,2.14666121537159,9.06446147530497));
#45203=CARTESIAN_POINT('Ctrl Pts',(0.318958121175769,2.14611878821643,9.06442736124056));
#45204=CARTESIAN_POINT('Ctrl Pts',(0.318990064368904,2.14589732590451,9.06441344841606));
#45205=CARTESIAN_POINT('Ctrl Pts',(0.319053011537075,2.14545767286302,9.06438585885645));
#45206=CARTESIAN_POINT('Ctrl Pts',(0.3190840223818,2.14523948335588,9.06437218174185));
#45207=CARTESIAN_POINT('Ctrl Pts',(0.319152806957575,2.14475193200619,9.06434165282261));
#45208=CARTESIAN_POINT('Ctrl Pts',(0.319190463602595,2.14448255336209,9.06432480769925));
#45209=CARTESIAN_POINT('Ctrl Pts',(0.319316743859785,2.14357078417664,9.0642678669987));
#45210=CARTESIAN_POINT('Ctrl Pts',(0.319403770341209,2.14292816851452,9.06422786142024));
#45211=CARTESIAN_POINT('Ctrl Pts',(0.320269202997353,2.13638934369698,9.06382203549159));
#45212=CARTESIAN_POINT('Ctrl Pts',(0.320886251865582,2.13047246428515,9.06346508941599));
#45213=CARTESIAN_POINT('Ctrl Pts',(0.323441846839036,2.09701018556772,9.06148722178926));
#45214=CARTESIAN_POINT('Ctrl Pts',(0.321997935908956,2.06932018636643,9.05999733937826));
#45215=CARTESIAN_POINT('Ctrl Pts',(0.314292801448586,2.0270923927585,9.05756126713257));
#45216=CARTESIAN_POINT('Ctrl Pts',(0.310476159033951,2.01225065333368,9.05667383182674));
#45217=CARTESIAN_POINT('Ctrl Pts',(0.30484645385447,1.99542583108715,9.05560356648724));
#45218=CARTESIAN_POINT('Ctrl Pts',(0.304046802647151,1.9931231618751,9.05545568430393));
#45219=CARTESIAN_POINT('Ctrl Pts',(0.302981924785872,1.99016545400573,9.05526384283466));
#45220=CARTESIAN_POINT('Ctrl Pts',(0.302740543854714,1.98950186727925,9.05522067807311));
#45221=CARTESIAN_POINT('Ctrl Pts',(0.302347433612376,1.98843211482623,9.05515089164556));
#45222=CARTESIAN_POINT('Ctrl Pts',(0.302197061184328,1.98802545011126,9.05512431531084));
#45223=CARTESIAN_POINT('Ctrl Pts',(0.301908660365595,1.98725031599607,9.05507356829797));
#45224=CARTESIAN_POINT('Ctrl Pts',(0.301770776820922,1.98688179323624,9.05504940250127));
#45225=CARTESIAN_POINT('Ctrl Pts',(0.301454265192153,1.98604054668975,9.05499414814593));
#45226=CARTESIAN_POINT('Ctrl Pts',(0.301275199745717,1.9855679895534,9.05496304498086));
#45227=CARTESIAN_POINT('Ctrl Pts',(0.30072349520115,1.98412230195733,9.05486769143431));
#45228=CARTESIAN_POINT('Ctrl Pts',(0.300347249945259,1.98315056320575,9.05480332016054));
#45229=CARTESIAN_POINT('Ctrl Pts',(0.297516323594727,1.97594306553049,9.05432377768877));
#45230=CARTESIAN_POINT('Ctrl Pts',(0.2948725444212,1.96978380486147,9.0539022525128));
#45231=CARTESIAN_POINT('Ctrl Pts',(0.291217933122498,1.96195269162055,9.05335041249823));
#45232=CARTESIAN_POINT('Ctrl Pts',(0.290381143857444,1.9602010909893,9.05322593610089));
#45233=CARTESIAN_POINT('Ctrl Pts',(0.27846000916854,1.93581617674233,9.05147834770176));
#45234=CARTESIAN_POINT('Ctrl Pts',(0.264775143928008,1.91455445850191,9.0497665067054));
#45235=CARTESIAN_POINT('Ctrl Pts',(0.243445277099092,1.88865812894333,9.04750186303316));
#45236=CARTESIAN_POINT('Ctrl Pts',(0.237884061857403,1.88241742774186,9.04694088822569));
#45237=CARTESIAN_POINT('Ctrl Pts',(0.227945398587033,1.87210157551521,9.04599533383968));
#45238=CARTESIAN_POINT('Ctrl Pts',(0.223685570082029,1.86791903994608,9.04560635236445));
#45239=CARTESIAN_POINT('Ctrl Pts',(0.217255524220957,1.86194730047875,9.04504566256325));
#45240=CARTESIAN_POINT('Ctrl Pts',(0.215174351774094,1.86006448741249,9.04486806539365));
#45241=CARTESIAN_POINT('Ctrl Pts',(0.212803541462991,1.85797530428771,9.04467033448277));
#45242=CARTESIAN_POINT('Ctrl Pts',(0.2125379306748,1.85774202052125,9.04464824578138));
#45243=CARTESIAN_POINT('Ctrl Pts',(0.212088717189864,1.85734878743746,9.04461099679562));
#45244=CARTESIAN_POINT('Ctrl Pts',(0.211905316868588,1.85718860899648,9.04459581958623));
#45245=CARTESIAN_POINT('Ctrl Pts',(0.211545516882796,1.85687508448724,9.04456610439144));
#45246=CARTESIAN_POINT('Ctrl Pts',(0.211369131633147,1.85672172219908,9.04455156519638));
#45247=CARTESIAN_POINT('Ctrl Pts',(0.211030004580025,1.85642750747307,9.04452366566168));
#45248=CARTESIAN_POINT('Ctrl Pts',(0.210867288988695,1.85628662658034,9.04451030322114));
#45249=CARTESIAN_POINT('Ctrl Pts',(0.210487500401477,1.85595846666311,9.0444791699838));
#45250=CARTESIAN_POINT('Ctrl Pts',(0.210270317852951,1.85577131362137,9.04446140862002));
#45251=CARTESIAN_POINT('Ctrl Pts',(0.209606348590944,1.85520069256718,9.04440723640677));
#45252=CARTESIAN_POINT('Ctrl Pts',(0.209158757354753,1.85481815621063,9.04437089434597));
#45253=CARTESIAN_POINT('Ctrl Pts',(0.205531508013453,1.8517352685052,9.04407777831632));
#45254=CARTESIAN_POINT('Ctrl Pts',(0.202300560411064,1.8490955062827,9.04382534361546));
#45255=CARTESIAN_POINT('Ctrl Pts',(0.181547100657378,1.83280104723667,9.04225115014173));
#45256=CARTESIAN_POINT('Ctrl Pts',(0.16270130230223,1.82092443297682,9.04102735911498));
#45257=CARTESIAN_POINT('Ctrl Pts',(0.121029404880365,1.80033057584383,9.03842561374909));
#45258=CARTESIAN_POINT('Ctrl Pts',(0.0981369415389545,1.79207344374456,
9.03704870673249));
#45259=CARTESIAN_POINT('Ctrl Pts',(0.0734154974143381,1.78619644911943,
9.03550351910789));
#45260=CARTESIAN_POINT('Ctrl Pts',(0.0722928674158459,1.78593592202765,
9.03543324751682));
#45261=CARTESIAN_POINT('Ctrl Pts',(0.0706552562619125,1.78556512961063,
9.03533058278696));
#45262=CARTESIAN_POINT('Ctrl Pts',(0.0701413552161801,1.78545009420212,
9.03529834286745));
#45263=CARTESIAN_POINT('Ctrl Pts',(0.0692400311697343,1.7852506538068,9.03524175733529));
#45264=CARTESIAN_POINT('Ctrl Pts',(0.0688527290332559,1.78516570303121,
9.035217429281));
#45265=CARTESIAN_POINT('Ctrl Pts',(0.0681011762461286,1.78500231072156,
9.0351701954408));
#45266=CARTESIAN_POINT('Ctrl Pts',(0.0677369442102503,1.78492378565796,
9.03514729237321));
#45267=CARTESIAN_POINT('Ctrl Pts',(0.066868251327575,1.78473807943477,9.03509264034739));
#45268=CARTESIAN_POINT('Ctrl Pts',(0.0663636689485715,1.78463147742231,
9.03506087289785));
#45269=CARTESIAN_POINT('Ctrl Pts',(0.0648408445792485,1.78431357018751,
9.03496492944956));
#45270=CARTESIAN_POINT('Ctrl Pts',(0.063821840994417,1.78410598349297,9.03490063471555));
#45271=CARTESIAN_POINT('Ctrl Pts',(0.0532164249663374,1.7819989070027,9.03423047268535));
#45272=CARTESIAN_POINT('Ctrl Pts',(0.043550273294837,1.78053165508633,9.03361088607919));
#45273=CARTESIAN_POINT('Ctrl Pts',(0.00554897002411346,1.77652002141396,
9.03113751115445));
#45274=CARTESIAN_POINT('Ctrl Pts',(-0.0230039376590502,1.7772920234737,
9.02918395385637));
#45275=CARTESIAN_POINT('Ctrl Pts',(-0.0621378739288327,1.78357380052631,
9.02653261276485));
#45276=CARTESIAN_POINT('Ctrl Pts',(-0.0730992921926841,1.7859248409161,
9.02579509619019));
#45277=CARTESIAN_POINT('Ctrl Pts',(-0.0849046541894938,1.78910866601992,
9.02502162414042));
#45278=CARTESIAN_POINT('Ctrl Pts',(-0.0858909613162905,1.78937970981253,
9.02495716554849));
#45279=CARTESIAN_POINT('Ctrl Pts',(-0.0875907078029674,1.78985552656309,
9.02484638280143));
#45280=CARTESIAN_POINT('Ctrl Pts',(-0.0883047542407849,1.79005807495393,
9.0247999362208));
#45281=CARTESIAN_POINT('Ctrl Pts',(-0.0893171112507754,1.79034902542769,
9.02473422265243));
#45282=CARTESIAN_POINT('Ctrl Pts',(-0.0896159965050874,1.79043539351516,
9.02471483858047));
#45283=CARTESIAN_POINT('Ctrl Pts',(-0.0901296263993662,1.79058462201141,
9.0246815571545));
#45284=CARTESIAN_POINT('Ctrl Pts',(-0.0903444311065973,1.79064727339188,
9.02466764753554));
#45285=CARTESIAN_POINT('Ctrl Pts',(-0.0907560797482924,1.79076780292068,
9.02464100877524));
#45286=CARTESIAN_POINT('Ctrl Pts',(-0.0909529333496585,1.79082564524614,
9.02462827754002));
#45287=CARTESIAN_POINT('Ctrl Pts',(-0.0914171584975182,1.79096253221916,
9.02459827212528));
#45288=CARTESIAN_POINT('Ctrl Pts',(-0.0916844834848828,1.79104173607164,
9.02458100731142));
#45289=CARTESIAN_POINT('Ctrl Pts',(-0.0924757061242073,1.79127727924403,
9.02452994743874));
#45290=CARTESIAN_POINT('Ctrl Pts',(-0.0929993124530325,1.79143460591355,
9.02449620977019));
#45291=CARTESIAN_POINT('Ctrl Pts',(-0.0976615504268147,1.79284840203872,
9.02419625066563));
#45292=CARTESIAN_POINT('Ctrl Pts',(-0.101775141995487,1.79418680948757,
9.02393471142627));
#45293=CARTESIAN_POINT('Ctrl Pts',(-0.106070870010879,1.79568076689874,
9.02366367251167));
#45294=CARTESIAN_POINT('Ctrl Pts',(-0.106280882674865,1.79575404837766,
9.02365042703469));
#45295=CARTESIAN_POINT('Ctrl Pts',(-0.106622902779422,1.79587378966598,
9.02362886419469));
#45296=CARTESIAN_POINT('Ctrl Pts',(-0.106754955782624,1.79592011801898,
9.0236205408681));
#45297=CARTESIAN_POINT('Ctrl Pts',(-0.108187752979767,1.79642383678992,
9.0235302529396));
#45298=CARTESIAN_POINT('Ctrl Pts',(-0.109485598642127,1.79688949115594,
9.02344866188049));
#45299=CARTESIAN_POINT('Ctrl Pts',(-0.111181615058106,1.79751031983139,
9.02334224359467));
#45300=CARTESIAN_POINT('Ctrl Pts',(-0.111582503837899,1.79765797021254,
9.0233171044336));
#45301=CARTESIAN_POINT('Ctrl Pts',(-0.113693401612754,1.79844020018005,
9.0231848064235));
#45302=CARTESIAN_POINT('Ctrl Pts',(-0.115398322945125,1.79908850182212,
9.02307820639711));
#45303=CARTESIAN_POINT('Ctrl Pts',(-0.134534306301749,1.80655157786709,
9.02188363831265));
#45304=CARTESIAN_POINT('Ctrl Pts',(-0.151346725007813,1.8148583982693,9.0208502612785));
#45305=CARTESIAN_POINT('Ctrl Pts',(-0.187512548633575,1.83683245761938,
9.01848001257931));
#45306=CARTESIAN_POINT('Ctrl Pts',(-0.206270632575485,1.8512626085099,9.01713761193124));
#45307=CARTESIAN_POINT('Ctrl Pts',(-0.22411424970349,1.86840703063721,9.01563285797275));
#45308=CARTESIAN_POINT('Ctrl Pts',(-0.224939926906504,1.86920890483401,
9.01556267660811));
#45309=CARTESIAN_POINT('Ctrl Pts',(-0.226136895537483,1.87038389181608,
9.01546011952452));
#45310=CARTESIAN_POINT('Ctrl Pts',(-0.226511602865042,1.87075352473119,
9.01542789656799));
#45311=CARTESIAN_POINT('Ctrl Pts',(-0.227166967055043,1.87140318924002,
9.01537133067856));
#45312=CARTESIAN_POINT('Ctrl Pts',(-0.227448016554379,1.87168282461929,
9.01534700526632));
#45313=CARTESIAN_POINT('Ctrl Pts',(-0.227992252469832,1.87222632432509,
9.01529976909432));
#45314=CARTESIAN_POINT('Ctrl Pts',(-0.228255498730688,1.87249012809524,
9.01527686103908));
#45315=CARTESIAN_POINT('Ctrl Pts',(-0.228882151080609,1.87312028996735,
9.01522218523509));
#45316=CARTESIAN_POINT('Ctrl Pts',(-0.229245135157493,1.87348706458689,
9.01519039895804));
#45317=CARTESIAN_POINT('Ctrl Pts',(-0.2303378265689,1.87459648345323,9.01509436151209));
#45318=CARTESIAN_POINT('Ctrl Pts',(-0.231064812175091,1.87534178814511,
9.0150299912858));
#45319=CARTESIAN_POINT('Ctrl Pts',(-0.238609479032454,1.88315193128667,
9.01435694658384));
#45320=CARTESIAN_POINT('Ctrl Pts',(-0.24510387495697,1.89052058553551,9.01373442375532));
#45321=CARTESIAN_POINT('Ctrl Pts',(-0.261372982739389,1.91077380234019,
9.01205260599942));
#45322=CARTESIAN_POINT('Ctrl Pts',(-0.270531293858631,1.92411622972707,
9.01097237938289));
#45323=CARTESIAN_POINT('Ctrl Pts',(-0.286454423578706,1.95151977401775,
9.00883113761967));
#45324=CARTESIAN_POINT('Ctrl Pts',(-0.293278096205452,1.96549905498365,
9.00777401835445));
#45325=CARTESIAN_POINT('Ctrl Pts',(-0.301416414131682,1.98576744852609,
9.00632936518169));
#45326=CARTESIAN_POINT('Ctrl Pts',(-0.303593743880346,1.99168665674952,
9.00591764222151));
#45327=CARTESIAN_POINT('Ctrl Pts',(-0.306533254430586,2.00046483342446,
9.00532553806829));
#45328=CARTESIAN_POINT('Ctrl Pts',(-0.307431933958939,2.00327620275091,
9.0051386393623));
#45329=CARTESIAN_POINT('Ctrl Pts',(-0.308438544093791,2.00658108630446,
9.00492244088721));
#45330=CARTESIAN_POINT('Ctrl Pts',(-0.308584057440197,2.00706287921039,
9.00489100982645));
#45331=CARTESIAN_POINT('Ctrl Pts',(-0.308804604647059,2.00779933701887,
9.00484309965251));
#45332=CARTESIAN_POINT('Ctrl Pts',(-0.308880452607366,2.0080537542709,9.0048265730773));
#45333=CARTESIAN_POINT('Ctrl Pts',(-0.309011945093891,2.00849681919218,
9.00479783523089));
#45334=CARTESIAN_POINT('Ctrl Pts',(-0.309067731145831,2.00868542354199,
9.00478561564598));
#45335=CARTESIAN_POINT('Ctrl Pts',(-0.309193645609045,2.00911255887575,
9.00475797251417));
#45336=CARTESIAN_POINT('Ctrl Pts',(-0.309263670525435,2.00935111951457,
9.00474255512473));
#45337=CARTESIAN_POINT('Ctrl Pts',(-0.309452926383905,2.00999864752818,
9.00470076566954));
#45338=CARTESIAN_POINT('Ctrl Pts',(-0.309571623161641,2.01040777247811,
9.00467442490373));
#45339=CARTESIAN_POINT('Ctrl Pts',(-0.310103373853132,2.01225428872853,
9.00455581883096));
#45340=CARTESIAN_POINT('Ctrl Pts',(-0.310507238955926,2.01369433923061,
9.00446408159209));
#45341=CARTESIAN_POINT('Ctrl Pts',(-0.31842399826761,2.04269795961806,9.00263072165039));
#45342=CARTESIAN_POINT('Ctrl Pts',(-0.322250185622535,2.07114183972887,
9.00108379223631));
#45343=CARTESIAN_POINT('Ctrl Pts',(-0.322292708606286,2.12035583316686,
8.99831611482888));
#45344=CARTESIAN_POINT('Ctrl Pts',(-0.320328910151724,2.1409407739969,8.99713186083544));
#45345=CARTESIAN_POINT('Ctrl Pts',(-0.316165064019319,2.16247010811578,
8.99580001641923));
#45346=CARTESIAN_POINT('Ctrl Pts',(-0.315910768786297,2.16374361302958,
8.99572089933968));
#45347=CARTESIAN_POINT('Ctrl Pts',(-0.315545571964718,2.16551663449504,
8.99561026985634));
#45348=CARTESIAN_POINT('Ctrl Pts',(-0.315441165041495,2.16601748839965,
8.99557896509489));
#45349=CARTESIAN_POINT('Ctrl Pts',(-0.315258883359595,2.16688161270045,
8.99552486179717));
#45350=CARTESIAN_POINT('Ctrl Pts',(-0.315181572043718,2.16724500202043,
8.99550208132881));
#45351=CARTESIAN_POINT('Ctrl Pts',(-0.315020322116303,2.16799654393578,
8.99545490875717));
#45352=CARTESIAN_POINT('Ctrl Pts',(-0.314936294104923,2.16838467654912,
8.99543051382292));
#45353=CARTESIAN_POINT('Ctrl Pts',(-0.314738349805155,2.16929089534494,
8.99537347915603));
#45354=CARTESIAN_POINT('Ctrl Pts',(-0.314623871594004,2.16980885641241,
8.99534082144955));
#45355=CARTESIAN_POINT('Ctrl Pts',(-0.314252121547686,2.17147136423865,
8.99523580911401));
#45356=CARTESIAN_POINT('Ctrl Pts',(-0.313989881200544,2.17261477982269,
8.99516329512414));
#45357=CARTESIAN_POINT('Ctrl Pts',(-0.30986008649212,2.19018070326438,8.99404475084708));
#45358=CARTESIAN_POINT('Ctrl Pts',(-0.30471568917956,2.20627330785332,8.99295680877604));
#45359=CARTESIAN_POINT('Ctrl Pts',(-0.286003041000068,2.25207516615333,
8.98967376032413));
#45360=CARTESIAN_POINT('Ctrl Pts',(-0.269160515135467,2.28021407332836,
8.98739486096164));
#45361=CARTESIAN_POINT('Ctrl Pts',(-0.247449965475695,2.30647478025376,
8.98524051035267));
#45362=CARTESIAN_POINT('Ctrl Pts',(-0.246509136248264,2.307597124822,8.98514842101837));
#45363=CARTESIAN_POINT('Ctrl Pts',(-0.245287000093308,2.30903502524108,
8.98503046383317));
#45364=CARTESIAN_POINT('Ctrl Pts',(-0.245012697250623,2.30935647203548,
8.98500409571169));
#45365=CARTESIAN_POINT('Ctrl Pts',(-0.244576498250371,2.30986560834017,
8.98496233528198));
#45366=CARTESIAN_POINT('Ctrl Pts',(-0.244415017655317,2.31005365077986,
8.9849469124647));
#45367=CARTESIAN_POINT('Ctrl Pts',(-0.244124944600493,2.31039065039245,
8.98491927428553));
#45368=CARTESIAN_POINT('Ctrl Pts',(-0.243996433596923,2.31053967498084,
8.98490705305784));
#45369=CARTESIAN_POINT('Ctrl Pts',(-0.243693544845779,2.31089026260071,
8.98487830344671));
#45370=CARTESIAN_POINT('Ctrl Pts',(-0.243519053745588,2.31109172679994,
8.98486178364085));
#45371=CARTESIAN_POINT('Ctrl Pts',(-0.243011121440188,2.31167670809135,
8.98481381827052));
#45372=CARTESIAN_POINT('Ctrl Pts',(-0.242677020812362,2.31205965545101,
8.9847824215498));
#45373=CARTESIAN_POINT('Ctrl Pts',(-0.240324256752888,2.3147435601289,8.98456238353995));
#45374=CARTESIAN_POINT('Ctrl Pts',(-0.238273720840372,2.31701654455705,
8.98437607272098));
#45375=CARTESIAN_POINT('Ctrl Pts',(-0.231899027474132,2.3238834827933,8.98381206216466));
#45376=CARTESIAN_POINT('Ctrl Pts',(-0.227471905891558,2.3283801998085,8.98344111021582));
#45377=CARTESIAN_POINT('Ctrl Pts',(-0.211525873034527,2.34365281756978,
8.98216294440703));
#45378=CARTESIAN_POINT('Ctrl Pts',(-0.199350304318846,2.35371127627374,
8.98128673834704));
#45379=CARTESIAN_POINT('Ctrl Pts',(-0.166102657100906,2.37730082735027,
8.97900723737632));
#45380=CARTESIAN_POINT('Ctrl Pts',(-0.144109231529997,2.38934083550274,
8.97759673687758));
#45381=CARTESIAN_POINT('Ctrl Pts',(-0.119477176403842,2.39931404240088,
8.97598578725849));
#45382=CARTESIAN_POINT('Ctrl Pts',(-0.118002562302105,2.39989846083276,
8.97588927213166));
#45383=CARTESIAN_POINT('Ctrl Pts',(-0.115946824777426,2.40069568054871,
8.97575459766051));
#45384=CARTESIAN_POINT('Ctrl Pts',(-0.115369295456056,2.40091773648985,
8.97571674930933));
#45385=CARTESIAN_POINT('Ctrl Pts',(-0.114442717035968,2.40127093981285,
8.9756560030889));
#45386=CARTESIAN_POINT('Ctrl Pts',(-0.114094071616117,2.40140314775804,
8.97563314079787));
#45387=CARTESIAN_POINT('Ctrl Pts',(-0.113374343346964,2.40167464427719,
8.97558593383146));
#45388=CARTESIAN_POINT('Ctrl Pts',(-0.113003231529128,2.40181385387506,
8.97556158655962));
#45389=CARTESIAN_POINT('Ctrl Pts',(-0.112139327363209,2.40213610050925,
8.97550489448225));
#45390=CARTESIAN_POINT('Ctrl Pts',(-0.111646343156095,2.40231861673912,
8.97547253234952));
#45391=CARTESIAN_POINT('Ctrl Pts',(-0.110075838821987,2.40289569502334,
8.97536939972284));
#45392=CARTESIAN_POINT('Ctrl Pts',(-0.108996666007821,2.40328570540108,
8.97529847778512));
#45393=CARTESIAN_POINT('Ctrl Pts',(-0.0868648430226985,2.41115071012363,
8.97384280770841));
#45394=CARTESIAN_POINT('Ctrl Pts',(-0.0650979507228045,2.41642084420599,
8.97238249461339));
#45395=CARTESIAN_POINT('Ctrl Pts',(-0.0182843976412439,2.42271818418676,
8.96920744559877));
#45396=CARTESIAN_POINT('Ctrl Pts',(0.00669868180510105,2.42316648092403,
8.9674930727563));
#45397=CARTESIAN_POINT('Ctrl Pts',(0.0349364409174678,2.4203945215587,8.96567083961214));
#45398=CARTESIAN_POINT('Ctrl Pts',(0.0383825767318535,2.41999997588158,
8.9654505767972));
#45399=CARTESIAN_POINT('Ctrl Pts',(0.0423860005883355,2.41947601836279,
8.96519768941333));
#45400=CARTESIAN_POINT('Ctrl Pts',(0.0429499705841629,2.41940068784114,
8.96516213408975));
#45401=CARTESIAN_POINT('Ctrl Pts',(0.0437902246788931,2.41928618778304,
8.96510926699912));
#45402=CARTESIAN_POINT('Ctrl Pts',(0.044066658343582,2.41924815286904,8.96509189154038));
#45403=CARTESIAN_POINT('Ctrl Pts',(0.0445598138381334,2.41917964614282,
8.96506092495953));
#45404=CARTESIAN_POINT('Ctrl Pts',(0.0447765538375248,2.41914931262442,
8.96504732600611));
#45405=CARTESIAN_POINT('Ctrl Pts',(0.0452375734798722,2.41908431243781,
8.96501842313523));
#45406=CARTESIAN_POINT('Ctrl Pts',(0.0454818435490422,2.41904958612513,
8.96500312269235));
#45407=CARTESIAN_POINT('Ctrl Pts',(0.0461393344312507,2.41895534442267,
8.96496197539287));
#45408=CARTESIAN_POINT('Ctrl Pts',(0.0465524816531471,2.41889530629054,
8.96493615821471));
#45409=CARTESIAN_POINT('Ctrl Pts',(0.0485552434214584,2.41860029196252,
8.96481118933897));
#45410=CARTESIAN_POINT('Ctrl Pts',(0.0501432381348293,2.41835422664574,
8.96471265681813));
#45411=CARTESIAN_POINT('Ctrl Pts',(0.0635608965792229,2.41617222399697,
8.96388431309233));
#45412=CARTESIAN_POINT('Ctrl Pts',(0.0752773515315732,2.41358930501394,
8.96318852696976));
#45413=CARTESIAN_POINT('Ctrl Pts',(0.117537622248395,2.40176687051425,8.96069233819842));
#45414=CARTESIAN_POINT('Ctrl Pts',(0.146804152557456,2.38866408124679,8.9589706277231));
#45415=CARTESIAN_POINT('Ctrl Pts',(0.178498312820205,2.36838846429613,8.95674041182552));
#45416=CARTESIAN_POINT('Ctrl Pts',(0.183242155104524,2.36517224922392,8.95639639842107));
#45417=CARTESIAN_POINT('Ctrl Pts',(0.188695261160442,2.36125894847615,8.95598777410386));
#45418=CARTESIAN_POINT('Ctrl Pts',(0.189490371719116,2.36068283168546,8.9559278573092));
#45419=CARTESIAN_POINT('Ctrl Pts',(0.190686374103685,2.35980787585897,8.95583721715207));
#45420=CARTESIAN_POINT('Ctrl Pts',(0.191089228604709,2.35951171906864,8.95580659792171));
#45421=CARTESIAN_POINT('Ctrl Pts',(0.191800513675727,2.35898626659435,8.95575237864401));
#45422=CARTESIAN_POINT('Ctrl Pts',(0.192109227060549,2.35875735391853,8.95572879355539));
#45423=CARTESIAN_POINT('Ctrl Pts',(0.192758361392288,2.35827421523649,8.95567908943722));
#45424=CARTESIAN_POINT('Ctrl Pts',(0.193098690316879,2.35801986733161,8.95565296566828));
#45425=CARTESIAN_POINT('Ctrl Pts',(0.193793265388457,2.35749862647714,8.9555995166495));
#45426=CARTESIAN_POINT('Ctrl Pts',(0.194147465407783,2.35723167382755,8.95557218908974));
#45427=CARTESIAN_POINT('Ctrl Pts',(0.195018847812145,2.35657210730539,8.95550478327031));
#45428=CARTESIAN_POINT('Ctrl Pts',(0.195535395207684,2.35617866121166,8.95546467227329));
#45429=CARTESIAN_POINT('Ctrl Pts',(0.196959371378606,2.35508722482703,8.95535367046186));
#45430=CARTESIAN_POINT('Ctrl Pts',(0.197864268776542,2.35438596134803,8.95528265029677));
#45431=CARTESIAN_POINT('Ctrl Pts',(0.205501478352194,2.3484019908619,8.9546791204128));
#45432=CARTESIAN_POINT('Ctrl Pts',(0.212024090459961,2.34285833187865,8.9541361913825));
#45433=CARTESIAN_POINT('Ctrl Pts',(0.224168486834585,2.33167417619807,8.95306947637679));
#45434=CARTESIAN_POINT('Ctrl Pts',(0.229817181758235,2.32607185168192,8.95254742044238));
#45435=CARTESIAN_POINT('Ctrl Pts',(0.257242519874192,2.29678062415542,8.94988183748435));
#45436=CARTESIAN_POINT('Ctrl Pts',(0.27559034740127,2.27013588003509,8.94763543925744));
#45437=CARTESIAN_POINT('Ctrl Pts',(0.290345347851738,2.23986781376392,8.94550570342855));
#45438=CARTESIAN_POINT('Ctrl Pts',(0.290993322765,2.23851466586678,8.94541134559361));
#45439=CARTESIAN_POINT('Ctrl Pts',(0.29181335448455,2.2367710629973,8.94529089941957));
#45440=CARTESIAN_POINT('Ctrl Pts',(0.291994104369485,2.23638475188741,8.94526428490244));
#45441=CARTESIAN_POINT('Ctrl Pts',(0.292279054024963,2.23577257482244,8.94522222390675));
#45442=CARTESIAN_POINT('Ctrl Pts',(0.292383759300813,2.23554694682571,8.94520674616891));
#45443=CARTESIAN_POINT('Ctrl Pts',(0.292570783243073,2.23514270640986,8.94517906011033));
#45444=CARTESIAN_POINT('Ctrl Pts',(0.292653199038719,2.23496414114858,8.94516684579498));
#45445=CARTESIAN_POINT('Ctrl Pts',(0.292846420927111,2.23454448994531,8.94513817678665));
#45446=CARTESIAN_POINT('Ctrl Pts',(0.292957092615639,2.23430334289164,8.94512173051664));
#45447=CARTESIAN_POINT('Ctrl Pts',(0.29327652698835,2.23360504075043,8.94507418640213));
#45448=CARTESIAN_POINT('Ctrl Pts',(0.293484519488421,2.23314753105111,8.94504313608902));
#45449=CARTESIAN_POINT('Ctrl Pts',(0.294900120369972,2.23001427814458,8.94483115481095));
#45450=CARTESIAN_POINT('Ctrl Pts',(0.296072239614899,2.22732251925763,8.94465236412164));
#45451=CARTESIAN_POINT('Ctrl Pts',(0.299634455832136,2.21882661437801,8.94409727093751));
#45452=CARTESIAN_POINT('Ctrl Pts',(0.301891998853246,2.21296815128478,8.94372783939342));
#45453=CARTESIAN_POINT('Ctrl Pts',(0.30909005691855,2.19252813083278,8.9424723225053));
#45454=CARTESIAN_POINT('Ctrl Pts',(0.313156549867154,2.17766052067162,8.94161596071431));
#45455=CARTESIAN_POINT('Ctrl Pts',(0.321121207420197,2.1374103291937,8.93932219374339));
#45456=CARTESIAN_POINT('Ctrl Pts',(0.323078537173186,2.11176271215937,8.93787820700149));
#45457=CARTESIAN_POINT('Ctrl Pts',(0.321912382753885,2.08464123871511,8.9362318284216));
#45458=CARTESIAN_POINT('Ctrl Pts',(0.321836576388005,2.08312719066163,8.93613956100835));
#45459=CARTESIAN_POINT('Ctrl Pts',(0.32171891920722,2.08106824899228,8.93601358131835));
#45460=CARTESIAN_POINT('Ctrl Pts',(0.32168635952416,2.08052282714623,8.93598016047328));
#45461=CARTESIAN_POINT('Ctrl Pts',(0.321628747941538,2.07959732341589,8.93592336706059));
#45462=CARTESIAN_POINT('Ctrl Pts',(0.321604408881728,2.07921719701158,8.93590001689319));
#45463=CARTESIAN_POINT('Ctrl Pts',(0.321554098679207,2.0784527112016,8.93585300837592));
#45464=CARTESIAN_POINT('Ctrl Pts',(0.32152811215982,2.07806835343854,8.93582934957913));
#45465=CARTESIAN_POINT('Ctrl Pts',(0.321467676195962,2.07719766478742,8.93577569921355));
#45466=CARTESIAN_POINT('Ctrl Pts',(0.321432812234558,2.0767113644711,8.93574569467723));
#45467=CARTESIAN_POINT('Ctrl Pts',(0.321357647312751,2.07569525854642,8.93568291799324));
#45468=CARTESIAN_POINT('Ctrl Pts',(0.321317139388195,2.07516547013787,8.93565013941998));
#45469=CARTESIAN_POINT('Ctrl Pts',(0.321207777936866,2.07378024540166,8.93556430904741));
#45470=CARTESIAN_POINT('Ctrl Pts',(0.321136817598861,2.07292498387878,8.93551119112973));
#45471=CARTESIAN_POINT('Ctrl Pts',(0.320916543076602,2.07039287026271,8.93535355403983));
#45472=CARTESIAN_POINT('Ctrl Pts',(0.320757506625762,2.06871691317103,8.93524873011148));
#45473=CARTESIAN_POINT('Ctrl Pts',(0.319707721563203,2.05850546777471,8.93460701214871));
#45474=CARTESIAN_POINT('Ctrl Pts',(0.318489532873857,2.05000781531759,8.93405990624707));
#45475=CARTESIAN_POINT('Ctrl Pts',(0.314312099914136,2.02734893471528,8.93256479503429));
#45476=CARTESIAN_POINT('Ctrl Pts',(0.310736520749154,2.01332237691127,8.93159992639516));
#45477=CARTESIAN_POINT('Ctrl Pts',(0.29854148451261,1.97613180143265,8.92895885542711));
#45478=CARTESIAN_POINT('Ctrl Pts',(0.28818190441021,1.95363830269271,8.927266313279));
#45479=CARTESIAN_POINT('Ctrl Pts',(0.274629641904422,1.93135336991565,8.92561821836771));
#45480=CARTESIAN_POINT('Ctrl Pts',(0.273896219253183,1.93016482314203,8.92553043246503));
#45481=CARTESIAN_POINT('Ctrl Pts',(0.27293491263177,1.92862940385282,8.9254172130759));
#45482=CARTESIAN_POINT('Ctrl Pts',(0.27271406713878,1.92827817451944,8.92539132672099));
#45483=CARTESIAN_POINT('Ctrl Pts',(0.272374237248879,1.92774002321153,8.92535168458257));
#45484=CARTESIAN_POINT('Ctrl Pts',(0.27225573836794,1.92755279751037,8.92533789673751));
#45485=CARTESIAN_POINT('Ctrl Pts',(0.272020310035568,1.92718167329858,8.92531057398072));
#45486=CARTESIAN_POINT('Ctrl Pts',(0.271903387869235,1.92699777232215,8.92529703879343));
#45487=CARTESIAN_POINT('Ctrl Pts',(0.27164265878354,1.92658860193306,8.92526693226882));
#45488=CARTESIAN_POINT('Ctrl Pts',(0.271498758520322,1.92636339333629,8.92525036730849));
#45489=CARTESIAN_POINT('Ctrl Pts',(0.27107853923966,1.92570753602694,8.92520214247647));
#45490=CARTESIAN_POINT('Ctrl Pts',(0.27080147294032,1.92527736352725,8.92517053226548));
#45491=CARTESIAN_POINT('Ctrl Pts',(0.268816034559599,1.92221084392562,8.92494532654881));
#45492=CARTESIAN_POINT('Ctrl Pts',(0.267070144493558,1.91959882440127,8.92475418797184));
#45493=CARTESIAN_POINT('Ctrl Pts',(0.263025817735089,1.91373555439769,8.92432569909603));
#45494=CARTESIAN_POINT('Ctrl Pts',(0.260704740675812,1.91050048654899,8.92408968293203));
#45495=CARTESIAN_POINT('Ctrl Pts',(0.25509024589099,1.9029736130099,8.92353939919904));
#45496=CARTESIAN_POINT('Ctrl Pts',(0.251747501057024,1.89872001686354,8.92322749953457));
#45497=CARTESIAN_POINT('Ctrl Pts',(0.245814024755871,1.89154895709316,8.92269629141062));
#45498=CARTESIAN_POINT('Ctrl Pts',(0.243274575785754,1.88859079007196,8.92247550361953));
#45499=CARTESIAN_POINT('Ctrl Pts',(0.221823240302397,1.86450094371551,8.92065713405116));
#45500=CARTESIAN_POINT('Ctrl Pts',(0.200253500314111,1.8459058574269,8.91910789502148));
#45501=CARTESIAN_POINT('Ctrl Pts',(0.175953758339042,1.82999643846547,8.91739023868974));
#45502=CARTESIAN_POINT('Ctrl Pts',(0.17537734985347,1.8296216845545,8.91734951742613));
#45503=CARTESIAN_POINT('Ctrl Pts',(0.170118742585208,1.82622667405693,8.9169782062856));
#45504=CARTESIAN_POINT('Ctrl Pts',(0.165360386692497,1.82332662342835,8.91664357027405));
#45505=CARTESIAN_POINT('Ctrl Pts',(0.159685325519364,1.82006657907711,8.91624509712742));
#45506=CARTESIAN_POINT('Ctrl Pts',(0.158839002724313,1.81958549517413,8.91618568965848));
#45507=CARTESIAN_POINT('Ctrl Pts',(0.157556297828978,1.81886402428992,8.91609567093746));
#45508=CARTESIAN_POINT('Ctrl Pts',(0.157121511452811,1.81862079952774,8.91606516168915));
#45509=CARTESIAN_POINT('Ctrl Pts',(0.156357822821913,1.81819590484193,8.91601157864527));
#45510=CARTESIAN_POINT('Ctrl Pts',(0.156029162759445,1.8180137996778,8.91598852049458));
#45511=CARTESIAN_POINT('Ctrl Pts',(0.155329273446141,1.81762760067327,8.91593942104365));
#45512=CARTESIAN_POINT('Ctrl Pts',(0.15495795903092,1.8174236633738,8.91591337420449));
#45513=CARTESIAN_POINT('Ctrl Pts',(0.153991795727045,1.81689549377225,8.91584560480206));
#45514=CARTESIAN_POINT('Ctrl Pts',(0.153396326906438,1.81657240522823,8.91580384156326));
#45515=CARTESIAN_POINT('Ctrl Pts',(0.152096863839651,1.81587263924744,8.91571271172374));
#45516=CARTESIAN_POINT('Ctrl Pts',(0.151392481053797,1.81549669636357,8.91566331931151));
#45517=CARTESIAN_POINT('Ctrl Pts',(0.14933858460968,1.81441027901373,8.9155193078939));
#45518=CARTESIAN_POINT('Ctrl Pts',(0.14798542980885,1.81370676916525,8.9154244434577));
#45519=CARTESIAN_POINT('Ctrl Pts',(0.14336626766393,1.81134674842189,8.91510063054031));
#45520=CARTESIAN_POINT('Ctrl Pts',(0.140077135829765,1.8097363601954,8.91487008302287));
#45521=CARTESIAN_POINT('Ctrl Pts',(0.125637366351748,1.80296910910093,8.91385775288157));
#45522=CARTESIAN_POINT('Ctrl Pts',(0.114225613111398,1.79839670557855,8.91305666183672));
#45523=CARTESIAN_POINT('Ctrl Pts',(0.072302779921104,1.78432030579174,8.91011735455033));
#45524=CARTESIAN_POINT('Ctrl Pts',(0.0406825312678802,1.77871160054212,
8.90788832038193));
#45525=CARTESIAN_POINT('Ctrl Pts',(0.00722131733163397,1.77780226300678,
8.90577055369863));
#45526=CARTESIAN_POINT('Ctrl Pts',(0.00568744959775808,1.77777153712539,
8.90567404666536));
#45527=CARTESIAN_POINT('Ctrl Pts',(0.00372831739244894,1.77774628630985,
8.90555156317903));
#45528=CARTESIAN_POINT('Ctrl Pts',(0.00330323623296926,1.77774164871489,
8.90552503431747));
#45529=CARTESIAN_POINT('Ctrl Pts',(0.00262725833906431,1.77773561151226,
8.90548292316825));
#45530=CARTESIAN_POINT('Ctrl Pts',(0.00237636887303145,1.77773366380311,
8.9054673102258));
#45531=CARTESIAN_POINT('Ctrl Pts',(0.00190721407715574,1.77773056955404,
8.90543814596918));
#45532=CARTESIAN_POINT('Ctrl Pts',(0.00168895151087381,1.77772935177291,
8.90542459077929));
#45533=CARTESIAN_POINT('Ctrl Pts',(0.00119796797696843,1.77772711117085,
8.90539412680842));
#45534=CARTESIAN_POINT('Ctrl Pts',(0.000925247483336966,1.7777262127942,
8.90537722514122));
#45535=CARTESIAN_POINT('Ctrl Pts',(0.000114630137799438,1.77772457149672,
8.90532704559099));
#45536=CARTESIAN_POINT('Ctrl Pts',(-0.000423271175453538,1.77772482905374,
8.90529382373696));
#45537=CARTESIAN_POINT('Ctrl Pts',(-0.00480631989839939,1.77773790140136,
8.90502371724979));
#45538=CARTESIAN_POINT('Ctrl Pts',(-0.00865116152121387,1.77781818563893,
8.90479053599131));
#45539=CARTESIAN_POINT('Ctrl Pts',(-0.0213767894154967,1.77831189967048,
8.90402849727908));
#45540=CARTESIAN_POINT('Ctrl Pts',(-0.030242428481046,1.77902395309238,
8.90351328953682));
#45541=CARTESIAN_POINT('Ctrl Pts',(-0.0474653381832505,1.78112732140132,
8.90252396081068));
#45542=CARTESIAN_POINT('Ctrl Pts',(-0.0558193649145247,1.78248314833279,
8.90204943872156));
#45543=CARTESIAN_POINT('Ctrl Pts',(-0.0664106658111328,1.78463305907576,
8.90144486087313));
#45544=CARTESIAN_POINT('Ctrl Pts',(-0.0687055765129701,1.78512506014655,
8.90131368657694));
#45545=CARTESIAN_POINT('Ctrl Pts',(-0.0787911153721566,1.78740278848947,
8.90073577129273));
#45546=CARTESIAN_POINT('Ctrl Pts',(-0.0865190162529853,1.78945288146303,
8.90028908001325));
#45547=CARTESIAN_POINT('Ctrl Pts',(-0.11228109147801,1.79732351716305,8.89876881473115));
#45548=CARTESIAN_POINT('Ctrl Pts',(-0.129873411024156,1.80444487324056,
8.89767549261018));
#45549=CARTESIAN_POINT('Ctrl Pts',(-0.14788611527399,1.81365660823182,8.89644663602256));
#45550=CARTESIAN_POINT('Ctrl Pts',(-0.149031561792272,1.81425109866493,
8.89636801047566));
#45551=CARTESIAN_POINT('Ctrl Pts',(-0.150624858377512,1.81509021074049,
8.89625795906056));
#45552=CARTESIAN_POINT('Ctrl Pts',(-0.151075755514668,1.81532904597046,
8.89622673797687));
#45553=CARTESIAN_POINT('Ctrl Pts',(-0.151853660469536,1.81574346236267,
8.8961727403337));
#45554=CARTESIAN_POINT('Ctrl Pts',(-0.152180936607668,1.81591853999442,
8.8961499816763));
#45555=CARTESIAN_POINT('Ctrl Pts',(-0.152850934218001,1.81627844785031,
8.89610330576918));
#45556=CARTESIAN_POINT('Ctrl Pts',(-0.153193624537801,1.81646333456774,
8.8960793865355));
#45557=CARTESIAN_POINT('Ctrl Pts',(-0.153990038869609,1.81689487772322,
8.89602369184627));
#45558=CARTESIAN_POINT('Ctrl Pts',(-0.154443505787119,1.81714200409809,
8.8959918996666));
#45559=CARTESIAN_POINT('Ctrl Pts',(-0.155869902550256,1.81792380183361,
8.89589164128323));
#45560=CARTESIAN_POINT('Ctrl Pts',(-0.156840656921119,1.81846240680832,
8.89582303449112));
#45561=CARTESIAN_POINT('Ctrl Pts',(-0.159083827480577,1.81972219035738,
8.89566362230592));
#45562=CARTESIAN_POINT('Ctrl Pts',(-0.160354148208884,1.82044703224143,
8.8955726859007));
#45563=CARTESIAN_POINT('Ctrl Pts',(-0.164613953556208,1.82291625504607,
8.89526549019098));
#45564=CARTESIAN_POINT('Ctrl Pts',(-0.167580177155531,1.82470009417534,
8.89504781023066));
#45565=CARTESIAN_POINT('Ctrl Pts',(-0.178644464480926,1.8315990525726,8.89422126627417));
#45566=CARTESIAN_POINT('Ctrl Pts',(-0.18654123790089,1.83702614128944,8.89360122173697));
#45567=CARTESIAN_POINT('Ctrl Pts',(-0.207516830895129,1.85286233179443,
8.89187054301329));
#45568=CARTESIAN_POINT('Ctrl Pts',(-0.220045777198337,1.86394908401373,
8.89073961128161));
#45569=CARTESIAN_POINT('Ctrl Pts',(-0.24468775366206,1.88942847297504,8.88834181451892));
#45570=CARTESIAN_POINT('Ctrl Pts',(-0.256519209425027,1.9040139292652,8.88707967750188));
#45571=CARTESIAN_POINT('Ctrl Pts',(-0.267638122912724,1.92046659675861,
8.88582830665293));
#45572=CARTESIAN_POINT('Ctrl Pts',(-0.268254903786033,1.9213894896829,8.88575865488878));
#45573=CARTESIAN_POINT('Ctrl Pts',(-0.269075854877119,1.92263172898813,
8.88566564675022));
#45574=CARTESIAN_POINT('Ctrl Pts',(-0.269284238550323,1.92294826148417,
8.88564201204997));
#45575=CARTESIAN_POINT('Ctrl Pts',(-0.269609604586752,1.92344439210727,
8.88560506902315));
#45576=CARTESIAN_POINT('Ctrl Pts',(-0.269726966085424,1.92362373932187,
8.88559173519679));
#45577=CARTESIAN_POINT('Ctrl Pts',(-0.269951952671543,1.92396830469015,
8.88556615806725));
#45578=CARTESIAN_POINT('Ctrl Pts',(-0.270059604253384,1.92413350331689,
8.88555391303651));
#45579=CARTESIAN_POINT('Ctrl Pts',(-0.270314401075191,1.92452529187905,
8.88552491421587));
#45580=CARTESIAN_POINT('Ctrl Pts',(-0.270461412871649,1.92475196786405,
8.88550816947602));
#45581=CARTESIAN_POINT('Ctrl Pts',(-0.270893583714525,1.92542016673176,
8.88545890543826));
#45582=CARTESIAN_POINT('Ctrl Pts',(-0.271177949625862,1.92586220534413,
8.88542643913957));
#45583=CARTESIAN_POINT('Ctrl Pts',(-0.273343522524734,1.92924669479738,
8.88517878765719));
#45584=CARTESIAN_POINT('Ctrl Pts',(-0.275177960780942,1.93221899730117,
8.88496664930818));
#45585=CARTESIAN_POINT('Ctrl Pts',(-0.281372607860134,1.94263106254193,
8.88423977736053));
#45586=CARTESIAN_POINT('Ctrl Pts',(-0.285482604409545,1.95021604135559,
8.88373851046058));
#45587=CARTESIAN_POINT('Ctrl Pts',(-0.303220245512051,1.98634047410008,
8.88143807042266));
#45588=CARTESIAN_POINT('Ctrl Pts',(-0.312903755503468,2.01661899418232,
8.87973653620455));
#45589=CARTESIAN_POINT('Ctrl Pts',(-0.318382667603507,2.05001422405198,
8.87774438373441));
#45590=CARTESIAN_POINT('Ctrl Pts',(-0.318719327775165,2.05220783965774,
8.87761311441661));
#45591=CARTESIAN_POINT('Ctrl Pts',(-0.319758522969623,2.05947915970704,
8.87717642298226));
#45592=CARTESIAN_POINT('Ctrl Pts',(-0.320362541585604,2.06456994318815,
8.87686815458609));
#45593=CARTESIAN_POINT('Ctrl Pts',(-0.32092617521019,2.07053286432804,8.87650341668156));
#45594=CARTESIAN_POINT('Ctrl Pts',(-0.321004015653553,2.07139328870271,
8.87645069831059));
#45595=CARTESIAN_POINT('Ctrl Pts',(-0.321122870811927,2.07276868825779,
8.87636628270478));
#45596=CARTESIAN_POINT('Ctrl Pts',(-0.321166109015685,2.07328347117399,
8.87633465538975));
#45597=CARTESIAN_POINT('Ctrl Pts',(-0.321240332758155,2.0741933860506,8.87627869393556));
#45598=CARTESIAN_POINT('Ctrl Pts',(-0.321271827549024,2.07458847633085,
8.87625437584876));
#45599=CARTESIAN_POINT('Ctrl Pts',(-0.321331007833172,2.07534856953882,
8.87620755406841));
#45600=CARTESIAN_POINT('Ctrl Pts',(-0.32135880045428,2.07571356370952,8.87618505378024));
#45601=CARTESIAN_POINT('Ctrl Pts',(-0.321416849642537,2.07649345942085,
8.87613694078914));
#45602=CARTESIAN_POINT('Ctrl Pts',(-0.321446924801162,2.07690837343497,
8.87611132242547));
#45603=CARTESIAN_POINT('Ctrl Pts',(-0.321517156069859,2.07790400877492,
8.87604979563889));
#45604=CARTESIAN_POINT('Ctrl Pts',(-0.321556542209109,2.07848478141234,
8.8760138630883));
#45605=CARTESIAN_POINT('Ctrl Pts',(-0.32165802359338,2.08004374299165,8.87591729333295));
#45606=CARTESIAN_POINT('Ctrl Pts',(-0.321717229749107,2.08102210801356,
8.87585656561722));
#45607=CARTESIAN_POINT('Ctrl Pts',(-0.322110117426355,2.08804573548621,
8.87541970523543));
#45608=CARTESIAN_POINT('Ctrl Pts',(-0.322277825444617,2.09409865735488,
8.8750384054719));
#45609=CARTESIAN_POINT('Ctrl Pts',(-0.322274963997748,2.10015233269624,
8.8746519335206));
#45610=CARTESIAN_POINT('',(-0.322274890249976,2.09973403126875,8.62424191572231));
#45611=CARTESIAN_POINT('Ctrl Pts',(-0.322274964147435,2.10015201568935,
8.87465195375859));
#45612=CARTESIAN_POINT('Ctrl Pts',(-0.322258391129396,2.1352869995652,8.87240890655654));
#45613=CARTESIAN_POINT('Ctrl Pts',(-0.316495278814541,2.17018327590654,
8.86997185423784));
#45614=CARTESIAN_POINT('Ctrl Pts',(-0.303201477941531,2.20940561370631,
8.86723288440724));
#45615=CARTESIAN_POINT('Ctrl Pts',(-0.301008738192233,2.21530167007367,
8.86682227231232));
#45616=CARTESIAN_POINT('Ctrl Pts',(-0.297538892961549,2.22385652456047,
8.86623183913865));
#45617=CARTESIAN_POINT('Ctrl Pts',(-0.296395750444973,2.22656773728122,
8.86604552801538));
#45618=CARTESIAN_POINT('Ctrl Pts',(-0.295013894593567,2.22972366974637,
8.86582993012531));
#45619=CARTESIAN_POINT('Ctrl Pts',(-0.294811119235905,2.23018384108156,
8.8657985254511));
#45620=CARTESIAN_POINT('Ctrl Pts',(-0.29449968156297,2.23088614753796,8.86575064715497));
#45621=CARTESIAN_POINT('Ctrl Pts',(-0.294391797015212,2.23112862353198,
8.86573412616783));
#45622=CARTESIAN_POINT('Ctrl Pts',(-0.294203441482384,2.23155055805761,
8.86570539444121));
#45623=CARTESIAN_POINT('Ctrl Pts',(-0.294123105971324,2.23173007568437,
8.86569317539954));
#45624=CARTESIAN_POINT('Ctrl Pts',(-0.293953866619167,2.23210733109096,
8.86566750822513));
#45625=CARTESIAN_POINT('Ctrl Pts',(-0.293864927857752,2.23230505207344,
8.86565406233586));
#45626=CARTESIAN_POINT('Ctrl Pts',(-0.293614936321597,2.23285931602285,
8.86561638744191));
#45627=CARTESIAN_POINT('Ctrl Pts',(-0.293453433029836,2.23321565723309,
8.86559218621455));
#45628=CARTESIAN_POINT('Ctrl Pts',(-0.292792392733212,2.23466714243999,
8.8654936866138));
#45629=CARTESIAN_POINT('Ctrl Pts',(-0.292287362768263,2.23575979584757,
8.86541972206155));
#45630=CARTESIAN_POINT('Ctrl Pts',(-0.283205356135972,2.2551234858498,8.86411178006015));
#45631=CARTESIAN_POINT('Ctrl Pts',(-0.27293520880172,2.27255494296648,8.8629778907046));
#45632=CARTESIAN_POINT('Ctrl Pts',(-0.251610402689442,2.30202832183549,
8.86094267409749));
#45633=CARTESIAN_POINT('Ctrl Pts',(-0.241146535991518,2.31440978391395,
8.8600426420395));
#45634=CARTESIAN_POINT('Ctrl Pts',(-0.223920133129191,2.33192933691747,
8.85863237868484));
#45635=CARTESIAN_POINT('Ctrl Pts',(-0.217812387476607,2.33767454884246,
8.85814427240509));
#45636=CARTESIAN_POINT('Ctrl Pts',(-0.208804240202796,2.34550888985677,
8.85743515123233));
#45637=CARTESIAN_POINT('Ctrl Pts',(-0.206082137876216,2.34779825803244,
8.85722220078001));
#45638=CARTESIAN_POINT('Ctrl Pts',(-0.202164859817855,2.35098360985124,
8.85691731034613));
#45639=CARTESIAN_POINT('Ctrl Pts',(-0.201000427174315,2.35191711160528,
8.8568268713154));
#45640=CARTESIAN_POINT('Ctrl Pts',(-0.198944692864906,2.35354182473953,
8.8566675173254));
#45641=CARTESIAN_POINT('Ctrl Pts',(-0.198056162076588,2.35423651257091,
8.85659874174787));
#45642=CARTESIAN_POINT('Ctrl Pts',(-0.196752533285843,2.35524475873978,
8.85649797472096));
#45643=CARTESIAN_POINT('Ctrl Pts',(-0.196340286842383,2.35556200417152,
8.85646612928448));
#45644=CARTESIAN_POINT('Ctrl Pts',(-0.195617632044584,2.35611534462456,
8.85641033955645));
#45645=CARTESIAN_POINT('Ctrl Pts',(-0.195307559037038,2.35635187750379,
8.85638641258563));
#45646=CARTESIAN_POINT('Ctrl Pts',(-0.194702369016668,2.35681179903014,
8.85633973376936));
#45647=CARTESIAN_POINT('Ctrl Pts',(-0.194407294873696,2.35703524334207,
8.85631698416082));
#45648=CARTESIAN_POINT('Ctrl Pts',(-0.193707701939626,2.35756311487901,
8.85626306957427));
#45649=CARTESIAN_POINT('Ctrl Pts',(-0.193302850334388,2.35786709752282,
8.85623188724451));
#45650=CARTESIAN_POINT('Ctrl Pts',(-0.191882133025795,2.35892861660629,
8.85612252226931));
#45651=CARTESIAN_POINT('Ctrl Pts',(-0.190862527056998,2.35968110667515,
8.85604414314863));
#45652=CARTESIAN_POINT('Ctrl Pts',(-0.176489233984687,2.37015851064257,
8.85494068431225));
#45653=CARTESIAN_POINT('Ctrl Pts',(-0.162413757944563,2.37884706693344,
8.85387552979629));
#45654=CARTESIAN_POINT('Ctrl Pts',(-0.140168012870308,2.39032158777346,
8.85221547139683));
#45655=CARTESIAN_POINT('Ctrl Pts',(-0.132448189165778,2.39392373387985,
8.85164371513995));
#45656=CARTESIAN_POINT('Ctrl Pts',(-0.109471094890872,2.40355590560844,
8.84996179006769));
#45657=CARTESIAN_POINT('Ctrl Pts',(-0.0938848563783912,2.40873252822349,
8.84884450845167));
#45658=CARTESIAN_POINT('Ctrl Pts',(-0.0719279392973073,2.41420749284543,
8.84734844953099));
#45659=CARTESIAN_POINT('Ctrl Pts',(-0.0658410652126833,2.4155391290063,
8.84694188310539));
#45660=CARTESIAN_POINT('Ctrl Pts',(-0.0568570630955382,2.41723324549202,
8.84635729458988));
#45661=CARTESIAN_POINT('Ctrl Pts',(-0.0539877986153758,2.41773412899398,
8.84617288876034));
#45662=CARTESIAN_POINT('Ctrl Pts',(-0.050616877067789,2.41827560206698,
8.84595923930876));
#45663=CARTESIAN_POINT('Ctrl Pts',(-0.0501215473080758,2.4183539816285,
8.84592792090021));
#45664=CARTESIAN_POINT('Ctrl Pts',(-0.0493640942356354,2.41847202719149,
8.84588014683649));
#45665=CARTESIAN_POINT('Ctrl Pts',(-0.0491021044189213,2.41851252604255,
8.8458636441319));
#45666=CARTESIAN_POINT('Ctrl Pts',(-0.048645689122768,2.41858250301045,
8.84583493240884));
#45667=CARTESIAN_POINT('Ctrl Pts',(-0.0484512872049761,2.41861212635975,
8.84582271512735));
#45668=CARTESIAN_POINT('Ctrl Pts',(-0.0480107533808782,2.41867884325877,
8.84579505670633));
#45669=CARTESIAN_POINT('Ctrl Pts',(-0.0477646060570305,2.41871582952556,
8.84577962176556));
#45670=CARTESIAN_POINT('Ctrl Pts',(-0.0470958140158975,2.41881553049978,
8.84573773580946));
#45671=CARTESIAN_POINT('Ctrl Pts',(-0.0466730851405237,2.41887769021074,
8.8457113163409));
#45672=CARTESIAN_POINT('Ctrl Pts',(-0.0447585058983298,2.41915532866074,
8.84559190724501));
#45673=CARTESIAN_POINT('Ctrl Pts',(-0.0432652473613167,2.41936118461947,
8.84549945443645));
#45674=CARTESIAN_POINT('Ctrl Pts',(-0.010703100775816,2.42361751806054,
8.84349712853597));
#45675=CARTESIAN_POINT('Ctrl Pts',(0.0207963479565396,2.42312711933527,
8.84181961176984));
#45676=CARTESIAN_POINT('Ctrl Pts',(0.0627563563993194,2.416302898963,8.83941420827099));
#45677=CARTESIAN_POINT('Ctrl Pts',(0.07367735903237,2.41393868726541,8.83877345348209));
#45678=CARTESIAN_POINT('Ctrl Pts',(0.0890711320598588,2.40975862927589,
8.83783402705313));
#45679=CARTESIAN_POINT('Ctrl Pts',(0.0936605350674244,2.40840197086546,
8.83754928513161));
#45680=CARTESIAN_POINT('Ctrl Pts',(0.099988903899937,2.40637697769911,8.83714933946639));
#45681=CARTESIAN_POINT('Ctrl Pts',(0.101754976879823,2.40579496043265,8.83703692652034));
#45682=CARTESIAN_POINT('Ctrl Pts',(0.104390170740409,2.40490116461715,8.83686795344129));
#45683=CARTESIAN_POINT('Ctrl Pts',(0.105263169643407,2.4046008749513,8.83681177057736));
#45684=CARTESIAN_POINT('Ctrl Pts',(0.106662195909936,2.40411291242285,8.83672140087538));
#45685=CARTESIAN_POINT('Ctrl Pts',(0.107189050990016,2.40392761454058,8.83668729261168));
#45686=CARTESIAN_POINT('Ctrl Pts',(0.108188962679898,2.40357301662697,8.83662241290063));
#45687=CARTESIAN_POINT('Ctrl Pts',(0.108662110704774,2.40340397782893,8.83659165019409));
#45688=CARTESIAN_POINT('Ctrl Pts',(0.109500333444407,2.40310229869367,8.83653704010925));
#45689=CARTESIAN_POINT('Ctrl Pts',(0.10986556812357,2.40297010320586,8.83651320758313));
#45690=CARTESIAN_POINT('Ctrl Pts',(0.110580971958508,2.40270970139934,8.83646645159755));
#45691=CARTESIAN_POINT('Ctrl Pts',(0.110931159470307,2.40258154692136,8.83644352989701));
#45692=CARTESIAN_POINT('Ctrl Pts',(0.111766189101242,2.40227431538224,8.83638878909601));
#45693=CARTESIAN_POINT('Ctrl Pts',(0.11225082326147,2.40209467959262,8.8363569513661));
#45694=CARTESIAN_POINT('Ctrl Pts',(0.113980941618331,2.40144865123023,8.83624305026901));
#45695=CARTESIAN_POINT('Ctrl Pts',(0.115223955262968,2.40097572066402,8.83616076829903));
#45696=CARTESIAN_POINT('Ctrl Pts',(0.13754296612354,2.39232545996975,8.83467513619296));
#45697=CARTESIAN_POINT('Ctrl Pts',(0.15769937683074,2.38196234921396,8.83319439165369));
#45698=CARTESIAN_POINT('Ctrl Pts',(0.189249583749443,2.36129362961791,8.83065656739356));
#45699=CARTESIAN_POINT('Ctrl Pts',(0.201297763568959,2.35212888610402,8.82962637665499));
#45700=CARTESIAN_POINT('Ctrl Pts',(0.221198742087984,2.33465185199917,8.82785376456689));
#45701=CARTESIAN_POINT('Ctrl Pts',(0.229337661131533,2.3267039288392,8.82710492717565));
#45702=CARTESIAN_POINT('Ctrl Pts',(0.238098718966128,2.31719257869832,8.82628681525841));
#45703=CARTESIAN_POINT('Ctrl Pts',(0.239148793768166,2.31603580927408,8.82618855201648));
#45704=CARTESIAN_POINT('Ctrl Pts',(0.240466090493364,2.3145632910722,8.82606507154993));
#45705=CARTESIAN_POINT('Ctrl Pts',(0.240741149469571,2.31425462774352,8.82603927634103));
#45706=CARTESIAN_POINT('Ctrl Pts',(0.241178805207112,2.31376159610902,8.82599821509051));
#45707=CARTESIAN_POINT('Ctrl Pts',(0.241341785143525,2.31357757091257,8.82598292025497));
#45708=CARTESIAN_POINT('Ctrl Pts',(0.241649577653699,2.31322923161248,8.82595402839717));
#45709=CARTESIAN_POINT('Ctrl Pts',(0.241794432083298,2.31306495771965,8.8259404282607));
#45710=CARTESIAN_POINT('Ctrl Pts',(0.242124456874303,2.31268991917092,8.82590943586624));
#45711=CARTESIAN_POINT('Ctrl Pts',(0.242309519241405,2.31247906066255,8.82589205177167));
#45712=CARTESIAN_POINT('Ctrl Pts',(0.242874056093596,2.31183413538602,8.82583900487923));
#45713=CARTESIAN_POINT('Ctrl Pts',(0.243252643928795,2.31139928872137,8.82580340814456));
#45714=CARTESIAN_POINT('Ctrl Pts',(0.246000278779147,2.30822619621829,8.82554487652267));
#45715=CARTESIAN_POINT('Ctrl Pts',(0.248324314629643,2.30544907736837,8.82532519598492));
#45716=CARTESIAN_POINT('Ctrl Pts',(0.268295082413906,2.28075077150841,8.82342245628961));
#45717=CARTESIAN_POINT('Ctrl Pts',(0.283049220727119,2.25664198318754,8.82190292955994));
#45718=CARTESIAN_POINT('Ctrl Pts',(0.301411122958605,2.2153396298116,8.81935047247661));
#45719=CARTESIAN_POINT('Ctrl Pts',(0.307089414477461,2.19923643556888,8.81836789228067));
#45720=CARTESIAN_POINT('Ctrl Pts',(0.311905691228041,2.18111061368538,8.81723751338018));
#45721=CARTESIAN_POINT('Ctrl Pts',(0.312331101845052,2.17945674622789,8.81713417676748));
#45722=CARTESIAN_POINT('Ctrl Pts',(0.312952698447476,2.17695801616957,8.81697772485113));
#45723=CARTESIAN_POINT('Ctrl Pts',(0.313158655537868,2.17611559733112,8.81692492310101));
#45724=CARTESIAN_POINT('Ctrl Pts',(0.313486194032711,2.17475204431786,8.81683936336113));
#45725=CARTESIAN_POINT('Ctrl Pts',(0.31360988302727,2.17423141680598,8.81680667311262));
#45726=CARTESIAN_POINT('Ctrl Pts',(0.313844429535547,2.17323312180967,8.81674394673153));
#45727=CARTESIAN_POINT('Ctrl Pts',(0.313955494735914,2.17275550426882,8.81671391736054));
#45728=CARTESIAN_POINT('Ctrl Pts',(0.314151873092776,2.17190218831735,8.81666023202597));
#45729=CARTESIAN_POINT('Ctrl Pts',(0.314237603619513,2.17152658611943,8.81663658952335));
#45730=CARTESIAN_POINT('Ctrl Pts',(0.314406494761794,2.17078047660374,8.81658960114287));
#45731=CARTESIAN_POINT('Ctrl Pts',(0.314489674473583,2.17040997418143,8.81656625591905));
#45732=CARTESIAN_POINT('Ctrl Pts',(0.314690014970887,2.16951017183316,8.81650953071797));
#45733=CARTESIAN_POINT('Ctrl Pts',(0.314806495105262,2.1689807229917,8.81647612896315));
#45734=CARTESIAN_POINT('Ctrl Pts',(0.315237647551024,2.16699712503661,8.81635089539432));
#45735=CARTESIAN_POINT('Ctrl Pts',(0.315543580943449,2.16554111383636,8.81625878416259));
#45736=CARTESIAN_POINT('Ctrl Pts',(0.320829598311132,2.13948847596449,8.81460714097402));
#45737=CARTESIAN_POINT('Ctrl Pts',(0.322928907278759,2.11440064866209,8.81295085521546));
#45738=CARTESIAN_POINT('Ctrl Pts',(0.321575294586588,2.07354295150555,8.81019005788158));
#45739=CARTESIAN_POINT('Ctrl Pts',(0.319892513314197,2.05781640879362,8.80911470829689));
#45740=CARTESIAN_POINT('Ctrl Pts',(0.315922015802501,2.03600736377452,8.80764769451655));
#45741=CARTESIAN_POINT('Ctrl Pts',(0.314594957788282,2.02977321384923,8.80723137527691));
#45742=CARTESIAN_POINT('Ctrl Pts',(0.312369426940675,2.0206552222702,8.80663079307427));
#45743=CARTESIAN_POINT('Ctrl Pts',(0.311613989060734,2.01773836817381,8.80643994202002));
#45744=CARTESIAN_POINT('Ctrl Pts',(0.310683984893116,2.01434433315743,8.80621970739463));
#45745=CARTESIAN_POINT('Ctrl Pts',(0.310549095406724,2.01385656681047,8.8061881014509));
#45746=CARTESIAN_POINT('Ctrl Pts',(0.310341533513148,2.01311283756492,8.80613998005061));
#45747=CARTESIAN_POINT('Ctrl Pts',(0.310269692920295,2.01285664640556,8.80612341648813));
#45748=CARTESIAN_POINT('Ctrl Pts',(0.310144180310748,2.01241117793715,8.80609463807247));
#45749=CARTESIAN_POINT('Ctrl Pts',(0.310090652391283,2.01222186131375,8.80608241482701));
#45750=CARTESIAN_POINT('Ctrl Pts',(0.309969205618494,2.01179382793134,8.80605479491235));
#45751=CARTESIAN_POINT('Ctrl Pts',(0.309901184488626,2.01155514104082,8.80603940433732));
#45752=CARTESIAN_POINT('Ctrl Pts',(0.30971620053363,2.01090886373348,8.80599776224506));
#45753=CARTESIAN_POINT('Ctrl Pts',(0.309598708370879,2.01050142339561,8.8059715416524));
#45754=CARTESIAN_POINT('Ctrl Pts',(0.309068163660543,2.00867514278023,8.80585415255439));
#45755=CARTESIAN_POINT('Ctrl Pts',(0.308646150980751,2.00725889252491,8.80576349900202));
#45756=CARTESIAN_POINT('Ctrl Pts',(0.298723920763738,1.97477848725974,8.80369212014311));
#45757=CARTESIAN_POINT('Ctrl Pts',(0.284589220661479,1.94531893942745,8.8019607846075));
#45758=CARTESIAN_POINT('Ctrl Pts',(0.257658652035014,1.90581537589126,8.79924753053001));
#45759=CARTESIAN_POINT('Ctrl Pts',(0.248143700584506,1.89379558218733,8.79835979927943));
#45760=CARTESIAN_POINT('Ctrl Pts',(0.236726227343944,1.88131197069719,8.79733926168038));
#45761=CARTESIAN_POINT('Ctrl Pts',(0.235632236138761,1.88013365418685,8.79724190235935));
#45762=CARTESIAN_POINT('Ctrl Pts',(0.233960342745177,1.87835970074025,8.7970937274901));
#45763=CARTESIAN_POINT('Ctrl Pts',(0.233388871081552,1.87775801686327,8.79704318684502));
#45764=CARTESIAN_POINT('Ctrl Pts',(0.2324559235661,1.87678331373997,8.79696084756931));
#45765=CARTESIAN_POINT('Ctrl Pts',(0.232095856035157,1.87640894688689,8.79692910986779));
#45766=CARTESIAN_POINT('Ctrl Pts',(0.231401749737383,1.87569075891015,8.79686800610749));
#45767=CARTESIAN_POINT('Ctrl Pts',(0.231067845576486,1.87534680915566,8.79683864594794));
#45768=CARTESIAN_POINT('Ctrl Pts',(0.230464917885386,1.87472850848115,8.79678569136082));
#45769=CARTESIAN_POINT('Ctrl Pts',(0.230196168241127,1.87445389076271,8.79676210895446));
#45770=CARTESIAN_POINT('Ctrl Pts',(0.229657245024002,1.87390516688515,8.79671486204584));
#45771=CARTESIAN_POINT('Ctrl Pts',(0.229387070259408,1.87363106275585,8.79669119750977));
#45772=CARTESIAN_POINT('Ctrl Pts',(0.228638518691238,1.87287434059298,8.79662569077882));
#45773=CARTESIAN_POINT('Ctrl Pts',(0.228159107517079,1.87239275267227,8.79658380292305));
#45774=CARTESIAN_POINT('Ctrl Pts',(0.226270216922729,1.87050725028489,8.79641901884803));
#45775=CARTESIAN_POINT('Ctrl Pts',(0.224849296983503,1.86911490607044,8.79629561419394));
#45776=CARTESIAN_POINT('Ctrl Pts',(0.198302798233882,1.84357974910357,8.79399990217424));
#45777=CARTESIAN_POINT('Ctrl Pts',(0.169442811289288,1.82366111070891,8.79162741423922));
#45778=CARTESIAN_POINT('Ctrl Pts',(0.129260022952872,1.804625836683,8.78863726731228));
#45779=CARTESIAN_POINT('Ctrl Pts',(0.120369320674749,1.80089248638821,8.78799554522044));
#45780=CARTESIAN_POINT('Ctrl Pts',(0.106569656358533,1.79581296736276,8.78704195618732));
#45781=CARTESIAN_POINT('Ctrl Pts',(0.101774320886311,1.79417515262052,8.78671817614134));
#45782=CARTESIAN_POINT('Ctrl Pts',(0.0963975791075244,1.7924792555061,8.78636504808064));
#45783=CARTESIAN_POINT('Ctrl Pts',(0.0958526596333032,1.79230897119842,
8.78632937169529));
#45784=CARTESIAN_POINT('Ctrl Pts',(0.095040361381617,1.79205749983083,8.78627635988433));
#45785=CARTESIAN_POINT('Ctrl Pts',(0.09477332859457,1.79197521221416,8.78625896025765));
#45786=CARTESIAN_POINT('Ctrl Pts',(0.0943164914383339,1.79183508564711,
8.7862292402805));
#45787=CARTESIAN_POINT('Ctrl Pts',(0.0941267406500158,1.79177707468323,
8.78621690976533));
#45788=CARTESIAN_POINT('Ctrl Pts',(0.0937356731449697,1.79165791161053,
8.78619152589889));
#45789=CARTESIAN_POINT('Ctrl Pts',(0.0935343506301318,1.79159678155836,
8.78617847387446));
#45790=CARTESIAN_POINT('Ctrl Pts',(0.0930472530323935,1.79144939890752,
8.78614693217058));
#45791=CARTESIAN_POINT('Ctrl Pts',(0.092761417052072,1.79136334592346,8.78612845425707));
#45792=CARTESIAN_POINT('Ctrl Pts',(0.0917028979281487,1.79104627443141,
8.78606014021439));
#45793=CARTESIAN_POINT('Ctrl Pts',(0.0909294595890927,1.79081775690899,
8.78601044942425));
#45794=CARTESIAN_POINT('Ctrl Pts',(0.089729128387491,1.79046800479038,8.78593366876171));
#45795=CARTESIAN_POINT('Ctrl Pts',(0.0893028361319464,1.79034474652656,
8.78590646610379));
#45796=CARTESIAN_POINT('Ctrl Pts',(0.0705567198958229,1.78496642010374,
8.78471306299879));
#45797=CARTESIAN_POINT('Ctrl Pts',(0.0518038871183008,1.78134501789541,
8.78363676641466));
#45798=CARTESIAN_POINT('Ctrl Pts',(0.0163415571590964,1.77771266067331,
8.78164007620568));
#45799=CARTESIAN_POINT('Ctrl Pts',(-0.00026084758930146,1.77729876995707,
8.78072030726044));
#45800=CARTESIAN_POINT('Ctrl Pts',(-0.0234212244586126,1.77850924056617,
8.77939282038124));
#45801=CARTESIAN_POINT('Ctrl Pts',(-0.0300093092717888,1.7790571762351,
8.77901036164657));
#45802=CARTESIAN_POINT('Ctrl Pts',(-0.0443812583346605,1.78069888440511,
8.77816089752917));
#45803=CARTESIAN_POINT('Ctrl Pts',(-0.0521511147974133,1.78187558405598,
8.77769182383107));
#45804=CARTESIAN_POINT('Ctrl Pts',(-0.06084379941978,1.78351905215076,8.7771532245498));
#45805=CARTESIAN_POINT('Ctrl Pts',(-0.0618169696195012,1.7837076976719,
8.77709273178213));
#45806=CARTESIAN_POINT('Ctrl Pts',(-0.0632749158934978,1.78399730091927,
8.77700180710472));
#45807=CARTESIAN_POINT('Ctrl Pts',(-0.0637603611104964,1.78409489216793,
8.77697148273713));
#45808=CARTESIAN_POINT('Ctrl Pts',(-0.0645939163711931,1.78426446516969,
8.77691932695503));
#45809=CARTESIAN_POINT('Ctrl Pts',(-0.0649421367797968,1.78433590502632,
8.77689751290146));
#45810=CARTESIAN_POINT('Ctrl Pts',(-0.0656581858047297,1.78448404249139,
8.77685260305325));
#45811=CARTESIAN_POINT('Ctrl Pts',(-0.066025999823081,1.78456080752189,
8.77682950512842));
#45812=CARTESIAN_POINT('Ctrl Pts',(-0.0669098422248169,1.78474688443507,
8.77677393157729));
#45813=CARTESIAN_POINT('Ctrl Pts',(-0.0674257368630267,1.7848568200593,
8.77674143601491));
#45814=CARTESIAN_POINT('Ctrl Pts',(-0.0690042458680478,1.7851972491294,
8.77664183012726));
#45815=CARTESIAN_POINT('Ctrl Pts',(-0.0700659573848188,1.78543185241864,
8.77657458817877));
#45816=CARTESIAN_POINT('Ctrl Pts',(-0.082566391742672,1.78826046147643,
8.77577994070802));
#45817=CARTESIAN_POINT('Ctrl Pts',(-0.0938551195217636,1.79147138157918,
8.77503265697865));
#45818=CARTESIAN_POINT('Ctrl Pts',(-0.126411536034841,1.80268387264365,
8.77278632326269));
#45819=CARTESIAN_POINT('Ctrl Pts',(-0.1470369931003,1.81232543847618,8.77123987428361));
#45820=CARTESIAN_POINT('Ctrl Pts',(-0.172361167921185,1.82760312257363,
8.76924582197477));
#45821=CARTESIAN_POINT('Ctrl Pts',(-0.178132371198043,1.83134167248001,
8.76878482155745));
#45822=CARTESIAN_POINT('Ctrl Pts',(-0.189014416591842,1.83889593622301,
8.76790812777038));
#45823=CARTESIAN_POINT('Ctrl Pts',(-0.194140493756881,1.8426845090545,8.7674917744631));
#45824=CARTESIAN_POINT('Ctrl Pts',(-0.201523900810356,1.84848777219601,
8.76689082340601));
#45825=CARTESIAN_POINT('Ctrl Pts',(-0.203870408830755,1.85038601531031,
8.76669964554213));
#45826=CARTESIAN_POINT('Ctrl Pts',(-0.206579118315824,1.8526409495547,8.76647907745942));
#45827=CARTESIAN_POINT('Ctrl Pts',(-0.206967469610177,1.85296579489306,
8.76644745725479));
#45828=CARTESIAN_POINT('Ctrl Pts',(-0.207558777567178,1.85346278110653,
8.76639931863389));
#45829=CARTESIAN_POINT('Ctrl Pts',(-0.207762286952613,1.85363425853752,
8.76638275205903));
#45830=CARTESIAN_POINT('Ctrl Pts',(-0.208130462193819,1.85394526439354,
8.76635278350851));
#45831=CARTESIAN_POINT('Ctrl Pts',(-0.208295199655007,1.85408470562236,
8.76633937524737));
#45832=CARTESIAN_POINT('Ctrl Pts',(-0.208628859770835,1.85436770644124,
8.76631222004208));
#45833=CARTESIAN_POINT('Ctrl Pts',(-0.208797773646535,1.85451127421165,
8.76629847382842));
#45834=CARTESIAN_POINT('Ctrl Pts',(-0.209282801073053,1.85492438436248,
8.76625900466414));
#45835=CARTESIAN_POINT('Ctrl Pts',(-0.209598543240732,1.85519436509539,
8.76623331401213));
#45836=CARTESIAN_POINT('Ctrl Pts',(-0.210977006731922,1.85637766568778,
8.76612116226935));
#45837=CARTESIAN_POINT('Ctrl Pts',(-0.212034307586033,1.85729731826864,
8.76603516169694));
#45838=CARTESIAN_POINT('Ctrl Pts',(-0.231625129293555,1.87456338071227,
8.76444131186564));
#45839=CARTESIAN_POINT('Ctrl Pts',(-0.248227157922096,1.89298411282596,
8.76308102414789));
#45840=CARTESIAN_POINT('Ctrl Pts',(-0.270933930250317,1.92488736559119,
8.76089030280159));
#45841=CARTESIAN_POINT('Ctrl Pts',(-0.278505580799067,1.93719880935376,
8.7600782001685));
#45842=CARTESIAN_POINT('Ctrl Pts',(-0.28921599575796,1.95756142340511,8.75874263545194));
#45843=CARTESIAN_POINT('Ctrl Pts',(-0.292901504601842,1.9653028217717,8.75823672268849));
#45844=CARTESIAN_POINT('Ctrl Pts',(-0.297277709638582,1.97552652468542,
8.75756628403663));
#45845=CARTESIAN_POINT('Ctrl Pts',(-0.298253612942771,1.97788339795675,
8.75741158416918));
#45846=CARTESIAN_POINT('Ctrl Pts',(-0.299468108151004,1.9809179149308,8.75721213802128));
#45847=CARTESIAN_POINT('Ctrl Pts',(-0.299732573996378,1.9815851577869,8.75716826657549));
#45848=CARTESIAN_POINT('Ctrl Pts',(-0.300154169411509,1.98265929750893,
8.7570976132096));
#45849=CARTESIAN_POINT('Ctrl Pts',(-0.300312706761918,1.98306564221505,
8.75707087870232));
#45850=CARTESIAN_POINT('Ctrl Pts',(-0.300612479680231,1.98383861635501,
8.757020009813));
#45851=CARTESIAN_POINT('Ctrl Pts',(-0.300753870790224,1.98420518495053,
8.75699588070884));
#45852=CARTESIAN_POINT('Ctrl Pts',(-0.301073868688523,1.98503934689477,
8.7569409597348));
#45853=CARTESIAN_POINT('Ctrl Pts',(-0.301252056825614,1.98550709880833,
8.75691015389584));
#45854=CARTESIAN_POINT('Ctrl Pts',(-0.301777453038312,1.98689600562222,
8.75681865302804));
#45855=CARTESIAN_POINT('Ctrl Pts',(-0.302121528636534,1.9878183321287,8.75675785340166));
#45856=CARTESIAN_POINT('Ctrl Pts',(-0.304456251546629,1.9941654248197,8.75633918238207));
#45857=CARTESIAN_POINT('Ctrl Pts',(-0.306304800668973,1.99964100182158,
8.75597660998167));
#45858=CARTESIAN_POINT('Ctrl Pts',(-0.308349985626768,2.00628321520694,
8.75553474225812));
#45859=CARTESIAN_POINT('Ctrl Pts',(-0.30868877939069,2.00740525495893,8.75546003129757));
#45860=CARTESIAN_POINT('Ctrl Pts',(-0.31783312121401,2.03829811691552,8.75340113488072));
#45861=CARTESIAN_POINT('Ctrl Pts',(-0.322295631438074,2.06918103693808,
8.75127116455808));
#45862=CARTESIAN_POINT('Ctrl Pts',(-0.322269154620022,2.10886972844207,
8.74861283212634));
#45863=CARTESIAN_POINT('Ctrl Pts',(-0.321914745083371,2.11752141763719,
8.74803976958711));
#45864=CARTESIAN_POINT('Ctrl Pts',(-0.320867752131873,2.13038262836019,
8.74720673582359));
#45865=CARTESIAN_POINT('Ctrl Pts',(-0.320439411291253,2.13460934092905,
8.74693603903327));
#45866=CARTESIAN_POINT('Ctrl Pts',(-0.319862068320647,2.139366594609,8.74663575632411));
#45867=CARTESIAN_POINT('Ctrl Pts',(-0.319795165777148,2.13990643403366,
8.74660174514411));
#45868=CARTESIAN_POINT('Ctrl Pts',(-0.319691993869274,2.14072200905505,
8.74655046142097));
#45869=CARTESIAN_POINT('Ctrl Pts',(-0.319656734309688,2.14099786796274,
8.74653313249642));
#45870=CARTESIAN_POINT('Ctrl Pts',(-0.319594863964523,2.14147698850269,
8.74650306537378));
#45871=CARTESIAN_POINT('Ctrl Pts',(-0.319568416312683,2.14168027043694,
8.74649031793341));
#45872=CARTESIAN_POINT('Ctrl Pts',(-0.319512674810286,2.14210553878426,
8.74646367016527));
#45873=CARTESIAN_POINT('Ctrl Pts',(-0.319483343586603,2.14232751979276,
8.74644977204835));
#45874=CARTESIAN_POINT('Ctrl Pts',(-0.319412595040628,2.14285868716626,
8.74641654297014));
#45875=CARTESIAN_POINT('Ctrl Pts',(-0.319370959955131,2.1431678453887,8.74639722439659));
#45876=CARTESIAN_POINT('Ctrl Pts',(-0.319228085787161,2.14421722565805,
8.74633172405359));
#45877=CARTESIAN_POINT('Ctrl Pts',(-0.31912472062933,2.14495716305199,8.74628566186668));
#45878=CARTESIAN_POINT('Ctrl Pts',(-0.318872539392964,2.14671769445226,
8.7461763456104));
#45879=CARTESIAN_POINT('Ctrl Pts',(-0.318721394305429,2.14773795378419,
8.74611321867082));
#45880=CARTESIAN_POINT('Ctrl Pts',(-0.316844044285325,2.16000394046458,
8.74535678435133));
#45881=CARTESIAN_POINT('Ctrl Pts',(-0.314528173850799,2.17115271986926,
8.74469449513376));
#45882=CARTESIAN_POINT('Ctrl Pts',(-0.305079892523304,2.20699078096389,
8.74258112977049));
#45883=CARTESIAN_POINT('Ctrl Pts',(-0.295587837310875,2.23095296272004,
8.74118538011886));
#45884=CARTESIAN_POINT('Ctrl Pts',(-0.282704134124632,2.25473007357149,
8.73962713097325));
#45885=CARTESIAN_POINT('Ctrl Pts',(-0.282049037358633,2.2559210171223,8.73954861721519));
#45886=CARTESIAN_POINT('Ctrl Pts',(-0.279796441977427,2.25995550741794,
8.73928099367464));
#45887=CARTESIAN_POINT('Ctrl Pts',(-0.278163351384818,2.26277887541246,
8.73909090676196));
#45888=CARTESIAN_POINT('Ctrl Pts',(-0.275592896415891,2.26707113606438,
8.73879723565893));
#45889=CARTESIAN_POINT('Ctrl Pts',(-0.274685980246266,2.26855806464664,
8.73869462281087));
#45890=CARTESIAN_POINT('Ctrl Pts',(-0.27347784228096,2.27050321375478,8.73855918582393));
#45891=CARTESIAN_POINT('Ctrl Pts',(-0.273187430528504,2.27096813713506,
8.73852672307088));
#45892=CARTESIAN_POINT('Ctrl Pts',(-0.269880772797685,2.2762318653979,8.73815814483891));
#45893=CARTESIAN_POINT('Ctrl Pts',(-0.266739773217482,2.28095079222971,
8.73781782674773));
#45894=CARTESIAN_POINT('Ctrl Pts',(-0.262912613326235,2.28638425619373,
8.73741320540388));
#45895=CARTESIAN_POINT('Ctrl Pts',(-0.262345467537189,2.287181700047,8.73735349110978));
#45896=CARTESIAN_POINT('Ctrl Pts',(-0.261483480713575,2.28838209634735,
8.73726309797873));
#45897=CARTESIAN_POINT('Ctrl Pts',(-0.261191317148046,2.28878697188191,
8.7372325224252));
#45898=CARTESIAN_POINT('Ctrl Pts',(-0.260667652856102,2.28950911490108,
8.7371778303382));
#45899=CARTESIAN_POINT('Ctrl Pts',(-0.260436510309424,2.28982664189144,
8.73715372770711));
#45900=CARTESIAN_POINT('Ctrl Pts',(-0.259947022103561,2.29049648867263,
8.73710276580063));
#45901=CARTESIAN_POINT('Ctrl Pts',(-0.259688539483514,2.29084870697764,
8.7370759012338));
#45902=CARTESIAN_POINT('Ctrl Pts',(-0.259001631223251,2.29178073515796,
8.73700463245885));
#45903=CARTESIAN_POINT('Ctrl Pts',(-0.258571976689877,2.2923596324888,8.73696018039082));
#45904=CARTESIAN_POINT('Ctrl Pts',(-0.256594168726203,2.29500584291444,
8.73675612556665));
#45905=CARTESIAN_POINT('Ctrl Pts',(-0.255023175874761,2.2970558939418,8.73659562883457));
#45906=CARTESIAN_POINT('Ctrl Pts',(-0.242977289283136,2.3123897181956,8.73537646883157));
#45907=CARTESIAN_POINT('Ctrl Pts',(-0.231497352663814,2.32484699126091,
8.73427669168106));
#45908=CARTESIAN_POINT('Ctrl Pts',(-0.199231117070066,2.35475825075898,
8.7313421767124));
#45909=CARTESIAN_POINT('Ctrl Pts',(-0.177126483035226,2.37059376250626,
8.72946823584323));
#45910=CARTESIAN_POINT('Ctrl Pts',(-0.153012936905855,2.38363413902653,
8.72769287112027));
#45911=CARTESIAN_POINT('Ctrl Pts',(-0.152723549730563,2.38379006508564,
8.72767160284876));
#45912=CARTESIAN_POINT('Ctrl Pts',(-0.151945065732852,2.38420798806613,
8.72761449163078));
#45913=CARTESIAN_POINT('Ctrl Pts',(-0.151455527776677,2.38446916633555,
8.72757868699199));
#45914=CARTESIAN_POINT('Ctrl Pts',(-0.147502410743754,2.38656513613873,
8.72729044857387));
#45915=CARTESIAN_POINT('Ctrl Pts',(-0.144006102439163,2.38833796891551,
8.72704102283465));
#45916=CARTESIAN_POINT('Ctrl Pts',(-0.139947019703821,2.39030390205763,
8.72675846312227));
#45917=CARTESIAN_POINT('Ctrl Pts',(-0.139415197144291,2.39055967836607,
8.72672157901884));
#45918=CARTESIAN_POINT('Ctrl Pts',(-0.138627084666661,2.39093605353073,
8.72666712592486));
#45919=CARTESIAN_POINT('Ctrl Pts',(-0.138371337315835,2.39105777580768,
8.72664948754754));
#45920=CARTESIAN_POINT('Ctrl Pts',(-0.137917258826756,2.39127315950779,
8.72661822783701));
#45921=CARTESIAN_POINT('Ctrl Pts',(-0.137718992559633,2.39136695560995,
8.72660459809659));
#45922=CARTESIAN_POINT('Ctrl Pts',(-0.13729969437438,2.39156479422013,8.72657581455237));
#45923=CARTESIAN_POINT('Ctrl Pts',(-0.137078640476376,2.39166878754852,
8.72656066384871));
#45924=CARTESIAN_POINT('Ctrl Pts',(-0.13648933756291,2.391945203236,8.72652033719244));
#45925=CARTESIAN_POINT('Ctrl Pts',(-0.136120878597832,2.39211718089653,
8.72649518889914));
#45926=CARTESIAN_POINT('Ctrl Pts',(-0.134400945495759,2.39291599627391,
8.72637810087898));
#45927=CARTESIAN_POINT('Ctrl Pts',(-0.133045432540324,2.39353416854733,
8.72628668977969));
#45928=CARTESIAN_POINT('Ctrl Pts',(-0.122160889991647,2.39840709905856,
8.72555922142188));
#45929=CARTESIAN_POINT('Ctrl Pts',(-0.112433534147441,2.4022065990743,8.72494903641194));
#45930=CARTESIAN_POINT('Ctrl Pts',(-0.0734711500019861,2.41528273782643,
8.72259592651542));
#45931=CARTESIAN_POINT('Ctrl Pts',(-0.0431617179237742,2.42084020970614,
8.72094533364573));
#45932=CARTESIAN_POINT('Ctrl Pts',(-0.0106362385681566,2.4221049648031,
8.71904032795771));
#45933=CARTESIAN_POINT('Ctrl Pts',(-0.00874967847752063,2.42216173088752,
8.71892943022806));
#45934=CARTESIAN_POINT('Ctrl Pts',(-0.000181261329068391,2.42234423428214,
8.71842373912622));
#45935=CARTESIAN_POINT('Ctrl Pts',(0.00650263556893807,2.4222786746552,
8.71802366270603));
#45936=CARTESIAN_POINT('Ctrl Pts',(0.0142196486096833,2.42196282598536,
8.71755362294204));
#45937=CARTESIAN_POINT('Ctrl Pts',(0.0152597557318807,2.42191520550943,
8.71749010087077));
#45938=CARTESIAN_POINT('Ctrl Pts',(0.0168041393489657,2.4218369955958,8.71739552335311));
#45939=CARTESIAN_POINT('Ctrl Pts',(0.0173086112853697,2.42181025901013,
8.71736458877296));
#45940=CARTESIAN_POINT('Ctrl Pts',(0.0182058676322534,2.42176058928044,
8.71730949485646));
#45941=CARTESIAN_POINT('Ctrl Pts',(0.0185986777074702,2.42173812272669,
8.71728535020527));
#45942=CARTESIAN_POINT('Ctrl Pts',(0.0194243549030181,2.4216893814323,8.71723454561747));
#45943=CARTESIAN_POINT('Ctrl Pts',(0.0198572118083085,2.42166295221235,
8.71720788087932));
#45944=CARTESIAN_POINT('Ctrl Pts',(0.0209951273250252,2.42159116813012,
8.71713770191949));
#45945=CARTESIAN_POINT('Ctrl Pts',(0.0217000895644193,2.42154436846395,
8.71709414242385));
#45946=CARTESIAN_POINT('Ctrl Pts',(0.0248402447371625,2.42132553218599,
8.71689974205555));
#45947=CARTESIAN_POINT('Ctrl Pts',(0.0272735388199031,2.4211281503482,8.71674810739714));
#45948=CARTESIAN_POINT('Ctrl Pts',(0.0449860174032254,2.41948860011334,
8.71563682087728));
#45949=CARTESIAN_POINT('Ctrl Pts',(0.0601448649880876,2.41698451070976,
8.71464356157887));
#45950=CARTESIAN_POINT('Ctrl Pts',(0.103896583758847,2.40650541148109,8.71165709658134));
#45951=CARTESIAN_POINT('Ctrl Pts',(0.131634332567747,2.39565581002674,8.70959697358945));
#45952=CARTESIAN_POINT('Ctrl Pts',(0.160975594939883,2.37922021272131,8.70742952650427));
#45953=CARTESIAN_POINT('Ctrl Pts',(0.164417532341585,2.37720740975228,8.7071757522863));
#45954=CARTESIAN_POINT('Ctrl Pts',(0.168327723642775,2.37482231495264,8.70688879029276));
#45955=CARTESIAN_POINT('Ctrl Pts',(0.168833177704902,2.37451208618576,8.70685172200223));
#45956=CARTESIAN_POINT('Ctrl Pts',(0.16957666681898,2.37405293015971,8.70679723888245));
#45957=CARTESIAN_POINT('Ctrl Pts',(0.169815364548814,2.37390508652296,8.70677975341445));
#45958=CARTESIAN_POINT('Ctrl Pts',(0.17024042506662,2.37364104503969,8.7067486280095));
#45959=CARTESIAN_POINT('Ctrl Pts',(0.170426862352229,2.37352496859919,8.70673498005822));
#45960=CARTESIAN_POINT('Ctrl Pts',(0.17081524182776,2.37328261106572,8.70670655776558));
#45961=CARTESIAN_POINT('Ctrl Pts',(0.171017162145569,2.3731562970245,8.70669178570865));
#45962=CARTESIAN_POINT('Ctrl Pts',(0.17154678230169,2.37282416838126,8.70665305200281));
#45963=CARTESIAN_POINT('Ctrl Pts',(0.171874253045955,2.37261798641067,8.70662911471545));
#45964=CARTESIAN_POINT('Ctrl Pts',(0.172591425503731,2.37216463477988,8.70657671626444));
#45965=CARTESIAN_POINT('Ctrl Pts',(0.172980970096583,2.37191721639661,8.70654827140853));
#45966=CARTESIAN_POINT('Ctrl Pts',(0.174126761392463,2.37118601096484,8.70646464862688));
#45967=CARTESIAN_POINT('Ctrl Pts',(0.174881527030134,2.37069989494528,8.7064096202658));
#45968=CARTESIAN_POINT('Ctrl Pts',(0.183079596058085,2.36537123030725,8.70581241854418));
#45969=CARTESIAN_POINT('Ctrl Pts',(0.190322500077258,2.36022568267457,8.70528929092011));
#45970=CARTESIAN_POINT('Ctrl Pts',(0.215843560059731,2.34045844725737,8.70342668209469));
#45971=CARTESIAN_POINT('Ctrl Pts',(0.232728193425783,2.32415716309023,8.70215165548536));
#45972=CARTESIAN_POINT('Ctrl Pts',(0.258664453089838,2.29299651068582,8.69985308230382));
#45973=CARTESIAN_POINT('Ctrl Pts',(0.268559478518763,2.27897103360197,8.69885825606967));
#45974=CARTESIAN_POINT('Ctrl Pts',(0.277941236473569,2.26313022017065,8.69773987756249));
#45975=CARTESIAN_POINT('Ctrl Pts',(0.278584124497709,2.26202988974519,8.69766223044251));
#45976=CARTESIAN_POINT('Ctrl Pts',(0.279473877294604,2.2604860900134,8.69755333047804));
#45977=CARTESIAN_POINT('Ctrl Pts',(0.279726252124453,2.2600457967134,8.69752227679395));
#45978=CARTESIAN_POINT('Ctrl Pts',(0.28016104707138,2.25928308309595,8.69746849030715));
#45979=CARTESIAN_POINT('Ctrl Pts',(0.280343953721204,2.25896094006638,8.69744577507593));
#45980=CARTESIAN_POINT('Ctrl Pts',(0.28072211390609,2.25829222541008,8.69739862642809));
#45981=CARTESIAN_POINT('Ctrl Pts',(0.280917281943962,2.25794560634657,8.69737418998722));
#45982=CARTESIAN_POINT('Ctrl Pts',(0.281373186066503,2.25713240109643,8.69731686468335));
#45983=CARTESIAN_POINT('Ctrl Pts',(0.281633403543088,2.25666552688703,8.69728395729759));
#45984=CARTESIAN_POINT('Ctrl Pts',(0.282471648749979,2.25515273551754,8.69717734041653));
#45985=CARTESIAN_POINT('Ctrl Pts',(0.283045015625288,2.254104259364,8.69710346463571));
#45986=CARTESIAN_POINT('Ctrl Pts',(0.284366976014723,2.25165461486203,8.69693089244573));
#45987=CARTESIAN_POINT('Ctrl Pts',(0.285111061972586,2.25025106140082,8.69683203782606));
#45988=CARTESIAN_POINT('Ctrl Pts',(0.292770420792738,2.23554159687508,8.69579616720342));
#45989=CARTESIAN_POINT('Ctrl Pts',(0.298758351674873,2.22177592697205,8.6948266314204));
#45990=CARTESIAN_POINT('Ctrl Pts',(0.313021045284607,2.18152777249815,8.69199533007313));
#45991=CARTESIAN_POINT('Ctrl Pts',(0.318868710546923,2.15432827586823,8.69007695579631));
#45992=CARTESIAN_POINT('Ctrl Pts',(0.321231682342236,2.125923285754,8.68821573052544));
#45993=CARTESIAN_POINT('Ctrl Pts',(0.321294792914689,2.12512899825819,8.6881638080771));
#45994=CARTESIAN_POINT('Ctrl Pts',(0.321421727756294,2.12345272885341,8.688054500639));
#45995=CARTESIAN_POINT('Ctrl Pts',(0.321484869196359,2.122570699484,8.68799714219029));
#45996=CARTESIAN_POINT('Ctrl Pts',(0.321553978010025,2.12154611776537,8.68793070472324));
#45997=CARTESIAN_POINT('Ctrl Pts',(0.321563481437544,2.12140381673283,8.68792148170687));
#45998=CARTESIAN_POINT('Ctrl Pts',(0.321605169862825,2.1207732938807,8.68788063446492));
#45999=CARTESIAN_POINT('Ctrl Pts',(0.321636337643961,2.12028500268697,8.68784905216766));
#46000=CARTESIAN_POINT('Ctrl Pts',(0.321911703935198,2.11581070379754,8.68756013384366));
#46001=CARTESIAN_POINT('Ctrl Pts',(0.32208291960246,2.11182032180296,8.68730592029225));
#46002=CARTESIAN_POINT('Ctrl Pts',(0.322194337704641,2.10723439299373,8.68701851381538));
#46003=CARTESIAN_POINT('Ctrl Pts',(0.322207111241453,2.10664117231213,8.68698142708442));
#46004=CARTESIAN_POINT('Ctrl Pts',(0.322223516614468,2.10576713369397,8.68692692205073));
#46005=CARTESIAN_POINT('Ctrl Pts',(0.322228419771395,2.10548634518676,8.68690943302799));
#46006=CARTESIAN_POINT('Ctrl Pts',(0.322236503432739,2.1049859518729,8.68687830358886));
#46007=CARTESIAN_POINT('Ctrl Pts',(0.322239826477187,2.10476635014712,8.68686465515051));
#46008=CARTESIAN_POINT('Ctrl Pts',(0.322245809724694,2.10434229735707,8.68683832507757));
#46009=CARTESIAN_POINT('Ctrl Pts',(0.322248499834516,2.10413784804252,8.68682564177988));
#46010=CARTESIAN_POINT('Ctrl Pts',(0.322255335360436,2.10357783444557,8.68679093108023));
#46011=CARTESIAN_POINT('Ctrl Pts',(0.322259086890187,2.10322226429441,8.68676892587348));
#46012=CARTESIAN_POINT('Ctrl Pts',(0.322271520043536,2.1018245754331,8.68668255689034));
#46013=CARTESIAN_POINT('Ctrl Pts',(0.32227573537832,2.10078240857744,8.68661844100109));
#46014=CARTESIAN_POINT('Ctrl Pts',(0.32227024399047,2.09396989111642,8.68620107267989));
#46015=CARTESIAN_POINT('Ctrl Pts',(0.322110616304971,2.08820029600263,8.68585579985326));
#46016=CARTESIAN_POINT('Ctrl Pts',(0.321465552348071,2.07638071823564,8.68515966243809));
#46017=CARTESIAN_POINT('Ctrl Pts',(0.320964025868544,2.07033396895897,8.68480955344859));
#46018=CARTESIAN_POINT('Ctrl Pts',(0.318434778769249,2.04763916976949,8.683506608538));
#46019=CARTESIAN_POINT('Ctrl Pts',(0.315279541988409,2.03114350080364,8.68258093942984));
#46020=CARTESIAN_POINT('Ctrl Pts',(0.305273343983131,1.99456353593097,8.68045018565243));
#46021=CARTESIAN_POINT('Ctrl Pts',(0.297697551010622,1.97476171169817,8.67923820492079));
#46022=CARTESIAN_POINT('Ctrl Pts',(0.287656152311748,1.95468378242558,8.67787475135588));
#46023=CARTESIAN_POINT('Ctrl Pts',(0.287067739606546,1.95352482171781,8.67779556578777));
#46024=CARTESIAN_POINT('Ctrl Pts',(0.286237882900444,1.9519145112768,8.67768485578309));
#46025=CARTESIAN_POINT('Ctrl Pts',(0.28600234469617,1.95146011848247,8.67765353938862));
#46026=CARTESIAN_POINT('Ctrl Pts',(0.28559394088151,1.95067681150095,8.67759942139728));
#46027=CARTESIAN_POINT('Ctrl Pts',(0.285421586513365,1.9503476306834,8.67757663789139));
#46028=CARTESIAN_POINT('Ctrl Pts',(0.285063862327353,1.94966727666626,8.67752946412748));
#46029=CARTESIAN_POINT('Ctrl Pts',(0.284878412045617,1.94931614665766,8.67750507104732));
#46030=CARTESIAN_POINT('Ctrl Pts',(0.284443797413027,1.94849692103725,8.67744804952074));
#46031=CARTESIAN_POINT('Ctrl Pts',(0.284194126303987,1.94802909689388,8.67741540312527));
#46032=CARTESIAN_POINT('Ctrl Pts',(0.283388882900536,1.94652918669054,8.67731046311394));
#46033=CARTESIAN_POINT('Ctrl Pts',(0.282828839056497,1.94549952353065,8.67723801044577));
#46034=CARTESIAN_POINT('Ctrl Pts',(0.274214563591115,1.92986563272967,8.67613154935595));
#46035=CARTESIAN_POINT('Ctrl Pts',(0.265045565021325,1.9159075817146,8.6750566207295));
#46036=CARTESIAN_POINT('Ctrl Pts',(0.241044556933921,1.884903420415,8.67245642616179));
#46037=CARTESIAN_POINT('Ctrl Pts',(0.225420090506573,1.86858113400703,8.67091035566852));
#46038=CARTESIAN_POINT('Ctrl Pts',(0.205275305210201,1.85152841751818,8.66915021836058));
#46039=CARTESIAN_POINT('Ctrl Pts',(0.202284175199631,1.84908728084921,8.66889434748372));
#46040=CARTESIAN_POINT('Ctrl Pts',(0.197713232714933,1.84549169900136,8.66851228137502));
#46041=CARTESIAN_POINT('Ctrl Pts',(0.196165651671012,1.84429697871749,8.66838442758327));
#46042=CARTESIAN_POINT('Ctrl Pts',(0.194344153216916,1.84291706650916,8.66823577467614));
#46043=CARTESIAN_POINT('Ctrl Pts',(0.194080736303882,1.84271814603576,8.66821432150253));
#46044=CARTESIAN_POINT('Ctrl Pts',(0.193421458917212,1.84222187840221,8.66816074033638));
#46045=CARTESIAN_POINT('Ctrl Pts',(0.19302521664863,1.84192503707702,8.66812863705441));
#46046=CARTESIAN_POINT('Ctrl Pts',(0.192444655962163,1.8414922003465,8.66808174875481));
#46047=CARTESIAN_POINT('Ctrl Pts',(0.192260875929563,1.84135548782649,8.66806692764648));
#46048=CARTESIAN_POINT('Ctrl Pts',(0.19183431155252,1.84103887580613,8.66803257747714));
#46049=CARTESIAN_POINT('Ctrl Pts',(0.191591419232093,1.84085912130544,8.66801305582987));
#46050=CARTESIAN_POINT('Ctrl Pts',(0.187953938292499,1.83817508261139,8.66772127581678));
#46051=CARTESIAN_POINT('Ctrl Pts',(0.184510547626401,1.83573719077625,8.66745248144098));
#46052=CARTESIAN_POINT('Ctrl Pts',(0.180570920494246,1.83306252972832,8.66715410717713));
#46053=CARTESIAN_POINT('Ctrl Pts',(0.18012098300644,1.832758719779,8.66712016299084));
#46054=CARTESIAN_POINT('Ctrl Pts',(0.17943963077834,1.83230115480346,8.66706896314954));
#46055=CARTESIAN_POINT('Ctrl Pts',(0.17920878420808,1.83214656157235,8.66705165137037));
#46056=CARTESIAN_POINT('Ctrl Pts',(0.178807318988723,1.83187845984461,8.66702160573603));
#46057=CARTESIAN_POINT('Ctrl Pts',(0.178636791943103,1.83176481553672,8.66700886267069));
#46058=CARTESIAN_POINT('Ctrl Pts',(0.178279662124944,1.83152730518608,8.66698221553311));
#46059=CARTESIAN_POINT('Ctrl Pts',(0.178093038708993,1.83140347107273,8.6669683136857));
#46060=CARTESIAN_POINT('Ctrl Pts',(0.177651150088129,1.83111091854968,8.66693545079649));
#46061=CARTESIAN_POINT('Ctrl Pts',(0.17739577254133,1.83094236837222,8.66691650116615));
#46062=CARTESIAN_POINT('Ctrl Pts',(0.176541859838724,1.83038052690974,8.66685327953433));
#46063=CARTESIAN_POINT('Ctrl Pts',(0.175942248318281,1.82998886351744,8.66680911635186));
#46064=CARTESIAN_POINT('Ctrl Pts',(0.174513053800377,1.82906210270635,8.6667043866079));
#46065=CARTESIAN_POINT('Ctrl Pts',(0.173682302489093,1.8285288081647,8.66664393629909));
#46066=CARTESIAN_POINT('Ctrl Pts',(0.170714462990907,1.82664282606932,8.66642944336876));
#46067=CARTESIAN_POINT('Ctrl Pts',(0.168563856244649,1.82531144971193,8.66627670423684));
#46068=CARTESIAN_POINT('Ctrl Pts',(0.162224400721188,1.82148937745178,8.66583360380263));
#46069=CARTESIAN_POINT('Ctrl Pts',(0.157994321674343,1.81906811797425,8.6655469234706));
#46070=CARTESIAN_POINT('Ctrl Pts',(0.14145318368664,1.81009197241098,8.66445380631727));
#46071=CARTESIAN_POINT('Ctrl Pts',(0.128775924541866,1.80424252860249,8.66367400179606));
#46072=CARTESIAN_POINT('Ctrl Pts',(0.0902808838479029,1.78942662905229,
8.66136823026948));
#46073=CARTESIAN_POINT('Ctrl Pts',(0.0636645717253811,1.78289903859826,
8.65984183268163));
#46074=CARTESIAN_POINT('Ctrl Pts',(0.0348389663162673,1.77960903193642,
8.65808454882584));
#46075=CARTESIAN_POINT('Ctrl Pts',(0.0331308795251033,1.77942790103473,
8.65798009055044));
#46076=CARTESIAN_POINT('Ctrl Pts',(0.0307848122892476,1.77919806709294,
8.65783613924487));
#46077=CARTESIAN_POINT('Ctrl Pts',(0.0301479922573071,1.77913759432096,
8.65779701671745));
#46078=CARTESIAN_POINT('Ctrl Pts',(0.029135633615279,1.77904450063876,8.6577347453277));
#46079=CARTESIAN_POINT('Ctrl Pts',(0.0287602082302013,1.77901064170757,
8.65771163543769));
#46080=CARTESIAN_POINT('Ctrl Pts',(0.0280310862812035,1.77894617294702,
8.65766671981459));
#46081=CARTESIAN_POINT('Ctrl Pts',(0.0276773966718144,1.77891548873328,
8.65764491645236));
#46082=CARTESIAN_POINT('Ctrl Pts',(0.0268334391513403,1.778843676346,8.65759285357545));
#46083=CARTESIAN_POINT('Ctrl Pts',(0.0263431274379504,1.77880308639069,
8.65756257719295));
#46084=CARTESIAN_POINT('Ctrl Pts',(0.0248801056886644,1.77868534411748,
8.65747214747316));
#46085=CARTESIAN_POINT('Ctrl Pts',(0.0239071427253281,1.77861148707964,
8.65741189077025));
#46086=CARTESIAN_POINT('Ctrl Pts',(0.0156465185784834,1.77802214697242,
8.65689928105501));
#46087=CARTESIAN_POINT('Ctrl Pts',(0.00834412754341373,1.77775023218287,
8.65643932518234));
#46088=CARTESIAN_POINT('Ctrl Pts',(-0.00846630807655281,1.777696022445,
8.65536355380563));
#46089=CARTESIAN_POINT('Ctrl Pts',(-0.0179677757964866,1.7780859369684,
8.65474297159538));
#46090=CARTESIAN_POINT('Ctrl Pts',(-0.0299776977436681,1.77911214844882,
8.6539439922575));
#46091=CARTESIAN_POINT('Ctrl Pts',(-0.0325152473042243,1.77935933831432,
8.65377436331968));
#46092=CARTESIAN_POINT('Ctrl Pts',(-0.0521011873566472,1.78150215037182,
8.65245919431146));
#46093=CARTESIAN_POINT('Ctrl Pts',(-0.0689763851792746,1.78472609890834,
8.65128943391358));
#46094=CARTESIAN_POINT('Ctrl Pts',(-0.0990715853535514,1.79300857801476,
8.64919149957954));
#46095=CARTESIAN_POINT('Ctrl Pts',(-0.112372585455829,1.79762371138241,
8.64826056144807));
#46096=CARTESIAN_POINT('Ctrl Pts',(-0.126071507899858,1.80340634436363,
8.64732650314877));
#46097=CARTESIAN_POINT('Ctrl Pts',(-0.126810842476563,1.80372169851464,
8.64727617196429));
#46098=CARTESIAN_POINT('Ctrl Pts',(-0.127822785695127,1.80415781240035,
8.64720740046214));
#46099=CARTESIAN_POINT('Ctrl Pts',(-0.128096410062603,1.8042761858804,8.64718881684159));
#46100=CARTESIAN_POINT('Ctrl Pts',(-0.128562763285297,1.80447870508954,
8.64715716445705));
#46101=CARTESIAN_POINT('Ctrl Pts',(-0.128755574069192,1.80456265978081,
8.64714408402609));
#46102=CARTESIAN_POINT('Ctrl Pts',(-0.129130186427699,1.80472621185523,
8.6471186819942));
#46103=CARTESIAN_POINT('Ctrl Pts',(-0.129311995272093,1.80480578784277,
8.6471063592551));
#46104=CARTESIAN_POINT('Ctrl Pts',(-0.129688458381443,1.80497097667044,
8.64708085438204));
#46105=CARTESIAN_POINT('Ctrl Pts',(-0.129883100944394,1.80505661401916,
8.64706767383437));
#46106=CARTESIAN_POINT('Ctrl Pts',(-0.13032741240479,1.80525262390133,8.64703760044733));
#46107=CARTESIAN_POINT('Ctrl Pts',(-0.130577026536933,1.80536312131158,
8.64702071526232));
#46108=CARTESIAN_POINT('Ctrl Pts',(-0.131821572161716,1.80591594012638,
8.64693657644676));
#46109=CARTESIAN_POINT('Ctrl Pts',(-0.132814413620418,1.80636299147854,
8.64686960961929));
#46110=CARTESIAN_POINT('Ctrl Pts',(-0.135332678692076,1.80751228803068,
8.64670010185249));
#46111=CARTESIAN_POINT('Ctrl Pts',(-0.136854934403849,1.80822144908281,
8.64659796347277));
#46112=CARTESIAN_POINT('Ctrl Pts',(-0.143110068558229,1.81119520164811,
8.6461793356589));
#46113=CARTESIAN_POINT('Ctrl Pts',(-0.147793097589866,1.81356342714628,
8.64586846301345));
#46114=CARTESIAN_POINT('Ctrl Pts',(-0.161902103771534,1.82113661928987,
8.64493343972686));
#46115=CARTESIAN_POINT('Ctrl Pts',(-0.171127303605349,1.8267006159989,8.64432413352563));
#46116=CARTESIAN_POINT('Ctrl Pts',(-0.200924333795429,1.84677355785067,
8.64230755728273));
#46117=CARTESIAN_POINT('Ctrl Pts',(-0.220071752590232,1.86322467442633,
8.64092216570651));
#46118=CARTESIAN_POINT('Ctrl Pts',(-0.23748135315962,1.88213747007581,8.63940934495352));
#46119=CARTESIAN_POINT('Ctrl Pts',(-0.237850918519618,1.88254100249033,
8.63937710379));
#46120=CARTESIAN_POINT('Ctrl Pts',(-0.239477879577936,1.88432660805946,
8.63923459779455));
#46121=CARTESIAN_POINT('Ctrl Pts',(-0.240724252346865,1.88571864074143,
8.63912392117508));
#46122=CARTESIAN_POINT('Ctrl Pts',(-0.245262576263303,1.89087691312943,
8.63871519712279));
#46123=CARTESIAN_POINT('Ctrl Pts',(-0.248478687910199,1.89470866016084,
8.6384142681002));
#46124=CARTESIAN_POINT('Ctrl Pts',(-0.252139840125557,1.89928275757837,
8.63805746401904));
#46125=CARTESIAN_POINT('Ctrl Pts',(-0.252672807723355,1.89995409877028,
8.63800515596503));
#46126=CARTESIAN_POINT('Ctrl Pts',(-0.253521439701633,1.90103186171989,
8.63792127361707));
#46127=CARTESIAN_POINT('Ctrl Pts',(-0.253838822447975,1.90143693029062,
8.63788976784797));
#46128=CARTESIAN_POINT('Ctrl Pts',(-0.254398735119936,1.90215507075262,
8.63783394752902));
#46129=CARTESIAN_POINT('Ctrl Pts',(-0.254641661288021,1.90246783352127,
8.6378096487685));
#46130=CARTESIAN_POINT('Ctrl Pts',(-0.25514417470238,1.9031172773439,8.63775921738535));
#46131=CARTESIAN_POINT('Ctrl Pts',(-0.255403673335457,1.90345402571145,
8.63773308132431));
#46132=CARTESIAN_POINT('Ctrl Pts',(-0.256069373670772,1.90432144189538,
8.63766579264622));
#46133=CARTESIAN_POINT('Ctrl Pts',(-0.25647459094744,1.90485285956069,8.63762460134289));
#46134=CARTESIAN_POINT('Ctrl Pts',(-0.258145998964497,1.90705900692752,
8.63745372984919));
#46135=CARTESIAN_POINT('Ctrl Pts',(-0.259397439642892,1.90874479991227,
8.6373234735796));
#46136=CARTESIAN_POINT('Ctrl Pts',(-0.267679179050108,1.92013179688353,
8.63644556146597));
#46137=CARTESIAN_POINT('Ctrl Pts',(-0.274179448455385,1.93020517253619,
8.63567768680478));
#46138=CARTESIAN_POINT('Ctrl Pts',(-0.285679611855011,1.950415696332,8.63415273527023));
#46139=CARTESIAN_POINT('Ctrl Pts',(-0.290737323169246,1.96050060939791,
8.63339877897254));
#46140=CARTESIAN_POINT('Ctrl Pts',(-0.297226608311066,1.97533367052695,
8.63230672759021));
#46141=CARTESIAN_POINT('Ctrl Pts',(-0.299093942896654,1.97988271169898,
8.63197406213613));
#46142=CARTESIAN_POINT('Ctrl Pts',(-0.30177013758237,1.98685206103709,8.63146884727493));
#46143=CARTESIAN_POINT('Ctrl Pts',(-0.30265556106367,1.98924223080309,8.63129636395728));
#46144=CARTESIAN_POINT('Ctrl Pts',(-0.304501734207848,1.99441342345963,
8.63092511771356));
#46145=CARTESIAN_POINT('Ctrl Pts',(-0.305452948814603,1.99719762836776,
8.63072642184364));
#46146=CARTESIAN_POINT('Ctrl Pts',(-0.3110870139823,2.01445753220449,8.62950314922358));
#46147=CARTESIAN_POINT('Ctrl Pts',(-0.314778686774291,2.02923880535573,
8.62849131203339));
#46148=CARTESIAN_POINT('Ctrl Pts',(-0.317569922439361,2.0451242382985,8.6274769783564));
#46149=CARTESIAN_POINT('Ctrl Pts',(-0.317723714409241,2.04602179875248,
8.6274199126478));
#46150=CARTESIAN_POINT('Ctrl Pts',(-0.317925433403785,2.0472298088842,8.62734345101829));
#46151=CARTESIAN_POINT('Ctrl Pts',(-0.317976712078569,2.04753968306305,
8.6273238676053));
#46152=CARTESIAN_POINT('Ctrl Pts',(-0.318062283034643,2.04806151871233,
8.62729094012427));
#46153=CARTESIAN_POINT('Ctrl Pts',(-0.318096816503776,2.0482734395261,8.62727758234351));
#46154=CARTESIAN_POINT('Ctrl Pts',(-0.318162642397224,2.04867995077836,
8.62725198674318));
#46155=CARTESIAN_POINT('Ctrl Pts',(-0.318193967879006,2.0488745339878,8.62723974714242));
#46156=CARTESIAN_POINT('Ctrl Pts',(-0.31825827209253,2.04927631826446,8.627214499222));
#46157=CARTESIAN_POINT('Ctrl Pts',(-0.318291226876738,2.04948352211374,
8.62720149232054));
#46158=CARTESIAN_POINT('Ctrl Pts',(-0.318365151784295,2.04995127058588,
8.62717216071327));
#46159=CARTESIAN_POINT('Ctrl Pts',(-0.318406004522026,2.05021183401547,
8.62715584268829));
#46160=CARTESIAN_POINT('Ctrl Pts',(-0.318508334209309,2.05086978163353,
8.62711469147931));
#46161=CARTESIAN_POINT('Ctrl Pts',(-0.318569387594239,2.05126723269236,
8.62708988210395));
#46162=CARTESIAN_POINT('Ctrl Pts',(-0.318740993133279,2.05239847080447,
8.62701940593629));
#46163=CARTESIAN_POINT('Ctrl Pts',(-0.318849755864242,2.05313253265157,
8.62697383788043));
#46164=CARTESIAN_POINT('Ctrl Pts',(-0.321152835815807,2.0690556394045,8.62598881250798));
#46165=CARTESIAN_POINT('Ctrl Pts',(-0.3222622218736,2.08438373205464,8.62510777473546));
#46166=CARTESIAN_POINT('Ctrl Pts',(-0.322274890249976,2.09973403126875,
8.62424191572231));
#46167=CARTESIAN_POINT('',(-0.322193764531691,2.10029569746695,8.37437729859741));
#46168=CARTESIAN_POINT('Ctrl Pts',(-0.322274889955221,2.09973367435276,
8.62424193585475));
#46169=CARTESIAN_POINT('Ctrl Pts',(-0.322289278827864,2.11714533708805,
8.6232598019252));
#46170=CARTESIAN_POINT('Ctrl Pts',(-0.320892615123807,2.13453003690225,
8.6222992791076));
#46171=CARTESIAN_POINT('Ctrl Pts',(-0.31561710362526,2.16697805015618,8.62043450130561));
#46172=CARTESIAN_POINT('Ctrl Pts',(-0.312041398813254,2.18203832932221,
8.61953862448343));
#46173=CARTESIAN_POINT('Ctrl Pts',(-0.306662861375602,2.19912152843302,
8.61845830205772));
#46174=CARTESIAN_POINT('Ctrl Pts',(-0.305899846109963,2.20145181902264,
8.61830954980833));
#46175=CARTESIAN_POINT('Ctrl Pts',(-0.304882469788176,2.20444307536386,
8.61811673638976));
#46176=CARTESIAN_POINT('Ctrl Pts',(-0.304652404798807,2.20511226671195,
8.61807347977649));
#46177=CARTESIAN_POINT('Ctrl Pts',(-0.304277714658802,2.20619056582074,
8.6180035806767));
#46178=CARTESIAN_POINT('Ctrl Pts',(-0.304134463120211,2.20660015125213,
8.61797698378991));
#46179=CARTESIAN_POINT('Ctrl Pts',(-0.303859761421119,2.20738051859004,
8.61792622123663));
#46180=CARTESIAN_POINT('Ctrl Pts',(-0.303728458593311,2.20775135183335,
8.61790206050354));
#46181=CARTESIAN_POINT('Ctrl Pts',(-0.303427151032547,2.20859739577276,
8.61784685089513));
#46182=CARTESIAN_POINT('Ctrl Pts',(-0.303256708617738,2.20907244851964,
8.61781578749871));
#46183=CARTESIAN_POINT('Ctrl Pts',(-0.302732045036946,2.21052404099147,
8.61772067398586));
#46184=CARTESIAN_POINT('Ctrl Pts',(-0.302374220226622,2.21149926291777,
8.61765650386377));
#46185=CARTESIAN_POINT('Ctrl Pts',(-0.299697700737171,2.21868625111849,
8.61718157587235));
#46186=CARTESIAN_POINT('Ctrl Pts',(-0.297192662213035,2.22482647568947,
8.6167646005063));
#46187=CARTESIAN_POINT('Ctrl Pts',(-0.293612896988812,2.23288120842361,
8.61620193246884));
#46188=CARTESIAN_POINT('Ctrl Pts',(-0.292705341781809,2.23486857069105,
8.616061810938));
#46189=CARTESIAN_POINT('Ctrl Pts',(-0.281238644675409,2.2593173199937,8.61432194954758));
#46190=CARTESIAN_POINT('Ctrl Pts',(-0.26814029408882,2.2804926763812,8.61263682911569));
#46191=CARTESIAN_POINT('Ctrl Pts',(-0.248644309706695,2.30513625640713,
8.61051519751126));
#46192=CARTESIAN_POINT('Ctrl Pts',(-0.244384115203252,2.31019344991678,
8.61007064713891));
#46193=CARTESIAN_POINT('Ctrl Pts',(-0.233710476624205,2.32210034851475,
8.60900716801304));
#46194=CARTESIAN_POINT('Ctrl Pts',(-0.227147092450352,2.32880862399694,
8.60839360132089));
#46195=CARTESIAN_POINT('Ctrl Pts',(-0.21920078488741,2.33625083826131,8.60770513205838));
#46196=CARTESIAN_POINT('Ctrl Pts',(-0.218094601827136,2.3372723910163,8.60761045168332));
#46197=CARTESIAN_POINT('Ctrl Pts',(-0.21675887857997,2.33848868873116,8.60749755112829));
#46198=CARTESIAN_POINT('Ctrl Pts',(-0.216536198182731,2.33869089001106,
8.6074787764554));
#46199=CARTESIAN_POINT('Ctrl Pts',(-0.216148309989463,2.33904211598542,
8.60744615518428));
#46200=CARTESIAN_POINT('Ctrl Pts',(-0.215983230825327,2.33919128146539,
8.60743229797286));
#46201=CARTESIAN_POINT('Ctrl Pts',(-0.215651728743901,2.33949020363677,
8.60740452289326));
#46202=CARTESIAN_POINT('Ctrl Pts',(-0.215485303719271,2.33963995833407,
8.60739060517711));
#46203=CARTESIAN_POINT('Ctrl Pts',(-0.215166171961874,2.33992652230166,
8.60736396751872));
#46204=CARTESIAN_POINT('Ctrl Pts',(-0.21501349095821,2.34006335906808,8.60735124545063));
#46205=CARTESIAN_POINT('Ctrl Pts',(-0.214653311145667,2.34038554251016,
8.60732128537012));
#46206=CARTESIAN_POINT('Ctrl Pts',(-0.214445702298301,2.34057076672123,
8.60730405665412));
#46207=CARTESIAN_POINT('Ctrl Pts',(-0.213831128454681,2.34111764876116,
8.60725317369623));
#46208=CARTESIAN_POINT('Ctrl Pts',(-0.213423483985489,2.34147854673657,
8.60721957628624));
#46209=CARTESIAN_POINT('Ctrl Pts',(-0.209817517270556,2.34465473663088,
8.60692370565947));
#46210=CARTESIAN_POINT('Ctrl Pts',(-0.206564383351062,2.34740753931755,
8.60666597534273));
#46211=CARTESIAN_POINT('Ctrl Pts',(-0.195999380091241,2.35599393193254,
8.60585427656205));
#46212=CARTESIAN_POINT('Ctrl Pts',(-0.188487371326696,2.36157444414607,
8.60531462880073));
#46213=CARTESIAN_POINT('Ctrl Pts',(-0.172922498489049,2.37211799237987,
8.60424649194393));
#46214=CARTESIAN_POINT('Ctrl Pts',(-0.164873006885681,2.37706911390877,
8.60371865757591));
#46215=CARTESIAN_POINT('Ctrl Pts',(-0.148982057119743,2.38590531246562,
8.60270235863695));
#46216=CARTESIAN_POINT('Ctrl Pts',(-0.141177267910753,2.38983870620425,
8.60221434752027));
#46217=CARTESIAN_POINT('Ctrl Pts',(-0.117788144997574,2.40045705917763,
8.60076344184052));
#46218=CARTESIAN_POINT('Ctrl Pts',(-0.101827174683326,2.40623455535009,
8.5997862915574));
#46219=CARTESIAN_POINT('Ctrl Pts',(-0.0829942364726874,2.41141582815646,
8.59860897203718));
#46220=CARTESIAN_POINT('Ctrl Pts',(-0.0804930886085562,2.41207166388473,
8.59845218173404));
#46221=CARTESIAN_POINT('Ctrl Pts',(-0.0772845960211634,2.41287183796288,
8.59825040889319));
#46222=CARTESIAN_POINT('Ctrl Pts',(-0.0765842379138335,2.41304400691,8.59820632659876));
#46223=CARTESIAN_POINT('Ctrl Pts',(-0.0754586436800834,2.41331670821684,
8.59813541455056));
#46224=CARTESIAN_POINT('Ctrl Pts',(-0.0750337679833222,2.41341872983777,
8.59810863283789));
#46225=CARTESIAN_POINT('Ctrl Pts',(-0.0742266218374024,2.41361080733379,
8.59805772660293));
#46226=CARTESIAN_POINT('Ctrl Pts',(-0.0738443913814698,2.41370102920659,
8.59803360747543));
#46227=CARTESIAN_POINT('Ctrl Pts',(-0.0729759689617699,2.41390433694146,
8.59797878129875));
#46228=CARTESIAN_POINT('Ctrl Pts',(-0.0724896781119359,2.41401699215062,
8.59794806046244));
#46229=CARTESIAN_POINT('Ctrl Pts',(-0.071049822467201,2.41434702940355,
8.59785703965663));
#46230=CARTESIAN_POINT('Ctrl Pts',(-0.0700955340421101,2.41456119951615,
8.59779663671507));
#46231=CARTESIAN_POINT('Ctrl Pts',(-0.0636138809691888,2.41598491189389,
8.59738582991462));
#46232=CARTESIAN_POINT('Ctrl Pts',(-0.0580567645082365,2.41705298600654,
8.59703092261629));
#46233=CARTESIAN_POINT('Ctrl Pts',(-0.0520926999182333,2.41803722443612,
8.59664682972004));
#46234=CARTESIAN_POINT('Ctrl Pts',(-0.0517106023972528,2.41809957420507,
8.59662220836619));
#46235=CARTESIAN_POINT('Ctrl Pts',(-0.0284735726931505,2.42184836350535,
8.59512403328706));
#46236=CARTESIAN_POINT('Ctrl Pts',(-0.00529170856375248,2.42306154822161,
8.59357241161624));
#46237=CARTESIAN_POINT('Ctrl Pts',(0.0282928311121755,2.42120211310135,
8.59129625747692));
#46238=CARTESIAN_POINT('Ctrl Pts',(0.0387356602430444,2.42011067380137,
8.59058574465203));
#46239=CARTESIAN_POINT('Ctrl Pts',(0.0560058430313619,2.41744802418545,
8.5894211508617));
#46240=CARTESIAN_POINT('Ctrl Pts',(0.0628689017969807,2.41616042902419,
8.5889612146127));
#46241=CARTESIAN_POINT('Ctrl Pts',(0.0738716749152643,2.41372366492334,
8.58823386467368));
#46242=CARTESIAN_POINT('Ctrl Pts',(0.078039538443443,2.4127129629377,8.5879607098021));
#46243=CARTESIAN_POINT('Ctrl Pts',(0.0827173182496458,2.41147924900187,
8.58765776530736));
#46244=CARTESIAN_POINT('Ctrl Pts',(0.083248050630079,2.41133782194597,8.58762344687613));
#46245=CARTESIAN_POINT('Ctrl Pts',(0.0839928229668553,2.41113731793815,
8.58757536526593));
#46246=CARTESIAN_POINT('Ctrl Pts',(0.0842071635040732,2.41107937658899,
8.58756153668274));
#46247=CARTESIAN_POINT('Ctrl Pts',(0.0846372534775072,2.41096263594445,
8.58753380689905));
#46248=CARTESIAN_POINT('Ctrl Pts',(0.084853002280755,2.41090383341932,8.58751990587278));
#46249=CARTESIAN_POINT('Ctrl Pts',(0.0852667450966799,2.41079060469843,
8.58749326574277));
#46250=CARTESIAN_POINT('Ctrl Pts',(0.0854647479678533,2.41073621392361,
8.58748052457947));
#46251=CARTESIAN_POINT('Ctrl Pts',(0.0859320898536088,2.41060735607322,
8.58745047018639));
#46252=CARTESIAN_POINT('Ctrl Pts',(0.0862013847843693,2.4105327277052,8.58743316639711));
#46253=CARTESIAN_POINT('Ctrl Pts',(0.0871356303680149,2.4102725159339,8.58737318436096));
#46254=CARTESIAN_POINT('Ctrl Pts',(0.0878000875582233,2.4100851445476,8.58733060951985));
#46255=CARTESIAN_POINT('Ctrl Pts',(0.0958354708488177,2.40779133457556,
8.58681672730123));
#46256=CARTESIAN_POINT('Ctrl Pts',(0.103130278963668,2.40542447665799,8.58636020686218));
#46257=CARTESIAN_POINT('Ctrl Pts',(0.114138293844963,2.40141336489655,8.58567692419823));
#46258=CARTESIAN_POINT('Ctrl Pts',(0.117915886118112,2.39995568438996,8.58544348338621));
#46259=CARTESIAN_POINT('Ctrl Pts',(0.141657516319181,2.39027651047187,8.58397716809752));
#46260=CARTESIAN_POINT('Ctrl Pts',(0.160780747619045,2.38013734566603,8.58279615851553));
#46261=CARTESIAN_POINT('Ctrl Pts',(0.1916143101985,2.35958478486062,8.58069420346629));
#46262=CARTESIAN_POINT('Ctrl Pts',(0.203845959245418,2.35009405432754,8.57979816856137));
#46263=CARTESIAN_POINT('Ctrl Pts',(0.217172729885274,2.33812432606454,8.57871765776444));
#46264=CARTESIAN_POINT('Ctrl Pts',(0.218978344923815,2.33646495133719,8.57856888927991));
#46265=CARTESIAN_POINT('Ctrl Pts',(0.221280360877282,2.33430040184641,8.57837605772921));
#46266=CARTESIAN_POINT('Ctrl Pts',(0.22179431096724,2.33381394317995,8.57833279940673));
#46267=CARTESIAN_POINT('Ctrl Pts',(0.2226208087827,2.33302647791551,8.57826289821028));
#46268=CARTESIAN_POINT('Ctrl Pts',(0.222934360047665,2.3327265241007,8.57823630094102));
#46269=CARTESIAN_POINT('Ctrl Pts',(0.223531019265905,2.3321534273026,8.57818553809768));
#46270=CARTESIAN_POINT('Ctrl Pts',(0.223814234960702,2.33188039720764,8.57816137745796));
#46271=CARTESIAN_POINT('Ctrl Pts',(0.224459653028552,2.33125590695729,8.5781061686781));
#46272=CARTESIAN_POINT('Ctrl Pts',(0.224821530477681,2.3309041137992,8.57807510601844));
#46273=CARTESIAN_POINT('Ctrl Pts',(0.225925679592945,2.32982567721043,8.57797999694929));
#46274=CARTESIAN_POINT('Ctrl Pts',(0.226665260308591,2.32909629925763,8.57791583055055));
#46275=CARTESIAN_POINT('Ctrl Pts',(0.232098665018089,2.32368578489707,8.57744098757749));
#46276=CARTESIAN_POINT('Ctrl Pts',(0.236650285195752,2.31886469031296,8.57702409600658));
#46277=CARTESIAN_POINT('Ctrl Pts',(0.242274814081534,2.31252646095577,8.57648316075803));
#46278=CARTESIAN_POINT('Ctrl Pts',(0.243487961862438,2.31113548814349,8.57636487356227));
#46279=CARTESIAN_POINT('Ctrl Pts',(0.245909477499344,2.30831039599949,8.57612547851468));
#46280=CARTESIAN_POINT('Ctrl Pts',(0.247117409246144,2.30687599674828,8.57600436045813));
#46281=CARTESIAN_POINT('Ctrl Pts',(0.258471698604419,2.29315161992836,8.57484959189341));
#46282=CARTESIAN_POINT('Ctrl Pts',(0.267704716243784,2.28013675302101,8.57378376599523));
#46283=CARTESIAN_POINT('Ctrl Pts',(0.284956180894196,2.25154526519327,8.57152746918955));
#46284=CARTESIAN_POINT('Ctrl Pts',(0.292746590281897,2.23588775999119,8.57033840233793));
#46285=CARTESIAN_POINT('Ctrl Pts',(0.301030828332621,2.21517429963108,8.5688761598379));
#46286=CARTESIAN_POINT('Ctrl Pts',(0.302729430566614,2.21063261869833,8.56856213475));
#46287=CARTESIAN_POINT('Ctrl Pts',(0.30484659452487,2.20455736067678,8.56815229933356));
#46288=CARTESIAN_POINT('Ctrl Pts',(0.305357150458607,2.20305677446312,8.56805188773756));
#46289=CARTESIAN_POINT('Ctrl Pts',(0.306184769451272,2.2005641437318,8.56788651581217));
#46290=CARTESIAN_POINT('Ctrl Pts',(0.306508125747099,2.19957423848631,8.56782121077517));
#46291=CARTESIAN_POINT('Ctrl Pts',(0.306935402575118,2.19824439214856,8.56773399090108));
#46292=CARTESIAN_POINT('Ctrl Pts',(0.307043562588505,2.19790583546679,8.56771183051866));
#46293=CARTESIAN_POINT('Ctrl Pts',(0.307213062093039,2.19737223376422,8.56767697396423));
#46294=CARTESIAN_POINT('Ctrl Pts',(0.30727477600167,2.19717730940141,8.56766425570861));
#46295=CARTESIAN_POINT('Ctrl Pts',(0.307402401735869,2.1967728643523,8.56763789775847));
#46296=CARTESIAN_POINT('Ctrl Pts',(0.307468284350025,2.19656333666064,8.56762425994196));
#46297=CARTESIAN_POINT('Ctrl Pts',(0.307617949578613,2.19608564747666,8.56759320697851));
#46298=CARTESIAN_POINT('Ctrl Pts',(0.307701595659562,2.19581744404834,8.56757579997582));
#46299=CARTESIAN_POINT('Ctrl Pts',(0.307960983465421,2.19498189853027,8.5675216573617));
#46300=CARTESIAN_POINT('Ctrl Pts',(0.30813550888236,2.19441417565431,8.56748499302369));
#46301=CARTESIAN_POINT('Ctrl Pts',(0.30947530661344,2.19001259090472,8.5672016658689));
#46302=CARTESIAN_POINT('Ctrl Pts',(0.310570617794281,2.18615757000808,8.56695899955717));
#46303=CARTESIAN_POINT('Ctrl Pts',(0.311715709647907,2.18182126838335,8.56669110162066));
#46304=CARTESIAN_POINT('Ctrl Pts',(0.311836591027326,2.18135935166222,8.56666262819123));
#46305=CARTESIAN_POINT('Ctrl Pts',(0.311991942503021,2.18076028377085,8.56662578128387));
#46306=CARTESIAN_POINT('Ctrl Pts',(0.312027348865919,2.18062337862807,8.56661736611381));
#46307=CARTESIAN_POINT('Ctrl Pts',(0.312281121192132,2.179639450669,8.56655692582009));
#46308=CARTESIAN_POINT('Ctrl Pts',(0.312496130127134,2.1787915569222,8.56650504920344));
#46309=CARTESIAN_POINT('Ctrl Pts',(0.313170645801836,2.17608538953229,8.56634010826773));
#46310=CARTESIAN_POINT('Ctrl Pts',(0.313617056639271,2.1742238638879,8.56622759390601));
#46311=CARTESIAN_POINT('Ctrl Pts',(0.319926115006788,2.14684156900942,8.5645849480828));
#46312=CARTESIAN_POINT('Ctrl Pts',(0.32267409085372,2.12070134580295,8.56316716286454));
#46313=CARTESIAN_POINT('Ctrl Pts',(0.321966911334884,2.07915879202717,8.56080957855629));
#46314=CARTESIAN_POINT('Ctrl Pts',(0.320608231087173,2.06384314292637,8.55991934275485));
#46315=CARTESIAN_POINT('Ctrl Pts',(0.317774322136969,2.0462727174578,8.55884574134688));
#46316=CARTESIAN_POINT('Ctrl Pts',(0.317358036363327,2.04386608023926,8.55869756984175));
#46317=CARTESIAN_POINT('Ctrl Pts',(0.316786098720414,2.04076958037542,8.55850540512337));
#46318=CARTESIAN_POINT('Ctrl Pts',(0.316655467593175,2.04007513218849,8.55846220976323));
#46319=CARTESIAN_POINT('Ctrl Pts',(0.316440978780081,2.03895517499018,8.55839238580152));
#46320=CARTESIAN_POINT('Ctrl Pts',(0.316358543751782,2.03852939316946,8.55836580262057));
#46321=CARTESIAN_POINT('Ctrl Pts',(0.316199684300522,2.03771765841098,8.55831505044109));
#46322=CARTESIAN_POINT('Ctrl Pts',(0.316123412003408,2.03733167620957,8.55829088634132));
#46323=CARTESIAN_POINT('Ctrl Pts',(0.315947602396905,2.03645046558745,8.55823564694098));
#46324=CARTESIAN_POINT('Ctrl Pts',(0.315847607377566,2.03595533048224,8.5582045570625));
#46325=CARTESIAN_POINT('Ctrl Pts',(0.315537984811538,2.03444056623767,8.55810928374757));
#46326=CARTESIAN_POINT('Ctrl Pts',(0.315324582400139,2.03342172345565,8.55804497971556));
#46327=CARTESIAN_POINT('Ctrl Pts',(0.313705632610896,2.0258748159736,8.55756698449485));
#46328=CARTESIAN_POINT('Ctrl Pts',(0.312102518901936,2.0193912301101,8.55714698526234));
#46329=CARTESIAN_POINT('Ctrl Pts',(0.309739747417511,2.01096766388689,8.55658838978149));
#46330=CARTESIAN_POINT('Ctrl Pts',(0.309160997580292,2.00897832527316,8.55645551656806));
#46331=CARTESIAN_POINT('Ctrl Pts',(0.30126930825418,1.98279610430242,8.55469410554572));
#46332=CARTESIAN_POINT('Ctrl Pts',(0.291155009018485,1.95954242309954,8.55297656199692));
#46333=CARTESIAN_POINT('Ctrl Pts',(0.270221128211279,1.9236266338944,8.55017108654684));
#46334=CARTESIAN_POINT('Ctrl Pts',(0.260952209590638,1.91018137617041,8.54908265695147));
#46335=CARTESIAN_POINT('Ctrl Pts',(0.250304739574772,1.89699971205137,8.54801683388345));
#46336=CARTESIAN_POINT('Ctrl Pts',(0.249903911506828,1.89650647531082,8.54797695605127));
#46337=CARTESIAN_POINT('Ctrl Pts',(0.249183373178297,1.8956251606377,8.54790571378721));
#46338=CARTESIAN_POINT('Ctrl Pts',(0.248864210273479,1.8952366407631,8.5478743112462));
#46339=CARTESIAN_POINT('Ctrl Pts',(0.248376167890504,1.89464536899852,8.5478265292745));
#46340=CARTESIAN_POINT('Ctrl Pts',(0.248207948338979,1.89444207718436,8.5478101023019));
#46341=CARTESIAN_POINT('Ctrl Pts',(0.247913651623383,1.8940873102421,8.54778143834851));
#46342=CARTESIAN_POINT('Ctrl Pts',(0.247787685412635,1.89393574443108,8.54776919330902));
#46343=CARTESIAN_POINT('Ctrl Pts',(0.247524157156473,1.89361925144892,8.547743625827));
#46344=CARTESIAN_POINT('Ctrl Pts',(0.247386569703223,1.89345434674233,8.54773030535057));
#46345=CARTESIAN_POINT('Ctrl Pts',(0.247004371138156,1.89299719444839,8.54769338081598));
#46346=CARTESIAN_POINT('Ctrl Pts',(0.246759405297072,1.89270524182077,8.5476698027293));
#46347=CARTESIAN_POINT('Ctrl Pts',(0.245787644795391,1.89155125180641,8.54757661584557));
#46348=CARTESIAN_POINT('Ctrl Pts',(0.245056835066731,1.89069258342567,8.54750729738346));
#46349=CARTESIAN_POINT('Ctrl Pts',(0.231204144164507,1.87458830890502,8.54620723538208));
#46350=CARTESIAN_POINT('Ctrl Pts',(0.216685557709048,1.86059778108319,8.54507641194588));
#46351=CARTESIAN_POINT('Ctrl Pts',(0.188405562137587,1.83804162282798,8.54305240499374));
#46352=CARTESIAN_POINT('Ctrl Pts',(0.175126238737614,1.82898409710304,8.54216020050904));
#46353=CARTESIAN_POINT('Ctrl Pts',(0.156233829829782,1.81806838676072,8.54090913700315));
#46354=CARTESIAN_POINT('Ctrl Pts',(0.151163268239895,1.81531753564531,8.54057517817261));
#46355=CARTESIAN_POINT('Ctrl Pts',(0.139457460407964,1.80936790501967,8.53980517864555));
#46356=CARTESIAN_POINT('Ctrl Pts',(0.132781129652931,1.80625766952256,8.53936666972128));
#46357=CARTESIAN_POINT('Ctrl Pts',(0.124568472999773,1.80276893583573,8.53882555851535));
#46358=CARTESIAN_POINT('Ctrl Pts',(0.123128042608866,1.80216935187994,8.53873059357326));
#46359=CARTESIAN_POINT('Ctrl Pts',(0.121131914920536,1.80135541285289,8.53859889219197));
#46360=CARTESIAN_POINT('Ctrl Pts',(0.120579876001654,1.80113209650332,8.53856245899979));
#46361=CARTESIAN_POINT('Ctrl Pts',(0.119647278325489,1.80075783715867,8.53850089092351));
#46362=CARTESIAN_POINT('Ctrl Pts',(0.119267043640176,1.80060608634855,8.53847578335171));
#46363=CARTESIAN_POINT('Ctrl Pts',(0.118514311687826,1.80030733423381,8.53842606820371));
#46364=CARTESIAN_POINT('Ctrl Pts',(0.118141827483509,1.80016030185208,8.5384014617286));
#46365=CARTESIAN_POINT('Ctrl Pts',(0.11732051866197,1.7998378709188,8.5383471936368));
#46366=CARTESIAN_POINT('Ctrl Pts',(0.116871573357984,1.79966278423998,8.53831752159487));
#46367=CARTESIAN_POINT('Ctrl Pts',(0.115303233475435,1.7990551876398,8.53821383687887));
#46368=CARTESIAN_POINT('Ctrl Pts',(0.114181827616396,1.79862792777678,8.53813964833862));
#46369=CARTESIAN_POINT('Ctrl Pts',(0.102384579787537,1.79420842873743,8.53735859642527));
#46370=CARTESIAN_POINT('Ctrl Pts',(0.0915077199919616,1.79077941215271,
8.53663302107544));
#46371=CARTESIAN_POINT('Ctrl Pts',(0.059646714208816,1.7825633488805,8.53448924977191));
#46372=CARTESIAN_POINT('Ctrl Pts',(0.0383369386996806,1.77929166876649,
8.53302925433063));
#46373=CARTESIAN_POINT('Ctrl Pts',(-0.00061308625369795,1.77725076947602,
8.53039440946308));
#46374=CARTESIAN_POINT('Ctrl Pts',(-0.0181376951682772,1.77775997224327,
8.5292230118871));
#46375=CARTESIAN_POINT('Ctrl Pts',(-0.0362385210700665,1.77976813952959,
8.52808043858649));
#46376=CARTESIAN_POINT('Ctrl Pts',(-0.0369405346626418,1.77984836125532,
8.52803623408479));
#46377=CARTESIAN_POINT('Ctrl Pts',(-0.037945127639853,1.77996650816732,
8.52797313761739));
#46378=CARTESIAN_POINT('Ctrl Pts',(-0.0382479195091772,1.78000255428944,
8.52795414080838));
#46379=CARTESIAN_POINT('Ctrl Pts',(-0.0387716975116797,1.78006566195025,
8.52792131636));
#46380=CARTESIAN_POINT('Ctrl Pts',(-0.0389927072337549,1.78009252278973,
8.52790747732112));
#46381=CARTESIAN_POINT('Ctrl Pts',(-0.0394187703746862,1.78014475327584,
8.5278808204495));
#46382=CARTESIAN_POINT('Ctrl Pts',(-0.0396238267703211,1.78017009103665,
8.52786800081712));
#46383=CARTESIAN_POINT('Ctrl Pts',(-0.0401110597167236,1.78023077167172,
8.52783756325244));
#46384=CARTESIAN_POINT('Ctrl Pts',(-0.0403932147010553,1.78026629094695,
8.52781995534992));
#46385=CARTESIAN_POINT('Ctrl Pts',(-0.0412394189988933,1.78037395397081,
8.52776720208886));
#46386=CARTESIAN_POINT('Ctrl Pts',(-0.0418033285563329,1.78044721764185,
8.52773211960848));
#46387=CARTESIAN_POINT('Ctrl Pts',(-0.0472989555515489,1.78117601106265,
8.52739089903997));
#46388=CARTESIAN_POINT('Ctrl Pts',(-0.0522153922839701,1.78194420840323,
8.52709096897759));
#46389=CARTESIAN_POINT('Ctrl Pts',(-0.0576514372948319,1.78292305760914,
8.52676331364816));
#46390=CARTESIAN_POINT('Ctrl Pts',(-0.0581902392782435,1.78302149650437,
8.52673088115274));
#46391=CARTESIAN_POINT('Ctrl Pts',(-0.0594289335595994,1.7832510702173,
8.52665641441541));
#46392=CARTESIAN_POINT('Ctrl Pts',(-0.0601286495151927,1.78338315239774,
8.52661441925532));
#46393=CARTESIAN_POINT('Ctrl Pts',(-0.0640974524223875,1.78414595633043,
8.52637658892838));
#46394=CARTESIAN_POINT('Ctrl Pts',(-0.0673571468810866,1.78482500661229,
8.52618266571173));
#46395=CARTESIAN_POINT('Ctrl Pts',(-0.0939570689454248,1.79079777274573,
8.52460758253531));
#46396=CARTESIAN_POINT('Ctrl Pts',(-0.116652702769177,1.79862606677382,
8.52330505956185));
#46397=CARTESIAN_POINT('Ctrl Pts',(-0.152177925289865,1.81550042258348,
8.52107365207062));
#46398=CARTESIAN_POINT('Ctrl Pts',(-0.165589600697517,1.82309185214857,
8.52018148354223));
#46399=CARTESIAN_POINT('Ctrl Pts',(-0.18044329501253,1.83296559364849,8.51910557955796));
#46400=CARTESIAN_POINT('Ctrl Pts',(-0.182464502823773,1.83434258604206,
8.51895720877051));
#46401=CARTESIAN_POINT('Ctrl Pts',(-0.185049503894568,1.83614709296875,
8.51876482142896));
#46402=CARTESIAN_POINT('Ctrl Pts',(-0.1856278702302,1.83655366918151,8.51872160502484));
#46403=CARTESIAN_POINT('Ctrl Pts',(-0.186558927169982,1.83721276577405,
8.51865175524905));
#46404=CARTESIAN_POINT('Ctrl Pts',(-0.186912456152261,1.83746410243329,
8.51862516735949));
#46405=CARTESIAN_POINT('Ctrl Pts',(-0.187585667564541,1.83794476205304,
8.51857441162068));
#46406=CARTESIAN_POINT('Ctrl Pts',(-0.187905439826657,1.8381739583379,8.5185502486821));
#46407=CARTESIAN_POINT('Ctrl Pts',(-0.188634696279859,1.83869867586434,
8.51849501953882));
#46408=CARTESIAN_POINT('Ctrl Pts',(-0.189043906424451,1.83899457462573,
8.51846393877576));
#46409=CARTESIAN_POINT('Ctrl Pts',(-0.190293911732564,1.83990293191513,
8.51836872048318));
#46410=CARTESIAN_POINT('Ctrl Pts',(-0.191132432326863,1.84051849595587,
8.51830446256138));
#46411=CARTESIAN_POINT('Ctrl Pts',(-0.197318575266951,1.84510604319358,
8.51782752560934));
#46412=CARTESIAN_POINT('Ctrl Pts',(-0.202544537704322,1.84923866140214,
8.51740856985307));
#46413=CARTESIAN_POINT('Ctrl Pts',(-0.209063715133185,1.85473073588962,
8.51686434549041));
#46414=CARTESIAN_POINT('Ctrl Pts',(-0.210478551995268,1.85594380190856,
8.51674488268412));
#46415=CARTESIAN_POINT('Ctrl Pts',(-0.21377955950078,1.85882410445391,8.51646295705187));
#46416=CARTESIAN_POINT('Ctrl Pts',(-0.215656855500674,1.86050128853268,
8.51630011975769));
#46417=CARTESIAN_POINT('Ctrl Pts',(-0.238900199308489,1.88176186253411,
8.51425242374418));
#46418=CARTESIAN_POINT('Ctrl Pts',(-0.257548298085593,1.9041183484057,8.51225441121164));
#46419=CARTESIAN_POINT('Ctrl Pts',(-0.27700718463596,1.93511721110082,8.50981832344622));
#46420=CARTESIAN_POINT('Ctrl Pts',(-0.280830892652184,1.9417175237896,8.50931740457639));
#46421=CARTESIAN_POINT('Ctrl Pts',(-0.285971060699911,1.95136404341727,
8.50861652560779));
#46422=CARTESIAN_POINT('Ctrl Pts',(-0.287480143188643,1.95430420553925,
8.50840692419111));
#46423=CARTESIAN_POINT('Ctrl Pts',(-0.289173389079175,1.95773195936524,
8.50816762379397));
#46424=CARTESIAN_POINT('Ctrl Pts',(-0.289401853078545,1.95819727865373,
8.5081352454797));
#46425=CARTESIAN_POINT('Ctrl Pts',(-0.289747020442032,1.95890459982595,
8.50808619227389));
#46426=CARTESIAN_POINT('Ctrl Pts',(-0.289864544181349,1.9591461969519,8.50806946638598));
#46427=CARTESIAN_POINT('Ctrl Pts',(-0.290076879762431,1.95958409287362,
8.50803920358847));
#46428=CARTESIAN_POINT('Ctrl Pts',(-0.290171794236656,1.95978034026154,
8.50802566027761));
#46429=CARTESIAN_POINT('Ctrl Pts',(-0.290362409942377,1.96017548414179,
8.50799842960865));
#46430=CARTESIAN_POINT('Ctrl Pts',(-0.290458105538497,1.96037438175527,
8.50798474261956));
#46431=CARTESIAN_POINT('Ctrl Pts',(-0.290731258298616,1.9609436096115,8.50794562752195));
#46432=CARTESIAN_POINT('Ctrl Pts',(-0.290908212893175,1.96131418264468,
8.50792023079673));
#46433=CARTESIAN_POINT('Ctrl Pts',(-0.291668265761645,1.96291371798913,
8.5078108957311));
#46434=CARTESIAN_POINT('Ctrl Pts',(-0.292244299202433,1.96414605009278,
8.5077273899757));
#46435=CARTESIAN_POINT('Ctrl Pts',(-0.302951756978391,1.98743623537348,
8.50616221346712));
#46436=CARTESIAN_POINT('Ctrl Pts',(-0.310568753063442,2.0105694090921,8.50482337218961));
#46437=CARTESIAN_POINT('Ctrl Pts',(-0.318506063112586,2.04871165398499,
8.5026445285078));
#46438=CARTESIAN_POINT('Ctrl Pts',(-0.320511050883701,2.06326813640315,
8.50182002241191));
#46439=CARTESIAN_POINT('Ctrl Pts',(-0.322020665383746,2.08524009578906,
8.50054282176863));
#46440=CARTESIAN_POINT('Ctrl Pts',(-0.322273441735044,2.0925851041351,8.50011063335046));
#46441=CARTESIAN_POINT('Ctrl Pts',(-0.322275785453835,2.10368636016889,
8.49944597289085));
#46442=CARTESIAN_POINT('Ctrl Pts',(-0.322210971854595,2.10744035923576,
8.49921924710806));
#46443=CARTESIAN_POINT('Ctrl Pts',(-0.322053560396658,2.11197020470806,
8.49894302119048));
#46444=CARTESIAN_POINT('Ctrl Pts',(-0.322023708370871,2.11274805064671,
8.49889549491129));
#46445=CARTESIAN_POINT('Ctrl Pts',(-0.321970211184815,2.11402159052878,
8.49881752524605));
#46446=CARTESIAN_POINT('Ctrl Pts',(-0.321948238545141,2.11451735460327,
8.49878713432552));
#46447=CARTESIAN_POINT('Ctrl Pts',(-0.321906840582164,2.1154050511086,8.49873264716256));
#46448=CARTESIAN_POINT('Ctrl Pts',(-0.321887844281587,2.11579700335002,
8.49870856442063));
#46449=CARTESIAN_POINT('Ctrl Pts',(-0.321846097182538,2.11662701931167,
8.4986575132848));
#46450=CARTESIAN_POINT('Ctrl Pts',(-0.32182316779078,2.11706507289467,8.49863053933591));
#46451=CARTESIAN_POINT('Ctrl Pts',(-0.321759761867809,2.11823080992015,
8.49855867392898));
#46452=CARTESIAN_POINT('Ctrl Pts',(-0.321717711300987,2.1189584020656,8.49851373317104));
#46453=CARTESIAN_POINT('Ctrl Pts',(-0.321510499093469,2.12234431857016,
8.49830419113506));
#46454=CARTESIAN_POINT('Ctrl Pts',(-0.32131485862497,2.12500061082128,8.49813863609256));
#46455=CARTESIAN_POINT('Ctrl Pts',(-0.319551091077461,2.14547936150679,
8.4968529344725));
#46456=CARTESIAN_POINT('Ctrl Pts',(-0.316534473950642,2.16314276994974,
8.49568659032966));
#46457=CARTESIAN_POINT('Ctrl Pts',(-0.308147156200516,2.19567255712307,
8.49344010755191));
#46458=CARTESIAN_POINT('Ctrl Pts',(-0.303118679325512,2.21057552285883,
8.49237030271836));
#46459=CARTESIAN_POINT('Ctrl Pts',(-0.291355934509451,2.23851451077511,
8.49033006846181));
#46460=CARTESIAN_POINT('Ctrl Pts',(-0.284778302024963,2.25157830538204,
8.48936058054594));
#46461=CARTESIAN_POINT('Ctrl Pts',(-0.276872479281622,2.26493524181735,
8.48838445998296));
#46462=CARTESIAN_POINT('Ctrl Pts',(-0.276405630831196,2.26571641762082,
8.48832743180554));
#46463=CARTESIAN_POINT('Ctrl Pts',(-0.275773252301414,2.26676446724762,
8.48825101284272));
#46464=CARTESIAN_POINT('Ctrl Pts',(-0.275610637857428,2.2670330821219,8.48823143482726));
#46465=CARTESIAN_POINT('Ctrl Pts',(-0.275336178426266,2.26748495624063,
8.48819851424768));
#46466=CARTESIAN_POINT('Ctrl Pts',(-0.275224542880367,2.26766834141905,
8.48818515798214));
#46467=CARTESIAN_POINT('Ctrl Pts',(-0.275010070036646,2.26801986742623,
8.48815956355868));
#46468=CARTESIAN_POINT('Ctrl Pts',(-0.274907262497061,2.26818802424107,
8.48814732362291));
#46469=CARTESIAN_POINT('Ctrl Pts',(-0.274663545388898,2.26858583883783,
8.48811837526481));
#46470=CARTESIAN_POINT('Ctrl Pts',(-0.274522502198236,2.26881541401881,
8.48810167579746));
#46471=CARTESIAN_POINT('Ctrl Pts',(-0.274107321816106,2.26948930443415,
8.48805267440352));
#46472=CARTESIAN_POINT('Ctrl Pts',(-0.273832391017473,2.26993313340687,
8.48802042462228));
#46473=CARTESIAN_POINT('Ctrl Pts',(-0.271759371546199,2.27326157590052,
8.48777872796356));
#46474=CARTESIAN_POINT('Ctrl Pts',(-0.26991673964707,2.2761183851991,8.48757216496842));
#46475=CARTESIAN_POINT('Ctrl Pts',(-0.263489649158483,2.28574503870713,
8.48687722803608));
#46476=CARTESIAN_POINT('Ctrl Pts',(-0.258692667108727,2.29236980059292,
8.48640089321402));
#46477=CARTESIAN_POINT('Ctrl Pts',(-0.239115499277049,2.31734758910587,
8.48458271450017));
#46478=CARTESIAN_POINT('Ctrl Pts',(-0.222592864509201,2.3342407165758,8.48329903224635));
#46479=CARTESIAN_POINT('Ctrl Pts',(-0.201550953132475,2.35149897478235,
8.48174834833523));
#46480=CARTESIAN_POINT('Ctrl Pts',(-0.19868723042998,2.35376742186803,8.4815390326261));
#46481=CARTESIAN_POINT('Ctrl Pts',(-0.186348391828434,2.36320450452221,
8.48064275049407));
#46482=CARTESIAN_POINT('Ctrl Pts',(-0.176520255926883,2.36989420827705,
8.47994210978705));
#46483=CARTESIAN_POINT('Ctrl Pts',(-0.165411866279095,2.37658864728621,
8.47915376593937));
#46484=CARTESIAN_POINT('Ctrl Pts',(-0.164474824113691,2.37714688795046,
8.47908729646465));
#46485=CARTESIAN_POINT('Ctrl Pts',(-0.16307973226661,2.37796844365138,8.47898837364845));
#46486=CARTESIAN_POINT('Ctrl Pts',(-0.162623833112833,2.37823541047208,
8.4789560529578));
#46487=CARTESIAN_POINT('Ctrl Pts',(-0.161842382388833,2.3786904380095,8.47890066203942));
#46488=CARTESIAN_POINT('Ctrl Pts',(-0.161517153375179,2.37887905288648,
8.47887761192549));
#46489=CARTESIAN_POINT('Ctrl Pts',(-0.160883857216363,2.37924485028636,
8.47883273316718));
#46490=CARTESIAN_POINT('Ctrl Pts',(-0.160575825437108,2.37942209327093,
8.4788109067476));
#46491=CARTESIAN_POINT('Ctrl Pts',(-0.159838435219886,2.37984476918095,
8.47875866228929));
#46492=CARTESIAN_POINT('Ctrl Pts',(-0.159408804745186,2.38008972344024,
8.47872822705235));
#46493=CARTESIAN_POINT('Ctrl Pts',(-0.158118907401681,2.38082123057493,
8.4786368618463));
#46494=CARTESIAN_POINT('Ctrl Pts',(-0.157256970349238,2.38130481272324,
8.47857582528764));
#46495=CARTESIAN_POINT('Ctrl Pts',(-0.149619138838061,2.38554387638036,
8.47803507981947));
#46496=CARTESIAN_POINT('Ctrl Pts',(-0.142712617699471,2.38905757912737,
8.47754680689738));
#46497=CARTESIAN_POINT('Ctrl Pts',(-0.129698918525619,2.3950981941825,8.47662685578607));
#46498=CARTESIAN_POINT('Ctrl Pts',(-0.123627528937131,2.39769275836787,
8.4761977146619));
#46499=CARTESIAN_POINT('Ctrl Pts',(-0.102087708102175,2.40612504804404,
8.47467633409553));
#46500=CARTESIAN_POINT('Ctrl Pts',(-0.0862546391665527,2.41095738997894,
8.473558415275));
#46501=CARTESIAN_POINT('Ctrl Pts',(-0.0513200531372833,2.41874522977344,
8.47113669395405));
#46502=CARTESIAN_POINT('Ctrl Pts',(-0.0321773583053179,2.42124301462419,
8.46983732056639));
#46503=CARTESIAN_POINT('Ctrl Pts',(-0.0125010861032906,2.42203272781696,
8.46859627546926));
#46504=CARTESIAN_POINT('Ctrl Pts',(-0.012077936103984,2.42204887579857,
8.46856963153581));
#46505=CARTESIAN_POINT('Ctrl Pts',(-0.0108549200461107,2.42209313390064,
8.46849275730078));
#46506=CARTESIAN_POINT('Ctrl Pts',(-0.0100549721379043,2.42211909872408,
8.46844264094765));
#46507=CARTESIAN_POINT('Ctrl Pts',(-0.00895739237750149,2.42215063145364,
8.46837411265111));
#46508=CARTESIAN_POINT('Ctrl Pts',(-0.00865984582271966,2.4221587672193,
8.46835555873018));
#46509=CARTESIAN_POINT('Ctrl Pts',(-0.00815219178171078,2.42217194409805,
8.46832394409944));
#46510=CARTESIAN_POINT('Ctrl Pts',(-0.0079420906038569,2.42217719191801,
8.46831087178187));
#46511=CARTESIAN_POINT('Ctrl Pts',(-0.00753352610410729,2.42218699697156,
8.46828547464068));
#46512=CARTESIAN_POINT('Ctrl Pts',(-0.00733506520782097,2.42219157632017,
8.4682731486985));
#46513=CARTESIAN_POINT('Ctrl Pts',(-0.00685662109197878,2.42220217379484,
8.46824345940072));
#46514=CARTESIAN_POINT('Ctrl Pts',(-0.00657663424233016,2.42220801035106,
8.46822610637579));
#46515=CARTESIAN_POINT('Ctrl Pts',(-0.00572272634429809,2.42222469726816,
8.46817324667176));
#46516=CARTESIAN_POINT('Ctrl Pts',(-0.00514877965845295,2.42223437930549,
8.46813780537541));
#46517=CARTESIAN_POINT('Ctrl Pts',(0.000633699465098556,2.42231647186573,
8.46778159438697));
#46518=CARTESIAN_POINT('Ctrl Pts',(0.00584359965130935,2.42226413012393,
8.46746766646999));
#46519=CARTESIAN_POINT('Ctrl Pts',(0.0159055491386708,2.42191891892699,
8.46687100309641));
#46520=CARTESIAN_POINT('Ctrl Pts',(0.0207566471348524,2.4216425700655,8.4665876715227));
#46521=CARTESIAN_POINT('Ctrl Pts',(0.0591317254156498,2.41858458927343,
8.4643679690945));
#46522=CARTESIAN_POINT('Ctrl Pts',(0.0920384184708004,2.41067979644696,
8.46257190175339));
#46523=CARTESIAN_POINT('Ctrl Pts',(0.123606318708089,2.39762883011885,8.46056071873003));
#46524=CARTESIAN_POINT('Ctrl Pts',(0.124083288093251,2.39743029461414,8.46053026657131));
#46525=CARTESIAN_POINT('Ctrl Pts',(0.130704846505074,2.39465541277089,8.46010660320732));
#46526=CARTESIAN_POINT('Ctrl Pts',(0.136768205745549,2.39189042007938,8.45970771039502));
#46527=CARTESIAN_POINT('Ctrl Pts',(0.143673888286678,2.38847889288015,8.45923894994212));
#46528=CARTESIAN_POINT('Ctrl Pts',(0.144604321393027,2.38801362469066,8.4591754835637));
#46529=CARTESIAN_POINT('Ctrl Pts',(0.145983053473978,2.38731581708626,8.45908097307208));
#46530=CARTESIAN_POINT('Ctrl Pts',(0.146433091216151,2.38708671240903,8.45905004957351));
#46531=CARTESIAN_POINT('Ctrl Pts',(0.147232778409009,2.38667723902394,8.45899496812197));
#46532=CARTESIAN_POINT('Ctrl Pts',(0.147582640338916,2.38649728564306,8.45897082482998));
#46533=CARTESIAN_POINT('Ctrl Pts',(0.148317533156538,2.38611758619669,8.45892001568865));
#46534=CARTESIAN_POINT('Ctrl Pts',(0.148702491793071,2.3859177026773,8.45889334502304));
#46535=CARTESIAN_POINT('Ctrl Pts',(0.149701272873249,2.3853965390907,8.45882400306558));
#46536=CARTESIAN_POINT('Ctrl Pts',(0.150314462530237,2.3850740569871,8.45878128930344));
#46537=CARTESIAN_POINT('Ctrl Pts',(0.152985651004681,2.38365823971665,8.45859459350925));
#46538=CARTESIAN_POINT('Ctrl Pts',(0.155032755127375,2.38254459957924,8.45844989170558));
#46539=CARTESIAN_POINT('Ctrl Pts',(0.169542717954004,2.37444590541897,8.45741237007705));
#46540=CARTESIAN_POINT('Ctrl Pts',(0.181539300580954,2.36666209093851,8.45649054429966));
#46541=CARTESIAN_POINT('Ctrl Pts',(0.2124066727379,2.34358369364697,8.45394117253054));
#46542=CARTESIAN_POINT('Ctrl Pts',(0.230130546939323,2.32691274725929,8.45227329355706));
#46543=CARTESIAN_POINT('Ctrl Pts',(0.252479637583739,2.30055271265595,8.44997520428305));
#46544=CARTESIAN_POINT('Ctrl Pts',(0.258763476280781,2.29237689819328,8.44930239343237));
#46545=CARTESIAN_POINT('Ctrl Pts',(0.265065210977219,2.28330889483427,8.44860924859008));
#46546=CARTESIAN_POINT('Ctrl Pts',(0.265483033300111,2.28270324586698,8.44856319831509));
#46547=CARTESIAN_POINT('Ctrl Pts',(0.266061090679892,2.28185916024782,8.44849936400496));
#46548=CARTESIAN_POINT('Ctrl Pts',(0.266223082592409,2.28162193820238,8.44848146176619));
#46549=CARTESIAN_POINT('Ctrl Pts',(0.266501471483465,2.28121309093134,8.44845067305878));
#46550=CARTESIAN_POINT('Ctrl Pts',(0.266618020005385,2.28104156991339,8.44843777625843));
#46551=CARTESIAN_POINT('Ctrl Pts',(0.266859066383636,2.28068609147783,8.44841108870784));
#46552=CARTESIAN_POINT('Ctrl Pts',(0.26698353939582,2.2805021181499,8.44839729972045));
#46553=CARTESIAN_POINT('Ctrl Pts',(0.267276786472405,2.28006772679039,8.44836479511365));
#46554=CARTESIAN_POINT('Ctrl Pts',(0.267445399497575,2.27981719914357,8.44834609048887));
#46555=CARTESIAN_POINT('Ctrl Pts',(0.267980947217316,2.27901905506402,8.44828663210428));
#46556=CARTESIAN_POINT('Ctrl Pts',(0.268346557008565,2.27847054520906,8.44824596752253));
#46557=CARTESIAN_POINT('Ctrl Pts',(0.273075573071226,2.2713284044254,8.44771897692713));
#46558=CARTESIAN_POINT('Ctrl Pts',(0.277197006048649,2.26457683598257,8.4472484414298));
#46559=CARTESIAN_POINT('Ctrl Pts',(0.284822210338678,2.25098481652014,8.44634047671439));
#46560=CARTESIAN_POINT('Ctrl Pts',(0.288337954436874,2.24415735384519,8.44590276863756));
#46561=CARTESIAN_POINT('Ctrl Pts',(0.301709367289927,2.21573975733092,8.44412959504599));
#46562=CARTESIAN_POINT('Ctrl Pts',(0.30940958498516,2.19321983332688,8.44283028537474));
#46563=CARTESIAN_POINT('Ctrl Pts',(0.315331971276558,2.16662789759444,8.44125389909873));
#46564=CARTESIAN_POINT('Ctrl Pts',(0.316039833925883,2.16318505377851,8.44104916535892));
#46565=CARTESIAN_POINT('Ctrl Pts',(0.317021805566758,2.15797871684312,8.4407381637471));
#46566=CARTESIAN_POINT('Ctrl Pts',(0.317337820803846,2.15622334148638,8.440633068467));
#46567=CARTESIAN_POINT('Ctrl Pts',(0.317708020680221,2.15406435822743,8.44050347653155));
#46568=CARTESIAN_POINT('Ctrl Pts',(0.317776036828847,2.15366313120131,8.44047937901269));
#46569=CARTESIAN_POINT('Ctrl Pts',(0.317893641023428,2.15296132014564,8.44043720331767));
#46570=CARTESIAN_POINT('Ctrl Pts',(0.317943563248465,2.15266079208174,8.44041913484589));
#46571=CARTESIAN_POINT('Ctrl Pts',(0.318882065954678,2.14696109310315,8.44007629903359));
#46572=CARTESIAN_POINT('Ctrl Pts',(0.319633380678859,2.14154049495462,8.43974757154402));
#46573=CARTESIAN_POINT('Ctrl Pts',(0.320345136182677,2.13522708411542,8.43936073343787));
#46574=CARTESIAN_POINT('Ctrl Pts',(0.320440355906064,2.13435013848163,8.43930691289814));
#46575=CARTESIAN_POINT('Ctrl Pts',(0.320586183607758,2.13295370874127,8.43922106639881));
#46576=CARTESIAN_POINT('Ctrl Pts',(0.320639132422318,2.13243446923247,8.43918911417061));
#46577=CARTESIAN_POINT('Ctrl Pts',(0.320730157307969,2.13151982883124,8.43913277382025));
#46578=CARTESIAN_POINT('Ctrl Pts',(0.320768764226409,2.13112448089151,8.43910840245615));
#46579=CARTESIAN_POINT('Ctrl Pts',(0.320846891352525,2.13030884586814,8.43905808361597));
#46580=CARTESIAN_POINT('Ctrl Pts',(0.320886316885579,2.12988855067324,8.43903213321063));
#46581=CARTESIAN_POINT('Ctrl Pts',(0.320983589669415,2.12882919583166,8.43896667116294));
#46582=CARTESIAN_POINT('Ctrl Pts',(0.321040354101242,2.12819004076621,8.43892712554302));
#46583=CARTESIAN_POINT('Ctrl Pts',(0.321257221662141,2.1256625160985,8.43877054455687));
#46584=CARTESIAN_POINT('Ctrl Pts',(0.321402572872833,2.12377294905575,8.43865304664614));
#46585=CARTESIAN_POINT('Ctrl Pts',(0.322225779338296,2.11167699452783,8.43789797771844));
#46586=CARTESIAN_POINT('Ctrl Pts',(0.322433989746081,2.10144551402398,8.43724575640955));
#46587=CARTESIAN_POINT('Ctrl Pts',(0.321563493707716,2.06949692422061,8.43516507676452));
#46588=CARTESIAN_POINT('Ctrl Pts',(0.318775428963706,2.04788923723111,8.43368979177019));
#46589=CARTESIAN_POINT('Ctrl Pts',(0.310748519454833,2.01350793662296,8.43130476958646));
#46590=CARTESIAN_POINT('Ctrl Pts',(0.306828908671587,2.0004931760395,8.43039422463863));
#46591=CARTESIAN_POINT('Ctrl Pts',(0.300682585840457,1.98394952672803,8.42925620202979));
#46592=CARTESIAN_POINT('Ctrl Pts',(0.299193432046476,1.98016251080655,8.42899711582324));
#46593=CARTESIAN_POINT('Ctrl Pts',(0.297426861299292,1.97590839526436,8.42870850438163));
#46594=CARTESIAN_POINT('Ctrl Pts',(0.29721960556284,1.97541280054856,8.42867491957264));
#46595=CARTESIAN_POINT('Ctrl Pts',(0.296903849808689,1.97466303032856,8.42862416994687));
#46596=CARTESIAN_POINT('Ctrl Pts',(0.296796261687967,1.97440847541695,8.42860695037642));
#46597=CARTESIAN_POINT('Ctrl Pts',(0.296608469552856,1.97396574570263,8.42857702019208));
#46598=CARTESIAN_POINT('Ctrl Pts',(0.296528413784995,1.973777508797,8.42856430053891));
#46599=CARTESIAN_POINT('Ctrl Pts',(0.296360195310437,1.97338301624875,8.4285376561597));
#46600=CARTESIAN_POINT('Ctrl Pts',(0.296271996507548,1.97317677647808,8.42852373373438));
#46601=CARTESIAN_POINT('Ctrl Pts',(0.296059792160569,1.97268199764916,8.42849035008443));
#46602=CARTESIAN_POINT('Ctrl Pts',(0.295935579585396,1.97239354642408,8.42847090154602));
#46603=CARTESIAN_POINT('Ctrl Pts',(0.295517978832963,1.97142766707352,8.4284058228726));
#46604=CARTESIAN_POINT('Ctrl Pts',(0.295222681928338,1.97075105916104,8.42836030852752));
#46605=CARTESIAN_POINT('Ctrl Pts',(0.292143635000749,1.9637617088338,8.42789085175711));
#46606=CARTESIAN_POINT('Ctrl Pts',(0.289159934428492,1.9575383408469,8.42747880457437));
#46607=CARTESIAN_POINT('Ctrl Pts',(0.282763545180118,1.94522733872143,8.42666641568514));
#46608=CARTESIAN_POINT('Ctrl Pts',(0.279348460350714,1.93914526063271,8.42626645641119));
#46609=CARTESIAN_POINT('Ctrl Pts',(0.266007025349944,1.91709326114014,8.42480436291184));
#46610=CARTESIAN_POINT('Ctrl Pts',(0.254886617234915,1.90189029489291,8.42377037554917));
#46611=CARTESIAN_POINT('Ctrl Pts',(0.230964781842949,1.87455951953245,8.42171324401345));
#46612=CARTESIAN_POINT('Ctrl Pts',(0.218371364463552,1.86234067864355,8.42069754663236));
#46613=CARTESIAN_POINT('Ctrl Pts',(0.203861959295889,1.85039408860272,8.41955585838056));
#46614=CARTESIAN_POINT('Ctrl Pts',(0.202870376834871,1.84958750114612,8.41947797902535));
#46615=CARTESIAN_POINT('Ctrl Pts',(0.201477930148679,1.84846853575541,8.41936880569683));
#46616=CARTESIAN_POINT('Ctrl Pts',(0.201081076601369,1.84815116742341,8.41933771221324));
#46617=CARTESIAN_POINT('Ctrl Pts',(0.200393484686969,1.84760395352241,8.41928387554943));
#46618=CARTESIAN_POINT('Ctrl Pts',(0.20010309655223,1.84737366778016,8.41926115001916));
#46619=CARTESIAN_POINT('Ctrl Pts',(0.199500293510443,1.84689731991891,8.41921399781411));
#46620=CARTESIAN_POINT('Ctrl Pts',(0.199187819217273,1.84665133422842,8.41918956814596));
#46621=CARTESIAN_POINT('Ctrl Pts',(0.198567510927362,1.84616487276236,8.41914109607354));
#46622=CARTESIAN_POINT('Ctrl Pts',(0.198259693412566,1.84592437704209,8.41911705452394));
#46623=CARTESIAN_POINT('Ctrl Pts',(0.197228884254685,1.84512202676671,8.41903658410609));
#46624=CARTESIAN_POINT('Ctrl Pts',(0.196503940468409,1.84456269775824,8.41898005534832));
#46625=CARTESIAN_POINT('Ctrl Pts',(0.191265966621974,1.84055684314574,8.4185720605005));
#46626=CARTESIAN_POINT('Ctrl Pts',(0.186665168955711,1.83722722801407,8.41821603991749));
#46627=CARTESIAN_POINT('Ctrl Pts',(0.171377611646791,1.82676769722387,8.41703950718014));
#46628=CARTESIAN_POINT('Ctrl Pts',(0.160353250784354,1.82015550037184,8.41620043054406));
#46629=CARTESIAN_POINT('Ctrl Pts',(0.137801481081588,1.80840025676526,8.41450692534501));
#46630=CARTESIAN_POINT('Ctrl Pts',(0.126307138110754,1.80324060512717,8.41365461028903));
#46631=CARTESIAN_POINT('Ctrl Pts',(0.0966802994926767,1.79197528325571,
8.41151010847482));
#46632=CARTESIAN_POINT('Ctrl Pts',(0.0782485205103509,1.78678496188719,
8.41022172776056));
#46633=CARTESIAN_POINT('Ctrl Pts',(0.058344093607787,1.78304820632988,8.40894512949826));
#46634=CARTESIAN_POINT('Ctrl Pts',(0.0572235998657943,1.78284399346681,
8.40887364978822));
#46635=CARTESIAN_POINT('Ctrl Pts',(0.0557251203960356,1.78257909161456,
8.4087785922144));
#46636=CARTESIAN_POINT('Ctrl Pts',(0.0553480926923045,1.78251313292935,
8.40875472025652));
#46637=CARTESIAN_POINT('Ctrl Pts',(0.0547590036467049,1.78241115666591,
8.40871749288854));
#46638=CARTESIAN_POINT('Ctrl Pts',(0.0545470238067666,1.78237467971657,
8.40870411131649));
#46639=CARTESIAN_POINT('Ctrl Pts',(0.0541408224708725,1.78230520026609,
8.40867849709148));
#46640=CARTESIAN_POINT('Ctrl Pts',(0.0539466086350098,1.78227216386844,
8.40866626260428));
#46641=CARTESIAN_POINT('Ctrl Pts',(0.0534874977743349,1.78219450072746,
8.40863736974818));
#46642=CARTESIAN_POINT('Ctrl Pts',(0.0532225754954017,1.78215002714343,
8.40862072022937));
#46643=CARTESIAN_POINT('Ctrl Pts',(0.0526740413257244,1.78205864749855,
8.40858629285446));
#46644=CARTESIAN_POINT('Ctrl Pts',(0.0523904215075124,1.78201178953329,
8.40856851774219));
#46645=CARTESIAN_POINT('Ctrl Pts',(0.0508314461480352,1.78175636733094,
8.40847095178339));
#46646=CARTESIAN_POINT('Ctrl Pts',(0.0495548837201791,1.7815550922314,8.40839156992871));
#46647=CARTESIAN_POINT('Ctrl Pts',(0.0236233562991574,1.777626190203,8.40678874700665));
#46648=CARTESIAN_POINT('Ctrl Pts',(-0.00138522393482243,1.77676407707121,
8.40541678110286));
#46649=CARTESIAN_POINT('Ctrl Pts',(-0.0347810103223249,1.77949292861138,
8.40354215422207));
#46650=CARTESIAN_POINT('Ctrl Pts',(-0.0432842144054608,1.78053017184378,
8.40306158698686));
#46651=CARTESIAN_POINT('Ctrl Pts',(-0.0577936612301802,1.78289002405372,
8.40222543633497));
#46652=CARTESIAN_POINT('Ctrl Pts',(-0.0638219180456825,1.78404810238222,
8.40187320858196));
#46653=CARTESIAN_POINT('Ctrl Pts',(-0.072535324184587,1.78598156579259,
8.40135441934715));
#46654=CARTESIAN_POINT('Ctrl Pts',(-0.0752494111104413,1.78662087531697,
8.40119144936464));
#46655=CARTESIAN_POINT('Ctrl Pts',(-0.079838386749779,1.78776487067895,
8.40091332266734));
#46656=CARTESIAN_POINT('Ctrl Pts',(-0.0817176553062199,1.78825143373672,
8.40079868626428));
#46657=CARTESIAN_POINT('Ctrl Pts',(-0.088992108317433,1.7902051639539,8.4003519056634));
#46658=CARTESIAN_POINT('Ctrl Pts',(-0.0943529026362266,1.79179558779443,
8.40001613091516));
#46659=CARTESIAN_POINT('Ctrl Pts',(-0.100596184668807,1.7938259758455,8.39961642189194));
#46660=CARTESIAN_POINT('Ctrl Pts',(-0.101521608472813,1.79413158316484,
8.39955694895443));
#46661=CARTESIAN_POINT('Ctrl Pts',(-0.102918198846199,1.79459982252448,
8.39946685033177));
#46662=CARTESIAN_POINT('Ctrl Pts',(-0.103390403441528,1.79475935963963,
8.39943632692282));
#46663=CARTESIAN_POINT('Ctrl Pts',(-0.104233935602673,1.79504653392846,
8.399381692835));
#46664=CARTESIAN_POINT('Ctrl Pts',(-0.10460540436797,1.79517375576385,8.39935759594498));
#46665=CARTESIAN_POINT('Ctrl Pts',(-0.105390164036805,1.79544412622543,
8.3993066094367));
#46666=CARTESIAN_POINT('Ctrl Pts',(-0.105803397573905,1.79558743786579,
8.39927971445341));
#46667=CARTESIAN_POINT('Ctrl Pts',(-0.106642644603475,1.7958804086175,8.3992249969192));
#46668=CARTESIAN_POINT('Ctrl Pts',(-0.107068637754152,1.79603012268181,
8.39919717259082));
#46669=CARTESIAN_POINT('Ctrl Pts',(-0.108917066695695,1.79668411543232,
8.39907622029489));
#46670=CARTESIAN_POINT('Ctrl Pts',(-0.11033624690742,1.79719748062028,8.3989827904266));
#46671=CARTESIAN_POINT('Ctrl Pts',(-0.113762990340338,1.7984643377506,8.39875580114505));
#46672=CARTESIAN_POINT('Ctrl Pts',(-0.115766719405575,1.79922792699545,
8.39862190716099));
#46673=CARTESIAN_POINT('Ctrl Pts',(-0.123165075515661,1.80213220426508,
8.3981231198733));
#46674=CARTESIAN_POINT('Ctrl Pts',(-0.128508934187481,1.80439839912792,
8.39775406462739));
#46675=CARTESIAN_POINT('Ctrl Pts',(-0.142785921160656,1.81091321740087,
8.3967436828037));
#46676=CARTESIAN_POINT('Ctrl Pts',(-0.151588901810466,1.81543056617613,
8.39609401549238));
#46677=CARTESIAN_POINT('Ctrl Pts',(-0.167330418135048,1.82444636903274,
8.39488538772586));
#46678=CARTESIAN_POINT('Ctrl Pts',(-0.174330754932642,1.8288209983483,8.3943297014222));
#46679=CARTESIAN_POINT('Ctrl Pts',(-0.200266671530347,1.84644842700787,
8.39220992213573));
#46680=CARTESIAN_POINT('Ctrl Pts',(-0.217927563232293,1.86145663900082,
8.3906327048897));
#46681=CARTESIAN_POINT('Ctrl Pts',(-0.234696034382311,1.87913686989421,
8.38909498778569));
#46682=CARTESIAN_POINT('Ctrl Pts',(-0.235554393265944,1.88005255461656,
8.38901616330019));
#46683=CARTESIAN_POINT('Ctrl Pts',(-0.236677776230974,1.88126508249625,
8.38891288304588));
#46684=CARTESIAN_POINT('Ctrl Pts',(-0.236947616132483,1.88155741919167,
8.3888880657537));
#46685=CARTESIAN_POINT('Ctrl Pts',(-0.237364572506812,1.88201081924435,
8.38884970508989));
#46686=CARTESIAN_POINT('Ctrl Pts',(-0.23751206674639,1.88217153225899,8.38883613284982));
#46687=CARTESIAN_POINT('Ctrl Pts',(-0.23780544369527,1.88249185456545,8.38880913184293));
#46688=CARTESIAN_POINT('Ctrl Pts',(-0.23795132789488,1.88265145978188,8.3887957030185));
#46689=CARTESIAN_POINT('Ctrl Pts',(-0.238280542499722,1.883012367121,8.38876539296139));
#46690=CARTESIAN_POINT('Ctrl Pts',(-0.238463778095125,1.88321375437011,
8.38874851901017));
#46691=CARTESIAN_POINT('Ctrl Pts',(-0.238843356330097,1.88363199788749,
8.38871355548009));
#46692=CARTESIAN_POINT('Ctrl Pts',(-0.239039659474542,1.88384888989162,
8.3886954688972));
#46693=CARTESIAN_POINT('Ctrl Pts',(-0.239551123299324,1.88441554645347,
8.38864833118855));
#46694=CARTESIAN_POINT('Ctrl Pts',(-0.239865814738414,1.88476573643738,
8.38861931507781));
#46695=CARTESIAN_POINT('Ctrl Pts',(-0.243518763967195,1.88884871570301,
8.38828232115739));
#46696=CARTESIAN_POINT('Ctrl Pts',(-0.246770572182945,1.89265838646294,
8.3879806374866));
#46697=CARTESIAN_POINT('Ctrl Pts',(-0.257529154300123,1.90587451144742,
8.38697045727812));
#46698=CARTESIAN_POINT('Ctrl Pts',(-0.264597929459058,1.91562549457053,
8.38628549334185));
#46699=CARTESIAN_POINT('Ctrl Pts',(-0.273707122562489,1.92979793258131,
8.38533767482097));
#46700=CARTESIAN_POINT('Ctrl Pts',(-0.27621804062337,1.93390386019887,8.38506836014099));
#46701=CARTESIAN_POINT('Ctrl Pts',(-0.281201868151471,1.94247933827735,
8.38451379867739));
#46702=CARTESIAN_POINT('Ctrl Pts',(-0.283662348445672,1.9469545121841,8.38422866279686));
#46703=CARTESIAN_POINT('Ctrl Pts',(-0.296649314992381,1.97196548136546,
8.38265011148892));
#46704=CARTESIAN_POINT('Ctrl Pts',(-0.305051293354224,1.99352403315218,
8.38133791330004));
#46705=CARTESIAN_POINT('Ctrl Pts',(-0.311458891657275,2.01719514329423,
8.37985002401901));
#46706=CARTESIAN_POINT('Ctrl Pts',(-0.311828935184469,2.01859975085764,
8.37976159215863));
#46707=CARTESIAN_POINT('Ctrl Pts',(-0.3123226726781,2.02052666006364,8.37964006625184));
#46708=CARTESIAN_POINT('Ctrl Pts',(-0.312454579989572,2.02104685524011,
8.37960723773207));
#46709=CARTESIAN_POINT('Ctrl Pts',(-0.312677237688357,2.0219342346737,8.37955120031392));
#46710=CARTESIAN_POINT('Ctrl Pts',(-0.312768642430599,2.02230125487148,
8.37952801257533));
#46711=CARTESIAN_POINT('Ctrl Pts',(-0.312944483596293,2.02301265339138,
8.37948304659252));
#46712=CARTESIAN_POINT('Ctrl Pts',(-0.313028998241659,2.02335701200079,
8.3794612709058));
#46713=CARTESIAN_POINT('Ctrl Pts',(-0.313228666596841,2.02417640888751,
8.37940943298678));
#46714=CARTESIAN_POINT('Ctrl Pts',(-0.313343307958032,2.0246515700166,8.37937935429695));
#46715=CARTESIAN_POINT('Ctrl Pts',(-0.3135784583592,2.02563603032065,8.37931699724269));
#46716=CARTESIAN_POINT('Ctrl Pts',(-0.313698808584223,2.02614536560879,
8.37928471385741));
#46717=CARTESIAN_POINT('Ctrl Pts',(-0.314008906526423,2.02747216738436,
8.37920055996129));
#46718=CARTESIAN_POINT('Ctrl Pts',(-0.314196701951677,2.02829008197489,
8.37914862680255));
#46719=CARTESIAN_POINT('Ctrl Pts',(-0.319650775055618,2.05247723809825,
8.37761117391605));
#46720=CARTESIAN_POINT('Ctrl Pts',(-0.322297014532377,2.07635434457231,
8.37603790742453));
#46721=CARTESIAN_POINT('Ctrl Pts',(-0.322274862071682,2.10029816384487,
8.37442397213274));
#46722=CARTESIAN_POINT('',(-0.322758995413397,2.09993443928603,8.24935848523156));
#46723=CARTESIAN_POINT('Ctrl Pts',(-0.322791832858883,2.09993556662301,
8.24937734492731));
#46724=CARTESIAN_POINT('Ctrl Pts',(-0.322801292110665,2.09647160517377,
8.24959213483258));
#46725=CARTESIAN_POINT('Ctrl Pts',(-0.321180065660157,1.98619899400209,
8.25643037257877));
#46726=CARTESIAN_POINT('Ctrl Pts',(-0.195796246402531,1.77307658662262,
8.2698920581659));
#46727=CARTESIAN_POINT('Ctrl Pts',(0.168895013338677,1.75840145962115,8.2897624016887));
#46728=CARTESIAN_POINT('Ctrl Pts',(0.378648091321469,2.05709648897531,8.30963274521149));
#46729=CARTESIAN_POINT('Ctrl Pts',(0.24104309379967,2.39514964890902,8.32950308873427));
#46730=CARTESIAN_POINT('Ctrl Pts',(-0.117686127229278,2.46244318696509,
8.34937343225707));
#46731=CARTESIAN_POINT('Ctrl Pts',(-0.306460346708295,2.26280590555498,
8.36433150221144));
#46732=CARTESIAN_POINT('Ctrl Pts',(-0.322442531075311,2.12802537045353,
8.37266612432489));
#46733=CARTESIAN_POINT('Ctrl Pts',(-0.322193764531691,2.10029569746695,
8.37437729859741));
#46734=CARTESIAN_POINT('',(-0.322274935754178,2.10020349358851,7.99961864007736));
#46735=CARTESIAN_POINT('Ctrl Pts',(-0.32227498952282,2.09991782295878,8.24908050368635));
#46736=CARTESIAN_POINT('Ctrl Pts',(-0.322282430347236,2.12909862059907,
8.24731739895166));
#46737=CARTESIAN_POINT('Ctrl Pts',(-0.318326636673908,2.15815172661552,
8.24574482695574));
#46738=CARTESIAN_POINT('Ctrl Pts',(-0.306877789527729,2.19935460858732,
8.24333071811698));
#46739=CARTESIAN_POINT('Ctrl Pts',(-0.302423067387966,2.2121853311125,8.24255263359147));
#46740=CARTESIAN_POINT('Ctrl Pts',(-0.294911155652155,2.23008754209254,
8.2414018613405));
#46741=CARTESIAN_POINT('Ctrl Pts',(-0.292502791452486,2.23541590989614,
8.24105080179699));
#46742=CARTESIAN_POINT('Ctrl Pts',(-0.289546968746822,2.24150825083486,
8.24063833070744));
#46743=CARTESIAN_POINT('Ctrl Pts',(-0.289139401550848,2.24233916751049,
8.24058183290494));
#46744=CARTESIAN_POINT('Ctrl Pts',(-0.288514333431861,2.24359974558511,
8.24049574742057));
#46745=CARTESIAN_POINT('Ctrl Pts',(-0.288299436856062,2.24403069892286,
8.24046625083573));
#46746=CARTESIAN_POINT('Ctrl Pts',(-0.287925047383808,2.244777304119,8.24041503323732));
#46747=CARTESIAN_POINT('Ctrl Pts',(-0.287765998899282,2.24509317893973,
8.240393327835));
#46748=CARTESIAN_POINT('Ctrl Pts',(-0.287434350113652,2.24574915251239,
8.24034817691505));
#46749=CARTESIAN_POINT('Ctrl Pts',(-0.287261665464136,2.24608920780181,
8.24032472845817));
#46750=CARTESIAN_POINT('Ctrl Pts',(-0.286839322200057,2.2469172533412,8.24026752707046));
#46751=CARTESIAN_POINT('Ctrl Pts',(-0.286589022089496,2.24740491342343,
8.24023375158812));
#46752=CARTESIAN_POINT('Ctrl Pts',(-0.285636487836732,2.2492491402012,8.24010568470052));
#46753=CARTESIAN_POINT('Ctrl Pts',(-0.284925864602599,2.2506013299609,8.24001109740566));
#46754=CARTESIAN_POINT('Ctrl Pts',(-0.283921320898047,2.25248023763483,
8.23987868891264));
#46755=CARTESIAN_POINT('Ctrl Pts',(-0.28363548624749,2.25301127495336,8.23984115664337));
#46756=CARTESIAN_POINT('Ctrl Pts',(-0.266787156679002,2.28410347563907,
8.23763718284402));
#46757=CARTESIAN_POINT('Ctrl Pts',(-0.245393290271939,2.31177894559571,
8.23527113764941));
#46758=CARTESIAN_POINT('Ctrl Pts',(-0.213954374122118,2.34114993382704,
8.23237726724694));
#46759=CARTESIAN_POINT('Ctrl Pts',(-0.207686493921321,2.34656865521063,
8.23182484419027));
#46760=CARTESIAN_POINT('Ctrl Pts',(-0.197755079015446,2.35450685665233,
8.23099389648358));
#46761=CARTESIAN_POINT('Ctrl Pts',(-0.194236806860526,2.35720201897057,
8.23070755889719));
#46762=CARTESIAN_POINT('Ctrl Pts',(-0.189466740624686,2.36070238721776,
8.23033109808522));
#46763=CARTESIAN_POINT('Ctrl Pts',(-0.188263517250055,2.36157260707121,
8.23023711172103));
#46764=CARTESIAN_POINT('Ctrl Pts',(-0.186510893398122,2.36282181715218,
8.23010166601934));
#46765=CARTESIAN_POINT('Ctrl Pts',(-0.185966283356383,2.36320745126316,
8.23005977944542));
#46766=CARTESIAN_POINT('Ctrl Pts',(-0.185115629236839,2.3638058345674,8.22999467353943));
#46767=CARTESIAN_POINT('Ctrl Pts',(-0.184810411062298,2.36401974643168,
8.22997137695607));
#46768=CARTESIAN_POINT('Ctrl Pts',(-0.184298652055851,2.36437708997849,
8.22993242306291));
#46769=CARTESIAN_POINT('Ctrl Pts',(-0.184092314192659,2.36452080959975,
8.22991674628231));
#46770=CARTESIAN_POINT('Ctrl Pts',(-0.183689281966663,2.36480083191344,
8.229886182628));
#46771=CARTESIAN_POINT('Ctrl Pts',(-0.183492603645741,2.36493715726504,
8.22987129420697));
#46772=CARTESIAN_POINT('Ctrl Pts',(-0.183119949541493,2.36519484421937,
8.22984313501947));
#46773=CARTESIAN_POINT('Ctrl Pts',(-0.182944006291985,2.36531624881019,
8.22982986136353));
#46774=CARTESIAN_POINT('Ctrl Pts',(-0.182537022179148,2.36559647919987,
8.22979920632851));
#46775=CARTESIAN_POINT('Ctrl Pts',(-0.182305895074204,2.36575517841054,
8.22978183368115));
#46776=CARTESIAN_POINT('Ctrl Pts',(-0.181599608315366,2.3662387823416,8.22972885579778));
#46777=CARTESIAN_POINT('Ctrl Pts',(-0.181123781750677,2.36656271805986,
8.22969331637367));
#46778=CARTESIAN_POINT('Ctrl Pts',(-0.177661502568308,2.36890623587703,
8.22943580027706));
#46779=CARTESIAN_POINT('Ctrl Pts',(-0.174642067099587,2.37087695404254,
8.22921704965939));
#46780=CARTESIAN_POINT('Ctrl Pts',(-0.170435880374202,2.37352265983096,
8.22891933706323));
#46781=CARTESIAN_POINT('Ctrl Pts',(-0.169277100534252,2.37424131365929,
8.22883803919112));
#46782=CARTESIAN_POINT('Ctrl Pts',(-0.156516338341294,2.38204360353047,
8.22795023944417));
#46783=CARTESIAN_POINT('Ctrl Pts',(-0.144480681022667,2.38839445779987,
8.22717997714227));
#46784=CARTESIAN_POINT('Ctrl Pts',(-0.120292574008706,2.39926214379793,
8.22569196139057));
#46785=CARTESIAN_POINT('Ctrl Pts',(-0.108198631363857,2.40384401985012,
8.22497475516177));
#46786=CARTESIAN_POINT('Ctrl Pts',(-0.0828192209699291,2.41175116422438,
8.22347450226434));
#46787=CARTESIAN_POINT('Ctrl Pts',(-0.0695321839170615,2.41498100032869,
8.22269142277447));
#46788=CARTESIAN_POINT('Ctrl Pts',(-0.0503041495783892,2.41837883784802,
8.22153414787132));
#46789=CARTESIAN_POINT('Ctrl Pts',(-0.0445006331968898,2.41924172464982,
8.22118191122227));
#46790=CARTESIAN_POINT('Ctrl Pts',(-0.0377574753976918,2.42005688039645,
8.2207681801342));
#46791=CARTESIAN_POINT('Ctrl Pts',(-0.036837413269538,2.42016408073518,
8.22071163403207));
#46792=CARTESIAN_POINT('Ctrl Pts',(-0.0354381805681159,2.42032100000866,
8.22062548989499));
#46793=CARTESIAN_POINT('Ctrl Pts',(-0.0349593341849089,2.42037361414115,
8.22059598314825));
#46794=CARTESIAN_POINT('Ctrl Pts',(-0.0341287258698034,2.42046299440585,
8.22054475417693));
#46795=CARTESIAN_POINT('Ctrl Pts',(-0.0337770171093503,2.42050025557971,
8.22052304758494));
#46796=CARTESIAN_POINT('Ctrl Pts',(-0.033045992419723,2.42057648605206,
8.2204779002501));
#46797=CARTESIAN_POINT('Ctrl Pts',(-0.032666667409429,2.42061536123977,
8.22045445657863));
#46798=CARTESIAN_POINT('Ctrl Pts',(-0.0317421644739875,2.42070845136719,
8.2203972772143));
#46799=CARTESIAN_POINT('Ctrl Pts',(-0.0311969170151554,2.42076194934353,
8.22036351900591));
#46800=CARTESIAN_POINT('Ctrl Pts',(-0.0291327553487398,2.42095916554851,
8.22023558393343));
#46801=CARTESIAN_POINT('Ctrl Pts',(-0.0276129823642547,2.42109348554627,
8.22014111195705));
#46802=CARTESIAN_POINT('Ctrl Pts',(-0.0254893632654973,2.42126598630649,
8.22000870341162));
#46803=CARTESIAN_POINT('Ctrl Pts',(-0.0248862595631177,2.42131326719275,
8.21997105461301));
#46804=CARTESIAN_POINT('Ctrl Pts',(0.0112130011942717,2.42404105707372,
8.2177148314453));
#46805=CARTESIAN_POINT('Ctrl Pts',(0.0469020093077426,2.42082262785708,
8.21528545039867));
#46806=CARTESIAN_POINT('Ctrl Pts',(0.088677716470874,2.40992761333734,8.21238663493858));
#46807=CARTESIAN_POINT('Ctrl Pts',(0.0959575043947503,2.40775157817024,
8.21188109144788));
#46808=CARTESIAN_POINT('Ctrl Pts',(0.107255482601194,2.40393449878442,8.21110226414418));
#46809=CARTESIAN_POINT('Ctrl Pts',(0.111328869481974,2.40246620471191,8.21082268367161));
#46810=CARTESIAN_POINT('Ctrl Pts',(0.11673492184586,2.4003935175192,8.21045440107374));
#46811=CARTESIAN_POINT('Ctrl Pts',(0.118094660862702,2.39986156573622,8.21036200751817));
#46812=CARTESIAN_POINT('Ctrl Pts',(0.120062896011062,2.39907609567392,8.21022866115198));
#46813=CARTESIAN_POINT('Ctrl Pts',(0.120674280771127,2.39882993153351,8.2101872958129));
#46814=CARTESIAN_POINT('Ctrl Pts',(0.121627187826496,2.39844285766162,8.2101229151703));
#46815=CARTESIAN_POINT('Ctrl Pts',(0.12196922604661,2.39830323499525,8.2100998247213));
#46816=CARTESIAN_POINT('Ctrl Pts',(0.122542406888266,2.3980681074612,8.21006116210491));
#46817=CARTESIAN_POINT('Ctrl Pts',(0.122773678705264,2.39797292157115,8.210045570911));
#46818=CARTESIAN_POINT('Ctrl Pts',(0.123225130344947,2.39778650016235,8.21001515366888));
#46819=CARTESIAN_POINT('Ctrl Pts',(0.123445320152582,2.3976952894501,8.21000032613019));
#46820=CARTESIAN_POINT('Ctrl Pts',(0.123863081242261,2.39752169425319,8.20997220981573));
#46821=CARTESIAN_POINT('Ctrl Pts',(0.124060670004641,2.39743935786033,8.2099589183064));
#46822=CARTESIAN_POINT('Ctrl Pts',(0.124518514364245,2.39724803584759,8.20992813506939));
#46823=CARTESIAN_POINT('Ctrl Pts',(0.124778708661678,2.39713890539765,8.20991065230337));
#46824=CARTESIAN_POINT('Ctrl Pts',(0.125577592158592,2.39680260403766,8.20985700853089));
#46825=CARTESIAN_POINT('Ctrl Pts',(0.126115810589976,2.39657430729546,8.20982091578144));
#46826=CARTESIAN_POINT('Ctrl Pts',(0.130144483554119,2.39485251023115,8.20955109117706));
#46827=CARTESIAN_POINT('Ctrl Pts',(0.133609106145702,2.3932988223843,8.20932094199588));
#46828=CARTESIAN_POINT('Ctrl Pts',(0.152805736639994,2.38427942851842,8.20805202978477));
#46829=CARTESIAN_POINT('Ctrl Pts',(0.167941785555306,2.3756085821367,8.20707444435108));
#46830=CARTESIAN_POINT('Ctrl Pts',(0.198114992574998,2.35491024004541,8.20502765545664));
#46831=CARTESIAN_POINT('Ctrl Pts',(0.212925057153106,2.34267599840696,8.2039619848802));
#46832=CARTESIAN_POINT('Ctrl Pts',(0.232599103675081,2.32322846842001,8.20235533616569));
#46833=CARTESIAN_POINT('Ctrl Pts',(0.238399853019653,2.31702254170269,8.2018538756302));
#46834=CARTESIAN_POINT('Ctrl Pts',(0.245589460343964,2.30869427151331,8.20119044116371));
#46835=CARTESIAN_POINT('Ctrl Pts',(0.247208159684032,2.30677429054296,8.20103812544327));
#46836=CARTESIAN_POINT('Ctrl Pts',(0.249257867814535,2.30428460632014,8.20084133573812));
#46837=CARTESIAN_POINT('Ctrl Pts',(0.249709679740041,2.30373208112137,8.20079770805883));
#46838=CARTESIAN_POINT('Ctrl Pts',(0.250434072073226,2.30284018497108,8.20072735375276));
#46839=CARTESIAN_POINT('Ctrl Pts',(0.250707808612591,2.30250175256527,8.20070067381655));
#46840=CARTESIAN_POINT('Ctrl Pts',(0.251227438767591,2.30185664257161,8.20064984755564));
#46841=CARTESIAN_POINT('Ctrl Pts',(0.251473458767252,2.30155006741121,8.20062570637293));
#46842=CARTESIAN_POINT('Ctrl Pts',(0.252032491148034,2.3008508182728,8.20057067318188));
#46843=CARTESIAN_POINT('Ctrl Pts',(0.252345147304278,2.30045786196248,8.2005397669895));
#46844=CARTESIAN_POINT('Ctrl Pts',(0.253272695351611,2.29928648085921,8.20044769783543));
#46845=CARTESIAN_POINT('Ctrl Pts',(0.253884908760411,2.29850595137779,8.20038642833549));
#46846=CARTESIAN_POINT('Ctrl Pts',(0.25812838953016,2.29304406585205,8.19995821605619));
#46847=CARTESIAN_POINT('Ctrl Pts',(0.261633359894596,2.28826644499301,8.19958632657241));
#46848=CARTESIAN_POINT('Ctrl Pts',(0.266128018919764,2.28177170073543,8.19908381024595));
#46849=CARTESIAN_POINT('Ctrl Pts',(0.267236582505666,2.28013795363976,8.1989576538504));
#46850=CARTESIAN_POINT('Ctrl Pts',(0.270249866876016,2.2756080868366,8.19860854117602));
#46851=CARTESIAN_POINT('Ctrl Pts',(0.272122942380612,2.27269132444765,8.19838450162629));
#46852=CARTESIAN_POINT('Ctrl Pts',(0.289230961540432,2.2450809847847,8.19627088781002));
#46853=CARTESIAN_POINT('Ctrl Pts',(0.301111610925658,2.21846690481955,8.19426949047631));
#46854=CARTESIAN_POINT('Ctrl Pts',(0.311923591539632,2.18157173735003,8.19171311728566));
#46855=CARTESIAN_POINT('Ctrl Pts',(0.314179134753239,2.17240016469395,8.19109592334484));
#46856=CARTESIAN_POINT('Ctrl Pts',(0.316211087159561,2.16223012552566,8.19044070508896));
#46857=CARTESIAN_POINT('Ctrl Pts',(0.316389315880017,2.16131754244665,8.19038216683029));
#46858=CARTESIAN_POINT('Ctrl Pts',(0.316652326023318,2.15993917052633,8.19029414957183));
#46859=CARTESIAN_POINT('Ctrl Pts',(0.316740032926459,2.15947395470129,8.19026451130572));
#46860=CARTESIAN_POINT('Ctrl Pts',(0.316880476768539,2.15871988828576,8.19021658363558));
#46861=CARTESIAN_POINT('Ctrl Pts',(0.316933844216575,2.15843115803301,8.19019825903072));
#46862=CARTESIAN_POINT('Ctrl Pts',(0.31703540988877,2.15787743123977,8.19016316798674));
#46863=CARTESIAN_POINT('Ctrl Pts',(0.317083670608547,2.15761244661475,8.190146398014));
#46864=CARTESIAN_POINT('Ctrl Pts',(0.317169668282853,2.15713687876541,8.19011634216466));
#46865=CARTESIAN_POINT('Ctrl Pts',(0.317207527694683,2.15692631876811,8.19010304929872));
#46866=CARTESIAN_POINT('Ctrl Pts',(0.317288784254605,2.15647180188791,8.19007438657624));
#46867=CARTESIAN_POINT('Ctrl Pts',(0.317332109607858,2.15622783327722,8.19005902089588));
#46868=CARTESIAN_POINT('Ctrl Pts',(0.31744850067743,2.1555680062489,8.19001751554603));
#46869=CARTESIAN_POINT('Ctrl Pts',(0.317521030905066,2.1551520519893,8.18999140645455));
#46870=CARTESIAN_POINT('Ctrl Pts',(0.317840945335316,2.15329582230688,8.18987513669094));
#46871=CARTESIAN_POINT('Ctrl Pts',(0.318079353906188,2.15185398746005,8.18978547906446));
#46872=CARTESIAN_POINT('Ctrl Pts',(0.32260526546391,2.12327596818615,8.1880204851893));
#46873=CARTESIAN_POINT('Ctrl Pts',(0.323416104845217,2.09569820721821,8.18652600070428));
#46874=CARTESIAN_POINT('Ctrl Pts',(0.318553053376049,2.04642250939486,8.1837467977001));
#46875=CARTESIAN_POINT('Ctrl Pts',(0.314147029591894,2.02478020232096,8.18248670981023));
#46876=CARTESIAN_POINT('Ctrl Pts',(0.307226595764991,2.00266393809037,8.18107747313594));
#46877=CARTESIAN_POINT('Ctrl Pts',(0.306878379555554,2.00157159860289,8.18100756323167));
#46878=CARTESIAN_POINT('Ctrl Pts',(0.306362069825668,1.99998133199268,8.18090533009312));
#46879=CARTESIAN_POINT('Ctrl Pts',(0.306198572630702,1.9994819126148,8.18087315825076));
#46880=CARTESIAN_POINT('Ctrl Pts',(0.305909624303154,1.99860653637977,8.18081665151407));
#46881=CARTESIAN_POINT('Ctrl Pts',(0.305784699456504,1.99823040590516,8.1807923340269));
#46882=CARTESIAN_POINT('Ctrl Pts',(0.305540882254735,1.99750080990798,8.18074509068159));
#46883=CARTESIAN_POINT('Ctrl Pts',(0.305422069525533,1.99714731824864,8.18072216748626));
#46884=CARTESIAN_POINT('Ctrl Pts',(0.305137095528242,1.99630431160062,8.18066741957006));
#46885=CARTESIAN_POINT('Ctrl Pts',(0.304970369868646,1.99581498976703,8.18063557620863));
#46886=CARTESIAN_POINT('Ctrl Pts',(0.304463108990381,1.99433788488598,8.18053925353634));
#46887=CARTESIAN_POINT('Ctrl Pts',(0.304118949211372,1.99335136195992,8.18047465418788));
#46888=CARTESIAN_POINT('Ctrl Pts',(0.300444621649078,1.98298144091922,8.17979275631169));
#46889=CARTESIAN_POINT('Ctrl Pts',(0.296686435758453,1.97375643593979,8.17916120911585));
#46890=CARTESIAN_POINT('Ctrl Pts',(0.291548250891119,1.9626463792024,8.17836830118015));
#46891=CARTESIAN_POINT('Ctrl Pts',(0.290566802905679,1.96058216610798,8.17821958031863));
#46892=CARTESIAN_POINT('Ctrl Pts',(0.277211063063621,1.9332456522401,8.17623148089844));
#46893=CARTESIAN_POINT('Ctrl Pts',(0.261600538370055,1.90969027660268,8.17429055103117));
#46894=CARTESIAN_POINT('Ctrl Pts',(0.237084450394834,1.88151177172715,8.171809207549));
#46895=CARTESIAN_POINT('Ctrl Pts',(0.230737899374581,1.8748196292276,8.17120703853088));
#46896=CARTESIAN_POINT('Ctrl Pts',(0.223453371006296,1.86777035515342,8.17056672611689));
#46897=CARTESIAN_POINT('Ctrl Pts',(0.222791496618811,1.86713530529249,8.17050898658756));
#46898=CARTESIAN_POINT('Ctrl Pts',(0.221787294950725,1.86618000269019,8.1704220576152));
#46899=CARTESIAN_POINT('Ctrl Pts',(0.221446972184405,1.86585766324651,8.17039271348946));
#46900=CARTESIAN_POINT('Ctrl Pts',(0.220893746145429,1.8653359558628,8.1703452015258));
#46901=CARTESIAN_POINT('Ctrl Pts',(0.220681274887295,1.86513613387177,8.17032699930655));
#46902=CARTESIAN_POINT('Ctrl Pts',(0.220273084224832,1.86475328738924,8.17029211704908));
#46903=CARTESIAN_POINT('Ctrl Pts',(0.22007740739198,1.86457021814357,8.17027543357961));
#46904=CARTESIAN_POINT('Ctrl Pts',(0.219725106838865,1.86424143958026,8.17024546540707));
#46905=CARTESIAN_POINT('Ctrl Pts',(0.219568566644015,1.86409564241125,8.17023217391268));
#46906=CARTESIAN_POINT('Ctrl Pts',(0.219229658710669,1.86378062259873,8.17020345092515));
#46907=CARTESIAN_POINT('Ctrl Pts',(0.219047240663644,1.8636114556987,8.17018802374208));
#46908=CARTESIAN_POINT('Ctrl Pts',(0.218551413995459,1.86315271345567,8.17014618044394));
#46909=CARTESIAN_POINT('Ctrl Pts',(0.218237624455327,1.86286354776227,8.17011979576643));
#46910=CARTESIAN_POINT('Ctrl Pts',(0.216816627321655,1.86155926922216,8.17000074224138));
#46911=CARTESIAN_POINT('Ctrl Pts',(0.215702882059124,1.86055126048716,8.16990860632842));
#46912=CARTESIAN_POINT('Ctrl Pts',(0.190642664679395,1.83818695302956,8.16786049859883));
#46913=CARTESIAN_POINT('Ctrl Pts',(0.163642520815101,1.82051361250132,8.16614774592186));
#46914=CARTESIAN_POINT('Ctrl Pts',(0.120255612203987,1.80059316440985,8.16344111173404));
#46915=CARTESIAN_POINT('Ctrl Pts',(0.105585315746141,1.79511065825562,8.16253527455687));
#46916=CARTESIAN_POINT('Ctrl Pts',(0.0882067855719214,1.79002123579892,
8.16144308098317));
#46917=CARTESIAN_POINT('Ctrl Pts',(0.0858295223003822,1.78935460110477,
8.1612933100735));
#46918=CARTESIAN_POINT('Ctrl Pts',(0.0827596812450026,1.78853168054126,
8.16109935925991));
#46919=CARTESIAN_POINT('Ctrl Pts',(0.0820738781155888,1.78835026490526,
8.16105599573748));
#46920=CARTESIAN_POINT('Ctrl Pts',(0.0809672549164702,1.78806143572786,
8.16098596549095));
#46921=CARTESIAN_POINT('Ctrl Pts',(0.0805468043056365,1.78795260526308,
8.16095934467981));
#46922=CARTESIAN_POINT('Ctrl Pts',(0.0797451844850896,1.78774684010737,
8.16090856392216));
#46923=CARTESIAN_POINT('Ctrl Pts',(0.0793640550229795,1.78764975255392,
8.16088440896934));
#46924=CARTESIAN_POINT('Ctrl Pts',(0.0784941550613436,1.78742985231104,
8.1608292508983));
#46925=CARTESIAN_POINT('Ctrl Pts',(0.0780052731810009,1.78730748816697,
8.16079823335736));
#46926=CARTESIAN_POINT('Ctrl Pts',(0.076511424768566,1.78693730839166,8.16070339620407));
#46927=CARTESIAN_POINT('Ctrl Pts',(0.0755055569837382,1.78669318899565,
8.16063945760279));
#46928=CARTESIAN_POINT('Ctrl Pts',(0.0681265068171763,1.78493992687024,
8.16016978888479));
#46929=CARTESIAN_POINT('Ctrl Pts',(0.0617102148068972,1.78362062353308,
8.15975799494796));
#46930=CARTESIAN_POINT('Ctrl Pts',(0.0534642928833599,1.78218549140897,
8.15922390417348));
#46931=CARTESIAN_POINT('Ctrl Pts',(0.0516674542015662,1.78188843710115,
8.1591072326862));
#46932=CARTESIAN_POINT('Ctrl Pts',(0.0477904624977187,1.78128120496461,
8.15885486773092));
#46933=CARTESIAN_POINT('Ctrl Pts',(0.0457096048281793,1.78097612890661,
8.15871903149516));
#46934=CARTESIAN_POINT('Ctrl Pts',(0.0411466172690072,1.78035270479501,
8.1584203269715));
#46935=CARTESIAN_POINT('Ctrl Pts',(0.0386634778724025,1.78004285845777,
8.15825723348964));
#46936=CARTESIAN_POINT('Ctrl Pts',(0.0111390565423589,1.77693344692627,
8.15644364292251));
#46937=CARTESIAN_POINT('Ctrl Pts',(-0.0141430083672298,1.77705140828866,
8.15471514715824));
#46938=CARTESIAN_POINT('Ctrl Pts',(-0.0479516692891071,1.78118897656373,
8.15243536489083));
#46939=CARTESIAN_POINT('Ctrl Pts',(-0.0567073223628983,1.78262933894312,
8.15184895715194));
#46940=CARTESIAN_POINT('Ctrl Pts',(-0.069184241786332,1.78521482453982,
8.1510287848672));
#46941=CARTESIAN_POINT('Ctrl Pts',(-0.0729611889849623,1.78606874282712,
8.15078258998365));
#46942=CARTESIAN_POINT('Ctrl Pts',(-0.0772453047936734,1.78711882642643,
8.1505064251594));
#46943=CARTESIAN_POINT('Ctrl Pts',(-0.0777682591425823,1.7872483992537,
8.15047276697869));
#46944=CARTESIAN_POINT('Ctrl Pts',(-0.0785556144877188,1.78744557988833,
8.15042217364282));
#46945=CARTESIAN_POINT('Ctrl Pts',(-0.0788202552489524,1.7875122122983,
8.15040518253307));
#46946=CARTESIAN_POINT('Ctrl Pts',(-0.0792964180697469,1.78763274603034,
8.15037463636519));
#46947=CARTESIAN_POINT('Ctrl Pts',(-0.079507969536768,1.78768652598338,
8.15036107431972));
#46948=CARTESIAN_POINT('Ctrl Pts',(-0.0799624435325836,1.78780255264627,
8.15033195878021));
#46949=CARTESIAN_POINT('Ctrl Pts',(-0.0802053473558922,1.7878648677793,
8.15031640936243));
#46950=CARTESIAN_POINT('Ctrl Pts',(-0.0808592968577339,1.78803344732757,
8.15027457878565));
#46951=CARTESIAN_POINT('Ctrl Pts',(-0.0812702074912553,1.78814024104756,
8.15024832831689));
#46952=CARTESIAN_POINT('Ctrl Pts',(-0.0831599327597951,1.78863536024943,
8.15012775662798));
#46953=CARTESIAN_POINT('Ctrl Pts',(-0.0846362147561983,1.78903340264228,
8.15003398958839));
#46954=CARTESIAN_POINT('Ctrl Pts',(-0.114063074932086,1.79719270285057,
8.1481724075239));
#46955=CARTESIAN_POINT('Ctrl Pts',(-0.140847299161554,1.80868348236693,
8.14660467575085));
#46956=CARTESIAN_POINT('Ctrl Pts',(-0.182698745868446,1.83377905825848,
8.14385781834547));
#46957=CARTESIAN_POINT('Ctrl Pts',(-0.198687528647069,1.84548965676049,
8.14272136036028));
#46958=CARTESIAN_POINT('Ctrl Pts',(-0.214697610556417,1.85964887455668,
8.14142555104108));
#46959=CARTESIAN_POINT('Ctrl Pts',(-0.215886326524282,1.86071602360955,
8.14132833572421));
#46960=CARTESIAN_POINT('Ctrl Pts',(-0.2175113569342,1.86219683229,8.14119402579213));
#46961=CARTESIAN_POINT('Ctrl Pts',(-0.217954534668935,1.86260295330861,
8.14115725058547));
#46962=CARTESIAN_POINT('Ctrl Pts',(-0.218698488379157,1.86328853983879,
8.14109526876992));
#46963=CARTESIAN_POINT('Ctrl Pts',(-0.218999872467176,1.86356734563968,
8.14107009031381));
#46964=CARTESIAN_POINT('Ctrl Pts',(-0.219593472460228,1.86411858469106,
8.14102036267368));
#46965=CARTESIAN_POINT('Ctrl Pts',(-0.219885716236577,1.8643909869548,8.14099581484031));
#46966=CARTESIAN_POINT('Ctrl Pts',(-0.220526685983122,1.86499067014821,
8.1409418297588));
#46967=CARTESIAN_POINT('Ctrl Pts',(-0.220875191016659,1.86531818490239,
8.14091238248336));
#46968=CARTESIAN_POINT('Ctrl Pts',(-0.222079647546895,1.86645515709603,
8.14081028074599));
#46969=CARTESIAN_POINT('Ctrl Pts',(-0.222931880897983,1.86726852399858,
8.14073745751257));
#46970=CARTESIAN_POINT('Ctrl Pts',(-0.231382057801173,1.8754223301856,8.14000954127762));
#46971=CARTESIAN_POINT('Ctrl Pts',(-0.238618366913309,1.88312672024413,
8.13933841667321));
#46972=CARTESIAN_POINT('Ctrl Pts',(-0.246920442604891,1.89288522183672,
8.13850641880879));
#46973=CARTESIAN_POINT('Ctrl Pts',(-0.248360132130102,1.89461382539915,
8.13835970132909));
#46974=CARTESIAN_POINT('Ctrl Pts',(-0.257873263555637,1.90628232789558,
8.13737380049157));
#46975=CARTESIAN_POINT('Ctrl Pts',(-0.26536557026227,1.91668000027914,8.13651610213014));
#46976=CARTESIAN_POINT('Ctrl Pts',(-0.280651432665216,1.94080162503451,
8.13458739023784));
#46977=CARTESIAN_POINT('Ctrl Pts',(-0.288097051504079,1.9547090214577,8.13351493207316));
#46978=CARTESIAN_POINT('Ctrl Pts',(-0.297080486811537,1.97492060331028,
8.13205134394475));
#46979=CARTESIAN_POINT('Ctrl Pts',(-0.299492499852902,1.98081138886207,
8.13163562131806));
#46980=CARTESIAN_POINT('Ctrl Pts',(-0.30278123411088,1.98957502409179,8.13103672867207));
#46981=CARTESIAN_POINT('Ctrl Pts',(-0.303794713668879,1.99239458859537,
8.13084696337125));
#46982=CARTESIAN_POINT('Ctrl Pts',(-0.304933047195492,1.99570585974084,
8.1306278368916));
#46983=CARTESIAN_POINT('Ctrl Pts',(-0.305096201675618,1.996184111545,8.13059627854352));
#46984=CARTESIAN_POINT('Ctrl Pts',(-0.305343496255879,1.99691461971689,
8.13054821462114));
#46985=CARTESIAN_POINT('Ctrl Pts',(-0.305428449167943,1.99716659699316,
8.13053166111657));
#46986=CARTESIAN_POINT('Ctrl Pts',(-0.305575708059959,1.99760517118283,
8.13050289374372));
#46987=CARTESIAN_POINT('Ctrl Pts',(-0.305638154884436,1.99779171949217,
8.13049067150456));
#46988=CARTESIAN_POINT('Ctrl Pts',(-0.30577903712467,1.99821386274984,8.1304630453328));
#46989=CARTESIAN_POINT('Ctrl Pts',(-0.305857370930534,1.99844949074644,
8.13044764751152));
#46990=CARTESIAN_POINT('Ctrl Pts',(-0.306068905305321,1.99908825099524,
8.13040596560416));
#46991=CARTESIAN_POINT('Ctrl Pts',(-0.306201582284039,1.9994915580976,8.13037971254391));
#46992=CARTESIAN_POINT('Ctrl Pts',(-0.306793966947754,2.00130432947855,
8.13026199573931));
#46993=CARTESIAN_POINT('Ctrl Pts',(-0.307244752071184,2.00271672261873,
8.13017105046223));
#46994=CARTESIAN_POINT('Ctrl Pts',(-0.317329448824932,2.03508335760211,
8.12810347486102));
#46995=CARTESIAN_POINT('Ctrl Pts',(-0.3222497397889,2.06731825056121,8.12637519961379));
#46996=CARTESIAN_POINT('Ctrl Pts',(-0.322280798131405,2.10734791894266,
8.12410385700108));
#46997=CARTESIAN_POINT('Ctrl Pts',(-0.32201799756462,2.11494336341435,8.12366825587914));
#46998=CARTESIAN_POINT('Ctrl Pts',(-0.320825442818891,2.13196623469806,
8.12267392177088));
#46999=CARTESIAN_POINT('Ctrl Pts',(-0.319748057848399,2.14137581189172,
8.1221116942627));
#47000=CARTESIAN_POINT('Ctrl Pts',(-0.31807781083264,2.15185552477025,8.12146635855013));
#47001=CARTESIAN_POINT('Ctrl Pts',(-0.317891387048666,2.15298636787354,
8.12139647245469));
#47002=CARTESIAN_POINT('Ctrl Pts',(-0.317611661640599,2.15462854703028,
8.12129461521317));
#47003=CARTESIAN_POINT('Ctrl Pts',(-0.317523147365805,2.15514069860507,
8.12126279620024));
#47004=CARTESIAN_POINT('Ctrl Pts',(-0.317364862083589,2.15604353164617,
8.12120661147408));
#47005=CARTESIAN_POINT('Ctrl Pts',(-0.317295607453776,2.15643430351316,
8.1211822622291));
#47006=CARTESIAN_POINT('Ctrl Pts',(-0.317151045270002,2.15724132285942,
8.12113191207952));
#47007=CARTESIAN_POINT('Ctrl Pts',(-0.31707563967692,2.15765755179774,8.12110590809674));
#47008=CARTESIAN_POINT('Ctrl Pts',(-0.316880722912232,2.15872152008999,
8.12103934545384));
#47009=CARTESIAN_POINT('Ctrl Pts',(-0.316760045440997,2.15936904140195,
8.12099874970265));
#47010=CARTESIAN_POINT('Ctrl Pts',(-0.316261108836302,2.16200136438478,
8.1208333638839));
#47011=CARTESIAN_POINT('Ctrl Pts',(-0.315866179305892,2.16398292443956,
8.12070804315914));
#47012=CARTESIAN_POINT('Ctrl Pts',(-0.309111904449023,2.19628484048246,
8.11865138185862));
#47013=CARTESIAN_POINT('Ctrl Pts',(-0.298432990079732,2.22552994818758,
8.11656678492813));
#47014=CARTESIAN_POINT('Ctrl Pts',(-0.276879239790065,2.26555725999323,
8.11349330499454));
#47015=CARTESIAN_POINT('Ctrl Pts',(-0.269152359661945,2.27784376478163,
8.11251890397409));
#47016=CARTESIAN_POINT('Ctrl Pts',(-0.258255636301397,2.29282481501028,
8.11132470603438));
#47017=CARTESIAN_POINT('Ctrl Pts',(-0.255826618415604,2.29603603745829,
8.11106839629576));
#47018=CARTESIAN_POINT('Ctrl Pts',(-0.252970312195753,2.29966860167403,
8.1107788697746));
#47019=CARTESIAN_POINT('Ctrl Pts',(-0.252601397837238,2.30013511228909,
8.11074169547676));
#47020=CARTESIAN_POINT('Ctrl Pts',(-0.252056219986532,2.30082060802589,
8.11068708639589));
#47021=CARTESIAN_POINT('Ctrl Pts',(-0.251880960726807,2.3010403846658,8.1106695805063));
#47022=CARTESIAN_POINT('Ctrl Pts',(-0.251568234624152,2.3014314950665,8.11063843191607));
#47023=CARTESIAN_POINT('Ctrl Pts',(-0.251430880106592,2.30160291765399,
8.11062478115732));
#47024=CARTESIAN_POINT('Ctrl Pts',(-0.251141269832963,2.3019636036843,8.11059606240507));
#47025=CARTESIAN_POINT('Ctrl Pts',(-0.25098897573914,2.30215283496606,8.1105809972924));
#47026=CARTESIAN_POINT('Ctrl Pts',(-0.250585068277143,2.30265354551364,
8.11054113931638));
#47027=CARTESIAN_POINT('Ctrl Pts',(-0.250333087098587,2.30296472959734,
8.11051637298542));
#47028=CARTESIAN_POINT('Ctrl Pts',(-0.249180686269022,2.30438247586825,
8.11040355597999));
#47029=CARTESIAN_POINT('Ctrl Pts',(-0.248273487131715,2.30548354341945,
8.11031598804553));
#47030=CARTESIAN_POINT('Ctrl Pts',(-0.241153547190104,2.31400902160593,
8.10963801765827));
#47031=CARTESIAN_POINT('Ctrl Pts',(-0.234615772718585,2.32115689801188,
8.10906991717256));
#47032=CARTESIAN_POINT('Ctrl Pts',(-0.207269627955935,2.34847487815264,
8.10684880373399));
#47033=CARTESIAN_POINT('Ctrl Pts',(-0.184106750047878,2.36609274299049,
8.10528716620653));
#47034=CARTESIAN_POINT('Ctrl Pts',(-0.156400346483884,2.38179489212323,
8.1034422622554));
#47035=CARTESIAN_POINT('Ctrl Pts',(-0.15388208827511,2.38317791555944,8.10327490524195));
#47036=CARTESIAN_POINT('Ctrl Pts',(-0.14978271746808,2.3853584541985,8.10300274058678));
#47037=CARTESIAN_POINT('Ctrl Pts',(-0.148212907339756,2.38617694485493,
8.10289858121165));
#47038=CARTESIAN_POINT('Ctrl Pts',(-0.140888862331924,2.38991923637497,
8.1024127566277));
#47039=CARTESIAN_POINT('Ctrl Pts',(-0.135054680980648,2.3926825232469,8.10202610871462));
#47040=CARTESIAN_POINT('Ctrl Pts',(-0.128197488708028,2.3956816560813,8.10157058417493));
#47041=CARTESIAN_POINT('Ctrl Pts',(-0.127251243822355,2.39609011932349,
8.1015077026631));
#47042=CARTESIAN_POINT('Ctrl Pts',(-0.125840226378234,2.39669119660459,
8.1014138963501));
#47043=CARTESIAN_POINT('Ctrl Pts',(-0.125376929382784,2.39688727539522,
8.10138308953611));
#47044=CARTESIAN_POINT('Ctrl Pts',(-0.124550719419933,2.39723466910647,
8.10132813910128));
#47045=CARTESIAN_POINT('Ctrl Pts',(-0.124187984284231,2.39738640652206,
8.1013040098868));
#47046=CARTESIAN_POINT('Ctrl Pts',(-0.123423565323021,2.39770453168053,
8.10125315165836));
#47047=CARTESIAN_POINT('Ctrl Pts',(-0.123021820937082,2.39787077102419,
8.10122641767172));
#47048=CARTESIAN_POINT('Ctrl Pts',(-0.121961747473028,2.39830691246371,
8.10115586102524));
#47049=CARTESIAN_POINT('Ctrl Pts',(-0.121302861555754,2.39857544714145,
8.10111199220174));
#47050=CARTESIAN_POINT('Ctrl Pts',(-0.118334655978815,2.39977371831736,
8.10091429826721));
#47051=CARTESIAN_POINT('Ctrl Pts',(-0.116015549370642,2.40067883986804,
8.10075964590625));
#47052=CARTESIAN_POINT('Ctrl Pts',(-0.0988405986406615,2.40715375402819,
8.0996126434107));
#47053=CARTESIAN_POINT('Ctrl Pts',(-0.0836042491240788,2.41164577220604,
8.09858429792765));
#47054=CARTESIAN_POINT('Ctrl Pts',(-0.0370331322954221,2.4217142444337,
8.09541622575253));
#47055=CARTESIAN_POINT('Ctrl Pts',(-0.00514434239926006,2.4237977694833,
8.09319868855161));
#47056=CARTESIAN_POINT('Ctrl Pts',(0.0280788392178759,2.42105320619793,
8.09108927986223));
#47057=CARTESIAN_POINT('Ctrl Pts',(0.0296240526461253,2.42091431590997,
8.09099167726233));
#47058=CARTESIAN_POINT('Ctrl Pts',(0.0315931487973007,2.42072298144491,
8.09086799789024));
#47059=CARTESIAN_POINT('Ctrl Pts',(0.0320179788368236,2.42068084899795,
8.09084135567073));
#47060=CARTESIAN_POINT('Ctrl Pts',(0.0326927681932383,2.42061257257573,
8.09079910505747));
#47061=CARTESIAN_POINT('Ctrl Pts',(0.0329427809252583,2.42058698035278,
8.09078346566574));
#47062=CARTESIAN_POINT('Ctrl Pts',(0.0334098262780731,2.4205386197544,8.09075427766141));
#47063=CARTESIAN_POINT('Ctrl Pts',(0.0336268640815612,2.42051592356457,
8.09074072511093));
#47064=CARTESIAN_POINT('Ctrl Pts',(0.0341145111030514,2.42046442831415,
8.09071029993471));
#47065=CARTESIAN_POINT('Ctrl Pts',(0.0343851063530482,2.42043550699777,
8.09069343434404));
#47066=CARTESIAN_POINT('Ctrl Pts',(0.0351876210774871,2.42034870568617,
8.09064346597799));
#47067=CARTESIAN_POINT('Ctrl Pts',(0.0357194367227065,2.42028984336355,
8.09061041852532));
#47068=CARTESIAN_POINT('Ctrl Pts',(0.0399869735877308,2.41980674338838,
8.09034574182049));
#47069=CARTESIAN_POINT('Ctrl Pts',(0.0437153515007418,2.41931846519247,
8.09011765108091));
#47070=CARTESIAN_POINT('Ctrl Pts',(0.0571660048219259,2.41731691139565,
8.08930342408048));
#47071=CARTESIAN_POINT('Ctrl Pts',(0.0668269705067426,2.41542378623534,
8.08873493636879));
#47072=CARTESIAN_POINT('Ctrl Pts',(0.107341452473838,2.4055392035933,8.08636450045496));
#47073=CARTESIAN_POINT('Ctrl Pts',(0.137003053535719,2.3934392911723,8.08464330611275));
#47074=CARTESIAN_POINT('Ctrl Pts',(0.169195079085567,2.37434499202061,8.0824229062492));
#47075=CARTESIAN_POINT('Ctrl Pts',(0.173907220737133,2.37138242802797,8.08208864757611));
#47076=CARTESIAN_POINT('Ctrl Pts',(0.179350251390957,2.36776035921035,8.08169058398228));
#47077=CARTESIAN_POINT('Ctrl Pts',(0.180157959174098,2.36721757493116,8.08163119825907));
#47078=CARTESIAN_POINT('Ctrl Pts',(0.181375364703121,2.36639144285402,8.08154120607925));
#47079=CARTESIAN_POINT('Ctrl Pts',(0.181786889240583,2.36611078640834,8.081510701536));
#47080=CARTESIAN_POINT('Ctrl Pts',(0.182521610584391,2.36560721270858,8.08145608840837));
#47081=CARTESIAN_POINT('Ctrl Pts',(0.182845054502296,2.36538465632932,8.08143199357174));
#47082=CARTESIAN_POINT('Ctrl Pts',(0.183520779633072,2.36491787937772,8.08138154493385));
#47083=CARTESIAN_POINT('Ctrl Pts',(0.183872981683724,2.3646735460431,8.08135518686374));
#47084=CARTESIAN_POINT('Ctrl Pts',(0.184798830870546,2.36402851619395,8.08128573104));
#47085=CARTESIAN_POINT('Ctrl Pts',(0.185371659969666,2.36362665442335,8.08124258876916));
#47086=CARTESIAN_POINT('Ctrl Pts',(0.186621615639251,2.36274367390256,8.08114807545155));
#47087=CARTESIAN_POINT('Ctrl Pts',(0.187298198513749,2.36226179747038,8.081096675435));
#47088=CARTESIAN_POINT('Ctrl Pts',(0.189280718492882,2.3608382209381,8.08094534788207));
#47089=CARTESIAN_POINT('Ctrl Pts',(0.190581455807145,2.35988935423807,8.0808451439038));
#47090=CARTESIAN_POINT('Ctrl Pts',(0.204207287660511,2.34979222915017,8.07978564501094));
#47091=CARTESIAN_POINT('Ctrl Pts',(0.215869092902148,2.33978570893113,8.07879223886357));
#47092=CARTESIAN_POINT('Ctrl Pts',(0.249827228802308,2.3061561169588,8.07561967357216));
#47093=CARTESIAN_POINT('Ctrl Pts',(0.269300412909237,2.27997551747219,8.07335292145059));
#47094=CARTESIAN_POINT('Ctrl Pts',(0.285231371271979,2.25002144755127,8.07120747984751));
#47095=CARTESIAN_POINT('Ctrl Pts',(0.285917930959642,2.24870879879461,8.07111432306661));
#47096=CARTESIAN_POINT('Ctrl Pts',(0.286789543296387,2.24701399124889,8.07099519397402));
#47097=CARTESIAN_POINT('Ctrl Pts',(0.286982911174575,2.24663616356739,8.07096870927996));
#47098=CARTESIAN_POINT('Ctrl Pts',(0.287288208621398,2.24603671611384,8.07092680663794));
#47099=CARTESIAN_POINT('Ctrl Pts',(0.287400628610753,2.2458153487852,8.07091135782692));
#47100=CARTESIAN_POINT('Ctrl Pts',(0.287601668457675,2.24541834350253,8.07088369707303));
#47101=CARTESIAN_POINT('Ctrl Pts',(0.287690382656494,2.2452427555988,8.07087147920332));
#47102=CARTESIAN_POINT('Ctrl Pts',(0.287898651188018,2.24482959987472,8.07084276814432));
#47103=CARTESIAN_POINT('Ctrl Pts',(0.288018072089719,2.24459196556757,8.0708262834588));
#47104=CARTESIAN_POINT('Ctrl Pts',(0.288363626333399,2.24390222433458,8.07077851947525));
#47105=CARTESIAN_POINT('Ctrl Pts',(0.288588991585186,2.24344973023557,8.07074728839139));
#47106=CARTESIAN_POINT('Ctrl Pts',(0.290144520970642,2.24030799653598,8.07053115206648));
#47107=CARTESIAN_POINT('Ctrl Pts',(0.291438196054578,2.23760071359634,8.07034848413073));
#47108=CARTESIAN_POINT('Ctrl Pts',(0.295358461970231,2.22909333590502,8.06978435756094));
#47109=CARTESIAN_POINT('Ctrl Pts',(0.297851247751539,2.22323293309606,8.06940991441361));
#47110=CARTESIAN_POINT('Ctrl Pts',(0.305905233084847,2.20262328210052,8.06812895886749));
#47111=CARTESIAN_POINT('Ctrl Pts',(0.310557454665563,2.18754245848042,8.06725331635007));
#47112=CARTESIAN_POINT('Ctrl Pts',(0.319721363269437,2.14766667953609,8.06496549653111));
#47113=CARTESIAN_POINT('Ctrl Pts',(0.32246501364835,2.12258142371212,8.06354590502199));
#47114=CARTESIAN_POINT('Ctrl Pts',(0.322252976516264,2.09595100963283,8.06193042872737));
#47115=CARTESIAN_POINT('Ctrl Pts',(0.32223093108271,2.09446808030353,8.06184014821756));
#47116=CARTESIAN_POINT('Ctrl Pts',(0.322186867061207,2.09244411347299,8.0617164735393));
#47117=CARTESIAN_POINT('Ctrl Pts',(0.322173719369848,2.09190288510134,8.06168335723248));
#47118=CARTESIAN_POINT('Ctrl Pts',(0.322149035116158,2.09098230408023,8.06162695274458));
#47119=CARTESIAN_POINT('Ctrl Pts',(0.32213819207,2.09060293269955,8.06160368632318));
#47120=CARTESIAN_POINT('Ctrl Pts',(0.322114979699215,2.08983809997434,8.06155673500013));
#47121=CARTESIAN_POINT('Ctrl Pts',(0.322102588552658,2.08945263993107,8.061533049451));
#47122=CARTESIAN_POINT('Ctrl Pts',(0.322072873211056,2.0885772005653,8.0614792031574));
#47123=CARTESIAN_POINT('Ctrl Pts',(0.32205512275342,2.08808723754139,8.06144902910326));
#47124=CARTESIAN_POINT('Ctrl Pts',(0.322015638373761,2.08706202357254,8.06138581267104));
#47125=CARTESIAN_POINT('Ctrl Pts',(0.321993687836996,2.08652678290577,8.0613527635811));
#47126=CARTESIAN_POINT('Ctrl Pts',(0.321932647428872,2.0851238241339,8.06126601642054));
#47127=CARTESIAN_POINT('Ctrl Pts',(0.321891384041812,2.08425620932182,8.06121225029567));
#47128=CARTESIAN_POINT('Ctrl Pts',(0.321758403661928,2.08167968083096,8.06105222076367));
#47129=CARTESIAN_POINT('Ctrl Pts',(0.321656582422651,2.07997133994103,8.06094564148171));
#47130=CARTESIAN_POINT('Ctrl Pts',(0.320386574462418,2.06118415379251,8.05976822250179));
#47131=CARTESIAN_POINT('Ctrl Pts',(0.317873182981182,2.04422635672385,8.05865468110537));
#47132=CARTESIAN_POINT('Ctrl Pts',(0.307668812296663,1.9999963910589,8.05562547090836));
#47133=CARTESIAN_POINT('Ctrl Pts',(0.297713271794349,1.97339973961096,8.05366536374296));
#47134=CARTESIAN_POINT('Ctrl Pts',(0.282802134777608,1.94541704220267,8.05162954693993));
#47135=CARTESIAN_POINT('Ctrl Pts',(0.281140968310523,1.94241606506763,8.05141177186864));
#47136=CARTESIAN_POINT('Ctrl Pts',(0.279149641021507,1.93895039568105,8.05116142960734));
#47137=CARTESIAN_POINT('Ctrl Pts',(0.278865852398877,1.9384594988518,8.05112599708508));
#47138=CARTESIAN_POINT('Ctrl Pts',(0.278440672648086,1.93772848345129,8.05107327684008));
#47139=CARTESIAN_POINT('Ctrl Pts',(0.278300265221675,1.93748779846827,8.05105592594053));
#47140=CARTESIAN_POINT('Ctrl Pts',(0.278049043318752,1.93705843681698,8.05102498652711));
#47141=CARTESIAN_POINT('Ctrl Pts',(0.277938348950077,1.93686969108423,8.05101139023574));
#47142=CARTESIAN_POINT('Ctrl Pts',(0.277702307145089,1.9364681522666,8.05098247520626));
#47143=CARTESIAN_POINT('Ctrl Pts',(0.277576907679287,1.93625539110862,8.05096715997913));
#47144=CARTESIAN_POINT('Ctrl Pts',(0.2772383220944,1.93568243070774,8.05092593157139));
#47145=CARTESIAN_POINT('Ctrl Pts',(0.277024677700733,1.93532250073147,8.05090004827204));
#47146=CARTESIAN_POINT('Ctrl Pts',(0.275981272494863,1.93357243671272,8.05077427100324));
#47147=CARTESIAN_POINT('Ctrl Pts',(0.275141727071516,1.9321881205908,8.05067500593205));
#47148=CARTESIAN_POINT('Ctrl Pts',(0.270244434652842,1.92424859567591,8.05010664221756));
#47149=CARTESIAN_POINT('Ctrl Pts',(0.265962593847072,1.91783378394697,8.04965118857925));
#47150=CARTESIAN_POINT('Ctrl Pts',(0.258846929950388,1.90796007629139,8.04894594465641));
#47151=CARTESIAN_POINT('Ctrl Pts',(0.256164548235499,1.90439633901164,8.04869048776538));
#47152=CARTESIAN_POINT('Ctrl Pts',(0.232350996346277,1.87408873376574,8.04649951573247));
#47153=CARTESIAN_POINT('Ctrl Pts',(0.207177000785526,1.85079999251665,8.04466206859706));
#47154=CARTESIAN_POINT('Ctrl Pts',(0.176441898913718,1.83030089612421,8.04244823063142));
#47155=CARTESIAN_POINT('Ctrl Pts',(0.174042324733345,1.8287462097464,8.04227576912201));
#47156=CARTESIAN_POINT('Ctrl Pts',(0.17052414771124,1.82653268126704,8.04202331085988));
#47157=CARTESIAN_POINT('Ctrl Pts',(0.169421704979912,1.82584831721764,8.04194425785081));
#47158=CARTESIAN_POINT('Ctrl Pts',(0.167879023817641,1.82490352499332,8.04183370370002));
#47159=CARTESIAN_POINT('Ctrl Pts',(0.167442242613306,1.82463745246869,8.041802409827));
#47160=CARTESIAN_POINT('Ctrl Pts',(0.166687124470691,1.82417992068118,8.04174832028122));
#47161=CARTESIAN_POINT('Ctrl Pts',(0.166369085529879,1.82398796946903,8.04172554265478));
#47162=CARTESIAN_POINT('Ctrl Pts',(0.165729247570845,1.82360330534216,8.04167972517321));
#47163=CARTESIAN_POINT('Ctrl Pts',(0.165407442570144,1.82341060349548,8.04165668495841));
#47164=CARTESIAN_POINT('Ctrl Pts',(0.164649682880766,1.82295864058669,8.04160243979793));
#47165=CARTESIAN_POINT('Ctrl Pts',(0.164213452036912,1.8226998466215,8.04157121790621));
#47166=CARTESIAN_POINT('Ctrl Pts',(0.16286114084714,1.82190189802909,8.04147444841107));
#47167=CARTESIAN_POINT('Ctrl Pts',(0.161943009624968,1.82136624915834,8.04140877377581));
#47168=CARTESIAN_POINT('Ctrl Pts',(0.159821323779478,1.82014246096992,8.04125705906597));
#47169=CARTESIAN_POINT('Ctrl Pts',(0.158615951684018,1.81945753002208,8.04117090449929));
#47170=CARTESIAN_POINT('Ctrl Pts',(0.15459595947063,1.81720743165206,8.04088367720096));
#47171=CARTESIAN_POINT('Ctrl Pts',(0.151762371691778,1.81567671793193,8.04068138350955));
#47172=CARTESIAN_POINT('Ctrl Pts',(0.140237277667855,1.80967219437791,8.03985903549178));
#47173=CARTESIAN_POINT('Ctrl Pts',(0.131367954096471,1.80555279269056,8.03922697312092));
#47174=CARTESIAN_POINT('Ctrl Pts',(0.106957891818811,1.79553799378884,8.03749067738725));
#47175=CARTESIAN_POINT('Ctrl Pts',(0.0911265576373418,1.79043099203813,
8.03636679112158));
#47176=CARTESIAN_POINT('Ctrl Pts',(0.0565041212295244,1.78214924480458,
8.03395833705492));
#47177=CARTESIAN_POINT('Ctrl Pts',(0.0376777574619463,1.77937188564178,
8.0326783544761));
#47178=CARTESIAN_POINT('Ctrl Pts',(0.0180560694005134,1.77823053461519,
8.03143937899188));
#47179=CARTESIAN_POINT('Ctrl Pts',(0.0173976118359405,1.77819426105755,
8.03139791433188));
#47180=CARTESIAN_POINT('Ctrl Pts',(0.0160684112849866,1.77812512874647,
8.03131444454388));
#47181=CARTESIAN_POINT('Ctrl Pts',(0.0153976670952883,1.77809234483634,
8.03127244360918));
#47182=CARTESIAN_POINT('Ctrl Pts',(0.0144582521664072,1.77804937203362,
8.03121379127825));
#47183=CARTESIAN_POINT('Ctrl Pts',(0.0141896696482295,1.77803742270223,
8.03119704206167));
#47184=CARTESIAN_POINT('Ctrl Pts',(0.0136983283558967,1.77801617877221,
8.0311664377313));
#47185=CARTESIAN_POINT('Ctrl Pts',(0.0134755744447666,1.77800677922275,
8.03115257669639));
#47186=CARTESIAN_POINT('Ctrl Pts',(0.0130227875341184,1.77798814365037,
8.03112442978471));
#47187=CARTESIAN_POINT('Ctrl Pts',(0.0127927542748233,1.77797892295107,
8.03111014479282));
#47188=CARTESIAN_POINT('Ctrl Pts',(0.0122199240160097,1.77795657627671,
8.03107460845182));
#47189=CARTESIAN_POINT('Ctrl Pts',(0.0118771145378527,1.77794375109427,
8.03105337408625));
#47190=CARTESIAN_POINT('Ctrl Pts',(0.0105881735384436,1.7778975900774,8.03097365355546));
#47191=CARTESIAN_POINT('Ctrl Pts',(0.00964190508810644,1.77786787552944,
8.03091536880736));
#47192=CARTESIAN_POINT('Ctrl Pts',(-0.00774447003574694,1.77739859189726,
8.02984868089291));
#47193=CARTESIAN_POINT('Ctrl Pts',(-0.0241969512990017,1.77821386357081,
8.02890797098904));
#47194=CARTESIAN_POINT('Ctrl Pts',(-0.0431726124904631,1.78061862203253,
8.02783132890242));
#47195=CARTESIAN_POINT('Ctrl Pts',(-0.0458235606833914,1.78098818116031,
8.02768112836416));
#47196=CARTESIAN_POINT('Ctrl Pts',(-0.0507395309361855,1.78173604133609,
8.02740253742015));
#47197=CARTESIAN_POINT('Ctrl Pts',(-0.0530056980163761,1.78210560963006,
8.02727409024294));
#47198=CARTESIAN_POINT('Ctrl Pts',(-0.0572493169203863,1.78284430162695,
8.02703324619687));
#47199=CARTESIAN_POINT('Ctrl Pts',(-0.0592276333631066,1.78320778299841,
8.02692083934999));
#47200=CARTESIAN_POINT('Ctrl Pts',(-0.0802942156020735,1.78728263776991,
8.02572147111086));
#47201=CARTESIAN_POINT('Ctrl Pts',(-0.0990106986380144,1.79269543703586,
8.02463187995649));
#47202=CARTESIAN_POINT('Ctrl Pts',(-0.118760480290052,1.80039991969175,
8.02338511435285));
#47203=CARTESIAN_POINT('Ctrl Pts',(-0.120391310018532,1.8010515226581,8.02328143981533));
#47204=CARTESIAN_POINT('Ctrl Pts',(-0.127337026156758,1.80389275656012,
8.02283665456937));
#47205=CARTESIAN_POINT('Ctrl Pts',(-0.132597884008566,1.80621093848339,
8.02249160052005));
#47206=CARTESIAN_POINT('Ctrl Pts',(-0.13868216245179,1.80908867434641,8.022081849102));
#47207=CARTESIAN_POINT('Ctrl Pts',(-0.139568688755252,1.80951295612126,
8.02202187569209));
#47208=CARTESIAN_POINT('Ctrl Pts',(-0.140903452457763,1.81015928009845,
8.02193116648259));
#47209=CARTESIAN_POINT('Ctrl Pts',(-0.141353141979542,1.81037832423035,
8.02190053505295));
#47210=CARTESIAN_POINT('Ctrl Pts',(-0.142155098322651,1.81077127048029,
8.0218457807109));
#47211=CARTESIAN_POINT('Ctrl Pts',(-0.1425075613067,1.81094477183943,8.02182167182255));
#47212=CARTESIAN_POINT('Ctrl Pts',(-0.143188406706408,1.81128146876597,
8.02177501539759));
#47213=CARTESIAN_POINT('Ctrl Pts',(-0.143516829713927,1.81144458126705,
8.02175247079539));
#47214=CARTESIAN_POINT('Ctrl Pts',(-0.144415006273544,1.81189257669022,
8.02169070903602));
#47215=CARTESIAN_POINT('Ctrl Pts',(-0.144984192468745,1.81217858778738,
8.02165145237759));
#47216=CARTESIAN_POINT('Ctrl Pts',(-0.14721619721012,1.81330845153457,8.02149704666146));
#47217=CARTESIAN_POINT('Ctrl Pts',(-0.148872501324297,1.81416502873655,
8.02138145083343));
#47218=CARTESIAN_POINT('Ctrl Pts',(-0.152995457160653,1.8163428206353,8.02109111151884));
#47219=CARTESIAN_POINT('Ctrl Pts',(-0.155452472016573,1.81768185770983,
8.02091574193494));
#47220=CARTESIAN_POINT('Ctrl Pts',(-0.165140770078455,1.82312665666009,
8.02021470272079));
#47221=CARTESIAN_POINT('Ctrl Pts',(-0.172228893430436,1.82747933914487,
8.01968033684558));
#47222=CARTESIAN_POINT('Ctrl Pts',(-0.204623256273757,1.84914098960359,
8.01713530310441));
#47223=CARTESIAN_POINT('Ctrl Pts',(-0.227540005864991,1.8697261825693,8.0150094693528));
#47224=CARTESIAN_POINT('Ctrl Pts',(-0.252173406775543,1.89917728888999,
8.01248278497806));
#47225=CARTESIAN_POINT('Ctrl Pts',(-0.256928214477433,1.90529739525086,
8.01198192667886));
#47226=CARTESIAN_POINT('Ctrl Pts',(-0.261862786940575,1.91214490878677,
8.01145240211319));
#47227=CARTESIAN_POINT('Ctrl Pts',(-0.262265552325784,1.91270762278394,
8.01140910726975));
#47228=CARTESIAN_POINT('Ctrl Pts',(-0.262828582499762,1.91349962441437,
8.01134848498512));
#47229=CARTESIAN_POINT('Ctrl Pts',(-0.262990362339847,1.91372782497048,
8.01133105423034));
#47230=CARTESIAN_POINT('Ctrl Pts',(-0.263270425042855,1.9141239630401,8.01130085936246));
#47231=CARTESIAN_POINT('Ctrl Pts',(-0.263388844490445,1.91429180304388,
8.01128808581576));
#47232=CARTESIAN_POINT('Ctrl Pts',(-0.2636358105623,1.91464254805303,8.01126143358217));
#47233=CARTESIAN_POINT('Ctrl Pts',(-0.26376432724217,1.91482547346377,8.01124755702378));
#47234=CARTESIAN_POINT('Ctrl Pts',(-0.264070626567328,1.91526241330215,
8.01121446681223));
#47235=CARTESIAN_POINT('Ctrl Pts',(-0.264248233804852,1.91551655172469,
8.01119526527826));
#47236=CARTESIAN_POINT('Ctrl Pts',(-0.264846205066268,1.91637482479557,
8.01113056768049));
#47237=CARTESIAN_POINT('Ctrl Pts',(-0.265264870216766,1.91698014872478,
8.01108518724908));
#47238=CARTESIAN_POINT('Ctrl Pts',(-0.266254312296448,1.91842125373026,
8.01097772702684));
#47239=CARTESIAN_POINT('Ctrl Pts',(-0.266823236996412,1.9192583053797,8.01091576868092));
#47240=CARTESIAN_POINT('Ctrl Pts',(-0.273519623984519,1.92921114269453,
8.01018430688131));
#47241=CARTESIAN_POINT('Ctrl Pts',(-0.27918185940648,1.93863283160152,8.00954374620886));
#47242=CARTESIAN_POINT('Ctrl Pts',(-0.297350731841026,1.97269518293874,
8.0073387619821));
#47243=CARTESIAN_POINT('Ctrl Pts',(-0.307162667955773,1.99863346019444,
8.00584326633498));
#47244=CARTESIAN_POINT('Ctrl Pts',(-0.314057772310764,2.0276551984056,8.00411465129187));
#47245=CARTESIAN_POINT('Ctrl Pts',(-0.314546233488024,2.02980939257973,
8.00398610096488));
#47246=CARTESIAN_POINT('Ctrl Pts',(-0.315466790921449,2.03407192833006,
8.00373111862418));
#47247=CARTESIAN_POINT('Ctrl Pts',(-0.315899989087747,2.03617991376101,
8.00360472378153));
#47248=CARTESIAN_POINT('Ctrl Pts',(-0.31758361691104,2.04481010996982,8.00308579924355));
#47249=CARTESIAN_POINT('Ctrl Pts',(-0.318653347641777,2.05136552577701,
8.0026881929111));
#47250=CARTESIAN_POINT('Ctrl Pts',(-0.319655382151488,2.05897936623701,
8.00222082297327));
#47251=CARTESIAN_POINT('Ctrl Pts',(-0.319786003265718,2.06001040374796,
8.00215741729286));
#47252=CARTESIAN_POINT('Ctrl Pts',(-0.319972656238297,2.06154314483822,
8.00206297985656));
#47253=CARTESIAN_POINT('Ctrl Pts',(-0.320032500991799,2.06204438442763,
8.00203206844131));
#47254=CARTESIAN_POINT('Ctrl Pts',(-0.320136888478763,2.06293650005617,
8.0019770005772));
#47255=CARTESIAN_POINT('Ctrl Pts',(-0.320181893718432,2.06332732180967,
8.00195285876294));
#47256=CARTESIAN_POINT('Ctrl Pts',(-0.320267439814649,2.06408235925827,
8.00190618456229));
#47257=CARTESIAN_POINT('Ctrl Pts',(-0.320308075287554,2.06444656379901,
8.00188365519855));
#47258=CARTESIAN_POINT('Ctrl Pts',(-0.320394550936059,2.06523380354441,
8.00183492385856));
#47259=CARTESIAN_POINT('Ctrl Pts',(-0.320440174624997,2.06565686139799,
8.00180871509913));
#47260=CARTESIAN_POINT('Ctrl Pts',(-0.320548702743619,2.06668226342327,
8.00174513963094));
#47261=CARTESIAN_POINT('Ctrl Pts',(-0.320610747213115,2.06728469525366,
8.00170774589222));
#47262=CARTESIAN_POINT('Ctrl Pts',(-0.320774454032542,2.06891943903787,
8.00160615785621));
#47263=CARTESIAN_POINT('Ctrl Pts',(-0.32087283035391,2.06995206613025,8.00154186034191));
#47264=CARTESIAN_POINT('Ctrl Pts',(-0.321844500656401,2.08070081173445,
8.00087123075178));
#47265=CARTESIAN_POINT('Ctrl Pts',(-0.322281094240882,2.09045023344166,
8.00025125180471));
#47266=CARTESIAN_POINT('Ctrl Pts',(-0.322274935754178,2.10020349358851,
7.99961864007736));
#47267=CARTESIAN_POINT('',(-0.32227487097392,2.09971161875376,7.74930651681519));
#47268=CARTESIAN_POINT('Ctrl Pts',(-0.322274936001444,2.10020310161215,
7.99961866550156));
#47269=CARTESIAN_POINT('Ctrl Pts',(-0.322257797933066,2.12739722297387,
7.99785481310939));
#47270=CARTESIAN_POINT('Ctrl Pts',(-0.318798481849687,2.15447919365321,
7.99599019670084));
#47271=CARTESIAN_POINT('Ctrl Pts',(-0.308742202953932,2.19330785843882,
7.9933020014482));
#47272=CARTESIAN_POINT('Ctrl Pts',(-0.30475322724803,2.20561089968102,7.99245041160271));
#47273=CARTESIAN_POINT('Ctrl Pts',(-0.299759189787279,2.21834769720163,
7.99159160860261));
#47274=CARTESIAN_POINT('Ctrl Pts',(-0.299480218221135,2.2190518719575,7.99154420524644));
#47275=CARTESIAN_POINT('Ctrl Pts',(-0.299082198592176,2.22004629320163,
7.99147737890527));
#47276=CARTESIAN_POINT('Ctrl Pts',(-0.298965208053927,2.22033735247817,
7.99145783341549));
#47277=CARTESIAN_POINT('Ctrl Pts',(-0.298763859835523,2.22083617820544,
7.99142436049074));
#47278=CARTESIAN_POINT('Ctrl Pts',(-0.298679710095587,2.22104402788017,
7.99141042042675));
#47279=CARTESIAN_POINT('Ctrl Pts',(-0.298518354332567,2.22144138349115,
7.99138378489321));
#47280=CARTESIAN_POINT('Ctrl Pts',(-0.298441184853786,2.22163090347979,
7.9913710872112));
#47281=CARTESIAN_POINT('Ctrl Pts',(-0.2982592584796,2.22207647969435,7.99134124831531));
#47282=CARTESIAN_POINT('Ctrl Pts',(-0.298154352067245,2.2223324752797,7.99132411621202));
#47283=CARTESIAN_POINT('Ctrl Pts',(-0.297844338678386,2.22308621106716,
7.99127370559063));
#47284=CARTESIAN_POINT('Ctrl Pts',(-0.29763831274228,2.22358357591294,7.99124048242729));
#47285=CARTESIAN_POINT('Ctrl Pts',(-0.295854491246779,2.22785954350532,
7.99095518955837));
#47286=CARTESIAN_POINT('Ctrl Pts',(-0.294205970394984,2.23160848624457,
7.99070731249554));
#47287=CARTESIAN_POINT('Ctrl Pts',(-0.29231741459194,2.23569033353268,7.99043883484352));
#47288=CARTESIAN_POINT('Ctrl Pts',(-0.292147792798575,2.23605515298583,
7.9904148518786));
#47289=CARTESIAN_POINT('Ctrl Pts',(-0.291859556853939,2.23667206120576,
7.99037431640091));
#47290=CARTESIAN_POINT('Ctrl Pts',(-0.291741298608684,2.2369243145988,7.99035774703223));
#47291=CARTESIAN_POINT('Ctrl Pts',(-0.29048472607817,2.23959565638916,7.99018233455661));
#47292=CARTESIAN_POINT('Ctrl Pts',(-0.28931664600126,2.2420007131416,7.99002489178643));
#47293=CARTESIAN_POINT('Ctrl Pts',(-0.274229074490091,2.27210654656531,
7.98805679135534));
#47294=CARTESIAN_POINT('Ctrl Pts',(-0.256412443957212,2.29767473439104,
7.98639920127045));
#47295=CARTESIAN_POINT('Ctrl Pts',(-0.229479495099375,2.32643045870218,
7.98412801474645));
#47296=CARTESIAN_POINT('Ctrl Pts',(-0.223506540323487,2.33232821802786,
7.98363686966656));
#47297=CARTESIAN_POINT('Ctrl Pts',(-0.215229993172497,2.33988573116558,
7.98296744806809));
#47298=CARTESIAN_POINT('Ctrl Pts',(-0.213124614195332,2.34175816852431,
7.98279808062119));
#47299=CARTESIAN_POINT('Ctrl Pts',(-0.209578584924454,2.34482954009607,
7.98251416295093));
#47300=CARTESIAN_POINT('Ctrl Pts',(-0.20815151657745,2.3460439653371,7.98240025592571));
#47301=CARTESIAN_POINT('Ctrl Pts',(-0.206223883561348,2.34765559459753,
7.98224683066609));
#47302=CARTESIAN_POINT('Ctrl Pts',(-0.205732591149816,2.34806387204932,
7.98220776501346));
#47303=CARTESIAN_POINT('Ctrl Pts',(-0.204957320887053,2.34870425560182,
7.98214617614296));
#47304=CARTESIAN_POINT('Ctrl Pts',(-0.204674153299718,2.34893734374122,
7.98212369282998));
#47305=CARTESIAN_POINT('Ctrl Pts',(-0.204086946610867,2.34941902109655,
7.98207709356682));
#47306=CARTESIAN_POINT('Ctrl Pts',(-0.203782849898272,2.3496675388329,7.9820529747804));
#47307=CARTESIAN_POINT('Ctrl Pts',(-0.20309124416718,2.35023063619736,7.98199815188093));
#47308=CARTESIAN_POINT('Ctrl Pts',(-0.202703457756257,2.35054487214529,
7.98196743398704));
#47309=CARTESIAN_POINT('Ctrl Pts',(-0.201553820070784,2.35147204486863,
7.98187642977763));
#47310=CARTESIAN_POINT('Ctrl Pts',(-0.200789912587256,2.35208241252613,
7.98181604054607));
#47311=CARTESIAN_POINT('Ctrl Pts',(-0.195590021029448,2.35619853154361,
7.98140550260741));
#47312=CARTESIAN_POINT('Ctrl Pts',(-0.191065459658687,2.3595903069749,7.98105085713667));
#47313=CARTESIAN_POINT('Ctrl Pts',(-0.185434416678194,2.36358455207834,
7.98061218544199));
#47314=CARTESIAN_POINT('Ctrl Pts',(-0.184410394007974,2.36430199676815,
7.98053251910685));
#47315=CARTESIAN_POINT('Ctrl Pts',(-0.17073499061825,2.37376501065391,7.97947001574154));
#47316=CARTESIAN_POINT('Ctrl Pts',(-0.15747913243314,2.38159888527657,7.9784545934656));
#47317=CARTESIAN_POINT('Ctrl Pts',(-0.134312703593152,2.39314100956954,
7.97671574137277));
#47318=CARTESIAN_POINT('Ctrl Pts',(-0.124685757814235,2.3973634272561,7.976003088547));
#47319=CARTESIAN_POINT('Ctrl Pts',(-0.099438261127418,2.4069951227345,7.97417687156147));
#47320=CARTESIAN_POINT('Ctrl Pts',(-0.0835747797115143,2.41168792223467,
7.97306912039826));
#47321=CARTESIAN_POINT('Ctrl Pts',(-0.0656226262062978,2.41552848378936,
7.97190494435722));
#47322=CARTESIAN_POINT('Ctrl Pts',(-0.063822179623753,2.41589758295875,
7.97178917985791));
#47323=CARTESIAN_POINT('Ctrl Pts',(-0.0615900041727687,2.41633532491882,
7.97164696545227));
#47324=CARTESIAN_POINT('Ctrl Pts',(-0.0611612105061166,2.41641850884593,
7.97161970617459));
#47325=CARTESIAN_POINT('Ctrl Pts',(-0.060485718753012,2.4165481266181,7.97157685913153));
#47326=CARTESIAN_POINT('Ctrl Pts',(-0.0602391352600067,2.41659514402886,
7.97156123810791));
#47327=CARTESIAN_POINT('Ctrl Pts',(-0.0597780578645253,2.41668250197535,
7.97153206661166));
#47328=CARTESIAN_POINT('Ctrl Pts',(-0.0595635795386323,2.41672291242092,
7.97151851224435));
#47329=CARTESIAN_POINT('Ctrl Pts',(-0.0590811787736625,2.41681329551993,
7.97148806020201));
#47330=CARTESIAN_POINT('Ctrl Pts',(-0.0588132345239964,2.41686314608932,
7.97147116961659));
#47331=CARTESIAN_POINT('Ctrl Pts',(-0.0581303648987129,2.41698929679926,
7.97142818264939));
#47332=CARTESIAN_POINT('Ctrl Pts',(-0.0577153507438399,2.41706512249355,
7.97140211330305));
#47333=CARTESIAN_POINT('Ctrl Pts',(-0.0553983270936908,2.41748375726197,
7.97125687451827));
#47334=CARTESIAN_POINT('Ctrl Pts',(-0.0534933605743605,2.41781027606978,
7.971138616362));
#47335=CARTESIAN_POINT('Ctrl Pts',(-0.0163286866872248,2.4238368102578,
7.96885184931841));
#47336=CARTESIAN_POINT('Ctrl Pts',(0.0196394734100666,2.42365451397915,
7.96697235185748));
#47337=CARTESIAN_POINT('Ctrl Pts',(0.0638330293052665,2.41602154803857,
7.96439671965998));
#47338=CARTESIAN_POINT('Ctrl Pts',(0.072745358366456,2.41408974248339,7.96386487807681));
#47339=CARTESIAN_POINT('Ctrl Pts',(0.0844711198538033,2.41102224913583,
7.96314199806779));
#47340=CARTESIAN_POINT('Ctrl Pts',(0.0873680549460995,2.41022093999398,
7.96296150882049));
#47341=CARTESIAN_POINT('Ctrl Pts',(0.0915176929709229,2.40901039185598,
7.96270005411243));
#47342=CARTESIAN_POINT('Ctrl Pts',(0.0927798105124144,2.40863379122095,
7.96262014148876));
#47343=CARTESIAN_POINT('Ctrl Pts',(0.0950138548546043,2.40795223751178,
7.96247797973064));
#47344=CARTESIAN_POINT('Ctrl Pts',(0.0959867163971077,2.40765039158239,
7.96241583239976));
#47345=CARTESIAN_POINT('Ctrl Pts',(0.0974338967053205,2.40719384806247,
7.96232302143826));
#47346=CARTESIAN_POINT('Ctrl Pts',(0.0979093202017549,2.40704265099139,
7.96229247280491));
#47347=CARTESIAN_POINT('Ctrl Pts',(0.0987437452809462,2.406775146976,7.96223875249521));
#47348=CARTESIAN_POINT('Ctrl Pts',(0.09910289811385,2.40665931196969,7.96221559638444));
#47349=CARTESIAN_POINT('Ctrl Pts',(0.0998183826008016,2.40642716364788,
7.96216939822123));
#47350=CARTESIAN_POINT('Ctrl Pts',(0.10017471647126,2.40631085893971,7.96214635648142));
#47351=CARTESIAN_POINT('Ctrl Pts',(0.101028806229109,2.40603044069447,7.96209104717703));
#47352=CARTESIAN_POINT('Ctrl Pts',(0.101526365062282,2.40586573445189,7.96205876009313));
#47353=CARTESIAN_POINT('Ctrl Pts',(0.103326908276328,2.40526482551238,7.96194168004091));
#47354=CARTESIAN_POINT('Ctrl Pts',(0.104627487180078,2.40482150925027,7.96185665221425));
#47355=CARTESIAN_POINT('Ctrl Pts',(0.127990192405451,2.39669094610912,7.96032088718429));
#47356=CARTESIAN_POINT('Ctrl Pts',(0.149150047050696,2.3866371413786,7.95878714149822));
#47357=CARTESIAN_POINT('Ctrl Pts',(0.181052430784703,2.36698399885061,7.95626268561711));
#47358=CARTESIAN_POINT('Ctrl Pts',(0.192571484804247,2.35879850087038,7.95530173375331));
#47359=CARTESIAN_POINT('Ctrl Pts',(0.212462190331338,2.34259862430589,7.95358400648746));
#47360=CARTESIAN_POINT('Ctrl Pts',(0.22101101020981,2.33483711237641,7.95282346353582));
#47361=CARTESIAN_POINT('Ctrl Pts',(0.23023336385096,2.32551331174303,7.95199369111833));
#47362=CARTESIAN_POINT('Ctrl Pts',(0.231332609827026,2.32438555986114,7.95189463137462));
#47363=CARTESIAN_POINT('Ctrl Pts',(0.23271076654647,2.32295077178292,7.95177029201083));
#47364=CARTESIAN_POINT('Ctrl Pts',(0.232997386575792,2.32265121908196,7.9517444246957));
#47365=CARTESIAN_POINT('Ctrl Pts',(0.233453208411968,2.32217298589373,7.95170327542622));
#47366=CARTESIAN_POINT('Ctrl Pts',(0.233622783766887,2.32199466454121,7.95168796446432));
#47367=CARTESIAN_POINT('Ctrl Pts',(0.23394286867813,2.32165729802465,7.95165905944883));
#47368=CARTESIAN_POINT('Ctrl Pts',(0.234093419140772,2.32149829500074,7.95164546224174));
#47369=CARTESIAN_POINT('Ctrl Pts',(0.234436192140971,2.32113553740562,7.95161449969089));
#47370=CARTESIAN_POINT('Ctrl Pts',(0.234628310825407,2.32093168593453,7.95159714245215));
#47371=CARTESIAN_POINT('Ctrl Pts',(0.235200503970359,2.32032296052593,7.95154543623974));
#47372=CARTESIAN_POINT('Ctrl Pts',(0.235579800477262,2.31991735179558,7.95151114713743));
#47373=CARTESIAN_POINT('Ctrl Pts',(0.238230420286007,2.31706812892288,7.95127141065425));
#47374=CARTESIAN_POINT('Ctrl Pts',(0.240464832723468,2.3145902422779,7.95106872121094));
#47375=CARTESIAN_POINT('Ctrl Pts',(0.252421575136603,2.30090929062258,7.94997787705335));
#47376=CARTESIAN_POINT('Ctrl Pts',(0.261401163742051,2.28907863262666,7.94913524804617));
#47377=CARTESIAN_POINT('Ctrl Pts',(0.286078058984446,2.25143064639639,7.9466074532951));
#47378=CARTESIAN_POINT('Ctrl Pts',(0.298992798346094,2.22399612680732,7.94494945878449));
#47379=CARTESIAN_POINT('Ctrl Pts',(0.308487998416017,2.19327512416568,7.94301594897095));
#47380=CARTESIAN_POINT('Ctrl Pts',(0.309055082084787,2.19137860759553,7.94289637272178));
#47381=CARTESIAN_POINT('Ctrl Pts',(0.309873049027505,2.18854831249368,7.9427175551475));
#47382=CARTESIAN_POINT('Ctrl Pts',(0.310137266634798,2.18761841114559,7.94265874568608));
#47383=CARTESIAN_POINT('Ctrl Pts',(0.310552377666413,2.18613204258623,7.94256464512358));
#47384=CARTESIAN_POINT('Ctrl Pts',(0.310705969973351,2.18557632996613,7.94252944155155));
#47385=CARTESIAN_POINT('Ctrl Pts',(0.310995237259413,2.18451868650653,7.94246239842274));
#47386=CARTESIAN_POINT('Ctrl Pts',(0.311131190516677,2.18401683313181,7.94243056799322));
#47387=CARTESIAN_POINT('Ctrl Pts',(0.311366908701548,2.18313829224161,7.94237481293953));
#47388=CARTESIAN_POINT('Ctrl Pts',(0.311467206278036,2.18276174770029,7.94235090563529));
#47389=CARTESIAN_POINT('Ctrl Pts',(0.311661361731219,2.18202748321121,7.94230426526997));
#47390=CARTESIAN_POINT('Ctrl Pts',(0.311755287308431,2.1816697816306,7.9422815344422));
#47391=CARTESIAN_POINT('Ctrl Pts',(0.31197603700959,2.1808231593365,7.94222771095885));
#47392=CARTESIAN_POINT('Ctrl Pts',(0.312102327545793,2.18033410165805,7.94219660109135));
#47393=CARTESIAN_POINT('Ctrl Pts',(0.312539735739782,2.17862364667735,7.94208773051031));
#47394=CARTESIAN_POINT('Ctrl Pts',(0.312844834399213,2.17740073481879,7.94200977565775));
#47395=CARTESIAN_POINT('Ctrl Pts',(0.316922081367403,2.16064008835287,7.9409396995577));
#47396=CARTESIAN_POINT('Ctrl Pts',(0.319539418380532,2.14484690618175,7.93991011923873));
#47397=CARTESIAN_POINT('Ctrl Pts',(0.322930326010057,2.10722107428564,7.93740867701181));
#47398=CARTESIAN_POINT('Ctrl Pts',(0.322679543694788,2.08537342549922,7.93591609115748));
#47399=CARTESIAN_POINT('Ctrl Pts',(0.319231820324013,2.05494123163268,7.93386609340602));
#47400=CARTESIAN_POINT('Ctrl Pts',(0.31787641775254,2.04620542715606,7.93328180917602));
#47401=CARTESIAN_POINT('Ctrl Pts',(0.315404922342017,2.03369592568333,7.9324608087739));
#47402=CARTESIAN_POINT('Ctrl Pts',(0.314576360130593,2.02987003216489,7.93221187891341));
#47403=CARTESIAN_POINT('Ctrl Pts',(0.313554334980625,2.02553426040452,7.9319329751747));
#47404=CARTESIAN_POINT('Ctrl Pts',(0.313429091100962,2.02500885238682,7.93189923149284));
#47405=CARTESIAN_POINT('Ctrl Pts',(0.313238513826322,2.02421818352803,7.93184853544579));
#47406=CARTESIAN_POINT('Ctrl Pts',(0.31317416387825,2.02395269016987,7.93183152678729));
#47407=CARTESIAN_POINT('Ctrl Pts',(0.313057783481313,2.0234751838766,7.93180096166106));
#47408=CARTESIAN_POINT('Ctrl Pts',(0.313005875302479,2.02326314244093,7.93178739816735));
#47409=CARTESIAN_POINT('Ctrl Pts',(0.312893923254408,2.02280782940814,7.93175829345114));
#47410=CARTESIAN_POINT('Ctrl Pts',(0.312833811292982,2.02256457578634,7.93174275627582));
#47411=CARTESIAN_POINT('Ctrl Pts',(0.312671288363382,2.02191017616747,7.93170099044551));
#47412=CARTESIAN_POINT('Ctrl Pts',(0.312568349725254,2.02149915982671,7.93167479231909));
#47413=CARTESIAN_POINT('Ctrl Pts',(0.3120921951187,2.01961374177849,7.93155476814143));
#47414=CARTESIAN_POINT('Ctrl Pts',(0.311709347641557,2.01814175929524,7.93146149018665));
#47415=CARTESIAN_POINT('Ctrl Pts',(0.303754752831987,1.98842295618111,7.92958587525625));
#47416=CARTESIAN_POINT('Ctrl Pts',(0.292382139559771,1.96132875076995,7.92800688573116));
#47417=CARTESIAN_POINT('Ctrl Pts',(0.267410735147483,1.9190387151782,7.92524112964321));
#47418=CARTESIAN_POINT('Ctrl Pts',(0.255757166163526,1.90291224619023,7.92409895428312));
#47419=CARTESIAN_POINT('Ctrl Pts',(0.242079092787087,1.88725657427769,7.92283673157989));
#47420=CARTESIAN_POINT('Ctrl Pts',(0.24145997203141,1.88655414215673,7.92277975575125));
#47421=CARTESIAN_POINT('Ctrl Pts',(0.240463067695954,1.88543297843627,7.92268825914674));
#47422=CARTESIAN_POINT('Ctrl Pts',(0.240087227712111,1.88501251954675,7.92265381959869));
#47423=CARTESIAN_POINT('Ctrl Pts',(0.239368382859633,1.88421257085575,7.922588053281));
#47424=CARTESIAN_POINT('Ctrl Pts',(0.239025573988094,1.88383290661061,7.92255673480699));
#47425=CARTESIAN_POINT('Ctrl Pts',(0.238420760373258,1.88316626727149,7.92250155770633));
#47426=CARTESIAN_POINT('Ctrl Pts',(0.238159137144458,1.88287894616504,7.92247771525793));
#47427=CARTESIAN_POINT('Ctrl Pts',(0.237645644266715,1.88231706035975,7.92243096855573));
#47428=CARTESIAN_POINT('Ctrl Pts',(0.237393816769984,1.88204245778838,7.92240806611322));
#47429=CARTESIAN_POINT('Ctrl Pts',(0.236792314067117,1.8813888347922,7.92235341706822));
#47430=CARTESIAN_POINT('Ctrl Pts',(0.236442205040468,1.88101021661859,7.92232165197905));
#47431=CARTESIAN_POINT('Ctrl Pts',(0.235383425253319,1.87987072004602,7.92222572031245));
#47432=CARTESIAN_POINT('Ctrl Pts',(0.234671984588109,1.87911243496771,7.92216143504011));
#47433=CARTESIAN_POINT('Ctrl Pts',(0.227239609495639,1.87126711525361,7.92149163325118));
#47434=CARTESIAN_POINT('Ctrl Pts',(0.220204130304307,1.86448634771157,7.92087241350607));
#47435=CARTESIAN_POINT('Ctrl Pts',(0.195193912095052,1.84248315365438,7.9187163178867));
#47436=CARTESIAN_POINT('Ctrl Pts',(0.175866265963533,1.82891633264268,7.91711755013175));
#47437=CARTESIAN_POINT('Ctrl Pts',(0.147839351214534,1.81351096267461,7.9149578351609));
#47438=CARTESIAN_POINT('Ctrl Pts',(0.140284045480136,1.80973659905472,7.9143905783939));
#47439=CARTESIAN_POINT('Ctrl Pts',(0.125319535028243,1.80298181714127,7.91330560824192));
#47440=CARTESIAN_POINT('Ctrl Pts',(0.117930112759263,1.79997116909613,7.91278726333764));
#47441=CARTESIAN_POINT('Ctrl Pts',(0.109241385718556,1.79680186005571,7.91220366808825));
#47442=CARTESIAN_POINT('Ctrl Pts',(0.108044248116191,1.79637320112335,7.91212382073251));
#47443=CARTESIAN_POINT('Ctrl Pts',(0.106482288030301,1.79582431815522,7.91202039786929));
#47444=CARTESIAN_POINT('Ctrl Pts',(0.106119765142266,1.79569765275354,7.91199644691518));
#47445=CARTESIAN_POINT('Ctrl Pts',(0.105531032421204,1.79549312971287,7.91195763776548));
#47446=CARTESIAN_POINT('Ctrl Pts',(0.105304962133066,1.79541487592629,7.91194275602299));
#47447=CARTESIAN_POINT('Ctrl Pts',(0.104870106553759,1.79526489353509,7.91191417058083));
#47448=CARTESIAN_POINT('Ctrl Pts',(0.104661335316596,1.79519312794698,7.91190046473836));
#47449=CARTESIAN_POINT('Ctrl Pts',(0.104179517818542,1.79502805546729,7.91186887424831));
#47450=CARTESIAN_POINT('Ctrl Pts',(0.103906419015623,1.79493490043293,7.91185099867832));
#47451=CARTESIAN_POINT('Ctrl Pts',(0.103032845071531,1.79463823021166,7.91179391474199));
#47452=CARTESIAN_POINT('Ctrl Pts',(0.102431889586267,1.79443611858779,7.91175478925918));
#47453=CARTESIAN_POINT('Ctrl Pts',(0.0970392932046791,1.79264019263358,
7.91140495965208));
#47454=CARTESIAN_POINT('Ctrl Pts',(0.0922110822577378,1.79115732346877,
7.91110063342681));
#47455=CARTESIAN_POINT('Ctrl Pts',(0.0863691812529429,1.78951235485459,
7.91074079754704));
#47456=CARTESIAN_POINT('Ctrl Pts',(0.0853873538144352,1.7892409082366,7.91068060317246));
#47457=CARTESIAN_POINT('Ctrl Pts',(0.0534910390827794,1.78058508723307,
7.90873373668274));
#47458=CARTESIAN_POINT('Ctrl Pts',(0.0214973645616857,1.77685057596685,
7.90702716714788));
#47459=CARTESIAN_POINT('Ctrl Pts',(-0.0218462293014116,1.77826683355827,
7.9045300110437));
#47460=CARTESIAN_POINT('Ctrl Pts',(-0.0331392048114361,1.77923335752483,
7.90386436326444));
#47461=CARTESIAN_POINT('Ctrl Pts',(-0.0463659463247003,1.78107134308125,
7.90305687892157));
#47462=CARTESIAN_POINT('Ctrl Pts',(-0.0483721174638344,1.78136945039266,
7.90293365370172));
#47463=CARTESIAN_POINT('Ctrl Pts',(-0.0510268182456624,1.78178957505528,
7.90276955642636));
#47464=CARTESIAN_POINT('Ctrl Pts',(-0.0516780082948458,1.78189468069167,
7.9027292209795));
#47465=CARTESIAN_POINT('Ctrl Pts',(-0.0527464657651205,1.7820705029648,
7.90266290177858));
#47466=CARTESIAN_POINT('Ctrl Pts',(-0.0531639268907506,1.78214004402786,
7.90263695539164));
#47467=CARTESIAN_POINT('Ctrl Pts',(-0.0539725016791286,1.78227637462965,
7.90258663273277));
#47468=CARTESIAN_POINT('Ctrl Pts',(-0.0543636315459367,1.78234306458243,
7.90256225966737));
#47469=CARTESIAN_POINT('Ctrl Pts',(-0.0552663115410769,1.78249869287234,
7.90250593846617));
#47470=CARTESIAN_POINT('Ctrl Pts',(-0.055777770865429,1.78258814532003,
7.90247397403264));
#47471=CARTESIAN_POINT('Ctrl Pts',(-0.0571484585988294,1.7828312890581,
7.90238816809724));
#47472=CARTESIAN_POINT('Ctrl Pts',(-0.0580072780052151,1.78298723496492,
7.90233425494789));
#47473=CARTESIAN_POINT('Ctrl Pts',(-0.0640702884933305,1.78411362936393,
7.90195256709336));
#47474=CARTESIAN_POINT('Ctrl Pts',(-0.0692502457351405,1.78520864193262,
7.90162083846191));
#47475=CARTESIAN_POINT('Ctrl Pts',(-0.0759430026804297,1.78679663356211,
7.9011845348271));
#47476=CARTESIAN_POINT('Ctrl Pts',(-0.0774826135918362,1.78717395752025,
7.90108363462428));
#47477=CARTESIAN_POINT('Ctrl Pts',(-0.0795557971862356,1.78769829181636,
7.90094704312417));
#47478=CARTESIAN_POINT('Ctrl Pts',(-0.0800918846675346,1.78783534504265,
7.90091165764534));
#47479=CARTESIAN_POINT('Ctrl Pts',(-0.0834399470897636,1.78870048478004,
7.90069025301422));
#47480=CARTESIAN_POINT('Ctrl Pts',(-0.0862422543900602,1.78946516191003,
7.90050313053605));
#47481=CARTESIAN_POINT('Ctrl Pts',(-0.116064224383297,1.79803760223737,
7.89849246057288));
#47482=CARTESIAN_POINT('Ctrl Pts',(-0.141959182766014,1.80931229895432,
7.89656090106894));
#47483=CARTESIAN_POINT('Ctrl Pts',(-0.175686060832555,1.8295895141688,7.89392813877432));
#47484=CARTESIAN_POINT('Ctrl Pts',(-0.185007447698949,1.83587933720208,
7.89318827318453));
#47485=CARTESIAN_POINT('Ctrl Pts',(-0.194800235201608,1.84326065039731,
7.89241251273499));
#47486=CARTESIAN_POINT('Ctrl Pts',(-0.195615444804508,1.84388123245592,
7.89234794770617));
#47487=CARTESIAN_POINT('Ctrl Pts',(-0.197016866630122,1.84495866572273,
7.89223699842934));
#47488=CARTESIAN_POINT('Ctrl Pts',(-0.19760447793628,1.84541367229913,7.89219049127293));
#47489=CARTESIAN_POINT('Ctrl Pts',(-0.198435973282791,1.84606213944095,
7.89212470718168));
#47490=CARTESIAN_POINT('Ctrl Pts',(-0.198681153415577,1.846253922597,7.89210531282292));
#47491=CARTESIAN_POINT('Ctrl Pts',(-0.199102121590258,1.8465841937001,7.89207201920991));
#47492=CARTESIAN_POINT('Ctrl Pts',(-0.199278043628648,1.84672250981771,
7.89205810766765));
#47493=CARTESIAN_POINT('Ctrl Pts',(-0.199614954285152,1.84698796919347,
7.89203146918543));
#47494=CARTESIAN_POINT('Ctrl Pts',(-0.199775965326588,1.84711508272431,
7.89201874014399));
#47495=CARTESIAN_POINT('Ctrl Pts',(-0.200155414152943,1.84741523508469,
7.89198874556836));
#47496=CARTESIAN_POINT('Ctrl Pts',(-0.200373749504362,1.84758840400453,
7.8919714893833));
#47497=CARTESIAN_POINT('Ctrl Pts',(-0.201019344344136,1.84810181196337,
7.89192047182162));
#47498=CARTESIAN_POINT('Ctrl Pts',(-0.20144596654637,1.84844285637419,7.8918867677015));
#47499=CARTESIAN_POINT('Ctrl Pts',(-0.205231054702886,1.85148448298315,
7.89158779935572));
#47500=CARTESIAN_POINT('Ctrl Pts',(-0.208536100993626,1.85425125227808,
7.89132718336066));
#47501=CARTESIAN_POINT('Ctrl Pts',(-0.232491599691991,1.87513667857228,
7.88943298318641));
#47502=CARTESIAN_POINT('Ctrl Pts',(-0.250807788085938,1.89576549787855,
7.8879476237939));
#47503=CARTESIAN_POINT('Ctrl Pts',(-0.276926822112255,1.9340796124684,7.88532867787026));
#47504=CARTESIAN_POINT('Ctrl Pts',(-0.286172938612336,1.9505914096165,7.88423695872313));
#47505=CARTESIAN_POINT('Ctrl Pts',(-0.294384116166399,1.96884950856838,
7.88301941628957));
#47506=CARTESIAN_POINT('Ctrl Pts',(-0.294843357859363,1.9698852293984,7.88295032683834));
#47507=CARTESIAN_POINT('Ctrl Pts',(-0.295506575852445,1.97140251661407,
7.88284907346148));
#47508=CARTESIAN_POINT('Ctrl Pts',(-0.295714860012506,1.9718822000348,7.88281705682201));
#47509=CARTESIAN_POINT('Ctrl Pts',(-0.296078787629978,1.97272594958408,
7.88276072935585));
#47510=CARTESIAN_POINT('Ctrl Pts',(-0.296234929826972,1.97308980048138,
7.8827364355922));
#47511=CARTESIAN_POINT('Ctrl Pts',(-0.296537132656912,1.97379760612631,
7.88268916908606));
#47512=CARTESIAN_POINT('Ctrl Pts',(-0.296683266426591,1.97414152915098,
7.88266619887845));
#47513=CARTESIAN_POINT('Ctrl Pts',(-0.297071416963216,1.97505946649003,
7.88260488146495));
#47514=CARTESIAN_POINT('Ctrl Pts',(-0.297312367222174,1.97563392754318,
7.88256649809822));
#47515=CARTESIAN_POINT('Ctrl Pts',(-0.298170841851653,1.97769741121766,
7.88242858583727));
#47516=CARTESIAN_POINT('Ctrl Pts',(-0.298778849927427,1.97919034460017,
7.88232873531422));
#47517=CARTESIAN_POINT('Ctrl Pts',(-0.308724402663005,2.00414550366828,
7.88065832628991));
#47518=CARTESIAN_POINT('Ctrl Pts',(-0.315281750750485,2.02861555758866,
7.87898980458297));
#47519=CARTESIAN_POINT('Ctrl Pts',(-0.321160253429432,2.06901465873945,
7.87623186467879));
#47520=CARTESIAN_POINT('Ctrl Pts',(-0.322282781442665,2.08457794132063,
7.87517139817404));
#47521=CARTESIAN_POINT('Ctrl Pts',(-0.322270477898228,2.10909031257621,
7.87354994536088));
#47522=CARTESIAN_POINT('Ctrl Pts',(-0.321894950252477,2.11801582031185,
7.87297001678884));
#47523=CARTESIAN_POINT('Ctrl Pts',(-0.321089454267323,2.12762694870816,
7.87236476429156));
#47524=CARTESIAN_POINT('Ctrl Pts',(-0.321027426366448,2.12833862170505,
7.87232006202176));
#47525=CARTESIAN_POINT('Ctrl Pts',(-0.320937469335541,2.12933252157952,
7.87225779812213));
#47526=CARTESIAN_POINT('Ctrl Pts',(-0.320911533849697,2.12961492004832,
7.87224012569037));
#47527=CARTESIAN_POINT('Ctrl Pts',(-0.320866077205716,2.13010280265549,
7.87220962688306));
#47528=CARTESIAN_POINT('Ctrl Pts',(-0.320846731384682,2.13030830231822,
7.87219679061606));
#47529=CARTESIAN_POINT('Ctrl Pts',(-0.320806094279767,2.13073556784925,
7.87217012313495));
#47530=CARTESIAN_POINT('Ctrl Pts',(-0.320784770493705,2.13095732994989,
7.87215629385888));
#47531=CARTESIAN_POINT('Ctrl Pts',(-0.320733634342674,2.13148340709602,
7.87212351501082));
#47532=CARTESIAN_POINT('Ctrl Pts',(-0.320703618702171,2.13178770319188,
7.87210457695863));
#47533=CARTESIAN_POINT('Ctrl Pts',(-0.320602332856928,2.13279978395838,
7.87204166148262));
#47534=CARTESIAN_POINT('Ctrl Pts',(-0.320529151641634,2.13350738174752,
7.87199779117199));
#47535=CARTESIAN_POINT('Ctrl Pts',(-0.319263965687572,2.14535705344153,
7.87126500036173));
#47536=CARTESIAN_POINT('Ctrl Pts',(-0.317493822310917,2.15643117280002,
7.87060789502809));
#47537=CARTESIAN_POINT('Ctrl Pts',(-0.311051974490813,2.1865557332177,7.86884240183433));
#47538=CARTESIAN_POINT('Ctrl Pts',(-0.305214368565636,2.20530663398111,
7.86776609413679));
#47539=CARTESIAN_POINT('Ctrl Pts',(-0.290272041468378,2.24135238093017,
7.86556628450477));
#47540=CARTESIAN_POINT('Ctrl Pts',(-0.28122973353486,2.2585812752271,7.86444722091061));
#47541=CARTESIAN_POINT('Ctrl Pts',(-0.269990992051644,2.27597645382458,
7.86318932760815));
#47542=CARTESIAN_POINT('Ctrl Pts',(-0.269282661703714,2.27705845396168,
7.86311053822641));
#47543=CARTESIAN_POINT('Ctrl Pts',(-0.268285555485195,2.27856174608138,
7.86300029409817));
#47544=CARTESIAN_POINT('Ctrl Pts',(-0.268002254918617,2.27898666933443,
7.86296904508655));
#47545=CARTESIAN_POINT('Ctrl Pts',(-0.267511252695481,2.27971934553032,
7.86291501218814));
#47546=CARTESIAN_POINT('Ctrl Pts',(-0.267304026441358,2.28002741714227,
7.86289224625872));
#47547=CARTESIAN_POINT('Ctrl Pts',(-0.266873969698084,2.28066437873853,
7.86284507929959));
#47548=CARTESIAN_POINT('Ctrl Pts',(-0.266651062603541,2.28099321605406,
7.86282067539631));
#47549=CARTESIAN_POINT('Ctrl Pts',(-0.266128598902884,2.28176090557921,
7.86276357736239));
#47550=CARTESIAN_POINT('Ctrl Pts',(-0.265828564530426,2.28219942981603,
7.86273086513824));
#47551=CARTESIAN_POINT('Ctrl Pts',(-0.264859935705621,2.28360767265562,
7.86262550376776));
#47552=CARTESIAN_POINT('Ctrl Pts',(-0.264187114821185,2.28457446005182,
7.86255269376736));
#47553=CARTESIAN_POINT('Ctrl Pts',(-0.262610733758786,2.28681330967597,
7.86238295917557));
#47554=CARTESIAN_POINT('Ctrl Pts',(-0.261703211062829,2.28808253331707,
7.86228588335337));
#47555=CARTESIAN_POINT('Ctrl Pts',(-0.252244973159093,2.3011094400684,7.86128060590163));
#47556=CARTESIAN_POINT('Ctrl Pts',(-0.242918415110829,2.31228064449698,
7.86034188266902));
#47557=CARTESIAN_POINT('Ctrl Pts',(-0.211466585408964,2.34515664796652,
7.85732973503402));
#47558=CARTESIAN_POINT('Ctrl Pts',(-0.186952015504273,2.36432682548592,
7.85517309581899));
#47559=CARTESIAN_POINT('Ctrl Pts',(-0.156952016439864,2.38149642729502,
7.85295107799569));
#47560=CARTESIAN_POINT('Ctrl Pts',(-0.15379291719028,2.38323473544812,7.85272196742056));
#47561=CARTESIAN_POINT('Ctrl Pts',(-0.150096099100366,2.38518882902178,
7.85246004215881));
#47562=CARTESIAN_POINT('Ctrl Pts',(-0.149586320936729,2.38545654619357,
7.85242405836527));
#47563=CARTESIAN_POINT('Ctrl Pts',(-0.148827226456137,2.38585260347645,
7.85237067927247));
#47564=CARTESIAN_POINT('Ctrl Pts',(-0.148578459258549,2.38598198491283,
7.85235321846998));
#47565=CARTESIAN_POINT('Ctrl Pts',(-0.148135096729644,2.3862118388593,7.85232215718805));
#47566=CARTESIAN_POINT('Ctrl Pts',(-0.147940567961566,2.38631243762472,
7.85230854869031));
#47567=CARTESIAN_POINT('Ctrl Pts',(-0.147527390943119,2.38652557480514,
7.85227968668254));
#47568=CARTESIAN_POINT('Ctrl Pts',(-0.147308717014252,2.38663806095577,
7.85226443652256));
#47569=CARTESIAN_POINT('Ctrl Pts',(-0.146721699348348,2.38693917442856,
7.85222356495147));
#47570=CARTESIAN_POINT('Ctrl Pts',(-0.146353119119047,2.38712734354304,
7.8521979725338));
#47571=CARTESIAN_POINT('Ctrl Pts',(-0.14458755156591,2.38802442548806,7.85207571120106));
#47572=CARTESIAN_POINT('Ctrl Pts',(-0.143185739294593,2.3887238716172,7.85197962949085));
#47573=CARTESIAN_POINT('Ctrl Pts',(-0.131518960131977,2.39443924045445,
7.85118770091166));
#47574=CARTESIAN_POINT('Ctrl Pts',(-0.120997805956815,2.39891687007916,
7.85052279783495));
#47575=CARTESIAN_POINT('Ctrl Pts',(-0.0787653261399857,2.41429381830125,
7.8479604802253));
#47576=CARTESIAN_POINT('Ctrl Pts',(-0.0456767017644045,2.42077771202408,
7.84615748053733));
#47577=CARTESIAN_POINT('Ctrl Pts',(-0.0114046110692441,2.42207408320491,
7.84411523672295));
#47578=CARTESIAN_POINT('Ctrl Pts',(-0.0106275070147806,2.42210066175847,
7.84406885376787));
#47579=CARTESIAN_POINT('Ctrl Pts',(-0.0091320901766239,2.42214639046467,
7.8439794461186));
#47580=CARTESIAN_POINT('Ctrl Pts',(-0.00841379395454737,2.42216595105535,
7.84393643385516));
#47581=CARTESIAN_POINT('Ctrl Pts',(-0.00509858566691138,2.4222451358241,
7.84373759889337));
#47582=CARTESIAN_POINT('Ctrl Pts',(-0.00250113361318201,2.42227576215142,
7.8435809134893));
#47583=CARTESIAN_POINT('Ctrl Pts',(0.00148793349062841,2.42227456956377,
7.84333878550451));
#47584=CARTESIAN_POINT('Ctrl Pts',(0.00287948367095603,2.42226514023795,
7.84325404188193));
#47585=CARTESIAN_POINT('Ctrl Pts',(0.00479782112107145,2.42223971545906,
7.84313681858831));
#47586=CARTESIAN_POINT('Ctrl Pts',(0.00532470950535287,2.4222314397605,
7.84310458067905));
#47587=CARTESIAN_POINT('Ctrl Pts',(0.00622710974699833,2.42221505210609,
7.84304929498346));
#47588=CARTESIAN_POINT('Ctrl Pts',(0.00660263325183739,2.42220757584473,
7.84302626714191));
#47589=CARTESIAN_POINT('Ctrl Pts',(0.00737308272021299,2.42219088957926,
7.84297897753579));
#47590=CARTESIAN_POINT('Ctrl Pts',(0.00776800642997994,2.42218160988892,
7.84295471362583));
#47591=CARTESIAN_POINT('Ctrl Pts',(0.00867961107137652,2.42215851242409,
7.84289864973776));
#47592=CARTESIAN_POINT('Ctrl Pts',(0.00919627676571361,2.42214417775949,
7.84286683361891));
#47593=CARTESIAN_POINT('Ctrl Pts',(0.0108134490212011,2.422095416371,7.84276711879866));
#47594=CARTESIAN_POINT('Ctrl Pts',(0.0119138062860855,2.42205659300582,
7.84269908251303));
#47595=CARTESIAN_POINT('Ctrl Pts',(0.0275545387255845,2.42142448194293,
7.84172927021112));
#47596=CARTESIAN_POINT('Ctrl Pts',(0.0420364847399454,2.41985274197984,
7.84079658266717));
#47597=CARTESIAN_POINT('Ctrl Pts',(0.0889056384387882,2.41152773410653,
7.83766175515394));
#47598=CARTESIAN_POINT('Ctrl Pts',(0.120362751052646,2.40077605220694,7.83535117881836));
#47599=CARTESIAN_POINT('Ctrl Pts',(0.152485647198109,2.38393603584016,7.83302589136675));
#47600=CARTESIAN_POINT('Ctrl Pts',(0.155315231038123,2.38239816926301,7.83282161463496));
#47601=CARTESIAN_POINT('Ctrl Pts',(0.15860006563939,2.38054856361472,7.83258553873825));
#47602=CARTESIAN_POINT('Ctrl Pts',(0.159078028161934,2.38027782347842,7.83255121508975));
#47603=CARTESIAN_POINT('Ctrl Pts',(0.159797559024813,2.37986781433505,7.83249958697359));
#47604=CARTESIAN_POINT('Ctrl Pts',(0.160039639597334,2.37972945345446,7.83248222447836));
#47605=CARTESIAN_POINT('Ctrl Pts',(0.160471388037626,2.37948194419821,7.83245127224259));
#47606=CARTESIAN_POINT('Ctrl Pts',(0.160661124128403,2.37937291691641,7.83243767469911));
#47607=CARTESIAN_POINT('Ctrl Pts',(0.161064657112157,2.37914048934187,7.83240876543298));
#47608=CARTESIAN_POINT('Ctrl Pts',(0.161278422692253,2.37901703699873,7.83239345720409));
#47609=CARTESIAN_POINT('Ctrl Pts',(0.161846567929465,2.37868805482285,7.83235278651482));
#47610=CARTESIAN_POINT('Ctrl Pts',(0.162200699358362,2.37848209382931,7.83232745202431));
#47611=CARTESIAN_POINT('Ctrl Pts',(0.16387747713634,2.3775026051066,7.83220756699285));
#47612=CARTESIAN_POINT('Ctrl Pts',(0.165195017150495,2.37672030984514,7.83211357715743));
#47613=CARTESIAN_POINT('Ctrl Pts',(0.175953208509584,2.37022836400244,7.83134742632148));
#47614=CARTESIAN_POINT('Ctrl Pts',(0.185101634170977,2.36404609661573,7.8307041494326));
#47615=CARTESIAN_POINT('Ctrl Pts',(0.213256392276101,2.34283581956301,7.82869121814771));
#47616=CARTESIAN_POINT('Ctrl Pts',(0.230893448297282,2.32613231349738,7.82737263657334));
#47617=CARTESIAN_POINT('Ctrl Pts',(0.250508229107794,2.30284387645286,7.82562952772105));
#47618=CARTESIAN_POINT('Ctrl Pts',(0.254383502849539,2.2979622145223,7.82526908205368));
#47619=CARTESIAN_POINT('Ctrl Pts',(0.259126448953529,2.29161814689843,7.82480458479692));
#47620=CARTESIAN_POINT('Ctrl Pts',(0.260127543554704,2.290256909749,7.82470514305407));
#47621=CARTESIAN_POINT('Ctrl Pts',(0.264888924039722,2.28367479578576,7.82422523863973));
#47622=CARTESIAN_POINT('Ctrl Pts',(0.268502793292778,2.27835025618281,7.82383978787106));
#47623=CARTESIAN_POINT('Ctrl Pts',(0.272507207444315,2.27205248551882,7.82338555750276));
#47624=CARTESIAN_POINT('Ctrl Pts',(0.273055529071874,2.27118093902943,7.82332273406909));
#47625=CARTESIAN_POINT('Ctrl Pts',(0.273865413876963,2.2698798505051,7.82322899771151));
#47626=CARTESIAN_POINT('Ctrl Pts',(0.27413016729602,2.26945229387459,7.82319820251538));
#47627=CARTESIAN_POINT('Ctrl Pts',(0.274600124939966,2.26868936419242,7.82314326510158));
#47628=CARTESIAN_POINT('Ctrl Pts',(0.274805718675819,2.26835423127911,7.82311913726494));
#47629=CARTESIAN_POINT('Ctrl Pts',(0.275237426062742,2.26764761866576,7.82306827403339));
#47630=CARTESIAN_POINT('Ctrl Pts',(0.275463401936569,2.2672760560885,7.82304153365009));
#47631=CARTESIAN_POINT('Ctrl Pts',(0.276057348758979,2.2662949870648,7.82297094211839));
#47632=CARTESIAN_POINT('Ctrl Pts',(0.276424051678866,2.26568471917216,7.82292704472378));
#47633=CARTESIAN_POINT('Ctrl Pts',(0.278035297684738,2.26298304131534,7.82273276488769));
#47634=CARTESIAN_POINT('Ctrl Pts',(0.279258123269032,2.26087883198473,7.82258159514348));
#47635=CARTESIAN_POINT('Ctrl Pts',(0.288030838082574,2.24538152012065,7.82146905131287));
#47636=CARTESIAN_POINT('Ctrl Pts',(0.294636451811711,2.23147923092952,7.82047393843302));
#47637=CARTESIAN_POINT('Ctrl Pts',(0.308967308678145,2.19475633390234,7.81785692729135));
#47638=CARTESIAN_POINT('Ctrl Pts',(0.315174460220739,2.17144588057499,7.81620222464014));
#47639=CARTESIAN_POINT('Ctrl Pts',(0.319342237946461,2.14357515414677,7.81433518532233));
#47640=CARTESIAN_POINT('Ctrl Pts',(0.319874849284993,2.13947584845354,7.81406354140369));
#47641=CARTESIAN_POINT('Ctrl Pts',(0.320442326152691,2.13433609640617,7.81372751935797));
#47642=CARTESIAN_POINT('Ctrl Pts',(0.320551198992344,2.13330436585477,7.81366029756568));
#47643=CARTESIAN_POINT('Ctrl Pts',(0.321089447693236,2.12795633749529,7.81331309910152));
#47644=CARTESIAN_POINT('Ctrl Pts',(0.321436658164977,2.12363196151648,7.81303656585807));
#47645=CARTESIAN_POINT('Ctrl Pts',(0.32173240778931,2.11870276309451,7.81272712705058));
#47646=CARTESIAN_POINT('Ctrl Pts',(0.321766668059672,2.11810378161634,7.81268962187897));
#47647=CARTESIAN_POINT('Ctrl Pts',(0.321814809025999,2.11721877786667,7.81263435407362));
#47648=CARTESIAN_POINT('Ctrl Pts',(0.321829981259079,2.11693283154018,7.81261651955036));
#47649=CARTESIAN_POINT('Ctrl Pts',(0.32185615801111,2.11642673917481,7.81258499493885));
#47650=CARTESIAN_POINT('Ctrl Pts',(0.321867317800919,2.1162066018156,7.81257129608775));
#47651=CARTESIAN_POINT('Ctrl Pts',(0.321890169427502,2.1157464971031,7.81254269289034));
#47652=CARTESIAN_POINT('Ctrl Pts',(0.321901818751774,2.11550652863439,7.81252779099392));
#47653=CARTESIAN_POINT('Ctrl Pts',(0.321931237283365,2.11488620407804,7.81248931045475));
#47654=CARTESIAN_POINT('Ctrl Pts',(0.321948600829022,2.1145058277403,7.81246575467461));
#47655=CARTESIAN_POINT('Ctrl Pts',(0.322019912069162,2.11288040736809,7.8123652641658));
#47656=CARTESIAN_POINT('Ctrl Pts',(0.322067312896367,2.11163506534729,7.81228869239922));
#47657=CARTESIAN_POINT('Ctrl Pts',(0.322358024204151,2.10262205350728,7.81173735516827));
#47658=CARTESIAN_POINT('Ctrl Pts',(0.322327541151314,2.09484740359178,7.81127702313948));
#47659=CARTESIAN_POINT('Ctrl Pts',(0.321193541598255,2.06658206212645,7.80963461122789));
#47660=CARTESIAN_POINT('Ctrl Pts',(0.318415639706246,2.0462072741071,7.80850787964424));
#47661=CARTESIAN_POINT('Ctrl Pts',(0.30886144148997,2.00557443408854,7.80616293623721));
#47662=CARTESIAN_POINT('Ctrl Pts',(0.301975871178473,1.98544892950335,7.80494729352734));
#47663=CARTESIAN_POINT('Ctrl Pts',(0.29262343557792,1.96496522569044,7.80357965753719));
#47664=CARTESIAN_POINT('Ctrl Pts',(0.292076404651883,1.96378605397924,7.80350046569507));
#47665=CARTESIAN_POINT('Ctrl Pts',(0.291304061465788,1.96214724750963,7.80338974831441));
#47666=CARTESIAN_POINT('Ctrl Pts',(0.291084760153022,1.96168478031134,7.8033584308546));
#47667=CARTESIAN_POINT('Ctrl Pts',(0.290704351213278,1.96088747762754,7.80330431151757));
#47668=CARTESIAN_POINT('Ctrl Pts',(0.290543764013779,1.96055239376027,7.80328152773345));
#47669=CARTESIAN_POINT('Ctrl Pts',(0.290210364532327,1.95985979297222,7.80323435385998));
#47670=CARTESIAN_POINT('Ctrl Pts',(0.290037470330294,1.95950231635369,7.80320996094933));
#47671=CARTESIAN_POINT('Ctrl Pts',(0.289632157402543,1.95866822649327,7.80315294062472));
#47672=CARTESIAN_POINT('Ctrl Pts',(0.289399222685224,1.958191866566,7.80312029526398));
#47673=CARTESIAN_POINT('Ctrl Pts',(0.288661173058712,1.95669192044654,7.80301724783825));
#47674=CARTESIAN_POINT('Ctrl Pts',(0.288151799398091,1.95567045019522,7.80294669705111));
#47675=CARTESIAN_POINT('Ctrl Pts',(0.277433365328805,1.9344592027054,7.80147376874622));
#47676=CARTESIAN_POINT('Ctrl Pts',(0.265134044538047,1.91540156826889,7.7999937643473));
#47677=CARTESIAN_POINT('Ctrl Pts',(0.241190608143404,1.88568735815783,7.79742737684056));
#47678=CARTESIAN_POINT('Ctrl Pts',(0.230574289135217,1.87430482335346,7.79636776524988));
#47679=CARTESIAN_POINT('Ctrl Pts',(0.215579665281473,1.86039475149057,7.79499943926648));
#47680=CARTESIAN_POINT('Ctrl Pts',(0.21190533034636,1.85713913050409,7.79467331343826));
#47681=CARTESIAN_POINT('Ctrl Pts',(0.206941185223378,1.85293915387112,7.79424607118036));
#47682=CARTESIAN_POINT('Ctrl Pts',(0.205716802756097,1.85191873696992,7.79414173770608));
#47683=CARTESIAN_POINT('Ctrl Pts',(0.203821834602831,1.85036312118565,7.79398191917302));
#47684=CARTESIAN_POINT('Ctrl Pts',(0.203156611486783,1.84982145822758,7.79392612561931));
#47685=CARTESIAN_POINT('Ctrl Pts',(0.198555301630045,1.84610526171244,7.79354238142064));
#47686=CARTESIAN_POINT('Ctrl Pts',(0.194546861882251,1.84302087326813,7.79321900835275));
#47687=CARTESIAN_POINT('Ctrl Pts',(0.189955585531988,1.83965704649889,7.79286222943857));
#47688=CARTESIAN_POINT('Ctrl Pts',(0.189442838143511,1.83928370015503,7.79282257190303));
#47689=CARTESIAN_POINT('Ctrl Pts',(0.188695186450588,1.83874268331621,7.79276502173149));
#47690=CARTESIAN_POINT('Ctrl Pts',(0.188461157912089,1.83857381372472,7.79274704661614));
#47691=CARTESIAN_POINT('Ctrl Pts',(0.188047701791405,1.8382763170549,7.79271535960726));
#47692=CARTESIAN_POINT('Ctrl Pts',(0.187868368622466,1.83814755980572,7.79270163864908));
#47693=CARTESIAN_POINT('Ctrl Pts',(0.187494445363039,1.8378796730423,7.79267307751555));
#47694=CARTESIAN_POINT('Ctrl Pts',(0.187299833058516,1.8377405761778,7.79265823961578));
#47695=CARTESIAN_POINT('Ctrl Pts',(0.186798742204781,1.83738326961243,7.79262010377106));
#47696=CARTESIAN_POINT('Ctrl Pts',(0.186492035004327,1.83716537889367,7.79259682792221));
#47697=CARTESIAN_POINT('Ctrl Pts',(0.185199766979882,1.83625072751848,7.7924990338178));
#47698=CARTESIAN_POINT('Ctrl Pts',(0.184210661079955,1.83555895765477,7.79242485472668));
#47699=CARTESIAN_POINT('Ctrl Pts',(0.181638965088731,1.8337817727217,7.79223365772499));
#47700=CARTESIAN_POINT('Ctrl Pts',(0.180050500735718,1.83270489013688,7.79211718438396));
#47701=CARTESIAN_POINT('Ctrl Pts',(0.173279097251479,1.82820204424906,7.79162708281972));
#47702=CARTESIAN_POINT('Ctrl Pts',(0.168006968349553,1.82491193524463,7.79126124294117));
#47703=CARTESIAN_POINT('Ctrl Pts',(0.148814489564583,1.81369249653791,7.78997259269385));
#47704=CARTESIAN_POINT('Ctrl Pts',(0.134401953137314,1.80665050933854,7.78908277337192));
#47705=CARTESIAN_POINT('Ctrl Pts',(0.107807982682133,1.79602995155379,7.78748154422638));
#47706=CARTESIAN_POINT('Ctrl Pts',(0.095827080469099,1.79204302629998,7.78677393003545));
#47707=CARTESIAN_POINT('Ctrl Pts',(0.0831665505998361,1.78864048950478,
7.78602043641045));
#47708=CARTESIAN_POINT('Ctrl Pts',(0.0826889382886714,1.78851330783432,
7.78599200376236));
#47709=CARTESIAN_POINT('Ctrl Pts',(0.0781513405067462,1.78731617906237,
7.78572179722553));
#47710=CARTESIAN_POINT('Ctrl Pts',(0.0740712218140315,1.78632460083417,
7.78547822022259));
#47711=CARTESIAN_POINT('Ctrl Pts',(0.068162845360006,1.78501041139755,7.78512387540157));
#47712=CARTESIAN_POINT('Ctrl Pts',(0.0663492696363843,1.78462341772982,
7.78501489174729));
#47713=CARTESIAN_POINT('Ctrl Pts',(0.0580182189914081,1.78292071959369,
7.78451307846395));
#47714=CARTESIAN_POINT('Ctrl Pts',(0.0514647109437782,1.78179133002675,
7.78411500331623));
#47715=CARTESIAN_POINT('Ctrl Pts',(0.0438517848115576,1.78072069052314,
7.78364712664919));
#47716=CARTESIAN_POINT('Ctrl Pts',(0.0428215837490908,1.78058088908663,
7.7835836988295));
#47717=CARTESIAN_POINT('Ctrl Pts',(0.0412901229764387,1.7803806071797,7.78348923474597));
#47718=CARTESIAN_POINT('Ctrl Pts',(0.0407893614334045,1.78031631491192,
7.7834583189227));
#47719=CARTESIAN_POINT('Ctrl Pts',(0.0398981248011359,1.7802040181031,7.78340324610236));
#47720=CARTESIAN_POINT('Ctrl Pts',(0.0395077081308421,1.78015555125011,
7.78337910374955));
#47721=CARTESIAN_POINT('Ctrl Pts',(0.0386865863317237,1.78005514245692,
7.78332829144348));
#47722=CARTESIAN_POINT('Ctrl Pts',(0.0382558634025644,1.78000335510719,
7.78330161666375));
#47723=CARTESIAN_POINT('Ctrl Pts',(0.037122686434553,1.77986942981624,7.78323138293221));
#47724=CARTESIAN_POINT('Ctrl Pts',(0.0364200671591778,1.77978873456782,
7.78318777857784));
#47725=CARTESIAN_POINT('Ctrl Pts',(0.0333332740169484,1.77944450993963,
7.78299596113615));
#47726=CARTESIAN_POINT('Ctrl Pts',(0.0309465155826444,1.77920529611985,
7.78284698432698));
#47727=CARTESIAN_POINT('Ctrl Pts',(0.0167979750887183,1.77794661748474,
7.78195975887065));
#47728=CARTESIAN_POINT('Ctrl Pts',(0.00499137278360443,1.77754755055566,
7.78120213407256));
#47729=CARTESIAN_POINT('Ctrl Pts',(-0.0257814858978446,1.77819789996264,
7.7791821709975));
#47730=CARTESIAN_POINT('Ctrl Pts',(-0.0446796350378662,1.78027373916416,
7.77789484631387));
#47731=CARTESIAN_POINT('Ctrl Pts',(-0.0778640185065421,1.78691934844391,
7.77560742949979));
#47732=CARTESIAN_POINT('Ctrl Pts',(-0.0922267060310288,1.79084530901711,
7.77460903173696));
#47733=CARTESIAN_POINT('Ctrl Pts',(-0.10945807921497,1.79686385551595,7.77343754464171));
#47734=CARTESIAN_POINT('Ctrl Pts',(-0.112630522582811,1.79802821188475,
7.77322303686281));
#47735=CARTESIAN_POINT('Ctrl Pts',(-0.116311044104446,1.799445120942,7.77297603392202));
#47736=CARTESIAN_POINT('Ctrl Pts',(-0.116837342481726,1.79964932209244,
7.77294075833967));
#47737=CARTESIAN_POINT('Ctrl Pts',(-0.117622149121257,1.79995619815735,
7.77288822583045));
#47738=CARTESIAN_POINT('Ctrl Pts',(-0.117881061867879,1.80005782516892,
7.77287090638192));
#47739=CARTESIAN_POINT('Ctrl Pts',(-0.118343373540004,1.80023998028533,
7.77284000170296));
#47740=CARTESIAN_POINT('Ctrl Pts',(-0.118546821825374,1.80032038021194,
7.77282640876402));
#47741=CARTESIAN_POINT('Ctrl Pts',(-0.118980067191222,1.8004921029728,7.77279747789632));
#47742=CARTESIAN_POINT('Ctrl Pts',(-0.119209840400209,1.80058348288175,
7.77278214352556));
#47743=CARTESIAN_POINT('Ctrl Pts',(-0.119678695294262,1.80077056990174,
7.77275087194513));
#47744=CARTESIAN_POINT('Ctrl Pts',(-0.119917767958958,1.80086629933572,
7.77273493609914));
#47745=CARTESIAN_POINT('Ctrl Pts',(-0.120993186746647,1.80129841477808,
7.77266329488608));
#47746=CARTESIAN_POINT('Ctrl Pts',(-0.121828244761371,1.80163802675737,
7.77260778261008));
#47747=CARTESIAN_POINT('Ctrl Pts',(-0.123881823364054,1.80248326122163,
7.772471528839));
#47748=CARTESIAN_POINT('Ctrl Pts',(-0.125098697203112,1.80299287532788,
7.77239101835187));
#47749=CARTESIAN_POINT('Ctrl Pts',(-0.129775397177239,1.80498527054054,
7.77208235476825));
#47750=CARTESIAN_POINT('Ctrl Pts',(-0.133212416317876,1.80652121177343,
7.77185710908267));
#47751=CARTESIAN_POINT('Ctrl Pts',(-0.144854536844566,1.81197054956875,
7.77109703406402));
#47752=CARTESIAN_POINT('Ctrl Pts',(-0.152921085902793,1.8161708845498,7.77057531927611));
#47753=CARTESIAN_POINT('Ctrl Pts',(-0.167594311899711,1.82461882649015,
7.76961642600287));
#47754=CARTESIAN_POINT('Ctrl Pts',(-0.17424398551058,1.82877742907326,7.76917782360765));
#47755=CARTESIAN_POINT('Ctrl Pts',(-0.203386322053105,1.84851712571542,
7.76721017529219));
#47756=CARTESIAN_POINT('Ctrl Pts',(-0.223987804625232,1.86667868438678,
7.76568090521249));
#47757=CARTESIAN_POINT('Ctrl Pts',(-0.24318432273746,1.88851589594493,7.76391988439744));
#47758=CARTESIAN_POINT('Ctrl Pts',(-0.244310881627447,1.88981833088322,
7.76381516093574));
#47759=CARTESIAN_POINT('Ctrl Pts',(-0.245841954379403,1.89161737320788,
7.76367090161053));
#47760=CARTESIAN_POINT('Ctrl Pts',(-0.246255520541489,1.89210626686843,
7.76363173832799));
#47761=CARTESIAN_POINT('Ctrl Pts',(-0.246910299660286,1.89288500359133,
7.76356941807465));
#47762=CARTESIAN_POINT('Ctrl Pts',(-0.2471524672449,1.89317404479008,7.76354630018665));
#47763=CARTESIAN_POINT('Ctrl Pts',(-0.24762161709205,1.8937360031932,7.76350137950916));
#47764=CARTESIAN_POINT('Ctrl Pts',(-0.247848656937928,1.89400887183544,
7.76347957910988));
#47765=CARTESIAN_POINT('Ctrl Pts',(-0.248389082951357,1.89466057168666,
7.7634275399302));
#47766=CARTESIAN_POINT('Ctrl Pts',(-0.248702053249451,1.89503974518287,
7.76339728432509));
#47767=CARTESIAN_POINT('Ctrl Pts',(-0.249632530575102,1.89617231731244,
7.76330697660469));
#47768=CARTESIAN_POINT('Ctrl Pts',(-0.250247486510243,1.89692779605999,
7.76324682154055));
#47769=CARTESIAN_POINT('Ctrl Pts',(-0.254626095356384,1.9023570480641,7.76281510071163));
#47770=CARTESIAN_POINT('Ctrl Pts',(-0.25826177073284,1.90713207926455,7.76243845132368));
#47771=CARTESIAN_POINT('Ctrl Pts',(-0.270341435707547,1.92395170213854,
7.76112079081288));
#47772=CARTESIAN_POINT('Ctrl Pts',(-0.278092077954107,1.9364695980472,7.76015454211314));
#47773=CARTESIAN_POINT('Ctrl Pts',(-0.287404480967353,1.95409858011864,
7.75881948955918));
#47774=CARTESIAN_POINT('Ctrl Pts',(-0.289735606609377,1.95878443393202,
7.75846707721003));
#47775=CARTESIAN_POINT('Ctrl Pts',(-0.293054948665906,1.9658852669772,7.75793768164209));
#47776=CARTESIAN_POINT('Ctrl Pts',(-0.294129664125993,1.96825894671478,
7.75776147727899));
#47777=CARTESIAN_POINT('Ctrl Pts',(-0.296410399793889,1.97346337827838,
7.75737702106168));
#47778=CARTESIAN_POINT('Ctrl Pts',(-0.297604909631107,1.97629891056668,
7.75716875407674));
#47779=CARTESIAN_POINT('Ctrl Pts',(-0.30573389346498,1.99639511638255,7.75570246028156));
#47780=CARTESIAN_POINT('Ctrl Pts',(-0.311204040011075,2.01421299714702,
7.75445062100555));
#47781=CARTESIAN_POINT('Ctrl Pts',(-0.31533074080164,2.03345045320751,7.75321125411676));
#47782=CARTESIAN_POINT('Ctrl Pts',(-0.315549746591385,2.03449674988814,
7.75314419601279));
#47783=CARTESIAN_POINT('Ctrl Pts',(-0.315838129484753,2.03590951199907,
7.75305413930554));
#47784=CARTESIAN_POINT('Ctrl Pts',(-0.315912079169682,2.03627502117175,
7.7530308839035));
#47785=CARTESIAN_POINT('Ctrl Pts',(-0.316027294024683,2.03684962014129,
7.7529943952908));
#47786=CARTESIAN_POINT('Ctrl Pts',(-0.316068986202367,2.03705862246095,
7.75298113762487));
#47787=CARTESIAN_POINT('Ctrl Pts',(-0.316148915213874,2.03746138760873,
7.75295561722452));
#47788=CARTESIAN_POINT('Ctrl Pts',(-0.316187180965619,2.03765514276249,
7.75294335293531));
#47789=CARTESIAN_POINT('Ctrl Pts',(-0.316265905696554,2.03805569501419,
7.75291802476659));
#47790=CARTESIAN_POINT('Ctrl Pts',(-0.316306339842971,2.03826249598511,
7.75290496236235));
#47791=CARTESIAN_POINT('Ctrl Pts',(-0.316397511664129,2.03873123614969,
7.75287538681526));
#47792=CARTESIAN_POINT('Ctrl Pts',(-0.316448127018677,2.03899319940705,
7.75285888067552));
#47793=CARTESIAN_POINT('Ctrl Pts',(-0.31657558598801,2.03965729871342,7.75281709289158));
#47794=CARTESIAN_POINT('Ctrl Pts',(-0.316651989016194,2.04005952036704,
7.75279183615509));
#47795=CARTESIAN_POINT('Ctrl Pts',(-0.316868191400554,2.04120966213146,
7.75271976285643));
#47796=CARTESIAN_POINT('Ctrl Pts',(-0.317006109978373,2.04195793929017,
7.75267305061626));
#47797=CARTESIAN_POINT('Ctrl Pts',(-0.320539387253856,2.0615160473925,7.75145659810435));
#47798=CARTESIAN_POINT('Ctrl Pts',(-0.322257763038556,2.08059297725488,
7.75037734620028));
#47799=CARTESIAN_POINT('Ctrl Pts',(-0.32227487097392,2.09971161875376,7.74930651681519));
#47800=CARTESIAN_POINT('',(-0.32227487212353,2.10029338639761,7.49935789418026));
#47801=CARTESIAN_POINT('Ctrl Pts',(-0.322274870797116,2.09971142123794,
7.74930652787799));
#47802=CARTESIAN_POINT('Ctrl Pts',(-0.322301050256033,2.12894774368805,
7.7476690100838));
#47803=CARTESIAN_POINT('Ctrl Pts',(-0.318349214822576,2.15804910749707,
7.74605150154093));
#47804=CARTESIAN_POINT('Ctrl Pts',(-0.310113917334948,2.18770931960783,
7.74419354706404));
#47805=CARTESIAN_POINT('Ctrl Pts',(-0.30968953566173,2.18919617617591,7.74409988129185));
#47806=CARTESIAN_POINT('Ctrl Pts',(-0.309027553797149,2.19145379722797,
7.74395683415946));
#47807=CARTESIAN_POINT('Ctrl Pts',(-0.308797728825796,2.1922268327919,7.74390770512513));
#47808=CARTESIAN_POINT('Ctrl Pts',(-0.308365837219326,2.19365982290545,
7.74381635512585));
#47809=CARTESIAN_POINT('Ctrl Pts',(-0.308164547040277,2.19432000809183,
7.74377415967596));
#47810=CARTESIAN_POINT('Ctrl Pts',(-0.307834406928609,2.19539045260446,
7.74370556200655));
#47811=CARTESIAN_POINT('Ctrl Pts',(-0.307706853144732,2.19580111200868,
7.74367920232366));
#47812=CARTESIAN_POINT('Ctrl Pts',(-0.307460730257454,2.19658794198916,
7.74362861327715));
#47813=CARTESIAN_POINT('Ctrl Pts',(-0.307342291671044,2.19696415284186,
7.74360438823824));
#47814=CARTESIAN_POINT('Ctrl Pts',(-0.307070938927745,2.19782059135435,
7.74354915632064));
#47815=CARTESIAN_POINT('Ctrl Pts',(-0.306917588571903,2.1983006787743,7.74351813514352));
#47816=CARTESIAN_POINT('Ctrl Pts',(-0.306437332376391,2.19979211717981,
7.74342157625674));
#47817=CARTESIAN_POINT('Ctrl Pts',(-0.306106551526138,2.20080220431422,
7.7433559110671));
#47818=CARTESIAN_POINT('Ctrl Pts',(-0.303503738106729,2.20861930868389,
7.74284560374043));
#47819=CARTESIAN_POINT('Ctrl Pts',(-0.30101007300084,2.21534988466393,7.74239365819215));
#47820=CARTESIAN_POINT('Ctrl Pts',(-0.289540160427978,2.24339621664072,
7.74045450421555));
#47821=CARTESIAN_POINT('Ctrl Pts',(-0.278509062640986,2.26379363343003,
7.73889819641893));
#47822=CARTESIAN_POINT('Ctrl Pts',(-0.261344909783403,2.28870861029079,
7.73685087185366));
#47823=CARTESIAN_POINT('Ctrl Pts',(-0.257102249814327,2.29444932126274,
7.73636836253759));
#47824=CARTESIAN_POINT('Ctrl Pts',(-0.246959242325551,2.3072607599163,7.73527271011933));
#47825=CARTESIAN_POINT('Ctrl Pts',(-0.240939051096981,2.31422952870395,
7.73466265478897));
#47826=CARTESIAN_POINT('Ctrl Pts',(-0.231746745709577,2.32399171840051,
7.73379767694872));
#47827=CARTESIAN_POINT('Ctrl Pts',(-0.228805399025349,2.32699545733285,
7.73353000558546));
#47828=CARTESIAN_POINT('Ctrl Pts',(-0.225529287577843,2.33021265480593,
7.73324247882924));
#47829=CARTESIAN_POINT('Ctrl Pts',(-0.225252126764099,2.33048385058421,
7.73321823497732));
#47830=CARTESIAN_POINT('Ctrl Pts',(-0.224789930044353,2.33093446993655,
7.73317794141341));
#47831=CARTESIAN_POINT('Ctrl Pts',(-0.224605168099941,2.33111417204084,
7.73316187013503));
#47832=CARTESIAN_POINT('Ctrl Pts',(-0.224242614408547,2.33146595155246,
7.73313040465807));
#47833=CARTESIAN_POINT('Ctrl Pts',(-0.224064839725677,2.33163804619398,
7.73311500911103));
#47834=CARTESIAN_POINT('Ctrl Pts',(-0.22372953212983,2.33196189325583,7.73308603386103));
#47835=CARTESIAN_POINT('Ctrl Pts',(-0.223572044189869,2.33211368879702,
7.73307245079983));
#47836=CARTESIAN_POINT('Ctrl Pts',(-0.223214115221895,2.33245797818098,
7.73304163905084));
#47837=CARTESIAN_POINT('Ctrl Pts',(-0.223013580060107,2.33265037280101,
7.73302441817162));
#47838=CARTESIAN_POINT('Ctrl Pts',(-0.222405796373231,2.33323197614759,
7.73297235064468));
#47839=CARTESIAN_POINT('Ctrl Pts',(-0.221997773265584,2.33362037932207,
7.73293756653933));
#47840=CARTESIAN_POINT('Ctrl Pts',(-0.21915214938016,2.33631498358247,7.73269614050075));
#47841=CARTESIAN_POINT('Ctrl Pts',(-0.21667956413232,2.33858416686921,7.73249228730989));
#47842=CARTESIAN_POINT('Ctrl Pts',(-0.203072647094565,2.35068567989956,
7.73139919443846));
#47843=CARTESIAN_POINT('Ctrl Pts',(-0.191302870889532,2.35977899251178,
7.73055553404026));
#47844=CARTESIAN_POINT('Ctrl Pts',(-0.167788575390083,2.37547806028539,
7.72896796469071));
#47845=CARTESIAN_POINT('Ctrl Pts',(-0.156176523573257,2.38222342241932,
7.72822378081531));
#47846=CARTESIAN_POINT('Ctrl Pts',(-0.132047898606532,2.39429319186261,
7.72670072915251));
#47847=CARTESIAN_POINT('Ctrl Pts',(-0.119548121083918,2.39958858683744,
7.72592301762301));
#47848=CARTESIAN_POINT('Ctrl Pts',(-0.101243987875153,2.4060145708186,7.72477312804479));
#47849=CARTESIAN_POINT('Ctrl Pts',(-0.0956839501782412,2.40779837177179,
7.72442256392184));
#47850=CARTESIAN_POINT('Ctrl Pts',(-0.0891863663322832,2.40968989586137,
7.72401036242171));
#47851=CARTESIAN_POINT('Ctrl Pts',(-0.0882928305514554,2.40994582685202,
7.72395362321472));
#47852=CARTESIAN_POINT('Ctrl Pts',(-0.0869338885493985,2.41032870855437,
7.72386724461564));
#47853=CARTESIAN_POINT('Ctrl Pts',(-0.0864692785510927,2.4104584870706,
7.7238376972781));
#47854=CARTESIAN_POINT('Ctrl Pts',(-0.0856634521705343,2.4106816276064,
7.72378642283914));
#47855=CARTESIAN_POINT('Ctrl Pts',(-0.0853223692893016,2.41077547211322,
7.72376471145582));
#47856=CARTESIAN_POINT('Ctrl Pts',(-0.0846136117890121,2.41096922273947,
7.72371957827158));
#47857=CARTESIAN_POINT('Ctrl Pts',(-0.0842459132938679,2.41106903877196,
7.72369615358426));
#47858=CARTESIAN_POINT('Ctrl Pts',(-0.0833501229305022,2.41131050669605,
7.72363906163552));
#47859=CARTESIAN_POINT('Ctrl Pts',(-0.0828218473107328,2.41145146680347,
7.72360537200116));
#47860=CARTESIAN_POINT('Ctrl Pts',(-0.0808251892907754,2.41197879708945,
7.72347795942955));
#47861=CARTESIAN_POINT('Ctrl Pts',(-0.0793544593852882,2.41235612801141,
7.72338394445073));
#47862=CARTESIAN_POINT('Ctrl Pts',(-0.0525607468767134,2.4190288847524,
7.72166805119647));
#47863=CARTESIAN_POINT('Ctrl Pts',(-0.0265738969956599,2.42223487768055,
7.71994089152942));
#47864=CARTESIAN_POINT('Ctrl Pts',(0.010581188389925,2.42229149911656,7.71742930079981));
#47865=CARTESIAN_POINT('Ctrl Pts',(0.0216471582448338,2.42173775042511,
7.71667778989407));
#47866=CARTESIAN_POINT('Ctrl Pts',(0.0408945858164924,2.41977691277874,
7.71538190785904));
#47867=CARTESIAN_POINT('Ctrl Pts',(0.0490916420477925,2.41862151790631,
7.7148337327451));
#47868=CARTESIAN_POINT('Ctrl Pts',(0.0603456261109347,2.41659053655771,
7.71409376263111));
#47869=CARTESIAN_POINT('Ctrl Pts',(0.0634472896557928,2.41598355267001,
7.71389117422289));
#47870=CARTESIAN_POINT('Ctrl Pts',(0.0682586692445174,2.41496827824923,
7.71357953996668));
#47871=CARTESIAN_POINT('Ctrl Pts',(0.0699747396147304,2.41459147855192,
7.71346891304632));
#47872=CARTESIAN_POINT('Ctrl Pts',(0.0721075518984737,2.4141048583619,7.71333214673509));
#47873=CARTESIAN_POINT('Ctrl Pts',(0.0725272260829327,2.41400822054398,
7.71330527028156));
#47874=CARTESIAN_POINT('Ctrl Pts',(0.073151048274662,2.41386325648438,7.71326537345835));
#47875=CARTESIAN_POINT('Ctrl Pts',(0.0733553426411092,2.41381557217778,
7.71325231626606));
#47876=CARTESIAN_POINT('Ctrl Pts',(0.0737514675816805,2.41372270478033,
7.71322701525823));
#47877=CARTESIAN_POINT('Ctrl Pts',(0.0739433030856167,2.41367754525097,
7.71321477012738));
#47878=CARTESIAN_POINT('Ctrl Pts',(0.0743440969143607,2.41358280724529,
7.71318920293883));
#47879=CARTESIAN_POINT('Ctrl Pts',(0.0745530464658049,2.41353319602426,
7.71317588284638));
#47880=CARTESIAN_POINT('Ctrl Pts',(0.0750676123437887,2.41341047836239,
7.71314310239469));
#47881=CARTESIAN_POINT('Ctrl Pts',(0.0753731724152606,2.41333713353568,
7.71312365582883));
#47882=CARTESIAN_POINT('Ctrl Pts',(0.0765648017193995,2.41304925794744,
7.71304789074373));
#47883=CARTESIAN_POINT('Ctrl Pts',(0.0774500773701396,2.41283141198785,
7.71299176155946));
#47884=CARTESIAN_POINT('Ctrl Pts',(0.0926054603769788,2.40903374396154,
7.71203338075983));
#47885=CARTESIAN_POINT('Ctrl Pts',(0.106617024733881,2.40448408924046,7.71118531400371));
#47886=CARTESIAN_POINT('Ctrl Pts',(0.136233246272949,2.39257088816415,7.7093804451085));
#47887=CARTESIAN_POINT('Ctrl Pts',(0.151656361097163,2.38488170619499,7.70843153731973));
#47888=CARTESIAN_POINT('Ctrl Pts',(0.17744460247778,2.36933463666151,7.7067282617686));
#47889=CARTESIAN_POINT('Ctrl Pts',(0.188085877727286,2.362014095635,7.70598646466654));
#47890=CARTESIAN_POINT('Ctrl Pts',(0.201214769239499,2.3517694350158,7.70499867108858));
#47891=CARTESIAN_POINT('Ctrl Pts',(0.20412996516913,2.34941168246824,7.70477442262453));
#47892=CARTESIAN_POINT('Ctrl Pts',(0.208192744827544,2.34600683963365,7.70445448997691));
#47893=CARTESIAN_POINT('Ctrl Pts',(0.209374978224071,2.34500143368869,7.70436048223005));
#47894=CARTESIAN_POINT('Ctrl Pts',(0.211437782899015,2.34322132929878,7.70419481985811));
#47895=CARTESIAN_POINT('Ctrl Pts',(0.212321479357396,2.34245028440836,7.70412331598305));
#47896=CARTESIAN_POINT('Ctrl Pts',(0.213598689401639,2.3413235521861,7.70401918228323));
#47897=CARTESIAN_POINT('Ctrl Pts',(0.213995571597392,2.3409716835755,7.70398671198336));
#47898=CARTESIAN_POINT('Ctrl Pts',(0.214688078406281,2.34035465944349,7.7039298591007));
#47899=CARTESIAN_POINT('Ctrl Pts',(0.21498408573375,2.34008993357682,7.70390549458936));
#47900=CARTESIAN_POINT('Ctrl Pts',(0.215556087166141,2.33957647412051,7.70385829007633));
#47901=CARTESIAN_POINT('Ctrl Pts',(0.21583214206669,2.33932780890549,7.70383545297818));
#47902=CARTESIAN_POINT('Ctrl Pts',(0.216487355882004,2.33873554864701,7.70378111652768));
#47903=CARTESIAN_POINT('Ctrl Pts',(0.216866126853119,2.33839152766715,7.70374959917338));
#47904=CARTESIAN_POINT('Ctrl Pts',(0.218203581893468,2.33717095079696,7.70363793241633));
#47905=CARTESIAN_POINT('Ctrl Pts',(0.219157774017282,2.33628951111215,7.70355757546932));
#47906=CARTESIAN_POINT('Ctrl Pts',(0.235278189763927,2.32121655156853,7.70218812143246));
#47907=CARTESIAN_POINT('Ctrl Pts',(0.249039851878306,2.30560019795321,7.70083435499544));
#47908=CARTESIAN_POINT('Ctrl Pts',(0.261841737704375,2.28788633079693,7.69936901788218));
#47909=CARTESIAN_POINT('Ctrl Pts',(0.262477083560678,2.28699772588632,7.69929569518324));
#47910=CARTESIAN_POINT('Ctrl Pts',(0.272256013528746,2.27317272881833,7.69815787819737));
#47911=CARTESIAN_POINT('Ctrl Pts',(0.280437930912508,2.25958286663693,7.69707776077898));
#47912=CARTESIAN_POINT('Ctrl Pts',(0.291550362917102,2.23761057363008,7.69542957510191));
#47913=CARTESIAN_POINT('Ctrl Pts',(0.295191809411358,2.22961521710622,7.69484881458794));
#47914=CARTESIAN_POINT('Ctrl Pts',(0.29882960426638,2.22067641400162,7.69422716191465));
#47915=CARTESIAN_POINT('Ctrl Pts',(0.299153598030281,2.21987098941035,7.69417139075256));
#47916=CARTESIAN_POINT('Ctrl Pts',(0.300248535594524,2.21711696640552,7.69398153965908));
#47917=CARTESIAN_POINT('Ctrl Pts',(0.301003746243188,2.21516211277538,7.69384822763014));
#47918=CARTESIAN_POINT('Ctrl Pts',(0.302193423898459,2.21199097101762,7.69363445990351));
#47919=CARTESIAN_POINT('Ctrl Pts',(0.302639729339874,2.21077922817762,7.69355335862578));
#47920=CARTESIAN_POINT('Ctrl Pts',(0.303209873544261,2.20920209233019,7.69344858729164));
#47921=CARTESIAN_POINT('Ctrl Pts',(0.303340348301456,2.20883913579255,7.69342452942272));
#47922=CARTESIAN_POINT('Ctrl Pts',(0.303551417213515,2.20824865354474,7.69338547895445));
#47923=CARTESIAN_POINT('Ctrl Pts',(0.303632407403628,2.20802127133939,7.69337046275133));
#47924=CARTESIAN_POINT('Ctrl Pts',(0.303786753505378,2.20758639530125,7.69334178477227));
#47925=CARTESIAN_POINT('Ctrl Pts',(0.303860151728064,2.20737891902645,7.69332812057505));
#47926=CARTESIAN_POINT('Ctrl Pts',(0.304027795567048,2.20690348838222,7.69329684979915));
#47927=CARTESIAN_POINT('Ctrl Pts',(0.304121899395974,2.20663548478306,7.69327925177198));
#47928=CARTESIAN_POINT('Ctrl Pts',(0.304417013387696,2.20579144486279,7.69322392111731));
#47929=CARTESIAN_POINT('Ctrl Pts',(0.304616743712643,2.20521495763587,7.69318626434405));
#47930=CARTESIAN_POINT('Ctrl Pts',(0.306243275281436,2.20047679917998,7.69287783985467));
#47931=CARTESIAN_POINT('Ctrl Pts',(0.307586443668984,2.19628663032616,7.69261190017591));
#47932=CARTESIAN_POINT('Ctrl Pts',(0.309068066355403,2.19131661433761,7.6923030020691));
#47933=CARTESIAN_POINT('Ctrl Pts',(0.309289911141217,2.19056237951671,7.6922563005768));
#47934=CARTESIAN_POINT('Ctrl Pts',(0.309580368312466,2.18956135761991,7.69219454212545));
#47935=CARTESIAN_POINT('Ctrl Pts',(0.309651447808156,2.18931529597151,7.69217937915355));
#47936=CARTESIAN_POINT('Ctrl Pts',(0.310049387808336,2.18793152990474,7.69209420707266));
#47937=CARTESIAN_POINT('Ctrl Pts',(0.310370275394789,2.18679210248744,7.69202445125741));
#47938=CARTESIAN_POINT('Ctrl Pts',(0.310865343323021,2.1849963234899,7.69191506889997));
#47939=CARTESIAN_POINT('Ctrl Pts',(0.311043736859899,2.18434115519104,7.69187527800773));
#47940=CARTESIAN_POINT('Ctrl Pts',(0.312250913383368,2.17985175269101,7.6916033822025));
#47941=CARTESIAN_POINT('Ctrl Pts',(0.313210878349691,2.17599923096801,7.69137386166672));
#47942=CARTESIAN_POINT('Ctrl Pts',(0.319194996612592,2.14994055075332,7.68984102013498));
#47943=CARTESIAN_POINT('Ctrl Pts',(0.321925106773675,2.12727320697862,7.68859865064319));
#47944=CARTESIAN_POINT('Ctrl Pts',(0.322452276600562,2.08957678888074,7.68645655304354));
#47945=CARTESIAN_POINT('Ctrl Pts',(0.321623277967013,2.07465250924172,7.68558980112057));
#47946=CARTESIAN_POINT('Ctrl Pts',(0.319565568121816,2.05826830383893,7.68459345918561));
#47947=CARTESIAN_POINT('Ctrl Pts',(0.319356507955438,2.05669748873085,7.68449749010102));
#47948=CARTESIAN_POINT('Ctrl Pts',(0.318969817998894,2.05394727782015,7.68432865493393));
#47949=CARTESIAN_POINT('Ctrl Pts',(0.318797208936006,2.05276719858829,7.68425594770765));
#47950=CARTESIAN_POINT('Ctrl Pts',(0.318537829094903,2.05106011563028,7.68415038172025));
#47951=CARTESIAN_POINT('Ctrl Pts',(0.318456290863451,2.05053231710819,7.68411768876079));
#47952=CARTESIAN_POINT('Ctrl Pts',(0.318311742732613,2.04961182438213,7.68406057651435));
#47953=CARTESIAN_POINT('Ctrl Pts',(0.318249316970781,2.04921903851926,7.68403617579677));
#47954=CARTESIAN_POINT('Ctrl Pts',(0.318127323567945,2.04846051086689,7.68398899565218));
#47955=CARTESIAN_POINT('Ctrl Pts',(0.318067851856139,2.04809475407585,7.68396621930408));
#47956=CARTESIAN_POINT('Ctrl Pts',(0.317925366198668,2.04722789421895,7.68391217535038));
#47957=CARTESIAN_POINT('Ctrl Pts',(0.317841798330907,2.04672688435821,7.68388089019409));
#47958=CARTESIAN_POINT('Ctrl Pts',(0.317543980476996,2.04496704026556,7.68377082123326));
#47959=CARTESIAN_POINT('Ctrl Pts',(0.317323435633818,2.04370929636171,7.683691837601));
#47960=CARTESIAN_POINT('Ctrl Pts',(0.313989508940211,2.02533872515421,7.68253346398495));
#47961=CARTESIAN_POINT('Ctrl Pts',(0.309503761528585,2.00850705349701,7.68140947520557));
#47962=CARTESIAN_POINT('Ctrl Pts',(0.29633089604837,1.97142476521467,7.67879294243829));
#47963=CARTESIAN_POINT('Ctrl Pts',(0.286882759074541,1.95153521874486,7.67728633007985));
#47964=CARTESIAN_POINT('Ctrl Pts',(0.270324818629718,1.92425989159784,7.67516073364978));
#47965=CARTESIAN_POINT('Ctrl Pts',(0.264772292228484,1.91600062753646,7.67450910296599));
#47966=CARTESIAN_POINT('Ctrl Pts',(0.258275410574658,1.90724132861538,7.67381983589781));
#47967=CARTESIAN_POINT('Ctrl Pts',(0.257701353896647,1.90647453564209,7.67375951421455));
#47968=CARTESIAN_POINT('Ctrl Pts',(0.256703317221129,1.90515372931929,7.67365565571933));
#47969=CARTESIAN_POINT('Ctrl Pts',(0.256280945013804,1.90459851711187,7.67361201209042));
#47970=CARTESIAN_POINT('Ctrl Pts',(0.255672196735265,1.90380368100727,7.67354955802662));
#47971=CARTESIAN_POINT('Ctrl Pts',(0.255487283471672,1.90356294709039,7.67353064581493));
#47972=CARTESIAN_POINT('Ctrl Pts',(0.255165626488035,1.90314541244769,7.67349785046666));
#47973=CARTESIAN_POINT('Ctrl Pts',(0.255029038665879,1.90296849231727,7.673483956254));
#47974=CARTESIAN_POINT('Ctrl Pts',(0.254766535228941,1.9026292058856,7.67345731488647));
#47975=CARTESIAN_POINT('Ctrl Pts',(0.254640648610336,1.90246681818537,7.67344456569951));
#47976=CARTESIAN_POINT('Ctrl Pts',(0.254342872797104,1.90208345936735,7.67341447181077));
#47977=CARTESIAN_POINT('Ctrl Pts',(0.254170850469058,1.90186259118507,7.67339713661001));
#47978=CARTESIAN_POINT('Ctrl Pts',(0.253571825685649,1.9010955367722,7.67333694270671));
#47979=CARTESIAN_POINT('Ctrl Pts',(0.253143344844011,1.90055049948498,7.67329418838059));
#47980=CARTESIAN_POINT('Ctrl Pts',(0.247865730512999,1.89388165981178,7.67277121500526));
#47981=CARTESIAN_POINT('Ctrl Pts',(0.242796793238019,1.88793413484025,7.6723063513108));
#47982=CARTESIAN_POINT('Ctrl Pts',(0.235061795773159,1.87949985309156,7.67163948122397));
#47983=CARTESIAN_POINT('Ctrl Pts',(0.232562226727042,1.8768651195644,7.67143000010558));
#47984=CARTESIAN_POINT('Ctrl Pts',(0.220114113797254,1.86418033252392,7.67041245032402));
#47985=CARTESIAN_POINT('Ctrl Pts',(0.209555669042481,1.85474993233711,7.66962698761722));
#47986=CARTESIAN_POINT('Ctrl Pts',(0.187017419806823,1.8371412325432,7.6680269456287));
#47987=CARTESIAN_POINT('Ctrl Pts',(0.175037743125708,1.82901661985489,7.66721372768));
#47988=CARTESIAN_POINT('Ctrl Pts',(0.155142907425573,1.81739512364424,7.66587635244263));
#47989=CARTESIAN_POINT('Ctrl Pts',(0.147562577890504,1.8133641607922,7.66536979145524));
#47990=CARTESIAN_POINT('Ctrl Pts',(0.138313832672107,1.80891016080787,7.66475095368425));
#47991=CARTESIAN_POINT('Ctrl Pts',(0.136791108982915,1.80819149579284,7.66464904792931));
#47992=CARTESIAN_POINT('Ctrl Pts',(0.134126284729243,1.80695924625846,7.66447064072923));
#47993=CARTESIAN_POINT('Ctrl Pts',(0.132986683523375,1.80644032030109,7.6643943240974));
#47994=CARTESIAN_POINT('Ctrl Pts',(0.131346967133883,1.8057051705048,7.66428447475699));
#47995=CARTESIAN_POINT('Ctrl Pts',(0.130849272853981,1.80548354845492,7.66425112738441));
#47996=CARTESIAN_POINT('Ctrl Pts',(0.129985601072845,1.80510157886302,7.66419324787234));
#47997=CARTESIAN_POINT('Ctrl Pts',(0.129619881822688,1.80494064748038,7.6641687357784));
#47998=CARTESIAN_POINT('Ctrl Pts',(0.128916815425657,1.8046328289998,7.66412160670282));
#47999=CARTESIAN_POINT('Ctrl Pts',(0.1285795139396,1.80448583858389,7.66409899329681));
#48000=CARTESIAN_POINT('Ctrl Pts',(0.127785359018117,1.80414137606551,7.66404574435649));
#48001=CARTESIAN_POINT('Ctrl Pts',(0.127328299366518,1.80394438442787,7.66401509248783));
#48002=CARTESIAN_POINT('Ctrl Pts',(0.125979991339732,1.80336696668039,7.66392465332999));
#48003=CARTESIAN_POINT('Ctrl Pts',(0.125087487227659,1.80298950324854,7.66386476537995));
#48004=CARTESIAN_POINT('Ctrl Pts',(0.117265435853685,1.79972286270666,7.66333968117115));
#48005=CARTESIAN_POINT('Ctrl Pts',(0.110239103848264,1.79707283652941,7.66286644664725));
#48006=CARTESIAN_POINT('Ctrl Pts',(0.0981072334794383,1.79297521244836,
7.66204572664159));
#48007=CARTESIAN_POINT('Ctrl Pts',(0.0930465495521231,1.79140384948237,
7.66170234868581));
#48008=CARTESIAN_POINT('Ctrl Pts',(0.0603274886091704,1.78212242975367,
7.6594764318773));
#48009=CARTESIAN_POINT('Ctrl Pts',(0.0317869188846806,1.77801428794589,
7.65749237595424));
#48010=CARTESIAN_POINT('Ctrl Pts',(-0.0032785813727824,1.77767890100403,
7.65517154459606));
#48011=CARTESIAN_POINT('Ctrl Pts',(-0.00964031750125043,1.77780640050279,
7.65475588859718));
#48012=CARTESIAN_POINT('Ctrl Pts',(-0.0190281107768603,1.77827289205018,
7.6541543236124));
#48013=CARTESIAN_POINT('Ctrl Pts',(-0.0220595511489733,1.77846651987733,
7.65396189790555));
#48014=CARTESIAN_POINT('Ctrl Pts',(-0.0255935536621075,1.77874246647417,
7.65374005698777));
#48015=CARTESIAN_POINT('Ctrl Pts',(-0.026099084727614,1.77878314082089,
7.65370838260688));
#48016=CARTESIAN_POINT('Ctrl Pts',(-0.0268699155485872,1.7788469925712,
7.65366017857142));
#48017=CARTESIAN_POINT('Ctrl Pts',(-0.0271352831383519,1.77886930549637,
7.65364360055792));
#48018=CARTESIAN_POINT('Ctrl Pts',(-0.0275966724623211,1.77890867652815,
7.65361480626225));
#48019=CARTESIAN_POINT('Ctrl Pts',(-0.0277927057233755,1.77892558518442,
7.65360258155675));
#48020=CARTESIAN_POINT('Ctrl Pts',(-0.0282042132336269,1.77896145905994,
7.65357693936672));
#48021=CARTESIAN_POINT('Ctrl Pts',(-0.0284196831959511,1.7789804616215,
7.65356352405902));
#48022=CARTESIAN_POINT('Ctrl Pts',(-0.0290223604883649,1.77903422401482,
7.65352603197075));
#48023=CARTESIAN_POINT('Ctrl Pts',(-0.0294095259536415,1.77906946772076,
7.65350198252304));
#48024=CARTESIAN_POINT('Ctrl Pts',(-0.0309763745742602,1.77921495726464,
7.65340479660584));
#48025=CARTESIAN_POINT('Ctrl Pts',(-0.0321555284653409,1.77933100942571,
7.6533319829053));
#48026=CARTESIAN_POINT('Ctrl Pts',(-0.053145567281961,1.7815137906095,7.65204119512836));
#48027=CARTESIAN_POINT('Ctrl Pts',(-0.0727268769049766,1.78540664800537,
7.65092082264426));
#48028=CARTESIAN_POINT('Ctrl Pts',(-0.107433872294403,1.79572335754646,
7.64889468959375));
#48029=CARTESIAN_POINT('Ctrl Pts',(-0.122667531086389,1.80153901420385,
7.64798993551845));
#48030=CARTESIAN_POINT('Ctrl Pts',(-0.149568954146757,1.81421790492987,
7.64628410424557));
#48031=CARTESIAN_POINT('Ctrl Pts',(-0.161369344547343,1.82071136276686,
7.6454942299687));
#48032=CARTESIAN_POINT('Ctrl Pts',(-0.173786365843938,1.82859431669487,
7.644600482914));
#48033=CARTESIAN_POINT('Ctrl Pts',(-0.174840344003534,1.8292720924564,7.64452411125783));
#48034=CARTESIAN_POINT('Ctrl Pts',(-0.176346978998829,1.83025342334575,
7.64441419676429));
#48035=CARTESIAN_POINT('Ctrl Pts',(-0.176802869575741,1.83055201258365,
7.64438083956893));
#48036=CARTESIAN_POINT('Ctrl Pts',(-0.177591717370694,1.83107153884446,
7.64432294848826));
#48037=CARTESIAN_POINT('Ctrl Pts',(-0.177925026087404,1.83129194208652,
7.64429843467079));
#48038=CARTESIAN_POINT('Ctrl Pts',(-0.17856442200477,1.83171645937319,7.64425130614526));
#48039=CARTESIAN_POINT('Ctrl Pts',(-0.178870571488163,1.83192047890429,
7.64422869502012));
#48040=CARTESIAN_POINT('Ctrl Pts',(-0.179589942148884,1.83240165196644,
7.64417545733146));
#48041=CARTESIAN_POINT('Ctrl Pts',(-0.180002871277948,1.83267923851936,
7.64414481445069));
#48042=CARTESIAN_POINT('Ctrl Pts',(-0.181217654310668,1.83349995243937,
7.64405441912576));
#48043=CARTESIAN_POINT('Ctrl Pts',(-0.18201769938503,1.83404573577127,7.64399456615848));
#48044=CARTESIAN_POINT('Ctrl Pts',(-0.188985559195315,1.83884531256288,
7.64347046600645));
#48045=CARTESIAN_POINT('Ctrl Pts',(-0.195005300669939,1.84330907706944,
7.64299821369596));
#48046=CARTESIAN_POINT('Ctrl Pts',(-0.20397453112219,1.85045763658458,7.64226315361172));
#48047=CARTESIAN_POINT('Ctrl Pts',(-0.207039114221632,1.85299432486107,
7.64200607128229));
#48048=CARTESIAN_POINT('Ctrl Pts',(-0.210778729385711,1.85620826231229,
7.64168493909231));
#48049=CARTESIAN_POINT('Ctrl Pts',(-0.21149883458691,1.85683271793421,7.64162275255913));
#48050=CARTESIAN_POINT('Ctrl Pts',(-0.232341510556716,1.87506954066465,
7.63981268522344));
#48051=CARTESIAN_POINT('Ctrl Pts',(-0.250195821429652,1.89511460141647,
7.63797371214083));
#48052=CARTESIAN_POINT('Ctrl Pts',(-0.267835062377407,1.92071118793796,
7.63589935327861));
#48053=CARTESIAN_POINT('Ctrl Pts',(-0.270230772097741,1.92434285849792,
7.63561102781066));
#48054=CARTESIAN_POINT('Ctrl Pts',(-0.27521311259121,1.93223891925396,7.63499848803226));
#48055=CARTESIAN_POINT('Ctrl Pts',(-0.27777586338533,1.93651723863508,7.63467526186131));
#48056=CARTESIAN_POINT('Ctrl Pts',(-0.281451229785814,1.94298913276123,
7.63420096549317));
#48057=CARTESIAN_POINT('Ctrl Pts',(-0.282639611846494,1.94513858492036,
7.634045792782));
#48058=CARTESIAN_POINT('Ctrl Pts',(-0.284029823044681,1.9477224123098,7.63386224360101));
#48059=CARTESIAN_POINT('Ctrl Pts',(-0.284255362659158,1.94814384142204,
7.63383240020002));
#48060=CARTESIAN_POINT('Ctrl Pts',(-0.284602165231953,1.94879533472415,
7.63378641161154));
#48061=CARTESIAN_POINT('Ctrl Pts',(-0.284724087499885,1.94902504428084,
7.63377022462839));
#48062=CARTESIAN_POINT('Ctrl Pts',(-0.284937529398125,1.94942836096993,
7.63374185365469));
#48063=CARTESIAN_POINT('Ctrl Pts',(-0.285029168105033,1.94960190337098,
7.63372966207365));
#48064=CARTESIAN_POINT('Ctrl Pts',(-0.285223201931387,1.94997017260727,
7.63370382483848));
#48065=CARTESIAN_POINT('Ctrl Pts',(-0.285325555848573,1.95016491996903,
7.63369018184432));
#48066=CARTESIAN_POINT('Ctrl Pts',(-0.28561674014468,1.95072033256433,7.63365132961324));
#48067=CARTESIAN_POINT('Ctrl Pts',(-0.28580508751784,1.95108125264486,7.63362615108747));
#48068=CARTESIAN_POINT('Ctrl Pts',(-0.286606060792816,1.95262323200482,
7.6335188676442));
#48069=CARTESIAN_POINT('Ctrl Pts',(-0.287212064810507,1.95380774370986,
7.63343717555367));
#48070=CARTESIAN_POINT('Ctrl Pts',(-0.298832582732669,1.97687269148309,
7.63185974129093));
#48071=CARTESIAN_POINT('Ctrl Pts',(-0.307326241200577,1.99993876185725,
7.63050971479041));
#48072=CARTESIAN_POINT('Ctrl Pts',(-0.316576616682861,2.03792484663418,
7.62832296292454));
#48073=CARTESIAN_POINT('Ctrl Pts',(-0.319062011034038,2.05231909367544,
7.62750290103042));
#48074=CARTESIAN_POINT('Ctrl Pts',(-0.321307279135699,2.07401883205741,
7.62623727577414));
#48075=CARTESIAN_POINT('Ctrl Pts',(-0.321808983891043,2.08122886849482,
7.62581216283101));
#48076=CARTESIAN_POINT('Ctrl Pts',(-0.322205907641382,2.09229629730358,
7.625149169922));
#48077=CARTESIAN_POINT('Ctrl Pts',(-0.322274934450132,2.09614531122044,
7.62491667787055));
#48078=CARTESIAN_POINT('Ctrl Pts',(-0.322275012560333,2.10073534831961,
7.62463685322158));
#48079=CARTESIAN_POINT('Ctrl Pts',(-0.322272470674025,2.10147617382821,
7.62459161021307));
#48080=CARTESIAN_POINT('Ctrl Pts',(-0.322264040947298,2.10270154660044,
7.62451664118377));
#48081=CARTESIAN_POINT('Ctrl Pts',(-0.322259614566028,2.10318610379868,
7.62448696097681));
#48082=CARTESIAN_POINT('Ctrl Pts',(-0.322249638207019,2.10406195006513,
7.62443325001728));
#48083=CARTESIAN_POINT('Ctrl Pts',(-0.322244468355237,2.10445324322182,
7.62440923121972));
#48084=CARTESIAN_POINT('Ctrl Pts',(-0.322231878006127,2.10529070336594,
7.62435777590945));
#48085=CARTESIAN_POINT('Ctrl Pts',(-0.322224243519934,2.10573686589341,
7.62433033274114));
#48086=CARTESIAN_POINT('Ctrl Pts',(-0.322201049386374,2.10694558371266,
7.62425590326289));
#48087=CARTESIAN_POINT('Ctrl Pts',(-0.322183709335855,2.10770809842889,
7.62420886126446));
#48088=CARTESIAN_POINT('Ctrl Pts',(-0.322083778834763,2.11150879818129,
7.62397393648265));
#48089=CARTESIAN_POINT('Ctrl Pts',(-0.32196092150771,2.11454568759986,7.62378479630448));
#48090=CARTESIAN_POINT('Ctrl Pts',(-0.320149619479709,2.14770030120993,
7.62170360951507));
#48091=CARTESIAN_POINT('Ctrl Pts',(-0.314283651835385,2.17743423378051,
7.61966890457982));
#48092=CARTESIAN_POINT('Ctrl Pts',(-0.299501198459806,2.21991722276558,
7.61662892371279));
#48093=CARTESIAN_POINT('Ctrl Pts',(-0.29366599319579,2.23357200756451,7.61563349308438));
#48094=CARTESIAN_POINT('Ctrl Pts',(-0.285393098602287,2.24974329184827,
7.61446801931277));
#48095=CARTESIAN_POINT('Ctrl Pts',(-0.2838298458655,2.25268560811725,7.61425657520329));
#48096=CARTESIAN_POINT('Ctrl Pts',(-0.281953167585538,2.25608938152167,
7.61401314920497));
#48097=CARTESIAN_POINT('Ctrl Pts',(-0.281683903331657,2.25657478197366,
7.61397846339922));
#48098=CARTESIAN_POINT('Ctrl Pts',(-0.281276896181146,2.25730404233566,
7.61392639733413));
#48099=CARTESIAN_POINT('Ctrl Pts',(-0.281140089068572,2.2575484191618,7.61390895758748));
#48100=CARTESIAN_POINT('Ctrl Pts',(-0.280895753895735,2.25798354032395,
7.61387791971167));
#48101=CARTESIAN_POINT('Ctrl Pts',(-0.280788350070565,2.25817435328037,
7.61386431361034));
#48102=CARTESIAN_POINT('Ctrl Pts',(-0.280559814423472,2.2585794019552,7.61383544171803));
#48103=CARTESIAN_POINT('Ctrl Pts',(-0.280438631993344,2.25879360780736,
7.61382017930754));
#48104=CARTESIAN_POINT('Ctrl Pts',(-0.280112584150046,2.25936840282566,
7.61377924057742));
#48105=CARTESIAN_POINT('Ctrl Pts',(-0.279907267003762,2.25972873724372,
7.61375359341748));
#48106=CARTESIAN_POINT('Ctrl Pts',(-0.278918237708143,2.26145673412273,
7.61363067831788));
#48107=CARTESIAN_POINT('Ctrl Pts',(-0.278125176680091,2.26281906108981,
7.61353400522015));
#48108=CARTESIAN_POINT('Ctrl Pts',(-0.271434516950736,2.27412079307144,
7.61273348041306));
#48109=CARTESIAN_POINT('Ctrl Pts',(-0.265015456679295,2.28374334872336,
7.61206128561747));
#48110=CARTESIAN_POINT('Ctrl Pts',(-0.245219124383414,2.31021616496064,
7.6101777642012));
#48111=CARTESIAN_POINT('Ctrl Pts',(-0.230655604560742,2.32610020952501,
7.60900129228236));
#48112=CARTESIAN_POINT('Ctrl Pts',(-0.2103688989993,2.34421006175128,7.60745496164659));
#48113=CARTESIAN_POINT('Ctrl Pts',(-0.206019484597079,2.34789028970342,
7.60712836035628));
#48114=CARTESIAN_POINT('Ctrl Pts',(-0.193324407773146,2.35806717188198,
7.60618467668596));
#48115=CARTESIAN_POINT('Ctrl Pts',(-0.184754129243422,2.36427044351863,
7.60555871226171));
#48116=CARTESIAN_POINT('Ctrl Pts',(-0.174907758963399,2.37068402242334,
7.60484427687951));
#48117=CARTESIAN_POINT('Ctrl Pts',(-0.173916883153688,2.37132173122931,
7.60477243577162));
#48118=CARTESIAN_POINT('Ctrl Pts',(-0.172518929807106,2.37221062295483,
7.60467114932794));
#48119=CARTESIAN_POINT('Ctrl Pts',(-0.172114748051081,2.37246636102584,
7.60464187304257));
#48120=CARTESIAN_POINT('Ctrl Pts',(-0.171371907842553,2.37293406611667,
7.60458808062709));
#48121=CARTESIAN_POINT('Ctrl Pts',(-0.171033421154564,2.37314630528429,
7.60456357462077));
#48122=CARTESIAN_POINT('Ctrl Pts',(-0.17034630544416,2.37357536511947,7.6045138387218));
#48123=CARTESIAN_POINT('Ctrl Pts',(-0.169997655088973,2.37379215007099,
7.60448860757195));
#48124=CARTESIAN_POINT('Ctrl Pts',(-0.169137563833894,2.37432466418967,
7.60442637723015));
#48125=CARTESIAN_POINT('Ctrl Pts',(-0.168625653609846,2.37463962900368,
7.60438935000865));
#48126=CARTESIAN_POINT('Ctrl Pts',(-0.16675038675377,2.37578621153987,7.60425374743221));
#48127=CARTESIAN_POINT('Ctrl Pts',(-0.165381752374354,2.37660911371873,
7.60415485354738));
#48128=CARTESIAN_POINT('Ctrl Pts',(-0.146978990865274,2.38748851527267,
7.60282595798942));
#48129=CARTESIAN_POINT('Ctrl Pts',(-0.12906353312393,2.39596421313499,7.60153778345662));
#48130=CARTESIAN_POINT('Ctrl Pts',(-0.0832043903394734,2.41270066680676,
7.59826908696113));
#48131=CARTESIAN_POINT('Ctrl Pts',(-0.0547007130052508,2.41892415240699,
7.59625520978267));
#48132=CARTESIAN_POINT('Ctrl Pts',(-0.0242493089166614,2.4213649157781,
7.59432298354425));
#48133=CARTESIAN_POINT('Ctrl Pts',(-0.0227491149093209,2.4214745962844,
7.59422837807063));
#48134=CARTESIAN_POINT('Ctrl Pts',(-0.0208221765119838,2.42160191985776,
7.59410766053092));
#48135=CARTESIAN_POINT('Ctrl Pts',(-0.0203961209035794,2.42162922153932,
7.59408101942023));
#48136=CARTESIAN_POINT('Ctrl Pts',(-0.0197216549529017,2.42167109579288,
7.59403892598978));
#48137=CARTESIAN_POINT('Ctrl Pts',(-0.0194732817371178,2.42168622731175,
7.59402344232937));
#48138=CARTESIAN_POINT('Ctrl Pts',(-0.0190285844068785,2.42171280247151,
7.59399575106658));
#48139=CARTESIAN_POINT('Ctrl Pts',(-0.0188322687539985,2.42172435399345,
7.5939835374557));
#48140=CARTESIAN_POINT('Ctrl Pts',(-0.0183711820407109,2.42175106158005,
7.59395487694845));
#48141=CARTESIAN_POINT('Ctrl Pts',(-0.0181064031620623,2.4217660704972,
7.59393843845871));
#48142=CARTESIAN_POINT('Ctrl Pts',(-0.0173404047640351,2.4218085423998,
7.5938909388223));
#48143=CARTESIAN_POINT('Ctrl Pts',(-0.0168391363612734,2.42183516136918,
7.59385992506942));
#48144=CARTESIAN_POINT('Ctrl Pts',(-0.0134187945711616,2.42200877961112,
7.59364877140263));
#48145=CARTESIAN_POINT('Ctrl Pts',(-0.0104977808456938,2.42211723989591,
7.59347075270674));
#48146=CARTESIAN_POINT('Ctrl Pts',(-0.00132634554620723,2.42233288829333,
7.59291792362431));
#48147=CARTESIAN_POINT('Ctrl Pts',(0.00492627010779293,2.42229798725449,
7.59254993392689));
#48148=CARTESIAN_POINT('Ctrl Pts',(0.0258773434048393,2.4215711085741,7.59133511651112));
#48149=CARTESIAN_POINT('Ctrl Pts',(0.0405291705360306,2.42005477347917,
7.59051509368766));
#48150=CARTESIAN_POINT('Ctrl Pts',(0.0809207473943615,2.41305532048777,
7.58822377012808));
#48151=CARTESIAN_POINT('Ctrl Pts',(0.106164201112711,2.40541889452105,7.58674752101773));
#48152=CARTESIAN_POINT('Ctrl Pts',(0.131638097417043,2.39416842278127,7.58505924560763));
#48153=CARTESIAN_POINT('Ctrl Pts',(0.133072233736145,2.39352245250589,7.58496353428421));
#48154=CARTESIAN_POINT('Ctrl Pts',(0.135061868145168,2.39260869357318,7.58482980213474));
#48155=CARTESIAN_POINT('Ctrl Pts',(0.135621429216146,2.39234976263117,7.58479208656868));
#48156=CARTESIAN_POINT('Ctrl Pts',(0.13651780691399,2.39193184605432,7.5847314989662));
#48157=CARTESIAN_POINT('Ctrl Pts',(0.13685509887333,2.39177387863853,7.58470866216084));
#48158=CARTESIAN_POINT('Ctrl Pts',(0.137550978047257,2.3914464982619,7.58466146640298));
#48159=CARTESIAN_POINT('Ctrl Pts',(0.137909527772785,2.39127700743138,7.58463710478184));
#48160=CARTESIAN_POINT('Ctrl Pts',(0.138743923894916,2.39088069218651,7.58458030846892));
#48161=CARTESIAN_POINT('Ctrl Pts',(0.139219527416752,2.39065336173052,7.5845478562532));
#48162=CARTESIAN_POINT('Ctrl Pts',(0.140711811462084,2.38993557203582,7.58444578394137));
#48163=CARTESIAN_POINT('Ctrl Pts',(0.14172646585146,2.38944094154418,7.58437601881658));
#48164=CARTESIAN_POINT('Ctrl Pts',(0.14407832963174,2.38827910749902,7.58421345639649));
#48165=CARTESIAN_POINT('Ctrl Pts',(0.14541353019546,2.38760791714572,7.58412052052132));
#48166=CARTESIAN_POINT('Ctrl Pts',(0.158768703088818,2.38077764948709,7.58318435867983));
#48167=CARTESIAN_POINT('Ctrl Pts',(0.170393314493812,2.37387884731757,7.58231487139548));
#48168=CARTESIAN_POINT('Ctrl Pts',(0.203905702221498,2.35102941570835,7.57963934501254));
#48169=CARTESIAN_POINT('Ctrl Pts',(0.224250369378604,2.33303403981466,7.57777069744263));
#48170=CARTESIAN_POINT('Ctrl Pts',(0.247673522535706,2.30637378384858,7.5754281009044));
#48171=CARTESIAN_POINT('Ctrl Pts',(0.25299007412235,2.2998208301106,7.57488132485539));
#48172=CARTESIAN_POINT('Ctrl Pts',(0.258466467468066,2.29250132071328,7.57430772057541));
#48173=CARTESIAN_POINT('Ctrl Pts',(0.258887231028642,2.29193507994713,7.57426357916349));
#48174=CARTESIAN_POINT('Ctrl Pts',(0.259473622729053,2.29114050928364,7.57420196883209));
#48175=CARTESIAN_POINT('Ctrl Pts',(0.259640811652717,2.29091334187836,7.57418439212511));
#48176=CARTESIAN_POINT('Ctrl Pts',(0.259929596537574,2.29051987536498,7.57415401382545));
#48177=CARTESIAN_POINT('Ctrl Pts',(0.260051331302166,2.29035367911808,7.57414120252334));
#48178=CARTESIAN_POINT('Ctrl Pts',(0.26030455590277,2.29000727240368,7.57411454183504));
#48179=CARTESIAN_POINT('Ctrl Pts',(0.260436017847515,2.28982704232549,7.57410069446151));
#48180=CARTESIAN_POINT('Ctrl Pts',(0.260744560786202,2.28940311610561,7.5740681789972));
#48181=CARTESIAN_POINT('Ctrl Pts',(0.260921488019095,2.28915930709794,7.57404952166692));
#48182=CARTESIAN_POINT('Ctrl Pts',(0.261504069283991,2.28835412674925,7.57398804619438));
#48183=CARTESIAN_POINT('Ctrl Pts',(0.26190825908423,2.28779169087037,7.57394532904591));
#48184=CARTESIAN_POINT('Ctrl Pts',(0.26285971052841,2.28645868565359,7.57384460599064));
#48185=CARTESIAN_POINT('Ctrl Pts',(0.263405405254352,2.2856869984904,7.57378670440569));
#48186=CARTESIAN_POINT('Ctrl Pts',(0.269521128736105,2.27695731504426,7.57313614234069));
#48187=CARTESIAN_POINT('Ctrl Pts',(0.274732630187969,2.2687529322488,7.5725662089561));
#48188=CARTESIAN_POINT('Ctrl Pts',(0.291256749695207,2.23993903986594,7.57065786270303));
#48189=CARTESIAN_POINT('Ctrl Pts',(0.300683125987645,2.21833512994233,7.56937754214408));
#48190=CARTESIAN_POINT('Ctrl Pts',(0.309340247696754,2.19055961705398,7.56772329617016));
#48191=CARTESIAN_POINT('Ctrl Pts',(0.310864643604397,2.18517982460951,7.56740283203414));
#48192=CARTESIAN_POINT('Ctrl Pts',(0.312738450200803,2.1778444570412,7.56696393816779));
#48193=CARTESIAN_POINT('Ctrl Pts',(0.313210903433455,2.17592119258759,7.56684868834335));
#48194=CARTESIAN_POINT('Ctrl Pts',(0.314233673941263,2.17158558258391,7.56658836759382));
#48195=CARTESIAN_POINT('Ctrl Pts',(0.314773991934716,2.16917102735421,7.56644303590235));
#48196=CARTESIAN_POINT('Ctrl Pts',(0.316625658353819,2.16042495009888,7.56591499409328));
#48197=CARTESIAN_POINT('Ctrl Pts',(0.317774126741131,2.15406086912351,7.56552767751639));
#48198=CARTESIAN_POINT('Ctrl Pts',(0.31888288275281,2.14664703678556,7.56507143013392));
#48199=CARTESIAN_POINT('Ctrl Pts',(0.319030504679153,2.14562648352688,7.56500851625671));
#48200=CARTESIAN_POINT('Ctrl Pts',(0.319242869932705,2.14410690220001,7.56491467096175));
#48201=CARTESIAN_POINT('Ctrl Pts',(0.319311347510404,2.14360839564927,7.56488385767587));
#48202=CARTESIAN_POINT('Ctrl Pts',(0.319431255130404,2.14272005948985,7.56482889998561));
#48203=CARTESIAN_POINT('Ctrl Pts',(0.319483139871732,2.14233029142974,7.5648047700017));
#48204=CARTESIAN_POINT('Ctrl Pts',(0.319590885417222,2.14150940337449,7.56475391455107));
#48205=CARTESIAN_POINT('Ctrl Pts',(0.319646587440673,2.14107826365432,7.56472718412046));
#48206=CARTESIAN_POINT('Ctrl Pts',(0.319791123668784,2.13994144123875,7.5646566468676));
#48207=CARTESIAN_POINT('Ctrl Pts',(0.319878494007736,2.13923557778284,7.56461279392752));
#48208=CARTESIAN_POINT('Ctrl Pts',(0.320254082230644,2.13611654603187,7.56441876834588));
#48209=CARTESIAN_POINT('Ctrl Pts',(0.320517328251993,2.13370050225922,7.56426781063846));
#48210=CARTESIAN_POINT('Ctrl Pts',(0.322241461733275,2.11602178832246,7.56315813270546));
#48211=CARTESIAN_POINT('Ctrl Pts',(0.322638615669189,2.10067736613264,7.56216586445049));
#48212=CARTESIAN_POINT('Ctrl Pts',(0.321024072160057,2.06516094890958,7.55980589436602));
#48213=CARTESIAN_POINT('Ctrl Pts',(0.318205749563082,2.04508888687443,7.55842310022286));
#48214=CARTESIAN_POINT('Ctrl Pts',(0.3112213683268,2.01572921455733,7.55639931242098));
#48215=CARTESIAN_POINT('Ctrl Pts',(0.30846929553496,2.00615419812249,7.55573987930658));
#48216=CARTESIAN_POINT('Ctrl Pts',(0.304164835325749,1.99343079867157,7.55487721536471));
#48217=CARTESIAN_POINT('Ctrl Pts',(0.302998466266723,1.99015841596484,7.55465660527946));
#48218=CARTESIAN_POINT('Ctrl Pts',(0.301579595397936,1.98637233037963,7.55440336276679));
#48219=CARTESIAN_POINT('Ctrl Pts',(0.301378419201365,1.98583981379132,7.55436779039634));
#48220=CARTESIAN_POINT('Ctrl Pts',(0.301076507557982,1.98504700911461,7.55431490292469));
#48221=CARTESIAN_POINT('Ctrl Pts',(0.300976844606996,1.9847863179625,7.55429752406024));
#48222=CARTESIAN_POINT('Ctrl Pts',(0.300798423864968,1.98432142927908,7.55426655370896));
#48223=CARTESIAN_POINT('Ctrl Pts',(0.300719796781136,1.98411718268589,7.55425295438335));
#48224=CARTESIAN_POINT('Ctrl Pts',(0.300552099837198,1.98368288274994,7.55422405318424));
#48225=CARTESIAN_POINT('Ctrl Pts',(0.300462974131646,1.98345285220625,7.5542087547803));
#48226=CARTESIAN_POINT('Ctrl Pts',(0.300225395873851,1.98284175425108,7.55416813741884));
#48227=CARTESIAN_POINT('Ctrl Pts',(0.300076481336337,1.98246086512246,7.55414284630165));
#48228=CARTESIAN_POINT('Ctrl Pts',(0.299389780388169,1.98071425303928,7.55402698182272));
#48229=CARTESIAN_POINT('Ctrl Pts',(0.29884338172013,1.97935190252861,7.55393691957966));
#48230=CARTESIAN_POINT('Ctrl Pts',(0.297341554388725,1.97568016480934,7.55369490980117));
#48231=CARTESIAN_POINT('Ctrl Pts',(0.296368519725182,1.97337803210946,7.55354394858653));
#48232=CARTESIAN_POINT('Ctrl Pts',(0.291443737818718,1.96209421278481,7.55280675364703));
#48233=CARTESIAN_POINT('Ctrl Pts',(0.287109661761195,1.95328416956538,7.55223970998044));
#48234=CARTESIAN_POINT('Ctrl Pts',(0.274293111893614,1.92998226696738,7.55072790677214));
#48235=CARTESIAN_POINT('Ctrl Pts',(0.265070226324213,1.91593330454104,7.54980203519208));
#48236=CARTESIAN_POINT('Ctrl Pts',(0.242464370990616,1.88674490658963,7.54772382239498));
#48237=CARTESIAN_POINT('Ctrl Pts',(0.228670644922105,1.87201697627745,7.54656617174874));
#48238=CARTESIAN_POINT('Ctrl Pts',(0.212623316888819,1.85781374409654,7.54526457019303));
#48239=CARTESIAN_POINT('Ctrl Pts',(0.211647041977099,1.85696011237066,7.54518556233573));
#48240=CARTESIAN_POINT('Ctrl Pts',(0.210278703804204,1.85577816683088,7.54507506127651));
#48241=CARTESIAN_POINT('Ctrl Pts',(0.209890962046846,1.85544485056259,7.54504377508017));
#48242=CARTESIAN_POINT('Ctrl Pts',(0.209220181226333,1.85487099444814,7.54498969522928));
#48243=CARTESIAN_POINT('Ctrl Pts',(0.208937515696878,1.85463001787552,7.54496691960581));
#48244=CARTESIAN_POINT('Ctrl Pts',(0.208351743984256,1.85413238491025,7.54491974892185));
#48245=CARTESIAN_POINT('Ctrl Pts',(0.208048578798419,1.85387579918065,7.54489535101623));
#48246=CARTESIAN_POINT('Ctrl Pts',(0.207339177167758,1.85327763997268,7.54483829532017));
#48247=CARTESIAN_POINT('Ctrl Pts',(0.206932570588245,1.8529365090702,7.54480561951618));
#48248=CARTESIAN_POINT('Ctrl Pts',(0.205653023738887,1.85186838169474,7.54470287462788));
#48249=CARTESIAN_POINT('Ctrl Pts',(0.204777088236436,1.85114500154472,7.5446326586909));
#48250=CARTESIAN_POINT('Ctrl Pts',(0.197609528716323,1.84528923114833,7.54405903884289));
#48251=CARTESIAN_POINT('Ctrl Pts',(0.191130324921618,1.84039206238747,7.54354625952028));
#48252=CARTESIAN_POINT('Ctrl Pts',(0.178579007283364,1.83163011975778,7.54256219323574));
#48253=CARTESIAN_POINT('Ctrl Pts',(0.172548761275471,1.8277138130265,7.54209317529982));
#48254=CARTESIAN_POINT('Ctrl Pts',(0.151675411926663,1.81512971494047,7.540483732037));
#48255=CARTESIAN_POINT('Ctrl Pts',(0.136272606435354,1.80744879769435,7.53931750175913));
#48256=CARTESIAN_POINT('Ctrl Pts',(0.106556436857898,1.79548822311279,7.53715255983061));
#48257=CARTESIAN_POINT('Ctrl Pts',(0.0924122603638716,1.7909016995955,7.53615570693693));
#48258=CARTESIAN_POINT('Ctrl Pts',(0.0747580804812318,1.78649788599447,
7.53498818197458));
#48259=CARTESIAN_POINT('Ctrl Pts',(0.0715026797447825,1.78573941538994,
7.53477604367247));
#48260=CARTESIAN_POINT('Ctrl Pts',(0.0676928872400136,1.7849140476611,7.53453190674288));
#48261=CARTESIAN_POINT('Ctrl Pts',(0.067149551285568,1.78479780756267,7.53449718650707));
#48262=CARTESIAN_POINT('Ctrl Pts',(0.0663317815304237,1.78462506617525,
7.53444507882713));
#48263=CARTESIAN_POINT('Ctrl Pts',(0.0660575737829031,1.78456751740933,
7.53442763175605));
#48264=CARTESIAN_POINT('Ctrl Pts',(0.065568924220027,1.78446562825542,7.5343965857413));
#48265=CARTESIAN_POINT('Ctrl Pts',(0.0653545124012318,1.78442114886214,
7.5343829788094));
#48266=CARTESIAN_POINT('Ctrl Pts',(0.0648990938932745,1.78432715705738,
7.53435411036995));
#48267=CARTESIAN_POINT('Ctrl Pts',(0.0646580764842503,1.78427770223506,
7.53433885223227));
#48268=CARTESIAN_POINT('Ctrl Pts',(0.0641663974572591,1.78417740030453,
7.53430776508113));
#48269=CARTESIAN_POINT('Ctrl Pts',(0.0639157314028306,1.78412657547466,
7.534291937355));
#48270=CARTESIAN_POINT('Ctrl Pts',(0.0628083458540102,1.78390341510573,
7.53422210579653));
#48271=CARTESIAN_POINT('Ctrl Pts',(0.0619509773232575,1.78373426404194,
7.53416828266879));
#48272=CARTESIAN_POINT('Ctrl Pts',(0.0519130690448392,1.78179626065547,
7.53354085279353));
#48273=CARTESIAN_POINT('Ctrl Pts',(0.042659420702781,1.78042403395442,7.53298901330319));
#48274=CARTESIAN_POINT('Ctrl Pts',(0.0178512208005186,1.7778423027169,7.53154894943875));
#48275=CARTESIAN_POINT('Ctrl Pts',(0.00224658758511204,1.77735583104859,
7.53068321965015));
#48276=CARTESIAN_POINT('Ctrl Pts',(-0.0379802010981444,1.77902146602183,
7.52843150563953));
#48277=CARTESIAN_POINT('Ctrl Pts',(-0.0624248212311037,1.78286815416693,
7.52703754896194));
#48278=CARTESIAN_POINT('Ctrl Pts',(-0.0877004801231903,1.7898834753987,
7.52544722052646));
#48279=CARTESIAN_POINT('Ctrl Pts',(-0.0892078935221977,1.79031373191127,
7.52535182891117));
#48280=CARTESIAN_POINT('Ctrl Pts',(-0.091243820050598,1.79091093840867,
7.52522223193371));
#48281=CARTESIAN_POINT('Ctrl Pts',(-0.0917751468354167,1.79106828406568,
7.52518833999142));
#48282=CARTESIAN_POINT('Ctrl Pts',(-0.0926730664815594,1.79133671241478,
7.52513094405815));
#48283=CARTESIAN_POINT('Ctrl Pts',(-0.0930398732411064,1.79144708016412,
7.52510746347001));
#48284=CARTESIAN_POINT('Ctrl Pts',(-0.0937445739298334,1.7916604870061,
7.52506228750086));
#48285=CARTESIAN_POINT('Ctrl Pts',(-0.0940824971307662,1.79176342827843,
7.52504059534894));
#48286=CARTESIAN_POINT('Ctrl Pts',(-0.0948773456276642,1.79200699120386,
7.52498950329017));
#48287=CARTESIAN_POINT('Ctrl Pts',(-0.0953341277067271,1.79214807411492,
7.52496008829877));
#48288=CARTESIAN_POINT('Ctrl Pts',(-0.0962761231922259,1.79244131891022,
7.52489931628724));
#48289=CARTESIAN_POINT('Ctrl Pts',(-0.0967612934914672,1.79259361378182,
7.52486795496452));
#48290=CARTESIAN_POINT('Ctrl Pts',(-0.0993671534427551,1.79341837305484,
7.5246991825705));
#48291=CARTESIAN_POINT('Ctrl Pts',(-0.101481155332473,1.7941116218667,7.52456108919647));
#48292=CARTESIAN_POINT('Ctrl Pts',(-0.106910936629241,1.795954702199,7.52420328642237));
#48293=CARTESIAN_POINT('Ctrl Pts',(-0.110215347118491,1.79713688375507,
7.52398252026518));
#48294=CARTESIAN_POINT('Ctrl Pts',(-0.123256843566522,1.80204428469662,
7.52309891674368));
#48295=CARTESIAN_POINT('Ctrl Pts',(-0.132829150366764,1.80618673115128,
7.522422561808));
#48296=CARTESIAN_POINT('Ctrl Pts',(-0.148908090752129,1.81409142863004,
7.52123918277111));
#48297=CARTESIAN_POINT('Ctrl Pts',(-0.155515365740656,1.81763092905609,
7.52073843167385));
#48298=CARTESIAN_POINT('Ctrl Pts',(-0.168562369622535,1.82521708521451,
7.51972297983916));
#48299=CARTESIAN_POINT('Ctrl Pts',(-0.174994489767446,1.82926794067524,
7.51920848888541));
#48300=CARTESIAN_POINT('Ctrl Pts',(-0.187441691855888,1.83773605815151,
7.5181898347031));
#48301=CARTESIAN_POINT('Ctrl Pts',(-0.193458833235073,1.84214258220365,
7.5176859579647));
#48302=CARTESIAN_POINT('Ctrl Pts',(-0.203570969802908,1.85010135992561,
7.51682453662116));
#48303=CARTESIAN_POINT('Ctrl Pts',(-0.207739287428554,1.85355555682766,
7.51646488231769));
#48304=CARTESIAN_POINT('Ctrl Pts',(-0.212515825302974,1.85772112144741,
7.51604902183058));
#48305=CARTESIAN_POINT('Ctrl Pts',(-0.213210247398883,1.85833200163361,
7.51598846870124));
#48306=CARTESIAN_POINT('Ctrl Pts',(-0.214971466007757,1.85989483835236,
7.5158346700473));
#48307=CARTESIAN_POINT('Ctrl Pts',(-0.216034585987816,1.86085093008981,
7.51574162411408));
#48308=CARTESIAN_POINT('Ctrl Pts',(-0.220696159768779,1.86509965827603,
7.51533283979826));
#48309=CARTESIAN_POINT('Ctrl Pts',(-0.224226190465064,1.86846687622728,
7.51502116480095));
#48310=CARTESIAN_POINT('Ctrl Pts',(-0.228078878583547,1.87231266928341,
7.51467995886498));
#48311=CARTESIAN_POINT('Ctrl Pts',(-0.228478062748095,1.87271324218259,
7.51464459312363));
#48312=CARTESIAN_POINT('Ctrl Pts',(-0.229075844019567,1.87331626936495,
7.5145916164118));
#48313=CARTESIAN_POINT('Ctrl Pts',(-0.22927522902502,1.87351793579856,7.51457394373858));
#48314=CARTESIAN_POINT('Ctrl Pts',(-0.229619274895249,1.87386683828749,
7.51454344462709));
#48315=CARTESIAN_POINT('Ctrl Pts',(-0.229764060532985,1.87401395017069,
7.51453060829693));
#48316=CARTESIAN_POINT('Ctrl Pts',(-0.230064824307084,1.87432013409637,
7.51450394079749));
#48317=CARTESIAN_POINT('Ctrl Pts',(-0.230220778636816,1.87447922858003,
7.51449011156606));
#48318=CARTESIAN_POINT('Ctrl Pts',(-0.230590386026518,1.87485706097979,
7.5144573330169));
#48319=CARTESIAN_POINT('Ctrl Pts',(-0.230803893717613,1.87507594222682,
7.51443839521842));
#48320=CARTESIAN_POINT('Ctrl Pts',(-0.231253604834724,1.87553828624729,
7.51439849951627));
#48321=CARTESIAN_POINT('Ctrl Pts',(-0.231489736260967,1.8757818189839,7.51437754723012));
#48322=CARTESIAN_POINT('Ctrl Pts',(-0.233345248485676,1.87770154601116,
7.5142128681196));
#48323=CARTESIAN_POINT('Ctrl Pts',(-0.234946842027292,1.87939494610053,
7.5140705035166));
#48324=CARTESIAN_POINT('Ctrl Pts',(-0.244971942730091,1.89022773659585,
7.51317680826665));
#48325=CARTESIAN_POINT('Ctrl Pts',(-0.252880151030457,1.89983168073971,
7.51245997667805));
#48326=CARTESIAN_POINT('Ctrl Pts',(-0.262793871626641,1.9133997002042,7.51150813021452));
#48327=CARTESIAN_POINT('Ctrl Pts',(-0.26530118673752,1.91698204352252,7.51126216520915));
#48328=CARTESIAN_POINT('Ctrl Pts',(-0.270338993073633,1.92450101960656,
7.51075461215123));
#48329=CARTESIAN_POINT('Ctrl Pts',(-0.272858184186224,1.92844395931527,
7.5104931973824));
#48330=CARTESIAN_POINT('Ctrl Pts',(-0.289000375558909,1.95496463270848,
7.50875785285587));
#48331=CARTESIAN_POINT('Ctrl Pts',(-0.299891877787051,1.97908236426809,
7.50727732056974));
#48332=CARTESIAN_POINT('Ctrl Pts',(-0.308198753504487,2.00578081184131,
7.50558244820183));
#48333=CARTESIAN_POINT('Ctrl Pts',(-0.308661949323304,2.00730950439274,
7.50548526057534));
#48334=CARTESIAN_POINT('Ctrl Pts',(-0.309289288275958,2.0094367796197,7.50534979821011));
#48335=CARTESIAN_POINT('Ctrl Pts',(-0.309463100668061,2.01003250562389,
7.50531183930185));
#48336=CARTESIAN_POINT('Ctrl Pts',(-0.309738690007361,2.01098731083547,
7.50525096096381));
#48337=CARTESIAN_POINT('Ctrl Pts',(-0.309841566292714,2.01134607332355,
7.50522807740225));
#48338=CARTESIAN_POINT('Ctrl Pts',(-0.310052361187806,2.01208603123744,
7.50518086075317));
#48339=CARTESIAN_POINT('Ctrl Pts',(-0.310160200518773,2.01246724845129,
7.50515652512878));
#48340=CARTESIAN_POINT('Ctrl Pts',(-0.310409172756363,2.01335361411052,
7.50509991841269));
#48341=CARTESIAN_POINT('Ctrl Pts',(-0.31054977567526,2.01385890909759,7.50506763015492));
#48342=CARTESIAN_POINT('Ctrl Pts',(-0.310841336687314,2.01491670506265,
7.50499999828144));
#48343=CARTESIAN_POINT('Ctrl Pts',(-0.310992056538391,2.01546926929101,
7.50496464704371));
#48344=CARTESIAN_POINT('Ctrl Pts',(-0.311390816912086,2.0169466938652,7.50487006571209));
#48345=CARTESIAN_POINT('Ctrl Pts',(-0.311636208425057,2.01787225752665,
7.50481074990936));
#48346=CARTESIAN_POINT('Ctrl Pts',(-0.318807568914593,2.04541604167657,
7.50304362771498));
#48347=CARTESIAN_POINT('Ctrl Pts',(-0.32229988735354,2.07280360298413,7.50121750797054));
#48348=CARTESIAN_POINT('Ctrl Pts',(-0.322274866506699,2.10029333102401,
7.49935788809917));
#48349=CARTESIAN_POINT('',(-0.322274930854165,2.09978888878902,7.24958594529397));
#48350=CARTESIAN_POINT('Ctrl Pts',(-0.3222748664569,2.10029338573071,7.49935788439838));
#48351=CARTESIAN_POINT('Ctrl Pts',(-0.322256148867363,2.12085406076409,
7.49796699976951));
#48352=CARTESIAN_POINT('Ctrl Pts',(-0.32026987284514,2.14136841321006,7.49656915266215));
#48353=CARTESIAN_POINT('Ctrl Pts',(-0.316036440817217,2.16312446084035,
7.49515703326928));
#48354=CARTESIAN_POINT('Ctrl Pts',(-0.315719530582268,2.16469086279529,
7.49505578198484));
#48355=CARTESIAN_POINT('Ctrl Pts',(-0.315246160168358,2.16694423279244,
7.49491079344328));
#48356=CARTESIAN_POINT('Ctrl Pts',(-0.315099084757041,2.16763311771638,
7.4948665587458));
#48357=CARTESIAN_POINT('Ctrl Pts',(-0.314867627852968,2.16870009180598,
7.49479819198427));
#48358=CARTESIAN_POINT('Ctrl Pts',(-0.314784822419493,2.16907851519781,
7.49477397283448));
#48359=CARTESIAN_POINT('Ctrl Pts',(-0.314645821839494,2.169708312048,7.49473371422418));
#48360=CARTESIAN_POINT('Ctrl Pts',(-0.314590007564058,2.1699597678068,7.49471765325297));
#48361=CARTESIAN_POINT('Ctrl Pts',(-0.314480012267058,2.17045252779108,
7.49468620532467));
#48362=CARTESIAN_POINT('Ctrl Pts',(-0.314425854843617,2.1706938370333,7.49467081702622));
#48363=CARTESIAN_POINT('Ctrl Pts',(-0.3143232702153,2.17114847348537,7.49464184787286));
#48364=CARTESIAN_POINT('Ctrl Pts',(-0.314274903972807,2.17136181199602,
7.49462826367718));
#48365=CARTESIAN_POINT('Ctrl Pts',(-0.314164558954814,2.17184624453556,
7.49459743937047));
#48366=CARTESIAN_POINT('Ctrl Pts',(-0.3141024466065,2.17211730717617,7.49458020709278));
#48367=CARTESIAN_POINT('Ctrl Pts',(-0.313913245118711,2.17293811440616,
7.49452807148614));
#48368=CARTESIAN_POINT('Ctrl Pts',(-0.313785062160527,2.17348760963862,
7.49449323094113));
#48369=CARTESIAN_POINT('Ctrl Pts',(-0.312880417515829,2.17732012028061,
7.49425064696944));
#48370=CARTESIAN_POINT('Ctrl Pts',(-0.312053854676782,2.1805912565325,7.49404572263869));
#48371=CARTESIAN_POINT('Ctrl Pts',(-0.306216681283326,2.20225387933492,
7.49269916672607));
#48372=CARTESIAN_POINT('Ctrl Pts',(-0.299633534603359,2.22018505556726,
7.49163389924475));
#48373=CARTESIAN_POINT('Ctrl Pts',(-0.289457747551807,2.24176878259547,
7.49029993250223));
#48374=CARTESIAN_POINT('Ctrl Pts',(-0.287316058560702,2.2460604585875,7.4900320691688));
#48375=CARTESIAN_POINT('Ctrl Pts',(-0.282909093467116,2.25441915591365,
7.48950273342651));
#48376=CARTESIAN_POINT('Ctrl Pts',(-0.280649907131427,2.25848804179969,
7.48924137168973));
#48377=CARTESIAN_POINT('Ctrl Pts',(-0.2717069996401,2.27380337679313,7.48823955893468));
#48378=CARTESIAN_POINT('Ctrl Pts',(-0.264429468513943,2.28468706850848,
7.48748912588319));
#48379=CARTESIAN_POINT('Ctrl Pts',(-0.252879255027259,2.29987309179203,
7.48635933114148));
#48380=CARTESIAN_POINT('Ctrl Pts',(-0.249114815842532,2.30454576941058,
7.48599934154322));
#48381=CARTESIAN_POINT('Ctrl Pts',(-0.244780983532403,2.3096280239124,7.48559262678683));
#48382=CARTESIAN_POINT('Ctrl Pts',(-0.244337990561368,2.31014419969589,
7.48555114017175));
#48383=CARTESIAN_POINT('Ctrl Pts',(-0.243500167241692,2.31111420138257,
7.48547283803754));
#48384=CARTESIAN_POINT('Ctrl Pts',(-0.243105693402326,2.31156833245967,
7.48543603732991));
#48385=CARTESIAN_POINT('Ctrl Pts',(-0.242439786592579,2.31233062459253,
7.48537402463752));
#48386=CARTESIAN_POINT('Ctrl Pts',(-0.242169030773929,2.31263937733743,
7.4853488408685));
#48387=CARTESIAN_POINT('Ctrl Pts',(-0.241633748075659,2.31324743133717,
7.48529911212876));
#48388=CARTESIAN_POINT('Ctrl Pts',(-0.241369253353059,2.31354676001872,
7.48527456852713));
#48389=CARTESIAN_POINT('Ctrl Pts',(-0.240787036270638,2.31420319152479,
7.48522060400899));
#48390=CARTESIAN_POINT('Ctrl Pts',(-0.240469074986136,2.31456008031968,
7.48519117309404));
#48391=CARTESIAN_POINT('Ctrl Pts',(-0.239365751913833,2.31579294838065,
7.48508918597513));
#48392=CARTESIAN_POINT('Ctrl Pts',(-0.23857639527869,2.31666532559936,7.4850164615074));
#48393=CARTESIAN_POINT('Ctrl Pts',(-0.230690068668203,2.32528574526313,
7.48429221632307));
#48394=CARTESIAN_POINT('Ctrl Pts',(-0.223223729345604,2.33268584008681,
7.48362484107357));
#48395=CARTESIAN_POINT('Ctrl Pts',(-0.203788037593394,2.35015147042133,
7.48192838818911));
#48396=CARTESIAN_POINT('Ctrl Pts',(-0.191423099767726,2.35973529640472,
7.4808829546149));
#48397=CARTESIAN_POINT('Ctrl Pts',(-0.166958339490506,2.37599871630057,
7.4788978917401));
#48398=CARTESIAN_POINT('Ctrl Pts',(-0.155027370340201,2.38287260654162,
7.47796288691117));
#48399=CARTESIAN_POINT('Ctrl Pts',(-0.135936493037989,2.39229990637292,
7.47654621627203));
#48400=CARTESIAN_POINT('Ctrl Pts',(-0.129064034909462,2.39539881158071,
7.47605130926519));
#48401=CARTESIAN_POINT('Ctrl Pts',(-0.120069346449577,2.39908073987667,
7.47542816131802));
#48402=CARTESIAN_POINT('Ctrl Pts',(-0.11804153945444,2.39988686612559,7.47528925393823));
#48403=CARTESIAN_POINT('Ctrl Pts',(-0.114763121449796,2.40115174787086,
7.47506738763831));
#48404=CARTESIAN_POINT('Ctrl Pts',(-0.113517617810498,2.40162344054064,
7.47498372271904));
#48405=CARTESIAN_POINT('Ctrl Pts',(-0.111997193671826,2.40218849819525,
7.47488238022768));
#48406=CARTESIAN_POINT('Ctrl Pts',(-0.111725049195026,2.40228922113732,
7.47486427140049));
#48407=CARTESIAN_POINT('Ctrl Pts',(-0.111198881186578,2.40248315269234,
7.47482931938073));
#48408=CARTESIAN_POINT('Ctrl Pts',(-0.110944875725595,2.40257640917852,
7.47481247334759));
#48409=CARTESIAN_POINT('Ctrl Pts',(-0.110505523445552,2.40273708694421,
7.47478338171066));
#48410=CARTESIAN_POINT('Ctrl Pts',(-0.110320232472824,2.40280465787592,
7.47477112711516));
#48411=CARTESIAN_POINT('Ctrl Pts',(-0.109933632884527,2.4029452390131,7.47474558868799));
#48412=CARTESIAN_POINT('Ctrl Pts',(-0.109732314139043,2.40301821845265,
7.47473230673486));
#48413=CARTESIAN_POINT('Ctrl Pts',(-0.109175432523116,2.40321946414261,
7.47469561317175));
#48414=CARTESIAN_POINT('Ctrl Pts',(-0.108819715038369,2.40334730610965,
7.47467222698715));
#48415=CARTESIAN_POINT('Ctrl Pts',(-0.107422883494162,2.40384654280272,
7.47458059674391));
#48416=CARTESIAN_POINT('Ctrl Pts',(-0.106380070833977,2.40421321155415,
7.47451263094273));
#48417=CARTESIAN_POINT('Ctrl Pts',(-0.0863796914773394,2.41113022973626,
7.47321715804945));
#48418=CARTESIAN_POINT('Ctrl Pts',(-0.0668500557929338,2.41590315961686,
7.47208915106601));
#48419=CARTESIAN_POINT('Ctrl Pts',(-0.029756093109937,2.42137141781679,
7.46999106991032));
#48420=CARTESIAN_POINT('Ctrl Pts',(-0.0123341175448777,2.42251022386957,
7.46902278526492));
#48421=CARTESIAN_POINT('Ctrl Pts',(0.0158488738851317,2.42206473698776,
7.46739919359314));
#48422=CARTESIAN_POINT('Ctrl Pts',(0.0265879506236351,2.42135638527742,
7.46676748368368));
#48423=CARTESIAN_POINT('Ctrl Pts',(0.0396630146128743,2.41983405270604,
7.46597331126771));
#48424=CARTESIAN_POINT('Ctrl Pts',(0.042052001768259,2.41952872274597,7.46582718977463));
#48425=CARTESIAN_POINT('Ctrl Pts',(0.0449529182336699,2.41912486864711,
7.46564845260593));
#48426=CARTESIAN_POINT('Ctrl Pts',(0.0454683659394383,2.41905183644757,
7.46561664366199));
#48427=CARTESIAN_POINT('Ctrl Pts',(0.0464654502293034,2.41890809731526,
7.46555501431353));
#48428=CARTESIAN_POINT('Ctrl Pts',(0.0469471082955741,2.4188375473761,7.46552519894448));
#48429=CARTESIAN_POINT('Ctrl Pts',(0.0477790582931503,2.41871376304104,
7.46547362275445));
#48430=CARTESIAN_POINT('Ctrl Pts',(0.0481294266619008,2.4186610416269,7.46545187821662));
#48431=CARTESIAN_POINT('Ctrl Pts',(0.0488544601962142,2.41855071972302,
7.46540683191041));
#48432=CARTESIAN_POINT('Ctrl Pts',(0.0492291119619132,2.41849303579615,
7.46538352752728));
#48433=CARTESIAN_POINT('Ctrl Pts',(0.0501369425737913,2.41835161991995,
7.46532699138407));
#48434=CARTESIAN_POINT('Ctrl Pts',(0.0506700131728285,2.41826720955152,
7.46529373815168));
#48435=CARTESIAN_POINT('Ctrl Pts',(0.0526563749244304,2.41794755731416,
7.46516961848217));
#48436=CARTESIAN_POINT('Ctrl Pts',(0.0541082435990096,2.41770369982331,
7.46507847896578));
#48437=CARTESIAN_POINT('Ctrl Pts',(0.0783998173217289,2.41345231953319,
7.46354645000756));
#48438=CARTESIAN_POINT('Ctrl Pts',(0.100738229690627,2.40700209701137,7.46202394020688));
#48439=CARTESIAN_POINT('Ctrl Pts',(0.139974304090959,2.39092586057203,7.45916737392671));
#48440=CARTESIAN_POINT('Ctrl Pts',(0.157073803193341,2.38206120185136,7.45785326633061));
#48441=CARTESIAN_POINT('Ctrl Pts',(0.176562180793679,2.36963328845313,7.45633337378648));
#48442=CARTESIAN_POINT('Ctrl Pts',(0.179804689857287,2.36748194349376,7.4560798043916));
#48443=CARTESIAN_POINT('Ctrl Pts',(0.185168879024069,2.36378126602448,7.45566014921166));
#48444=CARTESIAN_POINT('Ctrl Pts',(0.187311954218957,2.3622638039696,7.4554924455028));
#48445=CARTESIAN_POINT('Ctrl Pts',(0.190257157140956,2.36012385369726,7.45526217518852));
#48446=CARTESIAN_POINT('Ctrl Pts',(0.191075186377482,2.35952356024068,7.45519823978699));
#48447=CARTESIAN_POINT('Ctrl Pts',(0.192478318089588,2.35848367110059,7.45508863166866));
#48448=CARTESIAN_POINT('Ctrl Pts',(0.193064777710871,2.35804593155583,7.45504283681663));
#48449=CARTESIAN_POINT('Ctrl Pts',(0.193899626310528,2.35741835261863,7.45497767713172));
#48450=CARTESIAN_POINT('Ctrl Pts',(0.194149232494296,2.35723014767346,7.45495819943117));
#48451=CARTESIAN_POINT('Ctrl Pts',(0.194577250795883,2.3569064407297,7.45492480699595));
#48452=CARTESIAN_POINT('Ctrl Pts',(0.194755795848042,2.35677111558819,7.45491087978578));
#48453=CARTESIAN_POINT('Ctrl Pts',(0.195097331117153,2.35651169365386,7.45488424319191));
#48454=CARTESIAN_POINT('Ctrl Pts',(0.195260343893612,2.35638762780864,7.45487153164527));
#48455=CARTESIAN_POINT('Ctrl Pts',(0.195643937640691,2.35609510405909,7.4548416237388));
#48456=CARTESIAN_POINT('Ctrl Pts',(0.195864419927916,2.35592651614522,7.45482443659565));
#48457=CARTESIAN_POINT('Ctrl Pts',(0.19651466827868,2.35542798268336,7.45477375709313));
#48458=CARTESIAN_POINT('Ctrl Pts',(0.196943823100979,2.35509723585095,7.45474032092688));
#48459=CARTESIAN_POINT('Ctrl Pts',(0.200684744625027,2.35219906486205,7.45444894098944));
#48460=CARTESIAN_POINT('Ctrl Pts',(0.203947168455363,2.34956821030212,7.45419538982303));
#48461=CARTESIAN_POINT('Ctrl Pts',(0.207909278925225,2.34624351847994,7.45388685497364));
#48462=CARTESIAN_POINT('Ctrl Pts',(0.20865814578828,2.3456092768959,7.45382851242839));
#48463=CARTESIAN_POINT('Ctrl Pts',(0.209524006723595,2.34486913057721,7.45376100769521));
#48464=CARTESIAN_POINT('Ctrl Pts',(0.209643825882845,2.34476655566586,7.45375166522729));
#48465=CARTESIAN_POINT('Ctrl Pts',(0.218689053673119,2.33701159333229,7.45304631180361));
#48466=CARTESIAN_POINT('Ctrl Pts',(0.227189922892183,2.32887591523492,7.4523770134302));
#48467=CARTESIAN_POINT('Ctrl Pts',(0.248365887101111,2.30626434631992,7.45063386979542));
#48468=CARTESIAN_POINT('Ctrl Pts',(0.260222348964725,2.29108875917186,7.44957440173897));
#48469=CARTESIAN_POINT('Ctrl Pts',(0.274087031677675,2.26963909701135,7.44811295759442));
#48470=CARTESIAN_POINT('Ctrl Pts',(0.277361063397851,2.26423141685269,7.44774753750449));
#48471=CARTESIAN_POINT('Ctrl Pts',(0.284404303374136,2.25178619502868,7.44690917036536));
#48472=CARTESIAN_POINT('Ctrl Pts',(0.288075151265587,2.24469812598262,7.44643345189702));
#48473=CARTESIAN_POINT('Ctrl Pts',(0.291969671682161,2.23644123099065,7.44587833913174));
#48474=CARTESIAN_POINT('Ctrl Pts',(0.292454786025875,2.23539828940314,7.44580820716518));
#48475=CARTESIAN_POINT('Ctrl Pts',(0.293156055662486,2.2338692854938,7.44570536061037));
#48476=CARTESIAN_POINT('Ctrl Pts',(0.293376611096474,2.23338524141147,7.44567279767047));
#48477=CARTESIAN_POINT('Ctrl Pts',(0.293759832181104,2.23253865292845,7.44561583698913));
#48478=CARTESIAN_POINT('Ctrl Pts',(0.293923028004244,2.23217634860174,7.44559145752605));
#48479=CARTESIAN_POINT('Ctrl Pts',(0.294237347332648,2.23147508050822,7.44554426361299));
#48480=CARTESIAN_POINT('Ctrl Pts',(0.294388556292057,2.23113615551207,7.44552145213994));
#48481=CARTESIAN_POINT('Ctrl Pts',(0.294746207760265,2.23033076706264,7.44546723883642));
#48482=CARTESIAN_POINT('Ctrl Pts',(0.294952128409696,2.22986407422381,7.44543581919425));
#48483=CARTESIAN_POINT('Ctrl Pts',(0.295674766276936,2.22821572262734,7.44532482639256));
#48484=CARTESIAN_POINT('Ctrl Pts',(0.296185492182256,2.22703146494067,7.44524504896239));
#48485=CARTESIAN_POINT('Ctrl Pts',(0.304054344869696,2.20847993073549,7.44399469654815));
#48486=CARTESIAN_POINT('Ctrl Pts',(0.309879654226826,2.19050586986265,7.44277131467218));
#48487=CARTESIAN_POINT('Ctrl Pts',(0.318939143645388,2.15105428844335,7.44006934895851));
#48488=CARTESIAN_POINT('Ctrl Pts',(0.321645163145963,2.1295476166933,7.43858568653543));
#48489=CARTESIAN_POINT('Ctrl Pts',(0.322396680236011,2.09902481245934,7.4365598366538));
#48490=CARTESIAN_POINT('Ctrl Pts',(0.322246503158223,2.09011092691619,7.43597847884219));
#48491=CARTESIAN_POINT('Ctrl Pts',(0.321674558105754,2.08031590912717,7.4353588626651));
#48492=CARTESIAN_POINT('Ctrl Pts',(0.321618362843058,2.07941812708317,7.43530224939695));
#48493=CARTESIAN_POINT('Ctrl Pts',(0.321513969064208,2.07785529637812,7.43520402412813));
#48494=CARTESIAN_POINT('Ctrl Pts',(0.321467464533293,2.07719014539081,7.43516232148929));
#48495=CARTESIAN_POINT('Ctrl Pts',(0.321397069694121,2.07622629606025,7.43510204505617));
#48496=CARTESIAN_POINT('Ctrl Pts',(0.321374826981954,2.07592748473781,7.43508337963269));
#48497=CARTESIAN_POINT('Ctrl Pts',(0.321335399694965,2.07540760906809,7.43505094304603));
#48498=CARTESIAN_POINT('Ctrl Pts',(0.321318403685415,2.07518653101374,7.43503716121823));
#48499=CARTESIAN_POINT('Ctrl Pts',(0.321285021172363,2.07475808916135,7.4350104757295));
#48500=CARTESIAN_POINT('Ctrl Pts',(0.321268662115585,2.07455072426189,7.43499757053294));
#48501=CARTESIAN_POINT('Ctrl Pts',(0.321229042514617,2.07405463875162,7.43496672189154));
#48502=CARTESIAN_POINT('Ctrl Pts',(0.32120559341837,2.07376593276972,7.43494878911579));
#48503=CARTESIAN_POINT('Ctrl Pts',(0.321120017701663,2.07272963877179,7.43488449151448));
#48504=CARTESIAN_POINT('Ctrl Pts',(0.321055669488469,2.07198222910308,7.43483825079642));
#48505=CARTESIAN_POINT('Ctrl Pts',(0.319967583479091,2.05984025664069,7.43408911240768));
#48506=CARTESIAN_POINT('Ctrl Pts',(0.318340287821569,2.04850644511515,7.43341925405515));
#48507=CARTESIAN_POINT('Ctrl Pts',(0.311727611273277,2.0151770601363,7.4314744492046));
#48508=CARTESIAN_POINT('Ctrl Pts',(0.305035414923231,1.99359268157072,7.43024399081669));
#48509=CARTESIAN_POINT('Ctrl Pts',(0.293109356794663,1.96580857784914,7.42852521655843));
#48510=CARTESIAN_POINT('Ctrl Pts',(0.289820706986139,1.95884625418442,7.42808278107872));
#48511=CARTESIAN_POINT('Ctrl Pts',(0.282339133133295,1.94437331146014,7.42713050809979));
#48512=CARTESIAN_POINT('Ctrl Pts',(0.278088604211423,1.93689953913959,7.42661919375738));
#48513=CARTESIAN_POINT('Ctrl Pts',(0.272900112816633,1.92857015848397,7.42602278861851));
#48514=CARTESIAN_POINT('Ctrl Pts',(0.272249616564854,1.92753896569388,7.42594847575003));
#48515=CARTESIAN_POINT('Ctrl Pts',(0.271299672872987,1.92605184502713,7.42584060437575));
#48516=CARTESIAN_POINT('Ctrl Pts',(0.271004889310201,1.92559293854994,7.42580721922041));
#48517=CARTESIAN_POINT('Ctrl Pts',(0.270492082739039,1.92479906239208,7.42574929520246));
#48518=CARTESIAN_POINT('Ctrl Pts',(0.270274598308973,1.92446374485652,7.42572477647119));
#48519=CARTESIAN_POINT('Ctrl Pts',(0.269855777399204,1.92382063030852,7.42567764947841));
#48520=CARTESIAN_POINT('Ctrl Pts',(0.269654536532754,1.92351277149273,7.42565504482042));
#48521=CARTESIAN_POINT('Ctrl Pts',(0.269180042305668,1.92278959509691,7.42560183905484));
#48522=CARTESIAN_POINT('Ctrl Pts',(0.268906354645396,1.92237456486049,7.42557122167855));
#48523=CARTESIAN_POINT('Ctrl Pts',(0.268097555778,1.92115422543596,7.42548095069198));
#48524=CARTESIAN_POINT('Ctrl Pts',(0.267559783040139,1.92035069451732,7.42542119694882));
#48525=CARTESIAN_POINT('Ctrl Pts',(0.262847412993501,1.91337764506534,7.42489988256722));
#48526=CARTESIAN_POINT('Ctrl Pts',(0.258463992951908,1.90735261399201,7.42443041024048));
#48527=CARTESIAN_POINT('Ctrl Pts',(0.250763755561469,1.8975049543118,7.42362941149909));
#48528=CARTESIAN_POINT('Ctrl Pts',(0.247558409786082,1.89359860930794,7.42330221495336));
#48529=CARTESIAN_POINT('Ctrl Pts',(0.227274373922959,1.87003099896178,7.42126938137369));
#48530=CARTESIAN_POINT('Ctrl Pts',(0.207956845486481,1.85242568746729,7.41948098683476));
#48531=CARTESIAN_POINT('Ctrl Pts',(0.179563963667948,1.83224002846542,7.41715202669159));
#48532=CARTESIAN_POINT('Ctrl Pts',(0.172185123793336,1.82743637720393,7.41657118559141));
#48533=CARTESIAN_POINT('Ctrl Pts',(0.161585891772989,1.8211387134216,7.41577940151565));
#48534=CARTESIAN_POINT('Ctrl Pts',(0.158523928902531,1.81938677137533,7.41555543760338));
#48535=CARTESIAN_POINT('Ctrl Pts',(0.154973502691873,1.81743201698207,7.41530171542751));
#48536=CARTESIAN_POINT('Ctrl Pts',(0.154512715852589,1.81717978818243,7.4152689006621));
#48537=CARTESIAN_POINT('Ctrl Pts',(0.153812099487223,1.81679850310144,7.41521918209965));
#48538=CARTESIAN_POINT('Ctrl Pts',(0.153572722482009,1.81666862386063,7.41520222597913));
#48539=CARTESIAN_POINT('Ctrl Pts',(0.153142985802857,1.81643616541774,7.41517184189014));
#48540=CARTESIAN_POINT('Ctrl Pts',(0.152952687946802,1.81633347459669,7.41515840677859));
#48541=CARTESIAN_POINT('Ctrl Pts',(0.152541771750175,1.81611226476928,7.41512943847377));
#48542=CARTESIAN_POINT('Ctrl Pts',(0.15232111922182,1.81599381171681,7.41511390954674));
#48543=CARTESIAN_POINT('Ctrl Pts',(0.151727283766248,1.81567591373809,7.4150721873302));
#48544=CARTESIAN_POINT('Ctrl Pts',(0.151353844124926,1.81547694550141,7.41504602446059));
#48545=CARTESIAN_POINT('Ctrl Pts',(0.149641106194355,1.81456872682307,7.41492636783102));
#48546=CARTESIAN_POINT('Ctrl Pts',(0.14829717899231,1.81386817848286,7.41483341810335));
#48547=CARTESIAN_POINT('Ctrl Pts',(0.120073828011739,1.79940847331795,7.41289997768157));
#48548=CARTESIAN_POINT('Ctrl Pts',(0.0913925902575469,1.78948255503498,
7.4112758604954));
#48549=CARTESIAN_POINT('Ctrl Pts',(0.0510839991317009,1.78161411153394,
7.40895832228526));
#48550=CARTESIAN_POINT('Ctrl Pts',(0.0403259421009782,1.78007353913178,
7.40833791785853));
#48551=CARTESIAN_POINT('Ctrl Pts',(0.021815880439857,1.7783713901974,7.40724988394123));
#48552=CARTESIAN_POINT('Ctrl Pts',(0.0140980684805651,1.77794080501521,
7.40679024682563));
#48553=CARTESIAN_POINT('Ctrl Pts',(0.00476685903712009,1.77775625320704,
7.40622443236651));
#48554=CARTESIAN_POINT('Ctrl Pts',(0.00316084701995865,1.77773649881983,
7.40612669214987));
#48555=CARTESIAN_POINT('Ctrl Pts',(0.000952368904519933,1.77772584416042,
7.4059917745739));
#48556=CARTESIAN_POINT('Ctrl Pts',(0.000349957359429053,1.77772462698692,
7.40595492045286));
#48557=CARTESIAN_POINT('Ctrl Pts',(-0.000663289832376256,1.77772542070407,
7.4058928430748));
#48558=CARTESIAN_POINT('Ctrl Pts',(-0.00107412630767911,1.77772652814113,
7.40586764816554));
#48559=CARTESIAN_POINT('Ctrl Pts',(-0.00188425704504076,1.77773026104912,
7.40581791704918));
#48560=CARTESIAN_POINT('Ctrl Pts',(-0.00228355084812315,1.77773284303032,
7.40579338224959));
#48561=CARTESIAN_POINT('Ctrl Pts',(-0.00316025595985665,1.77774014157586,
7.40573946056711));
#48562=CARTESIAN_POINT('Ctrl Pts',(-0.00363766303676176,1.77774517695929,
7.40571006374594));
#48563=CARTESIAN_POINT('Ctrl Pts',(-0.00528814499552276,1.77776625330087,
7.40560831521979));
#48564=CARTESIAN_POINT('Ctrl Pts',(-0.00646113167826603,1.77778763880269,
7.40553579630545));
#48565=CARTESIAN_POINT('Ctrl Pts',(-0.0180192627843161,1.77806150153445,
7.40481914240755));
#48566=CARTESIAN_POINT('Ctrl Pts',(-0.0283854975871893,1.77880953589107,
7.40415951578061));
#48567=CARTESIAN_POINT('Ctrl Pts',(-0.0543160398544716,1.7819457943076,
7.40246458473418));
#48568=CARTESIAN_POINT('Ctrl Pts',(-0.0697744874143692,1.78497597981778,
7.40141207689148));
#48569=CARTESIAN_POINT('Ctrl Pts',(-0.0998122426420859,1.79318389065096,
7.39930800134372));
#48570=CARTESIAN_POINT('Ctrl Pts',(-0.114366181895931,1.79830641822693,
7.39825972134003));
#48571=CARTESIAN_POINT('Ctrl Pts',(-0.135591841955927,1.80753485634069,
7.39672907835154));
#48572=CARTESIAN_POINT('Ctrl Pts',(-0.142572839622313,1.81087370443397,
7.39622558390925));
#48573=CARTESIAN_POINT('Ctrl Pts',(-0.15087120020387,1.81521637737996,7.395632696245));
#48574=CARTESIAN_POINT('Ctrl Pts',(-0.152309204673227,1.815982857558,7.39553016773378));
#48575=CARTESIAN_POINT('Ctrl Pts',(-0.154110048343997,1.81696034801517,
7.39540209529559));
#48576=CARTESIAN_POINT('Ctrl Pts',(-0.154478338858534,1.81716118649566,
7.39537592046855));
#48577=CARTESIAN_POINT('Ctrl Pts',(-0.155063011207673,1.8174815063136,7.39533439588912));
#48578=CARTESIAN_POINT('Ctrl Pts',(-0.155279647931368,1.81760051760154,
7.39531901621088));
#48579=CARTESIAN_POINT('Ctrl Pts',(-0.155687774342498,1.81782533705452,
7.39529005428929));
#48580=CARTESIAN_POINT('Ctrl Pts',(-0.155879291648286,1.81793109011507,
7.3952764687259));
#48581=CARTESIAN_POINT('Ctrl Pts',(-0.156314198211469,1.81817181738217,
7.39524562939809));
#48582=CARTESIAN_POINT('Ctrl Pts',(-0.156557519949924,1.81830691164196,
7.39522838349663));
#48583=CARTESIAN_POINT('Ctrl Pts',(-0.157185567195963,1.81865667382187,
7.39518388956498));
#48584=CARTESIAN_POINT('Ctrl Pts',(-0.157570029661558,1.81887181664303,
7.39515667191887));
#48585=CARTESIAN_POINT('Ctrl Pts',(-0.159858453728367,1.82015857381842,
7.39499477447028));
#48586=CARTESIAN_POINT('Ctrl Pts',(-0.161751978224847,1.82124877185239,
7.39486126629297));
#48587=CARTESIAN_POINT('Ctrl Pts',(-0.174017628969615,1.82847780356479,
7.39399842437981));
#48588=CARTESIAN_POINT('Ctrl Pts',(-0.18405070328038,1.83517582507081,7.39330179875718));
#48589=CARTESIAN_POINT('Ctrl Pts',(-0.199162291029895,1.84653894597844,
7.39222913160857));
#48590=CARTESIAN_POINT('Ctrl Pts',(-0.204506090248203,1.85083060498966,
7.39184481462303));
#48591=CARTESIAN_POINT('Ctrl Pts',(-0.219921744576921,1.86404132753134,
7.39070892830626));
#48592=CARTESIAN_POINT('Ctrl Pts',(-0.229576323321482,1.8734238163882,7.38996066094249));
#48593=CARTESIAN_POINT('Ctrl Pts',(-0.248461513796116,1.89422682883049,
7.38836275525745));
#48594=CARTESIAN_POINT('Ctrl Pts',(-0.257554822598136,1.90572917544507,
7.38751164783962));
#48595=CARTESIAN_POINT('Ctrl Pts',(-0.266719764257067,1.91910168910019,
7.3865333247983));
#48596=CARTESIAN_POINT('Ctrl Pts',(-0.267596255156557,1.92040079169268,
7.3864384064434));
#48597=CARTESIAN_POINT('Ctrl Pts',(-0.269117157659774,1.92269086813482,
7.38627127035067));
#48598=CARTESIAN_POINT('Ctrl Pts',(-0.269765661814303,1.92367909812705,
7.38619920709758));
#48599=CARTESIAN_POINT('Ctrl Pts',(-0.270698194424697,1.92511733562127,
7.38609440733066));
#48600=CARTESIAN_POINT('Ctrl Pts',(-0.270986573188863,1.9255645222124,7.38606183324483));
#48601=CARTESIAN_POINT('Ctrl Pts',(-0.271488384100493,1.92634692388116,
7.3860048595828));
#48602=CARTESIAN_POINT('Ctrl Pts',(-0.271702306769198,1.92668182426231,
7.38598047830991));
#48603=CARTESIAN_POINT('Ctrl Pts',(-0.272114786630695,1.92733021045796,
7.38593328562743));
#48604=CARTESIAN_POINT('Ctrl Pts',(-0.272313423004919,1.92764364539386,
7.38591047720357));
#48605=CARTESIAN_POINT('Ctrl Pts',(-0.272783729899214,1.92838860077905,
7.38585627857566));
#48606=CARTESIAN_POINT('Ctrl Pts',(-0.273054917859889,1.92882042333252,
7.38582487058257));
#48607=CARTESIAN_POINT('Ctrl Pts',(-0.273863835219354,1.93011530554338,
7.38573071464839));
#48608=CARTESIAN_POINT('Ctrl Pts',(-0.274398502031193,1.9309802624049,7.38566785401126));
#48609=CARTESIAN_POINT('Ctrl Pts',(-0.279601652634539,1.93948741660023,
7.3850498996918));
#48610=CARTESIAN_POINT('Ctrl Pts',(-0.283953360639575,1.94731785685706,
7.38448331429251));
#48611=CARTESIAN_POINT('Ctrl Pts',(-0.298619715273436,1.97650971785774,
7.38237605312307));
#48612=CARTESIAN_POINT('Ctrl Pts',(-0.306893409966522,1.99880857378941,
7.38076884517529));
#48613=CARTESIAN_POINT('Ctrl Pts',(-0.316887498560611,2.03876964914914,
7.37798522620881));
#48614=CARTESIAN_POINT('Ctrl Pts',(-0.319742721260156,2.05605004994587,
7.37681345156066));
#48615=CARTESIAN_POINT('Ctrl Pts',(-0.321261833893553,2.07444704097285,
7.37565202786818));
#48616=CARTESIAN_POINT('Ctrl Pts',(-0.32133741256755,2.07541571693818,7.37559112814168));
#48617=CARTESIAN_POINT('Ctrl Pts',(-0.321434005681985,2.07673036905404,
7.37550883516746));
#48618=CARTESIAN_POINT('Ctrl Pts',(-0.321458843523721,2.07707604623518,
7.37548723044815));
#48619=CARTESIAN_POINT('Ctrl Pts',(-0.321499305517873,2.0776521695738,7.37545127958592));
#48620=CARTESIAN_POINT('Ctrl Pts',(-0.321515239552147,2.0778825926075,7.37543691598533));
#48621=CARTESIAN_POINT('Ctrl Pts',(-0.32154603052663,2.07833492804234,7.37540874921072));
#48622=CARTESIAN_POINT('Ctrl Pts',(-0.321560905463228,2.07855683865426,
7.37539494505593));
#48623=CARTESIAN_POINT('Ctrl Pts',(-0.321593115302456,2.07904492979591,
7.37536461366112));
#48624=CARTESIAN_POINT('Ctrl Pts',(-0.321610349513846,2.07931111738218,
7.37534809211314));
#48625=CARTESIAN_POINT('Ctrl Pts',(-0.321669001228642,2.08023479618238,
7.37529083070595));
#48626=CARTESIAN_POINT('Ctrl Pts',(-0.321708733508872,2.08089239848766,
7.37525018514761));
#48627=CARTESIAN_POINT('Ctrl Pts',(-0.322080389763401,2.08737369330454,
7.37485073649377));
#48628=CARTESIAN_POINT('Ctrl Pts',(-0.322256185453299,2.09320570549333,
7.37450046333265));
#48629=CARTESIAN_POINT('Ctrl Pts',(-0.322274376855821,2.09931072574119,
7.37414039069863));
#48630=CARTESIAN_POINT('Ctrl Pts',(-0.322274842551218,2.09958174618492,
7.37412441958737));
#48631=CARTESIAN_POINT('Ctrl Pts',(-0.322278290200018,2.10712826112714,
7.37368007800356));
#48632=CARTESIAN_POINT('Ctrl Pts',(-0.322035241626426,2.11440222611218,
7.37326136337437));
#48633=CARTESIAN_POINT('Ctrl Pts',(-0.319419132538126,2.15323497249832,
7.37104886101296));
#48634=CARTESIAN_POINT('Ctrl Pts',(-0.312654214176339,2.18432051894227,
7.36933920997919));
#48635=CARTESIAN_POINT('Ctrl Pts',(-0.299421176891205,2.21933839096461,
7.36712088884723));
#48636=CARTESIAN_POINT('Ctrl Pts',(-0.297229201161761,2.22469758712452,
7.3667734060394));
#48637=CARTESIAN_POINT('Ctrl Pts',(-0.294496872142401,2.23089590572305,
7.36636102440279));
#48638=CARTESIAN_POINT('Ctrl Pts',(-0.294095433399209,2.23179537873788,
7.36630091956592));
#48639=CARTESIAN_POINT('Ctrl Pts',(-0.293483736966334,2.23314924869876,
7.36621005007693));
#48640=CARTESIAN_POINT('Ctrl Pts',(-0.293276530989509,2.23360502482712,
7.36617939034792));
#48641=CARTESIAN_POINT('Ctrl Pts',(-0.292904822714833,2.23441761354625,
7.36612460443478));
#48642=CARTESIAN_POINT('Ctrl Pts',(-0.292740728037082,2.23477461239872,
7.36610049233638));
#48643=CARTESIAN_POINT('Ctrl Pts',(-0.292393119059852,2.23552722878661,
7.36604956917819));
#48644=CARTESIAN_POINT('Ctrl Pts',(-0.292209453885833,2.23592277540167,
7.36602275294438));
#48645=CARTESIAN_POINT('Ctrl Pts',(-0.291721520536685,2.23696804298165,
7.36595174776038));
#48646=CARTESIAN_POINT('Ctrl Pts',(-0.291415885950898,2.23761712009997,
7.365907511581));
#48647=CARTESIAN_POINT('Ctrl Pts',(-0.290014994441877,2.24056660374801,
7.36570583464253));
#48648=CARTESIAN_POINT('Ctrl Pts',(-0.288894673052914,2.24285494171508,
7.36554752517551));
#48649=CARTESIAN_POINT('Ctrl Pts',(-0.283890170236317,2.25277732455363,
7.36485284545483));
#48650=CARTESIAN_POINT('Ctrl Pts',(-0.279729958162931,2.26026748869724,
7.36430684009744));
#48651=CARTESIAN_POINT('Ctrl Pts',(-0.267773658320616,2.27990730521597,
7.36281498674291));
#48652=CARTESIAN_POINT('Ctrl Pts',(-0.259452143329316,2.2917130106613,7.36185234121339));
#48653=CARTESIAN_POINT('Ctrl Pts',(-0.234796304168245,2.32213403456118,
7.35921017214327));
#48654=CARTESIAN_POINT('Ctrl Pts',(-0.217062901940522,2.33949266701768,
7.35751392852395));
#48655=CARTESIAN_POINT('Ctrl Pts',(-0.19640863781921,2.35551280017933,7.35586215333832));
#48656=CARTESIAN_POINT('Ctrl Pts',(-0.19529438906468,2.3563654536708,7.35577395969225));
#48657=CARTESIAN_POINT('Ctrl Pts',(-0.193842865654234,2.35746124331218,
7.35566029047177));
#48658=CARTESIAN_POINT('Ctrl Pts',(-0.193510661323753,2.35771102485451,
7.35563435763584));
#48659=CARTESIAN_POINT('Ctrl Pts',(-0.193000497357154,2.35809307004673,
7.35559465980004));
#48660=CARTESIAN_POINT('Ctrl Pts',(-0.192822884481934,2.3582257926835,7.35558086259655));
#48661=CARTESIAN_POINT('Ctrl Pts',(-0.192472112117746,2.35848734642757,
7.35555366079469));
#48662=CARTESIAN_POINT('Ctrl Pts',(-0.192298961230918,2.35861618610652,
7.35554025565808));
#48663=CARTESIAN_POINT('Ctrl Pts',(-0.191912071493919,2.35890346313909,
7.35551035304808));
#48664=CARTESIAN_POINT('Ctrl Pts',(-0.191698266364508,2.35906180939029,
7.35549386202222));
#48665=CARTESIAN_POINT('Ctrl Pts',(-0.191077273525782,2.35952053328038,
7.35544606170872));
#48666=CARTESIAN_POINT('Ctrl Pts',(-0.190669571831301,2.35982021868611,
7.35541480074855));
#48667=CARTESIAN_POINT('Ctrl Pts',(-0.187830833735565,2.3618965826768,7.35519796744824));
#48668=CARTESIAN_POINT('Ctrl Pts',(-0.185375605020601,2.36364015012853,
7.35501464890999));
#48669=CARTESIAN_POINT('Ctrl Pts',(-0.17765005402529,2.36896511163954,7.35444962176683));
#48670=CARTESIAN_POINT('Ctrl Pts',(-0.172297462719188,2.37242497771716,
7.35407492401959));
#48671=CARTESIAN_POINT('Ctrl Pts',(-0.153340559219655,2.38389613067127,
7.35279234112182));
#48672=CARTESIAN_POINT('Ctrl Pts',(-0.139252632784307,2.39106547286348,
7.35191539258484));
#48673=CARTESIAN_POINT('Ctrl Pts',(-0.101588582525585,2.4068694483464,7.34963142863199));
#48674=CARTESIAN_POINT('Ctrl Pts',(-0.0774340145900101,2.41383565326267,
7.34821703666872));
#48675=CARTESIAN_POINT('Ctrl Pts',(-0.0512172280476047,2.4181827870406,
7.34660539321477));
#48676=CARTESIAN_POINT('Ctrl Pts',(-0.0497145547213379,2.41842103156508,
7.34651279331844));
#48677=CARTESIAN_POINT('Ctrl Pts',(-0.0476692025243479,2.41873048522473,
7.3463864282776));
#48678=CARTESIAN_POINT('Ctrl Pts',(-0.0471279295340625,2.41881096802479,
7.34635295686699));
#48679=CARTESIAN_POINT('Ctrl Pts',(-0.0462093245374925,2.41894516647066,
7.34629609883186));
#48680=CARTESIAN_POINT('Ctrl Pts',(-0.045832096123273,2.41899959224447,
7.34627273471443));
#48681=CARTESIAN_POINT('Ctrl Pts',(-0.0451045850859807,2.41910323901535,
7.34622764582581));
#48682=CARTESIAN_POINT('Ctrl Pts',(-0.044754316030545,2.41915255277207,
7.34620592402186));
#48683=CARTESIAN_POINT('Ctrl Pts',(-0.0439264503351217,2.41926771684787,
7.34615455270768));
#48684=CARTESIAN_POINT('Ctrl Pts',(-0.0434487867006476,2.41933307218411,
7.34612488759609));
#48685=CARTESIAN_POINT('Ctrl Pts',(-0.0420511389371274,2.41952110847646,
7.34603801376608));
#48686=CARTESIAN_POINT('Ctrl Pts',(-0.0411307751156371,2.4196408865547,
7.34598071348627));
#48687=CARTESIAN_POINT('Ctrl Pts',(-0.0343431254920052,2.42049444434363,
7.34555742397848));
#48688=CARTESIAN_POINT('Ctrl Pts',(-0.0284574843661114,2.42107055802009,
7.34518648974109));
#48689=CARTESIAN_POINT('Ctrl Pts',(-0.00870833655251587,2.42245642108072,
7.34392765343439));
#48690=CARTESIAN_POINT('Ctrl Pts',(0.00518957568460903,2.42253211086154,
7.34301767762375));
#48691=CARTESIAN_POINT('Ctrl Pts',(0.0489910324575595,2.41993875249917,
7.34008622731899));
#48692=CARTESIAN_POINT('Ctrl Pts',(0.078539777553973,2.41399441471167,7.3380017372432));
#48693=CARTESIAN_POINT('Ctrl Pts',(0.108262393998951,2.40355016344988,7.33600904021338));
#48694=CARTESIAN_POINT('Ctrl Pts',(0.109680997160865,2.40304047049415,7.33591423234958));
#48695=CARTESIAN_POINT('Ctrl Pts',(0.111492385849615,2.40237526656436,7.33579360610496));
#48696=CARTESIAN_POINT('Ctrl Pts',(0.111888483445022,2.40222892186143,7.33576725524625));
#48697=CARTESIAN_POINT('Ctrl Pts',(0.112518848244431,2.40199461424174,7.3357253631349));
#48698=CARTESIAN_POINT('Ctrl Pts',(0.112753300881688,2.40190715689195,7.3357097917631));
#48699=CARTESIAN_POINT('Ctrl Pts',(0.11319018783606,2.40174360601668,7.33568079382722));
#48700=CARTESIAN_POINT('Ctrl Pts',(0.113392645876778,2.40166758237466,7.33566736324266));
#48701=CARTESIAN_POINT('Ctrl Pts',(0.113850159354271,2.40149525894406,7.33563702940329));
#48702=CARTESIAN_POINT('Ctrl Pts',(0.114105168649582,2.40139883947936,7.33562013347761));
#48703=CARTESIAN_POINT('Ctrl Pts',(0.114862524619515,2.40111138289487,7.33556998756576));
#48704=CARTESIAN_POINT('Ctrl Pts',(0.115364519260963,2.40091941143166,7.33553679349584));
#48705=CARTESIAN_POINT('Ctrl Pts',(0.119441232509193,2.39934870482761,7.33526756255857));
#48706=CARTESIAN_POINT('Ctrl Pts',(0.122991774349946,2.39790750529514,7.33503520221813));
#48707=CARTESIAN_POINT('Ctrl Pts',(0.134701895679969,2.39290918897779,7.33427326269652));
#48708=CARTESIAN_POINT('Ctrl Pts',(0.142740276788091,2.38907720998697,7.33375740712057));
#48709=CARTESIAN_POINT('Ctrl Pts',(0.17305098587776,2.37305463345284,7.3318024839643));
#48710=CARTESIAN_POINT('Ctrl Pts',(0.194011581735737,2.35858279349514,7.33042234579628));
#48711=CARTESIAN_POINT('Ctrl Pts',(0.216621816156593,2.33866028603005,7.32868778452313));
#48712=CARTESIAN_POINT('Ctrl Pts',(0.220116126001885,2.33544135487682,7.32841201642164));
#48713=CARTESIAN_POINT('Ctrl Pts',(0.224759684467164,2.33096999089431,7.32803388701573));
#48714=CARTESIAN_POINT('Ctrl Pts',(0.225972140637662,2.32978390710425,7.32793403796357));
#48715=CARTESIAN_POINT('Ctrl Pts',(0.231690653957768,2.3241007463158,7.32745761168318));
#48716=CARTESIAN_POINT('Ctrl Pts',(0.236071923382834,2.31948061893626,7.32707615316345));
#48717=CARTESIAN_POINT('Ctrl Pts',(0.240997240512356,2.31396859428939,7.32662623892424));
#48718=CARTESIAN_POINT('Ctrl Pts',(0.241677520921126,2.31319991819872,7.32656361045812));
#48719=CARTESIAN_POINT('Ctrl Pts',(0.242685170795305,2.31205031421141,7.32647010897869));
#48720=CARTESIAN_POINT('Ctrl Pts',(0.243015345379898,2.31167184457665,7.32643935282436));
#48721=CARTESIAN_POINT('Ctrl Pts',(0.243602356099082,2.31099578728265,7.32638445913555));
#48722=CARTESIAN_POINT('Ctrl Pts',(0.243859535582839,2.31069849798041,7.32636033589695));
#48723=CARTESIAN_POINT('Ctrl Pts',(0.244394548530188,2.3100777524857,7.32630999841056));
#48724=CARTESIAN_POINT('Ctrl Pts',(0.244672285099172,2.30975421412282,7.3262837802298));
#48725=CARTESIAN_POINT('Ctrl Pts',(0.245395711272452,2.30890809521097,7.32621526111521));
#48726=CARTESIAN_POINT('Ctrl Pts',(0.245840372102121,2.30838464144127,7.32617291798999));
#48727=CARTESIAN_POINT('Ctrl Pts',(0.246808426734418,2.30723763864586,7.32608023395456));
#48728=CARTESIAN_POINT('Ctrl Pts',(0.247331136827681,2.30661352113219,7.32602986541983));
#48729=CARTESIAN_POINT('Ctrl Pts',(0.248852594441432,2.3047828487348,7.32588230456728));
#48730=CARTESIAN_POINT('Ctrl Pts',(0.249844906689727,2.30357099832226,7.32578485201683));
#48731=CARTESIAN_POINT('Ctrl Pts',(0.260016978710572,2.29096205888096,7.32477314469144));
#48732=CARTESIAN_POINT('Ctrl Pts',(0.268417835096313,2.27896115781958,7.32382795414517));
#48733=CARTESIAN_POINT('Ctrl Pts',(0.291978748267486,2.23989314833037,7.3208065539014));
#48734=CARTESIAN_POINT('Ctrl Pts',(0.304070818390767,2.21118658079329,7.31864771893823));
#48735=CARTESIAN_POINT('Ctrl Pts',(0.312755132968237,2.17782998656093,7.31643387634912));
#48736=CARTESIAN_POINT('Ctrl Pts',(0.313577163844854,2.17444894059029,7.31621291104345));
#48737=CARTESIAN_POINT('Ctrl Pts',(0.314469887312247,2.17049957413541,7.31595930531014));
#48738=CARTESIAN_POINT('Ctrl Pts',(0.314593983555409,2.16994373096986,7.31592371552658));
#48739=CARTESIAN_POINT('Ctrl Pts',(0.314776708573758,2.16911495704464,7.31587080723701));
#48740=CARTESIAN_POINT('Ctrl Pts',(0.31483645641633,2.16884227814676,7.31585342489455));
#48741=CARTESIAN_POINT('Ctrl Pts',(0.314942417145779,2.16835566844569,7.31582245069202));
#48742=CARTESIAN_POINT('Ctrl Pts',(0.31498876635459,2.16814176837854,7.31580885098557));
#48743=CARTESIAN_POINT('Ctrl Pts',(0.315086887659804,2.16768670246147,7.31577995149014));
#48744=CARTESIAN_POINT('Ctrl Pts',(0.315138600646858,2.1674455250448,7.31576465516559));
#48745=CARTESIAN_POINT('Ctrl Pts',(0.315277032718001,2.16679627465888,7.3157235304565));
#48746=CARTESIAN_POINT('Ctrl Pts',(0.315363236774179,2.16638809052636,7.31569773169403));
#48747=CARTESIAN_POINT('Ctrl Pts',(0.315776943715895,2.16441016062326,7.31557298699603));
#48748=CARTESIAN_POINT('Ctrl Pts',(0.316093527682285,2.16283811726516,7.31547465755566));
#48749=CARTESIAN_POINT('Ctrl Pts',(0.318667947646501,2.14954244991579,7.31464941495535));
#48750=CARTESIAN_POINT('Ctrl Pts',(0.32028470968847,2.13770262998914,7.31395625829021));
#48751=CARTESIAN_POINT('Ctrl Pts',(0.324139463425932,2.08970468478024,7.31121669033309));
#48752=CARTESIAN_POINT('Ctrl Pts',(0.320935100326457,2.05338302844752,7.30926952101144));
#48753=CARTESIAN_POINT('Ctrl Pts',(0.31124500741935,2.01638261234087,7.30695739214416));
#48754=CARTESIAN_POINT('Ctrl Pts',(0.310710466001575,2.01441771103415,7.30683370819671));
#48755=CARTESIAN_POINT('Ctrl Pts',(0.309970980285469,2.01179774532138,7.30666754204549));
#48756=CARTESIAN_POINT('Ctrl Pts',(0.309782504609037,2.01113804989642,7.30662559594255));
#48757=CARTESIAN_POINT('Ctrl Pts',(0.309484649409622,2.01010797283249,7.30655993157993));
#48758=CARTESIAN_POINT('Ctrl Pts',(0.309376707495542,2.00973717473065,7.3065362602307));
#48759=CARTESIAN_POINT('Ctrl Pts',(0.309159687876581,2.008996639508,7.30648891677847));
#48760=CARTESIAN_POINT('Ctrl Pts',(0.309050612745041,2.0086269022705,7.30646524479162));
#48761=CARTESIAN_POINT('Ctrl Pts',(0.308804991032578,2.00779977772831,7.3064122122064));
#48762=CARTESIAN_POINT('Ctrl Pts',(0.308668091338972,2.00734249701817,7.3063828401054));
#48763=CARTESIAN_POINT('Ctrl Pts',(0.308265331067375,2.00600797092438,7.30629696566834));
#48764=CARTESIAN_POINT('Ctrl Pts',(0.307996744711551,2.00513155905609,7.30624037418203));
#48765=CARTESIAN_POINT('Ctrl Pts',(0.307380861954413,2.00315208477729,7.30611210750035));
#48766=CARTESIAN_POINT('Ctrl Pts',(0.307031361305398,2.002049726403,7.30604036042177));
#48767=CARTESIAN_POINT('Ctrl Pts',(0.305900734768139,1.99854913629999,7.30581150506724));
#48768=CARTESIAN_POINT('Ctrl Pts',(0.305097399451094,1.99615822833283,7.30565366891226));
#48769=CARTESIAN_POINT('Ctrl Pts',(0.301881967844222,1.9869479132987,7.30503960144201));
#48770=CARTESIAN_POINT('Ctrl Pts',(0.299268761965905,1.98020145383,7.30457682750811));
#48771=CARTESIAN_POINT('Ctrl Pts',(0.289827622316989,1.95806919196521,7.3030145896575));
#48772=CARTESIAN_POINT('Ctrl Pts',(0.282022575789474,1.94313204305789,7.301885805813));
#48773=CARTESIAN_POINT('Ctrl Pts',(0.271817677192594,1.92684674367971,7.30058602440199));
#48774=CARTESIAN_POINT('Ctrl Pts',(0.270524726215543,1.92483358688585,7.30042410662612));
#48775=CARTESIAN_POINT('Ctrl Pts',(0.258182562717563,1.90607916164526,7.29890477822406));
#48776=CARTESIAN_POINT('Ctrl Pts',(0.245613975609272,1.89038726377007,7.29754825329908));
#48777=CARTESIAN_POINT('Ctrl Pts',(0.231396138878017,1.87568514613716,7.29625874382856));
#48778=CARTESIAN_POINT('Ctrl Pts',(0.231125385486507,1.87540618232358,7.29623426971602));
#48779=CARTESIAN_POINT('Ctrl Pts',(0.230249748547268,1.87450725254282,7.29615538581831));
#48780=CARTESIAN_POINT('Ctrl Pts',(0.22964286354414,1.87388922819549,7.29610112328574));
#48781=CARTESIAN_POINT('Ctrl Pts',(0.228817129157504,1.8730550912507,7.29602785625103));
#48782=CARTESIAN_POINT('Ctrl Pts',(0.228600458447214,1.87283684144923,7.29600868333411));
#48783=CARTESIAN_POINT('Ctrl Pts',(0.22823327278429,1.87246803710312,7.29597628024674));
#48784=CARTESIAN_POINT('Ctrl Pts',(0.22808292103852,1.87231732152694,7.29596303721644));
#48785=CARTESIAN_POINT('Ctrl Pts',(0.227792749712988,1.87202702389206,7.29593752734882));
#48786=CARTESIAN_POINT('Ctrl Pts',(0.227652952182814,1.87188742248624,7.29592525899036));
#48787=CARTESIAN_POINT('Ctrl Pts',(0.227319451894788,1.87155500199331,7.29589604312272));
#48788=CARTESIAN_POINT('Ctrl Pts',(0.227125632332043,1.87136230087075,7.29587910506971));
#48789=CARTESIAN_POINT('Ctrl Pts',(0.226547598482039,1.87078906292596,7.29582871208519));
#48790=CARTESIAN_POINT('Ctrl Pts',(0.22616266886089,1.87040924392279,7.29579531390105));
#48791=CARTESIAN_POINT('Ctrl Pts',(0.222969415901182,1.86727421062912,7.29551955498801));
#48792=CARTESIAN_POINT('Ctrl Pts',(0.220111660465156,1.86456951385418,7.29528107340163));
#48793=CARTESIAN_POINT('Ctrl Pts',(0.210688956881642,1.85597308488106,7.29451835985857));
#48794=CARTESIAN_POINT('Ctrl Pts',(0.203931126806355,1.85029799200357,7.29400730422448));
#48795=CARTESIAN_POINT('Ctrl Pts',(0.1734673723503,1.82677799396694,7.29181303135831));
#48796=CARTESIAN_POINT('Ctrl Pts',(0.147596644908991,1.81197826098531,7.29021000069539));
#48797=CARTESIAN_POINT('Ctrl Pts',(0.118345943486315,1.80023534701301,7.28836471931974));
#48798=CARTESIAN_POINT('Ctrl Pts',(0.116620372055996,1.79955982600164,7.28825581183764));
#48799=CARTESIAN_POINT('Ctrl Pts',(0.108679066119182,1.79652971267431,7.2877542004246));
#48800=CARTESIAN_POINT('Ctrl Pts',(0.102397595624481,1.79435301826717,7.28735625377473));
#48801=CARTESIAN_POINT('Ctrl Pts',(0.0950613449120288,1.79206234886448,
7.2868885159972));
#48802=CARTESIAN_POINT('Ctrl Pts',(0.0940675603863193,1.79175731910293,
7.28682509424341));
#48803=CARTESIAN_POINT('Ctrl Pts',(0.0925889846090709,1.79131130498307,
7.28673063746083));
#48804=CARTESIAN_POINT('Ctrl Pts',(0.0921053029886499,1.79116664095506,
7.28669972284522));
#48805=CARTESIAN_POINT('Ctrl Pts',(0.0912441069411747,1.79091126946035,
7.2866446513828));
#48806=CARTESIAN_POINT('Ctrl Pts',(0.0908667251276105,1.79080011536143,
7.2866205091776));
#48807=CARTESIAN_POINT('Ctrl Pts',(0.0900811212604811,1.7905702859341,7.28657023161557));
#48808=CARTESIAN_POINT('Ctrl Pts',(0.0896728662436124,1.79045172684806,
7.28654409252053));
#48809=CARTESIAN_POINT('Ctrl Pts',(0.0886198605506465,1.79014818725219,
7.28647664255024));
#48810=CARTESIAN_POINT('Ctrl Pts',(0.0879747671850356,1.78996441192181,
7.28643529250194));
#48811=CARTESIAN_POINT('Ctrl Pts',(0.0852195342448476,1.78918878786623,
7.28625855750337));
#48812=CARTESIAN_POINT('Ctrl Pts',(0.0831040002562024,1.78861646902098,
7.2861225395628));
#48813=CARTESIAN_POINT('Ctrl Pts',(0.0776514756705943,1.78720091127522,
7.28577109309131));
#48814=CARTESIAN_POINT('Ctrl Pts',(0.0743065844201144,1.78638949058253,
7.28555465393187));
#48815=CARTESIAN_POINT('Ctrl Pts',(0.0679548724346423,1.78495597905047,
7.28514194708354));
#48816=CARTESIAN_POINT('Ctrl Pts',(0.0649508852388535,1.78432297944141,
7.2849460474936));
#48817=CARTESIAN_POINT('Ctrl Pts',(0.0489983094532829,1.78119879345297,
7.28390188830195));
#48818=CARTESIAN_POINT('Ctrl Pts',(0.0359162941350299,1.77946139715869,
7.28303152000872));
#48819=CARTESIAN_POINT('Ctrl Pts',(-0.00555322865300899,1.77652460416277,
7.28024367511505));
#48820=CARTESIAN_POINT('Ctrl Pts',(-0.0340136046465727,1.77826971293727,
7.27827820440472));
#48821=CARTESIAN_POINT('Ctrl Pts',(-0.0633128102330076,1.78400189561135,
7.27639060802813));
#48822=CARTESIAN_POINT('Ctrl Pts',(-0.0647459983417925,1.78429242991623,
7.27629865686531));
#48823=CARTESIAN_POINT('Ctrl Pts',(-0.0665905215442268,1.78467943862106,
7.27618085146625));
#48824=CARTESIAN_POINT('Ctrl Pts',(-0.0670036838563688,1.78476697453727,
7.27615449851696));
#48825=CARTESIAN_POINT('Ctrl Pts',(-0.0676590006165786,1.78490716182497,
7.27611275659796));
#48826=CARTESIAN_POINT('Ctrl Pts',(-0.0679012666437988,1.78495928037348,
7.27609733716511));
#48827=CARTESIAN_POINT('Ctrl Pts',(-0.0683358148372503,1.78505328901188,
7.27606970191354));
#48828=CARTESIAN_POINT('Ctrl Pts',(-0.0685281173265546,1.78509507547883,
7.276057480237));
#48829=CARTESIAN_POINT('Ctrl Pts',(-0.0689808490857485,1.78519388640205,
7.27602872555198));
#48830=CARTESIAN_POINT('Ctrl Pts',(-0.0692412455857805,1.78525105780925,
7.27601220113079));
#48831=CARTESIAN_POINT('Ctrl Pts',(-0.0699981593338604,1.78541822693875,
7.27596420926816));
#48832=CARTESIAN_POINT('Ctrl Pts',(-0.0704944904180976,1.78552907752615,
7.2759327907536));
#48833=CARTESIAN_POINT('Ctrl Pts',(-0.0739842212752878,1.78631715113921,
7.27571223246819));
#48834=CARTESIAN_POINT('Ctrl Pts',(-0.0769682045136018,1.78703595761215,
7.27552543574102));
#48835=CARTESIAN_POINT('Ctrl Pts',(-0.0860205776454299,1.7893538785347,
7.27496298339328));
#48836=CARTESIAN_POINT('Ctrl Pts',(-0.0920532223458251,1.79108776736191,
7.27459396855571));
#48837=CARTESIAN_POINT('Ctrl Pts',(-0.111760921955877,1.79738079926167,
7.27339623264802));
#48838=CARTESIAN_POINT('Ctrl Pts',(-0.125181427419761,1.80268106761229,
7.27259261632321));
#48839=CARTESIAN_POINT('Ctrl Pts',(-0.144647510666331,1.81192159420228,
7.27138821056239));
#48840=CARTESIAN_POINT('Ctrl Pts',(-0.150988848894312,1.81519403910854,
7.27098941848078));
#48841=CARTESIAN_POINT('Ctrl Pts',(-0.166525370870993,1.82387647757747,
7.26998649998931));
#48842=CARTESIAN_POINT('Ctrl Pts',(-0.175569966390266,1.82953731988906,
7.26937888016225));
#48843=CARTESIAN_POINT('Ctrl Pts',(-0.19188632089873,1.84091321148929,7.26821868469773));
#48844=CARTESIAN_POINT('Ctrl Pts',(-0.1992249911041,1.84651291494113,7.26767031249534));
#48845=CARTESIAN_POINT('Ctrl Pts',(-0.207187543968832,1.85314823555549,
7.26703997234601));
#48846=CARTESIAN_POINT('Ctrl Pts',(-0.208058353732799,1.85388174920354,
7.2669705429999));
#48847=CARTESIAN_POINT('Ctrl Pts',(-0.209319919431502,1.85495589042277,
7.26686922992957));
#48848=CARTESIAN_POINT('Ctrl Pts',(-0.209713776154376,1.85529287628796,
7.26683749604175));
#48849=CARTESIAN_POINT('Ctrl Pts',(-0.210407566836464,1.85588939236692,
7.26678141056158));
#48850=CARTESIAN_POINT('Ctrl Pts',(-0.210707838619506,1.85614852946292,
7.26675707525264));
#48851=CARTESIAN_POINT('Ctrl Pts',(-0.211284315302471,1.8566478935153,7.26671023613378));
#48852=CARTESIAN_POINT('Ctrl Pts',(-0.211560590942305,1.85688803817631,
7.26668773576168));
#48853=CARTESIAN_POINT('Ctrl Pts',(-0.212149412531254,1.85740161822488,
7.2666396679338));
#48854=CARTESIAN_POINT('Ctrl Pts',(-0.21246184006064,1.85767518783101,7.26661409490643));
#48855=CARTESIAN_POINT('Ctrl Pts',(-0.213627323604747,1.85869970190939,
7.26651844039135));
#48856=CARTESIAN_POINT('Ctrl Pts',(-0.214476926434748,1.85945454645074,
7.26644819590931));
#48857=CARTESIAN_POINT('Ctrl Pts',(-0.22189152129636,1.86611268435279,7.26583058983186));
#48858=CARTESIAN_POINT('Ctrl Pts',(-0.228214778132141,1.8722784287313,7.26527210261639));
#48859=CARTESIAN_POINT('Ctrl Pts',(-0.239122452551744,1.8838254684735,7.2642479296849));
#48860=CARTESIAN_POINT('Ctrl Pts',(-0.243798290583492,1.88911292612937,
7.26378641386881));
#48861=CARTESIAN_POINT('Ctrl Pts',(-0.267588791183756,1.91786483594508,
7.26131770250931));
#48862=CARTESIAN_POINT('Ctrl Pts',(-0.283499060041731,1.94377876755195,
7.25921302538708));
#48863=CARTESIAN_POINT('Ctrl Pts',(-0.295689210127076,1.9718236785051,7.25723575291577));
#48864=CARTESIAN_POINT('Ctrl Pts',(-0.295816554758344,1.9721178499161,7.25721504582762));
#48865=CARTESIAN_POINT('Ctrl Pts',(-0.297604260642345,1.97626448396694,
7.25692363007918));
#48866=CARTESIAN_POINT('Ctrl Pts',(-0.299189785584497,1.98014904983922,
7.25665635035427));
#48867=CARTESIAN_POINT('Ctrl Pts',(-0.30089409443695,1.98456944352242,7.25635949622716));
#48868=CARTESIAN_POINT('Ctrl Pts',(-0.301087816299495,1.98507569307629,
7.25632560577614));
#48869=CARTESIAN_POINT('Ctrl Pts',(-0.301378821179852,1.98584195676327,
7.2562744732263));
#48870=CARTESIAN_POINT('Ctrl Pts',(-0.30147704579176,1.98610160864396,7.25625717520928));
#48871=CARTESIAN_POINT('Ctrl Pts',(-0.301647174900279,1.98655309845104,
7.25622714681826));
#48872=CARTESIAN_POINT('Ctrl Pts',(-0.301719231992952,1.98674487807388,
7.25621440725977));
#48873=CARTESIAN_POINT('Ctrl Pts',(-0.301869699123188,1.98714650842186,
7.25618776060194));
#48874=CARTESIAN_POINT('Ctrl Pts',(-0.301948073192932,1.98735637210419,
7.25617385573868));
#48875=CARTESIAN_POINT('Ctrl Pts',(-0.302135264606568,1.98785921711975,
7.25614058355759));
#48876=CARTESIAN_POINT('Ctrl Pts',(-0.30224387508507,1.98815227637806,7.25612122871087));
#48877=CARTESIAN_POINT('Ctrl Pts',(-0.302611870904131,1.98914967485583,
7.25605547816358));
#48878=CARTESIAN_POINT('Ctrl Pts',(-0.302869224389366,1.9898547688685,7.25600920329117));
#48879=CARTESIAN_POINT('Ctrl Pts',(-0.307001271438203,2.00129968706809,
7.25526132317705));
#48880=CARTESIAN_POINT('Ctrl Pts',(-0.310305510150295,2.01223845869604,
7.25459265640517));
#48881=CARTESIAN_POINT('Ctrl Pts',(-0.31915179159861,2.04835576843892,7.25246396644035));
#48882=CARTESIAN_POINT('Ctrl Pts',(-0.322258053448205,2.07402443595143,
7.25106566728904));
#48883=CARTESIAN_POINT('Ctrl Pts',(-0.322274930854165,2.09978888878902,
7.24958594529397));
#48884=CARTESIAN_POINT('',(-0.32227506499556,2.10009833267788,6.99910083188333));
#48885=CARTESIAN_POINT('Ctrl Pts',(-0.322274931120346,2.09978929552436,
7.24958592193406));
#48886=CARTESIAN_POINT('Ctrl Pts',(-0.322283452356173,2.11282262422254,
7.24883738236764));
#48887=CARTESIAN_POINT('Ctrl Pts',(-0.321501354546834,2.1258433373128,7.24807165738387));
#48888=CARTESIAN_POINT('Ctrl Pts',(-0.319826940648638,2.13965707673027,
7.24722632872068));
#48889=CARTESIAN_POINT('Ctrl Pts',(-0.319717057343064,2.14053342964926,
7.2471725611068));
#48890=CARTESIAN_POINT('Ctrl Pts',(-0.319533956312919,2.14194663212223,
7.24708562656257));
#48891=CARTESIAN_POINT('Ctrl Pts',(-0.319462984208659,2.14248377217532,
7.24705253038902));
#48892=CARTESIAN_POINT('Ctrl Pts',(-0.319337231928368,2.14341737105474,
7.24699491222241));
#48893=CARTESIAN_POINT('Ctrl Pts',(-0.319283066976374,2.14381391268599,
7.24697040968315));
#48894=CARTESIAN_POINT('Ctrl Pts',(-0.319177694297875,2.14457477356838,
7.24692333860086));
#48895=CARTESIAN_POINT('Ctrl Pts',(-0.319126601089601,2.14493910825994,
7.24690077371063));
#48896=CARTESIAN_POINT('Ctrl Pts',(-0.319018574666174,2.14569994638594,
7.24685359875328));
#48897=CARTESIAN_POINT('Ctrl Pts',(-0.318961525871904,2.1460964325396,7.24682898506544));
#48898=CARTESIAN_POINT('Ctrl Pts',(-0.318834156186697,2.14697008738754,
7.24677468240347));
#48899=CARTESIAN_POINT('Ctrl Pts',(-0.318763503085519,2.14744720599876,
7.24674498295549));
#48900=CARTESIAN_POINT('Ctrl Pts',(-0.318512924792828,2.14911353125983,
7.24664110415633));
#48901=CARTESIAN_POINT('Ctrl Pts',(-0.31832741533508,2.15030187666567,7.24656674805855));
#48902=CARTESIAN_POINT('Ctrl Pts',(-0.316296556871367,2.16284991393677,
7.24577864937169));
#48903=CARTESIAN_POINT('Ctrl Pts',(-0.313850853114973,2.17410270972909,
7.24504582241275));
#48904=CARTESIAN_POINT('Ctrl Pts',(-0.310214584241275,2.18736785440093,
7.24414927831901));
#48905=CARTESIAN_POINT('Ctrl Pts',(-0.309597553368278,2.18952979871242,
7.24400211942851));
#48906=CARTESIAN_POINT('Ctrl Pts',(-0.301800144268388,2.21580530406082,
7.24220109132334));
#48907=CARTESIAN_POINT('Ctrl Pts',(-0.291842408872386,2.23900352168179,
7.24047239287601));
#48908=CARTESIAN_POINT('Ctrl Pts',(-0.274060586976526,2.26988773744483,
7.23809391218775));
#48909=CARTESIAN_POINT('Ctrl Pts',(-0.268389740630484,2.27871218273794,
7.23740569282578));
#48910=CARTESIAN_POINT('Ctrl Pts',(-0.261430469991157,2.28846091259432,
7.23664836597244));
#48911=CARTESIAN_POINT('Ctrl Pts',(-0.260554260953618,2.28967046032523,
7.23655446062713));
#48912=CARTESIAN_POINT('Ctrl Pts',(-0.259428615238428,2.29120181706741,
7.23643569119007));
#48913=CARTESIAN_POINT('Ctrl Pts',(-0.25918695297812,2.29152927887054,7.23641030085365));
#48914=CARTESIAN_POINT('Ctrl Pts',(-0.258799189393296,2.29205263578715,
7.23636973391332));
#48915=CARTESIAN_POINT('Ctrl Pts',(-0.258653485436018,2.29224882266524,
7.23635452970303));
#48916=CARTESIAN_POINT('Ctrl Pts',(-0.258376594279502,2.29262076537378,
7.23632571030804));
#48917=CARTESIAN_POINT('Ctrl Pts',(-0.258245451913623,2.29279655155334,
7.2363120922314));
#48918=CARTESIAN_POINT('Ctrl Pts',(-0.257944620829139,2.29319893464911,
7.23628092516512));
#48919=CARTESIAN_POINT('Ctrl Pts',(-0.25777481316914,2.29342544160819,7.23626338467904));
#48920=CARTESIAN_POINT('Ctrl Pts',(-0.257250553497054,2.29412283667948,
7.2362093900317));
#48921=CARTESIAN_POINT('Ctrl Pts',(-0.256895105495645,2.29459297978185,
7.23617300543413));
#48922=CARTESIAN_POINT('Ctrl Pts',(-0.254176224270459,2.29816874960579,
7.23589637041318));
#48923=CARTESIAN_POINT('Ctrl Pts',(-0.251757717603252,2.30123235637591,
7.23565990846408));
#48924=CARTESIAN_POINT('Ctrl Pts',(-0.248922716738761,2.30469240756672,
7.23539250741941));
#48925=CARTESIAN_POINT('Ctrl Pts',(-0.248560235133508,2.30513242099549,
7.23535849571771));
#48926=CARTESIAN_POINT('Ctrl Pts',(-0.230754892628871,2.32662968975361,
7.23369637788475));
#48927=CARTESIAN_POINT('Ctrl Pts',(-0.210701969959911,2.34538526312127,
7.23221755769256));
#48928=CARTESIAN_POINT('Ctrl Pts',(-0.182759237044992,2.36553844137126,
7.23027168470304));
#48929=CARTESIAN_POINT('Ctrl Pts',(-0.176864236352622,2.36950071870509,
7.22986729058592));
#48930=CARTESIAN_POINT('Ctrl Pts',(-0.164008127537361,2.37753827124735,
7.22899173371935));
#48931=CARTESIAN_POINT('Ctrl Pts',(-0.157015396014096,2.38155338428239,
7.22851923169706));
#48932=CARTESIAN_POINT('Ctrl Pts',(-0.147459909293703,2.38657324243066,
7.22787412491723));
#48933=CARTESIAN_POINT('Ctrl Pts',(-0.1450239141004,2.38781367544894,7.22770972491688));
#48934=CARTESIAN_POINT('Ctrl Pts',(-0.140931092834088,2.38983262837445,
7.22743345155086));
#48935=CARTESIAN_POINT('Ctrl Pts',(-0.139282856150741,2.39062830413719,
7.22732217731717));
#48936=CARTESIAN_POINT('Ctrl Pts',(-0.137055832033402,2.39168008994256,
7.2271717769355));
#48937=CARTESIAN_POINT('Ctrl Pts',(-0.136482915396772,2.39194860807866,
7.22713308091363));
#48938=CARTESIAN_POINT('Ctrl Pts',(-0.135576847432173,2.39237001971763,
7.22707187461942));
#48939=CARTESIAN_POINT('Ctrl Pts',(-0.135244217538043,2.39252403595277,
7.22704940314875));
#48940=CARTESIAN_POINT('Ctrl Pts',(-0.134554268963572,2.39284207161545,
7.22700278823431));
#48941=CARTESIAN_POINT('Ctrl Pts',(-0.13419691161445,2.3930060052547,7.2269786418824));
#48942=CARTESIAN_POINT('Ctrl Pts',(-0.133381823548148,2.3933781137486,7.22692356145044));
#48943=CARTESIAN_POINT('Ctrl Pts',(-0.132923904620972,2.39358587168912,
7.22689261309599));
#48944=CARTESIAN_POINT('Ctrl Pts',(-0.131527027136855,2.39421569731012,
7.22679819208082));
#48945=CARTESIAN_POINT('Ctrl Pts',(-0.130586537632414,2.39463433533946,
7.22673460195383));
#48946=CARTESIAN_POINT('Ctrl Pts',(-0.123758000289313,2.3976347894515,7.2262727436864));
#48947=CARTESIAN_POINT('Ctrl Pts',(-0.117796231391091,2.40004424473148,
7.22586863626217));
#48948=CARTESIAN_POINT('Ctrl Pts',(-0.109381659778622,2.40315556137205,
7.22529648608735));
#48949=CARTESIAN_POINT('Ctrl Pts',(-0.106986294552996,2.40400916777737,
7.22513342106656));
#48950=CARTESIAN_POINT('Ctrl Pts',(-0.102696646688279,2.40548084007299,
7.22484105811657));
#48951=CARTESIAN_POINT('Ctrl Pts',(-0.100806240241989,2.40610986027482,
7.22471209885077));
#48952=CARTESIAN_POINT('Ctrl Pts',(-0.0818356509240542,2.41222741356439,
7.2234168413967));
#48953=CARTESIAN_POINT('Ctrl Pts',(-0.0643330111444237,2.41629758176658,
7.22221007407652));
#48954=CARTESIAN_POINT('Ctrl Pts',(-0.0445865415088202,2.41918222730724,
7.22085969722923));
#48955=CARTESIAN_POINT('Ctrl Pts',(-0.0425855737631327,2.41945535341325,
7.22072301703244));
#48956=CARTESIAN_POINT('Ctrl Pts',(-0.0382597680252735,2.42000444720887,
7.22042799224471));
#48957=CARTESIAN_POINT('Ctrl Pts',(-0.0359342134313587,2.42027392723696,
7.22026967150053));
#48958=CARTESIAN_POINT('Ctrl Pts',(-0.0254534482507859,2.42137282252102,
7.21955785388726));
#48959=CARTESIAN_POINT('Ctrl Pts',(-0.01727097020149,2.42191628428832,7.21900666982303));
#48960=CARTESIAN_POINT('Ctrl Pts',(-0.00280235358057257,2.42232393161631,
7.21804835948033));
#48961=CARTESIAN_POINT('Ctrl Pts',(0.00347592742284909,2.42231738827091,
7.21763796222558));
#48962=CARTESIAN_POINT('Ctrl Pts',(0.0129542458582698,2.42203049093876,
7.21703034426879));
#48963=CARTESIAN_POINT('Ctrl Pts',(0.0161566071396098,2.42188571815457,
7.21682712315192));
#48964=CARTESIAN_POINT('Ctrl Pts',(0.0198698412155998,2.42166229121435,
7.21659429571405));
#48965=CARTESIAN_POINT('Ctrl Pts',(0.0203831905111379,2.42163016918893,
7.21656217014895));
#48966=CARTESIAN_POINT('Ctrl Pts',(0.0211637200462756,2.42157945255515,
7.21651342167115));
#48967=CARTESIAN_POINT('Ctrl Pts',(0.021430954593989,2.42156175384879,7.2164967487164));
#48968=CARTESIAN_POINT('Ctrl Pts',(0.02191562384272,2.42152904776861,7.21646654171307));
#48969=CARTESIAN_POINT('Ctrl Pts',(0.0221330646196678,2.42151415299919,
7.21645300138065));
#48970=CARTESIAN_POINT('Ctrl Pts',(0.0225711882357416,2.42148369481008,
7.21642574234697));
#48971=CARTESIAN_POINT('Ctrl Pts',(0.0227918691725042,2.42146812480782,
7.21641202407988));
#48972=CARTESIAN_POINT('Ctrl Pts',(0.0234246533828474,2.42142282425357,
7.21637272202498));
#48973=CARTESIAN_POINT('Ctrl Pts',(0.0238367176664254,2.42139252827758,
7.21634717010233));
#48974=CARTESIAN_POINT('Ctrl Pts',(0.0256265963099393,2.42125747076871,
7.2162363554662));
#48975=CARTESIAN_POINT('Ctrl Pts',(0.0270038134870397,2.42114463903562,
7.2161515398941));
#48976=CARTESIAN_POINT('Ctrl Pts',(0.0528606683919066,2.41885874305175,
7.21456690480974));
#48977=CARTESIAN_POINT('Ctrl Pts',(0.0770176488386212,2.41390102689392,
7.21321323595677));
#48978=CARTESIAN_POINT('Ctrl Pts',(0.111858026860497,2.40248120113176,7.21116231304548));
#48979=CARTESIAN_POINT('Ctrl Pts',(0.123115759289336,2.39807647027641,7.21048383269289));
#48980=CARTESIAN_POINT('Ctrl Pts',(0.14217600910191,2.38935454503934,7.2092785936688));
#48981=CARTESIAN_POINT('Ctrl Pts',(0.150095990881827,2.38532655719339,7.20875984162946));
#48982=CARTESIAN_POINT('Ctrl Pts',(0.16040558235378,2.37953513259278,7.20805425119851));
#48983=CARTESIAN_POINT('Ctrl Pts',(0.162952150547441,2.37805833376962,7.20787741967476));
#48984=CARTESIAN_POINT('Ctrl Pts',(0.167143308929037,2.37555045963621,7.20758194130487));
#48985=CARTESIAN_POINT('Ctrl Pts',(0.168799484830783,2.37453902307455,7.20746400610214));
#48986=CARTESIAN_POINT('Ctrl Pts',(0.170995316034169,2.37317063503339,7.20730603118219));
#48987=CARTESIAN_POINT('Ctrl Pts',(0.17154320036794,2.3728269128002,7.20726647971671));
#48988=CARTESIAN_POINT('Ctrl Pts',(0.172442212527231,2.37225912740773,7.20720135671229));
#48989=CARTESIAN_POINT('Ctrl Pts',(0.172793949054234,2.37203602755107,7.20717582091043));
#48990=CARTESIAN_POINT('Ctrl Pts',(0.173479283756202,2.37159946720459,7.20712595518569));
#48991=CARTESIAN_POINT('Ctrl Pts',(0.173812923027298,2.37138607234871,7.2071016277334));
#48992=CARTESIAN_POINT('Ctrl Pts',(0.174579293328633,2.37089391084596,7.20704562852869));
#48993=CARTESIAN_POINT('Ctrl Pts',(0.1750117506886,2.37061472189915,7.20701394106837));
#48994=CARTESIAN_POINT('Ctrl Pts',(0.176348513768312,2.36974718023817,7.20691571981464));
#48995=CARTESIAN_POINT('Ctrl Pts',(0.1772505283705,2.36915532634849,7.20684905515689));
#48996=CARTESIAN_POINT('Ctrl Pts',(0.184745182303619,2.36418372089218,7.20629188372911));
#48997=CARTESIAN_POINT('Ctrl Pts',(0.191176880967053,2.35956733831276,7.20579245929526));
#48998=CARTESIAN_POINT('Ctrl Pts',(0.221493360286612,2.33606917130516,7.20332955709552));
#48999=CARTESIAN_POINT('Ctrl Pts',(0.242788511786008,2.31410523930215,7.20123790681877));
#49000=CARTESIAN_POINT('Ctrl Pts',(0.267246908682123,2.28045755534402,7.19845556444525));
#49001=CARTESIAN_POINT('Ctrl Pts',(0.273338805890672,2.27109001494013,7.197720550736));
#49002=CARTESIAN_POINT('Ctrl Pts',(0.279707582150361,2.26008509503176,7.19691624185754));
#49003=CARTESIAN_POINT('Ctrl Pts',(0.280472877734172,2.25874046190918,7.19681893842351));
#49004=CARTESIAN_POINT('Ctrl Pts',(0.281429705662243,2.25703078096227,7.19669649382041));
#49005=CARTESIAN_POINT('Ctrl Pts',(0.281630244482385,2.25667083581845,7.19667078626457));
#49006=CARTESIAN_POINT('Ctrl Pts',(0.28194916988366,2.25609580872142,7.19662983201779));
#49007=CARTESIAN_POINT('Ctrl Pts',(0.282068001113144,2.25588097589982,7.19661455679174));
#49008=CARTESIAN_POINT('Ctrl Pts',(0.28229240760431,2.25547417865965,7.19658568082903));
#49009=CARTESIAN_POINT('Ctrl Pts',(0.282398031738879,2.25528224396638,7.19657207702599));
#49010=CARTESIAN_POINT('Ctrl Pts',(0.282638730010926,2.25484380172487,7.19654104785051));
#49011=CARTESIAN_POINT('Ctrl Pts',(0.282773677190077,2.25459722547524,7.19652363071332));
#49012=CARTESIAN_POINT('Ctrl Pts',(0.283185728641204,2.25384197817957,7.19647038434953));
#49013=CARTESIAN_POINT('Ctrl Pts',(0.283461786178493,2.25333273279072,7.19643462191522));
#49014=CARTESIAN_POINT('Ctrl Pts',(0.28548153736812,2.24958278646854,7.19617228674096));
#49015=CARTESIAN_POINT('Ctrl Pts',(0.287171070719426,2.24631301081048,7.19594907724824));
#49016=CARTESIAN_POINT('Ctrl Pts',(0.302361229488563,2.21563799025867,7.19389941648426));
#49017=CARTESIAN_POINT('Ctrl Pts',(0.311958621743741,2.18646885261908,7.19226380063331));
#49018=CARTESIAN_POINT('Ctrl Pts',(0.319899085488931,2.14178086863705,7.18968402947187));
#49019=CARTESIAN_POINT('Ctrl Pts',(0.321482264034047,2.12702101796481,7.18882292142128));
#49020=CARTESIAN_POINT('Ctrl Pts',(0.322103555244842,2.11062857255866,7.18783308231737));
#49021=CARTESIAN_POINT('Ctrl Pts',(0.322151745455651,2.10905094579071,7.18773749094881));
#49022=CARTESIAN_POINT('Ctrl Pts',(0.322207327936335,2.10665459790115,7.18759176924137));
#49023=CARTESIAN_POINT('Ctrl Pts',(0.322223192788896,2.10583608248001,7.18754190287468));
#49024=CARTESIAN_POINT('Ctrl Pts',(0.322246691969549,2.10432691490307,7.18744978567184));
#49025=CARTESIAN_POINT('Ctrl Pts',(0.322255225146649,2.10363627995097,7.18740756312882));
#49026=CARTESIAN_POINT('Ctrl Pts',(0.322265440813055,2.10251865160049,7.18733912528933));
#49027=CARTESIAN_POINT('Ctrl Pts',(0.322268494985945,2.10209167039304,7.18731295300251));
#49028=CARTESIAN_POINT('Ctrl Pts',(0.322272730437829,2.10127171873353,7.18726264246497));
#49029=CARTESIAN_POINT('Ctrl Pts',(0.322274041538524,2.10087874947667,7.18723850832613));
#49030=CARTESIAN_POINT('Ctrl Pts',(0.32227538940038,2.09998455555533,7.18718354025327));
#49031=CARTESIAN_POINT('Ctrl Pts',(0.322274975605423,2.09948333212159,7.18715269225989));
#49032=CARTESIAN_POINT('Ctrl Pts',(0.322270273270931,2.09799452374927,7.1870609528806));
#49033=CARTESIAN_POINT('Ctrl Pts',(0.322262614428274,2.09700696204574,7.18699995608483));
#49034=CARTESIAN_POINT('Ctrl Pts',(0.322178293038253,2.09018060126358,7.18657731245154));
#49035=CARTESIAN_POINT('Ctrl Pts',(0.321947496486012,2.08434511578091,7.18621086310904));
#49036=CARTESIAN_POINT('Ctrl Pts',(0.321477691783002,2.07731227200151,7.18576259765456));
#49037=CARTESIAN_POINT('Ctrl Pts',(0.321390257004349,2.07610560827591,7.18568545150122));
#49038=CARTESIAN_POINT('Ctrl Pts',(0.318790910766332,2.04283300790411,7.18355171448453));
#49039=CARTESIAN_POINT('Ctrl Pts',(0.311499134134056,2.01132532123274,7.18133757903775));
#49040=CARTESIAN_POINT('Ctrl Pts',(0.295798277110193,1.97164390027254,7.17848903387987));
#49041=CARTESIAN_POINT('Ctrl Pts',(0.291449283442329,1.96205336831098,7.17779801476112));
#49042=CARTESIAN_POINT('Ctrl Pts',(0.285954104211748,1.95136061629933,7.17703786589357));
#49043=CARTESIAN_POINT('Ctrl Pts',(0.285260641862588,1.95003406215632,7.17694375095188));
#49044=CARTESIAN_POINT('Ctrl Pts',(0.284366748121627,1.94835273139477,7.17682475446838));
#49045=CARTESIAN_POINT('Ctrl Pts',(0.284174867034911,1.94799346572355,7.17679934424736));
#49046=CARTESIAN_POINT('Ctrl Pts',(0.283866735423601,1.94741916274283,7.17675875302679));
#49047=CARTESIAN_POINT('Ctrl Pts',(0.283750921223578,1.94720389375421,7.17674354436303));
#49048=CARTESIAN_POINT('Ctrl Pts',(0.28353074111487,1.94679574888189,7.17671472146792));
#49049=CARTESIAN_POINT('Ctrl Pts',(0.283426424129419,1.94660284936382,7.17670110433362));
#49050=CARTESIAN_POINT('Ctrl Pts',(0.283187056040634,1.94616129556381,7.17666994613733));
#49051=CARTESIAN_POINT('Ctrl Pts',(0.283051874501126,1.945912712937,7.17665241356167));
#49052=CARTESIAN_POINT('Ctrl Pts',(0.282634426323312,1.94514747892531,7.17659846707671));
#49053=CARTESIAN_POINT('Ctrl Pts',(0.282351069217079,1.94463141903462,7.176562122551));
#49054=CARTESIAN_POINT('Ctrl Pts',(0.280185720668092,1.94071329805586,7.17628643305963));
#49055=CARTESIAN_POINT('Ctrl Pts',(0.278243618191722,1.93734458600179,7.17605084763942));
#49056=CARTESIAN_POINT('Ctrl Pts',(0.260393911615578,1.90763876687956,7.17397891215303));
#49057=CARTESIAN_POINT('Ctrl Pts',(0.240849895705048,1.88366751165079,7.17233310962732));
#49058=CARTESIAN_POINT('Ctrl Pts',(0.207576909654839,1.8530559290688,7.16975997429924));
#49059=CARTESIAN_POINT('Ctrl Pts',(0.196310401855277,1.84400840893766,7.16892059427436));
#49060=CARTESIAN_POINT('Ctrl Pts',(0.183202319638029,1.83485758504372,7.16795576493343));
#49061=CARTESIAN_POINT('Ctrl Pts',(0.181921810003649,1.83397735990221,7.16786164168983));
#49062=CARTESIAN_POINT('Ctrl Pts',(0.179964709856736,1.8326527839542,7.1677179588935));
#49063=CARTESIAN_POINT('Ctrl Pts',(0.179292716059318,1.83220165670666,7.16766865440905));
#49064=CARTESIAN_POINT('Ctrl Pts',(0.178048956329662,1.83137346768915,7.16757745218211));
#49065=CARTESIAN_POINT('Ctrl Pts',(0.177477672792633,1.83099568709752,7.1675355816879));
#49066=CARTESIAN_POINT('Ctrl Pts',(0.176549676601648,1.83038626107404,7.16746759838611));
#49067=CARTESIAN_POINT('Ctrl Pts',(0.176193699927816,1.83015349431801,7.16744152763448));
#49068=CARTESIAN_POINT('Ctrl Pts',(0.175507634159402,1.82970682455841,7.1673912958986));
#49069=CARTESIAN_POINT('Ctrl Pts',(0.17517761200932,1.82949281971256,7.16736713877706));
#49070=CARTESIAN_POINT('Ctrl Pts',(0.174423620714499,1.8290058479909,7.16731196131098));
#49071=CARTESIAN_POINT('Ctrl Pts',(0.173999401822543,1.82873327139681,7.16728092650671));
#49072=CARTESIAN_POINT('Ctrl Pts',(0.172701248092291,1.82790345682002,7.1671859853633));
#49073=CARTESIAN_POINT('Ctrl Pts',(0.171825269655629,1.82734944237963,7.16712195965318));
#49074=CARTESIAN_POINT('Ctrl Pts',(0.165368791278093,1.82330950109726,7.16665031864639));
#49075=CARTESIAN_POINT('Ctrl Pts',(0.159685725592238,1.81999120001971,7.16623658213313));
#49076=CARTESIAN_POINT('Ctrl Pts',(0.152298047535376,1.81597565727743,7.16569995259205));
#49077=CARTESIAN_POINT('Ctrl Pts',(0.150683302517143,1.81511569950088,7.16558273528386));
#49078=CARTESIAN_POINT('Ctrl Pts',(0.146910906440143,1.81314769627703,7.16530906169921));
#49079=CARTESIAN_POINT('Ctrl Pts',(0.144747913307431,1.8120501785095,7.16515227313494));
#49080=CARTESIAN_POINT('Ctrl Pts',(0.122072477424548,1.80086455584873,7.16351000926168));
#49081=CARTESIAN_POINT('Ctrl Pts',(0.100556459459548,1.79296278833644,7.16195680674421));
#49082=CARTESIAN_POINT('Ctrl Pts',(0.0620117514286712,1.78329695932595,
7.15927393789732));
#49083=CARTESIAN_POINT('Ctrl Pts',(0.0453341799327445,1.78048279742726,
7.15814572829134));
#49084=CARTESIAN_POINT('Ctrl Pts',(0.0277536615550807,1.77892136813086,
7.15703775031985));
#49085=CARTESIAN_POINT('Ctrl Pts',(0.0269961689228732,1.77885679134695,
7.15699016954855));
#49086=CARTESIAN_POINT('Ctrl Pts',(0.0259253251524913,1.77876931678384,
7.15692313712521));
#49087=CARTESIAN_POINT('Ctrl Pts',(0.0256121656616808,1.77874419647902,
7.15690356195035));
#49088=CARTESIAN_POINT('Ctrl Pts',(0.0250753340672944,1.77870192411281,
7.15687005374922));
#49089=CARTESIAN_POINT('Ctrl Pts',(0.0248516802945224,1.77868454762483,
7.1568561080264));
#49090=CARTESIAN_POINT('Ctrl Pts',(0.0244240745994598,1.77865177449096,
7.15682947282573));
#49091=CARTESIAN_POINT('Ctrl Pts',(0.024220126413474,1.77863633849651,7.15681678111387));
#49092=CARTESIAN_POINT('Ctrl Pts',(0.023740661801027,1.77860050882581,7.15678697202778));
#49093=CARTESIAN_POINT('Ctrl Pts',(0.0234651330276437,1.77858027521153,
7.15676986371813));
#49094=CARTESIAN_POINT('Ctrl Pts',(0.0226541240340236,1.77852176669058,
7.15671956916412));
#49095=CARTESIAN_POINT('Ctrl Pts',(0.0221185704567568,1.77848447521429,
7.15668643791462));
#49096=CARTESIAN_POINT('Ctrl Pts',(0.0208332337005212,1.77839820186648,
7.15660711139009));
#49097=CARTESIAN_POINT('Ctrl Pts',(0.0200833634576213,1.77835050330016,
7.15656098624244));
#49098=CARTESIAN_POINT('Ctrl Pts',(0.000145393721831734,1.77715226349491,
7.15533852202367));
#49099=CARTESIAN_POINT('Ctrl Pts',(-0.0191105344568808,1.7777179681163,
7.1542536386443));
#49100=CARTESIAN_POINT('Ctrl Pts',(-0.0546232763953682,1.78195767842658,
7.15225072680636));
#49101=CARTESIAN_POINT('Ctrl Pts',(-0.0708673817861991,1.78517876452074,
7.15133331209747));
#49102=CARTESIAN_POINT('Ctrl Pts',(-0.0990689251306978,1.79306509479421,
7.14965661530244));
#49103=CARTESIAN_POINT('Ctrl Pts',(-0.111130108241283,1.79722330131339,
7.14891107296106));
#49104=CARTESIAN_POINT('Ctrl Pts',(-0.124928979902279,1.80291636860456,
7.14800926632561));
#49105=CARTESIAN_POINT('Ctrl Pts',(-0.12693694404102,1.8037687627243,7.14787680670359));
#49106=CARTESIAN_POINT('Ctrl Pts',(-0.129557369474019,1.80491268542092,
7.14770227054132));
#49107=CARTESIAN_POINT('Ctrl Pts',(-0.130177815104248,1.80518586931061,
7.14766082124836));
#49108=CARTESIAN_POINT('Ctrl Pts',(-0.131187896054326,1.80563442096466,
7.1475931381474));
#49109=CARTESIAN_POINT('Ctrl Pts',(-0.131578054911789,1.80580861050191,
7.14756694477202));
#49110=CARTESIAN_POINT('Ctrl Pts',(-0.132328472658957,1.80614543191475,
7.1475164689827));
#49111=CARTESIAN_POINT('Ctrl Pts',(-0.132688781231137,1.8063079517692,7.14749219045345));
#49112=CARTESIAN_POINT('Ctrl Pts',(-0.133513071423839,1.8066815804788,7.14743654892749));
#49113=CARTESIAN_POINT('Ctrl Pts',(-0.133976852114343,1.80689312774312,
7.14740517087892));
#49114=CARTESIAN_POINT('Ctrl Pts',(-0.135433397999181,1.80756169064322,
7.14730639813092));
#49115=CARTESIAN_POINT('Ctrl Pts',(-0.13642433360054,1.80802265288629,7.14723886737813));
#49116=CARTESIAN_POINT('Ctrl Pts',(-0.144574516915071,1.81186449389571,
7.14668066831389));
#49117=CARTESIAN_POINT('Ctrl Pts',(-0.151608737753756,1.81550284077843,
7.14618108099469));
#49118=CARTESIAN_POINT('Ctrl Pts',(-0.162680773043203,1.82175697325576,
7.14536455693147));
#49119=CARTESIAN_POINT('Ctrl Pts',(-0.166806697777298,1.82421070039919,
7.14505326363114));
#49120=CARTESIAN_POINT('Ctrl Pts',(-0.181464483258324,1.83337709232269,
7.14392204760567));
#49121=CARTESIAN_POINT('Ctrl Pts',(-0.191658172177291,1.84060795558669,
7.14308657625044));
#49122=CARTESIAN_POINT('Ctrl Pts',(-0.20941687879557,1.85482445180407,7.14155109658215));
#49123=CARTESIAN_POINT('Ctrl Pts',(-0.217116957025728,1.86161647230335,
7.1408544777012));
#49124=CARTESIAN_POINT('Ctrl Pts',(-0.232798327961972,1.87683969192324,
7.1393831028209));
#49125=CARTESIAN_POINT('Ctrl Pts',(-0.240675779895153,1.8853588955521,7.13861094035751));
#49126=CARTESIAN_POINT('Ctrl Pts',(-0.250469529860458,1.89716944848208,
7.13762416207072));
#49127=CARTESIAN_POINT('Ctrl Pts',(-0.25281116226563,1.90009567968783,7.13738600744693));
#49128=CARTESIAN_POINT('Ctrl Pts',(-0.255428053182532,1.90348544300511,
7.13711790691739));
#49129=CARTESIAN_POINT('Ctrl Pts',(-0.255753712611385,1.90390945979272,
7.13708450761479));
#49130=CARTESIAN_POINT('Ctrl Pts',(-0.256243489388205,1.90455045719791,
7.1370342254007));
#49131=CARTESIAN_POINT('Ctrl Pts',(-0.256408387587222,1.90476683577931,
7.13701728755449));
#49132=CARTESIAN_POINT('Ctrl Pts',(-0.256705059680292,1.90515715158784,
7.1369867987769));
#49133=CARTESIAN_POINT('Ctrl Pts',(-0.256836930584162,1.90533101343083,
7.13697324097551));
#49134=CARTESIAN_POINT('Ctrl Pts',(-0.257120336103367,1.90570545149304,
7.13694409187519));
#49135=CARTESIAN_POINT('Ctrl Pts',(-0.257271812194207,1.90590607049994,
7.13692850474179));
#49136=CARTESIAN_POINT('Ctrl Pts',(-0.257680062459309,1.90644808572561,
7.13688647459834));
#49137=CARTESIAN_POINT('Ctrl Pts',(-0.257936393968769,1.9067898170911,7.13686006277904));
#49138=CARTESIAN_POINT('Ctrl Pts',(-0.259122036675068,1.90837703535284,
7.13673778931918));
#49139=CARTESIAN_POINT('Ctrl Pts',(-0.26004303137767,1.90962875077835,7.13664250099883));
#49140=CARTESIAN_POINT('Ctrl Pts',(-0.279578882735,1.93658607356592,7.13461346247785));
#49141=CARTESIAN_POINT('Ctrl Pts',(-0.294308035287303,1.96489990757853,
7.13291710837441));
#49142=CARTESIAN_POINT('Ctrl Pts',(-0.309845184768981,2.00994492344333,
7.13021776030257));
#49143=CARTESIAN_POINT('Ctrl Pts',(-0.313909469118058,2.02533607985318,
7.1292978828455));
#49144=CARTESIAN_POINT('Ctrl Pts',(-0.317278022014857,2.04341338299091,
7.12818894739764));
#49145=CARTESIAN_POINT('Ctrl Pts',(-0.317706176241206,2.0458689228088,7.12803775565299));
#49146=CARTESIAN_POINT('Ctrl Pts',(-0.318219923563956,2.04903174938022,
7.12784221936802));
#49147=CARTESIAN_POINT('Ctrl Pts',(-0.318331723197484,2.0497347404502,7.12779870784932));
#49148=CARTESIAN_POINT('Ctrl Pts',(-0.318508067211456,2.05086777184486,
7.12772849604789));
#49149=CARTESIAN_POINT('Ctrl Pts',(-0.318574072251585,2.05129758518951,
7.12770184211314));
#49150=CARTESIAN_POINT('Ctrl Pts',(-0.318698099767292,2.05211627187661,
7.12765103595224));
#49151=CARTESIAN_POINT('Ctrl Pts',(-0.318756280958212,2.05250512067823,
7.12762688880299));
#49152=CARTESIAN_POINT('Ctrl Pts',(-0.318887264988565,2.05339162293256,
7.12757180112378));
#49153=CARTESIAN_POINT('Ctrl Pts',(-0.318959614596547,2.05388934139922,
7.12754084630556));
#49154=CARTESIAN_POINT('Ctrl Pts',(-0.319176575755416,2.05540683932996,
7.12744638645482));
#49155=CARTESIAN_POINT('Ctrl Pts',(-0.319317462827825,2.05642713707765,
7.12738276381433));
#49156=CARTESIAN_POINT('Ctrl Pts',(-0.320303813363428,2.06383204644101,
7.12692018234204));
#49157=CARTESIAN_POINT('Ctrl Pts',(-0.320962562003768,2.07023965959339,
7.1265153636209));
#49158=CARTESIAN_POINT('Ctrl Pts',(-0.321549566091602,2.07832445353951,
7.12599837015445));
#49159=CARTESIAN_POINT('Ctrl Pts',(-0.321657348866209,2.07998744078261,
7.12589170114141));
#49160=CARTESIAN_POINT('Ctrl Pts',(-0.322105333914157,2.08784299069095,
7.12538627388136));
#49161=CARTESIAN_POINT('Ctrl Pts',(-0.322279614612699,2.0940433830894,7.12498276239407));
#49162=CARTESIAN_POINT('Ctrl Pts',(-0.322262348256002,2.11678883775222,
7.1234866357659));
#49163=CARTESIAN_POINT('Ctrl Pts',(-0.320975845377665,2.13330628802755,
7.1223677248446));
#49164=CARTESIAN_POINT('Ctrl Pts',(-0.317188867608192,2.15759362591997,
7.12070459164423));
#49165=CARTESIAN_POINT('Ctrl Pts',(-0.315653523635841,2.16548788791474,
7.12016148990717));
#49166=CARTESIAN_POINT('Ctrl Pts',(-0.31289075550399,2.1773136375016,7.11935032801859));
#49167=CARTESIAN_POINT('Ctrl Pts',(-0.311880661653496,2.18129254918058,
7.11907784050749));
#49168=CARTESIAN_POINT('Ctrl Pts',(-0.31029086461408,2.18708836943625,7.11868251662596));
#49169=CARTESIAN_POINT('Ctrl Pts',(-0.309770638876115,2.18892106800197,
7.11855774716158));
#49170=CARTESIAN_POINT('Ctrl Pts',(-0.307596896968879,2.19632825372172,
7.11805470582299));
#49171=CARTESIAN_POINT('Ctrl Pts',(-0.305808790659011,2.20186254260865,
7.1176816975331));
#49172=CARTESIAN_POINT('Ctrl Pts',(-0.303652508737178,2.20796648955053,
7.11727578633766));
#49173=CARTESIAN_POINT('Ctrl Pts',(-0.303431347827496,2.208586491342,7.11723462030247));
#49174=CARTESIAN_POINT('Ctrl Pts',(-0.303117928155636,2.20945669627928,
7.11717693595468));
#49175=CARTESIAN_POINT('Ctrl Pts',(-0.303027258038863,2.20970746381378,
7.11716032404706));
#49176=CARTESIAN_POINT('Ctrl Pts',(-0.302860400179207,2.21016715973139,
7.11712989245255));
#49177=CARTESIAN_POINT('Ctrl Pts',(-0.302784307253642,2.21037612224525,
7.11711606708295));
#49178=CARTESIAN_POINT('Ctrl Pts',(-0.302628730876535,2.21080198660882,
7.11708790725663));
#49179=CARTESIAN_POINT('Ctrl Pts',(-0.302549230493761,2.21101888180324,
7.11707357384942));
#49180=CARTESIAN_POINT('Ctrl Pts',(-0.302349824077097,2.21156110307517,
7.11703776239858));
#49181=CARTESIAN_POINT('Ctrl Pts',(-0.302229625753394,2.21188632248157,
7.11701630190445));
#49182=CARTESIAN_POINT('Ctrl Pts',(-0.301770226153508,2.21312317338741,
7.11693475455009));
#49183=CARTESIAN_POINT('Ctrl Pts',(-0.30142741867156,2.21403347350754,7.11687488127779));
#49184=CARTESIAN_POINT('Ctrl Pts',(-0.295780582292549,2.22882483775608,
7.11590414141355));
#49185=CARTESIAN_POINT('Ctrl Pts',(-0.289526029835463,2.24232637429556,
7.11504838364258));
#49186=CARTESIAN_POINT('Ctrl Pts',(-0.267594551687138,2.28218867479503,
7.11247749035381));
#49187=CARTESIAN_POINT('Ctrl Pts',(-0.249078737845497,2.30678322651194,
7.11081119414682));
#49188=CARTESIAN_POINT('Ctrl Pts',(-0.223852827843128,2.33189590955406,
7.10869325372474));
#49189=CARTESIAN_POINT('Ctrl Pts',(-0.220255734483652,2.33531512638742,
7.10839467644041));
#49190=CARTESIAN_POINT('Ctrl Pts',(-0.215948150496158,2.33922437776374,
7.10804041553106));
#49191=CARTESIAN_POINT('Ctrl Pts',(-0.215312743509094,2.33979643258324,
7.10798824093273));
#49192=CARTESIAN_POINT('Ctrl Pts',(-0.214291747086897,2.3407083025167,7.10790453209253));
#49193=CARTESIAN_POINT('Ctrl Pts',(-0.213907605090611,2.34104973812388,
7.10787306592459));
#49194=CARTESIAN_POINT('Ctrl Pts',(-0.213226098019814,2.34165256775135,
7.10781729151451));
#49195=CARTESIAN_POINT('Ctrl Pts',(-0.212929064214269,2.34191433605347,
7.10779299897608));
#49196=CARTESIAN_POINT('Ctrl Pts',(-0.212311869174775,2.34245623689717,
7.10774255652722));
#49197=CARTESIAN_POINT('Ctrl Pts',(-0.21199163428715,2.34273628404572,7.10771640313179));
#49198=CARTESIAN_POINT('Ctrl Pts',(-0.211165966089647,2.3434554552358,7.10764901933406));
#49199=CARTESIAN_POINT('Ctrl Pts',(-0.2106597189778,2.34389363810488,7.10760775003477));
#49200=CARTESIAN_POINT('Ctrl Pts',(-0.208552391588162,2.34570618209572,
7.10743614801881));
#49201=CARTESIAN_POINT('Ctrl Pts',(-0.20693922697647,2.34706635536878,7.10730523302298));
#49202=CARTESIAN_POINT('Ctrl Pts',(-0.196002764203761,2.35610540881497,
7.10642051758089));
#49203=CARTESIAN_POINT('Ctrl Pts',(-0.186268585298666,2.36326985527563,
7.10564615994524));
#49204=CARTESIAN_POINT('Ctrl Pts',(-0.1605784018685,2.38003896309464,7.10363346739836));
#49205=CARTESIAN_POINT('Ctrl Pts',(-0.144150501134148,2.38883863456212,
7.10237260273249));
#49206=CARTESIAN_POINT('Ctrl Pts',(-0.113994571491387,2.40177550134341,
7.10015395213956));
#49207=CARTESIAN_POINT('Ctrl Pts',(-0.100574161219286,2.40650958317826,
7.0991980225727));
#49208=CARTESIAN_POINT('Ctrl Pts',(-0.0862582124319157,2.410517501423,7.0982371937021));
#49209=CARTESIAN_POINT('Ctrl Pts',(-0.0856319112603594,2.41069080078061,
7.0981952756991));
#49210=CARTESIAN_POINT('Ctrl Pts',(-0.0813239415530555,2.41186881253136,
7.09790776731883));
#49211=CARTESIAN_POINT('Ctrl Pts',(-0.0776250036226671,2.41281000893629,
7.09766502291111));
#49212=CARTESIAN_POINT('Ctrl Pts',(-0.0733401069799455,2.41381960928317,
7.09738923748937));
#49213=CARTESIAN_POINT('Ctrl Pts',(-0.0727698195909753,2.4139523400645,
7.09735264254896));
#49214=CARTESIAN_POINT('Ctrl Pts',(-0.0719240158753521,2.4141467670927,
7.09729853413486));
#49215=CARTESIAN_POINT('Ctrl Pts',(-0.0716487791612777,2.41420965577238,
7.09728095253309));
#49216=CARTESIAN_POINT('Ctrl Pts',(-0.071159679167616,2.4143207338766,7.09724975646111));
#49217=CARTESIAN_POINT('Ctrl Pts',(-0.070945849412669,2.414369066761,7.09723613370798));
#49218=CARTESIAN_POINT('Ctrl Pts',(-0.0704931399376714,2.41447090926267,
7.09720732600517));
#49219=CARTESIAN_POINT('Ctrl Pts',(-0.07025424918716,2.41452436475235,7.09719214423422));
#49220=CARTESIAN_POINT('Ctrl Pts',(-0.0696161940843432,2.41466637621393,
7.09715164741341));
#49221=CARTESIAN_POINT('Ctrl Pts',(-0.0692169200641963,2.41475444521024,
7.09712636043669));
#49222=CARTESIAN_POINT('Ctrl Pts',(-0.067339035429188,2.41516490945325,
7.09700768152716));
#49223=CARTESIAN_POINT('Ctrl Pts',(-0.0658583020331896,2.41547765389543,
7.09691483588526));
#49224=CARTESIAN_POINT('Ctrl Pts',(-0.0538617142636338,2.41792329663941,
7.09616814619585));
#49225=CARTESIAN_POINT('Ctrl Pts',(-0.0432463287161987,2.41954047285849,
7.0955416361842));
#49226=CARTESIAN_POINT('Ctrl Pts',(-0.00374570487007546,2.4235529263946,
7.09327136828312));
#49227=CARTESIAN_POINT('Ctrl Pts',(0.0253402457034932,2.4225810377561,7.09170666032807));
#49228=CARTESIAN_POINT('Ctrl Pts',(0.0635246185721014,2.41610280457003,
7.08945268296261));
#49229=CARTESIAN_POINT('Ctrl Pts',(0.0730635150517995,2.41403511591887,
7.08887377639065));
#49230=CARTESIAN_POINT('Ctrl Pts',(0.0834981643884885,2.41127208791527,
7.08821739663599));
#49231=CARTESIAN_POINT('Ctrl Pts',(0.0845017236306666,2.41100114925064,
7.08815403158137));
#49232=CARTESIAN_POINT('Ctrl Pts',(0.0860010778749563,2.41058856399406,
7.0880590003116));
#49233=CARTESIAN_POINT('Ctrl Pts',(0.0864978790376826,2.41045057319428,
7.08802745278791));
#49234=CARTESIAN_POINT('Ctrl Pts',(0.0873530860885475,2.41021081990455,
7.08797304259636));
#49235=CARTESIAN_POINT('Ctrl Pts',(0.0877116516631416,2.41010962673816,
7.08795019847981));
#49236=CARTESIAN_POINT('Ctrl Pts',(0.0884514726111471,2.40989945119519,
7.0879029995511));
#49237=CARTESIAN_POINT('Ctrl Pts',(0.0888327038064695,2.40979038653645,
7.08787864209107));
#49238=CARTESIAN_POINT('Ctrl Pts',(0.0897198698529599,2.40953480905256,
7.0878218759029));
#49239=CARTESIAN_POINT('Ctrl Pts',(0.0902256476431692,2.40938775923387,
7.08778944970768));
#49240=CARTESIAN_POINT('Ctrl Pts',(0.0918374350681469,2.40891485976337,
7.08768591146829));
#49241=CARTESIAN_POINT('Ctrl Pts',(0.0929420481157377,2.40858431700137,
7.08761464628972));
#49242=CARTESIAN_POINT('Ctrl Pts',(0.117515345708149,2.40108712898436,7.08602233493944));
#49243=CARTESIAN_POINT('Ctrl Pts',(0.140085985852169,2.39127091521655,7.08440889888853));
#49244=CARTESIAN_POINT('Ctrl Pts',(0.180693468313031,2.36779067969438,7.08124504750092));
#49245=CARTESIAN_POINT('Ctrl Pts',(0.198848083068947,2.35460074146565,7.07971244089955));
#49246=CARTESIAN_POINT('Ctrl Pts',(0.218288566364723,2.33711904232689,7.07802996917359));
#49247=CARTESIAN_POINT('Ctrl Pts',(0.221042759673337,2.33455370363494,7.07779064833099));
#49248=CARTESIAN_POINT('Ctrl Pts',(0.224171193438992,2.33153572441439,7.0775183391751));
#49249=CARTESIAN_POINT('Ctrl Pts',(0.224589764226304,2.33112973297562,7.07748189552711));
#49250=CARTESIAN_POINT('Ctrl Pts',(0.225209018172919,2.33052581894337,7.07742796755386));
#49251=CARTESIAN_POINT('Ctrl Pts',(0.22541054436719,2.33032876840609,7.0774104157548));
#49252=CARTESIAN_POINT('Ctrl Pts',(0.225764574135038,2.32998169156504,7.07737957899283));
#49253=CARTESIAN_POINT('Ctrl Pts',(0.225917186819065,2.32983177780779,7.07736628520659));
#49254=CARTESIAN_POINT('Ctrl Pts',(0.22623960122763,2.32951443380739,7.07733819856865));
#49255=CARTESIAN_POINT('Ctrl Pts',(0.226409365975204,2.32934696747321,7.07732340869076));
#49256=CARTESIAN_POINT('Ctrl Pts',(0.226756926662201,2.32900335035898,7.07729312663948));
#49257=CARTESIAN_POINT('Ctrl Pts',(0.22693470365029,2.3288271805208,7.07727763598735));
#49258=CARTESIAN_POINT('Ctrl Pts',(0.22737470564928,2.32839013917179,7.07723929222329));
#49259=CARTESIAN_POINT('Ctrl Pts',(0.227636687924422,2.32812902216508,7.0772164583242));
#49260=CARTESIAN_POINT('Ctrl Pts',(0.228365022906173,2.32740058883793,7.07715296595715));
#49261=CARTESIAN_POINT('Ctrl Pts',(0.228830393255474,2.32693228644475,7.07711238368087));
#49262=CARTESIAN_POINT('Ctrl Pts',(0.232941528664527,2.32276974384338,7.07675371606796));
#49263=CARTESIAN_POINT('Ctrl Pts',(0.23649923837744,2.31898911404884,7.07644221605307));
#49264=CARTESIAN_POINT('Ctrl Pts',(0.244120794150171,2.3104874973938,7.07576797649159));
#49265=CARTESIAN_POINT('Ctrl Pts',(0.248142275551042,2.30573130113206,7.07540755742528));
#49266=CARTESIAN_POINT('Ctrl Pts',(0.270140389399782,2.27812994762096,7.07338966899759));
#49267=CARTESIAN_POINT('Ctrl Pts',(0.285098472785188,2.25305259135261,7.07181989266189));
#49268=CARTESIAN_POINT('Ctrl Pts',(0.300266264072809,2.21744826514252,7.06956643019965));
#49269=CARTESIAN_POINT('Ctrl Pts',(0.303641391143685,2.20842417619989,7.06899477192354));
#49270=CARTESIAN_POINT('Ctrl Pts',(0.30695721761685,2.19818214310459,7.06834012956416));
#49271=CARTESIAN_POINT('Ctrl Pts',(0.307301465948203,2.19709930816444,7.06827084926733));
#49272=CARTESIAN_POINT('Ctrl Pts',(0.307782621052962,2.19555764249331,7.0681721080388));
#49273=CARTESIAN_POINT('Ctrl Pts',(0.307924245447499,2.19510028350532,7.06814280187033));
#49274=CARTESIAN_POINT('Ctrl Pts',(0.308182215087405,2.19426058375324,7.068088971861));
#49275=CARTESIAN_POINT('Ctrl Pts',(0.308298869499309,2.19387833833664,7.06806445819768));
#49276=CARTESIAN_POINT('Ctrl Pts',(0.308533871648709,2.19310313685073,7.06801472465271));
#49277=CARTESIAN_POINT('Ctrl Pts',(0.308652180384782,2.19271016981555,7.06798950354797));
#49278=CARTESIAN_POINT('Ctrl Pts',(0.308941688302218,2.19174186166235,7.06792733107386));
#49279=CARTESIAN_POINT('Ctrl Pts',(0.309112030743056,2.19116626785396,7.06789035179104));
#49280=CARTESIAN_POINT('Ctrl Pts',(0.309728214511656,2.18906257698508,7.06775511683512));
#49281=CARTESIAN_POINT('Ctrl Pts',(0.310164335041205,2.18753167773042,7.0676565448922));
#49282=CARTESIAN_POINT('Ctrl Pts',(0.312620747519642,2.17866009722345,7.06708434329595));
#49283=CARTESIAN_POINT('Ctrl Pts',(0.314391596739544,2.17125342618661,7.06660268708062));
#49284=CARTESIAN_POINT('Ctrl Pts',(0.317330007324402,2.15670227733301,7.06564785982438));
#49285=CARTESIAN_POINT('Ctrl Pts',(0.318522446416637,2.14956733737658,7.06517574758331));
#49286=CARTESIAN_POINT('Ctrl Pts',(0.323976617061947,2.10847023081411,7.06243676288768));
#49287=CARTESIAN_POINT('Ctrl Pts',(0.323045970377624,2.07404492333451,7.06003718736388));
#49288=CARTESIAN_POINT('Ctrl Pts',(0.316474364236885,2.0391157400501,7.05779294239871));
#49289=CARTESIAN_POINT('Ctrl Pts',(0.316222454182139,2.03782061481557,7.05771004776966));
#49290=CARTESIAN_POINT('Ctrl Pts',(0.315882676039987,2.03612923009927,7.0576022405151));
#49291=CARTESIAN_POINT('Ctrl Pts',(0.31580200781607,2.0357315619177,7.0575769261146));
#49292=CARTESIAN_POINT('Ctrl Pts',(0.315676497389088,2.03511877848992,7.05753796949047));
#49293=CARTESIAN_POINT('Ctrl Pts',(0.315632186242368,2.03490355680197,7.0575242969312));
#49294=CARTESIAN_POINT('Ctrl Pts',(0.315544326903235,2.034479017911,7.05749734644004));
#49295=CARTESIAN_POINT('Ctrl Pts',(0.315500790824919,2.03426970010696,7.05748406797733));
#49296=CARTESIAN_POINT('Ctrl Pts',(0.315405367894482,2.03381319374924,7.05745512907025));
#49297=CARTESIAN_POINT('Ctrl Pts',(0.31535339888674,2.03356602352724,7.05743947345737));
#49298=CARTESIAN_POINT('Ctrl Pts',(0.315243172507686,2.03304481871844,7.05740648766453));
#49299=CARTESIAN_POINT('Ctrl Pts',(0.315184848227973,2.03277079829383,7.05738916133066));
#49300=CARTESIAN_POINT('Ctrl Pts',(0.31503374645828,2.03206540715891,7.05734459916072));
#49301=CARTESIAN_POINT('Ctrl Pts',(0.314940439874659,2.03163414851711,7.05731739327539));
#49302=CARTESIAN_POINT('Ctrl Pts',(0.314666085167614,2.03037857559652,7.05723829371443));
#49303=CARTESIAN_POINT('Ctrl Pts',(0.314482682716142,2.02955477163909,7.05718653086192));
#49304=CARTESIAN_POINT('Ctrl Pts',(0.312531345229022,2.02094929709104,7.05664714546488));
#49305=CARTESIAN_POINT('Ctrl Pts',(0.31047803265197,2.01323439415378,7.0561749505838));
#49306=CARTESIAN_POINT('Ctrl Pts',(0.308061057403647,2.00534465918494,7.05569644159124));
#49307=CARTESIAN_POINT('Ctrl Pts',(0.307981588315334,2.00508640828148,7.0556807837279));
#49308=CARTESIAN_POINT('Ctrl Pts',(0.30328152645721,1.98988066091884,7.05475912775252));
#49309=CARTESIAN_POINT('Ctrl Pts',(0.297578603027083,1.97528836196526,7.05388947261322));
#49310=CARTESIAN_POINT('Ctrl Pts',(0.284102340143277,1.94705720713177,7.05214041432178));
#49311=CARTESIAN_POINT('Ctrl Pts',(0.276349279724215,1.93345672455976,7.051263060015));
#49312=CARTESIAN_POINT('Ctrl Pts',(0.266616700666186,1.9189472796498,7.05024803770579));
#49313=CARTESIAN_POINT('Ctrl Pts',(0.265579992063179,1.91742995792557,7.05014088697745));
#49314=CARTESIAN_POINT('Ctrl Pts',(0.263466573161175,1.91439286333949,7.04992429425137));
#49315=CARTESIAN_POINT('Ctrl Pts',(0.262389553014563,1.91287339411709,7.04981484509499));
#49316=CARTESIAN_POINT('Ctrl Pts',(0.257400862899707,1.90596306129242,7.0493119011768));
#49317=CARTESIAN_POINT('Ctrl Pts',(0.25333604974078,1.90068523893572,7.04891314660957));
#49318=CARTESIAN_POINT('Ctrl Pts',(0.24845093764706,1.89473337053546,7.04844453558066));
#49319=CARTESIAN_POINT('Ctrl Pts',(0.247787131298227,1.89393254717773,7.04838107571662));
#49320=CARTESIAN_POINT('Ctrl Pts',(0.246795325312391,1.89274774299909,7.04828657306534));
#49321=CARTESIAN_POINT('Ctrl Pts',(0.246470276735994,1.8923612913999,7.04825565086332));
#49322=CARTESIAN_POINT('Ctrl Pts',(0.245890370136613,1.89167511842218,7.04820057086992));
#49323=CARTESIAN_POINT('Ctrl Pts',(0.245635868468282,1.89137509609352,7.04817642773671));
#49324=CARTESIAN_POINT('Ctrl Pts',(0.245099613774348,1.89074526741301,7.04812561806141));
#49325=CARTESIAN_POINT('Ctrl Pts',(0.244817743184334,1.89041556259687,7.04809894670132));
#49326=CARTESIAN_POINT('Ctrl Pts',(0.244074708871005,1.88954997753592,7.04802873162201));
#49327=CARTESIAN_POINT('Ctrl Pts',(0.243612447782053,1.88901504617982,7.04798514254404));
#49328=CARTESIAN_POINT('Ctrl Pts',(0.241543161637114,1.88663632268509,7.04779042954016));
#49329=CARTESIAN_POINT('Ctrl Pts',(0.23991697205436,1.88480937817624,7.04763850868369));
#49330=CARTESIAN_POINT('Ctrl Pts',(0.227903786403204,1.87161859838849,7.04652387378808));
#49331=CARTESIAN_POINT('Ctrl Pts',(0.216736665122448,1.86099519923503,7.04552733244548));
#49332=CARTESIAN_POINT('Ctrl Pts',(0.193710829799644,1.84203551557076,7.0435470418137));
#49333=CARTESIAN_POINT('Ctrl Pts',(0.18196352586825,1.83361908252853,7.04256875825986));
#49334=CARTESIAN_POINT('Ctrl Pts',(0.157242853619734,1.8183081315146,7.04060212307349));
#49335=CARTESIAN_POINT('Ctrl Pts',(0.144281038323525,1.81145419656402,7.03961618300631));
#49336=CARTESIAN_POINT('Ctrl Pts',(0.130346571959502,1.80526060731785,7.03863058960457));
#49337=CARTESIAN_POINT('Ctrl Pts',(0.129795478809724,1.80501750541462,7.03859172872708));
#49338=CARTESIAN_POINT('Ctrl Pts',(0.125701075398107,1.80322505030837,7.03830390128516));
#49339=CARTESIAN_POINT('Ctrl Pts',(0.122130619371397,1.80173795709965,7.03805786104215));
#49340=CARTESIAN_POINT('Ctrl Pts',(0.117987463328093,1.80009921700317,7.03777873233548));
#49341=CARTESIAN_POINT('Ctrl Pts',(0.11744026196051,1.79988451218187,7.03774199378621));
#49342=CARTESIAN_POINT('Ctrl Pts',(0.116628948483193,1.79956873670526,7.03768771415969));
#49343=CARTESIAN_POINT('Ctrl Pts',(0.116365289754814,1.79946651612355,7.03767010433063));
#49344=CARTESIAN_POINT('Ctrl Pts',(0.115904223122728,1.79928845814008,7.03763936213499));
#49345=CARTESIAN_POINT('Ctrl Pts',(0.115706875086156,1.79921246800396,7.03762622052711));
#49346=CARTESIAN_POINT('Ctrl Pts',(0.115288021760231,1.79905165904837,7.03759836445504));
#49347=CARTESIAN_POINT('Ctrl Pts',(0.115066498124971,1.79896689070295,7.03758365307852));
#49348=CARTESIAN_POINT('Ctrl Pts',(0.114486317669273,1.7987456125459,7.03754517822606));
#49349=CARTESIAN_POINT('Ctrl Pts',(0.114127508899802,1.79860949814274,7.03752143859003));
#49350=CARTESIAN_POINT('Ctrl Pts',(0.113341821941568,1.79831305140509,7.0374695739202));
#49351=CARTESIAN_POINT('Ctrl Pts',(0.112914844016257,1.79815298318473,7.03744146454163));
#49352=CARTESIAN_POINT('Ctrl Pts',(0.111659957412499,1.79768557855027,7.03735907087312));
#49353=CARTESIAN_POINT('Ctrl Pts',(0.110831115537407,1.79738073528566,7.03730493092383));
#49354=CARTESIAN_POINT('Ctrl Pts',(0.107958577736139,1.79633761711331,7.03711823122184));
#49355=CARTESIAN_POINT('Ctrl Pts',(0.105908624798248,1.79561658874118,7.03698662746997));
#49356=CARTESIAN_POINT('Ctrl Pts',(0.0968195354459518,1.79252263314644,
7.03640965729422));
#49357=CARTESIAN_POINT('Ctrl Pts',(0.0897063901530078,1.79037258860609,
7.03597532285138));
#49358=CARTESIAN_POINT('Ctrl Pts',(0.0543872650622043,1.78101649230613,
7.03387397843983));
#49359=CARTESIAN_POINT('Ctrl Pts',(0.0253694705129781,1.77740887647372,
7.03230575919116));
#49360=CARTESIAN_POINT('Ctrl Pts',(-0.00698259479660888,1.77778433352114,
7.0304318434941));
#49361=CARTESIAN_POINT('Ctrl Pts',(-0.010224497878336,1.77787090933579,
7.03024284387156));
#49362=CARTESIAN_POINT('Ctrl Pts',(-0.021276461800953,1.7783330578041,7.0295935880953));
#49363=CARTESIAN_POINT('Ctrl Pts',(-0.0290734210578596,1.7789438829891,
7.02912704993763));
#49364=CARTESIAN_POINT('Ctrl Pts',(-0.0379084492797415,1.7799604996421,
7.028586007225));
#49365=CARTESIAN_POINT('Ctrl Pts',(-0.0389762625904412,1.78008878852612,
7.02852041092111));
#49366=CARTESIAN_POINT('Ctrl Pts',(-0.040553489288687,1.78028629307028,
7.02842321109846));
#49367=CARTESIAN_POINT('Ctrl Pts',(-0.0410634189600968,1.78035138744131,
7.0283917376933));
#49368=CARTESIAN_POINT('Ctrl Pts',(-0.0419658189716715,1.78046877706466,
7.02833595489603));
#49369=CARTESIAN_POINT('Ctrl Pts',(-0.0423583537076367,1.78052057615322,
7.02831166122327));
#49370=CARTESIAN_POINT('Ctrl Pts',(-0.0431723950779367,1.78062952412216,
7.02826122081048));
#49371=CARTESIAN_POINT('Ctrl Pts',(-0.0435938858058917,1.78068678436872,
7.02823507059398));
#49372=CARTESIAN_POINT('Ctrl Pts',(-0.0446783049670126,1.7808362917329,
7.02816770423745));
#49373=CARTESIAN_POINT('Ctrl Pts',(-0.0453410591795403,1.78092976956286,
7.02812644923911));
#49374=CARTESIAN_POINT('Ctrl Pts',(-0.0480900439311412,1.78132623662172,
7.02795498138124));
#49375=CARTESIAN_POINT('Ctrl Pts',(-0.0501735304390813,1.78164762244515,
7.02782418738384));
#49376=CARTESIAN_POINT('Ctrl Pts',(-0.0641545443459592,1.78394490247736,
7.02694072312956));
#49377=CARTESIAN_POINT('Ctrl Pts',(-0.0759348263133994,1.7865666399145,
7.02616755813896));
#49378=CARTESIAN_POINT('Ctrl Pts',(-0.102770014943821,1.79414063616274,
7.0243383787038));
#49379=CARTESIAN_POINT('Ctrl Pts',(-0.117662081075645,1.79955502941144,
7.02327128856972));
#49380=CARTESIAN_POINT('Ctrl Pts',(-0.139114226304058,1.80919486349171,
7.02167973772876));
#49381=CARTESIAN_POINT('Ctrl Pts',(-0.146018417557063,1.81259954576611,
7.02115887252852));
#49382=CARTESIAN_POINT('Ctrl Pts',(-0.159072875774539,1.81962908825824,
7.02016372087672));
#49383=CARTESIAN_POINT('Ctrl Pts',(-0.165237959194082,1.82321767393432,
7.01968909304237));
#49384=CARTESIAN_POINT('Ctrl Pts',(-0.176789487094563,1.83046527398876,
7.01879714209522));
#49385=CARTESIAN_POINT('Ctrl Pts',(-0.182194315061004,1.83408885459154,
7.01837865058815));
#49386=CARTESIAN_POINT('Ctrl Pts',(-0.187982182717425,1.83822863698592,
7.01793236177384));
#49387=CARTESIAN_POINT('Ctrl Pts',(-0.188477189113209,1.83858481927819,
7.01789420844203));
#49388=CARTESIAN_POINT('Ctrl Pts',(-0.189209832866408,1.839115156504,7.01783776548697));
#49389=CARTESIAN_POINT('Ctrl Pts',(-0.189448243638212,1.83928823309377,
7.01781940249247));
#49390=CARTESIAN_POINT('Ctrl Pts',(-0.189855654552497,1.83958485089738,
7.01778803034999));
#49391=CARTESIAN_POINT('Ctrl Pts',(-0.190024771683044,1.8397082298745,7.01777500997241));
#49392=CARTESIAN_POINT('Ctrl Pts',(-0.190368614716663,1.83995959340003,
7.0177485422127));
#49393=CARTESIAN_POINT('Ctrl Pts',(-0.190543331373119,1.84008758897803,
7.01773509574301));
#49394=CARTESIAN_POINT('Ctrl Pts',(-0.190948932848502,1.8403853571173,7.01770388571654));
#49395=CARTESIAN_POINT('Ctrl Pts',(-0.191179721085091,1.84055526214154,
7.01768613142032));
#49396=CARTESIAN_POINT('Ctrl Pts',(-0.191665781114701,1.8409140975815,7.01764874766298));
#49397=CARTESIAN_POINT('Ctrl Pts',(-0.191921001122467,1.84110309810175,
7.01762912308646));
#49398=CARTESIAN_POINT('Ctrl Pts',(-0.192602322693779,1.84160920481811,
7.01757674613616));
#49399=CARTESIAN_POINT('Ctrl Pts',(-0.193027922628295,1.84192698932877,
7.01754404024286));
#49400=CARTESIAN_POINT('Ctrl Pts',(-0.194323272981757,1.8428991911382,7.01744452808297));
#49401=CARTESIAN_POINT('Ctrl Pts',(-0.195190506016894,1.84355697167317,
7.01737794786246));
#49402=CARTESIAN_POINT('Ctrl Pts',(-0.198348405524655,1.84597748161646,
7.0171355953482));
#49403=CARTESIAN_POINT('Ctrl Pts',(-0.200618737009237,1.84776666861259,
7.01696153207827));
#49404=CARTESIAN_POINT('Ctrl Pts',(-0.208549356609901,1.85419140850358,
7.01635289538663));
#49405=CARTESIAN_POINT('Ctrl Pts',(-0.214075883094494,1.85898915188719,
7.01592762920278));
#49406=CARTESIAN_POINT('Ctrl Pts',(-0.238614424206793,1.88180249401936,
7.01400894883816));
#49407=CARTESIAN_POINT('Ctrl Pts',(-0.255549485726991,1.90190513946523,
7.01258879534681));
#49408=CARTESIAN_POINT('Ctrl Pts',(-0.270952827447319,1.92550158926302,
7.01096842668715));
#49409=CARTESIAN_POINT('Ctrl Pts',(-0.27202438237476,1.92717678035148,7.01085367388661));
#49410=CARTESIAN_POINT('Ctrl Pts',(-0.274571356972268,1.93124091425272,
7.01057581224792));
#49411=CARTESIAN_POINT('Ctrl Pts',(-0.27603117631089,1.93363940314634,7.01041226987453));
#49412=CARTESIAN_POINT('Ctrl Pts',(-0.278372731157117,1.93760227423902,
7.01014253190899));
#49413=CARTESIAN_POINT('Ctrl Pts',(-0.27927307574866,1.93915551680862,7.01003692579288));
#49414=CARTESIAN_POINT('Ctrl Pts',(-0.283365489180155,1.94635356190852,
7.00954790329499));
#49415=CARTESIAN_POINT('Ctrl Pts',(-0.28639952388579,1.95208606518621,7.0091594690034));
#49416=CARTESIAN_POINT('Ctrl Pts',(-0.289713480954574,1.95883222838706,
7.00870201336474));
#49417=CARTESIAN_POINT('Ctrl Pts',(-0.290164072810823,1.95976073445727,
7.00863904550273));
#49418=CARTESIAN_POINT('Ctrl Pts',(-0.290827781224833,1.96114528934606,
7.00854513519034));
#49419=CARTESIAN_POINT('Ctrl Pts',(-0.291044304912739,1.96159970528837,
7.00851431111334));
#49420=CARTESIAN_POINT('Ctrl Pts',(-0.291428078337402,1.96241000977351,
7.00845934132245));
#49421=CARTESIAN_POINT('Ctrl Pts',(-0.291595743367116,1.96276570143743,
7.00843521005259));
#49422=CARTESIAN_POINT('Ctrl Pts',(-0.291947354211031,1.96351517704731,
7.00838435921913));
#49423=CARTESIAN_POINT('Ctrl Pts',(-0.29213115512795,1.96390902775014,7.00835763470621));
#49424=CARTESIAN_POINT('Ctrl Pts',(-0.292613457736634,1.96494799057286,
7.00828712972692));
#49425=CARTESIAN_POINT('Ctrl Pts',(-0.292910621554807,1.96559371790599,
7.00824330321898));
#49426=CARTESIAN_POINT('Ctrl Pts',(-0.294236129383136,1.9684992770775,7.00804606305707));
#49427=CARTESIAN_POINT('Ctrl Pts',(-0.295240452219731,1.97076991533785,
7.00789182680763));
#49428=CARTESIAN_POINT('Ctrl Pts',(-0.302439557748369,1.98756817643144,
7.00674980513678));
#49429=CARTESIAN_POINT('Ctrl Pts',(-0.307584287626813,2.00251987872177,
7.00572636306098));
#49430=CARTESIAN_POINT('Ctrl Pts',(-0.318700063766326,2.04465176146148,
7.00282978814953));
#49431=CARTESIAN_POINT('Ctrl Pts',(-0.322283427778208,2.07231762602878,
7.00090542424288));
#49432=CARTESIAN_POINT('Ctrl Pts',(-0.322274985117328,2.10009794195348,
6.99910071866258));
#49433=CARTESIAN_POINT('',(-0.322274994862272,2.1000575458305,6.74968051971722));
#49434=CARTESIAN_POINT('Ctrl Pts',(-0.32227498500109,2.10009832368563,6.99910069386394));
#49435=CARTESIAN_POINT('Ctrl Pts',(-0.322273394266979,2.10531226383204,
6.99876197848564));
#49436=CARTESIAN_POINT('Ctrl Pts',(-0.322145272370923,2.11052583289153,
6.99842819032332));
#49437=CARTESIAN_POINT('Ctrl Pts',(-0.321867792789241,2.11620244344203,
6.99807173565523));
#49438=CARTESIAN_POINT('Ctrl Pts',(-0.321843893543514,2.11667043502029,
6.99804240060918));
#49439=CARTESIAN_POINT('Ctrl Pts',(-0.321803465791486,2.11742957447782,
6.99799490147959));
#49440=CARTESIAN_POINT('Ctrl Pts',(-0.321787562812519,2.11772075288088,
6.99797670303981));
#49441=CARTESIAN_POINT('Ctrl Pts',(-0.321759019854199,2.11823065457684,
6.99794487094262));
#49442=CARTESIAN_POINT('Ctrl Pts',(-0.321746552046533,2.11844938672925,
6.99793122768086));
#49443=CARTESIAN_POINT('Ctrl Pts',(-0.321721866840363,2.11887482176612,
6.99790471451509));
#49444=CARTESIAN_POINT('Ctrl Pts',(-0.321709673247518,2.11908152614001,
6.99789184325585));
#49445=CARTESIAN_POINT('Ctrl Pts',(-0.321685015419126,2.11949278007728,
6.99786625615442));
#49446=CARTESIAN_POINT('Ctrl Pts',(-0.321672555309565,2.11969732929989,
6.99785354009536));
#49447=CARTESIAN_POINT('Ctrl Pts',(-0.321642742305764,2.12017917593869,
6.99782360979231));
#49448=CARTESIAN_POINT('Ctrl Pts',(-0.321625225872823,2.12045646360296,
6.99780640479926));
#49449=CARTESIAN_POINT('Ctrl Pts',(-0.321572420438914,2.12127554517366,
6.99775563797857));
#49450=CARTESIAN_POINT('Ctrl Pts',(-0.321536120631604,2.12181727638075,
6.99772213261776));
#49451=CARTESIAN_POINT('Ctrl Pts',(-0.32120570653987,2.12656829426715,6.99742889318035));
#49452=CARTESIAN_POINT('Ctrl Pts',(-0.320830302455053,2.13077176228369,
6.99717361353515));
#49453=CARTESIAN_POINT('Ctrl Pts',(-0.32033974101806,2.13526636794511,6.99690396535509));
#49454=CARTESIAN_POINT('Ctrl Pts',(-0.320306634053047,2.13556580614128,
6.9968860167309));
#49455=CARTESIAN_POINT('Ctrl Pts',(-0.320118844803548,2.13724274782419,
6.99678558545158));
#49456=CARTESIAN_POINT('Ctrl Pts',(-0.319955694016345,2.13861930930996,
6.99670346994184));
#49457=CARTESIAN_POINT('Ctrl Pts',(-0.315779900155303,2.17200741899123,
6.99471878398271));
#49458=CARTESIAN_POINT('Ctrl Pts',(-0.306991855219437,2.20324023676939,
6.99300120510939));
#49459=CARTESIAN_POINT('Ctrl Pts',(-0.289054325424564,2.24295688091424,
6.99049160961168));
#49460=CARTESIAN_POINT('Ctrl Pts',(-0.283860587421136,2.2530104494352,6.98982699886512));
#49461=CARTESIAN_POINT('Ctrl Pts',(-0.277126329547365,2.26451832250975,
6.98902073630722));
#49462=CARTESIAN_POINT('Ctrl Pts',(-0.276086535752685,2.26625734707131,
6.98889763324885));
#49463=CARTESIAN_POINT('Ctrl Pts',(-0.274686733095346,2.2685491295007,6.98873367449715));
#49464=CARTESIAN_POINT('Ctrl Pts',(-0.27434131110749,2.26911077849646,6.98869335426107));
#49465=CARTESIAN_POINT('Ctrl Pts',(-0.273771384873471,2.27003112513138,
6.98862705367126));
#49466=CARTESIAN_POINT('Ctrl Pts',(-0.273547892310323,2.27039044955294,
6.9886011106434));
#49467=CARTESIAN_POINT('Ctrl Pts',(-0.273113459798528,2.27108585900339,
6.98855078992826));
#49468=CARTESIAN_POINT('Ctrl Pts',(-0.272902605469578,2.27142199683741,
6.98852641543805));
#49469=CARTESIAN_POINT('Ctrl Pts',(-0.27241433569225,2.27219719820903,6.98847008433365));
#49470=CARTESIAN_POINT('Ctrl Pts',(-0.272136479151973,2.2726359813927,6.98843811140357));
#49471=CARTESIAN_POINT('Ctrl Pts',(-0.271243171722151,2.27403915146648,
6.98833558221727));
#49472=CARTESIAN_POINT('Ctrl Pts',(-0.270623651009538,2.27500092545252,
6.98826487470105));
#49473=CARTESIAN_POINT('Ctrl Pts',(-0.264866287043823,2.28383525279775,
6.98761137079271));
#49474=CARTESIAN_POINT('Ctrl Pts',(-0.259391885455071,2.29148203631538,
6.9870159303062));
#49475=CARTESIAN_POINT('Ctrl Pts',(-0.235552082798775,2.32188042687472,
6.98451933145408));
#49476=CARTESIAN_POINT('Ctrl Pts',(-0.214467866925369,2.34231946544718,
6.98250932336448));
#49477=CARTESIAN_POINT('Ctrl Pts',(-0.184030761605687,2.36470187333624,
6.97998487286626));
#49478=CARTESIAN_POINT('Ctrl Pts',(-0.176937026545758,2.36949529789416,
6.97942031534484));
#49479=CARTESIAN_POINT('Ctrl Pts',(-0.167631499824653,2.37525724384033,
6.97871713224788));
#49480=CARTESIAN_POINT('Ctrl Pts',(-0.165588693619503,2.37649096789478,
6.97856498740824));
#49481=CARTESIAN_POINT('Ctrl Pts',(-0.162717171365165,2.37818194158573,
6.97835440533843));
#49482=CARTESIAN_POINT('Ctrl Pts',(-0.161899916087764,2.37865837095621,
6.97829483936127));
#49483=CARTESIAN_POINT('Ctrl Pts',(-0.160665351903121,2.37937081117379,
6.97820542327895));
#49484=CARTESIAN_POINT('Ctrl Pts',(-0.160249603381173,2.37960949565634,
6.97817540791408));
#49485=CARTESIAN_POINT('Ctrl Pts',(-0.159486550367137,2.38004530946413,
6.97812049680117));
#49486=CARTESIAN_POINT('Ctrl Pts',(-0.159139409983029,2.38024272210929,
6.97809558313884));
#49487=CARTESIAN_POINT('Ctrl Pts',(-0.158582223805795,2.38055821495373,
6.97805570390672));
#49488=CARTESIAN_POINT('Ctrl Pts',(-0.158372412372924,2.380676704921,6.9780407119037));
#49489=CARTESIAN_POINT('Ctrl Pts',(-0.157982181064083,2.38089650924615,
6.97801287429366));
#49490=CARTESIAN_POINT('Ctrl Pts',(-0.157801797929628,2.38099788435305,
6.97800002481374));
#49491=CARTESIAN_POINT('Ctrl Pts',(-0.157382180554519,2.38123317733665,
6.97797017614492));
#49492=CARTESIAN_POINT('Ctrl Pts',(-0.157142873320758,2.38136696351348,
6.97795318554275));
#49493=CARTESIAN_POINT('Ctrl Pts',(-0.156530316076124,2.38170839214302,
6.97790977569463));
#49494=CARTESIAN_POINT('Ctrl Pts',(-0.156156821997096,2.38191559907786,
6.97788338440571));
#49495=CARTESIAN_POINT('Ctrl Pts',(-0.154031874119382,2.38308895846926,
6.97773366502484));
#49496=CARTESIAN_POINT('Ctrl Pts',(-0.152271817580715,2.38403955833609,
6.97761131482827));
#49497=CARTESIAN_POINT('Ctrl Pts',(-0.132996409234559,2.39421946570283,
6.97628812709693));
#49498=CARTESIAN_POINT('Ctrl Pts',(-0.114672298495858,2.40183379499441,
6.97517851398256));
#49499=CARTESIAN_POINT('Ctrl Pts',(-0.0938863658221463,2.40830242909191,
6.97396111011352));
#49500=CARTESIAN_POINT('Ctrl Pts',(-0.0920046665540028,2.40886919369937,
6.97385127803034));
#49501=CARTESIAN_POINT('Ctrl Pts',(-0.0879526054814601,2.41004935255688,
6.97361538203055));
#49502=CARTESIAN_POINT('Ctrl Pts',(-0.0857807539178932,2.41065724530525,
6.97348932208326));
#49503=CARTESIAN_POINT('Ctrl Pts',(-0.0810520792391858,2.41192741328235,
6.97321539659832));
#49504=CARTESIAN_POINT('Ctrl Pts',(-0.0784931409081298,2.41258115331239,
6.9730675001931));
#49505=CARTESIAN_POINT('Ctrl Pts',(-0.0667661940520024,2.41542398889303,
6.97239038693641));
#49506=CARTESIAN_POINT('Ctrl Pts',(-0.0575132821026026,2.41724158985611,
6.97185778658866));
#49507=CARTESIAN_POINT('Ctrl Pts',(-0.0367958541192967,2.42037499802886,
6.97065226152938));
#49508=CARTESIAN_POINT('Ctrl Pts',(-0.0253141728361465,2.42148596013398,
6.96997527966138));
#49509=CARTESIAN_POINT('Ctrl Pts',(-0.0117501107282478,2.42206725093508,
6.96915443788295));
#49510=CARTESIAN_POINT('Ctrl Pts',(-0.00970096885915303,2.42213548411976,
6.96902988130061));
#49511=CARTESIAN_POINT('Ctrl Pts',(-0.00698920707422366,2.42219988406561,
6.96886427509015));
#49512=CARTESIAN_POINT('Ctrl Pts',(-0.00632701975015583,2.42221356755757,
6.96882377469974));
#49513=CARTESIAN_POINT('Ctrl Pts',(-0.00524104965174637,2.42223265918029,
6.96875725365457));
#49514=CARTESIAN_POINT('Ctrl Pts',(-0.00481728781338862,2.42223927286918,
6.96873127081524));
#49515=CARTESIAN_POINT('Ctrl Pts',(-0.00399701985856119,2.42225045647054,
6.96868092680914));
#49516=CARTESIAN_POINT('Ctrl Pts',(-0.00360051573593683,2.42225513052149,
6.96865656895111));
#49517=CARTESIAN_POINT('Ctrl Pts',(-0.00268628056280024,2.42226422014744,
6.96860035401023));
#49518=CARTESIAN_POINT('Ctrl Pts',(-0.00216854650016921,2.42226811988093,
6.96856848082419));
#49519=CARTESIAN_POINT('Ctrl Pts',(-0.000515452643909905,2.42227658772934,
6.96846658740692));
#49520=CARTESIAN_POINT('Ctrl Pts',(0.000619913366854447,2.42227640364203,
6.96839641854809));
#49521=CARTESIAN_POINT('Ctrl Pts',(0.0108824700208385,2.42222050867727,
6.96776043564784));
#49522=CARTESIAN_POINT('Ctrl Pts',(0.0200026256392138,2.42178308238356,
6.96718271374627));
#49523=CARTESIAN_POINT('Ctrl Pts',(0.0596250680880687,2.41819176736287,
6.96461456766074));
#49524=CARTESIAN_POINT('Ctrl Pts',(0.0896057403424972,2.4110809580207,6.96250024377681));
#49525=CARTESIAN_POINT('Ctrl Pts',(0.125298904738283,2.39701996736983,6.95994595440756));
#49526=CARTESIAN_POINT('Ctrl Pts',(0.132372546605577,2.39393571427577,6.95943902950059));
#49527=CARTESIAN_POINT('Ctrl Pts',(0.141312269856743,2.38964953762658,6.95880326612892));
#49528=CARTESIAN_POINT('Ctrl Pts',(0.143285631997231,2.3886784379294,6.95866324562129));
#49529=CARTESIAN_POINT('Ctrl Pts',(0.146044286349171,2.38728563458223,6.95846811341724));
#49530=CARTESIAN_POINT('Ctrl Pts',(0.146837956253646,2.38688078370494,6.95841204504113));
#49531=CARTESIAN_POINT('Ctrl Pts',(0.148037893508134,2.38626241165553,6.95832739632403));
#49532=CARTESIAN_POINT('Ctrl Pts',(0.148445392674245,2.38605130945526,6.95829867067977));
#49533=CARTESIAN_POINT('Ctrl Pts',(0.149194454012507,2.38566123154884,6.95824590825582));
#49534=CARTESIAN_POINT('Ctrl Pts',(0.149536147759728,2.38548251231025,6.9582218556822));
#49535=CARTESIAN_POINT('Ctrl Pts',(0.150087939196921,2.38519264125609,6.95818304023658));
#49536=CARTESIAN_POINT('Ctrl Pts',(0.150298234827975,2.38508187021884,6.95816825331665));
#49537=CARTESIAN_POINT('Ctrl Pts',(0.150694815817619,2.38487241451412,6.95814037974676));
#49538=CARTESIAN_POINT('Ctrl Pts',(0.15088112537651,2.38477378051843,6.95812729007382));
#49539=CARTESIAN_POINT('Ctrl Pts',(0.151316019368364,2.38454299703938,6.95809674700003));
#49540=CARTESIAN_POINT('Ctrl Pts',(0.15156452726259,2.38441070471899,6.95807930282999));
#49541=CARTESIAN_POINT('Ctrl Pts',(0.152325769628742,2.38400417889688,6.95802589296917));
#49542=CARTESIAN_POINT('Ctrl Pts',(0.152837939128523,2.38372888132738,6.95798999467129));
#49543=CARTESIAN_POINT('Ctrl Pts',(0.156627816565253,2.38167853454191,6.95772460772769));
#49544=CARTESIAN_POINT('Ctrl Pts',(0.159875421734633,2.37984803408106,6.95749857086763));
#49545=CARTESIAN_POINT('Ctrl Pts',(0.164132834958942,2.377350046031,6.95720310573676));
#49546=CARTESIAN_POINT('Ctrl Pts',(0.165171534876961,2.37673272248986,6.95713108838754));
#49547=CARTESIAN_POINT('Ctrl Pts',(0.190569902439562,2.3614439357857,6.95537118471046));
#49548=CARTESIAN_POINT('Ctrl Pts',(0.212887726553306,2.34361663975742,6.95383950088785));
#49549=CARTESIAN_POINT('Ctrl Pts',(0.243368060118813,2.31183989033175,6.95134275884058));
#49550=CARTESIAN_POINT('Ctrl Pts',(0.253326655899653,2.29982407804502,6.95043992887395));
#49551=CARTESIAN_POINT('Ctrl Pts',(0.263806903086126,2.28513012725054,6.94935131992476));
#49552=CARTESIAN_POINT('Ctrl Pts',(0.265214503632972,2.2831079263007,6.94920185564619));
#49553=CARTESIAN_POINT('Ctrl Pts',(0.266997025919563,2.28048342380292,6.94900824714265));
#49554=CARTESIAN_POINT('Ctrl Pts',(0.267393363670245,2.27989571192773,6.94896491573033));
#49555=CARTESIAN_POINT('Ctrl Pts',(0.268029330631227,2.27894591939361,6.9488949248741));
#49556=CARTESIAN_POINT('Ctrl Pts',(0.268270174264727,2.27858465147739,6.94886831124896));
#49557=CARTESIAN_POINT('Ctrl Pts',(0.268727803179391,2.27789518861216,6.94881753597199));
#49558=CARTESIAN_POINT('Ctrl Pts',(0.268944719300638,2.27756708110204,6.94879337929579));
#49559=CARTESIAN_POINT('Ctrl Pts',(0.269438315988197,2.27681748699173,6.94873820580667));
#49560=CARTESIAN_POINT('Ctrl Pts',(0.269714608703757,2.27639574732913,6.94870717454158));
#49561=CARTESIAN_POINT('Ctrl Pts',(0.270555703094034,2.27510528498643,6.94861225472244));
#49562=CARTESIAN_POINT('Ctrl Pts',(0.271117301563292,2.27423449159038,6.9485482468758));
#49563=CARTESIAN_POINT('Ctrl Pts',(0.275210790886447,2.26781956931179,6.9480770109686));
#49564=CARTESIAN_POINT('Ctrl Pts',(0.278576293876997,2.26217159275179,6.94766367350334));
#49565=CARTESIAN_POINT('Ctrl Pts',(0.282653724290684,2.25482696303102,6.94712756585211));
#49566=CARTESIAN_POINT('Ctrl Pts',(0.283527253119232,2.25322145039925,6.94701046102636));
#49567=CARTESIAN_POINT('Ctrl Pts',(0.285298737847155,2.24989850383514,6.94676826308245));
#49568=CARTESIAN_POINT('Ctrl Pts',(0.286194952593266,2.24818022855193,6.94664311911745));
#49569=CARTESIAN_POINT('Ctrl Pts',(0.298091782716582,2.22486034925084,6.94494602460441));
#49570=CARTESIAN_POINT('Ctrl Pts',(0.306635215845854,2.20209484628449,6.94329581408604));
#49571=CARTESIAN_POINT('Ctrl Pts',(0.316142480546548,2.16428602616906,6.94066684637796));
#49572=CARTESIAN_POINT('Ctrl Pts',(0.318753728565432,2.14974864251369,6.93968324102719));
#49573=CARTESIAN_POINT('Ctrl Pts',(0.320486526218191,2.13392515833847,6.93867441178746));
#49574=CARTESIAN_POINT('Ctrl Pts',(0.320606940511019,2.13276766160089,6.93860097298848));
#49575=CARTESIAN_POINT('Ctrl Pts',(0.320775798152535,2.13105437365884,6.93849282528215));
#49576=CARTESIAN_POINT('Ctrl Pts',(0.320829070886706,2.13049908340601,6.93845785974242));
#49577=CARTESIAN_POINT('Ctrl Pts',(0.320911428320434,2.12961652816779,6.93840242657818));
#49578=CARTESIAN_POINT('Ctrl Pts',(0.320941454527024,2.12928935533131,6.93838190737019));
#49579=CARTESIAN_POINT('Ctrl Pts',(0.320997415878419,2.12866916729754,6.9383430696867));
#49580=CARTESIAN_POINT('Ctrl Pts',(0.32102345023802,2.12837616170463,6.93832474569242));
#49581=CARTESIAN_POINT('Ctrl Pts',(0.321068071608576,2.12786604564961,6.93829288756417));
#49582=CARTESIAN_POINT('Ctrl Pts',(0.321086839633682,2.12764895154931,6.93827934317457));
#49583=CARTESIAN_POINT('Ctrl Pts',(0.321123004925041,2.12722561607012,6.93825295843833));
#49584=CARTESIAN_POINT('Ctrl Pts',(0.321140423656682,2.12701937742996,6.93824011688432));
#49585=CARTESIAN_POINT('Ctrl Pts',(0.321181417325203,2.1265283704418,6.93820957339484));
#49586=CARTESIAN_POINT('Ctrl Pts',(0.321204812283448,2.12624358665925,6.93819188165318));
#49587=CARTESIAN_POINT('Ctrl Pts',(0.321286379545042,2.12523422938029,6.93812925889149));
#49588=CARTESIAN_POINT('Ctrl Pts',(0.32134247968654,2.12450948360557,6.93808444370854));
#49589=CARTESIAN_POINT('Ctrl Pts',(0.322111366347603,2.11411966174511,6.93744404656483));
#49590=CARTESIAN_POINT('Ctrl Pts',(0.32239036438792,2.10442631684681,6.93687214513714));
#49591=CARTESIAN_POINT('Ctrl Pts',(0.321852418837991,2.07150810366417,6.93497269784012));
#49592=CARTESIAN_POINT('Ctrl Pts',(0.318962891790567,2.04839014403216,6.93370646204764));
#49593=CARTESIAN_POINT('Ctrl Pts',(0.309982060241883,2.01044081060017,6.93149636702036));
#49594=CARTESIAN_POINT('Ctrl Pts',(0.305231036311781,1.99538813201605,6.9305837977769));
#49595=CARTESIAN_POINT('Ctrl Pts',(0.298480471687236,1.97844040335145,6.9294835779352));
#49596=CARTESIAN_POINT('Ctrl Pts',(0.297536105993452,1.9761468909733,6.92933312352238));
#49597=CARTESIAN_POINT('Ctrl Pts',(0.296287271464342,1.97321067355542,6.92913840986515));
#49598=CARTESIAN_POINT('Ctrl Pts',(0.296007001659939,1.97255771703389,6.9290949749859));
#49599=CARTESIAN_POINT('Ctrl Pts',(0.295551847947904,1.97150692761235,6.929024857203));
#49600=CARTESIAN_POINT('Ctrl Pts',(0.295378313704991,1.97110850971881,6.92899822042185));
#49601=CARTESIAN_POINT('Ctrl Pts',(0.295046214880956,1.97035023583254,6.928947427445));
#49602=CARTESIAN_POINT('Ctrl Pts',(0.294887796349065,1.9699903164127,6.92892327628318));
#49603=CARTESIAN_POINT('Ctrl Pts',(0.294525050592844,1.96917024923822,6.92886815228869));
#49604=CARTESIAN_POINT('Ctrl Pts',(0.294320303394191,1.96871028937319,6.92883716509837));
#49605=CARTESIAN_POINT('Ctrl Pts',(0.293692340120795,1.9673084356217,6.92874251061871));
#49606=CARTESIAN_POINT('Ctrl Pts',(0.293265677318592,1.96636810122615,6.92867872501006));
#49607=CARTESIAN_POINT('Ctrl Pts',(0.290121850734225,1.95952690461709,6.92821250125667));
#49608=CARTESIAN_POINT('Ctrl Pts',(0.287231503819866,1.95370771684781,6.92780409887163));
#49609=CARTESIAN_POINT('Ctrl Pts',(0.283899414759614,1.94747911349576,6.92735345722573));
#49610=CARTESIAN_POINT('Ctrl Pts',(0.283630048128706,1.94697877822692,6.92731716159109));
#49611=CARTESIAN_POINT('Ctrl Pts',(0.271417985970904,1.92443850200028,6.92567768107543));
#49612=CARTESIAN_POINT('Ctrl Pts',(0.256947513233204,1.90386961286809,6.92398352181387));
#49613=CARTESIAN_POINT('Ctrl Pts',(0.228040005636204,1.87153956041951,6.92105111557454));
#49614=CARTESIAN_POINT('Ctrl Pts',(0.214693091686178,1.85895338038718,6.91982126999722));
#49615=CARTESIAN_POINT('Ctrl Pts',(0.199886318280011,1.84720169636082,6.91863315240455));
#49616=CARTESIAN_POINT('Ctrl Pts',(0.199423949828565,1.84683679018081,6.91859621737979));
#49617=CARTESIAN_POINT('Ctrl Pts',(0.198692118076695,1.84626246967197,6.91853802232602));
#49618=CARTESIAN_POINT('Ctrl Pts',(0.198423320908865,1.84605221441247,6.91851670391454));
#49619=CARTESIAN_POINT('Ctrl Pts',(0.197914904149887,1.84565582687712,6.91847648815419));
#49620=CARTESIAN_POINT('Ctrl Pts',(0.197675354960741,1.84546960549047,6.91845758452485));
#49621=CARTESIAN_POINT('Ctrl Pts',(0.197262134182775,1.84514931002756,6.91842505337062));
#49622=CARTESIAN_POINT('Ctrl Pts',(0.197088588311663,1.8450150747198,6.9184114143137));
#49623=CARTESIAN_POINT('Ctrl Pts',(0.196752807257615,1.84475590038029,6.91838507069755));
#49624=CARTESIAN_POINT('Ctrl Pts',(0.196590590281329,1.84463093889852,6.91837236450968));
#49625=CARTESIAN_POINT('Ctrl Pts',(0.196208491037982,1.84433717416897,6.91834248324089));
#49626=CARTESIAN_POINT('Ctrl Pts',(0.195988509435892,1.8441684995202,6.91832531733573));
#49627=CARTESIAN_POINT('Ctrl Pts',(0.195338983689398,1.84367179400804,6.91827474164998));
#49628=CARTESIAN_POINT('Ctrl Pts',(0.194908828971717,1.84334455755875,6.91824138773807));
#49629=CARTESIAN_POINT('Ctrl Pts',(0.191166823699058,1.84051269277339,6.91795243149008));
#49630=CARTESIAN_POINT('Ctrl Pts',(0.187807489204289,1.83807106295716,6.91770114147994));
#49631=CARTESIAN_POINT('Ctrl Pts',(0.183566128132596,1.83511192874879,6.91739255719391));
#49632=CARTESIAN_POINT('Ctrl Pts',(0.182727772609372,1.83453291191579,6.91733197590658));
#49633=CARTESIAN_POINT('Ctrl Pts',(0.181778311629421,1.833883788022,6.91726381478149));
#49634=CARTESIAN_POINT('Ctrl Pts',(0.181669902560216,1.83380976847332,6.91725603875078));
#49635=CARTESIAN_POINT('Ctrl Pts',(0.154562124296756,1.81532539184354,6.91531327142513));
#49636=CARTESIAN_POINT('Ctrl Pts',(0.124917153115547,1.80112648572427,6.91357604414492));
#49637=CARTESIAN_POINT('Ctrl Pts',(0.0826551035956213,1.78829325885977,
6.91103437492983));
#49638=CARTESIAN_POINT('Ctrl Pts',(0.0715014141846555,1.78554736039482,
6.91036013049811));
#49639=CARTESIAN_POINT('Ctrl Pts',(0.0582169252453551,1.78302027344488,
6.90954251553464));
#49640=CARTESIAN_POINT('Ctrl Pts',(0.0562044489489573,1.78265725618581,
6.90941827987079));
#49641=CARTESIAN_POINT('Ctrl Pts',(0.0535364302666989,1.78220216476578,
6.90925303725696));
#49642=CARTESIAN_POINT('Ctrl Pts',(0.0528838338990607,1.78209291680256,
6.90921257648701));
#49643=CARTESIAN_POINT('Ctrl Pts',(0.0518128402288578,1.78191701600195,
6.90914610393067));
#49644=CARTESIAN_POINT('Ctrl Pts',(0.0513946375285838,1.78184917672231,
6.90912012985185));
#49645=CARTESIAN_POINT('Ctrl Pts',(0.0505847061135226,1.78171943129307,
6.9090697910182));
#49646=CARTESIAN_POINT('Ctrl Pts',(0.0501929943173326,1.78165742316143,
6.90904542954759));
#49647=CARTESIAN_POINT('Ctrl Pts',(0.0492892917034664,1.78151607610713,
6.90898918926951));
#49648=CARTESIAN_POINT('Ctrl Pts',(0.0487772230392013,1.78143724862688,
6.90895729431251));
#49649=CARTESIAN_POINT('Ctrl Pts',(0.0471405363606278,1.78118933704483,
6.90885526233408));
#49650=CARTESIAN_POINT('Ctrl Pts',(0.0460152219047196,1.78102497232196,
6.90878497611335));
#49651=CARTESIAN_POINT('Ctrl Pts',(0.0357923533436014,1.77958703118773,
6.90814521714678));
#49652=CARTESIAN_POINT('Ctrl Pts',(0.0266459279117729,1.77869713677329,
6.90756367982536));
#49653=CARTESIAN_POINT('Ctrl Pts',(0.00364717829017836,1.77744824073949,
6.90607653057318));
#49654=CARTESIAN_POINT('Ctrl Pts',(-0.010212887235651,1.77758945001044,
6.90515729329815));
#49655=CARTESIAN_POINT('Ctrl Pts',(-0.0265538545387822,1.77881076178086,
6.90405449597907));
#49656=CARTESIAN_POINT('Ctrl Pts',(-0.0290857581000178,1.77903013784536,
6.90388311388462));
#49657=CARTESIAN_POINT('Ctrl Pts',(-0.0473557742994512,1.78083109058061,
6.90264333602232));
#49658=CARTESIAN_POINT('Ctrl Pts',(-0.0629615621932782,1.78353952297314,
6.90156639038665));
#49659=CARTESIAN_POINT('Ctrl Pts',(-0.0844770125753363,1.78892881189273,
6.90009845058249));
#49660=CARTESIAN_POINT('Ctrl Pts',(-0.0906016051843381,1.79065713166265,
6.8996827449379));
#49661=CARTESIAN_POINT('Ctrl Pts',(-0.0995682394324341,1.79347665235741,
6.89908117617267));
#49662=CARTESIAN_POINT('Ctrl Pts',(-0.102452177267187,1.79442848631939,
6.89888879313964));
#49663=CARTESIAN_POINT('Ctrl Pts',(-0.105801639720041,1.79558671868842,
6.89866699574018));
#49664=CARTESIAN_POINT('Ctrl Pts',(-0.106280535921204,1.79575358588968,
6.89863532320484));
#49665=CARTESIAN_POINT('Ctrl Pts',(-0.107010300769191,1.79600979938799,
6.89858712139764));
#49666=CARTESIAN_POINT('Ctrl Pts',(-0.107261453077407,1.79609832638862,
6.89857054377367));
#49667=CARTESIAN_POINT('Ctrl Pts',(-0.107697985044939,1.79625280518676,
6.89854174990624));
#49668=CARTESIAN_POINT('Ctrl Pts',(-0.107883413551028,1.79631861528745,
6.89852952524031));
#49669=CARTESIAN_POINT('Ctrl Pts',(-0.108272567874009,1.79645713076986,
6.89850388288329));
#49670=CARTESIAN_POINT('Ctrl Pts',(-0.108476280120566,1.7965298712124,6.89849046736948));
#49671=CARTESIAN_POINT('Ctrl Pts',(-0.109045926371561,1.79673392422367,
6.89845297404889));
#49672=CARTESIAN_POINT('Ctrl Pts',(-0.109411697792418,1.79686569450991,
6.89842892357794));
#49673=CARTESIAN_POINT('Ctrl Pts',(-0.11089131205112,1.79740175706444,6.8983317290609));
#49674=CARTESIAN_POINT('Ctrl Pts',(-0.112003177681355,1.79781153561437,
6.89825890785515));
#49675=CARTESIAN_POINT('Ctrl Pts',(-0.133033896288026,1.80569443604825,
6.89688516202767));
#49676=CARTESIAN_POINT('Ctrl Pts',(-0.15217022967051,1.81511702769419,6.89569552689938));
#49677=CARTESIAN_POINT('Ctrl Pts',(-0.177466088700415,1.83085434710069,
6.89402990459643));
#49678=CARTESIAN_POINT('Ctrl Pts',(-0.184510869422828,1.83563409586334,
6.89355506812021));
#49679=CARTESIAN_POINT('Ctrl Pts',(-0.199152301628688,1.84643863259523,
6.89253001432184));
#49680=CARTESIAN_POINT('Ctrl Pts',(-0.206682798440024,1.85253846872658,
6.89197893038096));
#49681=CARTESIAN_POINT('Ctrl Pts',(-0.220306927764705,1.86463049405708,
6.89092121995001));
#49682=CARTESIAN_POINT('Ctrl Pts',(-0.226459214838741,1.87054379084444,
6.89041759134046));
#49683=CARTESIAN_POINT('Ctrl Pts',(-0.233524292252185,1.87789561282,6.88980282404033));
#49684=CARTESIAN_POINT('Ctrl Pts',(-0.234669875517236,1.87910635309918,
6.8897019350941));
#49685=CARTESIAN_POINT('Ctrl Pts',(-0.236652622161543,1.88123470401018,
6.88952516406352));
#49686=CARTESIAN_POINT('Ctrl Pts',(-0.23749397519268,1.88214837621656,6.88944946219417));
#49687=CARTESIAN_POINT('Ctrl Pts',(-0.238695527869264,1.88346844236531,
6.88934034107425));
#49688=CARTESIAN_POINT('Ctrl Pts',(-0.239060021999111,1.8838709266374,6.88930710375749));
#49689=CARTESIAN_POINT('Ctrl Pts',(-0.239690743247952,1.88457093366397,
6.88924935376238));
#49690=CARTESIAN_POINT('Ctrl Pts',(-0.239957438701744,1.88486803438226,
6.88922486087993));
#49691=CARTESIAN_POINT('Ctrl Pts',(-0.240469132796051,1.88544020068298,
6.88917772522342));
#49692=CARTESIAN_POINT('Ctrl Pts',(-0.240714213426203,1.88571519241089,
6.88915508594329));
#49693=CARTESIAN_POINT('Ctrl Pts',(-0.241290417501792,1.88636395576756,
6.88910170962166));
#49694=CARTESIAN_POINT('Ctrl Pts',(-0.241621144049332,1.8867380771978,6.88907095605185));
#49695=CARTESIAN_POINT('Ctrl Pts',(-0.242595339857808,1.88784527307461,
6.8889800203446));
#49696=CARTESIAN_POINT('Ctrl Pts',(-0.24323634765787,1.88858049706319,6.88891973597902));
#49697=CARTESIAN_POINT('Ctrl Pts',(-0.248896934846785,1.89513290339866,
6.8883833424007));
#49698=CARTESIAN_POINT('Ctrl Pts',(-0.253709947105928,1.90112451670273,
6.88789880889892));
#49699=CARTESIAN_POINT('Ctrl Pts',(-0.260527534124088,1.91026227071752,
6.8871675209828));
#49700=CARTESIAN_POINT('Ctrl Pts',(-0.262699276584188,1.91328071790586,
6.88692715164194));
#49701=CARTESIAN_POINT('Ctrl Pts',(-0.281289752809788,1.94008562529847,
6.88480315419676));
#49702=CARTESIAN_POINT('Ctrl Pts',(-0.294490548636968,1.9659424422099,6.88280943712105));
#49703=CARTESIAN_POINT('Ctrl Pts',(-0.307179345549023,2.00206989929026,
6.88026384908122));
#49704=CARTESIAN_POINT('Ctrl Pts',(-0.309904056222915,2.01106762273589,
6.87964961110476));
#49705=CARTESIAN_POINT('Ctrl Pts',(-0.312461565013822,2.02107087994329,
6.87899732298811));
#49706=CARTESIAN_POINT('Ctrl Pts',(-0.312687394113057,2.02197033118506,
6.87893894090026));
#49707=CARTESIAN_POINT('Ctrl Pts',(-0.313073645753839,2.02353733407688,
6.87883771157851));
#49708=CARTESIAN_POINT('Ctrl Pts',(-0.313235822130052,2.02420444141819,
6.87879476785278));
#49709=CARTESIAN_POINT('Ctrl Pts',(-0.313466119452912,2.02516512579215,
6.87873314904285));
#49710=CARTESIAN_POINT('Ctrl Pts',(-0.313535960878004,2.02545828227995,
6.87871437571435));
#49711=CARTESIAN_POINT('Ctrl Pts',(-0.313656541818026,2.02596758350624,
6.87868181318834));
#49712=CARTESIAN_POINT('Ctrl Pts',(-0.313707469283368,2.02618368314408,
6.87866801308739));
#49713=CARTESIAN_POINT('Ctrl Pts',(-0.313805570426962,2.02660188922292,
6.87864133836506));
#49714=CARTESIAN_POINT('Ctrl Pts',(-0.313852772069803,2.02680398807755,
6.87862846212074));
#49715=CARTESIAN_POINT('Ctrl Pts',(-0.31396498253148,2.02728653326359,6.878597751885));
#49716=CARTESIAN_POINT('Ctrl Pts',(-0.31402981099746,2.02756702196365,6.87857992834657));
#49717=CARTESIAN_POINT('Ctrl Pts',(-0.314259826703629,2.02856832770421,
6.87851639724098));
#49718=CARTESIAN_POINT('Ctrl Pts',(-0.314422910300101,2.02928963307569,
6.87847080995378));
#49719=CARTESIAN_POINT('Ctrl Pts',(-0.316881278798396,2.04033948004058,
6.87777508543917));
#49720=CARTESIAN_POINT('Ctrl Pts',(-0.318669321288063,2.05077562108578,
6.87715319211522));
#49721=CARTESIAN_POINT('Ctrl Pts',(-0.321483557307957,2.07403065497136,
6.87580740051804));
#49722=CARTESIAN_POINT('Ctrl Pts',(-0.322263057020988,2.08686078247903,
6.87509105270776));
#49723=CARTESIAN_POINT('Ctrl Pts',(-0.32229897683579,2.1259328765377,6.87290714437496));
#49724=CARTESIAN_POINT('Ctrl Pts',(-0.319121269284702,2.15206247705772,
6.87143427884424));
#49725=CARTESIAN_POINT('Ctrl Pts',(-0.312412576650348,2.17913492690807,
6.86974437954497));
#49726=CARTESIAN_POINT('Ctrl Pts',(-0.311999056071249,2.18074988268878,
6.86964297814424));
#49727=CARTESIAN_POINT('Ctrl Pts',(-0.311411575133442,2.18297231841413,
6.86950258942168));
#49728=CARTESIAN_POINT('Ctrl Pts',(-0.311248325083948,2.18358262303603,
6.86946394908589));
#49729=CARTESIAN_POINT('Ctrl Pts',(-0.310985212132392,2.18455480106472,
6.86940225547506));
#49730=CARTESIAN_POINT('Ctrl Pts',(-0.310886509077829,2.18491698899272,
6.86937923987444));
#49731=CARTESIAN_POINT('Ctrl Pts',(-0.310682617946147,2.1856600411719,6.86933195692072));
#49732=CARTESIAN_POINT('Ctrl Pts',(-0.310577361835775,2.18604088598107,
6.86930768738985));
#49733=CARTESIAN_POINT('Ctrl Pts',(-0.310332637111067,2.18692006533615,
6.86925157974321));
#49734=CARTESIAN_POINT('Ctrl Pts',(-0.310192668355467,2.18741825843543,
6.86921972540395));
#49735=CARTESIAN_POINT('Ctrl Pts',(-0.30975026040475,2.18897848726297,6.86911977358952));
#49736=CARTESIAN_POINT('Ctrl Pts',(-0.309443564630033,2.19003929851373,
6.86905153759129));
#49737=CARTESIAN_POINT('Ctrl Pts',(-0.304922044419433,2.20538251446122,
6.86806050901316));
#49738=CARTESIAN_POINT('Ctrl Pts',(-0.299728364704512,2.21935543494935,
6.86710530776711));
#49739=CARTESIAN_POINT('Ctrl Pts',(-0.286623742590941,2.24830088184217,
6.865010509881));
#49740=CARTESIAN_POINT('Ctrl Pts',(-0.278461422492394,2.26311184977095,
6.86386619262422));
#49741=CARTESIAN_POINT('Ctrl Pts',(-0.264277391184683,2.28465653957756,
6.86212181823417));
#49742=CARTESIAN_POINT('Ctrl Pts',(-0.259070742834407,2.29189304234128,
6.86152105719952));
#49743=CARTESIAN_POINT('Ctrl Pts',(-0.247524583768418,2.30661249131161,
6.86027935079376));
#49744=CARTESIAN_POINT('Ctrl Pts',(-0.241129453047439,2.31404151835647,
6.85964095243054));
#49745=CARTESIAN_POINT('Ctrl Pts',(-0.233905121393545,2.3216982194773,6.85898023644451));
#49746=CARTESIAN_POINT('Ctrl Pts',(-0.233403373055781,2.32222639763064,
6.85893464449148));
#49747=CARTESIAN_POINT('Ctrl Pts',(-0.232702142086055,2.32295957144292,
6.85887134358677));
#49748=CARTESIAN_POINT('Ctrl Pts',(-0.232504175859916,2.32316600466628,
6.85885351897409));
#49749=CARTESIAN_POINT('Ctrl Pts',(-0.232162429756917,2.32352141888784,
6.85882282828141));
#49750=CARTESIAN_POINT('Ctrl Pts',(-0.232018781097537,2.323670524904,6.85880995201896));
#49751=CARTESIAN_POINT('Ctrl Pts',(-0.231720573372341,2.32397946543423,
6.85878327182027));
#49752=CARTESIAN_POINT('Ctrl Pts',(-0.231565992828797,2.32413927818585,
6.85876946970545));
#49753=CARTESIAN_POINT('Ctrl Pts',(-0.231200200171516,2.32451666979619,
6.85873687470835));
#49754=CARTESIAN_POINT('Ctrl Pts',(-0.230988845431208,2.32473411148262,
6.85871809299356));
#49755=CARTESIAN_POINT('Ctrl Pts',(-0.230290663800027,2.32545037505574,
6.85865621896251));
#49756=CARTESIAN_POINT('Ctrl Pts',(-0.229802521242896,2.32594792032229,
6.85861322893988));
#49757=CARTESIAN_POINT('Ctrl Pts',(-0.228648662338361,2.32711639778117,
6.85851223275554));
#49758=CARTESIAN_POINT('Ctrl Pts',(-0.227981596976511,2.32778599698203,
6.85845432939142));
#49759=CARTESIAN_POINT('Ctrl Pts',(-0.220425463057356,2.3353043895243,6.85780373342245));
#49760=CARTESIAN_POINT('Ctrl Pts',(-0.213232313120236,2.34184201700761,
6.85723377035717));
#49761=CARTESIAN_POINT('Ctrl Pts',(-0.183443347434048,2.36655202265659,
6.85501013840131));
#49762=CARTESIAN_POINT('Ctrl Pts',(-0.15873783914129,2.38196439317632,6.85344755253178));
#49763=CARTESIAN_POINT('Ctrl Pts',(-0.130108501637404,2.39485376929827,
6.85162830829598));
#49764=CARTESIAN_POINT('Ctrl Pts',(-0.127903065425039,2.39581712753053,
6.85148821155526));
#49765=CARTESIAN_POINT('Ctrl Pts',(-0.123915760194919,2.39750589979528,
6.85123483952028));
#49766=CARTESIAN_POINT('Ctrl Pts',(-0.12213778270846,2.3982402351489,6.85112182866806));
#49767=CARTESIAN_POINT('Ctrl Pts',(-0.114141343490906,2.4014594044659,6.85061323526348));
#49768=CARTESIAN_POINT('Ctrl Pts',(-0.107853266991351,2.40376583374826,
6.85021236641828));
#49769=CARTESIAN_POINT('Ctrl Pts',(-0.100509445077585,2.4062027309649,6.8497414701628));
#49770=CARTESIAN_POINT('Ctrl Pts',(-0.0995190729652453,2.40652604306379,
6.84967791088624));
#49771=CARTESIAN_POINT('Ctrl Pts',(-0.0980460503357955,2.4069990276365,
6.84958328859491));
#49772=CARTESIAN_POINT('Ctrl Pts',(-0.09756458057457,2.40715237841976,6.84955234661465));
#49773=CARTESIAN_POINT('Ctrl Pts',(-0.0967075634716787,2.40742312471526,
6.84949724437207));
#49774=CARTESIAN_POINT('Ctrl Pts',(-0.0963321572107734,2.40754096625859,
6.8494730988111));
#49775=CARTESIAN_POINT('Ctrl Pts',(-0.0955426029602389,2.4077872230194,
6.84942229725377));
#49776=CARTESIAN_POINT('Ctrl Pts',(-0.0951284100125031,2.40791549041901,
6.84939563646569));
#49777=CARTESIAN_POINT('Ctrl Pts',(-0.0940389174119513,2.40825047672355,
6.84932547905196));
#49778=CARTESIAN_POINT('Ctrl Pts',(-0.0933631976591074,2.40845581158163,
6.84928193720288));
#49779=CARTESIAN_POINT('Ctrl Pts',(-0.0903512998932886,2.40936025070143,
6.84908772309549));
#49780=CARTESIAN_POINT('Ctrl Pts',(-0.0880079557402935,2.41003503238706,
6.84893625892184));
#49781=CARTESIAN_POINT('Ctrl Pts',(-0.0708900370722528,2.41475454659498,
6.84782696330667));
#49782=CARTESIAN_POINT('Ctrl Pts',(-0.0558535904380975,2.41776733076539,
6.84683565476908));
#49783=CARTESIAN_POINT('Ctrl Pts',(-0.0084360295732362,2.42379825147446,
6.84366292540376));
#49784=CARTESIAN_POINT('Ctrl Pts',(0.0242217874111559,2.42300106358828,
6.84139332157182));
#49785=CARTESIAN_POINT('Ctrl Pts',(0.0576635840449153,2.41707770709369,
6.83924570235275));
#49786=CARTESIAN_POINT('Ctrl Pts',(0.0591175564900687,2.41680984197825,
6.83915273031766));
#49787=CARTESIAN_POINT('Ctrl Pts',(0.0609862200646404,2.4164522656853,6.83903380395928));
#49788=CARTESIAN_POINT('Ctrl Pts',(0.0614026183801611,2.4163717338134,6.83900733935989));
#49789=CARTESIAN_POINT('Ctrl Pts',(0.0620624551829938,2.41624276890923,
6.83896546123088));
#49790=CARTESIAN_POINT('Ctrl Pts',(0.0623059969285247,2.41619487658477,
6.83895001689938));
#49791=CARTESIAN_POINT('Ctrl Pts',(0.0627424798570227,2.41610851863211,
6.83892236004706));
#49792=CARTESIAN_POINT('Ctrl Pts',(0.0629354397345218,2.41607015796517,
6.83891014160984));
#49793=CARTESIAN_POINT('Ctrl Pts',(0.0633892619933564,2.41597950546135,
6.83888142395937));
#49794=CARTESIAN_POINT('Ctrl Pts',(0.0636500944522861,2.41592706735115,
6.8388649332625));
#49795=CARTESIAN_POINT('Ctrl Pts',(0.0644067798867987,2.41577396715256,
6.83881713483455));
#49796=CARTESIAN_POINT('Ctrl Pts',(0.0649024639811346,2.4156724596858,6.83878587542501));
#49797=CARTESIAN_POINT('Ctrl Pts',(0.068345772989074,2.41495887674165,6.83856907837135));
#49798=CARTESIAN_POINT('Ctrl Pts',(0.0712850587277251,2.41430666665237,
6.83838579366968));
#49799=CARTESIAN_POINT('Ctrl Pts',(0.0804151148176153,2.412146088264,6.83782080679787));
#49800=CARTESIAN_POINT('Ctrl Pts',(0.0865708906523456,2.41049519025302,
6.83744611603596));
#49801=CARTESIAN_POINT('Ctrl Pts',(0.107791226756848,2.40412391628117,6.83616360107376));
#49802=CARTESIAN_POINT('Ctrl Pts',(0.122555507493681,2.39848034728892,6.83528671044205));
#49803=CARTESIAN_POINT('Ctrl Pts',(0.159571907990576,2.38111914319243,6.83300050531444));
#49804=CARTESIAN_POINT('Ctrl Pts',(0.180969608144942,2.367844939343,6.83158375222105));
#49805=CARTESIAN_POINT('Ctrl Pts',(0.201777977571167,2.35129475219088,6.82997103345412));
#49806=CARTESIAN_POINT('Ctrl Pts',(0.202939975357017,2.35035728668555,6.82988015308394));
#49807=CARTESIAN_POINT('Ctrl Pts',(0.20451556422199,2.34906797137611,6.82975578208097));
#49808=CARTESIAN_POINT('Ctrl Pts',(0.204934854792214,2.34872309032347,6.82972257337272));
#49809=CARTESIAN_POINT('Ctrl Pts',(0.205646093080466,2.34813505271073,6.82966605093025));
#49810=CARTESIAN_POINT('Ctrl Pts',(0.205938486916981,2.34789243551863,6.82964275914944));
#49811=CARTESIAN_POINT('Ctrl Pts',(0.206526704280569,2.3474025963376,6.82959579084211));
#49812=CARTESIAN_POINT('Ctrl Pts',(0.206822514587469,2.34715535946705,6.82957211372939));
#49813=CARTESIAN_POINT('Ctrl Pts',(0.207493628714051,2.34659239689058,6.82951826641001));
#49814=CARTESIAN_POINT('Ctrl Pts',(0.207868656210486,2.34627634462565,6.82948808285596));
#49815=CARTESIAN_POINT('Ctrl Pts',(0.208651132964943,2.345613856227,6.82942491089571));
#49816=CARTESIAN_POINT('Ctrl Pts',(0.209058443910769,2.34526725970321,6.82939191593651));
#49817=CARTESIAN_POINT('Ctrl Pts',(0.210123416734037,2.34435645319552,6.82930535228262));
#49818=CARTESIAN_POINT('Ctrl Pts',(0.210779665852636,2.34379060465451,6.82925171592332));
#49819=CARTESIAN_POINT('Ctrl Pts',(0.212720980003528,2.34210301523256,6.82909216584899));
#49820=CARTESIAN_POINT('Ctrl Pts',(0.213999414412069,2.34097372423042,6.82898593850427));
#49821=CARTESIAN_POINT('Ctrl Pts',(0.22793187112628,2.32846832941638,6.82781535843901));
#49822=CARTESIAN_POINT('Ctrl Pts',(0.239672819686541,2.3161191580839,6.82670883251865));
#49823=CARTESIAN_POINT('Ctrl Pts',(0.267889521755142,2.28129964699207,6.82371882625848));
#49824=CARTESIAN_POINT('Ctrl Pts',(0.282526080774365,2.2575225591566,6.82179283285765));
#49825=CARTESIAN_POINT('Ctrl Pts',(0.295558266089832,2.22853898313847,6.81974494487966));
#49826=CARTESIAN_POINT('Ctrl Pts',(0.297120437427373,2.22488557991926,6.81949206996655));
#49827=CARTESIAN_POINT('Ctrl Pts',(0.298837551465325,2.220655063975,6.81920601798216));
#49828=CARTESIAN_POINT('Ctrl Pts',(0.299058855293361,2.22010548577184,6.8191689875341));
#49829=CARTESIAN_POINT('Ctrl Pts',(0.299382760412788,2.21929466526526,6.81911454938806));
#49830=CARTESIAN_POINT('Ctrl Pts',(0.299486536384487,2.21903389819288,6.81909707121797));
#49831=CARTESIAN_POINT('Ctrl Pts',(0.299670905680956,2.21856884978255,6.81906595409309));
#49832=CARTESIAN_POINT('Ctrl Pts',(0.299751630875945,2.2183646215672,6.81905230713962));
#49833=CARTESIAN_POINT('Ctrl Pts',(0.299921294321935,2.21793410005134,6.81902357743977));
#49834=CARTESIAN_POINT('Ctrl Pts',(0.30001018501429,2.21770778917002,6.81900849761224));
#49835=CARTESIAN_POINT('Ctrl Pts',(0.300245173059328,2.21710752692598,6.81896855906664));
#49836=CARTESIAN_POINT('Ctrl Pts',(0.300390828484742,2.21673340128064,6.81894372707333));
#49837=CARTESIAN_POINT('Ctrl Pts',(0.301054724659993,2.21501866881518,6.81883018714444));
#49838=CARTESIAN_POINT('Ctrl Pts',(0.301564703095411,2.21367484965571,6.81874196955917));
#49839=CARTESIAN_POINT('Ctrl Pts',(0.305483327820432,2.2031370859973,6.81805581328721));
#49840=CARTESIAN_POINT('Ctrl Pts',(0.308480122244055,2.19379433520338,6.81748074788653));
#49841=CARTESIAN_POINT('Ctrl Pts',(0.319061978375157,2.15476307504405,6.81515837965903));
#49842=CARTESIAN_POINT('Ctrl Pts',(0.322821624500453,2.12420609338202,6.81351150595117));
#49843=CARTESIAN_POINT('Ctrl Pts',(0.322172002217396,2.09162150838969,6.81160982536418));
#49844=CARTESIAN_POINT('Ctrl Pts',(0.322115245046206,2.08966719658889,6.81149528676064));
#49845=CARTESIAN_POINT('Ctrl Pts',(0.322018291033916,2.08712593059078,6.81134565910995));
#49846=CARTESIAN_POINT('Ctrl Pts',(0.321994264107614,2.08653837679902,6.81131101653794));
#49847=CARTESIAN_POINT('Ctrl Pts',(0.321893102422582,2.08422001642839,6.81117413068363));
#49848=CARTESIAN_POINT('Ctrl Pts',(0.321803620214547,2.08248979946459,6.81107154488311));
#49849=CARTESIAN_POINT('Ctrl Pts',(0.321393227526319,2.07562772936836,6.81066288040297));
#49850=CARTESIAN_POINT('Ctrl Pts',(0.320963484599196,2.07050336874538,6.81035367325783));
#49851=CARTESIAN_POINT('Ctrl Pts',(0.320318493414498,2.06453189781462,6.80998792087809));
#49852=CARTESIAN_POINT('Ctrl Pts',(0.320222165529317,2.06367248732965,6.80993515068211));
#49853=CARTESIAN_POINT('Ctrl Pts',(0.320062742517292,2.06230008474536,6.80985066774492));
#49854=CARTESIAN_POINT('Ctrl Pts',(0.320001869904903,2.06178683459401,6.80981902510063));
#49855=CARTESIAN_POINT('Ctrl Pts',(0.319893131738617,2.06088848657177,6.80976355611619));
#49856=CARTESIAN_POINT('Ctrl Pts',(0.319845804671344,2.06050332357986,6.80973974681107));
#49857=CARTESIAN_POINT('Ctrl Pts',(0.319750186911184,2.05973659828906,6.80969229622416));
#49858=CARTESIAN_POINT('Ctrl Pts',(0.319701908613051,2.05935503506945,6.80966865537079));
#49859=CARTESIAN_POINT('Ctrl Pts',(0.319599651449307,2.05855830973338,6.80961923534234));
#49860=CARTESIAN_POINT('Ctrl Pts',(0.319545546428318,2.05814316478924,6.80959345221928));
#49861=CARTESIAN_POINT('Ctrl Pts',(0.31941341308455,2.05714450152621,6.80953135109108));
#49862=CARTESIAN_POINT('Ctrl Pts',(0.319334594700967,2.05656109085662,6.8094950081545));
#49863=CARTESIAN_POINT('Ctrl Pts',(0.319118104673788,2.05499107602903,6.80939703194188));
#49864=CARTESIAN_POINT('Ctrl Pts',(0.318977457243133,2.05400489479819,6.80933530467881));
#49865=CARTESIAN_POINT('Ctrl Pts',(0.318531696418294,2.05097975477293,6.80914537860551));
#49866=CARTESIAN_POINT('Ctrl Pts',(0.318211592553417,2.04894308948167,6.80901670702187));
#49867=CARTESIAN_POINT('Ctrl Pts',(0.316965477796275,2.04148212658251,6.8085423195098));
#49868=CARTESIAN_POINT('Ctrl Pts',(0.3159201674228,2.03607897456854,6.80819287481917));
#49869=CARTESIAN_POINT('Ctrl Pts',(0.313334566034227,2.02433512054876,6.80742009749783));
#49870=CARTESIAN_POINT('Ctrl Pts',(0.311739024109159,2.01800917022823,6.80699524967654));
#49871=CARTESIAN_POINT('Ctrl Pts',(0.305364395151487,1.99562359446648,6.80546207902814));
#49872=CARTESIAN_POINT('Ctrl Pts',(0.299526940903849,1.97989431047808,6.80432762766083));
#49873=CARTESIAN_POINT('Ctrl Pts',(0.284669060012023,1.94777630409352,6.80193392169563));
#49874=CARTESIAN_POINT('Ctrl Pts',(0.275390438610115,1.93156956110162,6.80067945065099));
#49875=CARTESIAN_POINT('Ctrl Pts',(0.264145249917297,1.91536622449466,6.7994369097627));
#49876=CARTESIAN_POINT('Ctrl Pts',(0.26352446078985,1.91448126036564,6.79936909254201));
#49877=CARTESIAN_POINT('Ctrl Pts',(0.262682575530885,1.91329386609797,6.79927817938233));
#49878=CARTESIAN_POINT('Ctrl Pts',(0.262465396915214,1.91298868657294,6.7992548203999));
#49879=CARTESIAN_POINT('Ctrl Pts',(0.262123621460219,1.91251019158715,6.79921820771644));
#49880=CARTESIAN_POINT('Ctrl Pts',(0.261999384522274,1.91233662132237,6.79920492927662));
#49881=CARTESIAN_POINT('Ctrl Pts',(0.26175991707467,1.91200276489418,6.79917939371607));
#49882=CARTESIAN_POINT('Ctrl Pts',(0.261644712601713,1.91184246238282,6.79916713499311));
#49883=CARTESIAN_POINT('Ctrl Pts',(0.261370387743824,1.91146148921364,6.79913800632488));
#49884=CARTESIAN_POINT('Ctrl Pts',(0.261211135329216,1.91124091433729,6.79912114567315));
#49885=CARTESIAN_POINT('Ctrl Pts',(0.260738077005979,1.91058744314044,6.79907120618498));
#49886=CARTESIAN_POINT('Ctrl Pts',(0.260423470946366,1.91015512309568,6.79903818257503));
#49887=CARTESIAN_POINT('Ctrl Pts',(0.257894764071611,1.9066983817606,6.79877423614928));
#49888=CARTESIAN_POINT('Ctrl Pts',(0.255629014007278,1.90371185691124,6.79854682997036));
#49889=CARTESIAN_POINT('Ctrl Pts',(0.246040120440922,1.89152031289622,6.79761804841922));
#49890=CARTESIAN_POINT('Ctrl Pts',(0.238267247308925,1.88267928084757,6.79694323285052));
#49891=CARTESIAN_POINT('Ctrl Pts',(0.22752539411124,1.87173231880931,6.79607665375847));
#49892=CARTESIAN_POINT('Ctrl Pts',(0.224980911478192,1.86922407116253,6.79587580155609));
#49893=CARTESIAN_POINT('Ctrl Pts',(0.207204920223891,1.85227469650503,6.79449852697421));
#49894=CARTESIAN_POINT('Ctrl Pts',(0.190637026185683,1.83931018601051,6.79333886599811));
#49895=CARTESIAN_POINT('Ctrl Pts',(0.172260752225997,1.82762520011724,6.79207606014041));
#49896=CARTESIAN_POINT('Ctrl Pts',(0.171593287026336,1.82720421153734,6.79203022820089));
#49897=CARTESIAN_POINT('Ctrl Pts',(0.16256510514686,1.82155613443301,6.79141073870724));
#49898=CARTESIAN_POINT('Ctrl Pts',(0.153971076620843,1.81671343587372,6.79082583959229));
#49899=CARTESIAN_POINT('Ctrl Pts',(0.144238471231809,1.81180297394246,6.79016297302303));
#49900=CARTESIAN_POINT('Ctrl Pts',(0.143305470210486,1.81133790588388,6.79009942632262));
#49901=CARTESIAN_POINT('Ctrl Pts',(0.141906994298655,1.81064926607465,6.79000416693733));
#49902=CARTESIAN_POINT('Ctrl Pts',(0.141443205558482,1.81042226976084,6.7899725737397));
#49903=CARTESIAN_POINT('Ctrl Pts',(0.140643664047032,1.81003332200704,6.78991810574866));
#49904=CARTESIAN_POINT('Ctrl Pts',(0.140308171142027,1.80987083619233,6.78989524959784));
#49905=CARTESIAN_POINT('Ctrl Pts',(0.139622471154554,1.80954020572264,6.78984853243412));
#49906=CARTESIAN_POINT('Ctrl Pts',(0.139272240515917,1.80937211151961,6.78982466971401));
#49907=CARTESIAN_POINT('Ctrl Pts',(0.138460753886303,1.80898443988319,6.78976937622959));
#49908=CARTESIAN_POINT('Ctrl Pts',(0.13799927896742,1.80876532555936,6.78973792947409));
#49909=CARTESIAN_POINT('Ctrl Pts',(0.137028056991712,1.80830700336677,6.78967174032411));
#49910=CARTESIAN_POINT('Ctrl Pts',(0.136518200538118,1.80806803257746,6.7896369898424));
#49911=CARTESIAN_POINT('Ctrl Pts',(0.135160752017659,1.80743612740108,6.78954445888791));
#49912=CARTESIAN_POINT('Ctrl Pts',(0.134312077867387,1.80704554254033,6.78948659752109));
#49913=CARTESIAN_POINT('Ctrl Pts',(0.131741608758437,1.80587605433886,6.78931130655577));
#49914=CARTESIAN_POINT('Ctrl Pts',(0.130014673004526,1.80510861075978,6.7891934851662));
#49915=CARTESIAN_POINT('Ctrl Pts',(0.123794281070761,1.80240955399807,6.78876884843833));
#49916=CARTESIAN_POINT('Ctrl Pts',(0.119263917830329,1.80056518024148,6.78845911112701));
#49917=CARTESIAN_POINT('Ctrl Pts',(0.103822662913714,1.79468484420899,6.78740141787451));
#49918=CARTESIAN_POINT('Ctrl Pts',(0.0927367257244031,1.79113701958502,
6.78663835755958));
#49919=CARTESIAN_POINT('Ctrl Pts',(0.0564731557588297,1.78166018872476,
6.78413870243388));
#49920=CARTESIAN_POINT('Ctrl Pts',(0.0307677559615217,1.77815724856511,
6.78235368600718));
#49921=CARTESIAN_POINT('Ctrl Pts',(-0.00104048037457064,1.77767154216208,
6.78027899071168));
#49922=CARTESIAN_POINT('Ctrl Pts',(-0.00700333927351832,1.77774593582544,
6.77989630499279));
#49923=CARTESIAN_POINT('Ctrl Pts',(-0.0135572761897419,1.77800973333096,
6.77948500394351));
#49924=CARTESIAN_POINT('Ctrl Pts',(-0.0141533403636898,1.77803538309729,
6.77944768216212));
#49925=CARTESIAN_POINT('Ctrl Pts',(-0.0150403895254106,1.77807602264171,
6.77939227074251));
#49926=CARTESIAN_POINT('Ctrl Pts',(-0.0153314267565426,1.77808975183987,
6.7793741113149));
#49927=CARTESIAN_POINT('Ctrl Pts',(-0.0158306651621511,1.77811398116298,
6.77934299726925));
#49928=CARTESIAN_POINT('Ctrl Pts',(-0.0160388748045849,1.77812428861782,
6.77933003182086));
#49929=CARTESIAN_POINT('Ctrl Pts',(-0.0164682598830051,1.77814596306891,
6.77930331602088));
#49930=CARTESIAN_POINT('Ctrl Pts',(-0.0166894331312736,1.77815735600392,
6.77928956724223));
#49931=CARTESIAN_POINT('Ctrl Pts',(-0.0172082157112406,1.77818461540867,
6.779257346841));
#49932=CARTESIAN_POINT('Ctrl Pts',(-0.0175058159926783,1.77820066678786,
6.77923888567066));
#49933=CARTESIAN_POINT('Ctrl Pts',(-0.0184705385395573,1.77825404233466,
6.77917911103764));
#49934=CARTESIAN_POINT('Ctrl Pts',(-0.0191375726896217,1.77829302867626,
6.77913789050687));
#49935=CARTESIAN_POINT('Ctrl Pts',(-0.0206991607475864,1.77838917331149,
6.77904163515628));
#49936=CARTESIAN_POINT('Ctrl Pts',(-0.0215936121264193,1.77844799012012,
6.77898669057593));
#49937=CARTESIAN_POINT('Ctrl Pts',(-0.031322465876583,1.77912851226527,
6.77839100680657));
#49938=CARTESIAN_POINT('Ctrl Pts',(-0.0401287939413119,1.78011045691583,
6.7778692134471));
#49939=CARTESIAN_POINT('Ctrl Pts',(-0.0576488989979258,1.78279910574574,
6.77684634475258));
#49940=CARTESIAN_POINT('Ctrl Pts',(-0.0663546813269928,1.78450535033996,
6.77634571202855));
#49941=CARTESIAN_POINT('Ctrl Pts',(-0.0777661773666632,1.78723521934586,
6.7756875040365));
#49942=CARTESIAN_POINT('Ctrl Pts',(-0.0805439835741911,1.787939023216,6.77552713176508));
#49943=CARTESIAN_POINT('Ctrl Pts',(-0.0927683553202072,1.79121037332254,
6.77481945176136));
#49944=CARTESIAN_POINT('Ctrl Pts',(-0.102104358231319,1.79417047730929,
6.77427370759598));
#49945=CARTESIAN_POINT('Ctrl Pts',(-0.129126432464411,1.80411368146494,
6.77264892522838));
#49946=CARTESIAN_POINT('Ctrl Pts',(-0.146343650576667,1.81224016443036,
6.77155238611826));
#49947=CARTESIAN_POINT('Ctrl Pts',(-0.163857420050215,1.82248677966368,
6.77031991618886));
#49948=CARTESIAN_POINT('Ctrl Pts',(-0.164967534365567,1.8231452472928,6.77024127968918));
#49949=CARTESIAN_POINT('Ctrl Pts',(-0.166510958814107,1.82407331299188,
6.77013121538963));
#49950=CARTESIAN_POINT('Ctrl Pts',(-0.166947639720453,1.82433730467197,
6.77009999243773));
#49951=CARTESIAN_POINT('Ctrl Pts',(-0.167700871900095,1.82479511094921,
6.77004599243645));
#49952=CARTESIAN_POINT('Ctrl Pts',(-0.168017719628093,1.82498843791103,
6.77002323329284));
#49953=CARTESIAN_POINT('Ctrl Pts',(-0.168666242689812,1.82538567810225,
6.76997655935361));
#49954=CARTESIAN_POINT('Ctrl Pts',(-0.168997883813226,1.82558964582392,
6.76995264257946));
#49955=CARTESIAN_POINT('Ctrl Pts',(-0.169768424540372,1.82606547461862,
6.76989696010574));
#49956=CARTESIAN_POINT('Ctrl Pts',(-0.170207041186248,1.82633778979823,
6.76986517770135));
#49957=CARTESIAN_POINT('Ctrl Pts',(-0.171129068123141,1.82691330445432,
6.7697981846339));
#49958=CARTESIAN_POINT('Ctrl Pts',(-0.171612330832229,1.82721673595988,
6.76976296545157));
#49959=CARTESIAN_POINT('Ctrl Pts',(-0.172900036528971,1.82803003825541,
6.7696688352144));
#49960=CARTESIAN_POINT('Ctrl Pts',(-0.173703024868347,1.82854219141202,
6.76960983952191));
#49961=CARTESIAN_POINT('Ctrl Pts',(-0.176134603562278,1.83010828071922,
6.76943027710532));
#49962=CARTESIAN_POINT('Ctrl Pts',(-0.17775593615286,1.83117335398858,6.76930929578685));
#49963=CARTESIAN_POINT('Ctrl Pts',(-0.204482774166398,1.84907804195431,
6.76729383632073));
#49964=CARTESIAN_POINT('Ctrl Pts',(-0.227100796113425,1.86934998064091,
6.76525511184102));
#49965=CARTESIAN_POINT('Ctrl Pts',(-0.256122004173941,1.90382857844438,
6.76220928080569));
#49966=CARTESIAN_POINT('Ctrl Pts',(-0.264889324021546,1.91583854269372,
6.76121240058435));
#49967=CARTESIAN_POINT('Ctrl Pts',(-0.274577314951453,1.93124086312546,
6.76004482899131));
#49968=CARTESIAN_POINT('Ctrl Pts',(-0.276312938994576,1.93409789007875,
6.75983267062555));
#49969=CARTESIAN_POINT('Ctrl Pts',(-0.278284942628973,1.93746085066125,
6.75958851315101));
#49970=CARTESIAN_POINT('Ctrl Pts',(-0.278564768508545,1.93794089313306,
6.75955379192174));
#49971=CARTESIAN_POINT('Ctrl Pts',(-0.278983829012849,1.9386640855941,6.75950168304108));
#49972=CARTESIAN_POINT('Ctrl Pts',(-0.279123988519422,1.938906694235,6.75948423575871));
#49973=CARTESIAN_POINT('Ctrl Pts',(-0.279373125432313,1.93933923826284,
6.75945318950914));
#49974=CARTESIAN_POINT('Ctrl Pts',(-0.279482225574177,1.93952910181294,
6.75943958255324));
#49975=CARTESIAN_POINT('Ctrl Pts',(-0.279713497114305,1.93993252769301,
6.75941071421316));
#49976=CARTESIAN_POINT('Ctrl Pts',(-0.279835617139131,1.94014611815788,
6.75939545619856));
#49977=CARTESIAN_POINT('Ctrl Pts',(-0.280162768393026,1.94071983626291,
6.75935454156856));
#49978=CARTESIAN_POINT('Ctrl Pts',(-0.280367350679459,1.94108022139677,
6.75932891405313));
#49979=CARTESIAN_POINT('Ctrl Pts',(-0.281345051647101,1.94281026999613,
6.75920623397734));
#49980=CARTESIAN_POINT('Ctrl Pts',(-0.282108849152745,1.94418521645598,
6.75910977350736));
#49981=CARTESIAN_POINT('Ctrl Pts',(-0.288377918613924,1.9556676750672,6.75831235244484));
#49982=CARTESIAN_POINT('Ctrl Pts',(-0.293348821378168,1.96605906077359,
6.75764279027653));
#49983=CARTESIAN_POINT('Ctrl Pts',(-0.311735391401225,2.01045854564617,
6.75490404792567));
#49984=CARTESIAN_POINT('Ctrl Pts',(-0.319872695744452,2.04635092979291,
6.75294300284295));
#49985=CARTESIAN_POINT('Ctrl Pts',(-0.321932128880303,2.08498432471426,
6.75060575887161));
#49986=CARTESIAN_POINT('Ctrl Pts',(-0.322024838845627,2.08712487153331,
6.75047567308695));
#49987=CARTESIAN_POINT('Ctrl Pts',(-0.322119515216439,2.08996587295851,
6.7503021900407));
#49988=CARTESIAN_POINT('Ctrl Pts',(-0.322140553303645,2.0906656712187,6.75025939087309));
#49989=CARTESIAN_POINT('Ctrl Pts',(-0.322169733260274,2.09175439961882,
6.75019269949785));
#49990=CARTESIAN_POINT('Ctrl Pts',(-0.322179451600182,2.09214328827607,
6.75016885671481));
#49991=CARTESIAN_POINT('Ctrl Pts',(-0.32219744674238,2.09291966434493,6.7501212148784));
#49992=CARTESIAN_POINT('Ctrl Pts',(-0.322205728705603,2.09330715101484,
6.75009741602585));
#49993=CARTESIAN_POINT('Ctrl Pts',(-0.322220666759002,2.09407050910491,
6.7500504900366));
#49994=CARTESIAN_POINT('Ctrl Pts',(-0.322227364204921,2.09444637915127,
6.7500273642363));
#49995=CARTESIAN_POINT('Ctrl Pts',(-0.322240973981441,2.09529337486586,
6.74997520672424));
#49996=CARTESIAN_POINT('Ctrl Pts',(-0.322247510790505,2.09576450496247,
6.74994616328499));
#49997=CARTESIAN_POINT('Ctrl Pts',(-0.32226789559115,2.09750957541692,6.74983846825088));
#49998=CARTESIAN_POINT('Ctrl Pts',(-0.322275222346017,2.09878356433945,
6.74975961279031));
#49999=CARTESIAN_POINT('Ctrl Pts',(-0.322274994862272,2.1000575458305,6.74968051971722));
#50000=CARTESIAN_POINT('',(-0.322274936831736,2.09979822016873,6.49915140185063));
#50001=CARTESIAN_POINT('Ctrl Pts',(-0.322274994880076,2.10005744603766,
6.7496805259127));
#50002=CARTESIAN_POINT('Ctrl Pts',(-0.322274683587777,2.10180381058933,
6.74957210572105));
#50003=CARTESIAN_POINT('Ctrl Pts',(-0.32226017734277,2.10355012243384,6.74946324132778));
#50004=CARTESIAN_POINT('Ctrl Pts',(-0.321619076867645,2.14255589360676,
6.74702138683848));
#50005=CARTESIAN_POINT('Ctrl Pts',(-0.314547986542146,2.17942209619581,
6.74445563806546));
#50006=CARTESIAN_POINT('Ctrl Pts',(-0.297384809473874,2.22469255122695,
6.74122753131725));
#50007=CARTESIAN_POINT('Ctrl Pts',(-0.292883902559978,2.23492604703357,
6.74049609629811));
#50008=CARTESIAN_POINT('Ctrl Pts',(-0.287540268053849,2.24554131882432,
6.73975045817491));
#50009=CARTESIAN_POINT('Ctrl Pts',(-0.287218443693046,2.24617539759807,
6.73970597109837));
#50010=CARTESIAN_POINT('Ctrl Pts',(-0.286755253236832,2.24708056917944,
6.73964254404661));
#50011=CARTESIAN_POINT('Ctrl Pts',(-0.286615598852468,2.24735252826254,
6.73962349772094));
#50012=CARTESIAN_POINT('Ctrl Pts',(-0.28637351084408,2.24782231746359,6.73959061505136));
#50013=CARTESIAN_POINT('Ctrl Pts',(-0.286271258863422,2.24802024051934,
6.7395767671977));
#50014=CARTESIAN_POINT('Ctrl Pts',(-0.286073865934775,2.24840135263357,
6.73955011351327));
#50015=CARTESIAN_POINT('Ctrl Pts',(-0.285978754418912,2.2485845559133,6.73953730584442));
#50016=CARTESIAN_POINT('Ctrl Pts',(-0.285752536085183,2.24901927457349,
6.73950692628023));
#50017=CARTESIAN_POINT('Ctrl Pts',(-0.285621272855375,2.24927070900693,
6.73948936432509));
#50018=CARTESIAN_POINT('Ctrl Pts',(-0.285227222460133,2.25002308887097,
6.73943683911131));
#50019=CARTESIAN_POINT('Ctrl Pts',(-0.284963446344544,2.25052351937679,
6.73940193797667));
#50020=CARTESIAN_POINT('Ctrl Pts',(-0.282410092139383,2.25533692193904,
6.739066552762));
#50021=CARTESIAN_POINT('Ctrl Pts',(-0.280023936749332,2.25959831015863,
6.73877204756151));
#50022=CARTESIAN_POINT('Ctrl Pts',(-0.277142026443082,2.26448127893417,
6.73843548548519));
#50023=CARTESIAN_POINT('Ctrl Pts',(-0.276739874174369,2.26515700410437,
6.73838893106606));
#50024=CARTESIAN_POINT('Ctrl Pts',(-0.275946688624445,2.26647874001302,
6.73829789596583));
#50025=CARTESIAN_POINT('Ctrl Pts',(-0.275555850389802,2.26712486102769,
6.73825340663306));
#50026=CARTESIAN_POINT('Ctrl Pts',(-0.274970328856967,2.26808518818476,
6.73818729190111));
#50027=CARTESIAN_POINT('Ctrl Pts',(-0.274777372553752,2.26840043875641,
6.73816558969062));
#50028=CARTESIAN_POINT('Ctrl Pts',(-0.273824553752443,2.26995114925842,
6.73805884111184));
#50029=CARTESIAN_POINT('Ctrl Pts',(-0.273056889174893,2.27118181785375,
6.73797413656782));
#50030=CARTESIAN_POINT('Ctrl Pts',(-0.261082301664139,2.29009315307375,
6.73667204301447));
#50031=CARTESIAN_POINT('Ctrl Pts',(-0.248186346764666,2.30664716869184,
6.73552313425646));
#50032=CARTESIAN_POINT('Ctrl Pts',(-0.219273126019941,2.3371166885887,6.73316315955346));
#50033=CARTESIAN_POINT('Ctrl Pts',(-0.203310226533078,2.35093780220172,
6.73195629172405));
#50034=CARTESIAN_POINT('Ctrl Pts',(-0.185340867568427,2.36364907846595,
6.73062005994007));
#50035=CARTESIAN_POINT('Ctrl Pts',(-0.184564768947334,2.36419295940752,
6.73056239791093));
#50036=CARTESIAN_POINT('Ctrl Pts',(-0.183319151871102,2.36505770611472,
6.73046992651676));
#50037=CARTESIAN_POINT('Ctrl Pts',(-0.182851159502597,2.36538076885031,
6.73043520071061));
#50038=CARTESIAN_POINT('Ctrl Pts',(-0.181957771642656,2.36599400392637,
6.7303689404597));
#50039=CARTESIAN_POINT('Ctrl Pts',(-0.181532530558714,2.36628439896102,
6.73033741458115));
#50040=CARTESIAN_POINT('Ctrl Pts',(-0.180784710427824,2.36679245779261,
6.73028199606463));
#50041=CARTESIAN_POINT('Ctrl Pts',(-0.180462428895546,2.36701055936885,
6.73025812005145));
#50042=CARTESIAN_POINT('Ctrl Pts',(-0.179831632944389,2.36743578200776,
6.73021140168496));
#50043=CARTESIAN_POINT('Ctrl Pts',(-0.179523153650696,2.36764295433853,
6.73018856131456));
#50044=CARTESIAN_POINT('Ctrl Pts',(-0.178788879918758,2.368134246354,6.73013420916219));
#50045=CARTESIAN_POINT('Ctrl Pts',(-0.178362766481501,2.36841788535541,
6.73010267935393));
#50046=CARTESIAN_POINT('Ctrl Pts',(-0.176851890242351,2.36941840168938,
6.72999092402845));
#50047=CARTESIAN_POINT('Ctrl Pts',(-0.175763477759199,2.37012972079664,
6.72991049053158));
#50048=CARTESIAN_POINT('Ctrl Pts',(-0.156532484412484,2.38253247589564,
6.72849050645493));
#50049=CARTESIAN_POINT('Ctrl Pts',(-0.137268674712566,2.39237646035813,
6.72708081041956));
#50050=CARTESIAN_POINT('Ctrl Pts',(-0.114781937834227,2.40115253818674,
6.72545975906167));
#50051=CARTESIAN_POINT('Ctrl Pts',(-0.112383339659688,2.40205583792874,
6.72528722165743));
#50052=CARTESIAN_POINT('Ctrl Pts',(-0.0939417376466633,2.40875077877548,
6.72396414575715));
#50053=CARTESIAN_POINT('Ctrl Pts',(-0.0774722289411833,2.41328928236835,
6.72280076151746));
#50054=CARTESIAN_POINT('Ctrl Pts',(-0.0544847525141653,2.41769939331023,
6.7212520867488));
#50055=CARTESIAN_POINT('Ctrl Pts',(-0.0482144467502013,2.41871126620656,
6.72083733263755));
#50056=CARTESIAN_POINT('Ctrl Pts',(-0.0389616864876357,2.41992507303045,
6.72024031619092));
#50057=CARTESIAN_POINT('Ctrl Pts',(-0.0360000767159645,2.42027185546765,
6.7200514709824));
#50058=CARTESIAN_POINT('Ctrl Pts',(-0.0325319478012861,2.42062922930276,
6.71983328394203));
#50059=CARTESIAN_POINT('Ctrl Pts',(-0.0320298168376149,2.42067977976887,
6.71980176619068));
#50060=CARTESIAN_POINT('Ctrl Pts',(-0.0312630656450533,2.42075515114722,
6.71975375129936));
#50061=CARTESIAN_POINT('Ctrl Pts',(-0.0309985329217474,2.42078082426936,
6.71973720637868));
#50062=CARTESIAN_POINT('Ctrl Pts',(-0.0305381546025398,2.42082492956925,
6.71970844842392));
#50063=CARTESIAN_POINT('Ctrl Pts',(-0.0303423244299566,2.42084350962504,
6.71969622703716));
#50064=CARTESIAN_POINT('Ctrl Pts',(-0.0298991573435592,2.42088514724345,
6.71966859549216));
#50065=CARTESIAN_POINT('Ctrl Pts',(-0.0296518112256919,2.4209080980956,
6.71965319145988));
#50066=CARTESIAN_POINT('Ctrl Pts',(-0.028981191449886,2.4209695418703,6.71961147542123));
#50067=CARTESIAN_POINT('Ctrl Pts',(-0.0285578659038651,2.42100748366077,
6.71958519452755));
#50068=CARTESIAN_POINT('Ctrl Pts',(-0.0266534817364965,2.42117437271335,
6.71946719615054));
#50069=CARTESIAN_POINT('Ctrl Pts',(-0.0251715860297762,2.42129391098022,
6.71937600016424));
#50070=CARTESIAN_POINT('Ctrl Pts',(0.00853843822551648,2.42377849369015,
6.71731459576104));
#50071=CARTESIAN_POINT('Ctrl Pts',(0.0409458027228496,2.42129378125581,
6.71559116419884));
#50072=CARTESIAN_POINT('Ctrl Pts',(0.0887280113091252,2.41027040967293,
6.71280947680115));
#50073=CARTESIAN_POINT('Ctrl Pts',(0.104690886584727,2.40525413371082,6.71183939542702));
#50074=CARTESIAN_POINT('Ctrl Pts',(0.121113537403473,2.39865309957655,6.71076540163711));
#50075=CARTESIAN_POINT('Ctrl Pts',(0.122033707666776,2.39827828782492,6.71070497083213));
#50076=CARTESIAN_POINT('Ctrl Pts',(0.123495322589924,2.39767503465,6.71060857005303));
#50077=CARTESIAN_POINT('Ctrl Pts',(0.124037906079948,2.39744935502298,6.71057269337264));
#50078=CARTESIAN_POINT('Ctrl Pts',(0.125067376440773,2.39701785534778,6.71050444913373));
#50079=CARTESIAN_POINT('Ctrl Pts',(0.125554380616749,2.3968123187266,6.71047209126576));
#50080=CARTESIAN_POINT('Ctrl Pts',(0.126401210108036,2.39645246329958,6.7104156957374));
#50081=CARTESIAN_POINT('Ctrl Pts',(0.126761264982699,2.39629868479452,6.71039167651049));
#50082=CARTESIAN_POINT('Ctrl Pts',(0.127459206657714,2.39599909069644,6.7103450369494));
#50083=CARTESIAN_POINT('Ctrl Pts',(0.127797125848452,2.39585335164243,6.71032241925458));
#50084=CARTESIAN_POINT('Ctrl Pts',(0.128591719167727,2.39550904109501,6.71026914916756));
#50085=CARTESIAN_POINT('Ctrl Pts',(0.129048183165817,2.39530998971346,6.71023848040879));
#50086=CARTESIAN_POINT('Ctrl Pts',(0.130620761706771,2.39461988914456,6.71013258962299));
#50087=CARTESIAN_POINT('Ctrl Pts',(0.131734539042031,2.39412356863438,6.71005718722562));
#50088=CARTESIAN_POINT('Ctrl Pts',(0.145084998032035,2.38808330513215,6.70914842351874));
#50089=CARTESIAN_POINT('Ctrl Pts',(0.156964640335449,2.38178655763873,6.7082888756615));
#50090=CARTESIAN_POINT('Ctrl Pts',(0.185469585128621,2.36431479954132,6.70609391199285));
#50091=CARTESIAN_POINT('Ctrl Pts',(0.201512117558669,2.35229745704333,6.70473402588221));
#50092=CARTESIAN_POINT('Ctrl Pts',(0.219593507946827,2.33592199226662,6.70308718197745));
#50093=CARTESIAN_POINT('Ctrl Pts',(0.222790770202542,2.33290506507437,6.70279126565455));
#50094=CARTESIAN_POINT('Ctrl Pts',(0.234061645222341,2.32182536589768,6.70173336434311));
#50095=CARTESIAN_POINT('Ctrl Pts',(0.241768421741876,2.31339971067415,6.70098159539294));
#50096=CARTESIAN_POINT('Ctrl Pts',(0.249668431686356,2.30378399526349,6.70019425095516));
#50097=CARTESIAN_POINT('Ctrl Pts',(0.250320292091769,2.3029827429618,6.70012915236932));
#50098=CARTESIAN_POINT('Ctrl Pts',(0.251437547999195,2.30159586942359,6.70001736870282));
#50099=CARTESIAN_POINT('Ctrl Pts',(0.251904773128048,2.3010117419812,6.69997055827822));
#50100=CARTESIAN_POINT('Ctrl Pts',(0.252564061745699,2.30018158692492,6.69990442126327));
#50101=CARTESIAN_POINT('Ctrl Pts',(0.252757803520423,2.29993690452432,6.69988497554123));
#50102=CARTESIAN_POINT('Ctrl Pts',(0.253089949152957,2.29951617330578,6.69985162104213));
#50103=CARTESIAN_POINT('Ctrl Pts',(0.253228525252826,2.29934026129268,6.69983769986165));
#50104=CARTESIAN_POINT('Ctrl Pts',(0.253493584458275,2.29900306598931,6.6998110626201));
#50105=CARTESIAN_POINT('Ctrl Pts',(0.253620096873674,2.29884180671335,6.6997983444196));
#50106=CARTESIAN_POINT('Ctrl Pts',(0.253917826415134,2.29846155880798,6.69976840349856));
#50107=CARTESIAN_POINT('Ctrl Pts',(0.254088914547036,2.29824246871329,6.69975119004522));
#50108=CARTESIAN_POINT('Ctrl Pts',(0.254593660243662,2.29759438037056,6.69970038181837));
#50109=CARTESIAN_POINT('Ctrl Pts',(0.254926518462334,2.29716475644778,6.6996668436417));
#50110=CARTESIAN_POINT('Ctrl Pts',(0.257843096552387,2.29338056232744,6.6993726692429));
#50111=CARTESIAN_POINT('Ctrl Pts',(0.26036170831508,2.28997602312923,6.69911651878526));
#50112=CARTESIAN_POINT('Ctrl Pts',(0.263477862549883,2.28558532447237,6.69879544708528));
#50113=CARTESIAN_POINT('Ctrl Pts',(0.264138080915469,2.28464444479839,6.69872717473694));
#50114=CARTESIAN_POINT('Ctrl Pts',(0.265510483958018,2.28266620312225,6.6985846895177));
#50115=CARTESIAN_POINT('Ctrl Pts',(0.266221656538199,2.28162816006969,6.69851052763677));
#50116=CARTESIAN_POINT('Ctrl Pts',(0.267308511790982,2.28002166351271,6.69839663762457));
#50117=CARTESIAN_POINT('Ctrl Pts',(0.267688494904383,2.27945614929111,6.69835671393887));
#50118=CARTESIAN_POINT('Ctrl Pts',(0.268545856470267,2.27817138880126,6.69826638243771));
#50119=CARTESIAN_POINT('Ctrl Pts',(0.26902214551959,2.27745141887039,6.69821602203589));
#50120=CARTESIAN_POINT('Ctrl Pts',(0.281902741157039,2.25780974995223,6.69684895660928));
#50121=CARTESIAN_POINT('Ctrl Pts',(0.29228400663753,2.23763466477447,6.6956127065966));
#50122=CARTESIAN_POINT('Ctrl Pts',(0.307582521662921,2.19819060504509,6.69322840279192));
#50123=CARTESIAN_POINT('Ctrl Pts',(0.313001933961916,2.17923393432893,6.69209495183434));
#50124=CARTESIAN_POINT('Ctrl Pts',(0.3168181236952,2.15906087500548,6.6908473451199));
#50125=CARTESIAN_POINT('Ctrl Pts',(0.316974098547536,2.158217963602,6.69079514824213));
#50126=CARTESIAN_POINT('Ctrl Pts',(0.317221227853585,2.15685200177996,6.6907104497536));
#50127=CARTESIAN_POINT('Ctrl Pts',(0.317314456682427,2.15632932701864,6.690678014028));
#50128=CARTESIAN_POINT('Ctrl Pts',(0.317490834435083,2.1553261553484,6.6906157081945));
#50129=CARTESIAN_POINT('Ctrl Pts',(0.317574185263021,2.15484569505729,6.69058584458403));
#50130=CARTESIAN_POINT('Ctrl Pts',(0.317721372180488,2.15398567794411,6.69053234771643));
#50131=CARTESIAN_POINT('Ctrl Pts',(0.317785619522712,2.1536061916743,6.69050872757399));
#50132=CARTESIAN_POINT('Ctrl Pts',(0.317912120046597,2.15285077813563,6.69046167976442));
#50133=CARTESIAN_POINT('Ctrl Pts',(0.317974386626068,2.15247485369105,6.69043825256271));
#50134=CARTESIAN_POINT('Ctrl Pts',(0.318124398872332,2.15155910758006,6.69038114903178));
#50135=CARTESIAN_POINT('Ctrl Pts',(0.318211437165747,2.15101917270357,6.69034745031074));
#50136=CARTESIAN_POINT('Ctrl Pts',(0.31853500360557,2.14897891406945,6.69021999823612));
#50137=CARTESIAN_POINT('Ctrl Pts',(0.318762295857689,2.14747716459709,6.69012595264792));
#50138=CARTESIAN_POINT('Ctrl Pts',(0.322629609821283,2.12064471846475,6.68844127334209));
#50139=CARTESIAN_POINT('Ctrl Pts',(0.323249581840282,2.09497651837931,6.68674972250763));
#50140=CARTESIAN_POINT('Ctrl Pts',(0.319370138550048,2.0541539967077,6.68397895336181));
#50141=CARTESIAN_POINT('Ctrl Pts',(0.316809963252761,2.03892119311113,6.68292946436056));
#50142=CARTESIAN_POINT('Ctrl Pts',(0.311341951084789,2.01641024425161,6.68139743627792));
#50143=CARTESIAN_POINT('Ctrl Pts',(0.309244962437868,2.00895807270674,6.68089372185862));
#50144=CARTESIAN_POINT('Ctrl Pts',(0.306383513590788,2.0000351176264,6.68030053879013));
#50145=CARTESIAN_POINT('Ctrl Pts',(0.305873731840747,1.99848598350857,6.68019792569656));
#50146=CARTESIAN_POINT('Ctrl Pts',(0.305218015435695,1.99654317447165,6.68006976237897));
#50147=CARTESIAN_POINT('Ctrl Pts',(0.305083053505842,1.99614586111659,6.68004358018279));
#50148=CARTESIAN_POINT('Ctrl Pts',(0.30486734968666,1.9955149014087,6.68000204661094));
#50149=CARTESIAN_POINT('Ctrl Pts',(0.304787114877964,1.99528108414447,6.67998666528726));
#50150=CARTESIAN_POINT('Ctrl Pts',(0.304635365116556,1.99484051252263,6.67995770198681));
#50151=CARTESIAN_POINT('Ctrl Pts',(0.304563909243897,1.99463374035012,6.67994411668606));
#50152=CARTESIAN_POINT('Ctrl Pts',(0.304401086219191,1.99416412817387,6.67991328023284));
#50153=CARTESIAN_POINT('Ctrl Pts',(0.304309589334357,1.99390133414047,6.67989603693768));
#50154=CARTESIAN_POINT('Ctrl Pts',(0.304031240038526,1.99310519152697,6.67984383548219));
#50155=CARTESIAN_POINT('Ctrl Pts',(0.303843323739952,1.99257221203078,6.67980894033994));
#50156=CARTESIAN_POINT('Ctrl Pts',(0.302518036455546,1.98884464843654,6.67956523079434));
#50157=CARTESIAN_POINT('Ctrl Pts',(0.301331655613393,1.98566754571356,6.67935926515628));
#50158=CARTESIAN_POINT('Ctrl Pts',(0.296482616776541,1.97328207549909,6.67856106051052));
#50159=CARTESIAN_POINT('Ctrl Pts',(0.292445915489521,1.96422519738477,6.67798764672803));
#50160=CARTESIAN_POINT('Ctrl Pts',(0.278777642612646,1.93700830394182,6.67625495843062));
#50161=CARTESIAN_POINT('Ctrl Pts',(0.267822884818316,1.91957213052554,6.67512851917487));
#50162=CARTESIAN_POINT('Ctrl Pts',(0.245149353689464,1.89014625266057,6.67301937148484));
#50163=CARTESIAN_POINT('Ctrl Pts',(0.234016658136712,1.87779989626547,6.67205428344464));
#50164=CARTESIAN_POINT('Ctrl Pts',(0.221332805272072,1.86574848780848,6.67099155635364));
#50165=CARTESIAN_POINT('Ctrl Pts',(0.220679376069303,1.86513281496587,6.67093690838455));
#50166=CARTESIAN_POINT('Ctrl Pts',(0.219623048756993,1.86414582413511,6.67084872126541));
#50167=CARTESIAN_POINT('Ctrl Pts',(0.21922175830618,1.86377278628926,6.67081525567561));
#50168=CARTESIAN_POINT('Ctrl Pts',(0.218452498066158,1.86306133359068,6.67075117085958));
#50169=CARTESIAN_POINT('Ctrl Pts',(0.218084687976577,1.86272274778884,6.67072055903436));
#50170=CARTESIAN_POINT('Ctrl Pts',(0.217430900771802,1.86212371149742,6.67066619733387));
#50171=CARTESIAN_POINT('Ctrl Pts',(0.217145239140507,1.86186291687623,6.67064246212712));
#50172=CARTESIAN_POINT('Ctrl Pts',(0.216580697541484,1.86134937936236,6.67059558880442));
#50173=CARTESIAN_POINT('Ctrl Pts',(0.216301842895133,1.86109660940751,6.67057245188582));
#50174=CARTESIAN_POINT('Ctrl Pts',(0.2156293854293,1.8604891976153,6.67051669556292));
#50175=CARTESIAN_POINT('Ctrl Pts',(0.215235350598025,1.86013503764165,6.67048405593303));
#50176=CARTESIAN_POINT('Ctrl Pts',(0.21379002602807,1.8588424035141,6.67036444674036));
#50177=CARTESIAN_POINT('Ctrl Pts',(0.212733468911141,1.85790986662868,6.67027722895001));
#50178=CARTESIAN_POINT('Ctrl Pts',(0.195215194089538,1.84265114872117,6.66883457321651));
#50179=CARTESIAN_POINT('Ctrl Pts',(0.177349721712035,1.83002938176795,6.66740739418118));
#50180=CARTESIAN_POINT('Ctrl Pts',(0.149206804324877,1.81415265074855,6.66523581012651));
#50181=CARTESIAN_POINT('Ctrl Pts',(0.139817253751994,1.80944448751456,6.66452363951018));
#50182=CARTESIAN_POINT('Ctrl Pts',(0.114051836474589,1.79806363136894,6.66262037585208));
#50183=CARTESIAN_POINT('Ctrl Pts',(0.0973266116169021,1.79226457097825,
6.66143664365141));
#50184=CARTESIAN_POINT('Ctrl Pts',(0.0794711688895155,1.78767630875198,
6.66027932505747));
#50185=CARTESIAN_POINT('Ctrl Pts',(0.0787334030158195,1.787489510453,6.66023169352785));
#50186=CARTESIAN_POINT('Ctrl Pts',(0.0776900177401195,1.78722926039604,
6.66016460215941));
#50187=CARTESIAN_POINT('Ctrl Pts',(0.0773849492829744,1.78715364148619,
6.66014501850574));
#50188=CARTESIAN_POINT('Ctrl Pts',(0.0768619283202994,1.78702480939567,
6.66011150022548));
#50189=CARTESIAN_POINT('Ctrl Pts',(0.0766440303894269,1.78697137740181,
6.66009755288307));
#50190=CARTESIAN_POINT('Ctrl Pts',(0.0762274060677701,1.78686967567683,
6.66007091776301));
#50191=CARTESIAN_POINT('Ctrl Pts',(0.0760286897687639,1.78682136762039,
6.6600582277452));
#50192=CARTESIAN_POINT('Ctrl Pts',(0.0755615208815455,1.78670826941778,
6.66002842712831));
#50193=CARTESIAN_POINT('Ctrl Pts',(0.0752930301973353,1.786643634987,6.66001132558069));
#50194=CARTESIAN_POINT('Ctrl Pts',(0.0745027738047079,1.78645446891009,
6.65996106399379));
#50195=CARTESIAN_POINT('Ctrl Pts',(0.0739807766175856,1.78633089397923,
6.65992795884736));
#50196=CARTESIAN_POINT('Ctrl Pts',(0.0695162087752438,1.78528573996641,
6.65964560542984));
#50197=CARTESIAN_POINT('Ctrl Pts',(0.0655566839218102,1.78443717957543,
6.65940045551308));
#50198=CARTESIAN_POINT('Ctrl Pts',(0.0611487147152334,1.78357906964804,
6.65913229563636));
#50199=CARTESIAN_POINT('Ctrl Pts',(0.0607152539548016,1.78349561074529,
6.65910597671003));
#50200=CARTESIAN_POINT('Ctrl Pts',(0.0595554264597815,1.78327476689968,
6.65903568659392));
#50201=CARTESIAN_POINT('Ctrl Pts',(0.0588287522527045,1.78313898941248,
6.65899178608695));
#50202=CARTESIAN_POINT('Ctrl Pts',(0.0573186857530803,1.78286221061923,
6.65890083470527));
#50203=CARTESIAN_POINT('Ctrl Pts',(0.056535224593241,1.78272160869003,6.65885380085295));
#50204=CARTESIAN_POINT('Ctrl Pts',(0.0533255441466637,1.78215785756886,
6.65866171373051));
#50205=CARTESIAN_POINT('Ctrl Pts',(0.0508949808578761,1.78175961494985,
6.65851765789609));
#50206=CARTESIAN_POINT('Ctrl Pts',(0.0186080583378787,1.77684884085909,
6.65661985516059));
#50207=CARTESIAN_POINT('Ctrl Pts',(-0.0117351319805428,1.77652583954778,
6.65500079427766));
#50208=CARTESIAN_POINT('Ctrl Pts',(-0.052449832174843,1.78183634691832,
6.65263182345073));
#50209=CARTESIAN_POINT('Ctrl Pts',(-0.0631388059993833,1.78378401613556,
6.65199269758384));
#50210=CARTESIAN_POINT('Ctrl Pts',(-0.0756320651681918,1.78671918144156,
6.65121644061594));
#50211=CARTESIAN_POINT('Ctrl Pts',(-0.0775515454949799,1.78718881401112,
6.65109635786801));
#50212=CARTESIAN_POINT('Ctrl Pts',(-0.0800995077087255,1.7878371081348,
6.65093582770652));
#50213=CARTESIAN_POINT('Ctrl Pts',(-0.0807319677813652,1.78800007762649,
6.65089588767806));
#50214=CARTESIAN_POINT('Ctrl Pts',(-0.081772041175835,1.78827145333573,
6.65083005213778));
#50215=CARTESIAN_POINT('Ctrl Pts',(-0.0821799469248575,1.78837873974289,
6.65080419292628));
#50216=CARTESIAN_POINT('Ctrl Pts',(-0.0829717573599277,1.78858866266157,
6.65075391938526));
#50217=CARTESIAN_POINT('Ctrl Pts',(-0.0833556853040245,1.78869120913865,
6.65072950801464));
#50218=CARTESIAN_POINT('Ctrl Pts',(-0.0842443294158892,1.78893032616989,
6.65067292348749));
#50219=CARTESIAN_POINT('Ctrl Pts',(-0.0847489038191593,1.78906741516558,
6.65064073355104));
#50220=CARTESIAN_POINT('Ctrl Pts',(-0.0861068966897092,1.78943992253722,
6.65055393295223));
#50221=CARTESIAN_POINT('Ctrl Pts',(-0.0869596778412041,1.7896776292693,
6.6504992480142));
#50222=CARTESIAN_POINT('Ctrl Pts',(-0.0931358100975883,1.79142663979053,
6.65010190515683));
#50223=CARTESIAN_POINT('Ctrl Pts',(-0.0984201520415046,1.79307123743203,
6.64975492026018));
#50224=CARTESIAN_POINT('Ctrl Pts',(-0.104356550236686,1.79508783506183,
6.64935678025263));
#50225=CARTESIAN_POINT('Ctrl Pts',(-0.105052995335693,1.79532708347909,
6.64930994029951));
#50226=CARTESIAN_POINT('Ctrl Pts',(-0.107361402723205,1.79612894217185,
6.64915425023359));
#50227=CARTESIAN_POINT('Ctrl Pts',(-0.108969693556249,1.79670196787344,
6.64904507154335));
#50228=CARTESIAN_POINT('Ctrl Pts',(-0.131573253173491,1.80495849131003,
6.64750060308036));
#50229=CARTESIAN_POINT('Ctrl Pts',(-0.151715020338753,1.81479257245665,
6.64599557362508));
#50230=CARTESIAN_POINT('Ctrl Pts',(-0.178132692410752,1.83128595671305,
6.64388808287417));
#50231=CARTESIAN_POINT('Ctrl Pts',(-0.185397917293255,1.83624611096482,
6.64329358844632));
#50232=CARTESIAN_POINT('Ctrl Pts',(-0.200944456264922,1.84782027489546,
6.64199956642229));
#50233=CARTESIAN_POINT('Ctrl Pts',(-0.209121766107187,1.85455871397967,
6.6413040805885));
#50234=CARTESIAN_POINT('Ctrl Pts',(-0.218063950077104,1.86269946160966,
6.64053943237398));
#50235=CARTESIAN_POINT('Ctrl Pts',(-0.219167625175041,1.86371842194622,
6.64044498466496));
#50236=CARTESIAN_POINT('Ctrl Pts',(-0.220561844094178,1.86502379939275,
6.64032562780793));
#50237=CARTESIAN_POINT('Ctrl Pts',(-0.220858999989643,1.86530308044206,
6.64030018610429));
#50238=CARTESIAN_POINT('Ctrl Pts',(-0.221333513363865,1.86575074963799,
6.64025955644224));
#50239=CARTESIAN_POINT('Ctrl Pts',(-0.221511209425123,1.8659187757783,6.6402443407279));
#50240=CARTESIAN_POINT('Ctrl Pts',(-0.221847869402671,1.86623784192354,
6.64021551227828));
#50241=CARTESIAN_POINT('Ctrl Pts',(-0.222006869105227,1.86638884064017,
6.64020189662269));
#50242=CARTESIAN_POINT('Ctrl Pts',(-0.222370549312114,1.86673492679859,
6.64017075240676));
#50243=CARTESIAN_POINT('Ctrl Pts',(-0.222575126952611,1.86693012112131,
6.64015323230564));
#50244=CARTESIAN_POINT('Ctrl Pts',(-0.223204117903708,1.86753184569167,
6.64009936172257));
#50245=CARTESIAN_POINT('Ctrl Pts',(-0.223627679310309,1.86793927071596,
6.64006308034086));
#50246=CARTESIAN_POINT('Ctrl Pts',(-0.226828153979922,1.8710347169569,6.63978887407476));
#50247=CARTESIAN_POINT('Ctrl Pts',(-0.229557774110707,1.87377147869617,
6.63955466358746));
#50248=CARTESIAN_POINT('Ctrl Pts',(-0.249557216689278,1.89455807697346,
6.63782982519433));
#50249=CARTESIAN_POINT('Ctrl Pts',(-0.26472750346581,1.91451445679514,6.63646622893819));
#50250=CARTESIAN_POINT('Ctrl Pts',(-0.287956828664474,1.9538179526262,6.63390288772782));
#50251=CARTESIAN_POINT('Ctrl Pts',(-0.296735117575865,1.97257781282311,
6.63272161881677));
#50252=CARTESIAN_POINT('Ctrl Pts',(-0.304327901150404,1.99393530565438,
6.63135078366399));
#50253=CARTESIAN_POINT('Ctrl Pts',(-0.304981477499188,1.99582951998574,
6.63122902998334));
#50254=CARTESIAN_POINT('Ctrl Pts',(-0.305825698700041,1.99835233029592,
6.63106660212111));
#50255=CARTESIAN_POINT('Ctrl Pts',(-0.306032157021054,1.99897561878129,
6.63102645076121));
#50256=CARTESIAN_POINT('Ctrl Pts',(-0.306368346594824,2.00000104812995,
6.63096035676862));
#50257=CARTESIAN_POINT('Ctrl Pts',(-0.306499194946625,2.00040282300822,
6.63093445100502));
#50258=CARTESIAN_POINT('Ctrl Pts',(-0.306751464593718,2.00118263185218,
6.63088415158185));
#50259=CARTESIAN_POINT('Ctrl Pts',(-0.30687297821767,2.00156063533511,6.63085976101402));
#50260=CARTESIAN_POINT('Ctrl Pts',(-0.307152291179562,2.0024350627221,6.63080331875745));
#50261=CARTESIAN_POINT('Ctrl Pts',(-0.307309585804897,2.00293164557779,
6.6307712505493));
#50262=CARTESIAN_POINT('Ctrl Pts',(-0.307728945588953,2.00426681050409,
6.63068498735583));
#50263=CARTESIAN_POINT('Ctrl Pts',(-0.3079887852483,2.00510608206454,6.63063071952063));
#50264=CARTESIAN_POINT('Ctrl Pts',(-0.309822187866375,2.011114757208,6.63024186974474));
#50265=CARTESIAN_POINT('Ctrl Pts',(-0.311268868949222,2.01632168745286,
6.6299031653194));
#50266=CARTESIAN_POINT('Ctrl Pts',(-0.313038737743376,2.02337483111253,
6.62944167140359));
#50267=CARTESIAN_POINT('Ctrl Pts',(-0.313477785404343,2.02519127282414,
6.62932258423232));
#50268=CARTESIAN_POINT('Ctrl Pts',(-0.319487064661382,2.05103529236545,
6.62762483912698));
#50269=CARTESIAN_POINT('Ctrl Pts',(-0.322295879094073,2.07561755170173,
6.6259589500366));
#50270=CARTESIAN_POINT('Ctrl Pts',(-0.322259321826866,2.11854910398288,
6.62305557491489));
#50271=CARTESIAN_POINT('Ctrl Pts',(-0.320689372072886,2.13679183935199,
6.6218268495696));
#50272=CARTESIAN_POINT('Ctrl Pts',(-0.317394801190109,2.15588302548084,
6.6206061851641));
#50273=CARTESIAN_POINT('Ctrl Pts',(-0.317203276167546,2.15696010910883,
6.62053754730237));
#50274=CARTESIAN_POINT('Ctrl Pts',(-0.316938468303947,2.15840654651988,
6.62044569989732));
#50275=CARTESIAN_POINT('Ctrl Pts',(-0.316870020188938,2.15877676136142,
6.62042222051305));
#50276=CARTESIAN_POINT('Ctrl Pts',(-0.316761677966465,2.15935706126999,
6.62038546358732));
#50277=CARTESIAN_POINT('Ctrl Pts',(-0.31672222352666,2.15956722652362,6.62037216097588));
#50278=CARTESIAN_POINT('Ctrl Pts',(-0.316645962703296,2.15997123358497,
6.62034660747485));
#50279=CARTESIAN_POINT('Ctrl Pts',(-0.316609187759051,2.16016507941311,
6.62033435492812));
#50280=CARTESIAN_POINT('Ctrl Pts',(-0.316521437390518,2.16062531532674,
6.62030528387959));
#50281=CARTESIAN_POINT('Ctrl Pts',(-0.316470303736836,2.16089167463815,
6.62028847456349));
#50282=CARTESIAN_POINT('Ctrl Pts',(-0.316318133471877,2.16167897247615,
6.62023883476007));
#50283=CARTESIAN_POINT('Ctrl Pts',(-0.316216145789568,2.1621997295841,6.62020605850546));
#50284=CARTESIAN_POINT('Ctrl Pts',(-0.315406065560184,2.16628257111189,
6.61994952374986));
#50285=CARTESIAN_POINT('Ctrl Pts',(-0.314639056723921,2.16983288710256,
6.61972906385438));
#50286=CARTESIAN_POINT('Ctrl Pts',(-0.311705713359139,2.18237920164775,
6.61895685616938));
#50287=CARTESIAN_POINT('Ctrl Pts',(-0.309212061746471,2.19129466079152,
6.61842067977414));
#50288=CARTESIAN_POINT('Ctrl Pts',(-0.300363237591256,2.21837728376119,
6.61679696242207));
#50289=CARTESIAN_POINT('Ctrl Pts',(-0.292763112877847,2.2360921192581,6.61573995573784));
#50290=CARTESIAN_POINT('Ctrl Pts',(-0.274898359517753,2.26920426749017,
6.61361374702799));
#50291=CARTESIAN_POINT('Ctrl Pts',(-0.264801439263323,2.28460563208022,
6.61255083334303));
#50292=CARTESIAN_POINT('Ctrl Pts',(-0.252653501148617,2.3000725817429,6.61135621500177));
#50293=CARTESIAN_POINT('Ctrl Pts',(-0.251853088440833,2.30107921666802,
6.61127785958688));
#50294=CARTESIAN_POINT('Ctrl Pts',(-0.250727208068352,2.30247790580335,
6.61116812599454));
#50295=CARTESIAN_POINT('Ctrl Pts',(-0.250406796002273,2.30287402917928,
6.6111369510394));
#50296=CARTESIAN_POINT('Ctrl Pts',(-0.249851466942024,2.3035572590397,6.61108301161048));
#50297=CARTESIAN_POINT('Ctrl Pts',(-0.24961699040183,2.30384472360525,6.61106026494753));
#50298=CARTESIAN_POINT('Ctrl Pts',(-0.249130262527172,2.30443934527068,
6.61101310518142));
#50299=CARTESIAN_POINT('Ctrl Pts',(-0.248877938352919,2.30474644172868,
6.61098868914785));
#50300=CARTESIAN_POINT('Ctrl Pts',(-0.248286218312451,2.30546389708571,
6.61093150591951));
#50301=CARTESIAN_POINT('Ctrl Pts',(-0.247946372907587,2.3058738821854,6.61089872047034));
#50302=CARTESIAN_POINT('Ctrl Pts',(-0.246847473299658,2.30719291271606,
6.61079288914048));
#50303=CARTESIAN_POINT('Ctrl Pts',(-0.246084430639593,2.30809860905581,
6.61071968038369));
#50304=CARTESIAN_POINT('Ctrl Pts',(-0.234651407080719,2.32151826212848,
6.60962679361422));
#50305=CARTESIAN_POINT('Ctrl Pts',(-0.223045665703547,2.33319970181887,
6.60856737408695));
#50306=CARTESIAN_POINT('Ctrl Pts',(-0.187577046801874,2.36382045285604,
6.60546187578407));
#50307=CARTESIAN_POINT('Ctrl Pts',(-0.161857270970549,2.38033632784369,
6.60334532445197));
#50308=CARTESIAN_POINT('Ctrl Pts',(-0.130766477397451,2.39457700068702,
6.60114438517799));
#50309=CARTESIAN_POINT('Ctrl Pts',(-0.127300139510424,2.39609146985853,
6.60090384315475));
#50310=CARTESIAN_POINT('Ctrl Pts',(-0.123268595509839,2.39776898766724,
6.60063029361198));
#50311=CARTESIAN_POINT('Ctrl Pts',(-0.122728816269785,2.39799186956201,
6.60059379574177));
#50312=CARTESIAN_POINT('Ctrl Pts',(-0.121927462265375,2.39832021236869,
6.60053980309165));
#50313=CARTESIAN_POINT('Ctrl Pts',(-0.121666353910043,2.39842679753981,
6.6005222406038));
#50314=CARTESIAN_POINT('Ctrl Pts',(-0.121202064911155,2.3986156109941,6.60049106591567));
#50315=CARTESIAN_POINT('Ctrl Pts',(-0.120998940352899,2.39869797472143,
6.60047744547432));
#50316=CARTESIAN_POINT('Ctrl Pts',(-0.120568619413325,2.39887195192582,
6.60044862944556));
#50317=CARTESIAN_POINT('Ctrl Pts',(-0.120341403196061,2.39896351334728,
6.6004334370636));
#50318=CARTESIAN_POINT('Ctrl Pts',(-0.119733958469073,2.39920749091188,
6.60039288211408));
#50319=CARTESIAN_POINT('Ctrl Pts',(-0.119353541801786,2.39935944196272,
6.60036754776159));
#50320=CARTESIAN_POINT('Ctrl Pts',(-0.117558821456246,2.40007234800676,
6.60024832034533));
#50321=CARTESIAN_POINT('Ctrl Pts',(-0.116140816368967,2.400624020211,6.60015497973448));
#50322=CARTESIAN_POINT('Ctrl Pts',(-0.104595262146491,2.40502191088111,
6.59940154865229));
#50323=CARTESIAN_POINT('Ctrl Pts',(-0.09428240192044,2.40836571941136,6.59876931500065));
#50324=CARTESIAN_POINT('Ctrl Pts',(-0.0556052603918844,2.418783681615,6.59647997861232));
#50325=CARTESIAN_POINT('Ctrl Pts',(-0.0264890291801961,2.42251114144918,
6.5949021085755));
#50326=CARTESIAN_POINT('Ctrl Pts',(0.0121434294342142,2.4221836344091,6.5926504233315));
#50327=CARTESIAN_POINT('Ctrl Pts',(0.0215460517823926,2.4216916204006,6.59209140229217));
#50328=CARTESIAN_POINT('Ctrl Pts',(0.0320521523153674,2.42067919291897,
6.59144953770405));
#50329=CARTESIAN_POINT('Ctrl Pts',(0.0331906547719284,2.42056335664285,
6.59137975629247));
#50330=CARTESIAN_POINT('Ctrl Pts',(0.0348449754134277,2.42038613128017,
6.59127802374368));
#50331=CARTESIAN_POINT('Ctrl Pts',(0.0353613091545143,2.42032955411283,
6.59124622421171));
#50332=CARTESIAN_POINT('Ctrl Pts',(0.0362718440417313,2.42022755411161,
6.59119006221195));
#50333=CARTESIAN_POINT('Ctrl Pts',(0.0366661032686878,2.42018265092185,
6.59116571617009));
#50334=CARTESIAN_POINT('Ctrl Pts',(0.0374806038395108,2.42008836124264,
6.59111536128445));
#50335=CARTESIAN_POINT('Ctrl Pts',(0.0379008326709435,2.42003887505631,
6.59108934934049));
#50336=CARTESIAN_POINT('Ctrl Pts',(0.0389755377077947,2.41991017129936,
6.5910227428645));
#50337=CARTESIAN_POINT('Ctrl Pts',(0.0396298681788365,2.41982977312659,
6.59098211114579));
#50338=CARTESIAN_POINT('Ctrl Pts',(0.0422932818733531,2.41949421819349,
6.590816398588));
#50339=CARTESIAN_POINT('Ctrl Pts',(0.0443001514093276,2.41922213807145,
6.59069078444226));
#50340=CARTESIAN_POINT('Ctrl Pts',(0.0770672839228347,2.41446481462806,
6.58862720030297));
#50341=CARTESIAN_POINT('Ctrl Pts',(0.107015769672301,2.40557188925545,6.58653480559351));
#50342=CARTESIAN_POINT('Ctrl Pts',(0.151410314067701,2.38505132634152,6.5832286254383));
#50343=CARTESIAN_POINT('Ctrl Pts',(0.166954479375147,2.37623488579184,6.58203155674657));
#50344=CARTESIAN_POINT('Ctrl Pts',(0.182507440372719,2.3656185005857,6.58084632664786));
#50345=CARTESIAN_POINT('Ctrl Pts',(0.183321683230509,2.36505719036264,6.58078431960711));
#50346=CARTESIAN_POINT('Ctrl Pts',(0.184429686807892,2.3642858237448,6.5807000153466));
#50347=CARTESIAN_POINT('Ctrl Pts',(0.184725686528502,2.36407901610719,6.58067750093006));
#50348=CARTESIAN_POINT('Ctrl Pts',(0.185193907746836,2.36375070915435,6.58064189919249));
#50349=CARTESIAN_POINT('Ctrl Pts',(0.185366357590892,2.36362953840584,6.58062878940705));
#50350=CARTESIAN_POINT('Ctrl Pts',(0.185715250200877,2.36338387972074,6.58060227183979));
#50351=CARTESIAN_POINT('Ctrl Pts',(0.185891686187882,2.36325938399297,6.58058886474506));
#50352=CARTESIAN_POINT('Ctrl Pts',(0.186298200620303,2.36297192922799,6.58055798082721));
#50353=CARTESIAN_POINT('Ctrl Pts',(0.186528191075332,2.36280884507922,6.58054051265102));
#50354=CARTESIAN_POINT('Ctrl Pts',(0.187011833072078,2.36246494422835,6.58050378857623));
#50355=CARTESIAN_POINT('Ctrl Pts',(0.187265437283023,2.36228406100809,6.58048453725561));
#50356=CARTESIAN_POINT('Ctrl Pts',(0.187938784062659,2.36180232192658,6.58043343623169));
#50357=CARTESIAN_POINT('Ctrl Pts',(0.188358068536367,2.36150082284181,6.58040163007021));
#50358=CARTESIAN_POINT('Ctrl Pts',(0.189625570720635,2.36058475724289,6.58030551549271));
#50359=CARTESIAN_POINT('Ctrl Pts',(0.190471528581842,2.35996705492589,6.58024141536082));
#50360=CARTESIAN_POINT('Ctrl Pts',(0.200744108929318,2.35238915075826,6.57946343371671));
#50361=CARTESIAN_POINT('Ctrl Pts',(0.209788514531976,2.34492310024092,6.57878242133047));
#50362=CARTESIAN_POINT('Ctrl Pts',(0.241488246609738,2.31570780049324,6.57632765415075));
#50363=CARTESIAN_POINT('Ctrl Pts',(0.261337113803508,2.29117905325402,6.57463365179721));
#50364=CARTESIAN_POINT('Ctrl Pts',(0.280620525559445,2.25860356985345,6.57239771115475));
#50365=CARTESIAN_POINT('Ctrl Pts',(0.283745449642445,2.25294274294638,6.57201044179386));
#50366=CARTESIAN_POINT('Ctrl Pts',(0.287168828737621,2.24627475064916,6.5715542454528));
#50367=CARTESIAN_POINT('Ctrl Pts',(0.287635370120244,2.24535519492971,6.57149133385925));
#50368=CARTESIAN_POINT('Ctrl Pts',(0.28832299634454,2.24398360530252,6.57139749131474));
#50369=CARTESIAN_POINT('Ctrl Pts',(0.288547451679594,2.24353326075053,6.57136667848545));
#50370=CARTESIAN_POINT('Ctrl Pts',(0.288945424648095,2.24273006624821,6.57131172130711));
#50371=CARTESIAN_POINT('Ctrl Pts',(0.289119353320351,2.24237742015409,6.57128759137753));
#50372=CARTESIAN_POINT('Ctrl Pts',(0.289484217494473,2.24163422056622,6.57123673573114));
#50373=CARTESIAN_POINT('Ctrl Pts',(0.289675008868199,2.24124359754711,6.57121000504982));
#50374=CARTESIAN_POINT('Ctrl Pts',(0.290175874567537,2.24021285016091,6.57113946642967));
#50375=CARTESIAN_POINT('Ctrl Pts',(0.290484619836224,2.23957208588011,6.57109561236978));
#50376=CARTESIAN_POINT('Ctrl Pts',(0.291863423442889,2.23668614966501,6.57089807687009));
#50377=CARTESIAN_POINT('Ctrl Pts',(0.292909567846075,2.23442970639169,6.57074356980709));
#50378=CARTESIAN_POINT('Ctrl Pts',(0.300425392804924,2.21771437256489,6.56959830864876));
#50379=CARTESIAN_POINT('Ctrl Pts',(0.305846362315273,2.20281030430877,6.5685716778259));
#50380=CARTESIAN_POINT('Ctrl Pts',(0.318018798573217,2.15969884950924,6.56559334462402));
#50381=CARTESIAN_POINT('Ctrl Pts',(0.322095117045738,2.1308960169106,6.56358322026048));
#50382=CARTESIAN_POINT('Ctrl Pts',(0.322293895382364,2.09782486587061,6.56145005689894));
#50383=CARTESIAN_POINT('Ctrl Pts',(0.322239903828466,2.09371235099165,6.56118814585552));
#50384=CARTESIAN_POINT('Ctrl Pts',(0.322089815645785,2.0890630536818,6.56089668321325));
#50385=CARTESIAN_POINT('Ctrl Pts',(0.322071073429158,2.08852438203574,6.56086298454879));
#50386=CARTESIAN_POINT('Ctrl Pts',(0.322040659918391,2.08770912471258,6.56081209224406));
#50387=CARTESIAN_POINT('Ctrl Pts',(0.322029983631112,2.0874325062179,6.56079484341768));
#50388=CARTESIAN_POINT('Ctrl Pts',(0.322010793865534,2.0869513928304,6.56076487662479));
#50389=CARTESIAN_POINT('Ctrl Pts',(0.322002441993572,2.08674689222477,6.56075214956509));
#50390=CARTESIAN_POINT('Ctrl Pts',(0.321984727422373,2.08632304373972,6.56072579345984));
#50391=CARTESIAN_POINT('Ctrl Pts',(0.321975335398093,2.08610369756302,6.5607121661422));
#50392=CARTESIAN_POINT('Ctrl Pts',(0.321952401135233,2.08558058654588,6.56067969570443));
#50393=CARTESIAN_POINT('Ctrl Pts',(0.321938653077535,2.0852768299085,6.56066086420566));
#50394=CARTESIAN_POINT('Ctrl Pts',(0.321908527065373,2.08463143429872,6.5606209011622));
#50395=CARTESIAN_POINT('Ctrl Pts',(0.321892035080365,2.08428980065445,6.56059977600045));
#50396=CARTESIAN_POINT('Ctrl Pts',(0.321845567337499,2.08335801747154,6.56054223570543));
#50397=CARTESIAN_POINT('Ctrl Pts',(0.321814512123512,2.08276791954618,6.56050587992766));
#50398=CARTESIAN_POINT('Ctrl Pts',(0.321712228515039,2.08092116656538,6.56039235709828));
#50399=CARTESIAN_POINT('Ctrl Pts',(0.321635260149936,2.0796648234084,6.56031549756488));
#50400=CARTESIAN_POINT('Ctrl Pts',(0.319682461462954,2.05058221953155,6.55854420973092));
#50401=CARTESIAN_POINT('Ctrl Pts',(0.314209481574766,2.02311080257267,6.55703144130547));
#50402=CARTESIAN_POINT('Ctrl Pts',(0.298576707610294,1.97692099675488,6.5542902562956));
#50403=CARTESIAN_POINT('Ctrl Pts',(0.289985835959451,1.95785743138839,6.55309371855112));
#50404=CARTESIAN_POINT('Ctrl Pts',(0.278968116826452,1.93863193183028,6.55174788249451));
#50405=CARTESIAN_POINT('Ctrl Pts',(0.278315312194932,1.93750861391712,6.55166873007036));
#50406=CARTESIAN_POINT('Ctrl Pts',(0.277395952932744,1.93594841427286,6.55155805903196));
#50407=CARTESIAN_POINT('Ctrl Pts',(0.277135117037612,1.93550816317265,6.5515267482663));
#50408=CARTESIAN_POINT('Ctrl Pts',(0.276683086279855,1.93474933149786,6.55147263738485));
#50409=CARTESIAN_POINT('Ctrl Pts',(0.276492386439839,1.93443045596283,6.55144985534888));
#50410=CARTESIAN_POINT('Ctrl Pts',(0.276096727534256,1.93377145141046,6.55140268216278));
#50411=CARTESIAN_POINT('Ctrl Pts',(0.275891690461676,1.93343137014039,6.55137828818624));
#50412=CARTESIAN_POINT('Ctrl Pts',(0.27541134477959,1.93263797299754,6.55132126030504));
#50413=CARTESIAN_POINT('Ctrl Pts',(0.275135545264565,1.93218495704413,6.55128860843934));
#50414=CARTESIAN_POINT('Ctrl Pts',(0.274246389646173,1.93073255370815,6.55118363345457));
#50415=CARTESIAN_POINT('Ctrl Pts',(0.27362870226348,1.92973584097797,6.55111115113403));
#50416=CARTESIAN_POINT('Ctrl Pts',(0.264093491446308,1.91453553504728,6.54999889305642));
#50417=CARTESIAN_POINT('Ctrl Pts',(0.254087554383901,1.90104826643011,6.54891772302961));
#50418=CARTESIAN_POINT('Ctrl Pts',(0.224088785208224,1.86658626590658,6.54588687498637));
#50419=CARTESIAN_POINT('Ctrl Pts',(0.20224961482957,1.8474277936976,6.54387976400894));
#50420=CARTESIAN_POINT('Ctrl Pts',(0.17407181074574,1.82873607912093,6.54168805340087));
#50421=CARTESIAN_POINT('Ctrl Pts',(0.169933617456621,1.82612469589766,6.54137541301936));
#50422=CARTESIAN_POINT('Ctrl Pts',(0.165251892355717,1.82331731525357,6.54103324705182));
#50423=CARTESIAN_POINT('Ctrl Pts',(0.164765717023042,1.82302752037242,6.54099785125269));
#50424=CARTESIAN_POINT('Ctrl Pts',(0.164034693755202,1.82259438477016,6.54094483703856));
#50425=CARTESIAN_POINT('Ctrl Pts',(0.163790419073719,1.82245008604291,6.54092715680016));
#50426=CARTESIAN_POINT('Ctrl Pts',(0.163368070351908,1.82220134659791,6.54089664815838));
#50427=CARTESIAN_POINT('Ctrl Pts',(0.163190086470525,1.82209675438957,6.54088380984867));
#50428=CARTESIAN_POINT('Ctrl Pts',(0.162832538957146,1.82188710356793,6.54085805654472));
#50429=CARTESIAN_POINT('Ctrl Pts',(0.162652974385194,1.82178204797511,6.54084514179551));
#50430=CARTESIAN_POINT('Ctrl Pts',(0.162222596407782,1.82153081119143,6.54081423277895));
#50431=CARTESIAN_POINT('Ctrl Pts',(0.161971686160794,1.82138479441208,6.54079624928597));
#50432=CARTESIAN_POINT('Ctrl Pts',(0.161173558919852,1.82092176819127,6.540739159766));
#50433=CARTESIAN_POINT('Ctrl Pts',(0.16062560167473,1.82060602786211,6.54070013580343));
#50434=CARTESIAN_POINT('Ctrl Pts',(0.15934374980918,1.81987242510667,6.54060923626793));
#50435=CARTESIAN_POINT('Ctrl Pts',(0.15860913112974,1.8194558281167,6.54055744002598));
#50436=CARTESIAN_POINT('Ctrl Pts',(0.15609027469624,1.8180404590163,6.54038082736188));
#50437=CARTESIAN_POINT('Ctrl Pts',(0.154298131855275,1.81705575886691,6.54025685479047));
#50438=CARTESIAN_POINT('Ctrl Pts',(0.147105768656463,1.81319254716358,6.53976552330466));
#50439=CARTESIAN_POINT('Ctrl Pts',(0.141633105896393,1.81045087565736,6.53940550745751));
#50440=CARTESIAN_POINT('Ctrl Pts',(0.125456476851448,1.80291527153451,6.53837163266596));
#50441=CARTESIAN_POINT('Ctrl Pts',(0.11456465480888,1.79854745620502,6.53771292899801));
#50442=CARTESIAN_POINT('Ctrl Pts',(0.081371271700429,1.78729600772826,6.53575177434347));
#50443=CARTESIAN_POINT('Ctrl Pts',(0.0585390382962561,1.78222942980033,
6.53445747884568));
#50444=CARTESIAN_POINT('Ctrl Pts',(0.0287112392533252,1.7789367734667,6.53268686712636));
#50445=CARTESIAN_POINT('Ctrl Pts',(0.0220408696398692,1.7784100111886,6.53228638481466));
#50446=CARTESIAN_POINT('Ctrl Pts',(0.0143189535286426,1.77804157419437,
6.53181590634271));
#50447=CARTESIAN_POINT('Ctrl Pts',(0.0132783977728525,1.77799698061966,
6.53175236520624));
#50448=CARTESIAN_POINT('Ctrl Pts',(0.0117327741854933,1.77793824675036,
6.53165776474484));
#50449=CARTESIAN_POINT('Ctrl Pts',(0.011227852623753,1.77792024866939,6.53162682637236));
#50450=CARTESIAN_POINT('Ctrl Pts',(0.0103296500411853,1.7778903466729,6.53157172818916));
#50451=CARTESIAN_POINT('Ctrl Pts',(0.00993638474178478,1.77787797546184,
6.53154758307193));
#50452=CARTESIAN_POINT('Ctrl Pts',(0.00910965772366165,1.77785348395876,
6.53149678003822));
#50453=CARTESIAN_POINT('Ctrl Pts',(0.00867619251796588,1.7778415182836,
6.5314701173252));
#50454=CARTESIAN_POINT('Ctrl Pts',(0.00753656667565948,1.77781236096473,
6.53139994941154));
#50455=CARTESIAN_POINT('Ctrl Pts',(0.00683037423865473,1.77779661615768,
6.53135639896288));
#50456=CARTESIAN_POINT('Ctrl Pts',(0.00368471339536192,1.77773682887269,
6.53116209410805));
#50457=CARTESIAN_POINT('Ctrl Pts',(0.00124489460553541,1.77771816947155,
6.53101054687556));
#50458=CARTESIAN_POINT('Ctrl Pts',(-0.0165269742594732,1.77778405987537,
6.52990028164857));
#50459=CARTESIAN_POINT('Ctrl Pts',(-0.0318331850297289,1.77893493016606,
6.52890802311551));
#50460=CARTESIAN_POINT('Ctrl Pts',(-0.0501437711971647,1.78163402893598,
6.52767945594422));
#50461=CARTESIAN_POINT('Ctrl Pts',(-0.0532828805152529,1.78214433586042,
6.52746739989681));
#50462=CARTESIAN_POINT('Ctrl Pts',(-0.0589618837880661,1.78315402873722,
6.52708135720204));
#50463=CARTESIAN_POINT('Ctrl Pts',(-0.0615043211097875,1.78363772124545,
6.52690764804384));
#50464=CARTESIAN_POINT('Ctrl Pts',(-0.0661756015597744,1.78458485945539,
6.52658699788433));
#50465=CARTESIAN_POINT('Ctrl Pts',(-0.0683061159734176,1.78503937466598,
6.52644017877712));
#50466=CARTESIAN_POINT('Ctrl Pts',(-0.0876362694546695,1.789368548689,6.52510332449872));
#50467=CARTESIAN_POINT('Ctrl Pts',(-0.104495958698296,1.794627030072,6.52390086560803));
#50468=CARTESIAN_POINT('Ctrl Pts',(-0.122261377290685,1.80181268025934,
6.52263909205611));
#50469=CARTESIAN_POINT('Ctrl Pts',(-0.123677324419373,1.80239717474075,
6.52253857815013));
#50470=CARTESIAN_POINT('Ctrl Pts',(-0.125393920482938,1.80312014256981,
6.52241682921519));
#50471=CARTESIAN_POINT('Ctrl Pts',(-0.125698572189652,1.80324900338345,
6.52239522603158));
#50472=CARTESIAN_POINT('Ctrl Pts',(-0.126382642550114,1.80353959218792,
6.52234672794862));
#50473=CARTESIAN_POINT('Ctrl Pts',(-0.126761950886306,1.80370158024603,
6.52231984336279));
#50474=CARTESIAN_POINT('Ctrl Pts',(-0.127960824949597,1.80421629692631,
6.52223489401904));
#50475=CARTESIAN_POINT('Ctrl Pts',(-0.128779244231137,1.80457170410686,
6.52217693884462));
#50476=CARTESIAN_POINT('Ctrl Pts',(-0.130189726635036,1.8051911959381,6.52207713244787));
#50477=CARTESIAN_POINT('Ctrl Pts',(-0.130782484686598,1.805453674974,6.5220352115436));
#50478=CARTESIAN_POINT('Ctrl Pts',(-0.13521274680968,1.80743144848045,6.52172208842481));
#50479=CARTESIAN_POINT('Ctrl Pts',(-0.139017384045852,1.8092199880199,6.52145426517325));
#50480=CARTESIAN_POINT('Ctrl Pts',(-0.143272370870119,1.81132284899061,
6.5211568654486));
#50481=CARTESIAN_POINT('Ctrl Pts',(-0.143757981903908,1.81156437040699,
6.52112295564231));
#50482=CARTESIAN_POINT('Ctrl Pts',(-0.144491305824928,1.81193140525848,
6.52107179885324));
#50483=CARTESIAN_POINT('Ctrl Pts',(-0.144739466957916,1.81205601336108,
6.52105449587812));
#50484=CARTESIAN_POINT('Ctrl Pts',(-0.145170451377914,1.81227311969275,
6.52102446127536));
#50485=CARTESIAN_POINT('Ctrl Pts',(-0.145353347558678,1.81236547154656,
6.52101172045395));
#50486=CARTESIAN_POINT('Ctrl Pts',(-0.145720881774483,1.81255149486372,
6.52098612754868));
#50487=CARTESIAN_POINT('Ctrl Pts',(-0.145905517457611,1.81264516975367,
6.52097327575344));
#50488=CARTESIAN_POINT('Ctrl Pts',(-0.146353135063906,1.81287281113039,
6.52094213095631));
#50489=CARTESIAN_POINT('Ctrl Pts',(-0.146616024364182,1.81300696152606,
6.52092384957982));
#50490=CARTESIAN_POINT('Ctrl Pts',(-0.147462792210968,1.81344052781285,
6.52086499689225));
#50491=CARTESIAN_POINT('Ctrl Pts',(-0.148045945500632,1.81374136829523,
6.52082451482246));
#50492=CARTESIAN_POINT('Ctrl Pts',(-0.149413585612766,1.81445221142105,
6.52072967924024));
#50493=CARTESIAN_POINT('Ctrl Pts',(-0.150197314667897,1.81486367148941,
6.52067541496352));
#50494=CARTESIAN_POINT('Ctrl Pts',(-0.152905147709779,1.81629955416785,
6.5204881765639));
#50495=CARTESIAN_POINT('Ctrl Pts',(-0.154820594487153,1.81734029070577,
6.5203561646394));
#50496=CARTESIAN_POINT('Ctrl Pts',(-0.163287939903117,1.82205282611388,
6.5197738823267));
#50497=CARTESIAN_POINT('Ctrl Pts',(-0.169721322019515,1.82593381658319,
6.51933490045365));
#50498=CARTESIAN_POINT('Ctrl Pts',(-0.200372413392151,1.84591802950562,
6.51723139287794));
#50499=CARTESIAN_POINT('Ctrl Pts',(-0.222469960322216,1.86502329037212,
6.51566445214189));
#50500=CARTESIAN_POINT('Ctrl Pts',(-0.243555069483027,1.88893148170922,
6.51381768202279));
#50501=CARTESIAN_POINT('Ctrl Pts',(-0.245376823130721,1.8910521468113,6.51365484733399));
#50502=CARTESIAN_POINT('Ctrl Pts',(-0.248325045853791,1.89457584586999,
6.51338562341313));
#50503=CARTESIAN_POINT('Ctrl Pts',(-0.249467782282284,1.89596510855371,
6.5132798133605));
#50504=CARTESIAN_POINT('Ctrl Pts',(-0.254680453659486,1.90241158535197,
6.51279020298307));
#50505=CARTESIAN_POINT('Ctrl Pts',(-0.258608409855853,1.90758119530096,
6.51240137608929));
#50506=CARTESIAN_POINT('Ctrl Pts',(-0.262976867573813,1.91370612314425,
6.51194349605141));
#50507=CARTESIAN_POINT('Ctrl Pts',(-0.263572288430144,1.91454949402686,
6.511880509261));
#50508=CARTESIAN_POINT('Ctrl Pts',(-0.264452013394673,1.91580835611516,
6.51178657615299));
#50509=CARTESIAN_POINT('Ctrl Pts',(-0.264739416852172,1.91622168183999,
6.51175574829349));
#50510=CARTESIAN_POINT('Ctrl Pts',(-0.265249588533674,1.916959059108,6.51170077426023));
#50511=CARTESIAN_POINT('Ctrl Pts',(-0.265472734831055,1.91728284886455,
6.51167664253873));
#50512=CARTESIAN_POINT('Ctrl Pts',(-0.265941248375334,1.91796534145726,
6.51162579331938));
#50513=CARTESIAN_POINT('Ctrl Pts',(-0.266186483607361,1.9183241335785,6.51159907087729));
#50514=CARTESIAN_POINT('Ctrl Pts',(-0.266830828512369,1.91927094964538,
6.51152857719188));
#50515=CARTESIAN_POINT('Ctrl Pts',(-0.267228718532436,1.91985979719879,
6.51148475993368));
#50516=CARTESIAN_POINT('Ctrl Pts',(-0.269007101821032,1.9225105300736,6.51128761882485));
#50517=CARTESIAN_POINT('Ctrl Pts',(-0.270365672135567,1.92458695732144,
6.51113347339291));
#50518=CARTESIAN_POINT('Ctrl Pts',(-0.280185294478183,1.93998030029493,
6.5099925363232));
#50519=CARTESIAN_POINT('Ctrl Pts',(-0.287680961252544,1.95388485552828,
6.5089701615377));
#50520=CARTESIAN_POINT('Ctrl Pts',(-0.303379233991276,1.98893886939149,
6.50641705632829));
#50521=CARTESIAN_POINT('Ctrl Pts',(-0.310427924740421,2.01051284673528,
6.50486282108069));
#50522=CARTESIAN_POINT('Ctrl Pts',(-0.315478494361835,2.0341452786251,6.50325608655099));
#50523=CARTESIAN_POINT('Ctrl Pts',(-0.315788123068088,2.03564639730103,
6.50315445543284));
#50524=CARTESIAN_POINT('Ctrl Pts',(-0.317795972171665,2.04574427959782,
6.50247388880638));
#50525=CARTESIAN_POINT('Ctrl Pts',(-0.319153847160087,2.05440594942296,
6.50190508699605));
#50526=CARTESIAN_POINT('Ctrl Pts',(-0.320238466186652,2.06381980468292,
6.50131044081574));
#50527=CARTESIAN_POINT('Ctrl Pts',(-0.320317555548087,2.0645268356471,6.50126592293545));
#50528=CARTESIAN_POINT('Ctrl Pts',(-0.320424842001705,2.06551556307584,
6.50120387381596));
#50529=CARTESIAN_POINT('Ctrl Pts',(-0.320455009451085,2.06579703695569,
6.50118623277031));
#50530=CARTESIAN_POINT('Ctrl Pts',(-0.320506518066305,2.06628368270037,
6.50115577349179));
#50531=CARTESIAN_POINT('Ctrl Pts',(-0.320528033126031,2.06648883535089,
6.50114294542723));
#50532=CARTESIAN_POINT('Ctrl Pts',(-0.320570840292977,2.06690082758617,
6.50111720908857));
#50533=CARTESIAN_POINT('Ctrl Pts',(-0.320592129157454,2.06710766680324,
6.50110430106405));
#50534=CARTESIAN_POINT('Ctrl Pts',(-0.320635302441027,2.06753115540728,
6.5010778987879));
#50535=CARTESIAN_POINT('Ctrl Pts',(-0.320657167529375,2.06774780699946,
6.5010644056214));
#50536=CARTESIAN_POINT('Ctrl Pts',(-0.320707432770591,2.06825096719705,
6.5010331005255));
#50537=CARTESIAN_POINT('Ctrl Pts',(-0.320735668654021,2.06853749258546,
6.50101529785008));
#50538=CARTESIAN_POINT('Ctrl Pts',(-0.32080799544783,2.06928164960522,6.50096912274472));
#50539=CARTESIAN_POINT('Ctrl Pts',(-0.320851491318806,2.06973934040992,
6.50094078339405));
#50540=CARTESIAN_POINT('Ctrl Pts',(-0.321807863194267,2.08003680381599,
6.50030451225739));
#50541=CARTESIAN_POINT('Ctrl Pts',(-0.3222687483972,2.08991429204376,6.49972142836674));
#50542=CARTESIAN_POINT('Ctrl Pts',(-0.322274936831736,2.09979822016873,
6.49915140185063));
#50543=CARTESIAN_POINT('',(-0.322023435600497,2.1002684890243,6.24937721618673));
#50544=CARTESIAN_POINT('Ctrl Pts',(-0.322274936536932,2.09979774986705,
6.49915142897391));
#50545=CARTESIAN_POINT('Ctrl Pts',(-0.322289363947956,2.1227870695989,6.49782558650495));
#50546=CARTESIAN_POINT('Ctrl Pts',(-0.319843928885221,2.14571420094704,
6.49657169036954));
#50547=CARTESIAN_POINT('Ctrl Pts',(-0.311612842615433,2.1837356855591,6.49436792214443));
#50548=CARTESIAN_POINT('Ctrl Pts',(-0.307100997708914,2.1990106369823,6.49344757464164));
#50549=CARTESIAN_POINT('Ctrl Pts',(-0.300599370908085,2.21622138617848,
6.49233807854255));
#50550=CARTESIAN_POINT('Ctrl Pts',(-0.299691227544351,2.21854349408354,
6.49218683954317));
#50551=CARTESIAN_POINT('Ctrl Pts',(-0.298489281371814,2.22151473715201,
6.49199125054724));
#50552=CARTESIAN_POINT('Ctrl Pts',(-0.298220127618156,2.22217380205915,
6.49194773412867));
#50553=CARTESIAN_POINT('Ctrl Pts',(-0.297783047106699,2.22323401151387,
6.49187751631622));
#50554=CARTESIAN_POINT('Ctrl Pts',(-0.29761648725322,2.22363571996017,6.49185086128474));
#50555=CARTESIAN_POINT('Ctrl Pts',(-0.297297790657745,2.22439997540648,
6.49180005427881));
#50556=CARTESIAN_POINT('Ctrl Pts',(-0.297145802414634,2.22476258379937,
6.49177590738404));
#50557=CARTESIAN_POINT('Ctrl Pts',(-0.296797891151552,2.22558837668843,
6.49172082201667));
#50558=CARTESIAN_POINT('Ctrl Pts',(-0.296601547063761,2.22605138169038,
6.49168986926025));
#50559=CARTESIAN_POINT('Ctrl Pts',(-0.295999851158662,2.22746106958395,
6.49159542179813));
#50560=CARTESIAN_POINT('Ctrl Pts',(-0.295591047716872,2.22840626392683,
6.49153180952966));
#50561=CARTESIAN_POINT('Ctrl Pts',(-0.292594228172048,2.23524505768283,
6.49106945889191));
#50562=CARTESIAN_POINT('Ctrl Pts',(-0.289834848081017,2.24106154398097,
6.49066486721432));
#50563=CARTESIAN_POINT('Ctrl Pts',(-0.286125349130607,2.24831175802512,
6.49014545875881));
#50564=CARTESIAN_POINT('Ctrl Pts',(-0.285335305315419,2.24982608701353,
6.49003612210623));
#50565=CARTESIAN_POINT('Ctrl Pts',(-0.2835144315212,2.2532496338463,6.48978699802224));
#50566=CARTESIAN_POINT('Ctrl Pts',(-0.282476290661486,2.25515485175525,
6.48964697498925));
#50567=CARTESIAN_POINT('Ctrl Pts',(-0.2677530676533,2.28153759911828,6.48768865786246));
#50568=CARTESIAN_POINT('Ctrl Pts',(-0.250950017996872,2.30413538369285,
6.48576277429686));
#50569=CARTESIAN_POINT('Ctrl Pts',(-0.225800962349839,2.33008861624592,
6.48334496710722));
#50570=CARTESIAN_POINT('Ctrl Pts',(-0.219943703483876,2.3356939382323,6.48280894383016));
#50571=CARTESIAN_POINT('Ctrl Pts',(-0.211651583520814,2.34305074571383,
6.48209278810084));
#50572=CARTESIAN_POINT('Ctrl Pts',(-0.2093947969536,2.34499771068934,6.48190196452543));
#50573=CARTESIAN_POINT('Ctrl Pts',(-0.20625844784051,2.34762848635439,6.48164269728681));
#50574=CARTESIAN_POINT('Ctrl Pts',(-0.20540194377157,2.34833939707171,6.48157248912644));
#50575=CARTESIAN_POINT('Ctrl Pts',(-0.203933791101918,2.34954519314751,
6.48145318042146));
#50576=CARTESIAN_POINT('Ctrl Pts',(-0.203323988830277,2.35004229676827,
6.48140392726026));
#50577=CARTESIAN_POINT('Ctrl Pts',(-0.202464492465143,2.35073772468319,
6.48133493731194));
#50578=CARTESIAN_POINT('Ctrl Pts',(-0.202216321377405,2.35093791395315,
6.48131506734327));
#50579=CARTESIAN_POINT('Ctrl Pts',(-0.20180856549008,2.35126583592247,6.48128250298456));
#50580=CARTESIAN_POINT('Ctrl Pts',(-0.201649156285479,2.35139378508009,
6.48126979291162));
#50581=CARTESIAN_POINT('Ctrl Pts',(-0.20131603602293,2.35166064200735,6.48124327588829));
#50582=CARTESIAN_POINT('Ctrl Pts',(-0.201142302867778,2.35179952162991,
6.48122947102099));
#50583=CARTESIAN_POINT('Ctrl Pts',(-0.200759863460464,2.352104589456,6.48119913610942));
#50584=CARTESIAN_POINT('Ctrl Pts',(-0.200551093888112,2.3522706989385,6.48118261176222));
#50585=CARTESIAN_POINT('Ctrl Pts',(-0.199825873323962,2.35284625831607,
6.48112533067243));
#50586=CARTESIAN_POINT('Ctrl Pts',(-0.199308368275348,2.35325438663055,
6.48108466831767));
#50587=CARTESIAN_POINT('Ctrl Pts',(-0.194190853107202,2.3572648932811,6.48068461575392));
#50588=CARTESIAN_POINT('Ctrl Pts',(-0.189494583313289,2.36074341045987,
6.48033378367909));
#50589=CARTESIAN_POINT('Ctrl Pts',(-0.18447679041442,2.36425284793337,6.47997265898156));
#50590=CARTESIAN_POINT('Ctrl Pts',(-0.18424739863405,2.36441283996816,6.47995617935902));
#50591=CARTESIAN_POINT('Ctrl Pts',(-0.175526387870635,2.37047855350393,
6.47933076280088));
#50592=CARTESIAN_POINT('Ctrl Pts',(-0.166754906978743,2.37597281329973,
6.47874137675951));
#50593=CARTESIAN_POINT('Ctrl Pts',(-0.151404828794657,2.38458817026186,
6.47774971628733));
#50594=CARTESIAN_POINT('Ctrl Pts',(-0.144957628901577,2.38792557628404,
6.47734441041212));
#50595=CARTESIAN_POINT('Ctrl Pts',(-0.123511210229985,2.39812426725498,
6.47601701437642));
#50596=CARTESIAN_POINT('Ctrl Pts',(-0.108098394190558,2.40405226722575,
6.47509403400635));
#50597=CARTESIAN_POINT('Ctrl Pts',(-0.0841368473669129,2.41121499016093,
6.47364181076376));
#50598=CARTESIAN_POINT('Ctrl Pts',(-0.0758800500399938,2.41333046198254,
6.47313873599704));
#50599=CARTESIAN_POINT('Ctrl Pts',(-0.065080345361436,2.41564553192866,
6.4724727765412));
#50600=CARTESIAN_POINT('Ctrl Pts',(-0.0626049803084835,2.41614580348251,
6.4723196109083));
#50601=CARTESIAN_POINT('Ctrl Pts',(-0.0594214273306145,2.41675034502254,
6.47212187386891));
#50602=CARTESIAN_POINT('Ctrl Pts',(-0.0587183723840552,2.41688142865982,
6.47207815888319));
#50603=CARTESIAN_POINT('Ctrl Pts',(-0.0575864055162117,2.41708858584607,
6.47200769746833));
#50604=CARTESIAN_POINT('Ctrl Pts',(-0.0571577627961288,2.41716613237124,
6.47198099798796));
#50605=CARTESIAN_POINT('Ctrl Pts',(-0.0563420881641146,2.41731199029763,
6.47193015652836));
#50606=CARTESIAN_POINT('Ctrl Pts',(-0.0559550856398134,2.41738046328375,
6.47190601973988));
#50607=CARTESIAN_POINT('Ctrl Pts',(-0.0550738918905029,2.41753471249628,
6.47185102706832));
#50608=CARTESIAN_POINT('Ctrl Pts',(-0.0545796246052274,2.41762004310414,
6.47182015707875));
#50609=CARTESIAN_POINT('Ctrl Pts',(-0.0531099387033823,2.4178702387132,
6.4717282931277));
#50610=CARTESIAN_POINT('Ctrl Pts',(-0.0521339646449518,2.41803176562116,
6.47166719333083));
#50611=CARTESIAN_POINT('Ctrl Pts',(-0.0453603506710568,2.41912080335949,
6.47124245674088));
#50612=CARTESIAN_POINT('Ctrl Pts',(-0.039539377326593,2.41989416823157,
6.47087396350974));
#50613=CARTESIAN_POINT('Ctrl Pts',(-0.0320972914708534,2.42067668959275,
6.47039798598908));
#50614=CARTESIAN_POINT('Ctrl Pts',(-0.0304925402671953,2.42083325919869,
6.47029506547638));
#50615=CARTESIAN_POINT('Ctrl Pts',(-0.00503455224490297,2.42312437534797,
6.46865778193836));
#50616=CARTESIAN_POINT('Ctrl Pts',(0.0189791195497994,2.42260524840724,
6.4670418216056));
#50617=CARTESIAN_POINT('Ctrl Pts',(0.0533982698818474,2.41800330445526,
6.46469280613183));
#50618=CARTESIAN_POINT('Ctrl Pts',(0.0640095259891257,2.41603841596354,
6.46396537252836));
#50619=CARTESIAN_POINT('Ctrl Pts',(0.0803395995316524,2.41215816008537,
6.46285722129163));
#50620=CARTESIAN_POINT('Ctrl Pts',(0.0861370094362089,2.41060842480609,
6.46246615024676));
#50621=CARTESIAN_POINT('Ctrl Pts',(0.0936712751173715,2.40836719794631,
6.46196386841972));
#50622=CARTESIAN_POINT('Ctrl Pts',(0.0954498318041072,2.40782132241288,
6.4618457402919));
#50623=CARTESIAN_POINT('Ctrl Pts',(0.0979746948723314,2.40702240211754,
6.46167877253147));
#50624=CARTESIAN_POINT('Ctrl Pts',(0.0987249161520031,2.40678198643061,
6.46162925285656));
#50625=CARTESIAN_POINT('Ctrl Pts',(0.100041727193081,2.40635467089282,6.46154250567203));
#50626=CARTESIAN_POINT('Ctrl Pts',(0.100608689968227,2.40616894531293,6.46150521197922));
#50627=CARTESIAN_POINT('Ctrl Pts',(0.101444892264135,2.40589244871556,6.46145029433889));
#50628=CARTESIAN_POINT('Ctrl Pts',(0.101714528609893,2.40580289570055,6.46143259919309));
#50629=CARTESIAN_POINT('Ctrl Pts',(0.102182880734432,2.40564665619653,6.46140188658492));
#50630=CARTESIAN_POINT('Ctrl Pts',(0.102381650135989,2.40558013233155,6.46138885946049));
#50631=CARTESIAN_POINT('Ctrl Pts',(0.102778272056816,2.40544696103385,6.4613628801426));
#50632=CARTESIAN_POINT('Ctrl Pts',(0.102976124204597,2.40538031543671,6.46134992788447));
#50633=CARTESIAN_POINT('Ctrl Pts',(0.103451033522702,2.40521983037496,6.4613188555992));
#50634=CARTESIAN_POINT('Ctrl Pts',(0.103728028562485,2.4051258056657,6.46130074659236));
#50635=CARTESIAN_POINT('Ctrl Pts',(0.104731721777431,2.40478358185627,6.46123517860861));
#50636=CARTESIAN_POINT('Ctrl Pts',(0.105457667747819,2.40453316019308,6.46118785025016));
#50637=CARTESIAN_POINT('Ctrl Pts',(0.118774015255495,2.39988623847911,6.4603213181985));
#50638=CARTESIAN_POINT('Ctrl Pts',(0.131082250697227,2.3947143772435,6.45954705233825));
#50639=CARTESIAN_POINT('Ctrl Pts',(0.150001398865264,2.38534395801593,6.45834743941981));
#50640=CARTESIAN_POINT('Ctrl Pts',(0.156839893794392,2.38164312183618,6.45791176460744));
#50641=CARTESIAN_POINT('Ctrl Pts',(0.17600601978327,2.37035609647484,6.4566677193847));
#50642=CARTESIAN_POINT('Ctrl Pts',(0.187965092694424,2.36218245694159,6.45586235071449));
#50643=CARTESIAN_POINT('Ctrl Pts',(0.210828236076154,2.34418559972121,6.45419992600459));
#50644=CARTESIAN_POINT('Ctrl Pts',(0.221691605684149,2.33436701470591,6.4533442289927));
#50645=CARTESIAN_POINT('Ctrl Pts',(0.232718862428239,2.32294544660744,6.45237948023086));
#50646=CARTESIAN_POINT('Ctrl Pts',(0.233582651805598,2.3220402796776,6.45230322449737));
#50647=CARTESIAN_POINT('Ctrl Pts',(0.234814839582412,2.32073391982234,6.4521934472704));
#50648=CARTESIAN_POINT('Ctrl Pts',(0.235187533489121,2.3203367793488,6.4521601107745));
#50649=CARTESIAN_POINT('Ctrl Pts',(0.235831879751446,2.31964667022975,6.45210224407062));
#50650=CARTESIAN_POINT('Ctrl Pts',(0.236103998133837,2.31935413675837,6.45207773388347));
#50651=CARTESIAN_POINT('Ctrl Pts',(0.236625699030957,2.3187912009022,6.4520306041917));
#50652=CARTESIAN_POINT('Ctrl Pts',(0.23687536394108,2.31852087541046,6.4520079882547));
#50653=CARTESIAN_POINT('Ctrl Pts',(0.237461728223945,2.31788380188759,6.45195472683323));
#50654=CARTESIAN_POINT('Ctrl Pts',(0.237798041090985,2.31751670084144,6.45192406499543));
#50655=CARTESIAN_POINT('Ctrl Pts',(0.238786863962891,2.31643232079314,6.45183357720972));
#50656=CARTESIAN_POINT('Ctrl Pts',(0.239436984592098,2.31571287922061,6.45177365044802));
#50657=CARTESIAN_POINT('Ctrl Pts',(0.245103592139093,2.30938487503538,6.45124747350817));
#50658=CARTESIAN_POINT('Ctrl Pts',(0.249925100396565,2.30360556382501,6.45077314818341));
#50659=CARTESIAN_POINT('Ctrl Pts',(0.2561745967295,2.29555781066855,6.45012003526765));
#50660=CARTESIAN_POINT('Ctrl Pts',(0.257783316577663,2.29343226817753,6.44994821312508));
#50661=CARTESIAN_POINT('Ctrl Pts',(0.268732731424178,2.2785859954076,6.4487527531376));
#50662=CARTESIAN_POINT('Ctrl Pts',(0.277153410662394,2.26521539087319,6.44769796780946));
#50663=CARTESIAN_POINT('Ctrl Pts',(0.292006516322775,2.23727706702139,6.44556054302719));
#50664=CARTESIAN_POINT('Ctrl Pts',(0.298408762742111,2.22273973513529,6.44448080440771));
#50665=CARTESIAN_POINT('Ctrl Pts',(0.306201657860934,2.20078200736725,6.44294094298618));
#50666=CARTESIAN_POINT('Ctrl Pts',(0.30844565149192,2.19368974073746,6.44245705377273));
#50667=CARTESIAN_POINT('Ctrl Pts',(0.310751821596372,2.18541550831121,6.44191275565621));
#50668=CARTESIAN_POINT('Ctrl Pts',(0.31105527515164,2.18430373406987,6.44184003792293));
#50669=CARTESIAN_POINT('Ctrl Pts',(0.311495732869811,2.18265525261129,6.44173285732982));
#50670=CARTESIAN_POINT('Ctrl Pts',(0.311637323649435,2.18211979602763,6.44169814306428));
#50671=CARTESIAN_POINT('Ctrl Pts',(0.311891230656627,2.18114947675622,6.4416354203436));
#50672=CARTESIAN_POINT('Ctrl Pts',(0.312004019164279,2.18071474071982,6.44160738526735));
#50673=CARTESIAN_POINT('Ctrl Pts',(0.312178744652064,2.18003543378289,6.44156368427713));
#50674=CARTESIAN_POINT('Ctrl Pts',(0.312241303321947,2.17979102564959,6.44154798245798));
#50675=CARTESIAN_POINT('Ctrl Pts',(0.312352297791932,2.17935525599371,6.44152002516878));
#50676=CARTESIAN_POINT('Ctrl Pts',(0.312400844535814,2.17916392438202,6.44150776328692));
#50677=CARTESIAN_POINT('Ctrl Pts',(0.312511908507595,2.17872450774421,6.44147963266823));
#50678=CARTESIAN_POINT('Ctrl Pts',(0.312574306001454,2.17847639331306,6.44146377097749));
#50679=CARTESIAN_POINT('Ctrl Pts',(0.312744756837474,2.17779519223009,6.44142028256408));
#50680=CARTESIAN_POINT('Ctrl Pts',(0.312852206493233,2.17736195293195,6.44139269079699));
#50681=CARTESIAN_POINT('Ctrl Pts',(0.31337600675642,2.17523104042144,6.44125729990608));
#50682=CARTESIAN_POINT('Ctrl Pts',(0.313779451004771,2.17353018089215,6.4411502333291));
#50683=CARTESIAN_POINT('Ctrl Pts',(0.322172721522925,2.13681780770209,6.43885909545669));
#50684=CARTESIAN_POINT('Ctrl Pts',(0.324270547994527,2.10071170233846,6.43697061180949));
#50685=CARTESIAN_POINT('Ctrl Pts',(0.3190658519913,2.05307430468784,6.43421870425496));
#50686=CARTESIAN_POINT('Ctrl Pts',(0.317098679172003,2.04123421732518,6.43351545444353));
#50687=CARTESIAN_POINT('Ctrl Pts',(0.314017085343398,2.0274820025562,6.43266362593403));
#50688=CARTESIAN_POINT('Ctrl Pts',(0.313537656528364,2.02543642004531,6.43253601057297));
#50689=CARTESIAN_POINT('Ctrl Pts',(0.312879375934788,2.02274640081529,6.43236694271357));
#50690=CARTESIAN_POINT('Ctrl Pts',(0.312718463593273,2.02209759317205,6.43232606902748));
#50691=CARTESIAN_POINT('Ctrl Pts',(0.312451903445196,2.02103694261136,6.43225909099663));
#50692=CARTESIAN_POINT('Ctrl Pts',(0.312347456591276,2.02062479759457,6.43223302548911));
#50693=CARTESIAN_POINT('Ctrl Pts',(0.312144153118055,2.01982918160539,6.43218263140641));
#50694=CARTESIAN_POINT('Ctrl Pts',(0.312045404632114,2.01944568358178,6.43215830636888));
#50695=CARTESIAN_POINT('Ctrl Pts',(0.311816733873345,2.01856435166032,6.43210232449799));
#50696=CARTESIAN_POINT('Ctrl Pts',(0.31168632601449,2.01806664589657,6.43207065198851));
#50697=CARTESIAN_POINT('Ctrl Pts',(0.311279085370032,2.01652744167327,6.43197251945149));
#50698=CARTESIAN_POINT('Ctrl Pts',(0.310998222106825,2.01548702594509,6.4319059288978));
#50699=CARTESIAN_POINT('Ctrl Pts',(0.308619378795712,2.00684741570483,6.43135078062598));
#50700=CARTESIAN_POINT('Ctrl Pts',(0.30624859182181,1.99932672990657,6.43085337694266));
#50701=CARTESIAN_POINT('Ctrl Pts',(0.302544833359033,1.98892442792998,6.43014446820187));
#50702=CARTESIAN_POINT('Ctrl Pts',(0.301441327045913,1.98596367161763,6.42994027856186));
#50703=CARTESIAN_POINT('Ctrl Pts',(0.289729204402164,1.95589804664805,6.42784213712809));
#50704=CARTESIAN_POINT('Ctrl Pts',(0.27553841285741,1.93033407979231,6.42583467983948));
#50705=CARTESIAN_POINT('Ctrl Pts',(0.252410612194767,1.89939891360368,6.42326561523751));
#50706=CARTESIAN_POINT('Ctrl Pts',(0.246370783741228,1.89202551100613,6.42264255788634));
#50707=CARTESIAN_POINT('Ctrl Pts',(0.239388787016557,1.88423378888635,6.42198153092982));
#50708=CARTESIAN_POINT('Ctrl Pts',(0.238762010188218,1.88354041543885,6.42192268431332));
#50709=CARTESIAN_POINT('Ctrl Pts',(0.237812022163772,1.88249863550182,6.42183424717789));
#50710=CARTESIAN_POINT('Ctrl Pts',(0.237491048838352,1.88214820824095,6.42180449560569));
#50711=CARTESIAN_POINT('Ctrl Pts',(0.236969991577548,1.88158185659127,6.42175640783133));
#50712=CARTESIAN_POINT('Ctrl Pts',(0.236770386300256,1.88136549574404,6.42173803611027));
#50713=CARTESIAN_POINT('Ctrl Pts',(0.236387188681781,1.88095127138636,6.42170286201616));
#50714=CARTESIAN_POINT('Ctrl Pts',(0.236203643794556,1.88075336458777,6.42168605607586));
#50715=CARTESIAN_POINT('Ctrl Pts',(0.235873870837986,1.88039868251449,6.42165593637765));
#50716=CARTESIAN_POINT('Ctrl Pts',(0.235727735165243,1.88024182276808,6.42164261559855));
#50717=CARTESIAN_POINT('Ctrl Pts',(0.23541250002525,1.87990413054572,6.42161393787557));
#50718=CARTESIAN_POINT('Ctrl Pts',(0.235243349137294,1.87972334756804,6.42159858502973));
#50719=CARTESIAN_POINT('Ctrl Pts',(0.234785797049737,1.8792354588778,6.42155715015281));
#50720=CARTESIAN_POINT('Ctrl Pts',(0.234497000445035,1.87892872212735,6.4215310985218));
#50721=CARTESIAN_POINT('Ctrl Pts',(0.233209516047678,1.87756662028266,6.42141540193207));
#50722=CARTESIAN_POINT('Ctrl Pts',(0.232204279171961,1.87651742862455,6.42132625397931));
#50723=CARTESIAN_POINT('Ctrl Pts',(0.212037763859331,1.85575209211646,6.41956038104622));
#50724=CARTESIAN_POINT('Ctrl Pts',(0.190434914493815,1.83855755336527,6.41806487081776));
#50725=CARTESIAN_POINT('Ctrl Pts',(0.148069031379972,1.81290819384524,6.41528504843489));
#50726=CARTESIAN_POINT('Ctrl Pts',(0.128114465860215,1.80346567503014,6.41402550333459));
#50727=CARTESIAN_POINT('Ctrl Pts',(0.106273995211203,1.79574956375146,6.4126168923438));
#50728=CARTESIAN_POINT('Ctrl Pts',(0.105190986995312,1.79537343153075,6.41254698449813));
#50729=CARTESIAN_POINT('Ctrl Pts',(0.103608682969578,1.79483333638086,6.41244475381663));
#50730=CARTESIAN_POINT('Ctrl Pts',(0.103110948141975,1.79466480035996,6.41241258236234));
#50731=CARTESIAN_POINT('Ctrl Pts',(0.102237098729272,1.79437129004487,6.41235607607454));
#50732=CARTESIAN_POINT('Ctrl Pts',(0.101861160679929,1.79424579046548,6.41233175864732));
#50733=CARTESIAN_POINT('Ctrl Pts',(0.101131038889841,1.79400354957456,6.4122845152467));
#50734=CARTESIAN_POINT('Ctrl Pts',(0.100776881961416,1.79388672887274,6.41226159193578));
#50735=CARTESIAN_POINT('Ctrl Pts',(0.0999313076776484,1.7936094377871,6.41220684346942));
#50736=CARTESIAN_POINT('Ctrl Pts',(0.0994397065629825,1.79344953495224,
6.41217499967255));
#50737=CARTESIAN_POINT('Ctrl Pts',(0.0979533280768954,1.79297001305426,
6.41207867482322));
#50738=CARTESIAN_POINT('Ctrl Pts',(0.0969573863139982,1.7926540506804,6.41201407372568));
#50739=CARTESIAN_POINT('Ctrl Pts',(0.0864537241506893,1.78937790048161,
6.41133210771968));
#50740=CARTESIAN_POINT('Ctrl Pts',(0.0768161575802389,1.78685534040216,
6.41070049103915));
#50741=CARTESIAN_POINT('Ctrl Pts',(0.0432147845312039,1.77970497602335,
6.40847516740393));
#50742=CARTESIAN_POINT('Ctrl Pts',(0.0188544607156668,1.77735373049607,
6.40681451785875));
#50743=CARTESIAN_POINT('Ctrl Pts',(-0.0136818548719435,1.77791242859161,
6.40462002506499));
#50744=CARTESIAN_POINT('Ctrl Pts',(-0.0218227583717758,1.77836141819219,
6.40407378936623));
#50745=CARTESIAN_POINT('Ctrl Pts',(-0.0372070247184155,1.77979677079254,
6.40305602296137));
#50746=CARTESIAN_POINT('Ctrl Pts',(-0.0444513346089827,1.78072180071052,
6.40258294040968));
#50747=CARTESIAN_POINT('Ctrl Pts',(-0.0528487570085928,1.78208548568207,
6.40204645032855));
#50748=CARTESIAN_POINT('Ctrl Pts',(-0.0540378743147184,1.78228544606827,
6.40197076139817));
#50749=CARTESIAN_POINT('Ctrl Pts',(-0.0555968006123472,1.78255659851908,
6.40187192742467));
#50750=CARTESIAN_POINT('Ctrl Pts',(-0.0559676266981874,1.7826217680002,
6.4018484468026));
#50751=CARTESIAN_POINT('Ctrl Pts',(-0.0565722364219961,1.78272911554425,
6.4018102117882));
#50752=CARTESIAN_POINT('Ctrl Pts',(-0.0568060877925933,1.78277090226825,
6.40179543512127));
#50753=CARTESIAN_POINT('Ctrl Pts',(-0.0572577912522653,1.78285213230937,
6.40176691603119));
#50754=CARTESIAN_POINT('Ctrl Pts',(-0.0574756483474143,1.78289154144508,
6.40175317174224));
#50755=CARTESIAN_POINT('Ctrl Pts',(-0.057981157954074,1.78298352337026,
6.40172130394564));
#50756=CARTESIAN_POINT('Ctrl Pts',(-0.0582687806467032,1.78303626337387,
6.40170319002785));
#50757=CARTESIAN_POINT('Ctrl Pts',(-0.0592004356534144,1.78320840750382,
6.40164457365094));
#50758=CARTESIAN_POINT('Ctrl Pts',(-0.0598441811182826,1.78332938459364,
6.40160416048426));
#50759=CARTESIAN_POINT('Ctrl Pts',(-0.0660960446177321,1.78452402286641,
6.40121250573043));
#50760=CARTESIAN_POINT('Ctrl Pts',(-0.0716754831360531,1.78574466721573,
6.40086943519134));
#50761=CARTESIAN_POINT('Ctrl Pts',(-0.0783162065420704,1.78738358582074,
6.40046569052639));
#50762=CARTESIAN_POINT('Ctrl Pts',(-0.0794110545744859,1.78765990476213,
6.40039927628031));
#50763=CARTESIAN_POINT('Ctrl Pts',(-0.110914987317835,1.79578726019632,
6.39849198513312));
#50764=CARTESIAN_POINT('Ctrl Pts',(-0.140017630672197,1.80803591730383,
6.39681510435875));
#50765=CARTESIAN_POINT('Ctrl Pts',(-0.176445759980808,1.83008737510312,
6.39436148348804));
#50766=CARTESIAN_POINT('Ctrl Pts',(-0.185692775037244,1.83636372811502,
6.39370477741718));
#50767=CARTESIAN_POINT('Ctrl Pts',(-0.196197495324445,1.84432097985333,
6.39290782572882));
#50768=CARTESIAN_POINT('Ctrl Pts',(-0.197788841202085,1.84555001959808,
6.39278565573822));
#50769=CARTESIAN_POINT('Ctrl Pts',(-0.199885105265159,1.84720056850615,
6.39262275541329));
#50770=CARTESIAN_POINT('Ctrl Pts',(-0.200400407015625,1.84760886559082,
6.3925825517828));
#50771=CARTESIAN_POINT('Ctrl Pts',(-0.201244982773947,1.84828227865517,
6.39251639385029));
#50772=CARTESIAN_POINT('Ctrl Pts',(-0.201574992636699,1.84854647214339,
6.39249047655854));
#50773=CARTESIAN_POINT('Ctrl Pts',(-0.202213892193419,1.84906001709925,
6.39244017060201));
#50774=CARTESIAN_POINT('Ctrl Pts',(-0.202522843000473,1.84930929160616,
6.39241578506164));
#50775=CARTESIAN_POINT('Ctrl Pts',(-0.203235752530189,1.84988667497086,
6.39235937744638));
#50776=CARTESIAN_POINT('Ctrl Pts',(-0.203639377825494,1.85021519210044,
6.39232733891551));
#50777=CARTESIAN_POINT('Ctrl Pts',(-0.204720997214866,1.85109990366835,
6.39224120657079));
#50778=CARTESIAN_POINT('Ctrl Pts',(-0.205397516209399,1.85165788724983,
6.39218704025213));
#50779=CARTESIAN_POINT('Ctrl Pts',(-0.210202059126783,1.85565366990804,
6.39180024885751));
#50780=CARTESIAN_POINT('Ctrl Pts',(-0.214245623151399,1.85919127499756,
6.39146355010964));
#50781=CARTESIAN_POINT('Ctrl Pts',(-0.218658434380346,1.86325107192618,
6.39108306711187));
#50782=CARTESIAN_POINT('Ctrl Pts',(-0.219116933460809,1.86367536029479,
6.39104337295234));
#50783=CARTESIAN_POINT('Ctrl Pts',(-0.221004000953644,1.86543183777833,
6.39087933353415));
#50784=CARTESIAN_POINT('Ctrl Pts',(-0.222421653920957,1.86677564713456,
6.39075451176141));
#50785=CARTESIAN_POINT('Ctrl Pts',(-0.226398825430387,1.87061489704599,
6.39039978941472));
#50786=CARTESIAN_POINT('Ctrl Pts',(-0.228929106863807,1.87314009584905,
6.39016869218125));
#50787=CARTESIAN_POINT('Ctrl Pts',(-0.232813196038101,1.87714754406849,
6.3898053799369));
#50788=CARTESIAN_POINT('Ctrl Pts',(-0.234196096327211,1.87860128822133,
6.38967426757451));
#50789=CARTESIAN_POINT('Ctrl Pts',(-0.252435623848281,1.89813731121435,
6.38792149041848));
#50790=CARTESIAN_POINT('Ctrl Pts',(-0.267169934448722,1.91808716056105,
6.38622603546088));
#50791=CARTESIAN_POINT('Ctrl Pts',(-0.283870766547797,1.94717197893642,
6.38398110724936));
#50792=CARTESIAN_POINT('Ctrl Pts',(-0.287948435399427,1.95500089705326,
6.38339766794261));
#50793=CARTESIAN_POINT('Ctrl Pts',(-0.293371144050865,1.9665458887325,6.38257633250866));
#50794=CARTESIAN_POINT('Ctrl Pts',(-0.29497720647738,1.97013438056736,6.38232630887702));
#50795=CARTESIAN_POINT('Ctrl Pts',(-0.29672909443182,1.97424900613177,6.38204631038258));
#50796=CARTESIAN_POINT('Ctrl Pts',(-0.296939644058674,1.97474699309961,
6.38201253285904));
#50797=CARTESIAN_POINT('Ctrl Pts',(-0.297254733445657,1.97549749497851,
6.38196179616467));
#50798=CARTESIAN_POINT('Ctrl Pts',(-0.297360205501846,1.97574961369193,
6.3819447805662));
#50799=CARTESIAN_POINT('Ctrl Pts',(-0.297549354402469,1.97620337250346,
6.38191420793582));
#50800=CARTESIAN_POINT('Ctrl Pts',(-0.297633146883127,1.97640496303552,
6.38190064386266));
#50801=CARTESIAN_POINT('Ctrl Pts',(-0.297812644013417,1.97683804387409,
6.38187154339523));
#50802=CARTESIAN_POINT('Ctrl Pts',(-0.297908283341287,1.97706955995891,
6.38185601103669));
#50803=CARTESIAN_POINT('Ctrl Pts',(-0.298164842522028,1.97769267579839,
6.38181427067643));
#50804=CARTESIAN_POINT('Ctrl Pts',(-0.298325261497764,1.97808448324068,
6.38178809313983));
#50805=CARTESIAN_POINT('Ctrl Pts',(-0.299057220305958,1.97988231537185,
6.38166828372946));
#50806=CARTESIAN_POINT('Ctrl Pts',(-0.299619607448771,1.981292080205,6.38157519757541));
#50807=CARTESIAN_POINT('Ctrl Pts',(-0.311833799180416,2.01254988000695,
6.37952915335565));
#50808=CARTESIAN_POINT('Ctrl Pts',(-0.31898197133815,2.04397181165803,6.37781852027982));
#50809=CARTESIAN_POINT('Ctrl Pts',(-0.32197094173668,2.08389069771,6.37554919832595));
#50810=CARTESIAN_POINT('Ctrl Pts',(-0.322270983047103,2.09186371415243,
6.3750922213039));
#50811=CARTESIAN_POINT('Ctrl Pts',(-0.322279658999331,2.10926320332244,
6.37407818456919));
#50812=CARTESIAN_POINT('Ctrl Pts',(-0.321871004133448,2.11868196904564,
6.37351846291403));
#50813=CARTESIAN_POINT('Ctrl Pts',(-0.320950643579636,2.12920908232873,
6.37287583992183));
#50814=CARTESIAN_POINT('Ctrl Pts',(-0.320844865489146,2.13034894299608,
6.37280603558363));
#50815=CARTESIAN_POINT('Ctrl Pts',(-0.320682259757542,2.13200521485414,
6.3727042757247));
#50816=CARTESIAN_POINT('Ctrl Pts',(-0.320630252085865,2.13252209930841,
6.37267247192477));
#50817=CARTESIAN_POINT('Ctrl Pts',(-0.320536314002029,2.13343358338143,
6.37261630494672));
#50818=CARTESIAN_POINT('Ctrl Pts',(-0.320494904022522,2.13382823650577,
6.37259195820381));
#50819=CARTESIAN_POINT('Ctrl Pts',(-0.320407835250848,2.13464352397203,
6.37254160435922));
#50820=CARTESIAN_POINT('Ctrl Pts',(-0.320362076807994,2.13506414670125,
6.37251559416221));
#50821=CARTESIAN_POINT('Ctrl Pts',(-0.320242916052121,2.13613979511352,
6.37244899730391));
#50822=CARTESIAN_POINT('Ctrl Pts',(-0.320168332558716,2.13679468560369,
6.3724083734769));
#50823=CARTESIAN_POINT('Ctrl Pts',(-0.3198565238103,2.13945981690589,6.37224273265895));
#50824=CARTESIAN_POINT('Ctrl Pts',(-0.319602374762253,2.14146799633634,
6.3721171829437));
#50825=CARTESIAN_POINT('Ctrl Pts',(-0.315139226506289,2.1742514267203,6.37005515926047));
#50826=CARTESIAN_POINT('Ctrl Pts',(-0.30652227252851,2.20425532833066,6.36796452482249));
#50827=CARTESIAN_POINT('Ctrl Pts',(-0.287706828389105,2.24595206613429,
6.36487206179435));
#50828=CARTESIAN_POINT('Ctrl Pts',(-0.280751059027885,2.25892183637936,
6.36388439727701));
#50829=CARTESIAN_POINT('Ctrl Pts',(-0.270935901922103,2.27455378561885,
6.36269663883162));
#50830=CARTESIAN_POINT('Ctrl Pts',(-0.268882762962979,2.27770016838185,
6.36245776004872));
#50831=CARTESIAN_POINT('Ctrl Pts',(-0.266447994067274,2.28129253084408,
6.3621859000184));
#50832=CARTESIAN_POINT('Ctrl Pts',(-0.266119706461407,2.28177408266266,
6.36214947607037));
#50833=CARTESIAN_POINT('Ctrl Pts',(-0.265630751533016,2.28248714713907,
6.36209557159766));
#50834=CARTESIAN_POINT('Ctrl Pts',(-0.265471086269037,2.28271934048574,
6.36207802368417));
#50835=CARTESIAN_POINT('Ctrl Pts',(-0.265186701639432,2.28313174746536,
6.36204686528725));
#50836=CARTESIAN_POINT('Ctrl Pts',(-0.26506210303209,2.28331204323071,6.36203324659469));
#50837=CARTESIAN_POINT('Ctrl Pts',(-0.264797766878953,2.28369370799222,
6.36200442415109));
#50838=CARTESIAN_POINT('Ctrl Pts',(-0.264657983892939,2.28389504414937,
6.36198922362599));
#50839=CARTESIAN_POINT('Ctrl Pts',(-0.264283631773973,2.2844329305986,6.36194862406341));
#50840=CARTESIAN_POINT('Ctrl Pts',(-0.264048648522266,2.28476919421489,
6.36192325335017));
#50841=CARTESIAN_POINT('Ctrl Pts',(-0.262935523687632,2.28635562791608,
6.36180360319612));
#50842=CARTESIAN_POINT('Ctrl Pts',(-0.26204912287177,2.28760001890148,6.36170988098252));
#50843=CARTESIAN_POINT('Ctrl Pts',(-0.254759027443678,2.29768186609809,
6.36095121166694));
#50844=CARTESIAN_POINT('Ctrl Pts',(-0.247918305474229,2.30619614527469,
6.36031453124));
#50845=CARTESIAN_POINT('Ctrl Pts',(-0.221175995114525,2.33622095573845,
6.35801732521308));
#50846=CARTESIAN_POINT('Ctrl Pts',(-0.198803623089132,2.35533585936913,
6.35643548996213));
#50847=CARTESIAN_POINT('Ctrl Pts',(-0.166364232920986,2.37616999642665,
6.3541870180284));
#50848=CARTESIAN_POINT('Ctrl Pts',(-0.158361285235065,2.38083554485971,
6.35363676609995));
#50849=CARTESIAN_POINT('Ctrl Pts',(-0.149160794628448,2.38568082134411,
6.35300439204209));
#50850=CARTESIAN_POINT('Ctrl Pts',(-0.148149664534789,2.38620648347659,
6.35293490006585));
#50851=CARTESIAN_POINT('Ctrl Pts',(-0.146674435006571,2.38696350747775,
6.35283351235944));
#50852=CARTESIAN_POINT('Ctrl Pts',(-0.146212523763191,2.38719913370041,
6.35280176677961));
#50853=CARTESIAN_POINT('Ctrl Pts',(-0.145396268924729,2.38761303508169,
6.3527456676773));
#50854=CARTESIAN_POINT('Ctrl Pts',(-0.145042160231166,2.38779177319614,
6.35272133046359));
#50855=CARTESIAN_POINT('Ctrl Pts',(-0.144309311028023,2.38815998632901,
6.35267096224757));
#50856=CARTESIAN_POINT('Ctrl Pts',(-0.143930525399679,2.38834936938715,
6.35264492808395));
#50857=CARTESIAN_POINT('Ctrl Pts',(-0.142959678225297,2.38883237834536,
6.35257819932122));
#50858=CARTESIAN_POINT('Ctrl Pts',(-0.142367086900955,2.38912492963399,
6.35253746726808));
#50859=CARTESIAN_POINT('Ctrl Pts',(-0.139943062903458,2.39031236580648,
6.35237084018093));
#50860=CARTESIAN_POINT('Ctrl Pts',(-0.138104090918512,2.39119167288872,
6.35224440438688));
#50861=CARTESIAN_POINT('Ctrl Pts',(-0.107779265025426,2.40533965737482,
6.35015871170442));
#50862=CARTESIAN_POINT('Ctrl Pts',(-0.0775173176241014,2.41438635670066,
6.34804123372469));
#50863=CARTESIAN_POINT('Ctrl Pts',(-0.0318070638249608,2.42104209142762,
6.3449195645139));
#50864=CARTESIAN_POINT('Ctrl Pts',(-0.0170475108066564,2.42216328814894,
6.34392744061303));
#50865=CARTESIAN_POINT('Ctrl Pts',(0.00106464553053257,2.42229040994249,
6.34276534014247));
#50866=CARTESIAN_POINT('Ctrl Pts',(0.00439147682843307,2.42226225171435,
6.34255420930228));
#50867=CARTESIAN_POINT('Ctrl Pts',(0.00827210163636751,2.42216929679074,
6.34231110418144));
#50868=CARTESIAN_POINT('Ctrl Pts',(0.00882674113468483,2.42215457797767,
6.34227643394949));
#50869=CARTESIAN_POINT('Ctrl Pts',(0.00966123643497917,2.42213027572916,
6.34222438670926));
#50870=CARTESIAN_POINT('Ctrl Pts',(0.00994111865508915,2.42212175988608,
6.34220695027683));
#50871=CARTESIAN_POINT('Ctrl Pts',(0.0104398380334422,2.42210593497981,
6.34217591608274));
#50872=CARTESIAN_POINT('Ctrl Pts',(0.0106586786929119,2.42209876767379,
6.34216231035613));
#50873=CARTESIAN_POINT('Ctrl Pts',(0.0111235123960802,2.42208306953528,
6.34213343689633));
#50874=CARTESIAN_POINT('Ctrl Pts',(0.0113695023111731,2.4220744799382,6.34211817254844));
#50875=CARTESIAN_POINT('Ctrl Pts',(0.0120300751653904,2.42205065599475,
6.34207722319629));
#50876=CARTESIAN_POINT('Ctrl Pts',(0.0124446406956274,2.4220349028563,6.34205156737804));
#50877=CARTESIAN_POINT('Ctrl Pts',(0.0144357563873208,2.42195539151796,
6.34192854854323));
#50878=CARTESIAN_POINT('Ctrl Pts',(0.0160118895148559,2.42188085501084,
6.34183178158524));
#50879=CARTESIAN_POINT('Ctrl Pts',(0.0291487266945746,2.42116287107689,
6.34102988192683));
#50880=CARTESIAN_POINT('Ctrl Pts',(0.0406689722397397,2.41990832425369,
6.34035652100778));
#50881=CARTESIAN_POINT('Ctrl Pts',(0.0712823096949903,2.41489351435652,
6.3385890888098));
#50882=CARTESIAN_POINT('Ctrl Pts',(0.0901433877386156,2.41002147007769,
6.3375213288434));
#50883=CARTESIAN_POINT('Ctrl Pts',(0.125510873020275,2.3973825942262,6.33539743380953));
#50884=CARTESIAN_POINT('Ctrl Pts',(0.142023863982611,2.38985938489501,6.33434915493812));
#50885=CARTESIAN_POINT('Ctrl Pts',(0.158935555980923,2.3803610406494,6.33317096256294));
#50886=CARTESIAN_POINT('Ctrl Pts',(0.160051216314129,2.3797256372784,6.33309273768266));
#50887=CARTESIAN_POINT('Ctrl Pts',(0.161603927162409,2.37882898980609,6.33298315770425));
#50888=CARTESIAN_POINT('Ctrl Pts',(0.162044210829552,2.37857334503238,6.33295200507567));
#50889=CARTESIAN_POINT('Ctrl Pts',(0.162804168625354,2.37812967451918,6.3328980938153));
#50890=CARTESIAN_POINT('Ctrl Pts',(0.163124128291243,2.37794213775046,6.3328753529502));
#50891=CARTESIAN_POINT('Ctrl Pts',(0.163786368400199,2.37755244400827,6.33282819529313));
#50892=CARTESIAN_POINT('Ctrl Pts',(0.164128599818109,2.37735020527886,6.33280377555355));
#50893=CARTESIAN_POINT('Ctrl Pts',(0.164919533580994,2.37688083314492,6.33274722338193));
#50894=CARTESIAN_POINT('Ctrl Pts',(0.165367961644774,2.37661324186656,6.33271507428852));
#50895=CARTESIAN_POINT('Ctrl Pts',(0.166793355891906,2.37575795890948,6.33261260737066));
#50896=CARTESIAN_POINT('Ctrl Pts',(0.167767846575844,2.3751661771973,6.33254214002349));
#50897=CARTESIAN_POINT('Ctrl Pts',(0.170026989353347,2.37377779929526,6.3323778007028));
#50898=CARTESIAN_POINT('Ctrl Pts',(0.171309209826656,2.37297731590511,6.33228378641074));
#50899=CARTESIAN_POINT('Ctrl Pts',(0.184215586495756,2.36479318809067,6.33132987479509));
#50900=CARTESIAN_POINT('Ctrl Pts',(0.195359216269885,2.35668171262402,6.33044265522849));
#50901=CARTESIAN_POINT('Ctrl Pts',(0.223245723064859,2.33351278602647,6.3280488289331));
#50902=CARTESIAN_POINT('Ctrl Pts',(0.238990301411144,2.31737149432935,6.32650854239552));
#50903=CARTESIAN_POINT('Ctrl Pts',(0.258078878926114,2.29319843079551,6.324445706739));
#50904=CARTESIAN_POINT('Ctrl Pts',(0.262978786223548,2.28647391164881,6.32389487193158));
#50905=CARTESIAN_POINT('Ctrl Pts',(0.267744127801934,2.27937199541742,6.32334175700654));
#50906=CARTESIAN_POINT('Ctrl Pts',(0.267874690604353,2.27917695400555,6.32332658834258));
#50907=CARTESIAN_POINT('Ctrl Pts',(0.27039753737059,2.27539927513003,6.3230332138234));
#50908=CARTESIAN_POINT('Ctrl Pts',(0.272718109649788,2.2717689468539,6.32275860573346));
#50909=CARTESIAN_POINT('Ctrl Pts',(0.275250172934361,2.26762701504709,6.32245440266168));
#50910=CARTESIAN_POINT('Ctrl Pts',(0.27553383806854,2.26716033609556,6.32242025581485));
#50911=CARTESIAN_POINT('Ctrl Pts',(0.275960449211904,2.26645444945866,6.32236880226892));
#50912=CARTESIAN_POINT('Ctrl Pts',(0.276104271713305,2.26621577667878,6.32235143866574));
#50913=CARTESIAN_POINT('Ctrl Pts',(0.276353433279654,2.26580107846497,6.32232132806152));
#50914=CARTESIAN_POINT('Ctrl Pts',(0.276458913862855,2.26562513894909,6.32230857175316));
#50915=CARTESIAN_POINT('Ctrl Pts',(0.276679114865641,2.26525705159953,6.32228192260095));
#50916=CARTESIAN_POINT('Ctrl Pts',(0.276793803064095,2.2650648850963,6.32226803193974));
#50917=CARTESIAN_POINT('Ctrl Pts',(0.277067545918565,2.26460512606663,6.32223485068834));
#50918=CARTESIAN_POINT('Ctrl Pts',(0.277226413758572,2.26433742131742,6.32221557239331));
#50919=CARTESIAN_POINT('Ctrl Pts',(0.277763292041226,2.26342974536991,6.32215034909471));
#50920=CARTESIAN_POINT('Ctrl Pts',(0.278139479927671,2.26278869066561,6.3221045223025));
#50921=CARTESIAN_POINT('Ctrl Pts',(0.279029007384789,2.26126077845419,6.32199584751489));
#50922=CARTESIAN_POINT('Ctrl Pts',(0.279540345199131,2.2603727567268,6.32193312466767));
#50923=CARTESIAN_POINT('Ctrl Pts',(0.285609502903421,2.24971544777673,6.32118542955653));
#50924=CARTESIAN_POINT('Ctrl Pts',(0.290657480614463,2.23966313388838,6.32053074067335));
#50925=CARTESIAN_POINT('Ctrl Pts',(0.307691021756868,2.20079839090929,6.31810972396772));
#50926=CARTESIAN_POINT('Ctrl Pts',(0.315998018233188,2.17056521578605,6.31642829071561));
#50927=CARTESIAN_POINT('Ctrl Pts',(0.320708489629304,2.13252888794293,6.31417160182846));
#50928=CARTESIAN_POINT('Ctrl Pts',(0.321349871299121,2.12542267143638,6.31374510675447));
#50929=CARTESIAN_POINT('Ctrl Pts',(0.321815184075115,2.1172420641479,6.3132465153317));
#50930=CARTESIAN_POINT('Ctrl Pts',(0.321870207197683,2.11618243349123,6.31318178806824));
#50931=CARTESIAN_POINT('Ctrl Pts',(0.321943628742833,2.11461947965904,6.31308609547695));
#50932=CARTESIAN_POINT('Ctrl Pts',(0.321966082106739,2.1141163466198,6.31305525732445));
#50933=CARTESIAN_POINT('Ctrl Pts',(0.322004014199881,2.11321915231268,6.31300020562241));
#50934=CARTESIAN_POINT('Ctrl Pts',(0.32201994920617,2.11282511051667,6.31297600642531));
#50935=CARTESIAN_POINT('Ctrl Pts',(0.322049286528548,2.11206510588908,6.31292929184389));
#50936=CARTESIAN_POINT('Ctrl Pts',(0.32206278841824,2.11169914732651,6.31290677961988));
#50937=CARTESIAN_POINT('Ctrl Pts',(0.322097425426804,2.11071480315456,6.31284617771041));
#50938=CARTESIAN_POINT('Ctrl Pts',(0.322117403383106,2.11009638065918,6.31280805181309));
#50939=CARTESIAN_POINT('Ctrl Pts',(0.322186462863438,2.10774918364025,6.3126631456919));
#50940=CARTESIAN_POINT('Ctrl Pts',(0.322223408273475,2.10602010572221,6.31255598599726));
#50941=CARTESIAN_POINT('Ctrl Pts',(0.322363696864557,2.09548429232617,6.31190042859222));
#50942=CARTESIAN_POINT('Ctrl Pts',(0.322119898456523,2.08667741254037,6.31134122847299));
#50943=CARTESIAN_POINT('Ctrl Pts',(0.320150950356518,2.05804280162445,6.30948458001554));
#50944=CARTESIAN_POINT('Ctrl Pts',(0.316951020075525,2.03836479888312,6.30814505236117));
#50945=CARTESIAN_POINT('Ctrl Pts',(0.308328024362657,2.0051095425196,6.30582013776111));
#50946=CARTESIAN_POINT('Ctrl Pts',(0.30375910474414,1.99136838009444,6.30484155112728));
#50947=CARTESIAN_POINT('Ctrl Pts',(0.297808557870049,1.97682206575994,6.30381345685935));
#50948=CARTESIAN_POINT('Ctrl Pts',(0.2973281587744,1.97566695245521,6.30373187800446));
#50949=CARTESIAN_POINT('Ctrl Pts',(0.296446460770463,1.97358125757994,6.30358472483933));
#50950=CARTESIAN_POINT('Ctrl Pts',(0.296047477301656,1.97264972017492,6.30351905506936));
#50951=CARTESIAN_POINT('Ctrl Pts',(0.293905142099454,1.96771232457915,6.30317132926428));
#50952=CARTESIAN_POINT('Ctrl Pts',(0.292084759526937,1.96374010289443,6.30289277112668));
#50953=CARTESIAN_POINT('Ctrl Pts',(0.289922542997893,1.95926458837135,6.30258129785063));
#50954=CARTESIAN_POINT('Ctrl Pts',(0.289659511150677,1.95872401252002,6.30254371653472));
#50955=CARTESIAN_POINT('Ctrl Pts',(0.289268851825449,1.95792681771759,6.30248835755455));
#50956=CARTESIAN_POINT('Ctrl Pts',(0.289142394115857,1.95766963188854,6.30247050766336));
#50957=CARTESIAN_POINT('Ctrl Pts',(0.288918054098805,1.95721490889505,6.30243896534237));
#50958=CARTESIAN_POINT('Ctrl Pts',(0.288820312056765,1.95701730324721,6.30242526411675));
#50959=CARTESIAN_POINT('Ctrl Pts',(0.288615680003369,1.95660466344608,6.30239666572005));
#50960=CARTESIAN_POINT('Ctrl Pts',(0.288508752644802,1.9563896489195,6.30238177097953));
#50961=CARTESIAN_POINT('Ctrl Pts',(0.288228404409888,1.95582748840154,6.30234284625592));
#50962=CARTESIAN_POINT('Ctrl Pts',(0.288054596023228,1.95548053444977,6.30231884061697));
#50963=CARTESIAN_POINT('Ctrl Pts',(0.287292092145774,1.95396527499257,6.30221407492678));
#50964=CARTESIAN_POINT('Ctrl Pts',(0.286696901818601,1.95280022505996,6.30213371714956));
#50965=CARTESIAN_POINT('Ctrl Pts',(0.282244268729266,1.94421392047236,6.30154269059245));
#50966=CARTESIAN_POINT('Ctrl Pts',(0.278105951896118,1.93694100376658,6.301048716059));
#50967=CARTESIAN_POINT('Ctrl Pts',(0.259022180913485,1.90624685825345,6.29895737526667));
#50968=CARTESIAN_POINT('Ctrl Pts',(0.241366732071269,1.88465122610918,6.29745883793543));
#50969=CARTESIAN_POINT('Ctrl Pts',(0.21782893338931,1.86244433573146,6.29560241270325));
#50970=CARTESIAN_POINT('Ctrl Pts',(0.214432224574083,1.85937382421525,6.29533769621932));
#50971=CARTESIAN_POINT('Ctrl Pts',(0.204159274414884,1.85047771662669,6.29454429144009));
#50972=CARTESIAN_POINT('Ctrl Pts',(0.197103332379081,1.84486742183,6.29400843946359));
#50973=CARTESIAN_POINT('Ctrl Pts',(0.18890758960432,1.83889393195384,6.29339164215806));
#50974=CARTESIAN_POINT('Ctrl Pts',(0.187989603426542,1.83823223053052,6.29332263500699));
#50975=CARTESIAN_POINT('Ctrl Pts',(0.186647132462481,1.83727525638094,6.29322182521874));
#50976=CARTESIAN_POINT('Ctrl Pts',(0.186225384851042,1.83697614367072,6.29319017031004));
#50977=CARTESIAN_POINT('Ctrl Pts',(0.185479018731242,1.83644949936867,6.29313417676769));
#50978=CARTESIAN_POINT('Ctrl Pts',(0.185154696019132,1.83622154880967,6.29310985424618));
#50979=CARTESIAN_POINT('Ctrl Pts',(0.184530086419158,1.83578426082886,6.29306302803668));
#50980=CARTESIAN_POINT('Ctrl Pts',(0.184229861668978,1.83557483537439,6.29304052776248));
#50981=CARTESIAN_POINT('Ctrl Pts',(0.183436256789134,1.83502325419877,6.29298106982739));
#50982=CARTESIAN_POINT('Ctrl Pts',(0.182942277871348,1.83468196616198,6.29294407919581));
#50983=CARTESIAN_POINT('Ctrl Pts',(0.181125874256248,1.8334345047443,6.29280812841259));
#50984=CARTESIAN_POINT('Ctrl Pts',(0.17979766399946,1.83253683345691,6.29270884676044));
#50985=CARTESIAN_POINT('Ctrl Pts',(0.176537858695669,1.83036894756828,6.29246547064173));
#50986=CARTESIAN_POINT('Ctrl Pts',(0.17459920962841,1.82910955067247,6.29232097637716));
#50987=CARTESIAN_POINT('Ctrl Pts',(0.16721998492646,1.82442793531935,6.29177180417491));
#50988=CARTESIAN_POINT('Ctrl Pts',(0.161691296857596,1.82114806559705,6.29136199151765));
#50989=CARTESIAN_POINT('Ctrl Pts',(0.142508366477141,1.81053021890289,6.2899450487336));
#50990=CARTESIAN_POINT('Ctrl Pts',(0.128425929393326,1.80401339499451,6.2889119709889));
#50991=CARTESIAN_POINT('Ctrl Pts',(0.0908525249739169,1.78981347864258,
6.28620148156929));
#50992=CARTESIAN_POINT('Ctrl Pts',(0.0668471699242258,1.7837698255814,6.28450966927148));
#50993=CARTESIAN_POINT('Ctrl Pts',(0.0410026721338429,1.78034095792689,
6.28286230561994));
#50994=CARTESIAN_POINT('Ctrl Pts',(0.0396183514507363,1.78016643594321,
6.2827746048338));
#50995=CARTESIAN_POINT('Ctrl Pts',(0.0378211073686939,1.77995170447906,
6.28266147937228));
#50996=CARTESIAN_POINT('Ctrl Pts',(0.0374092058753349,1.77990329750398,
6.28263560274289));
#50997=CARTESIAN_POINT('Ctrl Pts',(0.0367771312134968,1.77983025232553,
6.28259597225865));
#50998=CARTESIAN_POINT('Ctrl Pts',(0.0365570261324934,1.7798050460309,6.28258218637196));
#50999=CARTESIAN_POINT('Ctrl Pts',(0.0361203580484547,1.77975549520529,
6.28255486543507));
#51000=CARTESIAN_POINT('Ctrl Pts',(0.035903797691152,1.77973114352368,6.28254133011345));
#51001=CARTESIAN_POINT('Ctrl Pts',(0.0354215485262551,1.77967741107197,
6.28251122033203));
#51002=CARTESIAN_POINT('Ctrl Pts',(0.0351558484881496,1.77964814126359,
6.28249465225606));
#51003=CARTESIAN_POINT('Ctrl Pts',(0.0343812071433696,1.77956378126819,
6.2824464094988));
#51004=CARTESIAN_POINT('Ctrl Pts',(0.033872167628838,1.7795095727663,6.2824147845349));
#51005=CARTESIAN_POINT('Ctrl Pts',(0.0302327759318581,1.77913077536966,
6.28218921576922));
#51006=CARTESIAN_POINT('Ctrl Pts',(0.0270978084068554,1.77885082807592,
6.28199773791169));
#51007=CARTESIAN_POINT('Ctrl Pts',(0.0210770887529826,1.77840198364539,
6.28163455904428));
#51008=CARTESIAN_POINT('Ctrl Pts',(0.0181922143148818,1.77822589866855,
6.28146253871198));
#51009=CARTESIAN_POINT('Ctrl Pts',(0.00674542941357853,1.77768166170732,
6.28078654124249));
#51010=CARTESIAN_POINT('Ctrl Pts',(-0.00182783710657208,1.77761623644072,
6.28029471906875));
#51011=CARTESIAN_POINT('Ctrl Pts',(-0.0127601962555898,1.7779690115748,
6.2796749766125));
#51012=CARTESIAN_POINT('Ctrl Pts',(-0.0151254562761947,1.77807143507532,
6.27954134026152));
#51013=CARTESIAN_POINT('Ctrl Pts',(-0.035332817951963,1.77916967762503,
6.27840198635974));
#51014=CARTESIAN_POINT('Ctrl Pts',(-0.0530643443972307,1.78162180121795,
6.27741600552117));
#51015=CARTESIAN_POINT('Ctrl Pts',(-0.0764141372474246,1.78685662211536,
6.2760537143401));
#51016=CARTESIAN_POINT('Ctrl Pts',(-0.0822882659357707,1.78834870190204,
6.27570562767723));
#51017=CARTESIAN_POINT('Ctrl Pts',(-0.0975895275659313,1.79269811925516,
6.27478022025353));
#51018=CARTESIAN_POINT('Ctrl Pts',(-0.106933168102199,1.79582335785212,
6.27419601582167));
#51019=CARTESIAN_POINT('Ctrl Pts',(-0.117090421518247,1.79974661618089,
6.27353391246958));
#51020=CARTESIAN_POINT('Ctrl Pts',(-0.118060561102096,1.80012675147904,
6.27347039791165));
#51021=CARTESIAN_POINT('Ctrl Pts',(-0.119508559791905,1.80070224482395,
6.27337517888793));
#51022=CARTESIAN_POINT('Ctrl Pts',(-0.1199878272125,1.80089405985021,6.27334359376837));
#51023=CARTESIAN_POINT('Ctrl Pts',(-0.120812344967181,1.80122635347103,
6.27328913600132));
#51024=CARTESIAN_POINT('Ctrl Pts',(-0.12115781729771,1.80136628143753,6.27326628198026));
#51025=CARTESIAN_POINT('Ctrl Pts',(-0.121870227687585,1.80165627140686,
6.27321907869855));
#51026=CARTESIAN_POINT('Ctrl Pts',(-0.122237133038708,1.80180641171921,
6.27319472681807));
#51027=CARTESIAN_POINT('Ctrl Pts',(-0.122962841890948,1.80210494146638,
6.27314647866278));
#51028=CARTESIAN_POINT('Ctrl Pts',(-0.123321656128986,1.80225330310456,
6.27312258336512));
#51029=CARTESIAN_POINT('Ctrl Pts',(-0.12450518139215,1.80274517064069,6.27304363414393));
#51030=CARTESIAN_POINT('Ctrl Pts',(-0.125328726679441,1.80309145513457,
6.27298848592717));
#51031=CARTESIAN_POINT('Ctrl Pts',(-0.130910950126545,1.80546603290428,
6.27261321932604));
#51032=CARTESIAN_POINT('Ctrl Pts',(-0.135621403141066,1.80760512208367,
6.27228933568671));
#51033=CARTESIAN_POINT('Ctrl Pts',(-0.146938836682586,1.81307685811564,
6.27149281764672));
#51034=CARTESIAN_POINT('Ctrl Pts',(-0.153486218056481,1.81652534845163,
6.27101634969844));
#51035=CARTESIAN_POINT('Ctrl Pts',(-0.167653070494215,1.82462173927933,
6.26995041910129));
#51036=CARTESIAN_POINT('Ctrl Pts',(-0.17520980331825,1.82936695576433,6.26935828932215));
#51037=CARTESIAN_POINT('Ctrl Pts',(-0.205956175787806,1.85050193397043,
6.26685635537638));
#51038=CARTESIAN_POINT('Ctrl Pts',(-0.227125413261808,1.8696059663331,6.2648908044307));
#51039=CARTESIAN_POINT('Ctrl Pts',(-0.246465487858104,1.89235107073042,
6.2630031230539));
#51040=CARTESIAN_POINT('Ctrl Pts',(-0.24740529161617,1.89347170555832,6.26291115855634));
#51041=CARTESIAN_POINT('Ctrl Pts',(-0.248606641161095,1.89492417992802,
6.26279333850767));
#51042=CARTESIAN_POINT('Ctrl Pts',(-0.248875189131882,1.89525016667402,
6.26276698409329));
#51043=CARTESIAN_POINT('Ctrl Pts',(-0.249300288299547,1.89576826081635,
6.26272524038679));
#51044=CARTESIAN_POINT('Ctrl Pts',(-0.249457258910454,1.89596002103976,
6.26270982062711));
#51045=CARTESIAN_POINT('Ctrl Pts',(-0.249738484227849,1.89630438432064,
6.26268218509296));
#51046=CARTESIAN_POINT('Ctrl Pts',(-0.249862819423746,1.89645691900402,
6.26266996345988));
#51047=CARTESIAN_POINT('Ctrl Pts',(-0.25015526323524,1.8968163614582,6.26264120926538));
#51048=CARTESIAN_POINT('Ctrl Pts',(-0.250323254646118,1.89702336370907,
6.26262468529031));
#51049=CARTESIAN_POINT('Ctrl Pts',(-0.250810941065243,1.89762582659935,
6.26257669598879));
#51050=CARTESIAN_POINT('Ctrl Pts',(-0.251129959032216,1.89802183805551,
6.26254527958115));
#51051=CARTESIAN_POINT('Ctrl Pts',(-0.253367222983191,1.90081255016796,
6.26232477166439));
#51052=CARTESIAN_POINT('Ctrl Pts',(-0.255252204521904,1.90323388603487,
6.26213802198015));
#51053=CARTESIAN_POINT('Ctrl Pts',(-0.260888244066879,1.91069093268913,
6.26157539141749));
#51054=CARTESIAN_POINT('Ctrl Pts',(-0.264527157038789,1.91580990058281,
6.26120616292196));
#51055=CARTESIAN_POINT('Ctrl Pts',(-0.280725121447392,1.94006727641345,
6.25951748273053));
#51056=CARTESIAN_POINT('Ctrl Pts',(-0.291372574948194,1.96040329119677,
6.25826853624167));
#51057=CARTESIAN_POINT('Ctrl Pts',(-0.300648402140433,1.98390795472358,
6.25684030201397));
#51058=CARTESIAN_POINT('Ctrl Pts',(-0.301496391502955,1.9861283601449,6.25670557691139));
#51059=CARTESIAN_POINT('Ctrl Pts',(-0.304477866575999,1.99420200716584,
6.25621597003656));
#51060=CARTESIAN_POINT('Ctrl Pts',(-0.306466006636432,2.00010721877873,
6.25585833992316));
#51061=CARTESIAN_POINT('Ctrl Pts',(-0.311173390847604,2.01555638927262,
6.25491908409505));
#51062=CARTESIAN_POINT('Ctrl Pts',(-0.313625064429223,2.0251742612823,6.25433068022026));
#51063=CARTESIAN_POINT('Ctrl Pts',(-0.31584005359885,2.03591157761723,6.25366403910757));
#51064=CARTESIAN_POINT('Ctrl Pts',(-0.316045986100183,2.03693495444631,
6.25360040732598));
#51065=CARTESIAN_POINT('Ctrl Pts',(-0.316346412621837,2.03846635198416,
6.25350504111151));
#51066=CARTESIAN_POINT('Ctrl Pts',(-0.316444664157109,2.0389736357102,6.2534734265395));
#51067=CARTESIAN_POINT('Ctrl Pts',(-0.316611713492429,2.03984738134122,
6.25341893149327));
#51068=CARTESIAN_POINT('Ctrl Pts',(-0.316681096289379,2.04021373148304,
6.25339606970442));
#51069=CARTESIAN_POINT('Ctrl Pts',(-0.316822923714335,2.04096977264355,
6.25334886296308));
#51070=CARTESIAN_POINT('Ctrl Pts',(-0.316895285480426,2.04135947842366,
6.25332451541268));
#51071=CARTESIAN_POINT('Ctrl Pts',(-0.317037084279483,2.04213106643138,
6.25327627990272));
#51072=CARTESIAN_POINT('Ctrl Pts',(-0.317106550720927,2.0425129425994,6.25325239292746));
#51073=CARTESIAN_POINT('Ctrl Pts',(-0.31726550323091,2.04339580334904,6.2531971354726));
#51074=CARTESIAN_POINT('Ctrl Pts',(-0.317354492658577,2.04389687527847,
6.25316574923566));
#51075=CARTESIAN_POINT('Ctrl Pts',(-0.317581153164674,2.04519092638957,
6.25308462777441));
#51076=CARTESIAN_POINT('Ctrl Pts',(-0.317717040598631,2.04598421073572,
6.25303483595291));
#51077=CARTESIAN_POINT('Ctrl Pts',(-0.320810706929163,2.064460057515,6.25187368436787));
#51078=CARTESIAN_POINT('Ctrl Pts',(-0.322290242970631,2.0823546240026,6.25071470024017));
#51079=CARTESIAN_POINT('Ctrl Pts',(-0.322274881613702,2.1002762351798,6.24952200414216));
#51080=CARTESIAN_POINT('',(-0.3227631030959,2.10004611274009,6.12435703103352));
#51081=CARTESIAN_POINT('Ctrl Pts',(-0.322798597665563,2.10004734253964,
6.12437741302984));
#51082=CARTESIAN_POINT('Ctrl Pts',(-0.322580086172827,1.99582903567067,
6.13084004242903));
#51083=CARTESIAN_POINT('Ctrl Pts',(-0.211048222901441,1.78439851022638,
6.14392611966916));
#51084=CARTESIAN_POINT('Ctrl Pts',(0.149287431151383,1.74938860369369,6.16363564475023));
#51085=CARTESIAN_POINT('Ctrl Pts',(0.375612323430391,2.03573126104505,6.18350598827301));
#51086=CARTESIAN_POINT('Ctrl Pts',(0.257364043962396,2.38103173698883,6.20337633179581));
#51087=CARTESIAN_POINT('Ctrl Pts',(-0.0969807088903252,2.46852385326159,
6.22324667531859));
#51088=CARTESIAN_POINT('Ctrl Pts',(-0.301768811357061,2.27515652580511,
6.2385803034489));
#51089=CARTESIAN_POINT('Ctrl Pts',(-0.322286541621404,2.13412944815347,
6.24729048373829));
#51090=CARTESIAN_POINT('Ctrl Pts',(-0.322023435600497,2.1002684890243,6.24937721618673));
#51091=CARTESIAN_POINT('',(-0.322274893287392,2.10011804807506,5.87466618688513));
#51092=CARTESIAN_POINT('Ctrl Pts',(-0.322274998677053,2.10002920112239,
6.1240767475264));
#51093=CARTESIAN_POINT('Ctrl Pts',(-0.322274898616863,2.10113350447985,
6.12400672680945));
#51094=CARTESIAN_POINT('Ctrl Pts',(-0.32226912256732,2.10223782043467,6.12393698681781));
#51095=CARTESIAN_POINT('Ctrl Pts',(-0.32224942848518,2.10413679398095,6.12381757158123));
#51096=CARTESIAN_POINT('Ctrl Pts',(-0.322238247202919,2.10493145967723,
6.12376775308541));
#51097=CARTESIAN_POINT('Ctrl Pts',(-0.322218942390711,2.10601779972598,
6.12369986631237));
#51098=CARTESIAN_POINT('Ctrl Pts',(-0.322213362324257,2.10630950792266,
6.12368165850064));
#51099=CARTESIAN_POINT('Ctrl Pts',(-0.322202897407712,2.10682030422494,
6.12364981362972));
#51100=CARTESIAN_POINT('Ctrl Pts',(-0.322198185229367,2.10703939508986,
6.12363616694993));
#51101=CARTESIAN_POINT('Ctrl Pts',(-0.322188586701757,2.10746545950735,
6.12360965235869));
#51102=CARTESIAN_POINT('Ctrl Pts',(-0.322183724369211,2.10767243370905,
6.12359678308214));
#51103=CARTESIAN_POINT('Ctrl Pts',(-0.322173653480351,2.10808421934652,
6.12357120111331));
#51104=CARTESIAN_POINT('Ctrl Pts',(-0.322168449070601,2.10828903030222,
6.12355848820197));
#51105=CARTESIAN_POINT('Ctrl Pts',(-0.322155731978818,2.10877137734158,
6.12352857351878));
#51106=CARTESIAN_POINT('Ctrl Pts',(-0.322148055939749,2.1090489094846,6.12351138097397));
#51107=CARTESIAN_POINT('Ctrl Pts',(-0.322124331639828,2.10986835962504,
6.12346067505366));
#51108=CARTESIAN_POINT('Ctrl Pts',(-0.322107274433623,2.11041025086683,
6.12342721795403));
#51109=CARTESIAN_POINT('Ctrl Pts',(-0.322063618093307,2.11169413423134,
6.12334811926339));
#51110=CARTESIAN_POINT('Ctrl Pts',(-0.322035822007876,2.11243608634034,
6.12330254295059));
#51111=CARTESIAN_POINT('Ctrl Pts',(-0.321948266027934,2.11457553263276,
6.12317149312285));
#51112=CARTESIAN_POINT('Ctrl Pts',(-0.321881970882867,2.11597276205806,
6.12308636392612));
#51113=CARTESIAN_POINT('Ctrl Pts',(-0.32011194219942,2.14876619021454,6.12109815840227));
#51114=CARTESIAN_POINT('Ctrl Pts',(-0.313831599476083,2.17975114258912,
6.11941763538675));
#51115=CARTESIAN_POINT('Ctrl Pts',(-0.29794204085832,2.22380738493369,6.11676031854832));
#51116=CARTESIAN_POINT('Ctrl Pts',(-0.291695607772656,2.23788150193843,
6.11586886754736));
#51117=CARTESIAN_POINT('Ctrl Pts',(-0.283320200627048,2.253612547653,6.11479381841947));
#51118=CARTESIAN_POINT('Ctrl Pts',(-0.28214693977033,2.25575703756126,6.11464552157857));
#51119=CARTESIAN_POINT('Ctrl Pts',(-0.280603125080307,2.25850413702551,
6.11445321684188));
#51120=CARTESIAN_POINT('Ctrl Pts',(-0.280254804239856,2.2591192004347,6.11441000824338));
#51121=CARTESIAN_POINT('Ctrl Pts',(-0.27968948582083,2.26010982254473,6.11434016804255));
#51122=CARTESIAN_POINT('Ctrl Pts',(-0.279473747274201,2.26048610013216,
6.11431358189952));
#51123=CARTESIAN_POINT('Ctrl Pts',(-0.279060869291288,2.2612028586807,6.11426282748151));
#51124=CARTESIAN_POINT('Ctrl Pts',(-0.27886386454668,2.26154341665432,6.11423866411277));
#51125=CARTESIAN_POINT('Ctrl Pts',(-0.278412547935586,2.26232031247752,
6.11418343116762));
#51126=CARTESIAN_POINT('Ctrl Pts',(-0.278157833480306,2.26275641418911,
6.1141523470256));
#51127=CARTESIAN_POINT('Ctrl Pts',(-0.277375219009772,2.26408914077643,
6.11405710833899));
#51128=CARTESIAN_POINT('Ctrl Pts',(-0.276844004867481,2.26498380274963,
6.11399283332681));
#51129=CARTESIAN_POINT('Ctrl Pts',(-0.272876742437086,2.27159228795988,
6.11351550439498));
#51130=CARTESIAN_POINT('Ctrl Pts',(-0.269268669897204,2.27720045869222,
6.11309616215871));
#51131=CARTESIAN_POINT('Ctrl Pts',(-0.264430243480757,2.28423168398243,
6.11255122659846));
#51132=CARTESIAN_POINT('Ctrl Pts',(-0.263357652006095,2.28576171282842,
6.11243144755916));
#51133=CARTESIAN_POINT('Ctrl Pts',(-0.261166401172612,2.28883036033382,
6.1121887821376));
#51134=CARTESIAN_POINT('Ctrl Pts',(-0.260047302936068,2.29036857432157,
6.11206588349018));
#51135=CARTESIAN_POINT('Ctrl Pts',(-0.257804110611697,2.29339517769355,
6.11182156540464));
#51136=CARTESIAN_POINT('Ctrl Pts',(-0.256680581279543,2.29488389668715,
6.11170016844418));
#51137=CARTESIAN_POINT('Ctrl Pts',(-0.238222666097382,2.31890481292924,
6.10972152273238));
#51138=CARTESIAN_POINT('Ctrl Pts',(-0.217997998291099,2.33905200559161,
6.1077600500686));
#51139=CARTESIAN_POINT('Ctrl Pts',(-0.188977541424347,2.36117772422409,
6.10533712570136));
#51140=CARTESIAN_POINT('Ctrl Pts',(-0.182377142941742,2.3658287334372,6.10480920820219));
#51141=CARTESIAN_POINT('Ctrl Pts',(-0.174371764272286,2.37103106641102,
6.10420180647337));
#51142=CARTESIAN_POINT('Ctrl Pts',(-0.173129480306708,2.37182629448551,
6.1041084563732));
#51143=CARTESIAN_POINT('Ctrl Pts',(-0.171320054569274,2.37296713255524,
6.1039738489586));
#51144=CARTESIAN_POINT('Ctrl Pts',(-0.170757256368001,2.37331954918914,
6.10393217031264));
#51145=CARTESIAN_POINT('Ctrl Pts',(-0.169877975506854,2.37386636705761,
6.10386735366194));
#51146=CARTESIAN_POINT('Ctrl Pts',(-0.169562243150448,2.37406196246232,
6.10384413924988));
#51147=CARTESIAN_POINT('Ctrl Pts',(-0.168969732293502,2.37442760559793,
6.10380068787249));
#51148=CARTESIAN_POINT('Ctrl Pts',(-0.168693033856916,2.37459778126547,
6.10378044258198));
#51149=CARTESIAN_POINT('Ctrl Pts',(-0.168225132829522,2.37488457662624,
6.10374628611977));
#51150=CARTESIAN_POINT('Ctrl Pts',(-0.168034065868195,2.3750014154346,6.10373236045696));
#51151=CARTESIAN_POINT('Ctrl Pts',(-0.167653623978817,2.37523351383682,
6.10370467664237));
#51152=CARTESIAN_POINT('Ctrl Pts',(-0.167464251707707,2.3753487773222,6.1036909182416));
#51153=CARTESIAN_POINT('Ctrl Pts',(-0.167041871855284,2.37560526647514,
6.10366027932226));
#51154=CARTESIAN_POINT('Ctrl Pts',(-0.166808803420858,2.37574639247744,
6.10364340539893));
#51155=CARTESIAN_POINT('Ctrl Pts',(-0.166005329703341,2.37623151490913,
6.10358534582964));
#51156=CARTESIAN_POINT('Ctrl Pts',(-0.165434032082281,2.37657404138233,
6.10354425613104));
#51157=CARTESIAN_POINT('Ctrl Pts',(-0.159353654254091,2.38019400411052,
6.10310893216183));
#51158=CARTESIAN_POINT('Ctrl Pts',(-0.153748564696659,2.38330841758884,
6.1027250154061));
#51159=CARTESIAN_POINT('Ctrl Pts',(-0.141208622479554,2.38979422418645,
6.1018954175983));
#51160=CARTESIAN_POINT('Ctrl Pts',(-0.134238177005032,2.39308820090093,
6.10145318747766));
#51161=CARTESIAN_POINT('Ctrl Pts',(-0.120689053002301,2.3989061051128,6.10061709886834));
#51162=CARTESIAN_POINT('Ctrl Pts',(-0.114132783964845,2.40147042849115,
6.10022260601275));
#51163=CARTESIAN_POINT('Ctrl Pts',(-0.105491723022323,2.4045278306303,6.09970990897851));
#51164=CARTESIAN_POINT('Ctrl Pts',(-0.103478779845182,2.40521770164515,
6.09959098089353));
#51165=CARTESIAN_POINT('Ctrl Pts',(-0.0991404590385739,2.40665666929372,
6.09933550552864));
#51166=CARTESIAN_POINT('Ctrl Pts',(-0.0968131012961575,2.40739936048031,
6.09919896541882));
#51167=CARTESIAN_POINT('Ctrl Pts',(-0.0917337361133889,2.40895684733647,
6.0989017312117));
#51168=CARTESIAN_POINT('Ctrl Pts',(-0.0889788427003446,2.4097614844295,
6.09874100001503));
#51169=CARTESIAN_POINT('Ctrl Pts',(-0.0771559418465538,2.41304392814447,
6.09805218602418));
#51170=CARTESIAN_POINT('Ctrl Pts',(-0.0679929879320068,2.41516103852153,
6.09752063192441));
#51171=CARTESIAN_POINT('Ctrl Pts',(-0.047621525561036,2.41893806387761,
6.09632756279444));
#51172=CARTESIAN_POINT('Ctrl Pts',(-0.036392189163703,2.42041358372475,
6.09566238885254));
#51173=CARTESIAN_POINT('Ctrl Pts',(-0.023088225797105,2.4214532924999,6.09485546277121));
#51174=CARTESIAN_POINT('Ctrl Pts',(-0.0210657145563982,2.42159216534073,
6.09473229336176));
#51175=CARTESIAN_POINT('Ctrl Pts',(-0.0183837091142796,2.42175091268301,
6.09456825937055));
#51176=CARTESIAN_POINT('Ctrl Pts',(-0.0177252411940359,2.42178785929176,
6.09452793087126));
#51177=CARTESIAN_POINT('Ctrl Pts',(-0.0166440726068344,2.4218451950262,
6.09446162017107));
#51178=CARTESIAN_POINT('Ctrl Pts',(-0.0162214347506905,2.42186677331827,
6.09443567531845));
#51179=CARTESIAN_POINT('Ctrl Pts',(-0.0154024481545931,2.4219069704978,
6.0943853535479));
#51180=CARTESIAN_POINT('Ctrl Pts',(-0.0150061049320919,2.42192568999189,
6.09436097983218));
#51181=CARTESIAN_POINT('Ctrl Pts',(-0.0140909762060335,2.42196721832163,
6.0943046541099));
#51182=CARTESIAN_POINT('Ctrl Pts',(-0.0135721691582012,2.42198950526922,
6.09427268579729));
#51183=CARTESIAN_POINT('Ctrl Pts',(-0.0119106150685491,2.42205685954152,
6.09417018609633));
#51184=CARTESIAN_POINT('Ctrl Pts',(-0.01076769074757,2.42209709764446,6.09409950357062));
#51185=CARTESIAN_POINT('Ctrl Pts',(-0.000240865812410066,2.42241161650631,
6.0934468237269));
#51186=CARTESIAN_POINT('Ctrl Pts',(0.00914973685938343,2.42228180401299,
6.09285221746115));
#51187=CARTESIAN_POINT('Ctrl Pts',(0.0486213469336585,2.42000968734767,
6.09029724669452));
#51188=CARTESIAN_POINT('Ctrl Pts',(0.0783280863433009,2.41406111751519,
6.0882193768987));
#51189=CARTESIAN_POINT('Ctrl Pts',(0.114232440335848,2.40145434908952,6.08568376177453));
#51190=CARTESIAN_POINT('Ctrl Pts',(0.121599176659267,2.3985589308198,6.08516340436872));
#51191=CARTESIAN_POINT('Ctrl Pts',(0.130888543138024,2.39450687539588,6.08451335216291));
#51192=CARTESIAN_POINT('Ctrl Pts',(0.132915518547507,2.39359764292307,6.08437189446203));
#51193=CARTESIAN_POINT('Ctrl Pts',(0.135748078563823,2.39229170425354,6.08417492564908));
#51194=CARTESIAN_POINT('Ctrl Pts',(0.136561602216125,2.39191250410641,6.08411843815546));
#51195=CARTESIAN_POINT('Ctrl Pts',(0.137790921447534,2.39133322927272,6.08403321714094));
#51196=CARTESIAN_POINT('Ctrl Pts',(0.138207880937534,2.39113565594891,6.08400433599126));
#51197=CARTESIAN_POINT('Ctrl Pts',(0.13888495529807,2.39081304665947,6.08395747856859));
#51198=CARTESIAN_POINT('Ctrl Pts',(0.139145327220876,2.39068855641331,6.08393946918626));
#51199=CARTESIAN_POINT('Ctrl Pts',(0.13964509880361,2.3904487779416,6.08390492045685));
#51200=CARTESIAN_POINT('Ctrl Pts',(0.139884523634199,2.39033354314735,6.08388837782777));
#51201=CARTESIAN_POINT('Ctrl Pts',(0.140316533203192,2.39012495917646,6.08385854477205));
#51202=CARTESIAN_POINT('Ctrl Pts',(0.140509167030384,2.39003171448762,6.08384524788853));
#51203=CARTESIAN_POINT('Ctrl Pts',(0.140927025622294,2.38982893540355,6.08381641696886));
#51204=CARTESIAN_POINT('Ctrl Pts',(0.141152214995471,2.38971933064744,6.08380088745265));
#51205=CARTESIAN_POINT('Ctrl Pts',(0.141757559941735,2.38942382227757,6.08375916212097));
#51206=CARTESIAN_POINT('Ctrl Pts',(0.142137479152578,2.38923743140782,6.08373299673318));
#51207=CARTESIAN_POINT('Ctrl Pts',(0.143876640267258,2.38837993328814,6.08361331388479));
#51208=CARTESIAN_POINT('Ctrl Pts',(0.145231532451431,2.38769997520186,6.08352034074589));
#51209=CARTESIAN_POINT('Ctrl Pts',(0.172013478160711,2.37402193517599,6.08168684957241));
#51210=CARTESIAN_POINT('Ctrl Pts',(0.195610944716856,2.35770840732004,6.08014059976619));
#51211=CARTESIAN_POINT('Ctrl Pts',(0.21970093544351,2.3358146653514,6.07830988589373));
#51212=CARTESIAN_POINT('Ctrl Pts',(0.222600108438508,2.33307991808217,6.07808494552923));
#51213=CARTESIAN_POINT('Ctrl Pts',(0.237489126892852,2.31850410163867,6.07690208155974));
#51214=CARTESIAN_POINT('Ctrl Pts',(0.248585689296406,2.30579154243007,6.07592233106721));
#51215=CARTESIAN_POINT('Ctrl Pts',(0.259336645921011,2.29132970403322,6.07482669604394));
#51216=CARTESIAN_POINT('Ctrl Pts',(0.260031314459109,2.29038452407359,6.07475517924895));
#51217=CARTESIAN_POINT('Ctrl Pts',(0.261032599098126,2.28900645280984,6.07465103015971));
#51218=CARTESIAN_POINT('Ctrl Pts',(0.261343336403448,2.28857655609296,6.07461855745714));
#51219=CARTESIAN_POINT('Ctrl Pts',(0.261884851598014,2.2878234751956,6.0745617017807));
#51220=CARTESIAN_POINT('Ctrl Pts',(0.262116096734501,2.28750062709616,6.07453733688364));
#51221=CARTESIAN_POINT('Ctrl Pts',(0.262562527474419,2.28687491223974,6.07449013265401));
#51222=CARTESIAN_POINT('Ctrl Pts',(0.262777787356236,2.28657209900929,6.07446729622688));
#51223=CARTESIAN_POINT('Ctrl Pts',(0.26328824182051,2.28585138988293,6.07441296299691));
#51224=CARTESIAN_POINT('Ctrl Pts',(0.263582965130955,2.28543316286551,6.07438144819709));
#51225=CARTESIAN_POINT('Ctrl Pts',(0.264622296203507,2.28395081617401,6.0742697990933));
#51226=CARTESIAN_POINT('Ctrl Pts',(0.265361458400782,2.28288290990497,6.07418945733113));
#51227=CARTESIAN_POINT('Ctrl Pts',(0.277759066222317,2.26473803186194,6.07282581644883));
#51228=CARTESIAN_POINT('Ctrl Pts',(0.28775159622199,2.2465859498543,6.07147846067998));
#51229=CARTESIAN_POINT('Ctrl Pts',(0.307045587093238,2.20184029626405,6.06821207150958));
#51230=CARTESIAN_POINT('Ctrl Pts',(0.314743218343517,2.17473457287738,6.06627012501356));
#51231=CARTESIAN_POINT('Ctrl Pts',(0.319018726307291,2.14571485425047,6.06440853122825));
#51232=CARTESIAN_POINT('Ctrl Pts',(0.319196788323489,2.1444545394894,6.06432812477893));
#51233=CARTESIAN_POINT('Ctrl Pts',(0.319447231821962,2.14260277756494,6.06421066551856));
#51234=CARTESIAN_POINT('Ctrl Pts',(0.319525444722583,2.14201215018338,6.06417330289743));
#51235=CARTESIAN_POINT('Ctrl Pts',(0.319646234143863,2.14108015289036,6.06411450918562));
#51236=CARTESIAN_POINT('Ctrl Pts',(0.319689902232793,2.14073892950041,6.06409301818327));
#51237=CARTESIAN_POINT('Ctrl Pts',(0.319771303055945,2.14009467071225,6.06405250745693));
#51238=CARTESIAN_POINT('Ctrl Pts',(0.319809151549059,2.13979165069384,6.06403348127638));
#51239=CARTESIAN_POINT('Ctrl Pts',(0.31986406256352,2.13934688662655,6.06400559614002));
#51240=CARTESIAN_POINT('Ctrl Pts',(0.319881461542806,2.13920518547679,6.06399671807524));
#51241=CARTESIAN_POINT('Ctrl Pts',(0.31992475544746,2.13885064283601,6.06397452009062));
#51242=CARTESIAN_POINT('Ctrl Pts',(0.319950531945824,2.13863778855871,6.06396120709976));
#51243=CARTESIAN_POINT('Ctrl Pts',(0.320009959259841,2.13814291891631,6.06393028741672));
#51244=CARTESIAN_POINT('Ctrl Pts',(0.320043449674723,2.13786088497024,6.06391268992212));
#51245=CARTESIAN_POINT('Ctrl Pts',(0.320145841709243,2.13698876329907,6.06385834746378));
#51246=CARTESIAN_POINT('Ctrl Pts',(0.320213485006274,2.13639852479885,6.06382167337149));
#51247=CARTESIAN_POINT('Ctrl Pts',(0.320725128806687,2.13182221295607,6.06353810997254));
#51248=CARTESIAN_POINT('Ctrl Pts',(0.321096340773843,2.12782813358008,6.0632952246199));
#51249=CARTESIAN_POINT('Ctrl Pts',(0.323652420562508,2.09335156088208,6.06123025031372));
#51250=CARTESIAN_POINT('Ctrl Pts',(0.321566044928294,2.06270473051419,6.05959456051045));
#51251=CARTESIAN_POINT('Ctrl Pts',(0.312168733057205,2.01862317056703,6.0570299914393));
#51252=CARTESIAN_POINT('Ctrl Pts',(0.308191371039751,2.00466110367454,6.05618687050992));
#51253=CARTESIAN_POINT('Ctrl Pts',(0.302760946680964,1.98954904935848,6.05521773809992));
#51254=CARTESIAN_POINT('Ctrl Pts',(0.302223416544587,1.98808659734486,6.055123360547));
#51255=CARTESIAN_POINT('Ctrl Pts',(0.301261419243848,1.98552678415206,6.05495709954516));
#51256=CARTESIAN_POINT('Ctrl Pts',(0.300841505221578,1.98442773451244,6.05488536835715));
#51257=CARTESIAN_POINT('Ctrl Pts',(0.300223320311237,1.98283594565119,6.05478096393333));
#51258=CARTESIAN_POINT('Ctrl Pts',(0.300029831274837,1.98234134953173,6.05474845139882));
#51259=CARTESIAN_POINT('Ctrl Pts',(0.299689489102198,1.98147766650431,6.05469154939092));
#51260=CARTESIAN_POINT('Ctrl Pts',(0.299543174120842,1.98110836761603,6.05466717808328));
#51261=CARTESIAN_POINT('Ctrl Pts',(0.299258755925108,1.98039435411291,6.05461997848561));
#51262=CARTESIAN_POINT('Ctrl Pts',(0.299120738862869,1.98004960564362,6.05459715313265));
#51263=CARTESIAN_POINT('Ctrl Pts',(0.298791401571291,1.97923106751874,6.05454287308536));
#51264=CARTESIAN_POINT('Ctrl Pts',(0.298599550252134,1.97875749388097,6.05451140047626));
#51265=CARTESIAN_POINT('Ctrl Pts',(0.297917581837151,1.97708553214206,6.0544000426733));
#51266=CARTESIAN_POINT('Ctrl Pts',(0.297421375003508,1.97588965559209,6.05431995143931));
#51267=CARTESIAN_POINT('Ctrl Pts',(0.289258050740357,1.95654587140993,6.05301716211879));
#51268=CARTESIAN_POINT('Ctrl Pts',(0.279951422758845,1.93913903503645,6.05173661004203));
#51269=CARTESIAN_POINT('Ctrl Pts',(0.267917009404502,1.92087322533996,6.05027353164486));
#51270=CARTESIAN_POINT('Ctrl Pts',(0.266699556357598,1.91906555946356,6.05012739444293));
#51271=CARTESIAN_POINT('Ctrl Pts',(0.264039097231468,1.91520052727369,6.0498121116476));
#51272=CARTESIAN_POINT('Ctrl Pts',(0.262590172888067,1.91314740873039,6.04964287749077));
#51273=CARTESIAN_POINT('Ctrl Pts',(0.251571583443207,1.89791543399322,6.04837467838568));
#51274=CARTESIAN_POINT('Ctrl Pts',(0.241039042175458,1.88546180525178,6.04726459935883));
#51275=CARTESIAN_POINT('Ctrl Pts',(0.223491816647637,1.86764551801355,6.0456066973702));
#51276=CARTESIAN_POINT('Ctrl Pts',(0.217123386040066,1.86168369121783,6.04503827155683));
#51277=CARTESIAN_POINT('Ctrl Pts',(0.209847767465566,1.85540670646291,6.04443154508124));
#51278=CARTESIAN_POINT('Ctrl Pts',(0.209172756613997,1.85482919691145,6.04437564307485));
#51279=CARTESIAN_POINT('Ctrl Pts',(0.208146156011534,1.85395820867236,6.04429122161121));
#51280=CARTESIAN_POINT('Ctrl Pts',(0.207796321034468,1.85366268185127,6.04426255776883));
#51281=CARTESIAN_POINT('Ctrl Pts',(0.207226096709322,1.85318305785927,6.04421600765573));
#51282=CARTESIAN_POINT('Ctrl Pts',(0.207006090655745,1.85299850907732,6.04419808886513));
#51283=CARTESIAN_POINT('Ctrl Pts',(0.206582817225344,1.85264441523491,6.0441636944625));
#51284=CARTESIAN_POINT('Ctrl Pts',(0.20637958719456,1.85247482617348,6.04414721564308));
#51285=CARTESIAN_POINT('Ctrl Pts',(0.206011739110834,1.85216863650514,6.04411745291724));
#51286=CARTESIAN_POINT('Ctrl Pts',(0.205847194409926,1.85203194976444,6.04410416268811));
#51287=CARTESIAN_POINT('Ctrl Pts',(0.205514161518965,1.85175586037013,6.04407731052548));
#51288=CARTESIAN_POINT('Ctrl Pts',(0.205345668240044,1.85161646596211,6.04406374918618));
#51289=CARTESIAN_POINT('Ctrl Pts',(0.204868163875743,1.85122224480677,6.04402538465059));
#51290=CARTESIAN_POINT('Ctrl Pts',(0.204558818052361,1.85096782133639,6.04400061093507));
#51291=CARTESIAN_POINT('Ctrl Pts',(0.203261494048787,1.84990487717544,6.04389704770142));
#51292=CARTESIAN_POINT('Ctrl Pts',(0.202269173123293,1.84910163979189,6.04381863644171));
#51293=CARTESIAN_POINT('Ctrl Pts',(0.18359681564177,1.83417002034061,6.04235760867634));
#51294=CARTESIAN_POINT('Ctrl Pts',(0.164478638829028,1.82193436586509,6.04110004981311));
#51295=CARTESIAN_POINT('Ctrl Pts',(0.129208477798294,1.80428286553856,6.03889556054818));
#51296=CARTESIAN_POINT('Ctrl Pts',(0.113619585297817,1.79795035378823,6.03795578657513));
#51297=CARTESIAN_POINT('Ctrl Pts',(0.0895193974025224,1.79029125458355,
6.03648707606282));
#51298=CARTESIAN_POINT('Ctrl Pts',(0.0813318235494002,1.78804111587925,
6.03598582363374));
#51299=CARTESIAN_POINT('Ctrl Pts',(0.0706213690562402,1.78554794455058,
6.03532271352782));
#51300=CARTESIAN_POINT('Ctrl Pts',(0.06817076142114,1.78500758789841,6.03517050621778));
#51301=CARTESIAN_POINT('Ctrl Pts',(0.0650155828222821,1.78435041774936,
6.034973837378));
#51302=CARTESIAN_POINT('Ctrl Pts',(0.0643165432968785,1.78420724037722,
6.0349302208678));
#51303=CARTESIAN_POINT('Ctrl Pts',(0.0631903630350583,1.7839804704168,6.03485988026399));
#51304=CARTESIAN_POINT('Ctrl Pts',(0.0627635156971211,1.78389541896251,
6.03483320282798));
#51305=CARTESIAN_POINT('Ctrl Pts',(0.0619508297192864,1.78373519822124,
6.0347823785058));
#51306=CARTESIAN_POINT('Ctrl Pts',(0.0615650229858371,1.78365986961872,
6.03475823675538));
#51307=CARTESIAN_POINT('Ctrl Pts',(0.0606859728769294,1.78348990447915,
6.03470319835396));
#51308=CARTESIAN_POINT('Ctrl Pts',(0.0601926450416233,1.78339571489164,
6.03467228750895));
#51309=CARTESIAN_POINT('Ctrl Pts',(0.0586904424509208,1.78311254184685,
6.03457809168736));
#51310=CARTESIAN_POINT('Ctrl Pts',(0.0576808905213132,1.78292722601983,
6.03451469006433));
#51311=CARTESIAN_POINT('Ctrl Pts',(0.0504045683259694,1.78162746737534,
6.03405700118663));
#51312=CARTESIAN_POINT('Ctrl Pts',(0.0441072663605818,1.78069414384619,
6.03365699270359));
#51313=CARTESIAN_POINT('Ctrl Pts',(0.0361042220939283,1.77974926804714,
6.03314320680647));
#51314=CARTESIAN_POINT('Ctrl Pts',(0.0344201255587868,1.77956388943266,
6.03303479003378));
#51315=CARTESIAN_POINT('Ctrl Pts',(0.028005107675333,1.77890890463891,6.03262066645843));
#51316=CARTESIAN_POINT('Ctrl Pts',(0.0232656360752081,1.77853074142744,
6.03231232921712));
#51317=CARTESIAN_POINT('Ctrl Pts',(-0.00681942210835438,1.77679902498352,
6.03034053974536));
#51318=CARTESIAN_POINT('Ctrl Pts',(-0.0322408423240995,1.77833925592178,
6.02859929749724));
#51319=CARTESIAN_POINT('Ctrl Pts',(-0.0659607766006114,1.78442218769125,
6.02630594916846));
#51320=CARTESIAN_POINT('Ctrl Pts',(-0.0746397359638249,1.78636148937369,
6.02571827721844));
#51321=CARTESIAN_POINT('Ctrl Pts',(-0.0869442518918768,1.78965072944109,
6.02489858896583));
#51322=CARTESIAN_POINT('Ctrl Pts',(-0.0906425813657495,1.79071065588619,
6.02465401329631));
#51323=CARTESIAN_POINT('Ctrl Pts',(-0.0948356343225887,1.79199404636649,
6.02437947101997));
#51324=CARTESIAN_POINT('Ctrl Pts',(-0.0953496345896853,1.7921527778189,
6.02434586406068));
#51325=CARTESIAN_POINT('Ctrl Pts',(-0.0961236252215004,1.79239392287948,
6.02429533226696));
#51326=CARTESIAN_POINT('Ctrl Pts',(-0.0963839091117196,1.79247537972893,
6.0242783516804));
#51327=CARTESIAN_POINT('Ctrl Pts',(-0.0968523120901613,1.79262262134587,
6.02424781686923));
#51328=CARTESIAN_POINT('Ctrl Pts',(-0.0970604672825517,1.79268828698317,
6.02423425568043));
#51329=CARTESIAN_POINT('Ctrl Pts',(-0.0974768055761168,1.79282009226945,
6.02420714811128));
#51330=CARTESIAN_POINT('Ctrl Pts',(-0.0976849872237315,1.79288623181229,
6.02419360179971));
#51331=CARTESIAN_POINT('Ctrl Pts',(-0.0982735534011247,1.79307387895018,
6.02415532701133));
#51332=CARTESIAN_POINT('Ctrl Pts',(-0.0986537812620749,1.79319588247947,
6.02413062779119));
#51333=CARTESIAN_POINT('Ctrl Pts',(-0.100239395561168,1.79370791020667,
6.02402773766455));
#51334=CARTESIAN_POINT('Ctrl Pts',(-0.10144272454605,1.79410434057707,6.02394991893403));
#51335=CARTESIAN_POINT('Ctrl Pts',(-0.123522920440769,1.80152316715299,
6.02252634616796));
#51336=CARTESIAN_POINT('Ctrl Pts',(-0.143631667616612,1.81066178225136,
6.02129917779544));
#51337=CARTESIAN_POINT('Ctrl Pts',(-0.167219570451243,1.82445187487074,
6.01977193663774));
#51338=CARTESIAN_POINT('Ctrl Pts',(-0.171719484167394,1.82723348412446,
6.01947642355334));
#51339=CARTESIAN_POINT('Ctrl Pts',(-0.194915174171536,1.84237341179173,
6.017922588068));
#51340=CARTESIAN_POINT('Ctrl Pts',(-0.21234955954777,1.85654400640881,6.01664255370566));
#51341=CARTESIAN_POINT('Ctrl Pts',(-0.228982619826251,1.8732193732273,6.01521028728399));
#51342=CARTESIAN_POINT('Ctrl Pts',(-0.229788786618955,1.87403627204184,
6.01514030420375));
#51343=CARTESIAN_POINT('Ctrl Pts',(-0.230957840826026,1.87523361510915,
6.01503798373026));
#51344=CARTESIAN_POINT('Ctrl Pts',(-0.231324194338672,1.87561067511062,
6.01500579809776));
#51345=CARTESIAN_POINT('Ctrl Pts',(-0.231965136335691,1.87627358613908,
6.01494927540759));
#51346=CARTESIAN_POINT('Ctrl Pts',(-0.232240123869646,1.87655905120806,
6.01492495578768));
#51347=CARTESIAN_POINT('Ctrl Pts',(-0.232772764683201,1.87711403213526,
6.01487771439952));
#51348=CARTESIAN_POINT('Ctrl Pts',(-0.233030478376079,1.87738348939204,
6.01485479530534));
#51349=CARTESIAN_POINT('Ctrl Pts',(-0.233644207721466,1.87802741880968,
6.01480006691302));
#51350=CARTESIAN_POINT('Ctrl Pts',(-0.233999790721992,1.87840230023941,
6.01476823900474));
#51351=CARTESIAN_POINT('Ctrl Pts',(-0.235070999297314,1.87953709946738,
6.01467199357934));
#51352=CARTESIAN_POINT('Ctrl Pts',(-0.235783830624478,1.88029963496426,
6.0146074562905));
#51353=CARTESIAN_POINT('Ctrl Pts',(-0.243231301159998,1.88834439308857,
6.0139279708177));
#51354=CARTESIAN_POINT('Ctrl Pts',(-0.249629361385848,1.8959296471515,6.01329888364502));
#51355=CARTESIAN_POINT('Ctrl Pts',(-0.265389497456274,1.91646628861794,
6.01162228023401));
#51356=CARTESIAN_POINT('Ctrl Pts',(-0.274155777794372,1.92983915337881,
6.01055499286846));
#51357=CARTESIAN_POINT('Ctrl Pts',(-0.28945346325023,1.95744777940985,6.0084227322202));
#51358=CARTESIAN_POINT('Ctrl Pts',(-0.296012625978673,1.97162165460656,
6.00736126844103));
#51359=CARTESIAN_POINT('Ctrl Pts',(-0.303660631090676,1.99188819007557,
6.00592835565451));
#51360=CARTESIAN_POINT('Ctrl Pts',(-0.305641090502209,1.9976209205101,6.00553215993073));
#51361=CARTESIAN_POINT('Ctrl Pts',(-0.308417703654822,2.00645892476852,
6.00493858320126));
#51362=CARTESIAN_POINT('Ctrl Pts',(-0.309331217813061,2.00952562635994,
6.00473573256383));
#51363=CARTESIAN_POINT('Ctrl Pts',(-0.310338365460684,2.01310040933991,
6.00450328143803));
#51364=CARTESIAN_POINT('Ctrl Pts',(-0.310476598396289,2.01359559160164,
6.00447117085603));
#51365=CARTESIAN_POINT('Ctrl Pts',(-0.310685026021027,2.01434918604418,
6.00442244044864));
#51366=CARTESIAN_POINT('Ctrl Pts',(-0.310756083753009,2.01460735548816,
6.00440577063749));
#51367=CARTESIAN_POINT('Ctrl Pts',(-0.310884394583346,2.01507582010488,
6.00437556693913));
#51368=CARTESIAN_POINT('Ctrl Pts',(-0.310941755916316,2.01528608405448,
6.00436202677507));
#51369=CARTESIAN_POINT('Ctrl Pts',(-0.311056920752505,2.01570992565782,
6.00433476602475));
#51370=CARTESIAN_POINT('Ctrl Pts',(-0.311114717347823,2.0159235036949,6.00432104587656));
#51371=CARTESIAN_POINT('Ctrl Pts',(-0.311279850196348,2.01653622747345,
6.00428173257542));
#51372=CARTESIAN_POINT('Ctrl Pts',(-0.311386639094199,2.01693552226874,
6.00425617131675));
#51373=CARTESIAN_POINT('Ctrl Pts',(-0.31184742928036,2.01867184117808,6.0041452671306));
#51374=CARTESIAN_POINT('Ctrl Pts',(-0.312193596421089,2.02001095649239,
6.00406037223381));
#51375=CARTESIAN_POINT('Ctrl Pts',(-0.31897751323838,2.04696895907943,6.0023633848848));
#51376=CARTESIAN_POINT('Ctrl Pts',(-0.322251150394464,2.07328580773895,
6.00091967657762));
#51377=CARTESIAN_POINT('Ctrl Pts',(-0.322280469809755,2.10594897631948,
5.99908929551111));
#51378=CARTESIAN_POINT('Ctrl Pts',(-0.322104937854925,2.112185954157,5.99873841020408));
#51379=CARTESIAN_POINT('Ctrl Pts',(-0.320793648356167,2.13509843943699,
5.99743568333589));
#51380=CARTESIAN_POINT('Ctrl Pts',(-0.318542619957099,2.15168117635893,
5.99646440228957));
#51381=CARTESIAN_POINT('Ctrl Pts',(-0.314748459050056,2.16925457357357,
5.99537224748659));
#51382=CARTESIAN_POINT('Ctrl Pts',(-0.314473112307703,2.17049432600674,
5.99529486771595));
#51383=CARTESIAN_POINT('Ctrl Pts',(-0.314077656726483,2.17222643531318,
5.99518628253308));
#51384=CARTESIAN_POINT('Ctrl Pts',(-0.313963700776544,2.17272019666445,
5.99515527475656));
#51385=CARTESIAN_POINT('Ctrl Pts',(-0.313764468169048,2.17357425654713,
5.99510154612708));
#51386=CARTESIAN_POINT('Ctrl Pts',(-0.313679734047849,2.17393468169731,
5.99507884275521));
#51387=CARTESIAN_POINT('Ctrl Pts',(-0.313502646682352,2.17468215640289,
5.99503169809773));
#51388=CARTESIAN_POINT('Ctrl Pts',(-0.313410197371313,2.17506918238056,
5.99500725375206));
#51389=CARTESIAN_POINT('Ctrl Pts',(-0.313191710054619,2.17597640998326,
5.99494987381673));
#51390=CARTESIAN_POINT('Ctrl Pts',(-0.313065092673072,2.17649646962422,
5.99491691960107));
#51391=CARTESIAN_POINT('Ctrl Pts',(-0.312650611472097,2.17818061612235,
5.9948100000381));
#51392=CARTESIAN_POINT('Ctrl Pts',(-0.312357548481293,2.17934340196638,
5.99473586708172));
#51393=CARTESIAN_POINT('Ctrl Pts',(-0.308566050590067,2.194040308164,5.99379485257451));
#51394=CARTESIAN_POINT('Ctrl Pts',(-0.304197626761239,2.20733263945151,
5.99289954700486));
#51395=CARTESIAN_POINT('Ctrl Pts',(-0.292819429928974,2.23561126620143,
5.99089506870974));
#51396=CARTESIAN_POINT('Ctrl Pts',(-0.285491080960554,2.25042736661268,
5.98977897714405));
#51397=CARTESIAN_POINT('Ctrl Pts',(-0.267166092671871,2.28126974924426,
5.98735155126453));
#51398=CARTESIAN_POINT('Ctrl Pts',(-0.255788347070542,2.29699988415692,
5.98604459277556));
#51399=CARTESIAN_POINT('Ctrl Pts',(-0.242347743162633,2.31243808630275,
5.98475490369902));
#51400=CARTESIAN_POINT('Ctrl Pts',(-0.241626197965943,2.31325841053967,
5.98468635928188));
#51401=CARTESIAN_POINT('Ctrl Pts',(-0.240650576329608,2.31435628583397,
5.98459462144937));
#51402=CARTESIAN_POINT('Ctrl Pts',(-0.240400175807708,2.31463707191295,
5.98457115895934));
#51403=CARTESIAN_POINT('Ctrl Pts',(-0.240006716806598,2.31507672402036,
5.98453442227436));
#51404=CARTESIAN_POINT('Ctrl Pts',(-0.239863991975023,2.31523588613906,
5.98452112305604));
#51405=CARTESIAN_POINT('Ctrl Pts',(-0.239589229170906,2.31554168001766,
5.9844955720926));
#51406=CARTESIAN_POINT('Ctrl Pts',(-0.239457215891181,2.31568833143547,
5.98448331869795));
#51407=CARTESIAN_POINT('Ctrl Pts',(-0.239143346022571,2.31603636106496,
5.98445423965154));
#51408=CARTESIAN_POINT('Ctrl Pts',(-0.238961369928544,2.31623763070342,
5.98443742320047));
#51409=CARTESIAN_POINT('Ctrl Pts',(-0.238422384903588,2.31683224893654,
5.98438774179642));
#51410=CARTESIAN_POINT('Ctrl Pts',(-0.238064655185021,2.3172249473775,5.98435493121354));
#51411=CARTESIAN_POINT('Ctrl Pts',(-0.235242868563442,2.3203072259192,5.98409738544989));
#51412=CARTESIAN_POINT('Ctrl Pts',(-0.232734156049585,2.32295581704951,
5.98387597818845));
#51413=CARTESIAN_POINT('Ctrl Pts',(-0.223654953127177,2.33222096258806,
5.9830986238959));
#51414=CARTESIAN_POINT('Ctrl Pts',(-0.216842491176209,2.33859479822104,
5.98255849530007));
#51415=CARTESIAN_POINT('Ctrl Pts',(-0.202823565989846,2.35061388665305,
5.98150648290134));
#51416=CARTESIAN_POINT('Ctrl Pts',(-0.195634323301723,2.35626537271202,
5.98099471313661));
#51417=CARTESIAN_POINT('Ctrl Pts',(-0.171817592218757,2.37340064265486,
5.9793542666704));
#51418=CARTESIAN_POINT('Ctrl Pts',(-0.154349536410973,2.38362886316792,
5.97822903294836));
#51419=CARTESIAN_POINT('Ctrl Pts',(-0.134316469745295,2.39295712208554,
5.97693582857045));
#51420=CARTESIAN_POINT('Ctrl Pts',(-0.132586098954645,2.39374430306898,
5.97682413904472));
#51421=CARTESIAN_POINT('Ctrl Pts',(-0.124735168498417,2.39723234825744,
5.97631725263981));
#51422=CARTESIAN_POINT('Ctrl Pts',(-0.118538725756981,2.39975738815499,
5.97591676848745));
#51423=CARTESIAN_POINT('Ctrl Pts',(-0.11129224617215,2.40245048573662,5.97544628802601));
#51424=CARTESIAN_POINT('Ctrl Pts',(-0.110314226952202,2.40280857265338,
5.97538274680311));
#51425=CARTESIAN_POINT('Ctrl Pts',(-0.108859218324699,2.40333331746174,
5.97528814623771));
#51426=CARTESIAN_POINT('Ctrl Pts',(-0.108383538341173,2.40350360707685,
5.97525720784803));
#51427=CARTESIAN_POINT('Ctrl Pts',(-0.107536712262193,2.40380451930862,
5.97520210964551));
#51428=CARTESIAN_POINT('Ctrl Pts',(-0.107165722875459,2.40393558244291,
5.97517796452618));
#51429=CARTESIAN_POINT('Ctrl Pts',(-0.10638536511117,2.40420966084493,5.97512716149948));
#51430=CARTESIAN_POINT('Ctrl Pts',(-0.10597594651758,2.4043525298367,5.97510049879563));
#51431=CARTESIAN_POINT('Ctrl Pts',(-0.104898844066915,2.40472595409132,
5.97503033093204));
#51432=CARTESIAN_POINT('Ctrl Pts',(-0.104230691092841,2.40495514031584,
5.97498678052436));
#51433=CARTESIAN_POINT('Ctrl Pts',(-0.101251338948475,2.40596616628005,
5.97479247610219));
#51434=CARTESIAN_POINT('Ctrl Pts',(-0.0989321074319765,2.4067239249546,
5.97464092926571));
#51435=CARTESIAN_POINT('Ctrl Pts',(-0.0819774272182834,2.41205120143762,
5.97353066866323));
#51436=CARTESIAN_POINT('Ctrl Pts',(-0.0670431956381767,2.41559679751256,
5.97253841466143));
#51437=CARTESIAN_POINT('Ctrl Pts',(-0.0198712624586704,2.42329627054299,
5.96936576727488));
#51438=CARTESIAN_POINT('Ctrl Pts',(0.0127766637380169,2.42365415414283,
5.96709745798501));
#51439=CARTESIAN_POINT('Ctrl Pts',(0.0463915859274049,2.41892191238083,
5.96495081979399));
#51440=CARTESIAN_POINT('Ctrl Pts',(0.0478555348947601,2.418705527754,5.96485775813468));
#51441=CARTESIAN_POINT('Ctrl Pts',(0.0497372436924342,2.41841413633344,
5.96473873342076));
#51442=CARTESIAN_POINT('Ctrl Pts',(0.050156387219199,2.41834838220591,5.96471225906882));
#51443=CARTESIAN_POINT('Ctrl Pts',(0.0508205663555086,2.41824284325534,
5.96467036904285));
#51444=CARTESIAN_POINT('Ctrl Pts',(0.0510656860861607,2.41820360298634,
5.96465492253723));
#51445=CARTESIAN_POINT('Ctrl Pts',(0.0515049839696522,2.41813275680895,
5.96462726379184));
#51446=CARTESIAN_POINT('Ctrl Pts',(0.0516991771013884,2.41810125654566,
5.96461504563065));
#51447=CARTESIAN_POINT('Ctrl Pts',(0.052155874544087,2.41802674593969,5.96458633118205));
#51448=CARTESIAN_POINT('Ctrl Pts',(0.0524183541499164,2.41798358846312,
5.9645698434049));
#51449=CARTESIAN_POINT('Ctrl Pts',(0.0531797206979818,2.41785743456257,
5.96452206170778));
#51450=CARTESIAN_POINT('Ctrl Pts',(0.0536784689623207,2.41777358823274,
5.96449081605724));
#51451=CARTESIAN_POINT('Ctrl Pts',(0.0571397491327742,2.41718331879781,
5.96427434027958));
#51452=CARTESIAN_POINT('Ctrl Pts',(0.0600953926362167,2.41663662770907,
5.96409135548428));
#51453=CARTESIAN_POINT('Ctrl Pts',(0.0692896417962748,2.41480262583709,
5.9635267581205));
#51454=CARTESIAN_POINT('Ctrl Pts',(0.0754983272270876,2.41337160280435,
5.96315216030322));
#51455=CARTESIAN_POINT('Ctrl Pts',(0.0969192142704502,2.40776067135472,
5.96187032881164));
#51456=CARTESIAN_POINT('Ctrl Pts',(0.111864507978248,2.4026489085701,5.96099399972733));
#51457=CARTESIAN_POINT('Ctrl Pts',(0.149486696795473,2.38661132924035,5.95870712660777));
#51458=CARTESIAN_POINT('Ctrl Pts',(0.171362192526894,2.37409317631907,5.95728915670301));
#51459=CARTESIAN_POINT('Ctrl Pts',(0.192758675081555,2.35827792592324,5.95567521945505));
#51460=CARTESIAN_POINT('Ctrl Pts',(0.193950208734088,2.35738436287842,5.95558455959877));
#51461=CARTESIAN_POINT('Ctrl Pts',(0.195567120419863,2.35615419414918,5.95546044452395));
#51462=CARTESIAN_POINT('Ctrl Pts',(0.195997918702762,2.35582471660894,5.95542726973295));
#51463=CARTESIAN_POINT('Ctrl Pts',(0.196728973389977,2.35526267039162,5.95537079059267));
#51464=CARTESIAN_POINT('Ctrl Pts',(0.197029655144076,2.35503065474241,5.95534750812562));
#51465=CARTESIAN_POINT('Ctrl Pts',(0.197634769294365,2.35456202045618,5.95530054611185));
#51466=CARTESIAN_POINT('Ctrl Pts',(0.197939188567127,2.35432538591369,5.9552768659565));
#51467=CARTESIAN_POINT('Ctrl Pts',(0.198630086993066,2.35378633727417,5.9552229976437));
#51468=CARTESIAN_POINT('Ctrl Pts',(0.19901630085039,2.35348358613033,5.95519279610282));
#51469=CARTESIAN_POINT('Ctrl Pts',(0.199822355441396,2.35284874617137,5.95512957622368));
#51470=CARTESIAN_POINT('Ctrl Pts',(0.200242062958403,2.35251649132525,5.9550965512988));
#51471=CARTESIAN_POINT('Ctrl Pts',(0.201339898443672,2.35164294897854,5.95500988606244));
#51472=CARTESIAN_POINT('Ctrl Pts',(0.20201666823648,2.35109996855222,5.95495617787136));
#51473=CARTESIAN_POINT('Ctrl Pts',(0.204019806043015,2.3494794873847,5.95479636242501));
#51474=CARTESIAN_POINT('Ctrl Pts',(0.2053397895926,2.34839417568146,5.95468994029806));
#51475=CARTESIAN_POINT('Ctrl Pts',(0.219751845991815,2.33635096671437,5.95351558082101));
#51476=CARTESIAN_POINT('Ctrl Pts',(0.231959863109446,2.32438161509491,5.95240517867696));
#51477=CARTESIAN_POINT('Ctrl Pts',(0.26169602417353,2.29019459162271,5.94938181885288));
#51478=CARTESIAN_POINT('Ctrl Pts',(0.277348821603544,2.26654253993711,5.94742428259788));
#51479=CARTESIAN_POINT('Ctrl Pts',(0.291255757088953,2.23799846794826,5.94538451040464));
#51480=CARTESIAN_POINT('Ctrl Pts',(0.292741384938226,2.23481831193916,5.94516157700682));
#51481=CARTESIAN_POINT('Ctrl Pts',(0.294408049282037,2.23109310524211,5.94490595951939));
#51482=CARTESIAN_POINT('Ctrl Pts',(0.294639877845851,2.23057122239967,5.94487027366271));
#51483=CARTESIAN_POINT('Ctrl Pts',(0.294983088645123,2.22979303190937,5.94481725053138));
#51484=CARTESIAN_POINT('Ctrl Pts',(0.295095525055178,2.22953719470743,5.94479984901571));
#51485=CARTESIAN_POINT('Ctrl Pts',(0.295295439818329,2.22908069864701,5.94476885356888));
#51486=CARTESIAN_POINT('Ctrl Pts',(0.295383046435053,2.22888009706898,5.94475525174929));
#51487=CARTESIAN_POINT('Ctrl Pts',(0.295568862161798,2.22845343161714,5.94472636158116));
#51488=CARTESIAN_POINT('Ctrl Pts',(0.295667016053899,2.22822734494873,5.94471107666885));
#51489=CARTESIAN_POINT('Ctrl Pts',(0.295930278788776,2.22761903883301,5.9446700145525));
#51490=CARTESIAN_POINT('Ctrl Pts',(0.296094907169749,2.22723661002017,5.94464426681456));
#51491=CARTESIAN_POINT('Ctrl Pts',(0.296886350987121,2.22538824537119,5.94452014105262));
#51492=CARTESIAN_POINT('Ctrl Pts',(0.297503037678857,2.22391795792926,5.94442237215243));
#51493=CARTESIAN_POINT('Ctrl Pts',(0.30259505039819,2.2115205784368,5.94360560637735));
#51494=CARTESIAN_POINT('Ctrl Pts',(0.306478168540586,2.20035837091534,5.94291963772146));
#51495=CARTESIAN_POINT('Ctrl Pts',(0.318341698799888,2.15907383377874,5.94047450910394));
#51496=CARTESIAN_POINT('Ctrl Pts',(0.322558887653065,2.12805354962461,5.938792774593));
#51497=CARTESIAN_POINT('Ctrl Pts',(0.322196875576618,2.09030905245233,5.9365647005873));
#51498=CARTESIAN_POINT('Ctrl Pts',(0.32193083116601,2.08371284050106,5.93616947414742));
#51499=CARTESIAN_POINT('Ctrl Pts',(0.321388863541718,2.07609497404383,5.9357046766006));
#51500=CARTESIAN_POINT('Ctrl Pts',(0.321310247240895,2.07506053622989,5.93564138366107));
#51501=CARTESIAN_POINT('Ctrl Pts',(0.321185984072488,2.07352371415354,5.93554708193351));
#51502=CARTESIAN_POINT('Ctrl Pts',(0.321144149535001,2.07302102129983,5.93551619297808));
#51503=CARTESIAN_POINT('Ctrl Pts',(0.321068297467126,2.07213474784566,5.93546165762858));
#51504=CARTESIAN_POINT('Ctrl Pts',(0.321034772239056,2.07175112520049,5.93543802675674));
#51505=CARTESIAN_POINT('Ctrl Pts',(0.320978950135475,2.0711252990556,5.93539943475082));
#51506=CARTESIAN_POINT('Ctrl Pts',(0.320957066428401,2.07088305830175,5.93538448663814));
#51507=CARTESIAN_POINT('Ctrl Pts',(0.320886475169926,2.07011140129722,5.93533683694479));
#51508=CARTESIAN_POINT('Ctrl Pts',(0.32083673197218,2.0695820827241,5.93530410280659));
#51509=CARTESIAN_POINT('Ctrl Pts',(0.320728813819431,2.06846344513909,5.93523481985232));
#51510=CARTESIAN_POINT('Ctrl Pts',(0.320670323927075,2.06787415913122,5.93519826122022));
#51511=CARTESIAN_POINT('Ctrl Pts',(0.320508231973931,2.06628564010189,5.93509954486852));
#51512=CARTESIAN_POINT('Ctrl Pts',(0.320401581985314,2.06528673090893,5.93503729130609));
#51513=CARTESIAN_POINT('Ctrl Pts',(0.320059188162592,2.06221587322731,5.93484535594972));
#51514=CARTESIAN_POINT('Ctrl Pts',(0.319808006812089,2.0601457328145,5.93471518963316));
#51515=CARTESIAN_POINT('Ctrl Pts',(0.318809805718197,2.05253723199526,5.93423384800152));
#51516=CARTESIAN_POINT('Ctrl Pts',(0.317938890031717,2.04701639357965,5.93387882298313));
#51517=CARTESIAN_POINT('Ctrl Pts',(0.315646134731852,2.03459083195782,5.93306639739291));
#51518=CARTESIAN_POINT('Ctrl Pts',(0.314140434454107,2.02770464798979,5.93260667301109));
#51519=CARTESIAN_POINT('Ctrl Pts',(0.30393310534402,1.98740356213598,5.92986235944173));
#51520=CARTESIAN_POINT('Ctrl Pts',(0.29013392484836,1.95551699005566,5.92744024977939));
#51521=CARTESIAN_POINT('Ctrl Pts',(0.270843158176367,1.92533794121575,5.92517912198665));
#51522=CARTESIAN_POINT('Ctrl Pts',(0.270139436771538,1.92425149802984,5.925097807124));
#51523=CARTESIAN_POINT('Ctrl Pts',(0.269208202228769,1.92283261681688,5.92499175440138));
#51524=CARTESIAN_POINT('Ctrl Pts',(0.268986597510482,1.92249634320628,5.92496663063386));
#51525=CARTESIAN_POINT('Ctrl Pts',(0.268643444793574,1.92197774518707,5.92492790254007));
#51526=CARTESIAN_POINT('Ctrl Pts',(0.268522341214268,1.92179512939111,5.92491426844442));
#51527=CARTESIAN_POINT('Ctrl Pts',(0.268280286740075,1.92143093501072,5.92488708464774));
#51528=CARTESIAN_POINT('Ctrl Pts',(0.268159338552588,1.92124935700265,5.92487353499762));
#51529=CARTESIAN_POINT('Ctrl Pts',(0.267887485681955,1.92084212456348,5.92484315436187));
#51530=CARTESIAN_POINT('Ctrl Pts',(0.267736480586475,1.92061653844238,5.92482633032064));
#51531=CARTESIAN_POINT('Ctrl Pts',(0.267288810770249,1.91994959019485,5.92477660464376));
#51532=CARTESIAN_POINT('Ctrl Pts',(0.266991336582043,1.91950876854076,5.92474375752465));
#51533=CARTESIAN_POINT('Ctrl Pts',(0.264635364772894,1.91603606600753,5.92448512958724));
#51534=CARTESIAN_POINT('Ctrl Pts',(0.26252627535475,1.91303860604383,5.92426270821507));
#51535=CARTESIAN_POINT('Ctrl Pts',(0.254826313706799,1.90248265486284,5.92347983189168));
#51536=CARTESIAN_POINT('Ctrl Pts',(0.248956048744244,1.89513304706535,5.92293546255686));
#51537=CARTESIAN_POINT('Ctrl Pts',(0.240214227597833,1.88511996399137,5.92217846587377));
#51538=CARTESIAN_POINT('Ctrl Pts',(0.237603242617463,1.88223635465301,5.92195854345257));
#51539=CARTESIAN_POINT('Ctrl Pts',(0.223202400523936,1.86689930359885,5.9207741241878));
#51540=CARTESIAN_POINT('Ctrl Pts',(0.2104852581215,1.85535494589176,5.91982723580088));
#51541=CARTESIAN_POINT('Ctrl Pts',(0.183908419261698,1.83484229327832,5.91791995835766));
#51542=CARTESIAN_POINT('Ctrl Pts',(0.170160638361421,1.82581729145374,5.9169645702399));
#51543=CARTESIAN_POINT('Ctrl Pts',(0.154677802223691,1.81726769444894,5.91589011279933));
#51544=CARTESIAN_POINT('Ctrl Pts',(0.153565708197699,1.81666212343355,5.91581295591814));
#51545=CARTESIAN_POINT('Ctrl Pts',(0.152004181626461,1.81582371572771,5.91570463324324));
#51546=CARTESIAN_POINT('Ctrl Pts',(0.151557715509892,1.81558535438634,5.91567366381129));
#51547=CARTESIAN_POINT('Ctrl Pts',(0.150783807351327,1.81517451653371,5.91561998349051));
#51548=CARTESIAN_POINT('Ctrl Pts',(0.150456625356693,1.81500155004704,5.91559729000737));
#51549=CARTESIAN_POINT('Ctrl Pts',(0.149784034438824,1.81464746231234,5.91555063996773));
#51550=CARTESIAN_POINT('Ctrl Pts',(0.149438593308637,1.8144664037886,5.91552668123942));
#51551=CARTESIAN_POINT('Ctrl Pts',(0.14863175401872,1.81404537458357,5.91547072238281));
#51552=CARTESIAN_POINT('Ctrl Pts',(0.148170102946865,1.81380589333917,5.91543870505292));
#51553=CARTESIAN_POINT('Ctrl Pts',(0.147195913044414,1.81330352179404,5.91537114187637));
#51554=CARTESIAN_POINT('Ctrl Pts',(0.14668324550012,1.81304088633512,5.91533558718313));
#51555=CARTESIAN_POINT('Ctrl Pts',(0.145309441885275,1.81234174126003,5.91524031041911));
#51556=CARTESIAN_POINT('Ctrl Pts',(0.144447048815092,1.81190772697215,5.91518050097489));
#51557=CARTESIAN_POINT('Ctrl Pts',(0.141813698011413,1.8105972440271,5.91499786258184));
#51558=CARTESIAN_POINT('Ctrl Pts',(0.140036643444441,1.8097331945932,5.91487460219325));
#51559=CARTESIAN_POINT('Ctrl Pts',(0.133558834654711,1.80665684898303,5.91442518824468));
#51560=CARTESIAN_POINT('Ctrl Pts',(0.128812910809411,1.8045420578942,5.91409572371327));
#51561=CARTESIAN_POINT('Ctrl Pts',(0.117912560090552,1.79999739637808,5.91333825560152));
#51562=CARTESIAN_POINT('Ctrl Pts',(0.111730389756813,1.79764053745451,5.91290809901338));
#51563=CARTESIAN_POINT('Ctrl Pts',(0.0898216704454556,1.79005184795571,
5.91138272337882));
#51564=CARTESIAN_POINT('Ctrl Pts',(0.0737690610956677,1.78584425642561,
5.91026178316174));
#51565=CARTESIAN_POINT('Ctrl Pts',(0.0386575877370288,1.77948147245121,
5.90784752432679));
#51566=CARTESIAN_POINT('Ctrl Pts',(0.0195810999141629,1.77775273338049,
5.90655871763368));
#51567=CARTESIAN_POINT('Ctrl Pts',(-0.00067661604709986,1.77772369924387,
5.90528177230881));
#51568=CARTESIAN_POINT('Ctrl Pts',(-0.00181514948180812,1.77772810056933,
5.90521031844886));
#51569=CARTESIAN_POINT('Ctrl Pts',(-0.00333633254758036,1.77774204282283,
5.90511529014557));
#51570=CARTESIAN_POINT('Ctrl Pts',(-0.00371900521102961,1.77774623185643,
5.9050914218328));
#51571=CARTESIAN_POINT('Ctrl Pts',(-0.00431673729365212,1.77775383995341,
5.90505419883373));
#51572=CARTESIAN_POINT('Ctrl Pts',(-0.00453180069685644,1.77775679267247,
5.90504081799572));
#51573=CARTESIAN_POINT('Ctrl Pts',(-0.00494384746416748,1.77776286246143,
5.90501520434944));
#51574=CARTESIAN_POINT('Ctrl Pts',(-0.0051408295034581,1.77776594483344,
5.90500296970853));
#51575=CARTESIAN_POINT('Ctrl Pts',(-0.00560642471079884,1.77777365750069,
5.90497407526306));
#51576=CARTESIAN_POINT('Ctrl Pts',(-0.00587503466236217,1.77777844304346,
5.90495742431161));
#51577=CARTESIAN_POINT('Ctrl Pts',(-0.006661859954345,1.77779344529164,
5.90490870366227));
#51578=CARTESIAN_POINT('Ctrl Pts',(-0.00718006010154157,1.77780457635019,
5.90487668520465));
#51579=CARTESIAN_POINT('Ctrl Pts',(-0.0110002526933215,1.77789585595836,
5.90464113614396));
#51580=CARTESIAN_POINT('Ctrl Pts',(-0.0143010184661592,1.77802551638261,
5.90444032608791));
#51581=CARTESIAN_POINT('Ctrl Pts',(-0.0252021534360486,1.77862171443231,
5.90378438381918));
#51582=CARTESIAN_POINT('Ctrl Pts',(-0.0327884255692302,1.77930686316088,
5.90333955409475));
#51583=CARTESIAN_POINT('Ctrl Pts',(-0.048701459578559,1.78131472395007,
5.90241798501008));
#51584=CARTESIAN_POINT('Ctrl Pts',(-0.0570148664733614,1.78269659004878,
5.90194321083976));
#51585=CARTESIAN_POINT('Ctrl Pts',(-0.0679019689247061,1.78494802029648,
5.90132001395504));
#51586=CARTESIAN_POINT('Ctrl Pts',(-0.0705321362106861,1.78552639987211,
5.90116935253939));
#51587=CARTESIAN_POINT('Ctrl Pts',(-0.0819974202267397,1.78819871822848,
5.90051110452581));
#51588=CARTESIAN_POINT('Ctrl Pts',(-0.0907489467655755,1.79063251411109,
5.90000464139583));
#51589=CARTESIAN_POINT('Ctrl Pts',(-0.117835699815279,1.79941375014011,
5.89839925779277));
#51590=CARTESIAN_POINT('Ctrl Pts',(-0.135705014915195,1.8070472301034,5.89728159624567));
#51591=CARTESIAN_POINT('Ctrl Pts',(-0.153916945577696,1.81685265044588,
5.89602528760817));
#51592=CARTESIAN_POINT('Ctrl Pts',(-0.155051783402283,1.81747249322744,
5.89594650745762));
#51593=CARTESIAN_POINT('Ctrl Pts',(-0.156629550318885,1.81834663079213,
5.89583627418678));
#51594=CARTESIAN_POINT('Ctrl Pts',(-0.157075662291097,1.81859517998031,
5.89580502674775));
#51595=CARTESIAN_POINT('Ctrl Pts',(-0.157845084446694,1.81902625961212,
5.89575099583474));
#51596=CARTESIAN_POINT('Ctrl Pts',(-0.158168674379394,1.81920829087252,
5.89572823031501));
#51597=CARTESIAN_POINT('Ctrl Pts',(-0.158830932280142,1.81958234337956,
5.89568155170728));
#51598=CARTESIAN_POINT('Ctrl Pts',(-0.159169568217506,1.81977441989558,
5.89565763665518));
#51599=CARTESIAN_POINT('Ctrl Pts',(-0.15995575866852,1.82022223711906,5.89560200563611));
#51600=CARTESIAN_POINT('Ctrl Pts',(-0.16040304837092,1.82047843839467,5.89557027308259));
#51601=CARTESIAN_POINT('Ctrl Pts',(-0.161343566306664,1.82102015479653,
5.89550337467035));
#51602=CARTESIAN_POINT('Ctrl Pts',(-0.161836655254916,1.82130590708175,
5.89546820029038));
#51603=CARTESIAN_POINT('Ctrl Pts',(-0.163150253157912,1.82207181807494,
5.89537422304531));
#51604=CARTESIAN_POINT('Ctrl Pts',(-0.163969395150256,1.82255429930054,
5.89531533590432));
#51605=CARTESIAN_POINT('Ctrl Pts',(-0.16644935368748,1.82402983359876,5.89513618307501));
#51606=CARTESIAN_POINT('Ctrl Pts',(-0.168103348797263,1.82503421313449,
5.89501550500858));
#51607=CARTESIAN_POINT('Ctrl Pts',(-0.174041054638061,1.82871345111793,
5.89457789583224));
#51608=CARTESIAN_POINT('Ctrl Pts',(-0.178270611938832,1.83147390330209,
5.89425784224812));
#51609=CARTESIAN_POINT('Ctrl Pts',(-0.192682497592627,1.84137051750531,
5.89313756238466));
#51610=CARTESIAN_POINT('Ctrl Pts',(-0.202514669711804,1.84899501149601,
5.89231987447261));
#51611=CARTESIAN_POINT('Ctrl Pts',(-0.230444874012216,1.87336523848365,
5.88984146873517));
#51612=CARTESIAN_POINT('Ctrl Pts',(-0.247089556813021,1.89163758085672,
5.88814351750745));
#51613=CARTESIAN_POINT('Ctrl Pts',(-0.262043626896891,1.91239613418237,
5.88647352223353));
#51614=CARTESIAN_POINT('Ctrl Pts',(-0.262593904793257,1.91316714937911,
5.8864118434075));
#51615=CARTESIAN_POINT('Ctrl Pts',(-0.263208974171841,1.91403703193323,
5.88634265559898));
#51616=CARTESIAN_POINT('Ctrl Pts',(-0.263277114147539,1.91413351366381,
5.88633498725024));
#51617=CARTESIAN_POINT('Ctrl Pts',(-0.264038756012179,1.91521320772448,
5.88624923522975));
#51618=CARTESIAN_POINT('Ctrl Pts',(-0.264726809884665,1.91620027342262,
5.88617141342366));
#51619=CARTESIAN_POINT('Ctrl Pts',(-0.267660306862063,1.92045924452959,
5.88583816182218));
#51620=CARTESIAN_POINT('Ctrl Pts',(-0.269850860759941,1.92376879036839,
5.88558558128835));
#51621=CARTESIAN_POINT('Ctrl Pts',(-0.272297556971187,1.92761796247287,
5.88529982723488));
#51622=CARTESIAN_POINT('Ctrl Pts',(-0.272613893620358,1.92811867055181,
5.88526280920225));
#51623=CARTESIAN_POINT('Ctrl Pts',(-0.273079692903399,1.92886047385743,
5.88520819655203));
#51624=CARTESIAN_POINT('Ctrl Pts',(-0.27323021814581,1.92910089532711,5.88519053196105));
#51625=CARTESIAN_POINT('Ctrl Pts',(-0.273496599953841,1.92952761640603,
5.88515924280856));
#51626=CARTESIAN_POINT('Ctrl Pts',(-0.273612583707076,1.92971383558029,
5.88514560978239));
#51627=CARTESIAN_POINT('Ctrl Pts',(-0.273857197190315,1.93010747297492,
5.88511683710837));
#51628=CARTESIAN_POINT('Ctrl Pts',(-0.273985781126848,1.93031491835414,
5.88510170052476));
#51629=CARTESIAN_POINT('Ctrl Pts',(-0.274327421485821,1.93086748996669,
5.88506145119716));
#51630=CARTESIAN_POINT('Ctrl Pts',(-0.274540063124544,1.93121287408965,
5.88503636592523));
#51631=CARTESIAN_POINT('Ctrl Pts',(-0.275525158899786,1.93281970700101,
5.88491999366527));
#51632=CARTESIAN_POINT('Ctrl Pts',(-0.276289590659075,1.93408608905652,
5.88482922745906));
#51633=CARTESIAN_POINT('Ctrl Pts',(-0.282310292381125,1.94421718692567,
5.88411025696604));
#51634=CARTESIAN_POINT('Ctrl Pts',(-0.287147891904193,1.95332511813037,
5.88350729218234));
#51635=CARTESIAN_POINT('Ctrl Pts',(-0.306204172725652,1.99377431072008,
5.8809456550762));
#51636=CARTESIAN_POINT('Ctrl Pts',(-0.315788783613521,2.02704416444801,
5.87910369313275));
#51637=CARTESIAN_POINT('Ctrl Pts',(-0.320206132894077,2.06347018716599,
5.87692213068112));
#51638=CARTESIAN_POINT('Ctrl Pts',(-0.320457034050766,2.06574093252718,
5.87678560364946));
#51639=CARTESIAN_POINT('Ctrl Pts',(-0.320755003572805,2.06872831208986,
5.87660521435884));
#51640=CARTESIAN_POINT('Ctrl Pts',(-0.320823853346949,2.0694427440234,5.87656201615699));
#51641=CARTESIAN_POINT('Ctrl Pts',(-0.321121195060537,2.07263998764373,
5.8763684272592));
#51642=CARTESIAN_POINT('Ctrl Pts',(-0.321323251534889,2.07512511954268,
5.87621723427553));
#51643=CARTESIAN_POINT('Ctrl Pts',(-0.321548093505174,2.07835394040362,
5.87601978042419));
#51644=CARTESIAN_POINT('Ctrl Pts',(-0.321597171993456,2.07909575918394,
5.87597434615416));
#51645=CARTESIAN_POINT('Ctrl Pts',(-0.321671330922924,2.08027879852576,
5.875901775465));
#51646=CARTESIAN_POINT('Ctrl Pts',(-0.32169807158383,2.08071991541829,5.87587469119563));
#51647=CARTESIAN_POINT('Ctrl Pts',(-0.321746424284328,2.08154566461543,
5.87582394341814));
#51648=CARTESIAN_POINT('Ctrl Pts',(-0.321768254164313,2.08193028378087,
5.87580028679091));
#51649=CARTESIAN_POINT('Ctrl Pts',(-0.32181009389795,2.08269158074132,5.87575342358687));
#51650=CARTESIAN_POINT('Ctrl Pts',(-0.321830132164343,2.08306825641006,
5.87573021794098));
#51651=CARTESIAN_POINT('Ctrl Pts',(-0.321873936934282,2.0839198730813,5.87567771046431));
#51652=CARTESIAN_POINT('Ctrl Pts',(-0.321897313598774,2.08439483248053,
5.875648396445));
#51653=CARTESIAN_POINT('Ctrl Pts',(-0.321953706390739,2.08559468410446,
5.87557426672389));
#51654=CARTESIAN_POINT('Ctrl Pts',(-0.321985325483628,2.0863196365478,5.87552940728699));
#51655=CARTESIAN_POINT('Ctrl Pts',(-0.322189741514093,2.09140055695314,
5.87521450568765));
#51656=CARTESIAN_POINT('Ctrl Pts',(-0.32227657842632,2.09575931995697,5.87494178447891));
#51657=CARTESIAN_POINT('Ctrl Pts',(-0.322274978285881,2.10011830399491,
5.87466631836037));
#51658=CARTESIAN_POINT('',(-0.322274906241924,2.09975417128097,5.62420562594364));
#51659=CARTESIAN_POINT('Ctrl Pts',(-0.322274978376309,2.10011805739837,
5.87466633394405));
#51660=CARTESIAN_POINT('Ctrl Pts',(-0.322261304025871,2.13744651840769,
5.8723073616825));
#51661=CARTESIAN_POINT('Ctrl Pts',(-0.315761043457354,2.17448876595038,
5.86971828307802));
#51662=CARTESIAN_POINT('Ctrl Pts',(-0.300912371558147,2.21555646760403,
5.86682882722654));
#51663=CARTESIAN_POINT('Ctrl Pts',(-0.29857535205361,2.22146737439975,5.86641374952161));
#51664=CARTESIAN_POINT('Ctrl Pts',(-0.294885459834669,2.23004866868408,
5.86581614266381));
#51665=CARTESIAN_POINT('Ctrl Pts',(-0.293667886671735,2.23277524073928,
5.86562702548014));
#51666=CARTESIAN_POINT('Ctrl Pts',(-0.292200300874887,2.2359426889284,5.86540856071013));
#51667=CARTESIAN_POINT('Ctrl Pts',(-0.291986981329614,2.23640026849944,
5.8653770309333));
#51668=CARTESIAN_POINT('Ctrl Pts',(-0.291659704673618,2.23709800491725,
5.86532900151759));
#51669=CARTESIAN_POINT('Ctrl Pts',(-0.291546525466425,2.23733852253563,
5.86531245405373));
#51670=CARTESIAN_POINT('Ctrl Pts',(-0.291349071535339,2.23775678871357,
5.86528369330924));
#51671=CARTESIAN_POINT('Ctrl Pts',(-0.291264931875615,2.23793459965273,
5.86527147167055));
#51672=CARTESIAN_POINT('Ctrl Pts',(-0.291074185448169,2.23833674812616,
5.86524384172069));
#51673=CARTESIAN_POINT('Ctrl Pts',(-0.290967482330296,2.23856103905428,
5.86522843953113));
#51674=CARTESIAN_POINT('Ctrl Pts',(-0.290677546210389,2.23916867564697,
5.86518673361925));
#51675=CARTESIAN_POINT('Ctrl Pts',(-0.290493813421313,2.23955178437082,
5.86516046098384));
#51676=CARTESIAN_POINT('Ctrl Pts',(-0.289664334448925,2.24127262822696,
5.8650425462129));
#51677=CARTESIAN_POINT('Ctrl Pts',(-0.28901008841467,2.24260628012699,5.8649514246738));
#51678=CARTESIAN_POINT('Ctrl Pts',(-0.274952990325081,2.27076694888698,
5.86303192766152));
#51679=CARTESIAN_POINT('Ctrl Pts',(-0.257877352000274,2.29560280651141,
5.86141750102764));
#51680=CARTESIAN_POINT('Ctrl Pts',(-0.229374123297901,2.32670972971249,
5.85903797497653));
#51681=CARTESIAN_POINT('Ctrl Pts',(-0.220635648190775,2.33522258016575,
5.85834120709332));
#51682=CARTESIAN_POINT('Ctrl Pts',(-0.207655895312586,2.34650618596164,
5.85732981479167));
#51683=CARTESIAN_POINT('Ctrl Pts',(-0.203799303392252,2.3497040458331,5.8570320585353));
#51684=CARTESIAN_POINT('Ctrl Pts',(-0.198360977815014,2.35400353941477,
5.85661499626325));
#51685=CARTESIAN_POINT('Ctrl Pts',(-0.196841436312936,2.35518292313665,
5.85649875984245));
#51686=CARTESIAN_POINT('Ctrl Pts',(-0.194558575559887,2.35692222978957,
5.85632452821828));
#51687=CARTESIAN_POINT('Ctrl Pts',(-0.19380318130861,2.35749252099592,5.85626693894956));
#51688=CARTESIAN_POINT('Ctrl Pts',(-0.19259033178475,2.35839981143192,5.85617457089869));
#51689=CARTESIAN_POINT('Ctrl Pts',(-0.192134474652336,2.35873894582878,
5.85613987542671));
#51690=CARTESIAN_POINT('Ctrl Pts',(-0.191264902430163,2.35938229783766,
5.85607373182171));
#51691=CARTESIAN_POINT('Ctrl Pts',(-0.190851351972392,2.35968673585428,
5.85604229238287));
#51692=CARTESIAN_POINT('Ctrl Pts',(-0.190123106767869,2.36022015941282,
5.85598695801521));
#51693=CARTESIAN_POINT('Ctrl Pts',(-0.189808720779931,2.36044956633796,
5.85596307949456));
#51694=CARTESIAN_POINT('Ctrl Pts',(-0.189193410125803,2.36089685168069,
5.85591636308976));
#51695=CARTESIAN_POINT('Ctrl Pts',(-0.188892522613072,2.36111478041467,
5.85589352720101));
#51696=CARTESIAN_POINT('Ctrl Pts',(-0.188176397368744,2.36163157462699,
5.85583919655527));
#51697=CARTESIAN_POINT('Ctrl Pts',(-0.187760824427964,2.36192997188904,
5.85580768380528));
#51698=CARTESIAN_POINT('Ctrl Pts',(-0.186287929131073,2.36298226056254,
5.85569604886561));
#51699=CARTESIAN_POINT('Ctrl Pts',(-0.185226773365365,2.36373074196993,
5.85561571928685));
#51700=CARTESIAN_POINT('Ctrl Pts',(-0.167208512562438,2.37627745227219,
5.85425329440143));
#51701=CARTESIAN_POINT('Ctrl Pts',(-0.149163590855082,2.38642249401514,
5.85290726901761));
#51702=CARTESIAN_POINT('Ctrl Pts',(-0.119196983541462,2.39966641443426,
5.8507111766504));
#51703=CARTESIAN_POINT('Ctrl Pts',(-0.107851513131334,2.40393406844556,
5.84988898399211));
#51704=CARTESIAN_POINT('Ctrl Pts',(-0.0796365509684504,2.41276802243173,
5.84789180397521));
#51705=CARTESIAN_POINT('Ctrl Pts',(-0.0625813333070764,2.41662211195314,
5.84672370025639));
#51706=CARTESIAN_POINT('Ctrl Pts',(-0.0445963477278461,2.4191752505305,
5.84558405003193));
#51707=CARTESIAN_POINT('Ctrl Pts',(-0.0438965180187346,2.41927225139381,
5.84553984943952));
#51708=CARTESIAN_POINT('Ctrl Pts',(-0.0428942013346234,2.41940782096155,
5.84547675754714));
#51709=CARTESIAN_POINT('Ctrl Pts',(-0.0425919761426849,2.41944826211711,
5.84545776142461));
#51710=CARTESIAN_POINT('Ctrl Pts',(-0.0420689847243433,2.41951748890268,
5.84542493778293));
#51711=CARTESIAN_POINT('Ctrl Pts',(-0.0418482455951119,2.41954647476104,
5.8454110988658));
#51712=CARTESIAN_POINT('Ctrl Pts',(-0.0414225881143066,2.41960192037887,
5.8453844419481));
#51713=CARTESIAN_POINT('Ctrl Pts',(-0.041217674813951,2.4196284117526,5.84537162214842));
#51714=CARTESIAN_POINT('Ctrl Pts',(-0.0407306568584338,2.41969089773571,
5.8453411837737));
#51715=CARTESIAN_POINT('Ctrl Pts',(-0.0404485291875026,2.41972671610486,
5.84532357522967));
#51716=CARTESIAN_POINT('Ctrl Pts',(-0.0396021032452422,2.41983303838904,
5.84527081878165));
#51717=CARTESIAN_POINT('Ctrl Pts',(-0.0390376615991512,2.41990242264648,
5.84523573376646));
#51718=CARTESIAN_POINT('Ctrl Pts',(-0.0335322403891745,2.42056439111605,
5.84489443119215));
#51719=CARTESIAN_POINT('Ctrl Pts',(-0.0285780148947758,2.4210439903006,
5.84459442491015));
#51720=CARTESIAN_POINT('Ctrl Pts',(0.00366040774643581,2.4234125922658,
5.84267688648764));
#51721=CARTESIAN_POINT('Ctrl Pts',(0.0310824640225515,2.42193690608769,
5.84119878978093));
#51722=CARTESIAN_POINT('Ctrl Pts',(0.06909416337172,2.41498344560778,5.83901318761309));
#51723=CARTESIAN_POINT('Ctrl Pts',(0.0800818088619208,2.41237068676662,
5.83836585722197));
#51724=CARTESIAN_POINT('Ctrl Pts',(0.0955263338179536,2.40782958993038,
5.83741794104472));
#51725=CARTESIAN_POINT('Ctrl Pts',(0.100112324772235,2.40636882306435,5.83713161345061));
#51726=CARTESIAN_POINT('Ctrl Pts',(0.106429837464705,2.40419952707458,5.8367295806874));
#51727=CARTESIAN_POINT('Ctrl Pts',(0.108190622132576,2.40357775220463,5.83661669953718));
#51728=CARTESIAN_POINT('Ctrl Pts',(0.110816384508129,2.40262478772874,5.83644708202482));
#51729=CARTESIAN_POINT('Ctrl Pts',(0.111685519990436,2.40230510716807,5.8363907263837));
#51730=CARTESIAN_POINT('Ctrl Pts',(0.113077698801771,2.40178622053309,5.83630011110342));
#51731=CARTESIAN_POINT('Ctrl Pts',(0.113601626366577,2.40158938865717,5.83626593061311));
#51732=CARTESIAN_POINT('Ctrl Pts',(0.114594248785267,2.40121352144043,5.83620102246938));
#51733=CARTESIAN_POINT('Ctrl Pts',(0.115063043956052,2.40103475424653,5.83617030385437));
#51734=CARTESIAN_POINT('Ctrl Pts',(0.115894291816953,2.40071554639659,5.8361157207648));
#51735=CARTESIAN_POINT('Ctrl Pts',(0.116256912283089,2.40057554302473,5.83609187100535));
#51736=CARTESIAN_POINT('Ctrl Pts',(0.116966409613619,2.40030013870184,5.83604513088461));
#51737=CARTESIAN_POINT('Ctrl Pts',(0.1173133069793,2.40016479188276,5.8360222423727));
#51738=CARTESIAN_POINT('Ctrl Pts',(0.118139263257588,2.39984088306227,5.83596765980315));
#51739=CARTESIAN_POINT('Ctrl Pts',(0.118618105321567,2.39965177417065,5.83593594736216));
#51740=CARTESIAN_POINT('Ctrl Pts',(0.120320944671766,2.39897455130106,5.83582292698947));
#51741=CARTESIAN_POINT('Ctrl Pts',(0.121542386263503,2.39848008360864,5.8357414048548));
#51742=CARTESIAN_POINT('Ctrl Pts',(0.143245994100601,2.38953865233255,5.83428465426995));
#51743=CARTESIAN_POINT('Ctrl Pts',(0.162802085095929,2.37901105030961,5.83283527933183));
#51744=CARTESIAN_POINT('Ctrl Pts',(0.193887921975575,2.35788930853296,5.83030858301476));
#51745=CARTESIAN_POINT('Ctrl Pts',(0.206015010521904,2.34830874488463,5.82925655906084));
#51746=CARTESIAN_POINT('Ctrl Pts',(0.225902593486314,2.33013385407039,5.82745271371526));
#51747=CARTESIAN_POINT('Ctrl Pts',(0.23397556887387,2.32192130692495,5.82669426692387));
#51748=CARTESIAN_POINT('Ctrl Pts',(0.242633451848495,2.31211472515133,5.82586658072961));
#51749=CARTESIAN_POINT('Ctrl Pts',(0.243665615974822,2.31092822573732,5.82576766251313));
#51750=CARTESIAN_POINT('Ctrl Pts',(0.244958754286601,2.3094195693691,5.82564347571607));
#51751=CARTESIAN_POINT('Ctrl Pts',(0.245227824942748,2.30910442657871,5.82561762117162));
#51752=CARTESIAN_POINT('Ctrl Pts',(0.245655682344363,2.30860134680361,5.82557648749072));
#51753=CARTESIAN_POINT('Ctrl Pts',(0.245814861851628,2.30841374678795,5.8255611793846));
#51754=CARTESIAN_POINT('Ctrl Pts',(0.246115311936696,2.30805883015864,5.82553227670477));
#51755=CARTESIAN_POINT('Ctrl Pts',(0.246256625647555,2.30789155322347,5.82551867898451));
#51756=CARTESIAN_POINT('Ctrl Pts',(0.246578369036147,2.30750990833154,5.82548771117498));
#51757=CARTESIAN_POINT('Ctrl Pts',(0.246758689403117,2.30729544938994,5.82547034920103));
#51758=CARTESIAN_POINT('Ctrl Pts',(0.247295786657503,2.30665497406178,5.82541861603386));
#51759=CARTESIAN_POINT('Ctrl Pts',(0.247651743972001,2.30622826702841,5.82538430480438));
#51760=CARTESIAN_POINT('Ctrl Pts',(0.250141567183451,2.30322782643884,5.8251441107708));
#51761=CARTESIAN_POINT('Ctrl Pts',(0.252236472670122,2.30062182596584,5.82494099781612));
#51762=CARTESIAN_POINT('Ctrl Pts',(0.263409233166643,2.28627150758317,5.82384917322398));
#51763=CARTESIAN_POINT('Ctrl Pts',(0.271709004216018,2.27394199857122,5.82300602424876));
#51764=CARTESIAN_POINT('Ctrl Pts',(0.294231852242305,2.23491364438417,5.8204757104639));
#51765=CARTESIAN_POINT('Ctrl Pts',(0.305577187209028,2.20675435279571,5.81881562637419));
#51766=CARTESIAN_POINT('Ctrl Pts',(0.313304003825081,2.17553527465924,5.81688125887405));
#51767=CARTESIAN_POINT('Ctrl Pts',(0.313755209807903,2.17363860804277,5.81676346614677));
#51768=CARTESIAN_POINT('Ctrl Pts',(0.314401961195652,2.17080604656007,5.81658709669652));
#51769=CARTESIAN_POINT('Ctrl Pts',(0.314610601277312,2.16987316342066,5.81652893788738));
#51770=CARTESIAN_POINT('Ctrl Pts',(0.314937463478552,2.16838053088484,5.81643576101691));
#51771=CARTESIAN_POINT('Ctrl Pts',(0.315058352039031,2.16782136617775,5.81640082822223));
#51772=CARTESIAN_POINT('Ctrl Pts',(0.315285697474311,2.16675606414996,5.8163342223953));
#51773=CARTESIAN_POINT('Ctrl Pts',(0.315392426134213,2.16624998615022,5.81630255815529));
#51774=CARTESIAN_POINT('Ctrl Pts',(0.315577289248719,2.16536284456467,5.81624701091446));
#51775=CARTESIAN_POINT('Ctrl Pts',(0.315655953106971,2.16498189136318,5.81622314489794));
#51776=CARTESIAN_POINT('Ctrl Pts',(0.315808246711858,2.1642375622006,5.81617648806905));
#51777=CARTESIAN_POINT('Ctrl Pts',(0.315881939513622,2.16387419961159,5.81615369931177));
#51778=CARTESIAN_POINT('Ctrl Pts',(0.316055254684422,2.16301198607233,5.81609959545455));
#51779=CARTESIAN_POINT('Ctrl Pts',(0.316154323053205,2.16251302594218,5.81606826271168));
#51780=CARTESIAN_POINT('Ctrl Pts',(0.316498792268631,2.16075633488615,5.81595786705889));
#51781=CARTESIAN_POINT('Ctrl Pts',(0.316737870023572,2.15949738946507,5.81587860275574));
#51782=CARTESIAN_POINT('Ctrl Pts',(0.32019614432247,2.14067488846429,5.81469122353853));
#51783=CARTESIAN_POINT('Ctrl Pts',(0.321957166955455,2.12287806459793,5.81353600795519));
#51784=CARTESIAN_POINT('Ctrl Pts',(0.322543264728459,2.08532755459188,5.81103578064756));
#51785=CARTESIAN_POINT('Ctrl Pts',(0.321043150392427,2.0656391107074,5.80968829375565));
#51786=CARTESIAN_POINT('Ctrl Pts',(0.315822081177455,2.034795042447,5.8075933327428));
#51787=CARTESIAN_POINT('Ctrl Pts',(0.313275154605378,2.0234884802853,5.80682981808345));
#51788=CARTESIAN_POINT('Ctrl Pts',(0.309695503342594,2.01082399009489,5.80599708944635));
#51789=CARTESIAN_POINT('Ctrl Pts',(0.309255151750428,2.00930867246203,5.80589782989202));
#51790=CARTESIAN_POINT('Ctrl Pts',(0.30868498209923,2.00739908440096,5.80577327516655));
#51791=CARTESIAN_POINT('Ctrl Pts',(0.308565518394969,2.00700178170726,5.80574738985197));
#51792=CARTESIAN_POINT('Ctrl Pts',(0.308373955367174,2.00636912976164,5.8057062186117));
#51793=CARTESIAN_POINT('Ctrl Pts',(0.308302353557446,2.00613363220885,5.80569090362502));
#51794=CARTESIAN_POINT('Ctrl Pts',(0.308166547635754,2.00568879978513,5.80566199531376));
#51795=CARTESIAN_POINT('Ctrl Pts',(0.308102400514926,2.00547945003885,5.80564839882585));
#51796=CARTESIAN_POINT('Ctrl Pts',(0.307955734082109,2.00500252700914,5.80561744366719));
#51797=CARTESIAN_POINT('Ctrl Pts',(0.307873079518545,2.00473499625837,5.80560009308697));
#51798=CARTESIAN_POINT('Ctrl Pts',(0.307619976798715,2.0039195401112,5.80554724809682));
#51799=CARTESIAN_POINT('Ctrl Pts',(0.307448412649413,2.00337195816212,5.80551181901625));
#51800=CARTESIAN_POINT('Ctrl Pts',(0.30620032716099,1.99942541545164,5.80525686241967));
#51801=CARTESIAN_POINT('Ctrl Pts',(0.30506887653216,1.99604390088875,5.80504048894138));
#51802=CARTESIAN_POINT('Ctrl Pts',(0.294493729131883,1.96609941553954,5.80313725717975));
#51803=CARTESIAN_POINT('Ctrl Pts',(0.281657366288508,1.94086001307461,5.80161516039086));
#51804=CARTESIAN_POINT('Ctrl Pts',(0.256043267149803,1.90354633831779,5.79905942270686));
#51805=CARTESIAN_POINT('Ctrl Pts',(0.245288537666633,1.89027252831746,5.79807636470842));
#51806=CARTESIAN_POINT('Ctrl Pts',(0.232357792902995,1.87667523740651,5.79694543064981));
#51807=CARTESIAN_POINT('Ctrl Pts',(0.231170841441897,1.87544680940788,5.7968420653537));
#51808=CARTESIAN_POINT('Ctrl Pts',(0.229366525954607,1.87360891183762,5.79668557377957));
#51809=CARTESIAN_POINT('Ctrl Pts',(0.228756362602426,1.87299239093416,5.79663276124689));
#51810=CARTESIAN_POINT('Ctrl Pts',(0.22776571596125,1.87199947216841,5.79654718615519));
#51811=CARTESIAN_POINT('Ctrl Pts',(0.227386768211736,1.87162154283818,5.79651449137108));
#51812=CARTESIAN_POINT('Ctrl Pts',(0.226658546021859,1.87089888701902,5.79645173718722));
#51813=CARTESIAN_POINT('Ctrl Pts',(0.226309421870168,1.87055401066385,5.79642168450598));
#51814=CARTESIAN_POINT('Ctrl Pts',(0.225684599339732,1.86993960379489,5.79636795759394));
#51815=CARTESIAN_POINT('Ctrl Pts',(0.225409201855043,1.86966976751159,5.79634429684534));
#51816=CARTESIAN_POINT('Ctrl Pts',(0.224861531588896,1.86913507950386,5.79629728304853));
#51817=CARTESIAN_POINT('Ctrl Pts',(0.224589273431859,1.86887021359933,5.796273930675));
#51818=CARTESIAN_POINT('Ctrl Pts',(0.223927009818201,1.8682282065497,5.79621717241763));
#51819=CARTESIAN_POINT('Ctrl Pts',(0.223536520056469,1.86785156868807,5.79618374470276));
#51820=CARTESIAN_POINT('Ctrl Pts',(0.2220696412247,1.86644385728311,5.79605831566568));
#51821=CARTESIAN_POINT('Ctrl Pts',(0.220987067153297,1.86541928172667,5.79596603380541));
#51822=CARTESIAN_POINT('Ctrl Pts',(0.20146644999483,1.84719952360078,5.79430697774524));
#51823=CARTESIAN_POINT('Ctrl Pts',(0.181084603971428,1.8322227460614,5.79264247960456));
#51824=CARTESIAN_POINT('Ctrl Pts',(0.145501682547115,1.81201113453771,5.78987848022741));
#51825=CARTESIAN_POINT('Ctrl Pts',(0.131281770755558,1.80525697047362,5.78880830785901));
#51826=CARTESIAN_POINT('Ctrl Pts',(0.110701385478685,1.79726784032876,5.78734757530022));
#51827=CARTESIAN_POINT('Ctrl Pts',(0.104710271454859,1.79514375906814,5.78693247221359));
#51828=CARTESIAN_POINT('Ctrl Pts',(0.0958170873609895,1.79228393199961,
5.78633481790563));
#51829=CARTESIAN_POINT('Ctrl Pts',(0.0929616102911164,1.79140927862978,
5.78614567828058));
#51830=CARTESIAN_POINT('Ctrl Pts',(0.0896095238059031,1.79043326444257,
5.7859271905957));
#51831=CARTESIAN_POINT('Ctrl Pts',(0.0891244469151923,1.79029326211606,
5.78589565982756));
#51832=CARTESIAN_POINT('Ctrl Pts',(0.0883834728138306,1.7900812880484,5.78584762921457));
#51833=CARTESIAN_POINT('Ctrl Pts',(0.0881278150405387,1.79000849285541,
5.78583108154108));
#51834=CARTESIAN_POINT('Ctrl Pts',(0.0876828061165472,1.78988237742296,
5.78580232056664));
#51835=CARTESIAN_POINT('Ctrl Pts',(0.0874934967323825,1.78982891438509,
5.78579009890715));
#51836=CARTESIAN_POINT('Ctrl Pts',(0.0870650490739941,1.78970833954978,
5.78576246908865));
#51837=CARTESIAN_POINT('Ctrl Pts',(0.0868258825953968,1.78964133099309,
5.78574706705088));
#51838=CARTESIAN_POINT('Ctrl Pts',(0.0861773860394172,1.78946044651568,
5.78570536197318));
#51839=CARTESIAN_POINT('Ctrl Pts',(0.0857679060335804,1.78934710295515,
5.78567909001801));
#51840=CARTESIAN_POINT('Ctrl Pts',(0.0839259139530756,1.78884116145351,
5.78556118213063));
#51841=CARTESIAN_POINT('Ctrl Pts',(0.0824908926259773,1.7884576518811,5.78547006672072));
#51842=CARTESIAN_POINT('Ctrl Pts',(0.0497483552854235,1.77994930577037,
5.78340689894929));
#51843=CARTESIAN_POINT('Ctrl Pts',(0.0173913404426572,1.77657191857647,
5.78168207786853));
#51844=CARTESIAN_POINT('Ctrl Pts',(-0.0303441735639067,1.77878594144837,
5.77897111280782));
#51845=CARTESIAN_POINT('Ctrl Pts',(-0.0456837672685981,1.78060660481738,
5.77807696802879));
#51846=CARTESIAN_POINT('Ctrl Pts',(-0.0632378049101153,1.7839807704066,
5.77699870942219));
#51847=CARTESIAN_POINT('Ctrl Pts',(-0.0656374223046792,1.78447044239117,
5.77685013519579));
#51848=CARTESIAN_POINT('Ctrl Pts',(-0.0687225653146081,1.78513672021664,
5.77665752061109));
#51849=CARTESIAN_POINT('Ctrl Pts',(-0.0694134569845473,1.78528830985131,
5.77661428275099));
#51850=CARTESIAN_POINT('Ctrl Pts',(-0.0705272969504663,1.78553654547421,
5.77654440665554));
#51851=CARTESIAN_POINT('Ctrl Pts',(-0.0709505615512972,1.78563177377465,
5.77651781396503));
#51852=CARTESIAN_POINT('Ctrl Pts',(-0.0717572715552396,1.7858149838466,
5.77646705459217));
#51853=CARTESIAN_POINT('Ctrl Pts',(-0.0721407509518494,1.7859028136925,
5.77644289283263));
#51854=CARTESIAN_POINT('Ctrl Pts',(-0.0730159541299354,1.78610495236971,
5.77638767412367));
#51855=CARTESIAN_POINT('Ctrl Pts',(-0.0735075711692978,1.78621971467205,
5.77635660263584));
#51856=CARTESIAN_POINT('Ctrl Pts',(-0.0750105998791512,1.78657430545039,
5.77626144031217));
#51857=CARTESIAN_POINT('Ctrl Pts',(-0.0760211151709312,1.78681787071138,
5.77619722929066));
#51858=CARTESIAN_POINT('Ctrl Pts',(-0.0834826362918392,1.78865456703679,
5.77572136646752));
#51859=CARTESIAN_POINT('Ctrl Pts',(-0.0898837597899971,1.79044188215846,
5.77530346964419));
#51860=CARTESIAN_POINT('Ctrl Pts',(-0.098280069351014,1.7930686696114,5.77474183467616));
#51861=CARTESIAN_POINT('Ctrl Pts',(-0.100328892964028,1.79373226337854,
5.7746037123669));
#51862=CARTESIAN_POINT('Ctrl Pts',(-0.125783321773736,1.80225952572849,
5.77287423433374));
#51863=CARTESIAN_POINT('Ctrl Pts',(-0.148213958143662,1.8127664696498,5.77119840547065));
#51864=CARTESIAN_POINT('Ctrl Pts',(-0.176095641517313,1.82996899155539,
5.7689860278859));
#51865=CARTESIAN_POINT('Ctrl Pts',(-0.182808363734286,1.83446745241382,
5.76844314366138));
#51866=CARTESIAN_POINT('Ctrl Pts',(-0.194476692814756,1.84293929765491,
5.76748885006993));
#51867=CARTESIAN_POINT('Ctrl Pts',(-0.199497454972586,1.84681594557394,
5.76707448466603));
#51868=CARTESIAN_POINT('Ctrl Pts',(-0.206758363059428,1.8527724671951,5.76647337023529));
#51869=CARTESIAN_POINT('Ctrl Pts',(-0.209088395308526,1.85473989667044,
5.76628017755105));
#51870=CARTESIAN_POINT('Ctrl Pts',(-0.211773465900188,1.85707319515596,
5.76605755460009));
#51871=CARTESIAN_POINT('Ctrl Pts',(-0.212155894223305,1.85740711072704,
5.76602584713515));
#51872=CARTESIAN_POINT('Ctrl Pts',(-0.212737801821815,1.85791762914752,
5.76597760315692));
#51873=CARTESIAN_POINT('Ctrl Pts',(-0.212937851584951,1.85809357601512,
5.76596101816218));
#51874=CARTESIAN_POINT('Ctrl Pts',(-0.213285277486079,1.85839990738428,
5.76593221618894));
#51875=CARTESIAN_POINT('Ctrl Pts',(-0.213432752010577,1.85853017846088,
5.7659199907723));
#51876=CARTESIAN_POINT('Ctrl Pts',(-0.213742046386848,1.85880389722575,
5.76589435156682));
#51877=CARTESIAN_POINT('Ctrl Pts',(-0.213903840662034,1.85894737226529,
5.76588093994674));
#51878=CARTESIAN_POINT('Ctrl Pts',(-0.214355879565443,1.85934904233171,
5.76584346990755));
#51879=CARTESIAN_POINT('Ctrl Pts',(-0.214645803189693,1.8596076005616,5.76581943876788));
#51880=CARTESIAN_POINT('Ctrl Pts',(-0.215816446257672,1.86065540382703,
5.76572240723123));
#51881=CARTESIAN_POINT('Ctrl Pts',(-0.216693300071115,1.86144898239885,
5.7656497283223));
#51882=CARTESIAN_POINT('Ctrl Pts',(-0.232351593842768,1.87577777920176,
5.76435146915702));
#51883=CARTESIAN_POINT('Ctrl Pts',(-0.245845552949346,1.8906603371769,5.76322472049651));
#51884=CARTESIAN_POINT('Ctrl Pts',(-0.267613271164562,1.91969980399066,
5.76119407952408));
#51885=CARTESIAN_POINT('Ctrl Pts',(-0.276359105662823,1.93341477003469,
5.76029130180693));
#51886=CARTESIAN_POINT('Ctrl Pts',(-0.287695880101525,1.95456155558771,
5.75891464476735));
#51887=CARTESIAN_POINT('Ctrl Pts',(-0.291110440996095,1.961522712429,5.75846398847595));
#51888=CARTESIAN_POINT('Ctrl Pts',(-0.296761521501842,1.97417830515831,
5.75764347977848));
#51889=CARTESIAN_POINT('Ctrl Pts',(-0.299093192359397,1.97982614996347,
5.75727691812598));
#51890=CARTESIAN_POINT('Ctrl Pts',(-0.301595178384437,1.98641127018502,
5.75684785907323));
#51891=CARTESIAN_POINT('Ctrl Pts',(-0.301923701285814,1.98728740204127,
5.75679074127736));
#51892=CARTESIAN_POINT('Ctrl Pts',(-0.302416253927785,1.98861858794343,
5.75670390317121));
#51893=CARTESIAN_POINT('Ctrl Pts',(-0.302583084296901,1.98907260624739,
5.75667427642645));
#51894=CARTESIAN_POINT('Ctrl Pts',(-0.302870211292634,1.98985947160632,
5.75662291286098));
#51895=CARTESIAN_POINT('Ctrl Pts',(-0.302990983253272,1.99019214532241,
5.75660119192561));
#51896=CARTESIAN_POINT('Ctrl Pts',(-0.303240432305109,1.9908828127287,5.75655608565085));
#51897=CARTESIAN_POINT('Ctrl Pts',(-0.303369023960181,1.99124083651432,
5.75653269750685));
#51898=CARTESIAN_POINT('Ctrl Pts',(-0.303718044853324,1.9922180126599,5.75646884535007));
#51899=CARTESIAN_POINT('Ctrl Pts',(-0.303937213615156,1.99283761044965,
5.75642833952462));
#51900=CARTESIAN_POINT('Ctrl Pts',(-0.304760638896118,1.99518830958862,
5.75627458855151));
#51901=CARTESIAN_POINT('Ctrl Pts',(-0.305352004565568,1.99692386041463,
5.75616091720134));
#51902=CARTESIAN_POINT('Ctrl Pts',(-0.306527066306351,2.0004713271078,5.75592822628535));
#51903=CARTESIAN_POINT('Ctrl Pts',(-0.307109581823367,2.00228355507947,
5.75580917301125));
#51904=CARTESIAN_POINT('Ctrl Pts',(-0.317379047921046,2.03523136330209,
5.75364114179909));
#51905=CARTESIAN_POINT('Ctrl Pts',(-0.322299305162623,2.06764903880524,
5.75142184182319));
#51906=CARTESIAN_POINT('Ctrl Pts',(-0.322263896032269,2.1149554738878,5.74823733516237));
#51907=CARTESIAN_POINT('Ctrl Pts',(-0.321245161097404,2.12965378289162,
5.74726038670472));
#51908=CARTESIAN_POINT('Ctrl Pts',(-0.319099916130951,2.14513591319983,
5.74627740594293));
#51909=CARTESIAN_POINT('Ctrl Pts',(-0.318970925718339,2.14603863300754,
5.7462202615247));
#51910=CARTESIAN_POINT('Ctrl Pts',(-0.3187923292569,2.14725172161703,5.74614371042351));
#51911=CARTESIAN_POINT('Ctrl Pts',(-0.318746099839393,2.14756257171382,
5.74612411569842));
#51912=CARTESIAN_POINT('Ctrl Pts',(-0.318667512481556,2.148085738408,5.74609117375295));
#51913=CARTESIAN_POINT('Ctrl Pts',(-0.318635397000124,2.1482980903206,5.74607781279605));
#51914=CARTESIAN_POINT('Ctrl Pts',(-0.318573404021619,2.14870524319618,
5.74605221472523));
#51915=CARTESIAN_POINT('Ctrl Pts',(-0.318543560327155,2.1489000474343,5.74603997582303));
#51916=CARTESIAN_POINT('Ctrl Pts',(-0.318472514974431,2.14936096986873,
5.74601103786525));
#51917=CARTESIAN_POINT('Ctrl Pts',(-0.318431158500563,2.14962706356191,
5.74599434774502));
#51918=CARTESIAN_POINT('Ctrl Pts',(-0.318308755056396,2.15040817282588,
5.74594540049678));
#51919=CARTESIAN_POINT('Ctrl Pts',(-0.318226791334156,2.15092304703549,
5.74591319533897));
#51920=CARTESIAN_POINT('Ctrl Pts',(-0.317604053859782,2.15477469348178,
5.74567270147593));
#51921=CARTESIAN_POINT('Ctrl Pts',(-0.317012035522829,2.15810312910951,
5.74546726430517));
#51922=CARTESIAN_POINT('Ctrl Pts',(-0.314828137706103,2.16935182067675,
5.74477920737608));
#51923=CARTESIAN_POINT('Ctrl Pts',(-0.312990804308368,2.17722181463584,
5.74430832166821));
#51924=CARTESIAN_POINT('Ctrl Pts',(-0.3065353621125,2.20082629505893,5.74290562928294));
#51925=CARTESIAN_POINT('Ctrl Pts',(-0.301011042283634,2.2162853098696,5.74199920625989));
#51926=CARTESIAN_POINT('Ctrl Pts',(-0.288524885160847,2.24428450557417,
5.7402806638351));
#51927=CARTESIAN_POINT('Ctrl Pts',(-0.281857469217187,2.25691062747346,
5.73947357164822));
#51928=CARTESIAN_POINT('Ctrl Pts',(-0.273236127553258,2.27090324172775,
5.7385126180049));
#51929=CARTESIAN_POINT('Ctrl Pts',(-0.272077359460871,2.27274203193797,
5.73838496581106));
#51930=CARTESIAN_POINT('Ctrl Pts',(-0.267308184362823,2.2801429479829,5.73786533392497));
#51931=CARTESIAN_POINT('Ctrl Pts',(-0.263545307615271,2.28560444058553,
5.73746830524277));
#51932=CARTESIAN_POINT('Ctrl Pts',(-0.259001353804761,2.2917825683549,5.73700155967361));
#51933=CARTESIAN_POINT('Ctrl Pts',(-0.258381815859376,2.29261643748937,
5.73693818130351));
#51934=CARTESIAN_POINT('Ctrl Pts',(-0.257455306763621,2.29385096176754,
5.7368437767394));
#51935=CARTESIAN_POINT('Ctrl Pts',(-0.257151404350395,2.29425392041086,
5.73681287076288));
#51936=CARTESIAN_POINT('Ctrl Pts',(-0.256608945193304,2.29496968900571,
5.73675780901302));
#51937=CARTESIAN_POINT('Ctrl Pts',(-0.256370759386077,2.2952827798702,5.73673366786242));
#51938=CARTESIAN_POINT('Ctrl Pts',(-0.255868651698765,2.29594028932859,
5.73668285148313));
#51939=CARTESIAN_POINT('Ctrl Pts',(-0.255604606480336,2.29628461235516,
5.73665617141489));
#51940=CARTESIAN_POINT('Ctrl Pts',(-0.254908129074403,2.29718905163722,
5.73658590883799));
#51941=CARTESIAN_POINT('Ctrl Pts',(-0.254474547850597,2.29774827644576,
5.73654228085897));
#51942=CARTESIAN_POINT('Ctrl Pts',(-0.252530425392199,2.30023878615156,
5.73634715598701));
#51943=CARTESIAN_POINT('Ctrl Pts',(-0.250999747460072,2.30215418241752,
5.73619485801041));
#51944=CARTESIAN_POINT('Ctrl Pts',(-0.239658860514293,2.31601808140309,
5.73507579900811));
#51945=CARTESIAN_POINT('Ctrl Pts',(-0.229023482401768,2.32726262403565,
5.73407491891449));
#51946=CARTESIAN_POINT('Ctrl Pts',(-0.193787644780856,2.35952250849864,
5.73090250949542));
#51947=CARTESIAN_POINT('Ctrl Pts',(-0.166806463493108,2.37763484528071,
5.72864542612765));
#51948=CARTESIAN_POINT('Ctrl Pts',(-0.136239208305723,2.39206551130925,
5.72650776889335));
#51949=CARTESIAN_POINT('Ctrl Pts',(-0.134890734018903,2.39269074951912,
5.72641429385069));
#51950=CARTESIAN_POINT('Ctrl Pts',(-0.133151169938138,2.39348274596487,
5.7262948155963));
#51951=CARTESIAN_POINT('Ctrl Pts',(-0.132764037430547,2.39365807771122,
5.72626829636387));
#51952=CARTESIAN_POINT('Ctrl Pts',(-0.132150079737725,2.39393467599542,
5.72622635159065));
#51953=CARTESIAN_POINT('Ctrl Pts',(-0.131923484073053,2.39403644617334,
5.72621089508165));
#51954=CARTESIAN_POINT('Ctrl Pts',(-0.131517233199071,2.39421834016929,
5.72618322761232));
#51955=CARTESIAN_POINT('Ctrl Pts',(-0.131337623600715,2.39429856089954,
5.72617101070704));
#51956=CARTESIAN_POINT('Ctrl Pts',(-0.130915160230054,2.39448678593252,
5.72614231092519));
#51957=CARTESIAN_POINT('Ctrl Pts',(-0.130672246577873,2.39459465413079,
5.72612583653074));
#51958=CARTESIAN_POINT('Ctrl Pts',(-0.12996766376257,2.39490648812835,5.72607813148965));
#51959=CARTESIAN_POINT('Ctrl Pts',(-0.12950564588863,2.395109671233,5.72604694887368));
#51960=CARTESIAN_POINT('Ctrl Pts',(-0.126309968800665,2.39650609452702,
5.72583193699005));
#51961=CARTESIAN_POINT('Ctrl Pts',(-0.123560221627717,2.39766246904118,
5.72565031854719));
#51962=CARTESIAN_POINT('Ctrl Pts',(-0.114906770022824,2.40116099357221,
5.72508811778198));
#51963=CARTESIAN_POINT('Ctrl Pts',(-0.108949348527835,2.4033670390686,5.72471453610812));
#51964=CARTESIAN_POINT('Ctrl Pts',(-0.0880497203013235,2.41041102638192,
5.7234375654925));
#51965=CARTESIAN_POINT('Ctrl Pts',(-0.072821567161345,2.41433237614209,
5.72256489550529));
#51966=CARTESIAN_POINT('Ctrl Pts',(-0.0428376489126385,2.41975636438826,
5.7208611762729));
#51967=CARTESIAN_POINT('Ctrl Pts',(-0.0281451870300529,2.42138295424324,
5.72003266554318));
#51968=CARTESIAN_POINT('Ctrl Pts',(-0.0101383473961594,2.42213196985804,
5.71898884402014));
#51969=CARTESIAN_POINT('Ctrl Pts',(-0.0068810812781981,2.4222180036148,
5.71879894727686));
#51970=CARTESIAN_POINT('Ctrl Pts',(-0.00189330594087092,2.42227408169016,
5.71850615882642));
#51971=CARTESIAN_POINT('Ctrl Pts',(-0.00016336432746312,2.42227960142166,
5.71840424076998));
#51972=CARTESIAN_POINT('Ctrl Pts',(0.00216887711405079,2.42226826471898,
5.71826630085771));
#51973=CARTESIAN_POINT('Ctrl Pts',(0.00277122632638494,2.42226364792002,
5.71823062669442));
#51974=CARTESIAN_POINT('Ctrl Pts',(0.0090042002405497,2.42219839793129,
5.71786096559003));
#51975=CARTESIAN_POINT('Ctrl Pts',(0.0146320439378032,2.42199189519972,
5.71752283598708));
#51976=CARTESIAN_POINT('Ctrl Pts',(0.0212262050221727,2.42157670620926,
5.71712057188143));
#51977=CARTESIAN_POINT('Ctrl Pts',(0.0222007782505227,2.42151089432266,
5.71706096458906));
#51978=CARTESIAN_POINT('Ctrl Pts',(0.0236726425540074,2.4214047767629,5.71697070201268));
#51979=CARTESIAN_POINT('Ctrl Pts',(0.0241701700143458,2.42136774481667,
5.71694014956498));
#51980=CARTESIAN_POINT('Ctrl Pts',(0.0250591603829457,2.42129949941332,
5.71688548318985));
#51981=CARTESIAN_POINT('Ctrl Pts',(0.0254506568367829,2.42126872537917,
5.7168613831145));
#51982=CARTESIAN_POINT('Ctrl Pts',(0.02627779308269,2.42120218597838,5.71681041036384));
#51983=CARTESIAN_POINT('Ctrl Pts',(0.0267134179922768,2.42116624975666,
5.71678353236454));
#51984=CARTESIAN_POINT('Ctrl Pts',(0.0278682913960577,2.42106861429587,
5.71671219033035));
#51985=CARTESIAN_POINT('Ctrl Pts',(0.0285874049610076,2.42100538471379,
5.7166676782597));
#51986=CARTESIAN_POINT('Ctrl Pts',(0.031888081136572,2.42070398672882,5.7164629575731));
#51987=CARTESIAN_POINT('Ctrl Pts',(0.0344668651606478,2.42043709428932,
5.71630184783613));
#51988=CARTESIAN_POINT('Ctrl Pts',(0.0539605705825171,2.41818155123755,
5.71507485044191));
#51989=CARTESIAN_POINT('Ctrl Pts',(0.0706944722030677,2.41488628021309,
5.71396726861259));
#51990=CARTESIAN_POINT('Ctrl Pts',(0.116455667525205,2.40204251772472,5.71079617487498));
#51991=CARTESIAN_POINT('Ctrl Pts',(0.144504017689707,2.38967261991231,5.70867399907795));
#51992=CARTESIAN_POINT('Ctrl Pts',(0.171703673604288,2.37272953769918,5.70664647082098));
#51993=CARTESIAN_POINT('Ctrl Pts',(0.173006367511029,2.37190503726226,5.70654948694459));
#51994=CARTESIAN_POINT('Ctrl Pts',(0.174661350557042,2.37084085664952,5.7064264827988));
#51995=CARTESIAN_POINT('Ctrl Pts',(0.175019121405607,2.37060980055503,5.70639990446393));
#51996=CARTESIAN_POINT('Ctrl Pts',(0.175587083565339,2.37024140088314,5.70635773244519));
#51997=CARTESIAN_POINT('Ctrl Pts',(0.175797572632388,2.37010452073939,5.70634210795698));
#51998=CARTESIAN_POINT('Ctrl Pts',(0.176190726465049,2.3698482002248,5.70631293335261));
#51999=CARTESIAN_POINT('Ctrl Pts',(0.176373428488565,2.36972882118984,5.70629937933357));
#52000=CARTESIAN_POINT('Ctrl Pts',(0.176779354126597,2.36946299718756,5.70626927317869));
#52001=CARTESIAN_POINT('Ctrl Pts',(0.177002516546941,2.36931646075946,5.70625272734086));
#52002=CARTESIAN_POINT('Ctrl Pts',(0.177656931566837,2.3688855836936,5.70620422231186));
#52003=CARTESIAN_POINT('Ctrl Pts',(0.178087685506707,2.36860048162954,5.70617231410561));
#52004=CARTESIAN_POINT('Ctrl Pts',(0.179065201088069,2.36795011055405,5.7060999434479));
#52005=CARTESIAN_POINT('Ctrl Pts',(0.179611536075753,2.36758420004302,5.70605952325958));
#52006=CARTESIAN_POINT('Ctrl Pts',(0.194256997427316,2.35771026780845,5.70497663031193));
#52007=CARTESIAN_POINT('Ctrl Pts',(0.207584995705116,2.3471012168304,5.70400651664046));
#52008=CARTESIAN_POINT('Ctrl Pts',(0.236745396534201,2.31985686052574,5.70176307995427));
#52009=CARTESIAN_POINT('Ctrl Pts',(0.25176159907065,2.30248821601408,5.70050360685446));
#52010=CARTESIAN_POINT('Ctrl Pts',(0.265845525614916,2.28218295774062,5.69906802154962));
#52011=CARTESIAN_POINT('Ctrl Pts',(0.266867894727869,2.28068204165686,5.69896214191502));
#52012=CARTESIAN_POINT('Ctrl Pts',(0.268921924470235,2.27761110098055,5.69874590259292));
#52013=CARTESIAN_POINT('Ctrl Pts',(0.26995264991046,2.27604053868806,5.69863551855942));
#52014=CARTESIAN_POINT('Ctrl Pts',(0.27458400159836,2.26884721277617,5.69813070058535));
#52015=CARTESIAN_POINT('Ctrl Pts',(0.278022881426385,2.26312272313235,5.69773098904845));
#52016=CARTESIAN_POINT('Ctrl Pts',(0.281789380921575,2.25638735221986,5.69726134366988));
#52017=CARTESIAN_POINT('Ctrl Pts',(0.282293022279623,2.2554763926353,5.69719783875217));
#52018=CARTESIAN_POINT('Ctrl Pts',(0.283034495028333,2.25411977615095,5.69710328187821));
#52019=CARTESIAN_POINT('Ctrl Pts',(0.283275709579579,2.25367596797924,5.69707235071068));
#52020=CARTESIAN_POINT('Ctrl Pts',(0.283702949854325,2.25288546912238,5.69701726063319));
#52021=CARTESIAN_POINT('Ctrl Pts',(0.283889386385399,2.25253900065347,5.69699311640096));
#52022=CARTESIAN_POINT('Ctrl Pts',(0.284279996250785,2.2518099056283,5.69694231041289));
#52023=CARTESIAN_POINT('Ctrl Pts',(0.284484032478655,2.25142720685853,5.69691564385094));
#52024=CARTESIAN_POINT('Ctrl Pts',(0.285018487177012,2.25041986884669,5.69684545494302));
#52025=CARTESIAN_POINT('Ctrl Pts',(0.285347623420708,2.2497945552147,5.69680188729975));
#52026=CARTESIAN_POINT('Ctrl Pts',(0.286805243635251,2.24700303997135,5.69660740087385));
#52027=CARTESIAN_POINT('Ctrl Pts',(0.287911112270531,2.24482517888968,5.69645568744047));
#52028=CARTESIAN_POINT('Ctrl Pts',(0.295790421240226,2.22886094905362,5.69534348006815));
#52029=CARTESIAN_POINT('Ctrl Pts',(0.301594294018066,2.21462057602891,5.69434931830765));
#52030=CARTESIAN_POINT('Ctrl Pts',(0.315851898834108,2.17095075528838,5.69129971299677));
#52031=CARTESIAN_POINT('Ctrl Pts',(0.321156656626979,2.14067834545877,5.68917083618267));
#52032=CARTESIAN_POINT('Ctrl Pts',(0.322213828142119,2.1070062285022,5.68701272220404));
#52033=CARTESIAN_POINT('Ctrl Pts',(0.322266421657823,2.10389788555366,5.68681563153696));
#52034=CARTESIAN_POINT('Ctrl Pts',(0.322275363907552,2.10024594927253,5.68658695262188));
#52035=CARTESIAN_POINT('Ctrl Pts',(0.322275320699256,2.09970276066507,5.68655301379168));
#52036=CARTESIAN_POINT('Ctrl Pts',(0.32227318046278,2.09888205885579,5.68650185146313));
#52037=CARTESIAN_POINT('Ctrl Pts',(0.322272098313735,2.09860454743895,5.68648457146989));
#52038=CARTESIAN_POINT('Ctrl Pts',(0.322269522440866,2.09810834518969,5.68645371027364));
#52039=CARTESIAN_POINT('Ctrl Pts',(0.322268164571216,2.09788965473951,5.68644012144861));
#52040=CARTESIAN_POINT('Ctrl Pts',(0.322264830529612,2.0974283264848,5.68641148240982));
#52041=CARTESIAN_POINT('Ctrl Pts',(0.322262802945875,2.09718569025376,5.68639643516188));
#52042=CARTESIAN_POINT('Ctrl Pts',(0.322256634683385,2.09653543722573,5.68635615025939));
#52043=CARTESIAN_POINT('Ctrl Pts',(0.322251994639805,2.09612782390828,5.68633094068118));
#52044=CARTESIAN_POINT('Ctrl Pts',(0.322240059481081,2.09522916506435,5.68627545449753));
#52045=CARTESIAN_POINT('Ctrl Pts',(0.322232415299115,2.09473812407397,5.68624519720929));
#52046=CARTESIAN_POINT('Ctrl Pts',(0.322206194250205,2.09326946650015,5.68615487849985));
#52047=CARTESIAN_POINT('Ctrl Pts',(0.322184290450685,2.09229190442848,5.686094996838));
#52048=CARTESIAN_POINT('Ctrl Pts',(0.321879876659181,2.08100082454766,5.68540591922533));
#52049=CARTESIAN_POINT('Ctrl Pts',(0.321106669114624,2.07070533127981,5.6848023135118));
#52050=CARTESIAN_POINT('Ctrl Pts',(0.317805879462329,2.04400264937664,5.683260948556));
#52051=CARTESIAN_POINT('Ctrl Pts',(0.314503274945983,2.02772260956309,5.68234428644838));
#52052=CARTESIAN_POINT('Ctrl Pts',(0.306141697334235,1.99834792465086,5.68063145552539));
#52053=CARTESIAN_POINT('Ctrl Pts',(0.3014541483753,1.9851904535678,5.67984122179284));
#52054=CARTESIAN_POINT('Ctrl Pts',(0.295082760294708,1.97041640453826,5.67890042506923));
#52055=CARTESIAN_POINT('Ctrl Pts',(0.29421690389079,1.96846233690817,5.67877489485736));
#52056=CARTESIAN_POINT('Ctrl Pts',(0.29057838128421,1.96046660387529,5.67825647078186));
#52057=CARTESIAN_POINT('Ctrl Pts',(0.287638700329508,1.95450315225564,5.67785848172221));
#52058=CARTESIAN_POINT('Ctrl Pts',(0.284028625272619,1.94771737992242,5.67739069810518));
#52059=CARTESIAN_POINT('Ctrl Pts',(0.283535926000011,1.94680197462252,5.6773272743492));
#52060=CARTESIAN_POINT('Ctrl Pts',(0.282797387978917,1.94544558284828,5.67723281515676));
#52061=CARTESIAN_POINT('Ctrl Pts',(0.282554924747071,1.94500275807164,5.67720190014253));
#52062=CARTESIAN_POINT('Ctrl Pts',(0.282121672355839,1.94421587890324,5.6771468282319));
#52063=CARTESIAN_POINT('Ctrl Pts',(0.281931291430644,1.94387159992873,5.67712268597798));
#52064=CARTESIAN_POINT('Ctrl Pts',(0.281529644656134,1.94314840448331,5.67707187333779));
#52065=CARTESIAN_POINT('Ctrl Pts',(0.281318243272473,1.94276956453823,5.67704519812398));
#52066=CARTESIAN_POINT('Ctrl Pts',(0.280760186501039,1.94177423239412,5.6769749620248));
#52067=CARTESIAN_POINT('Ctrl Pts',(0.280412266902401,1.94115845500474,5.67693135573131));
#52068=CARTESIAN_POINT('Ctrl Pts',(0.27885085025985,1.93841604635052,5.67673646056181));
#52069=CARTESIAN_POINT('Ctrl Pts',(0.277615193542763,1.93630218526276,5.6765843729198));
#52070=CARTESIAN_POINT('Ctrl Pts',(0.268420593048042,1.92097637102988,5.67546778310713));
#52071=CARTESIAN_POINT('Ctrl Pts',(0.259547549768732,1.90833878953515,5.67446932488594));
#52072=CARTESIAN_POINT('Ctrl Pts',(0.234428682747998,1.87752148863825,5.67182949265537));
#52073=CARTESIAN_POINT('Ctrl Pts',(0.216966076158849,1.86046062677746,5.67015409278839));
#52074=CARTESIAN_POINT('Ctrl Pts',(0.19065567285789,1.84001475944158,5.66794946908287));
#52075=CARTESIAN_POINT('Ctrl Pts',(0.183332522709492,1.8347998270432,5.6673657281234));
#52076=CARTESIAN_POINT('Ctrl Pts',(0.175200675990513,1.82950709714011,5.66675684453527));
#52077=CARTESIAN_POINT('Ctrl Pts',(0.174599819420961,1.82911886288199,5.66671207939098));
#52078=CARTESIAN_POINT('Ctrl Pts',(0.173758823435224,1.82857942704932,5.66664974227395));
#52079=CARTESIAN_POINT('Ctrl Pts',(0.173519775156533,1.82842654074152,5.66663205915881));
#52080=CARTESIAN_POINT('Ctrl Pts',(0.173106454217469,1.82816296470914,5.66660154689277));
#52081=CARTESIAN_POINT('Ctrl Pts',(0.17293227707968,1.82805212670063,5.66658870783007));
#52082=CARTESIAN_POINT('Ctrl Pts',(0.172569949440291,1.82782204756103,5.66656203953184));
#52083=CARTESIAN_POINT('Ctrl Pts',(0.172381782056957,1.82770283428058,5.66654821222607));
#52084=CARTESIAN_POINT('Ctrl Pts',(0.17194038258395,1.82742382693615,5.66651582835683));
#52085=CARTESIAN_POINT('Ctrl Pts',(0.171687050280323,1.8272641900061,5.66649728230814));
#52086=CARTESIAN_POINT('Ctrl Pts',(0.170857353911134,1.82674297232584,5.66643667115047));
#52087=CARTESIAN_POINT('Ctrl Pts',(0.170280062281923,1.82638286061004,5.66639470298465));
#52088=CARTESIAN_POINT('Ctrl Pts',(0.168914776155318,1.82553719615057,5.66629591939255));
#52089=CARTESIAN_POINT('Ctrl Pts',(0.168125817008921,1.82505320150365,5.66623920336197));
#52090=CARTESIAN_POINT('Ctrl Pts',(0.165355068736371,1.82336984486522,5.66604126825538));
#52091=CARTESIAN_POINT('Ctrl Pts',(0.163362391365875,1.82218842490433,5.6659011388293));
#52092=CARTESIAN_POINT('Ctrl Pts',(0.157188250784807,1.81861730192732,5.66547320866404));
#52093=CARTESIAN_POINT('Ctrl Pts',(0.152965666118957,1.81629966716277,5.66518925467874));
#52094=CARTESIAN_POINT('Ctrl Pts',(0.137022174412028,1.80800833944024,5.66414330429391));
#52095=CARTESIAN_POINT('Ctrl Pts',(0.124990367536039,1.80265901351004,5.66340536470217));
#52096=CARTESIAN_POINT('Ctrl Pts',(0.0906877087635088,1.78985948056676,
5.66135753819177));
#52097=CARTESIAN_POINT('Ctrl Pts',(0.0678837871972534,1.78408377177473,
5.66005336241542));
#52098=CARTESIAN_POINT('Ctrl Pts',(0.0443095014057243,1.78078539184679,
5.65864459449509));
#52099=CARTESIAN_POINT('Ctrl Pts',(0.0439630147846903,1.78073748841599,
5.65862387743868));
#52100=CARTESIAN_POINT('Ctrl Pts',(0.0379381935890465,1.77991452187501,
5.65826343896273));
#52101=CARTESIAN_POINT('Ctrl Pts',(0.0322405523750295,1.77929053593703,
5.65791940293965));
#52102=CARTESIAN_POINT('Ctrl Pts',(0.0255509796251701,1.77873797730927,
5.65751075412378));
#52103=CARTESIAN_POINT('Ctrl Pts',(0.0245720410303623,1.77866161986268,
5.65745083609663));
#52104=CARTESIAN_POINT('Ctrl Pts',(0.0230941122956186,1.77855313408154,
5.65736019443623));
#52105=CARTESIAN_POINT('Ctrl Pts',(0.0225953651323818,1.77851769084193,
5.65732957494025));
#52106=CARTESIAN_POINT('Ctrl Pts',(0.021704633475605,1.77845647444453,5.65727483390327));
#52107=CARTESIAN_POINT('Ctrl Pts',(0.0213126797007923,1.77843025698497,
5.65725072636035));
#52108=CARTESIAN_POINT('Ctrl Pts',(0.0204851209619876,1.77837642194798,
5.65719978482904));
#52109=CARTESIAN_POINT('Ctrl Pts',(0.0200495061849004,1.77834897258276,
5.65717294561072));
#52110=CARTESIAN_POINT('Ctrl Pts',(0.0188960766874535,1.77827864384153,
5.65710181507925));
#52111=CARTESIAN_POINT('Ctrl Pts',(0.0181781749182886,1.77823728204488,
5.6570574762374));
#52112=CARTESIAN_POINT('Ctrl Pts',(0.0148995316412332,1.77805939115009,
5.65685467200544));
#52113=CARTESIAN_POINT('Ctrl Pts',(0.0123374126655923,1.77795102964437,
5.65669532597675));
#52114=CARTESIAN_POINT('Ctrl Pts',(0.00118108329803457,1.7776125117645,
5.65599755231745));
#52115=CARTESIAN_POINT('Ctrl Pts',(-0.00741842862448786,1.77769574626325,
5.65544942371332));
#52116=CARTESIAN_POINT('Ctrl Pts',(-0.0259853736189691,1.77861889337533,
5.65424301074626));
#52117=CARTESIAN_POINT('Ctrl Pts',(-0.0359377725378343,1.77957917692732,
5.65358189662956));
#52118=CARTESIAN_POINT('Ctrl Pts',(-0.0479490571053053,1.78130476658852,
5.65276933209553));
#52119=CARTESIAN_POINT('Ctrl Pts',(-0.0500661985594481,1.78163049853652,
5.65262555965485));
#52120=CARTESIAN_POINT('Ctrl Pts',(-0.0680565248867953,1.78458228068209,
5.65139954966809));
#52121=CARTESIAN_POINT('Ctrl Pts',(-0.0837155960282453,1.78837245570623,
5.65030229063019));
#52122=CARTESIAN_POINT('Ctrl Pts',(-0.103015365814818,1.79460421848962,
5.64894747261536));
#52123=CARTESIAN_POINT('Ctrl Pts',(-0.106979244317688,1.79597007938088,
5.64866917297206));
#52124=CARTESIAN_POINT('Ctrl Pts',(-0.118058533405901,1.80003127274252,
5.6478931331338));
#52125=CARTESIAN_POINT('Ctrl Pts',(-0.125107350737989,1.80290198987303,
5.64740152884588));
#52126=CARTESIAN_POINT('Ctrl Pts',(-0.132677236532066,1.80630219356559,
5.64688091896572));
#52127=CARTESIAN_POINT('Ctrl Pts',(-0.133305010669028,1.80658659752932,
5.64683780089367));
#52128=CARTESIAN_POINT('Ctrl Pts',(-0.134185856272308,1.80698906236297,
5.64677738515823));
#52129=CARTESIAN_POINT('Ctrl Pts',(-0.134439688324284,1.80710543910276,
5.64675998510387));
#52130=CARTESIAN_POINT('Ctrl Pts',(-0.134879864890374,1.80730794371257,
5.6467298287704));
#52131=CARTESIAN_POINT('Ctrl Pts',(-0.13506627841259,1.80739391974376,5.64671706311545));
#52132=CARTESIAN_POINT('Ctrl Pts',(-0.135440761480162,1.8075670697001,5.64669142958255));
#52133=CARTESIAN_POINT('Ctrl Pts',(-0.135628828869128,1.80765424686864,
5.6466785619821));
#52134=CARTESIAN_POINT('Ctrl Pts',(-0.13601515772189,1.80783377961885,5.64665214076689));
#52135=CARTESIAN_POINT('Ctrl Pts',(-0.136213409869735,1.80792615585394,
5.64663858841847));
#52136=CARTESIAN_POINT('Ctrl Pts',(-0.136881209538189,1.80823814710439,
5.64659295863402));
#52137=CARTESIAN_POINT('Ctrl Pts',(-0.137350324358735,1.80845869462952,
5.64656093877155));
#52138=CARTESIAN_POINT('Ctrl Pts',(-0.140844570835779,1.8101117697925,5.64632267520406));
#52139=CARTESIAN_POINT('Ctrl Pts',(-0.143847894497632,1.81159028355928,
5.64611922646788));
#52140=CARTESIAN_POINT('Ctrl Pts',(-0.153875716861637,1.81672253129519,
5.64544265856876));
#52141=CARTESIAN_POINT('Ctrl Pts',(-0.160788909888938,1.82058846334748,
5.64498077928952));
#52142=CARTESIAN_POINT('Ctrl Pts',(-0.173169909667254,1.8281239401837,5.64414930288855));
#52143=CARTESIAN_POINT('Ctrl Pts',(-0.17868089602663,1.83171367394219,5.64377754599345));
#52144=CARTESIAN_POINT('Ctrl Pts',(-0.200957885193175,1.84721552893903,
5.64225239834952));
#52145=CARTESIAN_POINT('Ctrl Pts',(-0.216673699879071,1.86054950013115,
5.64111892226011));
#52146=CARTESIAN_POINT('Ctrl Pts',(-0.232104167997648,1.87641269064684,
5.63984383717069));
#52147=CARTESIAN_POINT('Ctrl Pts',(-0.233188251522048,1.87754355716099,
5.63975331795452));
#52148=CARTESIAN_POINT('Ctrl Pts',(-0.235631762213985,1.88013000462552,
5.63954708109624));
#52149=CARTESIAN_POINT('Ctrl Pts',(-0.236986019245782,1.88159036491894,
5.63943119594179));
#52150=CARTESIAN_POINT('Ctrl Pts',(-0.240049828766292,1.88495626362243,
5.6391652458099));
#52151=CARTESIAN_POINT('Ctrl Pts',(-0.241750371143206,1.88686979003219,
5.63901487373053));
#52152=CARTESIAN_POINT('Ctrl Pts',(-0.247630908661074,1.89364777083966,
5.63848472424336));
#52153=CARTESIAN_POINT('Ctrl Pts',(-0.251688118290092,1.89861630702277,
5.63810047831109));
#52154=CARTESIAN_POINT('Ctrl Pts',(-0.25622079890972,1.90451819496466,5.63764755046925));
#52155=CARTESIAN_POINT('Ctrl Pts',(-0.256843477510074,1.90533705561698,
5.63758478566282));
#52156=CARTESIAN_POINT('Ctrl Pts',(-0.257764581652727,1.90656047772691,
5.63749111992739));
#52157=CARTESIAN_POINT('Ctrl Pts',(-0.258066002635016,1.90696278438782,
5.63746033646461));
#52158=CARTESIAN_POINT('Ctrl Pts',(-0.25860147708555,1.90768097795702,5.63740541219685));
#52159=CARTESIAN_POINT('Ctrl Pts',(-0.25883589664019,1.90799659170032,5.63738128574731));
#52160=CARTESIAN_POINT('Ctrl Pts',(-0.259328466589158,1.90866231093329,
5.63733041744136));
#52161=CARTESIAN_POINT('Ctrl Pts',(-0.259586486668148,1.90901251146422,
5.63730367058066));
#52162=CARTESIAN_POINT('Ctrl Pts',(-0.26026522713061,1.90993765565348,5.63723304372362));
#52163=CARTESIAN_POINT('Ctrl Pts',(-0.260684749652259,1.91051347151432,
5.63718911739745));
#52164=CARTESIAN_POINT('Ctrl Pts',(-0.262566917867694,1.91311492352801,
5.63699080517989));
#52165=CARTESIAN_POINT('Ctrl Pts',(-0.26400785492566,1.91515609250337,5.63683558567408));
#52166=CARTESIAN_POINT('Ctrl Pts',(-0.274479668810285,1.93036227005474,
5.63568176394858));
#52167=CARTESIAN_POINT('Ctrl Pts',(-0.282543538091337,1.94416335497829,
5.63464669965837));
#52168=CARTESIAN_POINT('Ctrl Pts',(-0.297615383437988,1.97500551822084,
5.6323635337471));
#52169=CARTESIAN_POINT('Ctrl Pts',(-0.304253923772735,1.99216668078398,
5.63111042013613));
#52170=CARTESIAN_POINT('Ctrl Pts',(-0.309886064193154,2.01148508737114,
5.62975751988349));
#52171=CARTESIAN_POINT('Ctrl Pts',(-0.310364023576022,2.01317583560878,
5.62963960736586));
#52172=CARTESIAN_POINT('Ctrl Pts',(-0.312726390681261,2.02180139433576,
5.62904080334086));
#52173=CARTESIAN_POINT('Ctrl Pts',(-0.31439240951314,2.02879436228716,5.62856428317902));
#52174=CARTESIAN_POINT('Ctrl Pts',(-0.316104906935959,2.03722369826351,
5.62800471248308));
#52175=CARTESIAN_POINT('Ctrl Pts',(-0.31637738612899,2.03861167919357,5.62791305117686));
#52176=CARTESIAN_POINT('Ctrl Pts',(-0.317417728464741,2.04410205608408,
5.62755247136607));
#52177=CARTESIAN_POINT('Ctrl Pts',(-0.318115050190996,2.04821763397942,
5.62728658232325));
#52178=CARTESIAN_POINT('Ctrl Pts',(-0.31881229817931,2.0528811384461,5.62699112419491));
#52179=CARTESIAN_POINT('Ctrl Pts',(-0.318890984834883,2.05341665119765,
5.62695728313937));
#52180=CARTESIAN_POINT('Ctrl Pts',(-0.319007959322328,2.05422692419948,
5.62690621245451));
#52181=CARTESIAN_POINT('Ctrl Pts',(-0.319047241641721,2.05450153649332,
5.62688892709596));
#52182=CARTESIAN_POINT('Ctrl Pts',(-0.319114910939878,2.05497899166809,
5.62685891456161));
#52183=CARTESIAN_POINT('Ctrl Pts',(-0.319143459130584,2.05518181094585,
5.62684617822489));
#52184=CARTESIAN_POINT('Ctrl Pts',(-0.319200470052503,2.05558965897626,
5.62682059263921));
#52185=CARTESIAN_POINT('Ctrl Pts',(-0.319228928580053,2.0557946877686,5.62680774368089));
#52186=CARTESIAN_POINT('Ctrl Pts',(-0.319287117427322,2.05621689458369,
5.62678131118779));
#52187=CARTESIAN_POINT('Ctrl Pts',(-0.319316823792063,2.05643407617212,
5.62676772900798));
#52188=CARTESIAN_POINT('Ctrl Pts',(-0.319385575835655,2.05694056669194,
5.62673608759647));
#52189=CARTESIAN_POINT('Ctrl Pts',(-0.319424450120711,2.05722989928284,
5.62671803805719));
#52190=CARTESIAN_POINT('Ctrl Pts',(-0.319524800616196,2.05798455381116,
5.62667102601109));
#52191=CARTESIAN_POINT('Ctrl Pts',(-0.3195856537926,2.05844996000358,5.62664209826355));
#52192=CARTESIAN_POINT('Ctrl Pts',(-0.321386042602537,2.07245733934876,
5.62577337477581));
#52193=CARTESIAN_POINT('Ctrl Pts',(-0.322264489247042,2.08609776830945,
5.62498113170366));
#52194=CARTESIAN_POINT('Ctrl Pts',(-0.322274906241924,2.09975417128097,
5.62420562594364));
#52195=CARTESIAN_POINT('',(-0.32227484120197,2.10029389008051,5.37446215688076));
#52196=CARTESIAN_POINT('Ctrl Pts',(-0.322274905917569,2.09975374642723,
5.62420565006981));
#52197=CARTESIAN_POINT('Ctrl Pts',(-0.322293894667884,2.12460454413308,
5.62279444786394));
#52198=CARTESIAN_POINT('Ctrl Pts',(-0.319438607195465,2.14937501801755,
5.62143993016761));
#52199=CARTESIAN_POINT('Ctrl Pts',(-0.311278981273533,2.18417309598891,
5.61937801561696));
#52200=CARTESIAN_POINT('Ctrl Pts',(-0.308258119663738,2.19463935704238,
5.6187372750986));
#52201=CARTESIAN_POINT('Ctrl Pts',(-0.304069280760107,2.20680339728441,
5.61795911815928));
#52202=CARTESIAN_POINT('Ctrl Pts',(-0.303407616867518,2.20866881304729,
5.61783884301304));
#52203=CARTESIAN_POINT('Ctrl Pts',(-0.302504689623937,2.21114187092898,
5.617678094228));
#52204=CARTESIAN_POINT('Ctrl Pts',(-0.302278690593447,2.21175507112102,
5.61763812973989));
#52205=CARTESIAN_POINT('Ctrl Pts',(-0.301903736363279,2.21276297073116,
5.61757226429109));
#52206=CARTESIAN_POINT('Ctrl Pts',(-0.301755867778648,2.21315807464206,
5.61754639969638));
#52207=CARTESIAN_POINT('Ctrl Pts',(-0.301467219349389,2.21392475222246,
5.61749612320407));
#52208=CARTESIAN_POINT('Ctrl Pts',(-0.301326527198473,2.21429635827734,
5.61747171428079));
#52209=CARTESIAN_POINT('Ctrl Pts',(-0.300999190531556,2.21515613780619,
5.6174151464042));
#52210=CARTESIAN_POINT('Ctrl Pts',(-0.300812045404396,2.21564411835274,
5.61738297070147));
#52211=CARTESIAN_POINT('Ctrl Pts',(-0.300304982880674,2.21695672377719,
5.61729623299978));
#52212=CARTESIAN_POINT('Ctrl Pts',(-0.2999828579708,2.21778048598279,5.61724159689273));
#52213=CARTESIAN_POINT('Ctrl Pts',(-0.297626458039936,2.22373407164333,
5.61684525043928));
#52214=CARTESIAN_POINT('Ctrl Pts',(-0.295464217979859,2.22881195138932,
5.61649923736257));
#52215=CARTESIAN_POINT('Ctrl Pts',(-0.280736314402415,2.26107504369753,
5.61424720354848));
#52216=CARTESIAN_POINT('Ctrl Pts',(-0.264564745827502,2.28644791314324,
5.61220782711879));
#52217=CARTESIAN_POINT('Ctrl Pts',(-0.241056891363572,2.31399095526909,
5.60976901817959));
#52218=CARTESIAN_POINT('Ctrl Pts',(-0.236844384934662,2.31864422515869,
5.6093487271038));
#52219=CARTESIAN_POINT('Ctrl Pts',(-0.226727449209503,2.32918397084104,
5.60838209454529));
#52220=CARTESIAN_POINT('Ctrl Pts',(-0.220724721958581,2.33497074926955,
5.60783993687223));
#52221=CARTESIAN_POINT('Ctrl Pts',(-0.213590463087684,2.34133335337852,
5.60723698184769));
#52222=CARTESIAN_POINT('Ctrl Pts',(-0.212672452975688,2.34214272905507,
5.60716014800779));
#52223=CARTESIAN_POINT('Ctrl Pts',(-0.211536672999875,2.34313266246771,
5.60706603358822));
#52224=CARTESIAN_POINT('Ctrl Pts',(-0.211323263392496,2.34331817427618,
5.60704839058749));
#52225=CARTESIAN_POINT('Ctrl Pts',(-0.210946452236227,2.34364485741056,
5.60701731118726));
#52226=CARTESIAN_POINT('Ctrl Pts',(-0.210783152840374,2.34378614549024,
5.60700386613649));
#52227=CARTESIAN_POINT('Ctrl Pts',(-0.210461243165171,2.34406409933609,
5.60697740933828));
#52228=CARTESIAN_POINT('Ctrl Pts',(-0.210302641353411,2.34420077497864,
5.60696439685787));
#52229=CARTESIAN_POINT('Ctrl Pts',(-0.209985884796363,2.34447320354668,
5.60693845365359));
#52230=CARTESIAN_POINT('Ctrl Pts',(-0.209827731937787,2.34460895726968,
5.60692552285198));
#52231=CARTESIAN_POINT('Ctrl Pts',(-0.209448290020109,2.34493402017479,
5.60689455233638));
#52232=CARTESIAN_POINT('Ctrl Pts',(-0.209226875373001,2.34512318342933,
5.60687652348263));
#52233=CARTESIAN_POINT('Ctrl Pts',(-0.208551515742056,2.3456985880163,5.60682166245034));
#52234=CARTESIAN_POINT('Ctrl Pts',(-0.208096752161335,2.34608387315052,
5.60678490034494));
#52235=CARTESIAN_POINT('Ctrl Pts',(-0.203094589444473,2.35029802707084,
5.60638246695065));
#52236=CARTESIAN_POINT('Ctrl Pts',(-0.198442798180099,2.35400193197372,
5.60602567825957));
#52237=CARTESIAN_POINT('Ctrl Pts',(-0.192125087800912,2.35875270851616,
5.60555980390401));
#52238=CARTESIAN_POINT('Ctrl Pts',(-0.190548595769804,2.35991584499391,
5.60544504616141));
#52239=CARTESIAN_POINT('Ctrl Pts',(-0.186044019973122,2.36317630939819,
5.60512105640865));
#52240=CARTESIAN_POINT('Ctrl Pts',(-0.183091193228606,2.36523906889371,
5.60491330171789));
#52241=CARTESIAN_POINT('Ctrl Pts',(-0.170188558587899,2.3739343105364,5.60402245979363));
#52242=CARTESIAN_POINT('Ctrl Pts',(-0.159908145039865,2.38005992486704,
5.60335515927367));
#52243=CARTESIAN_POINT('Ctrl Pts',(-0.138919793281672,2.39103255459073,
5.60203139366968));
#52244=CARTESIAN_POINT('Ctrl Pts',(-0.128240444816175,2.39589361271516,
5.60137591776683));
#52245=CARTESIAN_POINT('Ctrl Pts',(-0.104445479932888,2.40519404126875,
5.59991886336068));
#52246=CARTESIAN_POINT('Ctrl Pts',(-0.0912616916947774,2.40939213591887,
5.59911337662482));
#52247=CARTESIAN_POINT('Ctrl Pts',(-0.075625730148757,2.41328450242906,
5.59814054523436));
#52248=CARTESIAN_POINT('Ctrl Pts',(-0.0733954634364382,2.41381449305269,
5.59800140145558));
#52249=CARTESIAN_POINT('Ctrl Pts',(-0.070486325258787,2.41447309957748,
5.59781934661265));
#52250=CARTESIAN_POINT('Ctrl Pts',(-0.0698123903187466,2.41462339797391,
5.59777713284705));
#52251=CARTESIAN_POINT('Ctrl Pts',(-0.0687179137772091,2.41486379423668,
5.5977085127213));
#52252=CARTESIAN_POINT('Ctrl Pts',(-0.068297663235841,2.4149552187037,5.59768214894994));
#52253=CARTESIAN_POINT('Ctrl Pts',(-0.0674916840483304,2.41512886849212,
5.59763155702704));
#52254=CARTESIAN_POINT('Ctrl Pts',(-0.0671059847544436,2.41521122756137,
5.59760733321087));
#52255=CARTESIAN_POINT('Ctrl Pts',(-0.0662272027631062,2.41539718943548,
5.59755211092834));
#52256=CARTESIAN_POINT('Ctrl Pts',(-0.065734027222259,2.41550034413637,
5.59752109818129));
#52257=CARTESIAN_POINT('Ctrl Pts',(-0.0642004364224219,2.41581736461536,
5.59742459124282));
#52258=CARTESIAN_POINT('Ctrl Pts',(-0.0631592122802672,2.41602724200659,
5.59735896976916));
#52259=CARTESIAN_POINT('Ctrl Pts',(-0.0550916063346578,2.41761194996385,
5.59684973442431));
#52260=CARTESIAN_POINT('Ctrl Pts',(-0.0480226978021161,2.41875734205157,
5.5963988513845));
#52261=CARTESIAN_POINT('Ctrl Pts',(-0.0166224788965305,2.42277702701247,
5.59437311177226));
#52262=CARTESIAN_POINT('Ctrl Pts',(0.00794889355132273,2.42310640497271,
5.59271906379305));
#52263=CARTESIAN_POINT('Ctrl Pts',(0.0452498315668607,2.41934718794867,
5.59018347818709));
#52264=CARTESIAN_POINT('Ctrl Pts',(0.0580944713752727,2.41726212211376,
5.58930776522828));
#52265=CARTESIAN_POINT('Ctrl Pts',(0.0748610267401189,2.41348765742933,
5.58818655603967));
#52266=CARTESIAN_POINT('Ctrl Pts',(0.0789251841231117,2.41248920574225,
5.58791656508703));
#52267=CARTESIAN_POINT('Ctrl Pts',(0.0843454038256706,2.41104510540197,
5.5875599138755));
#52268=CARTESIAN_POINT('Ctrl Pts',(0.085719441284082,2.41066924903883,5.58746980004196));
#52269=CARTESIAN_POINT('Ctrl Pts',(0.0880120566407711,2.41002575497828,
5.58731999396892));
#52270=CARTESIAN_POINT('Ctrl Pts',(0.0889320012921847,2.40976311927848,
5.58726003111411));
#52271=CARTESIAN_POINT('Ctrl Pts',(0.0901817069604152,2.40940031367109,
5.58717878998671));
#52272=CARTESIAN_POINT('Ctrl Pts',(0.0905124849656022,2.40930370905965,
5.58715730731663));
#52273=CARTESIAN_POINT('Ctrl Pts',(0.091038990828018,2.40914902467175,5.5871231464867));
#52274=CARTESIAN_POINT('Ctrl Pts',(0.0912348183551359,2.40909128947083,
5.5871104481771));
#52275=CARTESIAN_POINT('Ctrl Pts',(0.0916422497778111,2.40897074683744,
5.58708404414975));
#52276=CARTESIAN_POINT('Ctrl Pts',(0.0918538434674642,2.40890790826087,
5.58707034039601));
#52277=CARTESIAN_POINT('Ctrl Pts',(0.0923416882031542,2.40876248376283,
5.58703876541266));
#52278=CARTESIAN_POINT('Ctrl Pts',(0.0926178939513587,2.4086797442029,5.587020903232));
#52279=CARTESIAN_POINT('Ctrl Pts',(0.0934999868431434,2.4084142159406,5.58696390463703));
#52280=CARTESIAN_POINT('Ctrl Pts',(0.094105451527379,2.40823001174897,5.58692485075662));
#52281=CARTESIAN_POINT('Ctrl Pts',(0.0995025782770252,2.40657062587088,
5.58657731345047));
#52282=CARTESIAN_POINT('Ctrl Pts',(0.104260072483303,2.40498550097454,5.58627511605419));
#52283=CARTESIAN_POINT('Ctrl Pts',(0.10925247496056,2.40319161732123,5.58596050949557));
#52284=CARTESIAN_POINT('Ctrl Pts',(0.109525864949491,2.40309296429817,5.58594328930999));
#52285=CARTESIAN_POINT('Ctrl Pts',(0.110096305234112,2.4028862478135,5.58590737471497));
#52286=CARTESIAN_POINT('Ctrl Pts',(0.110393330904645,2.40277811683474,5.58588868326479));
#52287=CARTESIAN_POINT('Ctrl Pts',(0.111022508505319,2.40254801838721,5.58584910829398));
#52288=CARTESIAN_POINT('Ctrl Pts',(0.111354619825424,2.40242594047179,5.58582822952333));
#52289=CARTESIAN_POINT('Ctrl Pts',(0.115022333895595,2.40107089658345,5.58559776541093));
#52290=CARTESIAN_POINT('Ctrl Pts',(0.118337623895132,2.3997833059733,5.58539048105336));
#52291=CARTESIAN_POINT('Ctrl Pts',(0.144040852626672,2.38930783664311,5.58378662377446));
#52292=CARTESIAN_POINT('Ctrl Pts',(0.16535174501644,2.37767921977826,5.58247038806492));
#52293=CARTESIAN_POINT('Ctrl Pts',(0.194784497416539,2.35701832717525,5.5804287686262));
#52294=CARTESIAN_POINT('Ctrl Pts',(0.204030193583439,2.3497419894129,5.57975023669485));
#52295=CARTESIAN_POINT('Ctrl Pts',(0.216969935110882,2.33835944860819,5.5787269029175));
#52296=CARTESIAN_POINT('Ctrl Pts',(0.220989615412571,2.33463751585345,5.57839765457339));
#52297=CARTESIAN_POINT('Ctrl Pts',(0.225564157568056,2.33017996168354,5.57800854652139));
#52298=CARTESIAN_POINT('Ctrl Pts',(0.226213290341575,2.32954204666287,5.57795298260532));
#52299=CARTESIAN_POINT('Ctrl Pts',(0.227199444637828,2.32856468838087,5.577868031874));
#52300=CARTESIAN_POINT('Ctrl Pts',(0.227538430694672,2.32822722662175,5.57783873249537));
#52301=CARTESIAN_POINT('Ctrl Pts',(0.228126478642944,2.3276392105419,5.57778773479919));
#52302=CARTESIAN_POINT('Ctrl Pts',(0.228375882803651,2.32738899838434,5.57776605167804));
#52303=CARTESIAN_POINT('Ctrl Pts',(0.228894762443821,2.32686672295988,5.57772082770776));
#52304=CARTESIAN_POINT('Ctrl Pts',(0.229164165321277,2.32659458861897,5.57769728370942));
#52305=CARTESIAN_POINT('Ctrl Pts',(0.22982192464791,2.32592778748829,5.57763964355417));
#52306=CARTESIAN_POINT('Ctrl Pts',(0.230209749182459,2.3255325998242,5.57760552412588));
#52307=CARTESIAN_POINT('Ctrl Pts',(0.231689606007087,2.32401685268078,5.57747481587128));
#52308=CARTESIAN_POINT('Ctrl Pts',(0.232774476901877,2.32288935950636,5.57737791535311));
#52309=CARTESIAN_POINT('Ctrl Pts',(0.250818142789262,2.30386138151041,5.5757478669752));
#52310=CARTESIAN_POINT('Ctrl Pts',(0.265671981487004,2.28408453242568,5.57412163651124));
#52311=CARTESIAN_POINT('Ctrl Pts',(0.286088100268379,2.2492088093593,5.57139342084446));
#52312=CARTESIAN_POINT('Ctrl Pts',(0.293043198854065,2.23503843736152,5.57031988158593));
#52313=CARTESIAN_POINT('Ctrl Pts',(0.302155152959246,2.21241789438034,5.5687037257685));
#52314=CARTESIAN_POINT('Ctrl Pts',(0.305054877336514,2.20429319618573,5.56814183355806));
#52315=CARTESIAN_POINT('Ctrl Pts',(0.307888536123916,2.19521871648552,5.567541627799));
#52316=CARTESIAN_POINT('Ctrl Pts',(0.308148162451034,2.19437512736893,5.56748608841484));
#52317=CARTESIAN_POINT('Ctrl Pts',(0.308536607966969,2.19309427979843,5.56740216243215));
#52318=CARTESIAN_POINT('Ctrl Pts',(0.308667968053393,2.19265780534169,5.56737363343976));
#52319=CARTESIAN_POINT('Ctrl Pts',(0.308905036577128,2.19186399112005,5.56732187775726));
#52320=CARTESIAN_POINT('Ctrl Pts',(0.309011051793809,2.19150674488712,5.56729863348237));
#52321=CARTESIAN_POINT('Ctrl Pts',(0.309184255345128,2.19091935629904,5.56726049428884));
#52322=CARTESIAN_POINT('Ctrl Pts',(0.309251806556559,2.19068932266567,5.56724557815371));
#52323=CARTESIAN_POINT('Ctrl Pts',(0.309380640668503,2.19024878321796,5.56721705063938));
#52324=CARTESIAN_POINT('Ctrl Pts',(0.309441964945319,2.19003829198646,5.56720343695138));
#52325=CARTESIAN_POINT('Ctrl Pts',(0.309581812423942,2.18955644499399,5.56717231145856));
#52326=CARTESIAN_POINT('Ctrl Pts',(0.309660193554651,2.18928504887613,5.56715480807657));
#52327=CARTESIAN_POINT('Ctrl Pts',(0.309900162912094,2.1884500335086,5.56710103912815));
#52328=CARTESIAN_POINT('Ctrl Pts',(0.310060571095411,2.18788607207843,5.56706484228345));
#52329=CARTESIAN_POINT('Ctrl Pts',(0.311258294179271,2.18363103456128,5.56679260890275));
#52330=CARTESIAN_POINT('Ctrl Pts',(0.31223126041805,2.17992195449762,5.56656022714857));
#52331=CARTESIAN_POINT('Ctrl Pts',(0.319877979054682,2.14849680332227,5.56462585872826));
#52332=CARTESIAN_POINT('Ctrl Pts',(0.322914036391696,2.1200217707311,5.56308899038667));
#52333=CARTESIAN_POINT('Ctrl Pts',(0.321681648631028,2.07322696637732,5.56044175154729));
#52334=CARTESIAN_POINT('Ctrl Pts',(0.319643736414476,2.05501544886811,5.55938282200033));
#52335=CARTESIAN_POINT('Ctrl Pts',(0.31584226296129,2.03592011826925,5.55819908850671));
#52336=CARTESIAN_POINT('Ctrl Pts',(0.315605668634554,2.03476482403635,5.55812719148735));
#52337=CARTESIAN_POINT('Ctrl Pts',(0.31525323014185,2.03309066498481,5.55802258961092));
#52338=CARTESIAN_POINT('Ctrl Pts',(0.315142432624692,2.03257073794644,5.55799004631638));
#52339=CARTESIAN_POINT('Ctrl Pts',(0.314946580069697,2.03166271015351,5.55793310850854));
#52340=CARTESIAN_POINT('Ctrl Pts',(0.314862092590016,2.03127448706113,5.55790873222972));
#52341=CARTESIAN_POINT('Ctrl Pts',(0.314697279025021,2.03052384582689,5.55786153612446));
#52342=CARTESIAN_POINT('Ctrl Pts',(0.314617044201586,2.03016140808618,5.55783871925944));
#52343=CARTESIAN_POINT('Ctrl Pts',(0.31442499543357,2.02930093057116,5.55778448001617));
#52344=CARTESIAN_POINT('Ctrl Pts',(0.314312624355159,2.02880301735542,5.55775303978618));
#52345=CARTESIAN_POINT('Ctrl Pts',(0.313911724398085,2.02704608794736,5.55764190520414));
#52346=CARTESIAN_POINT('Ctrl Pts',(0.31361681275725,2.02578855427604,5.55756200589506));
#52347=CARTESIAN_POINT('Ctrl Pts',(0.308828687669785,2.00590986330908,5.5562932808023));
#52348=CARTESIAN_POINT('Ctrl Pts',(0.302692483323738,1.9877274079924,5.55504991078165));
#52349=CARTESIAN_POINT('Ctrl Pts',(0.286572249620751,1.95109304796924,5.55237630930414));
#52350=CARTESIAN_POINT('Ctrl Pts',(0.276328586488783,1.93284914620568,5.55094532589311));
#52351=CARTESIAN_POINT('Ctrl Pts',(0.259065692322445,1.90808089219873,5.54893886601025));
#52352=CARTESIAN_POINT('Ctrl Pts',(0.253408900484507,1.90067127131184,5.54832998675162));
#52353=CARTESIAN_POINT('Ctrl Pts',(0.246847091766642,1.89280796198838,5.54768301353209));
#52354=CARTESIAN_POINT('Ctrl Pts',(0.246252749083555,1.89210192173584,5.54762491577301));
#52355=CARTESIAN_POINT('Ctrl Pts',(0.245350611575097,1.89103953792361,5.54753749858085));
#52356=CARTESIAN_POINT('Ctrl Pts',(0.245045061366366,1.8906813070507,5.54750802241737));
#52357=CARTESIAN_POINT('Ctrl Pts',(0.24448245293286,1.89002461814585,5.54745399137531));
#52358=CARTESIAN_POINT('Ctrl Pts',(0.244225631133095,1.88972596004632,5.54742941954106));
#52359=CARTESIAN_POINT('Ctrl Pts',(0.243811762763354,1.88924645357406,5.54738997149742));
#52360=CARTESIAN_POINT('Ctrl Pts',(0.243655062029273,1.88906530929861,5.54737506979359));
#52361=CARTESIAN_POINT('Ctrl Pts',(0.243354499688415,1.88871864445932,5.54734655324297));
#52362=CARTESIAN_POINT('Ctrl Pts',(0.243210672265955,1.88855309741232,5.54733293612317));
#52363=CARTESIAN_POINT('Ctrl Pts',(0.242880878483438,1.88817428258693,5.54730177806359));
#52364=CARTESIAN_POINT('Ctrl Pts',(0.242694800429434,1.88796111315036,5.54728424560988));
#52365=CARTESIAN_POINT('Ctrl Pts',(0.242120708284581,1.88730518380969,5.54723029986725));
#52366=CARTESIAN_POINT('Ctrl Pts',(0.24173175877594,1.88686323867884,5.54719395595913));
#52367=CARTESIAN_POINT('Ctrl Pts',(0.23876515558105,1.88351099288898,5.54691828101456));
#52368=CARTESIAN_POINT('Ctrl Pts',(0.236136103796485,1.88064632784557,5.54668270907939));
#52369=CARTESIAN_POINT('Ctrl Pts',(0.218386483405086,1.86199508612996,5.54514339696968));
#52370=CARTESIAN_POINT('Ctrl Pts',(0.201743263827784,1.84773247586465,5.54393662698129));
#52371=CARTESIAN_POINT('Ctrl Pts',(0.171893058436623,1.82701021600114,5.54190381826153));
#52372=CARTESIAN_POINT('Ctrl Pts',(0.1594621487787,1.81956743111643,5.54108988203961));
#52373=CARTESIAN_POINT('Ctrl Pts',(0.138923495294645,1.80907865097454,5.53975132959784));
#52374=CARTESIAN_POINT('Ctrl Pts',(0.131120492790419,1.80547943019854,5.53924433937148));
#52375=CARTESIAN_POINT('Ctrl Pts',(0.120817149001653,1.80121755419973,5.53857218626622));
#52376=CARTESIAN_POINT('Ctrl Pts',(0.118439254674684,1.80026699250859,5.53841689000507));
#52377=CARTESIAN_POINT('Ctrl Pts',(0.115379813999428,1.79908607421293,5.53821677982533));
#52378=CARTESIAN_POINT('Ctrl Pts',(0.114708431897085,1.79882950368659,5.53817284795284));
#52379=CARTESIAN_POINT('Ctrl Pts',(0.113628034736405,1.79842076365864,5.5381021204522));
#52380=CARTESIAN_POINT('Ctrl Pts',(0.113219556454756,1.7982671743023,5.53807537241661));
#52381=CARTESIAN_POINT('Ctrl Pts',(0.112442776375343,1.79797690155428,5.5380244928686));
#52382=CARTESIAN_POINT('Ctrl Pts',(0.112074533865669,1.79784006087773,5.53800036666766));
#52383=CARTESIAN_POINT('Ctrl Pts',(0.111236901310936,1.79753053450036,5.53794547307336));
#52384=CARTESIAN_POINT('Ctrl Pts',(0.11076735845625,1.79735826779999,5.53791469176346));
#52385=CARTESIAN_POINT('Ctrl Pts',(0.109374182318071,1.79685081342981,5.53782332954755));
#52386=CARTESIAN_POINT('Ctrl Pts',(0.108449421256802,1.79651875828853,5.5377626445148));
#52387=CARTESIAN_POINT('Ctrl Pts',(0.102108813984313,1.79427471014231,5.53734626252508));
#52388=CARTESIAN_POINT('Ctrl Pts',(0.0966445109294405,1.7925036676583,5.5369859225265));
#52389=CARTESIAN_POINT('Ctrl Pts',(0.0907289859771921,1.79075962932198,
5.53659388296296));
#52390=CARTESIAN_POINT('Ctrl Pts',(0.0903216591450512,1.79064041369291,
5.53656687854313));
#52391=CARTESIAN_POINT('Ctrl Pts',(0.0886600624377844,1.79015766217774,
5.536456680646));
#52392=CARTESIAN_POINT('Ctrl Pts',(0.087403837090714,1.78980095074159,5.53637327533756));
#52393=CARTESIAN_POINT('Ctrl Pts',(0.0821430834479778,1.78834162705317,
5.5360236078192));
#52394=CARTESIAN_POINT('Ctrl Pts',(0.0781197320298171,1.78730888621358,
5.53575524436712));
#52395=CARTESIAN_POINT('Ctrl Pts',(0.0733754512296643,1.78618836953102,
5.5354377312728));
#52396=CARTESIAN_POINT('Ctrl Pts',(0.0726726695424535,1.78602487463092,
5.53539067033124));
#52397=CARTESIAN_POINT('Ctrl Pts',(0.0452782300744373,1.77974874471338,
5.53355520272233));
#52398=CARTESIAN_POINT('Ctrl Pts',(0.0179176133821994,1.77706098853155,
5.53167013730327));
#52399=CARTESIAN_POINT('Ctrl Pts',(-0.0204371709266751,1.77818579322911,
5.52911314851227));
#52400=CARTESIAN_POINT('Ctrl Pts',(-0.0314049840513607,1.77907033868226,
5.52839368869949));
#52401=CARTESIAN_POINT('Ctrl Pts',(-0.0430107190615122,1.78060720556087,
5.52765918893693));
#52402=CARTESIAN_POINT('Ctrl Pts',(-0.0437138321390117,1.7807026777497,
5.52761479679176));
#52403=CARTESIAN_POINT('Ctrl Pts',(-0.0447191707553591,1.78084257067414,
5.52755148077596));
#52404=CARTESIAN_POINT('Ctrl Pts',(-0.0450216509713219,1.78088509926265,
5.52753245106234));
#52405=CARTESIAN_POINT('Ctrl Pts',(-0.045544585611618,1.78095938196836,
5.5274995879323));
#52406=CARTESIAN_POINT('Ctrl Pts',(-0.0457650680545207,1.7809909346434,
5.52748574304313));
#52407=CARTESIAN_POINT('Ctrl Pts',(-0.0461898915057663,1.78105217952795,
5.52745908831937));
#52408=CARTESIAN_POINT('Ctrl Pts',(-0.046394236240263,1.78108183948626,
5.52744627665958));
#52409=CARTESIAN_POINT('Ctrl Pts',(-0.0468794533654436,1.78115274335968,
5.52741587773129));
#52410=CARTESIAN_POINT('Ctrl Pts',(-0.0471603006068751,1.78119416212528,
5.52739830043288));
#52411=CARTESIAN_POINT('Ctrl Pts',(-0.0480015937746501,1.78131937031146,
5.52734569911124));
#52412=CARTESIAN_POINT('Ctrl Pts',(-0.0485618775625521,1.78140426744435,
5.52731073746318));
#52413=CARTESIAN_POINT('Ctrl Pts',(-0.0539781445485369,1.78223958839544,
5.52697341238737));
#52414=CARTESIAN_POINT('Ctrl Pts',(-0.0588169111640388,1.78309954773733,
5.52667710352944));
#52415=CARTESIAN_POINT('Ctrl Pts',(-0.084332624892313,1.78823890566646,
5.52513244071494));
#52416=CARTESIAN_POINT('Ctrl Pts',(-0.104573500604656,1.79443238944892,
5.52396705467592));
#52417=CARTESIAN_POINT('Ctrl Pts',(-0.146746379755469,1.81202319796713,
5.52141013587774));
#52418=CARTESIAN_POINT('Ctrl Pts',(-0.168267518248396,1.82404543989153,
5.52001706245288));
#52419=CARTESIAN_POINT('Ctrl Pts',(-0.189148382601726,1.83906821850734,
5.51845284771341));
#52420=CARTESIAN_POINT('Ctrl Pts',(-0.190080764579235,1.83974664629125,
5.51838253856672));
#52421=CARTESIAN_POINT('Ctrl Pts',(-0.191433725550719,1.84074224833561,
5.5182798290341));
#52422=CARTESIAN_POINT('Ctrl Pts',(-0.191857206859456,1.84105547843758,
5.51824758205778));
#52423=CARTESIAN_POINT('Ctrl Pts',(-0.192598136206746,1.8416063259489,5.51819098835226));
#52424=CARTESIAN_POINT('Ctrl Pts',(-0.192915917994448,1.84184349428685,
5.51816665919711));
#52425=CARTESIAN_POINT('Ctrl Pts',(-0.193531428825687,1.84230463626849,
5.51811942631984));
#52426=CARTESIAN_POINT('Ctrl Pts',(-0.193829208934796,1.84252854101099,
5.51809652532178));
#52427=CARTESIAN_POINT('Ctrl Pts',(-0.194538159041054,1.8430635367628,5.51804188316562));
#52428=CARTESIAN_POINT('Ctrl Pts',(-0.194948971105843,1.84337509839502,
5.51801012353151));
#52429=CARTESIAN_POINT('Ctrl Pts',(-0.196185715622039,1.8443177342251,5.51791421909141));
#52430=CARTESIAN_POINT('Ctrl Pts',(-0.197009338338682,1.84495181511588,
5.51784995568372));
#52431=CARTESIAN_POINT('Ctrl Pts',(-0.205529952321285,1.85157746294606,
5.5171809854742));
#52432=CARTESIAN_POINT('Ctrl Pts',(-0.212953473613203,1.85791096027722,
5.51656261252825));
#52433=CARTESIAN_POINT('Ctrl Pts',(-0.24124684114183,1.88435942972498,5.51405591492634));
#52434=CARTESIAN_POINT('Ctrl Pts',(-0.259648439283121,1.90691170300002,
5.51206297579435));
#52435=CARTESIAN_POINT('Ctrl Pts',(-0.280391262687232,1.94076103499131,
5.50941123382913));
#52436=CARTESIAN_POINT('Ctrl Pts',(-0.285537899331651,1.95018522254025,
5.50870605616307));
#52437=CARTESIAN_POINT('Ctrl Pts',(-0.290863299134398,1.96121236700717,
5.50793165752933));
#52438=CARTESIAN_POINT('Ctrl Pts',(-0.291511830774746,1.96257977373401,
5.50783649470384));
#52439=CARTESIAN_POINT('Ctrl Pts',(-0.292323324783649,1.96432237993624,
5.50771636381122));
#52440=CARTESIAN_POINT('Ctrl Pts',(-0.292495224231355,1.96469336082445,
5.50769085481153));
#52441=CARTESIAN_POINT('Ctrl Pts',(-0.292768914117127,1.96528697732778,
5.50765014298082));
#52442=CARTESIAN_POINT('Ctrl Pts',(-0.292871156985432,1.96550940197255,
5.50763491219748));
#52443=CARTESIAN_POINT('Ctrl Pts',(-0.293064481410822,1.96593123622593,
5.5076060718226));
#52444=CARTESIAN_POINT('Ctrl Pts',(-0.293155612172093,1.96613062061551,
5.50759245927366));
#52445=CARTESIAN_POINT('Ctrl Pts',(-0.293363641502988,1.96658699771594,
5.50756134468426));
#52446=CARTESIAN_POINT('Ctrl Pts',(-0.293480405678589,1.96684405075803,
5.50754385104543));
#52447=CARTESIAN_POINT('Ctrl Pts',(-0.29383828833047,1.96763467685022,5.50749014127575));
#52448=CARTESIAN_POINT('Ctrl Pts',(-0.2940782923008,1.96816875760393,5.50745399364673));
#52449=CARTESIAN_POINT('Ctrl Pts',(-0.295871612673212,1.97218869999091,
5.50718290196735));
#52450=CARTESIAN_POINT('Ctrl Pts',(-0.297364438556444,1.97570143447405,
5.5069515784283));
#52451=CARTESIAN_POINT('Ctrl Pts',(-0.299015871428391,1.97978755060825,
5.50668794942587));
#52452=CARTESIAN_POINT('Ctrl Pts',(-0.299235647092606,1.98033567000145,
5.50665269797099));
#52453=CARTESIAN_POINT('Ctrl Pts',(-0.299524662214626,1.98106224742794,
5.5066061138241));
#52454=CARTESIAN_POINT('Ctrl Pts',(-0.299595249622022,1.98124016391923,
5.50659471825437));
#52455=CARTESIAN_POINT('Ctrl Pts',(-0.309405440580394,2.00603128812938,
5.5050084255159));
#52456=CARTESIAN_POINT('Ctrl Pts',(-0.316076986674191,2.03175368944994,
5.50357282733193));
#52457=CARTESIAN_POINT('Ctrl Pts',(-0.321352720171683,2.07189531632057,
5.50129002417703));
#52458=CARTESIAN_POINT('Ctrl Pts',(-0.322270453599861,2.08588834095574,
5.50048798708834));
#52459=CARTESIAN_POINT('Ctrl Pts',(-0.322276865982724,2.10571836699165,
5.49931308438835));
#52460=CARTESIAN_POINT('Ctrl Pts',(-0.322120953444255,2.11153962048963,
5.49896364380085));
#52461=CARTESIAN_POINT('Ctrl Pts',(-0.321754330544614,2.11833848495581,
5.49854914231889));
#52462=CARTESIAN_POINT('Ctrl Pts',(-0.321696675001192,2.11932352229539,
5.49848893226455));
#52463=CARTESIAN_POINT('Ctrl Pts',(-0.32160292400506,2.12080831412132,5.49839793447864));
#52464=CARTESIAN_POINT('Ctrl Pts',(-0.321570184916,2.1213082808735,5.49836725211402));
#52465=CARTESIAN_POINT('Ctrl Pts',(-0.321509689437627,2.12220021695701,
5.49831244092881));
#52466=CARTESIAN_POINT('Ctrl Pts',(-0.321482381764131,2.12259221654261,
5.49828832624326));
#52467=CARTESIAN_POINT('Ctrl Pts',(-0.321423269456043,2.12341895573335,
5.49823741330481));
#52468=CARTESIAN_POINT('Ctrl Pts',(-0.321391299615117,2.12385368240307,
5.49821060990921));
#52469=CARTESIAN_POINT('Ctrl Pts',(-0.321304447842629,2.12500281608028,
5.49813967473842));
#52470=CARTESIAN_POINT('Ctrl Pts',(-0.321248065443725,2.12571710424626,
5.49809549590099));
#52471=CARTESIAN_POINT('Ctrl Pts',(-0.320981096913841,2.12896127990309,
5.49789444588954));
#52472=CARTESIAN_POINT('Ctrl Pts',(-0.320743009109898,2.13148875709897,
5.497736712605));
#52473=CARTESIAN_POINT('Ctrl Pts',(-0.319573011103134,2.14251260403641,
5.49704377104744));
#52474=CARTESIAN_POINT('Ctrl Pts',(-0.318333237040021,2.15097213975549,
5.49649896493205));
#52475=CARTESIAN_POINT('Ctrl Pts',(-0.314107253280467,2.17351849097337,
5.49501078221769));
#52476=CARTESIAN_POINT('Ctrl Pts',(-0.310511220005795,2.18747022524484,
5.49405068676668));
#52477=CARTESIAN_POINT('Ctrl Pts',(-0.298216336676489,2.22467027582034,
5.49140730119232));
#52478=CARTESIAN_POINT('Ctrl Pts',(-0.287747183095027,2.24723255818079,
5.48970685774586));
#52479=CARTESIAN_POINT('Ctrl Pts',(-0.274057626765783,2.26957470275187,
5.48805096014037));
#52480=CARTESIAN_POINT('Ctrl Pts',(-0.273313285612628,2.27077180880458,
5.48796234884667));
#52481=CARTESIAN_POINT('Ctrl Pts',(-0.272338916771984,2.27231617281539,
5.48784821907437));
#52482=CARTESIAN_POINT('Ctrl Pts',(-0.272116051929462,2.27266789883835,
5.4878222388131));
#52483=CARTESIAN_POINT('Ctrl Pts',(-0.271773386558472,2.27320638328987,
5.48778248415051));
#52484=CARTESIAN_POINT('Ctrl Pts',(-0.271654074864119,2.2733934498885,5.48776867740044));
#52485=CARTESIAN_POINT('Ctrl Pts',(-0.271418329197102,2.27376223058336,
5.48774146669893));
#52486=CARTESIAN_POINT('Ctrl Pts',(-0.2713019065783,2.27394394984873,5.48772806218924));
#52487=CARTESIAN_POINT('Ctrl Pts',(-0.27104168059063,2.27434922903433,5.48769817509327));
#52488=CARTESIAN_POINT('Ctrl Pts',(-0.270897783503091,2.27457272747079,
5.48768169892199));
#52489=CARTESIAN_POINT('Ctrl Pts',(-0.270479786466916,2.27522019179964,
5.48763398370626));
#52490=CARTESIAN_POINT('Ctrl Pts',(-0.2702049650226,2.27564369441235,5.48760279272412));
#52491=CARTESIAN_POINT('Ctrl Pts',(-0.268297965560087,2.27856733169868,
5.48738758729749));
#52492=CARTESIAN_POINT('Ctrl Pts',(-0.266632038985412,2.28104542965493,
5.48720578822395));
#52493=CARTESIAN_POINT('Ctrl Pts',(-0.261313809145535,2.28872372658117,
5.48664322048206));
#52494=CARTESIAN_POINT('Ctrl Pts',(-0.257541824439113,2.29383955116145,
5.48626945668818));
#52495=CARTESIAN_POINT('Ctrl Pts',(-0.243925213799659,2.3112074908391,5.48499168185766));
#52496=CARTESIAN_POINT('Ctrl Pts',(-0.233337482866846,2.32284927202884,
5.48411842030749));
#52497=CARTESIAN_POINT('Ctrl Pts',(-0.203686367941892,2.35101186068546,
5.48183186884205));
#52498=CARTESIAN_POINT('Ctrl Pts',(-0.183465026390983,2.36614924189718,
5.48041133467795));
#52499=CARTESIAN_POINT('Ctrl Pts',(-0.160376112338425,2.37954066762215,
5.47879259165192));
#52500=CARTESIAN_POINT('Ctrl Pts',(-0.159056980070522,2.3802933449642,5.47870015395734));
#52501=CARTESIAN_POINT('Ctrl Pts',(-0.157255744966577,2.38130429309308,
5.47857397689779));
#52502=CARTESIAN_POINT('Ctrl Pts',(-0.156778217671602,2.3815707106492,5.47854053014247));
#52503=CARTESIAN_POINT('Ctrl Pts',(-0.155966804355902,2.38202070268487,
5.4784837036182));
#52504=CARTESIAN_POINT('Ctrl Pts',(-0.155633265448059,2.38220490337309,
5.4784603463042));
#52505=CARTESIAN_POINT('Ctrl Pts',(-0.154989430400462,2.38255898009255,
5.47841526236468));
#52506=CARTESIAN_POINT('Ctrl Pts',(-0.15467917950265,2.38272893766578,5.47839353869087));
#52507=CARTESIAN_POINT('Ctrl Pts',(-0.153945226617312,2.38312943241208,
5.47834215039444));
#52508=CARTESIAN_POINT('Ctrl Pts',(-0.153521286518485,2.38335952935793,
5.47831247013925));
#52509=CARTESIAN_POINT('Ctrl Pts',(-0.152279091326095,2.38403013495172,
5.47822550902477));
#52510=CARTESIAN_POINT('Ctrl Pts',(-0.151459450707467,2.38446805440722,
5.47816813632279));
#52511=CARTESIAN_POINT('Ctrl Pts',(-0.145384368524918,2.3876801641316,5.47774293194926));
#52512=CARTESIAN_POINT('Ctrl Pts',(-0.140055283043021,2.39031190389838,
5.47737010451449));
#52513=CARTESIAN_POINT('Ctrl Pts',(-0.121897577070789,2.39866266305496,
5.47609912247734));
#52514=CARTESIAN_POINT('Ctrl Pts',(-0.108770068955668,2.40368962877323,
5.47517832157192));
#52515=CARTESIAN_POINT('Ctrl Pts',(-0.0668677783807147,2.4166693127497,
5.47224630628456));
#52516=CARTESIAN_POINT('Ctrl Pts',(-0.0372908192370373,2.42149684376432,
5.47017445976105));
#52517=CARTESIAN_POINT('Ctrl Pts',(-0.00598221325780764,2.42222291804165,
5.46819391060895));
#52518=CARTESIAN_POINT('Ctrl Pts',(-0.00449233699372369,2.42224713326685,
5.46810020094994));
#52519=CARTESIAN_POINT('Ctrl Pts',(-0.00257694369039802,2.42226497783755,
5.46798046537174));
#52520=CARTESIAN_POINT('Ctrl Pts',(-0.00215156442677821,2.4222680985684,
5.46795392074176));
#52521=CARTESIAN_POINT('Ctrl Pts',(-0.00147769125543491,2.42227170803633,
5.46791194498887));
#52522=CARTESIAN_POINT('Ctrl Pts',(-0.00122920271492537,2.42227275161544,
5.46789648282019));
#52523=CARTESIAN_POINT('Ctrl Pts',(-0.000784013611597522,2.42227410637275,
5.46786881040482));
#52524=CARTESIAN_POINT('Ctrl Pts',(-0.000587315399775385,2.42227452486449,
5.46785659420002));
#52525=CARTESIAN_POINT('Ctrl Pts',(-0.000124952233957228,2.42227508527478,
5.46782790266901));
#52526=CARTESIAN_POINT('Ctrl Pts',(0.000140712203431249,2.42227507878088,
5.46781143580907));
#52527=CARTESIAN_POINT('Ctrl Pts',(0.000910516995918739,2.42227410808326,
5.46776377390247));
#52528=CARTESIAN_POINT('Ctrl Pts',(0.00141465837598556,2.42227228942604,
5.46773262675243));
#52529=CARTESIAN_POINT('Ctrl Pts',(0.00488875817467803,2.42225160456992,
5.46751843280818));
#52530=CARTESIAN_POINT('Ctrl Pts',(0.00785846043961619,2.42219286571755,
5.46733757767998));
#52531=CARTESIAN_POINT('Ctrl Pts',(0.0171581674030124,2.42188025914563,
5.46677706451395));
#52532=CARTESIAN_POINT('Ctrl Pts',(0.0234820758094596,2.42148080358666,
5.46640438284897));
#52533=CARTESIAN_POINT('Ctrl Pts',(0.0453706828055154,2.4194487605064,5.46513138912766));
#52534=CARTESIAN_POINT('Ctrl Pts',(0.0608258639922243,2.41686951295002,
5.46426163966309));
#52535=CARTESIAN_POINT('Ctrl Pts',(0.100621616762986,2.40720788631713,5.4619719672567));
#52536=CARTESIAN_POINT('Ctrl Pts',(0.124417202303798,2.39836470541229,5.46054490197707));
#52537=CARTESIAN_POINT('Ctrl Pts',(0.148270629436193,2.38614551669515,5.45891934622149));
#52538=CARTESIAN_POINT('Ctrl Pts',(0.149603983702544,2.38545066862605,5.45882782870796));
#52539=CARTESIAN_POINT('Ctrl Pts',(0.151413515484319,2.3844915103285,5.4587027185203));
#52540=CARTESIAN_POINT('Ctrl Pts',(0.151893972011068,2.38423527821379,5.45866941211837));
#52541=CARTESIAN_POINT('Ctrl Pts',(0.152708958603905,2.38379798146093,5.45861276491664));
#52542=CARTESIAN_POINT('Ctrl Pts',(0.153043822841717,2.38361753931514,5.45858944627565));
#52543=CARTESIAN_POINT('Ctrl Pts',(0.153689639730539,2.38326806302306,5.45854439016439));
#52544=CARTESIAN_POINT('Ctrl Pts',(0.154000635106508,2.38309910857253,5.45852265555732));
#52545=CARTESIAN_POINT('Ctrl Pts',(0.154727533717985,2.38270265415583,5.45847176607049));
#52546=CARTESIAN_POINT('Ctrl Pts',(0.155143213740165,2.38247474857724,5.45844259673226));
#52547=CARTESIAN_POINT('Ctrl Pts',(0.156347308056751,2.38181111820341,5.45835790403401));
#52548=CARTESIAN_POINT('Ctrl Pts',(0.157134395470455,2.38137300654721,5.45830229526224));
#52549=CARTESIAN_POINT('Ctrl Pts',(0.158906659632299,2.38037676655368,5.45817651863588));
#52550=CARTESIAN_POINT('Ctrl Pts',(0.159890748660483,2.37981673670239,5.45810628272576));
#52551=CARTESIAN_POINT('Ctrl Pts',(0.16814507790996,2.37506156408967,5.4575137902397));
#52552=CARTESIAN_POINT('Ctrl Pts',(0.175251222535629,2.37058939213237,5.45698151285667));
#52553=CARTESIAN_POINT('Ctrl Pts',(0.188682598976473,2.3613853523159,5.45593029768668));
#52554=CARTESIAN_POINT('Ctrl Pts',(0.195024559863242,2.3566881992054,5.4554128409537));
#52555=CARTESIAN_POINT('Ctrl Pts',(0.219139782126374,2.33741740679355,5.45336369861132));
#52556=CARTESIAN_POINT('Ctrl Pts',(0.235504789198929,2.32119371898361,5.45178545924755));
#52557=CARTESIAN_POINT('Ctrl Pts',(0.256564615673412,2.29530446054654,5.44956552267682));
#52558=CARTESIAN_POINT('Ctrl Pts',(0.262731164915596,2.286926777387,5.44888656224427));
#52559=CARTESIAN_POINT('Ctrl Pts',(0.268890207525898,2.27765071101888,5.44818763724594));
#52560=CARTESIAN_POINT('Ctrl Pts',(0.269295785543312,2.27703530366225,5.44814150860983));
#52561=CARTESIAN_POINT('Ctrl Pts',(0.269856616078544,2.27617793567686,5.44807758319661));
#52562=CARTESIAN_POINT('Ctrl Pts',(0.270013657456531,2.27593715653396,5.44805966777851));
#52563=CARTESIAN_POINT('Ctrl Pts',(0.270283460928864,2.27552227607668,5.44802886242149));
#52564=CARTESIAN_POINT('Ctrl Pts',(0.270396377122332,2.27534827598381,5.44801596212548));
#52565=CARTESIAN_POINT('Ctrl Pts',(0.270629843543588,2.27498775023522,5.44798927327071));
#52566=CARTESIAN_POINT('Ctrl Pts',(0.270750368744672,2.27480120930266,5.44797548646491));
#52567=CARTESIAN_POINT('Ctrl Pts',(0.271034207450663,2.27436090468765,5.44794299698494));
#52568=CARTESIAN_POINT('Ctrl Pts',(0.271197358059685,2.27410703511096,5.44792430527646));
#52569=CARTESIAN_POINT('Ctrl Pts',(0.27173174612678,2.27327292996899,5.44786302555611));
#52570=CARTESIAN_POINT('Ctrl Pts',(0.272101483134963,2.27269172826021,5.44782053713983));
#52571=CARTESIAN_POINT('Ctrl Pts',(0.276846170942745,2.26518032855535,5.44727407700903));
#52572=CARTESIAN_POINT('Ctrl Pts',(0.280957525559753,2.25808617571687,5.44678705146307));
#52573=CARTESIAN_POINT('Ctrl Pts',(0.288506293656836,2.24383389999406,5.44584906930945));
#52574=CARTESIAN_POINT('Ctrl Pts',(0.291958547138894,2.23669049726903,5.44539777012987));
#52575=CARTESIAN_POINT('Ctrl Pts',(0.305341723786479,2.20617157126901,5.44351906431897));
#52576=CARTESIAN_POINT('Ctrl Pts',(0.312754930339056,2.18179421653629,5.44212900298032));
#52577=CARTESIAN_POINT('Ctrl Pts',(0.318819265534685,2.14792436198608,5.44012015199074));
#52578=CARTESIAN_POINT('Ctrl Pts',(0.32003506716393,2.13898719208069,5.43958401303356));
#52579=CARTESIAN_POINT('Ctrl Pts',(0.320979968617445,2.12888453377995,5.43896690539494));
#52580=CARTESIAN_POINT('Ctrl Pts',(0.321079425939802,2.12775713840329,5.438897888472));
#52581=CARTESIAN_POINT('Ctrl Pts',(0.321215667525561,2.1261139413605,5.43879706703203));
#52582=CARTESIAN_POINT('Ctrl Pts',(0.321257152896059,2.12559852936139,5.43876541029212));
#52583=CARTESIAN_POINT('Ctrl Pts',(0.32132825154408,2.12468780136103,5.43870941461969));
#52584=CARTESIAN_POINT('Ctrl Pts',(0.321358376244884,2.1242925254233,5.43868509180328));
#52585=CARTESIAN_POINT('Ctrl Pts',(0.321419218459153,2.12347427279631,5.4386347009419));
#52586=CARTESIAN_POINT('Ctrl Pts',(0.321449830517269,2.12305128924576,5.43860862963398));
#52587=CARTESIAN_POINT('Ctrl Pts',(0.321525268835573,2.12197953676884,5.43854251276637));
#52588=CARTESIAN_POINT('Ctrl Pts',(0.32156896629203,2.12133069254226,5.43850243184295));
#52589=CARTESIAN_POINT('Ctrl Pts',(0.32173675741375,2.11872146038745,5.43834103422671));
#52590=CARTESIAN_POINT('Ctrl Pts',(0.321844888455715,2.11676012083946,5.43821921782391));
#52591=CARTESIAN_POINT('Ctrl Pts',(0.322432636351808,2.10397343947409,5.43742170571779));
#52592=CARTESIAN_POINT('Ctrl Pts',(0.322383897912865,2.09313189967414,5.43672953335399));
#52593=CARTESIAN_POINT('Ctrl Pts',(0.32069052230028,2.06232102646898,5.43471541949836));
#52594=CARTESIAN_POINT('Ctrl Pts',(0.317730829991121,2.04247546417565,5.43335878411516));
#52595=CARTESIAN_POINT('Ctrl Pts',(0.309637878474823,2.00956831758908,5.43106752834243));
#52596=CARTESIAN_POINT('Ctrl Pts',(0.305459779482496,1.99632795488765,5.43013475321236));
#52597=CARTESIAN_POINT('Ctrl Pts',(0.300326460690109,1.98310135483789,5.42921594308472));
#52598=CARTESIAN_POINT('Ctrl Pts',(0.300211262406068,1.98280582711797,5.42919542084632));
#52599=CARTESIAN_POINT('Ctrl Pts',(0.299908418836599,1.98203229410519,5.42914172420527));
#52600=CARTESIAN_POINT('Ctrl Pts',(0.299720066270474,1.98155456444091,5.4291085810546));
#52601=CARTESIAN_POINT('Ctrl Pts',(0.298067112133717,1.97739126987797,5.42881993011546));
#52602=CARTESIAN_POINT('Ctrl Pts',(0.296535653133009,1.97373237148994,5.42856750226994));
#52603=CARTESIAN_POINT('Ctrl Pts',(0.294698281108808,1.96956055280517,5.42828190275605));
#52604=CARTESIAN_POINT('Ctrl Pts',(0.294458109043916,1.9690192826997,5.42824489116837));
#52605=CARTESIAN_POINT('Ctrl Pts',(0.294101931190119,1.9682225040807,5.42819047543847));
#52606=CARTESIAN_POINT('Ctrl Pts',(0.29398708312257,1.96796648410711,5.42817300090714));
#52607=CARTESIAN_POINT('Ctrl Pts',(0.293781759611228,1.96751037185233,5.42814188790965));
#52608=CARTESIAN_POINT('Ctrl Pts',(0.29369141400204,1.96731022198528,5.4281282414526));
#52609=CARTESIAN_POINT('Ctrl Pts',(0.29350059098803,1.96688862615203,5.4280995103009));
#52610=CARTESIAN_POINT('Ctrl Pts',(0.293400067767213,1.96666720211009,5.4280844285301));
#52611=CARTESIAN_POINT('Ctrl Pts',(0.293132859331976,1.96608038343414,5.42804447934433));
#52612=CARTESIAN_POINT('Ctrl Pts',(0.292965740870769,1.96571518476953,5.42801963867957));
#52613=CARTESIAN_POINT('Ctrl Pts',(0.292211652667885,1.96407540787467,5.42790819275321));
#52614=CARTESIAN_POINT('Ctrl Pts',(0.291617033324823,1.96280433409578,5.42782205288824));
#52615=CARTESIAN_POINT('Ctrl Pts',(0.28814752068478,1.95551228993735,5.42732907534745));
#52616=CARTESIAN_POINT('Ctrl Pts',(0.285094280581425,1.94957740358488,5.42693256799952));
#52617=CARTESIAN_POINT('Ctrl Pts',(0.278329834024467,1.93737573789517,5.42611854041927));
#52618=CARTESIAN_POINT('Ctrl Pts',(0.274586127028144,1.93113136192336,5.42570260439875));
#52619=CARTESIAN_POINT('Ctrl Pts',(0.259828133912047,1.90830596581136,5.424165114902));
#52620=CARTESIAN_POINT('Ctrl Pts',(0.247497502241578,1.89263012271813,5.42307156284944));
#52621=CARTESIAN_POINT('Ctrl Pts',(0.230500844902445,1.874714609338,5.42166477066251));
#52622=CARTESIAN_POINT('Ctrl Pts',(0.227125089732386,1.87131170155389,5.42138976452423));
#52623=CARTESIAN_POINT('Ctrl Pts',(0.221613274881717,1.86599800912481,5.420946238249));
#52624=CARTESIAN_POINT('Ctrl Pts',(0.219525398845091,1.86403819387262,5.42077943457096));
#52625=CARTESIAN_POINT('Ctrl Pts',(0.216101694065897,1.86090925778488,5.42050758014579));
#52626=CARTESIAN_POINT('Ctrl Pts',(0.214781814587858,1.85972287427596,5.42040316875304));
#52627=CARTESIAN_POINT('Ctrl Pts',(0.208613695126754,1.85427004763613,5.41991687675334));
#52628=CARTESIAN_POINT('Ctrl Pts',(0.203647973641547,1.85013928436124,5.41953000971795));
#52629=CARTESIAN_POINT('Ctrl Pts',(0.197749845275552,1.84552556728034,5.41907424830028));
#52630=CARTESIAN_POINT('Ctrl Pts',(0.196934886912207,1.84489435817163,5.41901135617647));
#52631=CARTESIAN_POINT('Ctrl Pts',(0.195717685494316,1.84396090857565,5.41891753708184));
#52632=CARTESIAN_POINT('Ctrl Pts',(0.195317734763219,1.84365567836387,5.41888672814565));
#52633=CARTESIAN_POINT('Ctrl Pts',(0.194603942961369,1.84311357448462,5.41883177533185));
#52634=CARTESIAN_POINT('Ctrl Pts',(0.194290379361589,1.84287633575352,5.41880764586522));
#52635=CARTESIAN_POINT('Ctrl Pts',(0.193629193260876,1.84237798975837,5.41875678854835));
#52636=CARTESIAN_POINT('Ctrl Pts',(0.193281475228625,1.84211701108004,5.41873005572834));
#52637=CARTESIAN_POINT('Ctrl Pts',(0.192374762481449,1.84143934465985,5.41866038028493));
#52638=CARTESIAN_POINT('Ctrl Pts',(0.191814943975307,1.84102376752825,5.418617394429));
#52639=CARTESIAN_POINT('Ctrl Pts',(0.18934745219006,1.83920443306523,5.41842806699322));
#52640=CARTESIAN_POINT('Ctrl Pts',(0.187425724830139,1.83781994245557,5.4182809805374));
#52641=CARTESIAN_POINT('Ctrl Pts',(0.182377334847451,1.83426674689942,5.41789544473136));
#52642=CARTESIAN_POINT('Ctrl Pts',(0.179227288298967,1.83213206386712,5.41765572453062));
#52643=CARTESIAN_POINT('Ctrl Pts',(0.164918298418156,1.82280073036235,5.41657019185037));
#52644=CARTESIAN_POINT('Ctrl Pts',(0.153360034625548,1.81624287598682,5.41570166793357));
#52645=CARTESIAN_POINT('Ctrl Pts',(0.131207925591312,1.80542384758623,5.41405770742067));
#52646=CARTESIAN_POINT('Ctrl Pts',(0.120727461197904,1.80097577056267,5.41328801707458));
#52647=CARTESIAN_POINT('Ctrl Pts',(0.102037788519311,1.79418658305347,5.41194242963219));
#52648=CARTESIAN_POINT('Ctrl Pts',(0.0939292555898534,1.79159951559482,
5.4113672259582));
#52649=CARTESIAN_POINT('Ctrl Pts',(0.0815339107971464,1.78817901947045,
5.41050804362356));
#52650=CARTESIAN_POINT('Ctrl Pts',(0.0773169957283992,1.78710674767852,
5.41021921162116));
#52651=CARTESIAN_POINT('Ctrl Pts',(0.0657471137855053,1.78441297344845,
5.40943825748318));
#52652=CARTESIAN_POINT('Ctrl Pts',(0.0583564098576204,1.78296308528809,
5.40895193056711));
#52653=CARTESIAN_POINT('Ctrl Pts',(0.0502422525964148,1.78166469841884,
5.40843641833261));
#52654=CARTESIAN_POINT('Ctrl Pts',(0.0495631091928234,1.78155825272675,
5.40839341082757));
#52655=CARTESIAN_POINT('Ctrl Pts',(0.0486079203664809,1.78141167079654,
5.40833312432616));
#52656=CARTESIAN_POINT('Ctrl Pts',(0.0483321616095003,1.78136971960813,
5.40831574351391));
#52657=CARTESIAN_POINT('Ctrl Pts',(0.0478534361076003,1.78129752685762,
5.40828561132349));
#52658=CARTESIAN_POINT('Ctrl Pts',(0.0476504948933998,1.78126712113224,
5.40827285060569));
#52659=CARTESIAN_POINT('Ctrl Pts',(0.0472262335667353,1.78120397031555,
5.40824620071383));
#52660=CARTESIAN_POINT('Ctrl Pts',(0.0470049085337124,1.78117126187632,
5.4082323137085));
#52661=CARTESIAN_POINT('Ctrl Pts',(0.0464758713151132,1.7810936411515,5.40819915598401));
#52662=CARTESIAN_POINT('Ctrl Pts',(0.0461681267694432,1.78104894356492,
5.40817989751453));
#52663=CARTESIAN_POINT('Ctrl Pts',(0.0451264751319401,1.78089919066125,
5.40811481027743));
#52664=CARTESIAN_POINT('Ctrl Pts',(0.0443922633853062,1.78079622142647,
5.4080690990508));
#52665=CARTESIAN_POINT('Ctrl Pts',(0.0381647343763009,1.77994474642084,
5.40768273457114));
#52666=CARTESIAN_POINT('Ctrl Pts',(0.0326529046138534,1.77933551948599,
5.40734970187929));
#52667=CARTESIAN_POINT('Ctrl Pts',(0.0192642221008671,1.77820450425854,
5.4065563883369));
#52668=CARTESIAN_POINT('Ctrl Pts',(0.0113784577495407,1.77782924057204,
5.40610215871798));
#52669=CARTESIAN_POINT('Ctrl Pts',(-0.0137561572696534,1.77755731632922,
5.40467413229642));
#52670=CARTESIAN_POINT('Ctrl Pts',(-0.0309861760079501,1.77875491439723,
5.40372344898987));
#52671=CARTESIAN_POINT('Ctrl Pts',(-0.0673168322274205,1.78423151182528,
5.40165246160266));
#52672=CARTESIAN_POINT('Ctrl Pts',(-0.0862891222075503,1.78888055311415,
5.40052931994267));
#52673=CARTESIAN_POINT('Ctrl Pts',(-0.105946983831741,1.79563494649698,
5.39926681692344));
#52674=CARTESIAN_POINT('Ctrl Pts',(-0.107167880059132,1.79606267984282,
5.39918800208811));
#52675=CARTESIAN_POINT('Ctrl Pts',(-0.108867178257717,1.79666953002278,
5.39907772802283));
#52676=CARTESIAN_POINT('Ctrl Pts',(-0.109347791099799,1.79684245499204,
5.3990464746756));
#52677=CARTESIAN_POINT('Ctrl Pts',(-0.110177064598686,1.79714305699424,
5.39899243630339));
#52678=CARTESIAN_POINT('Ctrl Pts',(-0.110525920453564,1.79727019572497,
5.39896966924437));
#52679=CARTESIAN_POINT('Ctrl Pts',(-0.111247561928675,1.79753460792449,
5.39892250185479));
#52680=CARTESIAN_POINT('Ctrl Pts',(-0.111620314866197,1.79767196831019,
5.39889809865401));
#52681=CARTESIAN_POINT('Ctrl Pts',(-0.112358354758705,1.79794548883466,
5.39884970212577));
#52682=CARTESIAN_POINT('Ctrl Pts',(-0.112723650539264,1.79808162327148,
5.3988257096936));
#52683=CARTESIAN_POINT('Ctrl Pts',(-0.113569732243776,1.79839868131572,
5.39877005007774));
#52684=CARTESIAN_POINT('Ctrl Pts',(-0.114050333417659,1.79858009197061,
5.39873836661556));
#52685=CARTESIAN_POINT('Ctrl Pts',(-0.116681519290509,1.79958046932987,
5.3985645368132));
#52686=CARTESIAN_POINT('Ctrl Pts',(-0.11882367432071,1.80042128691901,5.39842165866004));
#52687=CARTESIAN_POINT('Ctrl Pts',(-0.124354549868803,1.8026608657438,5.39804915134871));
#52688=CARTESIAN_POINT('Ctrl Pts',(-0.127728659690684,1.80409460541302,
5.39781835464009));
#52689=CARTESIAN_POINT('Ctrl Pts',(-0.140983777014739,1.80999597066668,
5.39689724830606));
#52690=CARTESIAN_POINT('Ctrl Pts',(-0.150660181207837,1.81490312124893,
5.39619236826437));
#52691=CARTESIAN_POINT('Ctrl Pts',(-0.167392974965766,1.82447876040177,
5.39491636639438));
#52692=CARTESIAN_POINT('Ctrl Pts',(-0.174548114375526,1.82895516076368,
5.39435082867938));
#52693=CARTESIAN_POINT('Ctrl Pts',(-0.202201408697887,1.84780506988692,
5.39209362140023));
#52694=CARTESIAN_POINT('Ctrl Pts',(-0.221172382961298,1.86426567315857,
5.39037543405836));
#52695=CARTESIAN_POINT('Ctrl Pts',(-0.239011923323253,1.88381368773901,
5.38870266575288));
#52696=CARTESIAN_POINT('Ctrl Pts',(-0.239968987558174,1.88487653245071,
5.38861274888465));
#52697=CARTESIAN_POINT('Ctrl Pts',(-0.241197085918644,1.88625876227192,
5.38849718074833));
#52698=CARTESIAN_POINT('Ctrl Pts',(-0.241474597981206,1.88657233193487,
5.3884710534253));
#52699=CARTESIAN_POINT('Ctrl Pts',(-0.241898533777412,1.88705323571404,
5.38843112256323));
#52700=CARTESIAN_POINT('Ctrl Pts',(-0.242045395451564,1.88722018045661,
5.38841728622338));
#52701=CARTESIAN_POINT('Ctrl Pts',(-0.242334442985935,1.8875494412091,5.38839004776032));
#52702=CARTESIAN_POINT('Ctrl Pts',(-0.242476637769516,1.88771174708801,
5.38837664501733));
#52703=CARTESIAN_POINT('Ctrl Pts',(-0.242793148449044,1.88807375585528,
5.38834680518022));
#52704=CARTESIAN_POINT('Ctrl Pts',(-0.242967380559522,1.88827353052501,
5.38833037440161));
#52705=CARTESIAN_POINT('Ctrl Pts',(-0.24347045005203,1.88885178911672,5.38828291883063));
#52706=CARTESIAN_POINT('Ctrl Pts',(-0.243798652803775,1.88923082790208,
5.38825194129602));
#52707=CARTESIAN_POINT('Ctrl Pts',(-0.245989326017422,1.89177278255795,
5.38804504422895));
#52708=CARTESIAN_POINT('Ctrl Pts',(-0.247823950678534,1.8939596801155,5.38787114475938));
#52709=CARTESIAN_POINT('Ctrl Pts',(-0.259167885967184,1.90785257956498,
5.38678976192762));
#52710=CARTESIAN_POINT('Ctrl Pts',(-0.267875889781211,1.92019108893208,
5.38593158015138));
#52711=CARTESIAN_POINT('Ctrl Pts',(-0.278556747133182,1.93783345257043,
5.38477274522406));
#52712=CARTESIAN_POINT('Ctrl Pts',(-0.281302513158801,1.94264451823446,
5.38446322460756));
#52713=CARTESIAN_POINT('Ctrl Pts',(-0.286700075641271,1.95269522624271,
5.38382556971354));
#52714=CARTESIAN_POINT('Ctrl Pts',(-0.289335382443309,1.95794133189071,
5.38349754836957));
#52715=CARTESIAN_POINT('Ctrl Pts',(-0.300817000593729,1.98244437719901,
5.38197729242602));
#52716=CARTESIAN_POINT('Ctrl Pts',(-0.30789236213191,2.00246906532676,5.38076338816379));
#52717=CARTESIAN_POINT('Ctrl Pts',(-0.31326175076767,2.02430362820246,5.37939773793129));
#52718=CARTESIAN_POINT('Ctrl Pts',(-0.313564505880587,2.025567710153,5.37931854899921));
#52719=CARTESIAN_POINT('Ctrl Pts',(-0.313975801721425,2.02733203236149,
5.37920783503972));
#52720=CARTESIAN_POINT('Ctrl Pts',(-0.314090813183097,2.02783076378029,
5.37917651807404));
#52721=CARTESIAN_POINT('Ctrl Pts',(-0.314287269731863,2.0286920356617,5.37912239936116));
#52722=CARTESIAN_POINT('Ctrl Pts',(-0.314369277024154,2.02905444795468,
5.3790996157061));
#52723=CARTESIAN_POINT('Ctrl Pts',(-0.314537626595867,2.02980445338761,
5.37905244188346));
#52724=CARTESIAN_POINT('Ctrl Pts',(-0.314623879614969,2.03019206576184,
5.37902804889419));
#52725=CARTESIAN_POINT('Ctrl Pts',(-0.314793323414977,2.03096022238409,
5.37897968168066));
#52726=CARTESIAN_POINT('Ctrl Pts',(-0.314876541083524,2.0313407600315,5.37895570836762));
#52727=CARTESIAN_POINT('Ctrl Pts',(-0.315067720504291,2.0322226429798,5.37890012134462));
#52728=CARTESIAN_POINT('Ctrl Pts',(-0.315175175672819,2.0327240959693,5.37886849145033));
#52729=CARTESIAN_POINT('Ctrl Pts',(-0.315450125074151,2.03402229860653,
5.37878654695159));
#52730=CARTESIAN_POINT('Ctrl Pts',(-0.315615797025389,2.03481942667491,
5.37873617413641));
#52731=CARTESIAN_POINT('Ctrl Pts',(-0.320119133983381,2.05690694135706,
5.3773387870345));
#52732=CARTESIAN_POINT('Ctrl Pts',(-0.322294686399018,2.07857588294554,
5.37592050230308));
#52733=CARTESIAN_POINT('Ctrl Pts',(-0.322274865791103,2.1002941161782,5.37446218470553));
#52734=CARTESIAN_POINT('',(-0.322274887569339,2.09973080273101,5.12450080716969));
#52735=CARTESIAN_POINT('Ctrl Pts',(-0.322274865994725,2.10029389297751,
5.37446219969282));
#52736=CARTESIAN_POINT('Ctrl Pts',(-0.322249612424585,2.12798625569297,
5.37260273655975));
#52737=CARTESIAN_POINT('Ctrl Pts',(-0.3186553232017,2.15556189805677,5.37068861547277));
#52738=CARTESIAN_POINT('Ctrl Pts',(-0.31132187915047,2.18331190230028,5.36887336880326));
#52739=CARTESIAN_POINT('Ctrl Pts',(-0.311060576370121,2.18428228397896,
5.36881005137164));
#52740=CARTESIAN_POINT('Ctrl Pts',(-0.310662201973125,2.18573460738666,
5.36871554284536));
#52741=CARTESIAN_POINT('Ctrl Pts',(-0.310528541506869,2.18621746665312,
5.36868416370155));
#52742=CARTESIAN_POINT('Ctrl Pts',(-0.310281228126122,2.18710287051207,
5.36862670520916));
#52743=CARTESIAN_POINT('Ctrl Pts',(-0.310167916801625,2.18750550822975,
5.36860060652096));
#52744=CARTESIAN_POINT('Ctrl Pts',(-0.309986472970255,2.188145465913,5.36855917485648));
#52745=CARTESIAN_POINT('Ctrl Pts',(-0.309918851561226,2.18838292840539,
5.36854381218281));
#52746=CARTESIAN_POINT('Ctrl Pts',(-0.309790784513868,2.18883070042786,
5.368514864467));
#52747=CARTESIAN_POINT('Ctrl Pts',(-0.309730398063365,2.18904102438796,
5.36850127614593));
#52748=CARTESIAN_POINT('Ctrl Pts',(-0.309592600187295,2.18951913334254,
5.36847040690646));
#52749=CARTESIAN_POINT('Ctrl Pts',(-0.309515055665193,2.18978687901418,
5.36845313390995));
#52750=CARTESIAN_POINT('Ctrl Pts',(-0.309278576337156,2.19059944776114,
5.36840075471699));
#52751=CARTESIAN_POINT('Ctrl Pts',(-0.309118548590051,2.19114395561384,
5.36836571217274));
#52752=CARTESIAN_POINT('Ctrl Pts',(-0.307978461256816,2.19498565672157,
5.36811885925182));
#52753=CARTESIAN_POINT('Ctrl Pts',(-0.306947060434243,2.19826755304104,
5.36790998148493));
#52754=CARTESIAN_POINT('Ctrl Pts',(-0.298003267217911,2.22521044057296,
5.36620698149002));
#52755=CARTESIAN_POINT('Ctrl Pts',(-0.287419251519737,2.24789908411726,
5.36484361909228));
#52756=CARTESIAN_POINT('Ctrl Pts',(-0.27018353699954,2.27585276902655,5.36300116544574));
#52757=CARTESIAN_POINT('Ctrl Pts',(-0.265800737583564,2.28240970523873,
5.36255631173721));
#52758=CARTESIAN_POINT('Ctrl Pts',(-0.253638006223584,2.29923545591094,
5.36136871451682));
#52759=CARTESIAN_POINT('Ctrl Pts',(-0.245476064301503,2.30920910116654,
5.36061641797045));
#52760=CARTESIAN_POINT('Ctrl Pts',(-0.235177163180014,2.32035921496239,
5.35970010914322));
#52761=CARTESIAN_POINT('Ctrl Pts',(-0.233596154298098,2.32203449725558,
5.35956030178224));
#52762=CARTESIAN_POINT('Ctrl Pts',(-0.231640788146569,2.32406245733014,
5.35938836825748));
#52763=CARTESIAN_POINT('Ctrl Pts',(-0.231283340830812,2.32443140548356,
5.35935697761181));
#52764=CARTESIAN_POINT('Ctrl Pts',(-0.230653085546425,2.32507883447451,
5.35930169749402));
#52765=CARTESIAN_POINT('Ctrl Pts',(-0.230380650887815,2.32535767857982,
5.35927782435349));
#52766=CARTESIAN_POINT('Ctrl Pts',(-0.22982957748871,2.3259196732258,5.35922957893271));
#52767=CARTESIAN_POINT('Ctrl Pts',(-0.229550919851689,2.32620280420907,
5.35920520584389));
#52768=CARTESIAN_POINT('Ctrl Pts',(-0.22901080095871,2.32674956787981,5.35915800750745));
#52769=CARTESIAN_POINT('Ctrl Pts',(-0.228749406054928,2.32701326550921,
5.35913518520563));
#52770=CARTESIAN_POINT('Ctrl Pts',(-0.228127347089528,2.32763863912682,
5.35908091982183));
#52771=CARTESIAN_POINT('Ctrl Pts',(-0.227766278580647,2.32799990975951,
5.35904945884774));
#52772=CARTESIAN_POINT('Ctrl Pts',(-0.226487702539206,2.32927313341205,
5.35893818128994));
#52773=CARTESIAN_POINT('Ctrl Pts',(-0.225565573772758,2.33018040958424,
5.35885815905579));
#52774=CARTESIAN_POINT('Ctrl Pts',(-0.210661457314349,2.3446689017759,5.3575684080615));
#52775=CARTESIAN_POINT('Ctrl Pts',(-0.19548378910435,2.35695711567857,5.35630210574563));
#52776=CARTESIAN_POINT('Ctrl Pts',(-0.169831299662873,2.37413158589911,
5.354238262045));
#52777=CARTESIAN_POINT('Ctrl Pts',(-0.160042000334104,2.37995953000421,
5.35346699606518));
#52778=CARTESIAN_POINT('Ctrl Pts',(-0.138994731187167,2.3910244937118,5.35185843227491));
#52779=CARTESIAN_POINT('Ctrl Pts',(-0.127699926459639,2.39615461849474,
5.35102261132419));
#52780=CARTESIAN_POINT('Ctrl Pts',(-0.111575249428453,2.40238395362104,
5.34988925278753));
#52781=CARTESIAN_POINT('Ctrl Pts',(-0.106973623711378,2.40404233455917,
5.34957240594026));
#52782=CARTESIAN_POINT('Ctrl Pts',(-0.100043522698501,2.40636304091178,
5.34910679245209));
#52783=CARTESIAN_POINT('Ctrl Pts',(-0.0977426235781468,2.40710486751691,
5.34895407842226));
#52784=CARTESIAN_POINT('Ctrl Pts',(-0.0949763744272689,2.40796248633253,
5.3487729011738));
#52785=CARTESIAN_POINT('Ctrl Pts',(-0.0945189167901363,2.40810319547728,
5.34874301868718));
#52786=CARTESIAN_POINT('Ctrl Pts',(-0.0938122788012034,2.40831882795594,
5.3486969827086));
#52787=CARTESIAN_POINT('Ctrl Pts',(-0.0935633207715556,2.40839446871393,
5.34868078728533));
#52788=CARTESIAN_POINT('Ctrl Pts',(-0.0931264173473537,2.4085266350497,
5.34865240732878));
#52789=CARTESIAN_POINT('Ctrl Pts',(-0.0929385127266302,2.4085832902083,
5.3486402151869));
#52790=CARTESIAN_POINT('Ctrl Pts',(-0.0925399413783279,2.40870306645484,
5.34861438279622));
#52791=CARTESIAN_POINT('Ctrl Pts',(-0.0923292624639065,2.40876614335528,
5.34860074519627));
#52792=CARTESIAN_POINT('Ctrl Pts',(-0.0917288138277761,2.40894524712427,
5.34856192518865));
#52793=CARTESIAN_POINT('Ctrl Pts',(-0.0913388870502348,2.40906075248026,
5.34853677341013));
#52794=CARTESIAN_POINT('Ctrl Pts',(-0.089675797757754,2.40954997580492,
5.34842973918893));
#52795=CARTESIAN_POINT('Ctrl Pts',(-0.0884005291084146,2.40991657396879,
5.34834826720676));
#52796=CARTESIAN_POINT('Ctrl Pts',(-0.0634419699234283,2.41692475275216,
5.34676485715235));
#52797=CARTESIAN_POINT('Ctrl Pts',(-0.0390731478370692,2.42084248359268,
5.34540985040712));
#52798=CARTESIAN_POINT('Ctrl Pts',(0.000772688522043308,2.42263613487547,
5.3431787682995));
#52799=CARTESIAN_POINT('Ctrl Pts',(0.0160665099609959,2.42223669669883,
5.3423194570174));
#52800=CARTESIAN_POINT('Ctrl Pts',(0.0408147933276175,2.41982375321389,
5.34087234814208));
#52801=CARTESIAN_POINT('Ctrl Pts',(0.0503091647327236,2.41846827311348,
5.34030369557085));
#52802=CARTESIAN_POINT('Ctrl Pts',(0.0609655111849718,2.41645847596923,
5.3396448103054));
#52803=CARTESIAN_POINT('Ctrl Pts',(0.0622012537301906,2.41621790672081,
5.33956809042691));
#52804=CARTESIAN_POINT('Ctrl Pts',(0.0638551262898368,2.41588586802663,
5.33946498103141));
#52805=CARTESIAN_POINT('Ctrl Pts',(0.0642745413199586,2.41580079497644,
5.33943879577942));
#52806=CARTESIAN_POINT('Ctrl Pts',(0.065106305784319,2.41563035641668,5.33938679214317));
#52807=CARTESIAN_POINT('Ctrl Pts',(0.0655186598730812,2.41554501762882,
5.33936097465887));
#52808=CARTESIAN_POINT('Ctrl Pts',(0.0663201302861099,2.41537751046522,
5.33931072361489));
#52809=CARTESIAN_POINT('Ctrl Pts',(0.0667092642640448,2.41529542947449,
5.33928629289381));
#52810=CARTESIAN_POINT('Ctrl Pts',(0.0676114193297003,2.4151033907833,5.33922957749078));
#52811=CARTESIAN_POINT('Ctrl Pts',(0.0681243247611521,2.41499290036056,
5.33919727578923));
#52812=CARTESIAN_POINT('Ctrl Pts',(0.0697829381395514,2.41463136023694,
5.33909263361659));
#52813=CARTESIAN_POINT('Ctrl Pts',(0.0709275360287182,2.41437531053588,
5.33902013296391));
#52814=CARTESIAN_POINT('Ctrl Pts',(0.0821855812576749,2.41179224287829,
5.33830414991492));
#52815=CARTESIAN_POINT('Ctrl Pts',(0.0921813998309867,2.4089845015729,5.33764520773177));
#52816=CARTESIAN_POINT('Ctrl Pts',(0.108425904298832,2.40356309824571,5.33653397192166));
#52817=CARTESIAN_POINT('Ctrl Pts',(0.114759211500483,2.40122590454839,5.33609029475168));
#52818=CARTESIAN_POINT('Ctrl Pts',(0.138697953576414,2.39152718591101,5.3343751204751));
#52819=CARTESIAN_POINT('Ctrl Pts',(0.155710020005394,2.38280653710142,5.33307276752409));
#52820=CARTESIAN_POINT('Ctrl Pts',(0.177895806852452,2.36882213886011,5.33131010566852));
#52821=CARTESIAN_POINT('Ctrl Pts',(0.183814092717787,2.36481059334195,5.33083337026686));
#52822=CARTESIAN_POINT('Ctrl Pts',(0.193003447917024,2.35812519800486,5.33008784690319));
#52823=CARTESIAN_POINT('Ctrl Pts',(0.196363719129032,2.35557825044378,5.32981405686595));
#52824=CARTESIAN_POINT('Ctrl Pts',(0.202151279633928,2.35100996515424,5.32934174934064));
#52825=CARTESIAN_POINT('Ctrl Pts',(0.204600594071199,2.34901755201746,5.32914162588617));
#52826=CARTESIAN_POINT('Ctrl Pts',(0.207414925368038,2.3466586496251,5.32891178695415));
#52827=CARTESIAN_POINT('Ctrl Pts',(0.207808716636984,2.34632697375386,5.32887962960817));
#52828=CARTESIAN_POINT('Ctrl Pts',(0.208406223419608,2.3458212632155,5.32883084280319));
#52829=CARTESIAN_POINT('Ctrl Pts',(0.208610517190153,2.34564791781694,5.32881416318259));
#52830=CARTESIAN_POINT('Ctrl Pts',(0.208964593694375,2.34534671994476,5.32878525677634));
#52831=CARTESIAN_POINT('Ctrl Pts',(0.209114475085133,2.34521898522771,5.32877302135175));
#52832=CARTESIAN_POINT('Ctrl Pts',(0.209428092491563,2.34495121171352,5.32874742106021));
#52833=CARTESIAN_POINT('Ctrl Pts',(0.20959180464835,2.34481114653845,5.32873405825423));
#52834=CARTESIAN_POINT('Ctrl Pts',(0.210047309458551,2.34442064412672,5.32869688022941));
#52835=CARTESIAN_POINT('Ctrl Pts',(0.210338795768285,2.34416984761533,5.32867309158664));
#52836=CARTESIAN_POINT('Ctrl Pts',(0.211502660477131,2.34316482092742,5.32857811271753));
#52837=CARTESIAN_POINT('Ctrl Pts',(0.212371450319303,2.34240642052001,5.32850722716675));
#52838=CARTESIAN_POINT('Ctrl Pts',(0.227537661166986,2.32902312433443,5.32726964584599));
#52839=CARTESIAN_POINT('Ctrl Pts',(0.240692974549557,2.31515599939262,5.32619265042133));
#52840=CARTESIAN_POINT('Ctrl Pts',(0.262322574185994,2.28787157662924,5.32424252485281));
#52841=CARTESIAN_POINT('Ctrl Pts',(0.27118275332493,2.27483923363588,5.32336922655604));
#52842=CARTESIAN_POINT('Ctrl Pts',(0.283417572359509,2.25366101669827,5.32197298481332));
#52843=CARTESIAN_POINT('Ctrl Pts',(0.287471425119374,2.24593625729544,5.32146829131679));
#52844=CARTESIAN_POINT('Ctrl Pts',(0.293947789745559,2.2322755120116,5.32057544604335));
#52845=CARTESIAN_POINT('Ctrl Pts',(0.296515779054099,2.22641399569016,5.32019228033022));
#52846=CARTESIAN_POINT('Ctrl Pts',(0.299303639607894,2.21949740504755,5.31973861473266));
#52847=CARTESIAN_POINT('Ctrl Pts',(0.299694930942479,2.21851264413984,5.3196739889381));
#52848=CARTESIAN_POINT('Ctrl Pts',(0.300271460621285,2.21704057978066,5.31957732579565));
#52849=CARTESIAN_POINT('Ctrl Pts',(0.300460387458403,2.21655472080673,5.31954541252896));
#52850=CARTESIAN_POINT('Ctrl Pts',(0.300791250263799,2.21569769789381,5.31948910239449));
#52851=CARTESIAN_POINT('Ctrl Pts',(0.300933680490832,2.21532672490426,5.31946472217123));
#52852=CARTESIAN_POINT('Ctrl Pts',(0.30120779724125,2.21460879645887,5.3194175287764));
#52853=CARTESIAN_POINT('Ctrl Pts',(0.301339571386652,2.21426187491633,5.31939471858546));
#52854=CARTESIAN_POINT('Ctrl Pts',(0.301651024765338,2.21343762607498,5.31934051145211));
#52855=CARTESIAN_POINT('Ctrl Pts',(0.30183017027645,2.21296009940515,5.31930909670753));
#52856=CARTESIAN_POINT('Ctrl Pts',(0.302363244962233,2.21152882418844,5.31921490732196));
#52857=CARTESIAN_POINT('Ctrl Pts',(0.302713790020077,2.21057382973645,5.31915201987342));
#52858=CARTESIAN_POINT('Ctrl Pts',(0.306110819346862,2.20118202771201,5.31853312797519));
#52859=CARTESIAN_POINT('Ctrl Pts',(0.308808064651436,2.19262391592803,5.31796559361946));
#52860=CARTESIAN_POINT('Ctrl Pts',(0.312328872844876,2.17957705695229,5.31709386886126));
#52861=CARTESIAN_POINT('Ctrl Pts',(0.31342002107324,2.17516462048126,5.31679798738802));
#52862=CARTESIAN_POINT('Ctrl Pts',(0.32011092718653,2.14542171626322,5.31479710262097));
#52863=CARTESIAN_POINT('Ctrl Pts',(0.322727303865083,2.11951854011185,5.31301276868194));
#52864=CARTESIAN_POINT('Ctrl Pts',(0.322010409968627,2.0834992474377,5.31061157037432));
#52865=CARTESIAN_POINT('Ctrl Pts',(0.321335976284749,2.07342532414392,5.30995012578004));
#52866=CARTESIAN_POINT('Ctrl Pts',(0.320080146487538,2.06243927694061,5.3092511849257));
#52867=CARTESIAN_POINT('Ctrl Pts',(0.319966163625463,2.0614803649815,5.3091903674611));
#52868=CARTESIAN_POINT('Ctrl Pts',(0.319761017517982,2.05981828765076,5.30908529815983));
#52869=CARTESIAN_POINT('Ctrl Pts',(0.319671841332871,2.05911489008313,5.30904093982269));
#52870=CARTESIAN_POINT('Ctrl Pts',(0.31954093823942,2.05810897878717,5.30897766335618));
#52871=CARTESIAN_POINT('Ctrl Pts',(0.319501102404894,2.05780622755562,5.30895863956429));
#52872=CARTESIAN_POINT('Ctrl Pts',(0.319431468599835,2.05728276585201,5.30892578339778));
#52873=CARTESIAN_POINT('Ctrl Pts',(0.319401872079469,2.05706202917679,5.30891193956358));
#52874=CARTESIAN_POINT('Ctrl Pts',(0.319344391188762,2.05663667347782,5.30888528446205));
#52875=CARTESIAN_POINT('Ctrl Pts',(0.319316539022994,2.05643205102634,5.3088724713741));
#52876=CARTESIAN_POINT('Ctrl Pts',(0.319249919914511,2.05594611367809,5.30884206552016));
#52877=CARTESIAN_POINT('Ctrl Pts',(0.319210977716427,2.05566482240652,5.30882448273496));
#52878=CARTESIAN_POINT('Ctrl Pts',(0.319093163325193,2.05482201572913,5.30877185418631));
#52879=CARTESIAN_POINT('Ctrl Pts',(0.31901318041588,2.05426065286748,5.308736870888));
#52880=CARTESIAN_POINT('Ctrl Pts',(0.318224209638734,2.04882598589505,5.30839884974354));
#52881=CARTESIAN_POINT('Ctrl Pts',(0.317405042719753,2.04396900297328,5.30810189374493));
#52882=CARTESIAN_POINT('Ctrl Pts',(0.314775937110119,2.03029924143429,5.30727584509019));
#52883=CARTESIAN_POINT('Ctrl Pts',(0.31270785295563,2.02154039527352,5.30675802724983));
#52884=CARTESIAN_POINT('Ctrl Pts',(0.304776102839767,1.99329199207191,5.30509291737144));
#52885=CARTESIAN_POINT('Ctrl Pts',(0.297434050760179,1.97426976662998,5.3039766664098));
#52886=CARTESIAN_POINT('Ctrl Pts',(0.281782076944971,1.94291360431153,5.30198390196496));
#52887=CARTESIAN_POINT('Ctrl Pts',(0.274325263971722,1.93022708835698,5.30112987465177));
#52888=CARTESIAN_POINT('Ctrl Pts',(0.26469148913167,1.91613806921593,5.30009992070704));
#52889=CARTESIAN_POINT('Ctrl Pts',(0.26333206950508,1.91419630058332,5.2999560914321));
#52890=CARTESIAN_POINT('Ctrl Pts',(0.261545026737307,1.91170273172328,5.29976887078169));
#52891=CARTESIAN_POINT('Ctrl Pts',(0.261136834419148,1.91113704452967,5.29972622835768));
#52892=CARTESIAN_POINT('Ctrl Pts',(0.260471215042895,1.91022088931447,5.29965688883998));
#52893=CARTESIAN_POINT('Ctrl Pts',(0.260214908131131,1.90986960710637,5.29963023516774));
#52894=CARTESIAN_POINT('Ctrl Pts',(0.259725502714694,1.90920169430879,5.29957942920904));
#52895=CARTESIAN_POINT('Ctrl Pts',(0.259492534028964,1.90888496920418,5.29955528199885));
#52896=CARTESIAN_POINT('Ctrl Pts',(0.258960229520762,1.90816405936498,5.29950019376614));
#52897=CARTESIAN_POINT('Ctrl Pts',(0.258660526480865,1.90776014817723,5.29946923845431));
#52898=CARTESIAN_POINT('Ctrl Pts',(0.257744174232607,1.90653119832636,5.29937477563744));
#52899=CARTESIAN_POINT('Ctrl Pts',(0.257124518588222,1.9057084189338,5.29931115051362));
#52900=CARTESIAN_POINT('Ctrl Pts',(0.252601311168233,1.89976203588523,5.29884851375601));
#52901=CARTESIAN_POINT('Ctrl Pts',(0.248549117561542,1.89475382785139,5.29844364065612));
#52902=CARTESIAN_POINT('Ctrl Pts',(0.243214854860084,1.88855085709718,5.29792185703795));
#52903=CARTESIAN_POINT('Ctrl Pts',(0.242069229697573,1.88724029162431,5.29781041887751));
#52904=CARTESIAN_POINT('Ctrl Pts',(0.219034718236723,1.86131629323071,5.2955820744102));
#52905=CARTESIAN_POINT('Ctrl Pts',(0.193511546820579,1.84019504360487,5.29330279454498));
#52906=CARTESIAN_POINT('Ctrl Pts',(0.157726692849757,1.81882371590439,5.29053899782507));
#52907=CARTESIAN_POINT('Ctrl Pts',(0.15003021819437,1.81464272094027,5.28996819446978));
#52908=CARTESIAN_POINT('Ctrl Pts',(0.14137323322767,1.81038719406892,5.28935909655454));
#52909=CARTESIAN_POINT('Ctrl Pts',(0.140572526422557,1.80999770123157,5.28930306313519));
#52910=CARTESIAN_POINT('Ctrl Pts',(0.139171354433488,1.80932328708003,5.28920555173677));
#52911=CARTESIAN_POINT('Ctrl Pts',(0.138571607514859,1.80903689763439,5.28916398643176));
#52912=CARTESIAN_POINT('Ctrl Pts',(0.137702223020234,1.80862504940321,5.28910398825334));
#52913=CARTESIAN_POINT('Ctrl Pts',(0.13743329600494,1.80849810770611,5.28908546411602));
#52914=CARTESIAN_POINT('Ctrl Pts',(0.136963882545658,1.80827732432458,5.28905319186774));
#52915=CARTESIAN_POINT('Ctrl Pts',(0.136763474773593,1.80818331679928,5.28903943340415));
#52916=CARTESIAN_POINT('Ctrl Pts',(0.13637397469899,1.80800109899868,5.28901273155151));
#52917=CARTESIAN_POINT('Ctrl Pts',(0.136184894151664,1.80791286613973,5.28899978674329));
#52918=CARTESIAN_POINT('Ctrl Pts',(0.135730940285783,1.80770156898069,5.28896874975771));
#52919=CARTESIAN_POINT('Ctrl Pts',(0.135465984535476,1.80757868073171,5.28895066854508));
#52920=CARTESIAN_POINT('Ctrl Pts',(0.13465669417487,1.80720466242878,5.28889554297786));
#52921=CARTESIAN_POINT('Ctrl Pts',(0.134111821689195,1.80695468902177,5.28885856962816));
#52922=CARTESIAN_POINT('Ctrl Pts',(0.128033224497069,1.80418649028142,5.28844763106513));
#52923=CARTESIAN_POINT('Ctrl Pts',(0.122429560912719,1.8018236202934,5.28808295895694));
#52924=CARTESIAN_POINT('Ctrl Pts',(0.0915041114146103,1.78980243769835,
5.28612915597707));
#52925=CARTESIAN_POINT('Ctrl Pts',(0.0651063897897951,1.78320823665236,
5.28466480923543));
#52926=CARTESIAN_POINT('Ctrl Pts',(0.0226599989319834,1.77814228589429,
5.28224129324522));
#52927=CARTESIAN_POINT('Ctrl Pts',(0.00701535455697281,1.77742202085685,
5.28133545919211));
#52928=CARTESIAN_POINT('Ctrl Pts',(-0.0110865448487909,1.77790628727999,
5.28024326934254));
#52929=CARTESIAN_POINT('Ctrl Pts',(-0.0135536986956862,1.77800067084132,
5.280093498751));
#52930=CARTESIAN_POINT('Ctrl Pts',(-0.0167279902989963,1.77815865211877,
5.27989954829253));
#52931=CARTESIAN_POINT('Ctrl Pts',(-0.0174363849161661,1.77819625338751,
5.27985618480338));
#52932=CARTESIAN_POINT('Ctrl Pts',(-0.0185782646566136,1.7782606453492,
5.27978615459769));
#52933=CARTESIAN_POINT('Ctrl Pts',(-0.0190118325690887,1.77828597408847,
5.279759533794));
#52934=CARTESIAN_POINT('Ctrl Pts',(-0.0198379317653035,1.77833591003223,
5.27970875304202));
#52935=CARTESIAN_POINT('Ctrl Pts',(-0.0202304720858855,1.77836035955044,
5.27968459808741));
#52936=CARTESIAN_POINT('Ctrl Pts',(-0.0211258969829911,1.77841777710515,
5.27962944000043));
#52937=CARTESIAN_POINT('Ctrl Pts',(-0.0216287500443039,1.77845120623419,
5.27959842244529));
#52938=CARTESIAN_POINT('Ctrl Pts',(-0.0231641490497526,1.77855689586124,
5.27950358520647));
#52939=CARTESIAN_POINT('Ctrl Pts',(-0.0241964195077273,1.77863295090733,
5.27943964653354));
#52940=CARTESIAN_POINT('Ctrl Pts',(-0.031757648939175,1.77922668023667,
5.27896997619658));
#52941=CARTESIAN_POINT('Ctrl Pts',(-0.0382694330121295,1.77993826956598,
5.27855818066542));
#52942=CARTESIAN_POINT('Ctrl Pts',(-0.0465582409532081,1.78110060722995,
5.27802408779569));
#52943=CARTESIAN_POINT('Ctrl Pts',(-0.0483596200392123,1.78136880339758,
5.27790741584851));
#52944=CARTESIAN_POINT('Ctrl Pts',(-0.0528260305989383,1.78207252724776,
5.27761664216174));
#52945=CARTESIAN_POINT('Ctrl Pts',(-0.055488010078569,1.78252630421174,
5.27744201681422));
#52946=CARTESIAN_POINT('Ctrl Pts',(-0.0853118551029541,1.78799680503545,
5.27547079466282));
#52947=CARTESIAN_POINT('Ctrl Pts',(-0.111724677724404,1.79645213079262,
5.27357269031489));
#52948=CARTESIAN_POINT('Ctrl Pts',(-0.142482069614941,1.81086269517012,
5.27130249284765));
#52949=CARTESIAN_POINT('Ctrl Pts',(-0.148153283664967,1.81372716738078,
5.27088187763395));
#52950=CARTESIAN_POINT('Ctrl Pts',(-0.158837942588785,1.81952651390357,
5.27009017637544));
#52951=CARTESIAN_POINT('Ctrl Pts',(-0.16386414149897,1.82243303133076,5.26971808846018));
#52952=CARTESIAN_POINT('Ctrl Pts',(-0.169308452348046,1.8257808052959,5.26931769588774));
#52953=CARTESIAN_POINT('Ctrl Pts',(-0.169806621729595,1.82608901078952,
5.26928108388257));
#52954=CARTESIAN_POINT('Ctrl Pts',(-0.170543686301537,1.82654779864226,
5.26922695512034));
#52955=CARTESIAN_POINT('Ctrl Pts',(-0.1707832248588,1.82669733723763,5.26920937016122));
#52956=CARTESIAN_POINT('Ctrl Pts',(-0.1711911297326,1.82695272885954,5.26917943636585));
#52957=CARTESIAN_POINT('Ctrl Pts',(-0.171359594702472,1.82705842295344,
5.26916707697144));
#52958=CARTESIAN_POINT('Ctrl Pts',(-0.171705179644935,1.82727568731986,
5.26914173007303));
#52959=CARTESIAN_POINT('Ctrl Pts',(-0.171882288340938,1.8273872739598,5.26912874372687));
#52960=CARTESIAN_POINT('Ctrl Pts',(-0.17230836727104,1.82765630360265,5.2690975103848));
#52961=CARTESIAN_POINT('Ctrl Pts',(-0.172557231150622,1.82781391589904,
5.26907927466371));
#52962=CARTESIAN_POINT('Ctrl Pts',(-0.17332050737381,1.82829878714813,5.2690233653839));
#52963=CARTESIAN_POINT('Ctrl Pts',(-0.173834211218235,1.82862716722948,
5.26898576562825));
#52964=CARTESIAN_POINT('Ctrl Pts',(-0.179812731395174,1.8324728189962,5.26854847287769));
#52965=CARTESIAN_POINT('Ctrl Pts',(-0.185171341773247,1.83615345516246,
5.26815940535848));
#52966=CARTESIAN_POINT('Ctrl Pts',(-0.194766520107832,1.84318048240553,
5.26746092743591));
#52967=CARTESIAN_POINT('Ctrl Pts',(-0.199037172804504,1.84647589638866,
5.26714934813183));
#52968=CARTESIAN_POINT('Ctrl Pts',(-0.208905315525695,1.85449369999891,
5.26642258027478));
#52969=CARTESIAN_POINT('Ctrl Pts',(-0.214428571849699,1.85930274472875,
5.26601035317778));
#52970=CARTESIAN_POINT('Ctrl Pts',(-0.229754959315943,1.87359390527383,
5.26483586848309));
#52971=CARTESIAN_POINT('Ctrl Pts',(-0.23912639425859,1.88351530880313,5.26407894679034));
#52972=CARTESIAN_POINT('Ctrl Pts',(-0.254054086170672,1.90147501058507,
5.26275597177458));
#52973=CARTESIAN_POINT('Ctrl Pts',(-0.259925289851452,1.90922664493999,
5.26219835814575));
#52974=CARTESIAN_POINT('Ctrl Pts',(-0.269607873615735,1.92328876929516,
5.26119714312606));
#52975=CARTESIAN_POINT('Ctrl Pts',(-0.273569922982116,1.92948680676459,
5.26075916025585));
#52976=CARTESIAN_POINT('Ctrl Pts',(-0.278110585263648,1.93715618296798,
5.26021866404168));
#52977=CARTESIAN_POINT('Ctrl Pts',(-0.278895117424574,1.93850349934175,
5.26012376867364));
#52978=CARTESIAN_POINT('Ctrl Pts',(-0.279965657936536,1.94037305862732,
5.25999214802981));
#52979=CARTESIAN_POINT('Ctrl Pts',(-0.280260050307567,1.94089049610431,
5.25995572550803));
#52980=CARTESIAN_POINT('Ctrl Pts',(-0.28075445283489,1.94176510999046,5.25989417032823));
#52981=CARTESIAN_POINT('Ctrl Pts',(-0.280955220029378,1.94212185857839,
5.2598690649564));
#52982=CARTESIAN_POINT('Ctrl Pts',(-0.281351054551799,1.94282837369371,
5.25981935012885));
#52983=CARTESIAN_POINT('Ctrl Pts',(-0.281546150732992,1.94317812327897,
5.25979474176635));
#52984=CARTESIAN_POINT('Ctrl Pts',(-0.281974613811734,1.94394960714206,
5.25974046462356));
#52985=CARTESIAN_POINT('Ctrl Pts',(-0.282207687216855,1.9443715025547,5.2597107854053));
#52986=CARTESIAN_POINT('Ctrl Pts',(-0.283018088563132,1.94584624890688,
5.25960704989086));
#52987=CARTESIAN_POINT('Ctrl Pts',(-0.28359047269195,1.94690179241485,5.25953281749829));
#52988=CARTESIAN_POINT('Ctrl Pts',(-0.289547709250379,1.95803567596174,
5.25874993066847));
#52989=CARTESIAN_POINT('Ctrl Pts',(-0.294398205576087,1.96838925223525,
5.25802246766615));
#52990=CARTESIAN_POINT('Ctrl Pts',(-0.299235365124926,1.98032755660327,
5.25718312586535));
#52991=CARTESIAN_POINT('Ctrl Pts',(-0.299773208131224,1.9816812735016,5.2570879503773));
#52992=CARTESIAN_POINT('Ctrl Pts',(-0.309387489097007,2.0063662185636,5.2553525046248));
#52993=CARTESIAN_POINT('Ctrl Pts',(-0.315723424834338,2.0306719952212,5.2536352899542));
#52994=CARTESIAN_POINT('Ctrl Pts',(-0.320758028711347,2.06675206657146,
5.25119692420123));
#52995=CARTESIAN_POINT('Ctrl Pts',(-0.321733513965345,2.07811979239006,
5.25044578398571));
#52996=CARTESIAN_POINT('Ctrl Pts',(-0.322138027217224,2.09054838527785,
5.24965905090197));
#52997=CARTESIAN_POINT('Ctrl Pts',(-0.322166654395369,2.09158047134321,
5.24959398025463));
#52998=CARTESIAN_POINT('Ctrl Pts',(-0.322207461487357,2.09336023363765,
5.24948224026227));
#52999=CARTESIAN_POINT('Ctrl Pts',(-0.322221999895217,2.09410784033823,
5.24943544570146));
#53000=CARTESIAN_POINT('Ctrl Pts',(-0.32223891769658,2.09516751365462,5.24936932714181));
#53001=CARTESIAN_POINT('Ctrl Pts',(-0.322243445879631,2.0954795362922,5.24934988410092));
#53002=CARTESIAN_POINT('Ctrl Pts',(-0.322250445061775,2.09601547659921,
5.24931653278148));
#53003=CARTESIAN_POINT('Ctrl Pts',(-0.322253135886101,2.09623939074842,
5.24930261210553));
#53004=CARTESIAN_POINT('Ctrl Pts',(-0.322257842731121,2.09666826821539,
5.2492759748053));
#53005=CARTESIAN_POINT('Ctrl Pts',(-0.322259896590546,2.09687323035054,
5.24926325604357));
#53006=CARTESIAN_POINT('Ctrl Pts',(-0.322264275426226,2.09735619594281,
5.24923331234097));
#53007=CARTESIAN_POINT('Ctrl Pts',(-0.322266436219366,2.09763420125487,
5.24921609667152));
#53008=CARTESIAN_POINT('Ctrl Pts',(-0.322272656705628,2.09859438660008,
5.24915670649722));
#53009=CARTESIAN_POINT('Ctrl Pts',(-0.322274910125506,2.09927658260931,
5.24911463271193));
#53010=CARTESIAN_POINT('Ctrl Pts',(-0.322276774331859,2.11385452741531,
5.2482180605504));
#53011=CARTESIAN_POINT('Ctrl Pts',(-0.321379814763137,2.12773790983263,
5.24741269427191));
#53012=CARTESIAN_POINT('Ctrl Pts',(-0.315022139962535,2.17667233039282,
5.24461296763276));
#53013=CARTESIAN_POINT('Ctrl Pts',(-0.304688950478254,2.21082538500583,
5.24269992718813));
#53014=CARTESIAN_POINT('Ctrl Pts',(-0.288117487796207,2.2444073956663,5.24043568955618));
#53015=CARTESIAN_POINT('Ctrl Pts',(-0.287214981102895,2.24619417583121,
5.2403140875302));
#53016=CARTESIAN_POINT('Ctrl Pts',(-0.285983113701354,2.24857758372335,
5.24015031821767));
#53017=CARTESIAN_POINT('Ctrl Pts',(-0.28566840838782,2.24918176881018,5.24010866763992));
#53018=CARTESIAN_POINT('Ctrl Pts',(-0.285172753450314,2.25012602940811,
5.24004335892914));
#53019=CARTESIAN_POINT('Ctrl Pts',(-0.28499310445422,2.25046678845427,5.24001974684825));
#53020=CARTESIAN_POINT('Ctrl Pts',(-0.284647751100432,2.25111901895891,
5.23997446761668));
#53021=CARTESIAN_POINT('Ctrl Pts',(-0.284482145272294,2.25143054222098,
5.2399528039837));
#53022=CARTESIAN_POINT('Ctrl Pts',(-0.284092931409167,2.25215980565254,
5.23990200314286));
#53023=CARTESIAN_POINT('Ctrl Pts',(-0.283868913422423,2.2525773250567,5.23987285139383));
#53024=CARTESIAN_POINT('Ctrl Pts',(-0.28322197266807,2.25377672131862,5.23978891371425));
#53025=CARTESIAN_POINT('Ctrl Pts',(-0.282796737115337,2.25455733975803,
5.23973404543842));
#53026=CARTESIAN_POINT('Ctrl Pts',(-0.279950793237332,2.25973066297264,
5.23936882408137));
#53027=CARTESIAN_POINT('Ctrl Pts',(-0.277431166943849,2.26406789559316,
5.23905493689193));
#53028=CARTESIAN_POINT('Ctrl Pts',(-0.269694283233309,2.27669786509595,
5.23811719803429));
#53029=CARTESIAN_POINT('Ctrl Pts',(-0.264199350090646,2.28481291543802,
5.23748343956776));
#53030=CARTESIAN_POINT('Ctrl Pts',(-0.248373357684495,2.30603398755055,
5.23574056374043));
#53031=CARTESIAN_POINT('Ctrl Pts',(-0.23738077891124,2.31860835147005,5.23461170913222));
#53032=CARTESIAN_POINT('Ctrl Pts',(-0.212025472155604,2.34343415760863,
5.2322111602948));
#53033=CARTESIAN_POINT('Ctrl Pts',(-0.197457119170619,2.35539353284754,
5.23094415646567));
#53034=CARTESIAN_POINT('Ctrl Pts',(-0.181324923253764,2.36642631196949,
5.22971237406465));
#53035=CARTESIAN_POINT('Ctrl Pts',(-0.180721536970899,2.36683596759337,
5.22966653748616));
#53036=CARTESIAN_POINT('Ctrl Pts',(-0.17961065180931,2.36758468169668,5.22958258743724));
#53037=CARTESIAN_POINT('Ctrl Pts',(-0.179103572209121,2.36792435230583,
5.22954443419822));
#53038=CARTESIAN_POINT('Ctrl Pts',(-0.178359051491941,2.36842001617057,
5.22948866349852));
#53039=CARTESIAN_POINT('Ctrl Pts',(-0.178122368004778,2.36857713668139,
5.22947097054284));
#53040=CARTESIAN_POINT('Ctrl Pts',(-0.177701956653994,2.36885542334633,
5.22943960855945));
#53041=CARTESIAN_POINT('Ctrl Pts',(-0.177518312275474,2.36897671436283,
5.22942593107253));
#53042=CARTESIAN_POINT('Ctrl Pts',(-0.177133014027207,2.36923062459127,
5.22939728119826));
#53043=CARTESIAN_POINT('Ctrl Pts',(-0.176931335883847,2.36936320509573,
5.22938231144218));
#53044=CARTESIAN_POINT('Ctrl Pts',(-0.176400456138511,2.36971134484431,
5.22934297565138));
#53045=CARTESIAN_POINT('Ctrl Pts',(-0.176071007067762,2.3699265287771,5.22931863491561));
#53046=CARTESIAN_POINT('Ctrl Pts',(-0.174601822260692,2.37088231164919,
5.2292103942187));
#53047=CARTESIAN_POINT('Ctrl Pts',(-0.173457780487889,2.37161631328595,
5.22912693029752));
#53048=CARTESIAN_POINT('Ctrl Pts',(-0.164773010845749,2.37711109193931,
5.2284992483708));
#53049=CARTESIAN_POINT('Ctrl Pts',(-0.15704147785986,2.38156475021108,5.22797398682604));
#53050=CARTESIAN_POINT('Ctrl Pts',(-0.134542901634906,2.39330924399824,
5.22650989287571));
#53051=CARTESIAN_POINT('Ctrl Pts',(-0.119388451271401,2.3997975442745,5.2255981322386));
#53052=CARTESIAN_POINT('Ctrl Pts',(-0.0813040140909026,2.41275497846031,
5.22334645200766));
#53053=CARTESIAN_POINT('Ctrl Pts',(-0.0580303231001466,2.41789661871543,
5.22199832453671));
#53054=CARTESIAN_POINT('Ctrl Pts',(-0.0329478271526801,2.42058971188798,
5.22046787271104));
#53055=CARTESIAN_POINT('Ctrl Pts',(-0.0314898860301568,2.42073619946888,
5.22037866963294));
#53056=CARTESIAN_POINT('Ctrl Pts',(-0.0294947155725804,2.42092293080252,
5.22025624673776));
#53057=CARTESIAN_POINT('Ctrl Pts',(-0.0289582935937396,2.42097177911488,
5.22022329755897));
#53058=CARTESIAN_POINT('Ctrl Pts',(-0.0280444559599168,2.42105268661818,
5.2201671062988));
#53059=CARTESIAN_POINT('Ctrl Pts',(-0.0276671003772481,2.42108542578194,
5.22014388562807));
#53060=CARTESIAN_POINT('Ctrl Pts',(-0.0269365572402991,2.42114750989516,
5.2200988975896));
#53061=CARTESIAN_POINT('Ctrl Pts',(-0.0265833770888911,2.42117693766646,
5.22007713285717));
#53062=CARTESIAN_POINT('Ctrl Pts',(-0.0257442744628854,2.42124546005649,
5.22002538641883));
#53063=CARTESIAN_POINT('Ctrl Pts',(-0.0252583114557175,2.42128403473062,
5.2199953884227));
#53064=CARTESIAN_POINT('Ctrl Pts',(-0.0238211524478474,2.42139483242993,
5.21990658658014));
#53065=CARTESIAN_POINT('Ctrl Pts',(-0.0228697274119282,2.42146393445204,
5.21984768486017));
#53066=CARTESIAN_POINT('Ctrl Pts',(-0.0153149981860956,2.42197892621476,
5.21937906127795));
#53067=CARTESIAN_POINT('Ctrl Pts',(-0.00870011223477689,2.42222550437639,
5.2189631198275));
#53068=CARTESIAN_POINT('Ctrl Pts',(0.00663077826136184,2.42232458213162,
5.21798507903022));
#53069=CARTESIAN_POINT('Ctrl Pts',(0.0153422657119557,2.42202747812151,
5.21741875745424));
#53070=CARTESIAN_POINT('Ctrl Pts',(0.0506838314702809,2.41938487875055,
5.21508064263407));
#53071=CARTESIAN_POINT('Ctrl Pts',(0.0769825413879906,2.41408443930217,
5.21323589837396));
#53072=CARTESIAN_POINT('Ctrl Pts',(0.11058169555953,2.40283444883238,5.21089423798737));
#53073=CARTESIAN_POINT('Ctrl Pts',(0.118725096218756,2.39973554721936,5.21032907812232));
#53074=CARTESIAN_POINT('Ctrl Pts',(0.127386948997826,2.39603081867868,5.20973790664558));
#53075=CARTESIAN_POINT('Ctrl Pts',(0.128039253576035,2.39574926872082,5.20969344966995));
#53076=CARTESIAN_POINT('Ctrl Pts',(0.128950012247246,2.3953525859196,5.20963147151242));
#53077=CARTESIAN_POINT('Ctrl Pts',(0.12920924777632,2.39523926899812,5.20961384085194));
#53078=CARTESIAN_POINT('Ctrl Pts',(0.129657195091897,2.39504275947453,5.20958339464927));
#53079=CARTESIAN_POINT('Ctrl Pts',(0.129845976284511,2.39495972708272,5.20957056929516));
#53080=CARTESIAN_POINT('Ctrl Pts',(0.130238639513694,2.39478657040735,5.20954390489615));
#53081=CARTESIAN_POINT('Ctrl Pts',(0.130442507511382,2.39469641590852,5.20953006782174));
#53082=CARTESIAN_POINT('Ctrl Pts',(0.130926456770839,2.39448180330434,5.20949723690781));
#53083=CARTESIAN_POINT('Ctrl Pts',(0.131206455293395,2.39435715661615,5.20947825468813));
#53084=CARTESIAN_POINT('Ctrl Pts',(0.132139473440044,2.39394021000074,5.20941504285569));
#53085=CARTESIAN_POINT('Ctrl Pts',(0.132791703429462,2.39364613230832,5.20937092174894));
#53086=CARTESIAN_POINT('Ctrl Pts',(0.14409488731944,2.38850438736617,5.20860737997982));
#53087=CARTESIAN_POINT('Ctrl Pts',(0.154476405955145,2.38308166319921,5.20792267004324));
#53088=CARTESIAN_POINT('Ctrl Pts',(0.196767554430835,2.35796981334613,5.205109754711));
#53089=CARTESIAN_POINT('Ctrl Pts',(0.225407533320787,2.33336145887135,5.20310698965065));
#53090=CARTESIAN_POINT('Ctrl Pts',(0.250519689444358,2.3027449991922,5.20071440985734));
#53091=CARTESIAN_POINT('Ctrl Pts',(0.251844919147699,2.30109645910873,5.20058597431179));
#53092=CARTESIAN_POINT('Ctrl Pts',(0.253584947958278,2.29888774520995,5.20041436526582));
#53093=CARTESIAN_POINT('Ctrl Pts',(0.254014316084633,2.29833907390565,5.20037177352289));
#53094=CARTESIAN_POINT('Ctrl Pts',(0.254680224637519,2.29748242858476,5.2003053319119));
#53095=CARTESIAN_POINT('Ctrl Pts',(0.254917995071817,2.29717540974369,5.2002815308521));
#53096=CARTESIAN_POINT('Ctrl Pts',(0.255392048046833,2.29656100258383,5.20023392244234));
#53097=CARTESIAN_POINT('Ctrl Pts',(0.255628331962342,2.29625361611552,5.20021011520046));
#53098=CARTESIAN_POINT('Ctrl Pts',(0.256152469940571,2.29556920201964,5.20015713128669));
#53099=CARTESIAN_POINT('Ctrl Pts',(0.256440047003135,2.29519196429271,5.20012794377593));
#53100=CARTESIAN_POINT('Ctrl Pts',(0.257270249870077,2.29409791965185,5.20004334203526));
#53101=CARTESIAN_POINT('Ctrl Pts',(0.257810707154714,2.29337947960308,5.199987842899));
#53102=CARTESIAN_POINT('Ctrl Pts',(0.259024672913913,2.29175159748644,5.19986221435802));
#53103=CARTESIAN_POINT('Ctrl Pts',(0.259696408763728,2.29084085395812,5.19979201662996));
#53104=CARTESIAN_POINT('Ctrl Pts',(0.265305360104281,2.28315175075807,5.19920005998425));
#53105=CARTESIAN_POINT('Ctrl Pts',(0.269980670352369,2.27618715750858,5.19866829940312));
#53106=CARTESIAN_POINT('Ctrl Pts',(0.280621370836128,2.25891649681372,5.19735868871463));
#53107=CARTESIAN_POINT('Ctrl Pts',(0.286297344025724,2.24844726078929,5.19657190175394));
#53108=CARTESIAN_POINT('Ctrl Pts',(0.303532352297848,2.21197410479837,5.19386710466406));
#53109=CARTESIAN_POINT('Ctrl Pts',(0.312226477123553,2.18476347292928,5.19189781300503));
#53110=CARTESIAN_POINT('Ctrl Pts',(0.317495769911637,2.15531527051852,5.19000617503632));
#53111=CARTESIAN_POINT('Ctrl Pts',(0.317745154876764,2.15386427214024,5.18991359406522));
#53112=CARTESIAN_POINT('Ctrl Pts',(0.318053455842723,2.15199378948639,5.18979509697316));
#53113=CARTESIAN_POINT('Ctrl Pts',(0.318121495402431,2.15157585759306,5.18976867502074));
#53114=CARTESIAN_POINT('Ctrl Pts',(0.318228087398852,2.15091288192473,5.18972684891775));
#53115=CARTESIAN_POINT('Ctrl Pts',(0.318267180650818,2.15066792749847,5.18971141409486));
#53116=CARTESIAN_POINT('Ctrl Pts',(0.318336775715639,2.15022859310585,5.18968376550876));
#53117=CARTESIAN_POINT('Ctrl Pts',(0.318367382107366,2.15003423177019,5.18967154585157));
#53118=CARTESIAN_POINT('Ctrl Pts',(0.318438987579735,2.14957678597483,5.18964281413764));
#53119=CARTESIAN_POINT('Ctrl Pts',(0.318479838577145,2.14931367903029,5.18962631062424));
#53120=CARTESIAN_POINT('Ctrl Pts',(0.318597521700832,2.14854947773591,5.18957843872311));
#53121=CARTESIAN_POINT('Ctrl Pts',(0.318673498044471,2.14804824944509,5.18954711888645));
#53122=CARTESIAN_POINT('Ctrl Pts',(0.31919570227801,2.14454745511765,5.18932890338729));
#53123=CARTESIAN_POINT('Ctrl Pts',(0.319600774120806,2.14154177296956,5.18914429442933));
#53124=CARTESIAN_POINT('Ctrl Pts',(0.320724483842525,2.13221035566627,5.18857840517347));
#53125=CARTESIAN_POINT('Ctrl Pts',(0.321298207093124,2.12586841299972,5.18820408300118));
#53126=CARTESIAN_POINT('Ctrl Pts',(0.323437308828386,2.09060441953885,5.18615925515112));
#53127=CARTESIAN_POINT('Ctrl Pts',(0.321286329393357,2.06159019594428,5.18460093381483));
#53128=CARTESIAN_POINT('Ctrl Pts',(0.314320926572631,2.02868880014485,5.18266388569069));
#53129=CARTESIAN_POINT('Ctrl Pts',(0.313255941796059,2.02414721942819,5.18239296153203));
#53130=CARTESIAN_POINT('Ctrl Pts',(0.310131184234953,2.01201308664056,5.18165767523588));
#53131=CARTESIAN_POINT('Ctrl Pts',(0.307891485164788,2.0044706013569,5.18118838902889));
#53132=CARTESIAN_POINT('Ctrl Pts',(0.305034123103405,1.9959975034611,5.18064439610691));
#53133=CARTESIAN_POINT('Ctrl Pts',(0.304684862442675,1.99497871597641,5.18057870884673));
#53134=CARTESIAN_POINT('Ctrl Pts',(0.304161260477422,1.99347597534082,5.18048139913861));
#53135=CARTESIAN_POINT('Ctrl Pts',(0.303990854150602,1.99299065090963,5.18044990722909));
#53136=CARTESIAN_POINT('Ctrl Pts',(0.303687206633742,1.99213242860905,5.18039410298152));
#53137=CARTESIAN_POINT('Ctrl Pts',(0.303554438369028,1.9917593635688,5.18036980640283));
#53138=CARTESIAN_POINT('Ctrl Pts',(0.303297615875805,1.99104190794798,5.18032300573338));
#53139=CARTESIAN_POINT('Ctrl Pts',(0.303173661739258,1.99069748198044,5.18030050500655));
#53140=CARTESIAN_POINT('Ctrl Pts',(0.302843669466593,1.98978542680583,5.18024083334214));
#53141=CARTESIAN_POINT('Ctrl Pts',(0.3026366229957,1.9892181662266,5.18020362882756));
#53142=CARTESIAN_POINT('Ctrl Pts',(0.301866260114837,1.98712582299045,5.18006606031803));
#53143=CARTESIAN_POINT('Ctrl Pts',(0.301293007276265,1.98560444745442,5.17996536477824));
#53144=CARTESIAN_POINT('Ctrl Pts',(0.299861883024081,1.9818917254122,5.17971796541122));
#53145=CARTESIAN_POINT('Ctrl Pts',(0.298991484020115,1.97970533915752,5.17957084452875));
#53146=CARTESIAN_POINT('Ctrl Pts',(0.294414519943299,1.96856492793829,5.17881373382568));
#53147=CARTESIAN_POINT('Ctrl Pts',(0.290329716441638,1.95977264181296,5.17819109231995));
#53148=CARTESIAN_POINT('Ctrl Pts',(0.278273027649334,1.93661424644853,5.17648211320755));
#53149=CARTESIAN_POINT('Ctrl Pts',(0.269589359543073,1.92265213197186,5.17537538829992));
#53150=CARTESIAN_POINT('Ctrl Pts',(0.24973663878972,1.89558124762562,5.17310361924909));
#53151=CARTESIAN_POINT('Ctrl Pts',(0.238503461464012,1.88257964314422,5.17194188848285));
#53152=CARTESIAN_POINT('Ctrl Pts',(0.223212478551798,1.86750049358797,5.17055485455683));
#53153=CARTESIAN_POINT('Ctrl Pts',(0.220076270264897,1.86452968156225,5.17027951536881));
#53154=CARTESIAN_POINT('Ctrl Pts',(0.216476857875146,1.86125485489575,5.1699745801794));
#53155=CARTESIAN_POINT('Ctrl Pts',(0.216071676525542,1.8608880912205,5.16994040845716));
#53156=CARTESIAN_POINT('Ctrl Pts',(0.215458420729558,1.8603358135493,5.16988892377945));
#53157=CARTESIAN_POINT('Ctrl Pts',(0.215251037898026,1.86014953822097,5.16987155382379));
#53158=CARTESIAN_POINT('Ctrl Pts',(0.214890604653809,1.85982663397509,5.16984143525201));
#53159=CARTESIAN_POINT('Ctrl Pts',(0.214737665422739,1.8596898820991,5.16982867731664));
#53160=CARTESIAN_POINT('Ctrl Pts',(0.214417645089925,1.85940428272639,5.16980202789545));
#53161=CARTESIAN_POINT('Ctrl Pts',(0.214250539649334,1.85925546328813,5.16978813858713));
#53162=CARTESIAN_POINT('Ctrl Pts',(0.213850683036311,1.85890010821325,5.16975496603623));
#53163=CARTESIAN_POINT('Ctrl Pts',(0.213617786657616,1.8586937346853,5.16973569507197));
#53164=CARTESIAN_POINT('Ctrl Pts',(0.212828107042354,1.85799602504557,5.16967052210728));
#53165=CARTESIAN_POINT('Ctrl Pts',(0.212269919344827,1.8575062714047,5.16962473806997));
#53166=CARTESIAN_POINT('Ctrl Pts',(0.210938372532199,1.85634609352077,5.16951617972235));
#53167=CARTESIAN_POINT('Ctrl Pts',(0.21016349735812,1.85567741080384,5.16945353020245));
#53168=CARTESIAN_POINT('Ctrl Pts',(0.200860187725624,1.84772607887438,5.16870740876328));
#53169=CARTESIAN_POINT('Ctrl Pts',(0.191959386419483,1.84088882988374,5.16805408888592));
#53170=CARTESIAN_POINT('Ctrl Pts',(0.163751671426793,1.82147393900853,5.16610015139519));
#53171=CARTESIAN_POINT('Ctrl Pts',(0.143439508798616,1.81048910865807,5.16484352497725));
#53172=CARTESIAN_POINT('Ctrl Pts',(0.108262271223417,1.79608389172537,5.16267438403878));
#53173=CARTESIAN_POINT('Ctrl Pts',(0.0940177835226997,1.79138003211136,
5.16179884426182));
#53174=CARTESIAN_POINT('Ctrl Pts',(0.0782914478583242,1.78737694015411,
5.1608128646853));
#53175=CARTESIAN_POINT('Ctrl Pts',(0.0770821108106107,1.787076564508,5.16073693143421));
#53176=CARTESIAN_POINT('Ctrl Pts',(0.0753825691881916,1.78666488143178,
5.16063005100006));
#53177=CARTESIAN_POINT('Ctrl Pts',(0.0748937891579322,1.78654769325044,
5.16059929329663));
#53178=CARTESIAN_POINT('Ctrl Pts',(0.0740455195771288,1.78634641248727,
5.160545879437));
#53179=CARTESIAN_POINT('Ctrl Pts',(0.0736861549897506,1.78626179306619,
5.16052324027157));
#53180=CARTESIAN_POINT('Ctrl Pts',(0.0729384689520039,1.78608709124875,
5.16047611516627));
#53181=CARTESIAN_POINT('Ctrl Pts',(0.0725501243478201,1.78599711149637,
5.1604516259688));
#53182=CARTESIAN_POINT('Ctrl Pts',(0.0717792064542373,1.78581999570137,
5.1604029860534));
#53183=CARTESIAN_POINT('Ctrl Pts',(0.0713966389815536,1.78573283734973,
5.16037883610215));
#53184=CARTESIAN_POINT('Ctrl Pts',(0.0700956251357066,1.78543893239755,
5.16029666547259));
#53185=CARTESIAN_POINT('Ctrl Pts',(0.0691764389663697,1.78523551315915,
5.16023853812906));
#53186=CARTESIAN_POINT('Ctrl Pts',(0.06214162405785,1.78371098588337,5.15979309984281));
#53187=CARTESIAN_POINT('Ctrl Pts',(0.0559899499688998,1.78256427652382,
5.15940024114404));
#53188=CARTESIAN_POINT('Ctrl Pts',(0.0425768557792685,1.78046600683525,
5.15853558189868));
#53189=CARTESIAN_POINT('Ctrl Pts',(0.0353086189814152,1.77958144606202,
5.15806195471429));
#53190=CARTESIAN_POINT('Ctrl Pts',(0.0167504593464377,1.7779619599821,5.15684028680054));
#53191=CARTESIAN_POINT('Ctrl Pts',(0.00544077935704302,1.77757257982312,
5.15608399689353));
#53192=CARTESIAN_POINT('Ctrl Pts',(-0.0308161556875546,1.77823254335554,
5.15363793883813));
#53193=CARTESIAN_POINT('Ctrl Pts',(-0.0556317085551485,1.781583215079,5.15192527646117));
#53194=CARTESIAN_POINT('Ctrl Pts',(-0.0811939182771575,1.78811740388909,
5.15025767293304));
#53195=CARTESIAN_POINT('Ctrl Pts',(-0.0825721580369343,1.78847946292789,
5.1501680885667));
#53196=CARTESIAN_POINT('Ctrl Pts',(-0.0843516828851688,1.78895957809642,
5.15005288656102));
#53197=CARTESIAN_POINT('Ctrl Pts',(-0.0847551751763398,1.78906928304034,
5.1500267965216));
#53198=CARTESIAN_POINT('Ctrl Pts',(-0.0853727848581228,1.7892384956017,
5.14998691032801));
#53199=CARTESIAN_POINT('Ctrl Pts',(-0.0855870541616043,1.78929743938782,
5.14997308148789));
#53200=CARTESIAN_POINT('Ctrl Pts',(-0.0860092666069014,1.78941405658195,
5.14994585008614));
#53201=CARTESIAN_POINT('Ctrl Pts',(-0.0862172115706606,1.78947171687481,
5.14993244692034));
#53202=CARTESIAN_POINT('Ctrl Pts',(-0.0866806469675839,1.7896007225675,
5.14990259522211));
#53203=CARTESIAN_POINT('Ctrl Pts',(-0.0869361066297151,1.78967217437906,
5.14988615303021));
#53204=CARTESIAN_POINT('Ctrl Pts',(-0.087675000769768,1.78987982632045,
5.14983863223153));
#53205=CARTESIAN_POINT('Ctrl Pts',(-0.0881582082064824,1.79001684204315,
5.14980760108401));
#53206=CARTESIAN_POINT('Ctrl Pts',(-0.0914570078763413,1.79096056942568,
5.14959605418239));
#53207=CARTESIAN_POINT('Ctrl Pts',(-0.0942619255837974,1.79180453478371,
5.14941766869033));
#53208=CARTESIAN_POINT('Ctrl Pts',(-0.1030276472398,1.7945729068964,5.14886375076047));
#53209=CARTESIAN_POINT('Ctrl Pts',(-0.108944388198496,1.79663300065862,
5.14849506348126));
#53210=CARTESIAN_POINT('Ctrl Pts',(-0.126172558665861,1.80320065429629,
5.14742673492484));
#53211=CARTESIAN_POINT('Ctrl Pts',(-0.137293301619349,1.80817821944364,
5.14674363169106));
#53212=CARTESIAN_POINT('Ctrl Pts',(-0.158877418228624,1.81934679470042,
5.14538422246422));
#53213=CARTESIAN_POINT('Ctrl Pts',(-0.169325183009241,1.82552371975195,
5.14470891064443));
#53214=CARTESIAN_POINT('Ctrl Pts',(-0.19357989509715,1.84177652286455,5.14305326335965));
#53215=CARTESIAN_POINT('Ctrl Pts',(-0.206980719399404,1.85238862119319,
5.14206231232925));
#53216=CARTESIAN_POINT('Ctrl Pts',(-0.220409938129574,1.86487820780833,
5.14094825134968));
#53217=CARTESIAN_POINT('Ctrl Pts',(-0.221337472170128,1.8657511551132,5.14087064406197));
#53218=CARTESIAN_POINT('Ctrl Pts',(-0.222627211277037,1.8669794904672,5.14076179099068));
#53219=CARTESIAN_POINT('Ctrl Pts',(-0.222993797243992,1.86733027818391,
5.14073074414034));
#53220=CARTESIAN_POINT('Ctrl Pts',(-0.223626575105206,1.86793865521845,
5.14067696626749));
#53221=CARTESIAN_POINT('Ctrl Pts',(-0.223893154864485,1.86819584119763,
5.14065425280302));
#53222=CARTESIAN_POINT('Ctrl Pts',(-0.224445104716863,1.86873018172551,
5.14060710475687));
#53223=CARTESIAN_POINT('Ctrl Pts',(-0.224730406115604,1.86900740609062,
5.14058266714561));
#53224=CARTESIAN_POINT('Ctrl Pts',(-0.225295009539006,1.86955806137732,
5.14053417251841));
#53225=CARTESIAN_POINT('Ctrl Pts',(-0.225574328879594,1.86983147359438,
5.14051011634514));
#53226=CARTESIAN_POINT('Ctrl Pts',(-0.226221638295365,1.87046740356031,
5.14045421566478));
#53227=CARTESIAN_POINT('Ctrl Pts',(-0.226589254792265,1.87083029853602,
5.14042235456631));
#53228=CARTESIAN_POINT('Ctrl Pts',(-0.22862195168902,1.87284656077199,5.1402455448671));
#53229=CARTESIAN_POINT('Ctrl Pts',(-0.230269773698166,1.8745171567504,5.14009983432692));
#53230=CARTESIAN_POINT('Ctrl Pts',(-0.239768937849669,1.88436033395053,
5.13924566302208));
#53231=CARTESIAN_POINT('Ctrl Pts',(-0.247202200108863,1.89292361167454,
5.13851938866038));
#53232=CARTESIAN_POINT('Ctrl Pts',(-0.258682140403213,1.9076497373701,5.13729632073514));
#53233=CARTESIAN_POINT('Ctrl Pts',(-0.262996425928488,1.91359199897851,
5.13680922056989));
#53234=CARTESIAN_POINT('Ctrl Pts',(-0.283414113068759,1.94383559384086,
5.13436664918898));
#53235=CARTESIAN_POINT('Ctrl Pts',(-0.296371318743832,1.97009610528975,
5.13234483393486));
#53236=CARTESIAN_POINT('Ctrl Pts',(-0.306105558473916,1.99918882369695,
5.13040406135502));
#53237=CARTESIAN_POINT('Ctrl Pts',(-0.306579678693467,2.00064001294697,
5.13030803007201));
#53238=CARTESIAN_POINT('Ctrl Pts',(-0.307172383800047,2.00249880874143,
5.13018606628796));
#53239=CARTESIAN_POINT('Ctrl Pts',(-0.307300490132461,2.0029033242819,5.13015958699455));
#53240=CARTESIAN_POINT('Ctrl Pts',(-0.307503018739293,2.00354725536647,
5.13011753683545));
#53241=CARTESIAN_POINT('Ctrl Pts',(-0.307577960626679,2.00378650500642,
5.13010193546454));
#53242=CARTESIAN_POINT('Ctrl Pts',(-0.307717629983874,2.00423422599131,
5.13007278154937));
#53243=CARTESIAN_POINT('Ctrl Pts',(-0.307782424342285,2.00444267406015,
5.13005922515666));
#53244=CARTESIAN_POINT('Ctrl Pts',(-0.307927771702084,2.0049119483978,5.1300287439884));
#53245=CARTESIAN_POINT('Ctrl Pts',(-0.308008204937849,2.00517281067543,
5.13001182636143));
#53246=CARTESIAN_POINT('Ctrl Pts',(-0.30824651265352,2.0059491959169,5.12996155324783));
#53247=CARTESIAN_POINT('Ctrl Pts',(-0.308403426009957,2.00646501645366,
5.12992825410458));
#53248=CARTESIAN_POINT('Ctrl Pts',(-0.309680047697135,2.01069978735975,
5.12965569059996));
#53249=CARTESIAN_POINT('Ctrl Pts',(-0.310733799261558,2.01443850629147,
5.12942020549679));
#53250=CARTESIAN_POINT('Ctrl Pts',(-0.313968565525912,2.02676473925569,
5.12865788095341));
#53251=CARTESIAN_POINT('Ctrl Pts',(-0.315863253984758,2.03542373370896,
5.12814448466333));
#53252=CARTESIAN_POINT('Ctrl Pts',(-0.320627858892563,2.06250148667257,
5.12657688193106));
#53253=CARTESIAN_POINT('Ctrl Pts',(-0.322259323361285,2.08109780017599,
5.12555199586756));
#53254=CARTESIAN_POINT('Ctrl Pts',(-0.322274887569339,2.09973080273101,
5.12450080716969));
#53255=CARTESIAN_POINT('',(-0.322275001354959,2.10019426933339,4.8741705987911));
#53256=CARTESIAN_POINT('Ctrl Pts',(-0.322274887825424,2.09973110948229,
5.12450078986419));
#53257=CARTESIAN_POINT('Ctrl Pts',(-0.322290989735653,2.11902982390781,
5.12341204450041));
#53258=CARTESIAN_POINT('Ctrl Pts',(-0.320573677161122,2.1382886947902,5.12229858258352));
#53259=CARTESIAN_POINT('Ctrl Pts',(-0.31699887790656,2.15808232175565,5.12107578042294));
#53260=CARTESIAN_POINT('Ctrl Pts',(-0.316850439140216,2.1588867038636,5.12102595671167));
#53261=CARTESIAN_POINT('Ctrl Pts',(-0.316603658603497,2.16019604330961,
5.12094463904795));
#53262=CARTESIAN_POINT('Ctrl Pts',(-0.316507166573223,2.16070134903135,
5.12091320393642));
#53263=CARTESIAN_POINT('Ctrl Pts',(-0.316335377410049,2.16158942119691,
5.12085786342632));
#53264=CARTESIAN_POINT('Ctrl Pts',(-0.316260594212975,2.16197228695529,
5.12083397443929));
#53265=CARTESIAN_POINT('Ctrl Pts',(-0.316108226223457,2.16274490309125,
5.12078570474398));
#53266=CARTESIAN_POINT('Ctrl Pts',(-0.316030615326477,2.16313464757288,
5.1207613232407));
#53267=CARTESIAN_POINT('Ctrl Pts',(-0.31587914143663,2.16388803741071,5.12071413071407));
#53268=CARTESIAN_POINT('Ctrl Pts',(-0.315805370834198,2.16425170090682,
5.12069132267755));
#53269=CARTESIAN_POINT('Ctrl Pts',(-0.315628740425976,2.16511477430685,
5.12063712591431));
#53270=CARTESIAN_POINT('Ctrl Pts',(-0.315525323381796,2.16561406797299,
5.12060571940141));
#53271=CARTESIAN_POINT('Ctrl Pts',(-0.31515640359698,2.16737415673281,5.12049481695449));
#53272=CARTESIAN_POINT('Ctrl Pts',(-0.314884527945459,2.16863359022284,
5.12041511718659));
#53273=CARTESIAN_POINT('Ctrl Pts',(-0.310551897787788,2.18813625666248,
5.11917552545883));
#53274=CARTESIAN_POINT('Ctrl Pts',(-0.304920064847378,2.2059906293523,5.11796382874564));
#53275=CARTESIAN_POINT('Ctrl Pts',(-0.2961155258687,2.22726187992745,5.11642780074655));
#53276=CARTESIAN_POINT('Ctrl Pts',(-0.294375885379781,2.23123576994947,
5.11613682321052));
#53277=CARTESIAN_POINT('Ctrl Pts',(-0.284204516917543,2.25324974741796,
5.1145041546049));
#53278=CARTESIAN_POINT('Ctrl Pts',(-0.274194972971028,2.27051348535402,
5.11314156421886));
#53279=CARTESIAN_POINT('Ctrl Pts',(-0.259912167036294,2.29060236542015,
5.11152282370122));
#53280=CARTESIAN_POINT('Ctrl Pts',(-0.25708355519201,2.29440073802936,5.11121531763284));
#53281=CARTESIAN_POINT('Ctrl Pts',(-0.252400458770424,2.30040830318866,
5.11072835750816));
#53282=CARTESIAN_POINT('Ctrl Pts',(-0.250598328203254,2.30265724484829,
5.11054592357357));
#53283=CARTESIAN_POINT('Ctrl Pts',(-0.248448301231652,2.30526779408155,
5.11033429227091));
#53284=CARTESIAN_POINT('Ctrl Pts',(-0.248129502894311,2.30565304635097,
5.11030306429527));
#53285=CARTESIAN_POINT('Ctrl Pts',(-0.247640518010151,2.30624116849087,
5.11025539952218));
#53286=CARTESIAN_POINT('Ctrl Pts',(-0.247470977779101,2.30644457100898,
5.11023891600546));
#53287=CARTESIAN_POINT('Ctrl Pts',(-0.247162829367344,2.30681334087063,
5.11020903418381));
#53288=CARTESIAN_POINT('Ctrl Pts',(-0.247024306381369,2.30697877727075,
5.11019562977755));
#53289=CARTESIAN_POINT('Ctrl Pts',(-0.246742582205981,2.30731455151985,
5.1101684260331));
#53290=CARTESIAN_POINT('Ctrl Pts',(-0.24659937135742,2.30748487943079,5.11015462753255));
#53291=CARTESIAN_POINT('Ctrl Pts',(-0.246185586894886,2.30797598066852,
5.11011484551426));
#53292=CARTESIAN_POINT('Ctrl Pts',(-0.245914561730789,2.30829637554048,
5.11008889511359));
#53293=CARTESIAN_POINT('Ctrl Pts',(-0.244711850989432,2.30971255178271,
5.10997420230622));
#53294=CARTESIAN_POINT('Ctrl Pts',(-0.243773443036006,2.31080264002487,
5.10988594642229));
#53295=CARTESIAN_POINT('Ctrl Pts',(-0.226104844866034,2.33105134517014,
5.10824628988625));
#53296=CARTESIAN_POINT('Ctrl Pts',(-0.207168815676109,2.34817265410367,
5.10685067631635));
#53297=CARTESIAN_POINT('Ctrl Pts',(-0.181621330405773,2.36628814159831,
5.10509742295786));
#53298=CARTESIAN_POINT('Ctrl Pts',(-0.176737616443746,2.36955425195539,
5.10476767319525));
#53299=CARTESIAN_POINT('Ctrl Pts',(-0.16087948564072,2.37954347251795,5.10370741742335));
#53300=CARTESIAN_POINT('Ctrl Pts',(-0.149591541705932,2.38574303696075,
5.1029676859577));
#53301=CARTESIAN_POINT('Ctrl Pts',(-0.134580793271711,2.39285354717694,
5.10198241911863));
#53302=CARTESIAN_POINT('Ctrl Pts',(-0.131170035778878,2.39439702783201,
5.10175849753345));
#53303=CARTESIAN_POINT('Ctrl Pts',(-0.125586000347327,2.39680768554956,
5.10139140383402));
#53304=CARTESIAN_POINT('Ctrl Pts',(-0.123428751275179,2.39771125037125,
5.10124947023267));
#53305=CARTESIAN_POINT('Ctrl Pts',(-0.120783640941969,2.39878546511438,
5.10107523573262));
#53306=CARTESIAN_POINT('Ctrl Pts',(-0.120304916509685,2.39897854294505,
5.101043693943));
#53307=CARTESIAN_POINT('Ctrl Pts',(-0.119463012927586,2.39931574772912,
5.10098820840468));
#53308=CARTESIAN_POINT('Ctrl Pts',(-0.119100030774898,2.39946036626518,
5.10096428125955));
#53309=CARTESIAN_POINT('Ctrl Pts',(-0.118367030246989,2.39975086316793,
5.10091595295899));
#53310=CARTESIAN_POINT('Ctrl Pts',(-0.117997003079354,2.39989671735684,
5.10089155104111));
#53311=CARTESIAN_POINT('Ctrl Pts',(-0.117281740319008,2.40017712488663,
5.10084437163062));
#53312=CARTESIAN_POINT('Ctrl Pts',(-0.116936540622828,2.40031176863861,
5.10082159722263));
#53313=CARTESIAN_POINT('Ctrl Pts',(-0.116117694219233,2.40062953046593,
5.10076756264189));
#53314=CARTESIAN_POINT('Ctrl Pts',(-0.115643846450979,2.40081212454332,
5.10073628493291));
#53315=CARTESIAN_POINT('Ctrl Pts',(-0.113977614955863,2.4014496768659,5.10062626705278));
#53316=CARTESIAN_POINT('Ctrl Pts',(-0.112782974021728,2.40189866692113,
5.10054732729816));
#53317=CARTESIAN_POINT('Ctrl Pts',(-0.0953332341643595,2.40833889359271,
5.09939332566543));
#53318=CARTESIAN_POINT('Ctrl Pts',(-0.0786263957461685,2.41301599125315,
5.09827403538385));
#53319=CARTESIAN_POINT('Ctrl Pts',(-0.0429353249489763,2.4199693352295,
5.09585681100981));
#53320=CARTESIAN_POINT('Ctrl Pts',(-0.0239580382526524,2.42194682999478,
5.09455651042902));
#53321=CARTESIAN_POINT('Ctrl Pts',(0.00347129750252263,2.42236553399417,
5.0927140680452));
#53322=CARTESIAN_POINT('Ctrl Pts',(0.0118638808303338,2.42216588041121,
5.09215580736258));
#53323=CARTESIAN_POINT('Ctrl Pts',(0.0259063952551296,2.42128223414555,
5.09124015626121));
#53324=CARTESIAN_POINT('Ctrl Pts',(0.0315632208922404,2.4207759160237,5.09087636766627));
#53325=CARTESIAN_POINT('Ctrl Pts',(0.0377836730736761,2.42005298012418,
5.09048406385771));
#53326=CARTESIAN_POINT('Ctrl Pts',(0.0383630423190885,2.41998405121819,
5.09044759924346));
#53327=CARTESIAN_POINT('Ctrl Pts',(0.0392220794861484,2.41987948290555,
5.09039364626036));
#53328=CARTESIAN_POINT('Ctrl Pts',(0.0395018888889973,2.41984504979568,
5.09037609032723));
#53329=CARTESIAN_POINT('Ctrl Pts',(0.039978935907294,2.41978570923523,5.09034619011822));
#53330=CARTESIAN_POINT('Ctrl Pts',(0.0401761957510601,2.41976098643082,
5.09033383534596));
#53331=CARTESIAN_POINT('Ctrl Pts',(0.0405812749875582,2.41970983662066,
5.09030848308549));
#53332=CARTESIAN_POINT('Ctrl Pts',(0.0407890909996474,2.41968338957112,
5.09029548678114));
#53333=CARTESIAN_POINT('Ctrl Pts',(0.0412896568049494,2.4196191905895,5.09026420652612));
#53334=CARTESIAN_POINT('Ctrl Pts',(0.0415823814510605,2.41958123897786,
5.09024593392468));
#53335=CARTESIAN_POINT('Ctrl Pts',(0.042652740496143,2.41944097190929,5.09017919016142));
#53336=CARTESIAN_POINT('Ctrl Pts',(0.0434300610083019,2.4193362187996,5.09013085577881));
#53337=CARTESIAN_POINT('Ctrl Pts',(0.0580704337395859,2.41730880987055,
5.0892229496975));
#53338=CARTESIAN_POINT('Ctrl Pts',(0.0717961418628959,2.41448764813134,
5.08841284188422));
#53339=CARTESIAN_POINT('Ctrl Pts',(0.0955639431645579,2.40796439391599,
5.08701557993845));
#53340=CARTESIAN_POINT('Ctrl Pts',(0.105685601139688,2.40463929526679,5.08642237373804));
#53341=CARTESIAN_POINT('Ctrl Pts',(0.130589283256337,2.3950671973472,5.08493056501713));
#53342=CARTESIAN_POINT('Ctrl Pts',(0.145103345660951,2.38820682651836,5.08403042934113));
#53343=CARTESIAN_POINT('Ctrl Pts',(0.164794450155189,2.37703366540393,5.08271226016531));
#53344=CARTESIAN_POINT('Ctrl Pts',(0.170441066592464,2.37359586367385,5.08232232142532));
#53345=CARTESIAN_POINT('Ctrl Pts',(0.178990390496495,2.36802340895069,5.08171059857379));
#53346=CARTESIAN_POINT('Ctrl Pts',(0.181969868958167,2.36600953522321,5.08149324894688));
#53347=CARTESIAN_POINT('Ctrl Pts',(0.185573031637483,2.36348523907211,5.08122501707319));
#53348=CARTESIAN_POINT('Ctrl Pts',(0.186229396230823,2.36302173530172,5.08117593287879));
#53349=CARTESIAN_POINT('Ctrl Pts',(0.187192887261557,2.36233593409902,5.08110355070279));
#53350=CARTESIAN_POINT('Ctrl Pts',(0.187501369377192,2.3621155391057,5.08108032589258));
#53351=CARTESIAN_POINT('Ctrl Pts',(0.188098286130516,2.36168747906486,5.08103528801968));
#53352=CARTESIAN_POINT('Ctrl Pts',(0.188386767670128,2.36147988012407,5.0810134775277));
#53353=CARTESIAN_POINT('Ctrl Pts',(0.188979644095424,2.3610517401541,5.08096856183576));
#53354=CARTESIAN_POINT('Ctrl Pts',(0.189283997651864,2.36083114298524,5.08094545448292));
#53355=CARTESIAN_POINT('Ctrl Pts',(0.190014969379065,2.36029937738361,5.0808898366956));
#53356=CARTESIAN_POINT('Ctrl Pts',(0.190441209035269,2.35998769269007,5.08085730625504));
#53357=CARTESIAN_POINT('Ctrl Pts',(0.191744645700283,2.35902963872904,5.08075752350956));
#53358=CARTESIAN_POINT('Ctrl Pts',(0.192619325452803,2.35837987210721,5.0806901389415));
#53359=CARTESIAN_POINT('Ctrl Pts',(0.20295330518261,2.35062151156219,5.07988892164561));
#53360=CARTESIAN_POINT('Ctrl Pts',(0.212016359303991,2.34300245051973,5.0791348521145));
#53361=CARTESIAN_POINT('Ctrl Pts',(0.222891291432097,2.33278787375085,5.07816112957286));
#53362=CARTESIAN_POINT('Ctrl Pts',(0.225112764582052,2.3306403353714,5.07795833917096));
#53363=CARTESIAN_POINT('Ctrl Pts',(0.246123641354727,2.30973598119556,5.07600306976637));
#53364=CARTESIAN_POINT('Ctrl Pts',(0.262556194573822,2.28875929145849,5.07417133286359));
#53365=CARTESIAN_POINT('Ctrl Pts',(0.280223431444274,2.25936157118612,5.07190287044791));
#53366=CARTESIAN_POINT('Ctrl Pts',(0.283976264665861,2.25257386622189,5.07139816912015));
#53367=CARTESIAN_POINT('Ctrl Pts',(0.288220675237953,2.24419673066484,5.07080365825575));
#53368=CARTESIAN_POINT('Ctrl Pts',(0.288949339107641,2.24273098636042,5.07070066325066));
#53369=CARTESIAN_POINT('Ctrl Pts',(0.289850976365465,2.24088209126622,5.07057208967466));
#53370=CARTESIAN_POINT('Ctrl Pts',(0.290034393342297,2.24050410251269,5.07054587427993));
#53371=CARTESIAN_POINT('Ctrl Pts',(0.290324606086949,2.23990303746364,5.07050430019729));
#53372=CARTESIAN_POINT('Ctrl Pts',(0.290431884340066,2.23968019670218,5.07048891146154));
#53373=CARTESIAN_POINT('Ctrl Pts',(0.290633566586655,2.2392600210066,5.07045994194081));
#53374=CARTESIAN_POINT('Ctrl Pts',(0.290728025414564,2.23906271504799,5.07044635781396));
#53375=CARTESIAN_POINT('Ctrl Pts',(0.290942104253013,2.23861437488134,5.07041553426673));
#53376=CARTESIAN_POINT('Ctrl Pts',(0.291061600065896,2.23836328241044,5.07039830267819));
#53377=CARTESIAN_POINT('Ctrl Pts',(0.29142255528913,2.23760228268504,5.07034617118902));
#53378=CARTESIAN_POINT('Ctrl Pts',(0.291663002460461,2.23709189231505,5.07031133405769));
#53379=CARTESIAN_POINT('Ctrl Pts',(0.293331380298038,2.23352621714782,5.07006882028422));
#53380=CARTESIAN_POINT('Ctrl Pts',(0.294712682314785,2.23044917169992,5.06986396089299));
#53381=CARTESIAN_POINT('Ctrl Pts',(0.301917961958978,2.21369945770151,5.06876957093372));
#53382=CARTESIAN_POINT('Ctrl Pts',(0.306839867066766,2.19965651831783,5.06792559619228));
#53383=CARTESIAN_POINT('Ctrl Pts',(0.315357967151924,2.16863054863798,5.06611908227535));
#53384=CARTESIAN_POINT('Ctrl Pts',(0.318588355039654,2.1515969625496,5.06516194281945));
#53385=CARTESIAN_POINT('Ctrl Pts',(0.321174776211667,2.12749505029734,5.06377860383119));
#53386=CARTESIAN_POINT('Ctrl Pts',(0.321691767704263,2.12058186235698,5.06337877322469));
#53387=CARTESIAN_POINT('Ctrl Pts',(0.322307005562279,2.10607735327945,5.06252841579754));
#53388=CARTESIAN_POINT('Ctrl Pts',(0.322360732275647,2.09848857118847,5.06207693490839));
#53389=CARTESIAN_POINT('Ctrl Pts',(0.32210207847004,2.08932661322413,5.06152120832134));
#53390=CARTESIAN_POINT('Ctrl Pts',(0.322045903016981,2.08774821026855,5.06142508999017));
#53391=CARTESIAN_POINT('Ctrl Pts',(0.321952508226176,2.08557382528188,5.06129213622317));
#53392=CARTESIAN_POINT('Ctrl Pts',(0.321925230711765,2.08497742053659,5.06125561252182));
#53393=CARTESIAN_POINT('Ctrl Pts',(0.321878554959674,2.08401546098945,5.06119661039005));
#53394=CARTESIAN_POINT('Ctrl Pts',(0.321860190771092,2.08364985549447,5.06117416441928));
#53395=CARTESIAN_POINT('Ctrl Pts',(0.321820619027484,2.08288794873296,5.06112734294976));
#53396=CARTESIAN_POINT('Ctrl Pts',(0.321799302278504,2.08249165397225,5.0611029640643));
#53397=CARTESIAN_POINT('Ctrl Pts',(0.321748376033813,2.08157641944752,5.06104660246538));
#53398=CARTESIAN_POINT('Ctrl Pts',(0.321718243039881,2.08105751095941,5.06101460338021));
#53399=CARTESIAN_POINT('Ctrl Pts',(0.321617631892016,2.07939445399211,5.06091190707832));
#53400=CARTESIAN_POINT('Ctrl Pts',(0.321542305108791,2.07825061745658,5.06084105790569));
#53401=CARTESIAN_POINT('Ctrl Pts',(0.320787889792605,2.06765710290873,5.06018286091458));
#53402=CARTESIAN_POINT('Ctrl Pts',(0.319698585932033,2.0582421626526,5.05958266785852));
#53403=CARTESIAN_POINT('Ctrl Pts',(0.313367349693663,2.01882599424673,5.05700191373256));
#53404=CARTESIAN_POINT('Ctrl Pts',(0.304301913772158,1.98960031671679,5.05490147069499));
#53405=CARTESIAN_POINT('Ctrl Pts',(0.287140701440011,1.95335495075952,5.05223271992611));
#53406=CARTESIAN_POINT('Ctrl Pts',(0.282614343617413,1.94481067941096,5.05160031452623));
#53407=CARTESIAN_POINT('Ctrl Pts',(0.276987258086444,1.93525393670418,5.05089953091354));
#53408=CARTESIAN_POINT('Ctrl Pts',(0.27625603161004,1.93403069051291,5.0508099618198));
#53409=CARTESIAN_POINT('Ctrl Pts',(0.275309056415208,1.93247012419787,5.0506959006802));
#53410=CARTESIAN_POINT('Ctrl Pts',(0.27510077520371,1.93212832485211,5.05067093153232));
#53411=CARTESIAN_POINT('Ctrl Pts',(0.27476509024119,1.93157975242092,5.05063087893878));
#53412=CARTESIAN_POINT('Ctrl Pts',(0.274638089424235,1.93137273515771,5.05061576910076));
#53413=CARTESIAN_POINT('Ctrl Pts',(0.274395771665549,1.9309787457948,5.05058702229763));
#53414=CARTESIAN_POINT('Ctrl Pts',(0.27428049853325,1.93079174959348,5.0505733826751));
#53415=CARTESIAN_POINT('Ctrl Pts',(0.274017247596186,1.93036567948253,5.05054231432302));
#53416=CARTESIAN_POINT('Ctrl Pts',(0.273869148267887,1.93012668159456,5.0505248937666));
#53417=CARTESIAN_POINT('Ctrl Pts',(0.273406626589571,1.92938245612943,5.05047066734592));
#53418=CARTESIAN_POINT('Ctrl Pts',(0.27309111526163,1.92887790172505,5.05043393307344));
#53419=CARTESIAN_POINT('Ctrl Pts',(0.270626167724756,1.92496022628656,5.05014890777184));
#53420=CARTESIAN_POINT('Ctrl Pts',(0.268414104928647,1.92158666819795,5.04990466695142));
#53421=CARTESIAN_POINT('Ctrl Pts',(0.265882829269675,1.91787997546941,5.04963660728115));
#53422=CARTESIAN_POINT('Ctrl Pts',(0.265625697060738,1.91750514719308,5.04960950401381));
#53423=CARTESIAN_POINT('Ctrl Pts',(0.26528888002001,1.91701638026136,5.04957416479857));
#53424=CARTESIAN_POINT('Ctrl Pts',(0.265209914550773,1.91690194927554,5.04956589131828));
#53425=CARTESIAN_POINT('Ctrl Pts',(0.264484257771594,1.91585183484934,5.04948996842644));
#53426=CARTESIAN_POINT('Ctrl Pts',(0.263832683031667,1.91491951813147,5.04942257307185));
#53427=CARTESIAN_POINT('Ctrl Pts',(0.262764931387842,1.91340880477609,5.04931335011777));
#53428=CARTESIAN_POINT('Ctrl Pts',(0.26235175342893,1.91282831199514,5.04927137713442));
#53429=CARTESIAN_POINT('Ctrl Pts',(0.258297495786963,1.90717209849313,5.04886231118013));
#53430=CARTESIAN_POINT('Ctrl Pts',(0.254511303215902,1.90220161647403,5.04850212272989));
#53431=CARTESIAN_POINT('Ctrl Pts',(0.236216575068306,1.87958029254415,5.04684375314817));
#53432=CARTESIAN_POINT('Ctrl Pts',(0.220002117708237,1.86339431269344,5.04559632204089));
#53433=CARTESIAN_POINT('Ctrl Pts',(0.198119025756772,1.84576063487912,5.04399216206107));
#53434=CARTESIAN_POINT('Ctrl Pts',(0.193946331663507,1.84256336681153,5.04368965737329));
#53435=CARTESIAN_POINT('Ctrl Pts',(0.182445540975262,1.83418940689309,5.04286188740506));
#53436=CARTESIAN_POINT('Ctrl Pts',(0.174976916742463,1.8292146549316,5.04233055739251));
#53437=CARTESIAN_POINT('Ctrl Pts',(0.166305791173099,1.82394757245131,5.04171607259803));
#53438=CARTESIAN_POINT('Ctrl Pts',(0.165297242854236,1.82334248540625,5.04164463942759));
#53439=CARTESIAN_POINT('Ctrl Pts',(0.163485821014944,1.82226914867095,5.04151639750932));
#53440=CARTESIAN_POINT('Ctrl Pts',(0.162684187691023,1.82179882369085,5.04145966466839));
#53441=CARTESIAN_POINT('Ctrl Pts',(0.161465443017888,1.82109084492593,5.04137343785837));
#53442=CARTESIAN_POINT('Ctrl Pts',(0.161049811954038,1.82085064188017,5.04134403625283));
#53443=CARTESIAN_POINT('Ctrl Pts',(0.160326126028349,1.8204345608476,5.04129285013193));
#53444=CARTESIAN_POINT('Ctrl Pts',(0.160018313801099,1.82025826070757,5.04127108090512));
#53445=CARTESIAN_POINT('Ctrl Pts',(0.159382076798349,1.81989524826401,5.04122608903721));
#53446=CARTESIAN_POINT('Ctrl Pts',(0.159053613638527,1.81970860459823,5.04120286396458));
#53447=CARTESIAN_POINT('Ctrl Pts',(0.158259178424362,1.81925902626332,5.04114669616668));
#53448=CARTESIAN_POINT('Ctrl Pts',(0.157792879472626,1.81899667426808,5.04111373256036));
#53449=CARTESIAN_POINT('Ctrl Pts',(0.156067027424413,1.81803131508584,5.04099174339158));
#53450=CARTESIAN_POINT('Ctrl Pts',(0.154803426542772,1.81733561359209,5.04090245662954));
#53451=CARTESIAN_POINT('Ctrl Pts',(0.132123422029216,1.80504635994124,5.03930024905909));
#53452=CARTESIAN_POINT('Ctrl Pts',(0.109470280984165,1.79591114036698,5.03769662236508));
#53453=CARTESIAN_POINT('Ctrl Pts',(0.0712673969030711,1.78533169691852,
5.03502197105733));
#53454=CARTESIAN_POINT('Ctrl Pts',(0.056252799806753,1.78230388280608,5.03398014918179));
#53455=CARTESIAN_POINT('Ctrl Pts',(0.0316871621711188,1.77914679892424,
5.03233312175335));
#53456=CARTESIAN_POINT('Ctrl Pts',(0.0222449271769151,1.77835414866932,
5.03171385417739));
#53457=CARTESIAN_POINT('Ctrl Pts',(0.0118497940664607,1.77794158022964,
5.03105658110516));
#53458=CARTESIAN_POINT('Ctrl Pts',(0.0109188324510574,1.77790867364718,
5.03099793357717));
#53459=CARTESIAN_POINT('Ctrl Pts',(0.00929906813292923,1.77785845088637,
5.03089628498103));
#53460=CARTESIAN_POINT('Ctrl Pts',(0.00861033391947493,1.77783930639503,
5.03085318635514));
#53461=CARTESIAN_POINT('Ctrl Pts',(0.00761982568529739,1.77781495229335,
5.03079138576122));
#53462=CARTESIAN_POINT('Ctrl Pts',(0.0073181035060271,1.77780795777662,
5.03077258474916));
#53463=CARTESIAN_POINT('Ctrl Pts',(0.00679432966799497,1.77779655179551,
5.03073998985571));
#53464=CARTESIAN_POINT('Ctrl Pts',(0.00657228282530661,1.77779194601909,
5.03072618500951));
#53465=CARTESIAN_POINT('Ctrl Pts',(0.00614285113018282,1.77778348268963,
5.03069951281746));
#53466=CARTESIAN_POINT('Ctrl Pts',(0.00593546784611308,1.77777959582036,
5.03068664382648));
#53467=CARTESIAN_POINT('Ctrl Pts',(0.00544069010948374,1.77777080030617,
5.03065596837073));
#53468=CARTESIAN_POINT('Ctrl Pts',(0.00515329196500484,1.7777660759206,
5.03063817230475));
#53469=CARTESIAN_POINT('Ctrl Pts',(0.00412911766850792,1.77775061060648,
5.03057483190725));
#53470=CARTESIAN_POINT('Ctrl Pts',(0.00339230423775913,1.77774201193097,
5.03052940691464));
#53471=CARTESIAN_POINT('Ctrl Pts',(-0.00772679117763137,1.77765039046605,
5.02984598613993));
#53472=CARTESIAN_POINT('Ctrl Pts',(-0.0181083723695242,1.7780666037564,
5.02923518388131));
#53473=CARTESIAN_POINT('Ctrl Pts',(-0.0379549990749316,1.77982568252373,
5.02808944697103));
#53474=CARTESIAN_POINT('Ctrl Pts',(-0.0474154973559427,1.78108941310515,
5.02755293200982));
#53475=CARTESIAN_POINT('Ctrl Pts',(-0.0730233954084606,1.78567503326315,
5.02609632587077));
#53476=CARTESIAN_POINT('Ctrl Pts',(-0.0889936083421476,1.78981825803421,
5.02518197589592));
#53477=CARTESIAN_POINT('Ctrl Pts',(-0.113676190606082,1.79828581146635,
5.0236872321499));
#53478=CARTESIAN_POINT('Ctrl Pts',(-0.122630978739701,1.80181323493596,
5.02312726758484));
#53479=CARTESIAN_POINT('Ctrl Pts',(-0.135807048012492,1.80769747134277,
5.02226758582056));
#53480=CARTESIAN_POINT('Ctrl Pts',(-0.14015533842918,1.80975734309257,5.02197783998102));
#53481=CARTESIAN_POINT('Ctrl Pts',(-0.145241276963538,1.81230759595482,
5.02163114716792));
#53482=CARTESIAN_POINT('Ctrl Pts',(-0.146025210563177,1.81270470638167,
5.02157748690999));
#53483=CARTESIAN_POINT('Ctrl Pts',(-0.147227376879879,1.81331986888282,
5.02149485324341));
#53484=CARTESIAN_POINT('Ctrl Pts',(-0.147646775706,1.81353564322915,5.02146596002464));
#53485=CARTESIAN_POINT('Ctrl Pts',(-0.148378877217293,1.81391433320574,
5.02141540998837));
#53486=CARTESIAN_POINT('Ctrl Pts',(-0.148691789796554,1.81407684319918,
5.02139376751383));
#53487=CARTESIAN_POINT('Ctrl Pts',(-0.149396932487417,1.81444452705379,
5.02134491381824));
#53488=CARTESIAN_POINT('Ctrl Pts',(-0.149789007239939,1.81464999584169,
5.02131769219879));
#53489=CARTESIAN_POINT('Ctrl Pts',(-0.150841311059495,1.81520422748594,
5.0212444746596));
#53490=CARTESIAN_POINT('Ctrl Pts',(-0.15150075046947,1.81555447664586,5.02119842611181));
#53491=CARTESIAN_POINT('Ctrl Pts',(-0.154381731918961,1.81709751771464,
5.02099651516158));
#53492=CARTESIAN_POINT('Ctrl Pts',(-0.156590400355959,1.81831404087424,
5.02083980967736));
#53493=CARTESIAN_POINT('Ctrl Pts',(-0.159360322513527,1.81988234423476,
5.02064080561667));
#53494=CARTESIAN_POINT('Ctrl Pts',(-0.15993511903893,1.82021013036475,5.02059937358226));
#53495=CARTESIAN_POINT('Ctrl Pts',(-0.161492626099176,1.82110468936661,
5.02048673536953));
#53496=CARTESIAN_POINT('Ctrl Pts',(-0.162473353175811,1.82167488070132,
5.02041540692031));
#53497=CARTESIAN_POINT('Ctrl Pts',(-0.174844416360484,1.82895504209535,
5.01951051788355));
#53498=CARTESIAN_POINT('Ctrl Pts',(-0.185813026579996,1.83635368112237,
5.01865207491566));
#53499=CARTESIAN_POINT('Ctrl Pts',(-0.202048255611407,1.848822185792,5.01729387039441));
#53500=CARTESIAN_POINT('Ctrl Pts',(-0.20765013893108,1.85343316513334,5.01680758028215));
#53501=CARTESIAN_POINT('Ctrl Pts',(-0.222879251480175,1.86685576212933,
5.01543908957125));
#53502=CARTESIAN_POINT('Ctrl Pts',(-0.232134107363772,1.87606886180473,
5.01455169401613));
#53503=CARTESIAN_POINT('Ctrl Pts',(-0.247318841527261,1.89314104138514,
5.01301926106832));
#53504=CARTESIAN_POINT('Ctrl Pts',(-0.253495756304145,1.90075850562912,
5.01236980037025));
#53505=CARTESIAN_POINT('Ctrl Pts',(-0.261543922447949,1.91166511778105,
5.01149801481006));
#53506=CARTESIAN_POINT('Ctrl Pts',(-0.263718793678523,1.91472276953452,
5.0112595741256));
#53507=CARTESIAN_POINT('Ctrl Pts',(-0.266142202101732,1.91825900329253,
5.01099118635538));
#53508=CARTESIAN_POINT('Ctrl Pts',(-0.266443422265544,1.91870089805796,
5.01095777764401));
#53509=CARTESIAN_POINT('Ctrl Pts',(-0.266896231026274,1.91936874158604,
5.01090748411884));
#53510=CARTESIAN_POINT('Ctrl Pts',(-0.267048633852031,1.91959413310173,
5.01089054433338));
#53511=CARTESIAN_POINT('Ctrl Pts',(-0.267322754595842,1.9200006441147,5.01086005347034));
#53512=CARTESIAN_POINT('Ctrl Pts',(-0.26744457369719,1.92018169379983,5.01084649551848));
#53513=CARTESIAN_POINT('Ctrl Pts',(-0.26770631802739,1.9205715571758,5.01081734765906));
#53514=CARTESIAN_POINT('Ctrl Pts',(-0.267846182451296,1.92078041024095,
5.01080176191374));
#53515=CARTESIAN_POINT('Ctrl Pts',(-0.268223030692836,1.92134456674432,
5.01075973911796));
#53516=CARTESIAN_POINT('Ctrl Pts',(-0.268459553859299,1.92170017955008,
5.01073333323974));
#53517=CARTESIAN_POINT('Ctrl Pts',(-0.26955288541927,1.92335111223036,5.01061112281839));
#53518=CARTESIAN_POINT('Ctrl Pts',(-0.270401048950577,1.92465217269202,
5.01051589088028));
#53519=CARTESIAN_POINT('Ctrl Pts',(-0.288387925022203,1.95268445361817,
5.00848592897194));
#53520=CARTESIAN_POINT('Ctrl Pts',(-0.301495468974115,1.98180211353624,
5.00678883480819));
#53521=CARTESIAN_POINT('Ctrl Pts',(-0.31445233744858,2.0276586973579,5.00408923342287));
#53522=CARTESIAN_POINT('Ctrl Pts',(-0.317635051215339,2.0432425206578,5.00317007649653));
#53523=CARTESIAN_POINT('Ctrl Pts',(-0.319972831598253,2.06146729296592,
5.00206200044817));
#53524=CARTESIAN_POINT('Ctrl Pts',(-0.320261140377203,2.0639419371161,5.00191088117988));
#53525=CARTESIAN_POINT('Ctrl Pts',(-0.320594881149092,2.06712745325744,
5.00171542574204));
#53526=CARTESIAN_POINT('Ctrl Pts',(-0.320666693853842,2.06783552288016,
5.00167192174122));
#53527=CARTESIAN_POINT('Ctrl Pts',(-0.320778601919084,2.0689765693541,5.00160171916253));
#53528=CARTESIAN_POINT('Ctrl Pts',(-0.320820167742375,2.06940940234282,
5.0015750669105));
#53529=CARTESIAN_POINT('Ctrl Pts',(-0.320897650528802,2.07023377578126,
5.00152426204562));
#53530=CARTESIAN_POINT('Ctrl Pts',(-0.320933727207909,2.0706253007265,5.00150011450546));
#53531=CARTESIAN_POINT('Ctrl Pts',(-0.321014323595677,2.0715178532656,5.00144502327685));
#53532=CARTESIAN_POINT('Ctrl Pts',(-0.321058386903391,2.07201892013148,
5.00141406529338));
#53533=CARTESIAN_POINT('Ctrl Pts',(-0.321189123749972,2.07354657295185,
5.001319586422));
#53534=CARTESIAN_POINT('Ctrl Pts',(-0.321272047231104,2.07457346570365,
5.0012559478567));
#53535=CARTESIAN_POINT('Ctrl Pts',(-0.321838053196802,2.08202803440889,
5.00079301173939));
#53536=CARTESIAN_POINT('Ctrl Pts',(-0.322133093955582,2.08846812520689,
5.00038784417965));
#53537=CARTESIAN_POINT('Ctrl Pts',(-0.322262523999165,2.09666583735707,
4.99986492775648));
#53538=CARTESIAN_POINT('Ctrl Pts',(-0.322275895377875,2.0984194669757,4.99975265313351));
#53539=CARTESIAN_POINT('Ctrl Pts',(-0.322271485723973,2.10662967802178,
4.99922505759846));
#53540=CARTESIAN_POINT('Ctrl Pts',(-0.322073989251974,2.11308433849747,
4.99880460416471));
#53541=CARTESIAN_POINT('Ctrl Pts',(-0.32066990953947,2.13621314073731,4.99727868082112));
#53542=CARTESIAN_POINT('Ctrl Pts',(-0.318360545268536,2.15279263742777,
4.99614703720909));
#53543=CARTESIAN_POINT('Ctrl Pts',(-0.31074640657444,2.18746947234569,4.99374543018148));
#53544=CARTESIAN_POINT('Ctrl Pts',(-0.3051187256686,2.20543710589109,4.99248024458738));
#53545=CARTESIAN_POINT('Ctrl Pts',(-0.297555743970668,2.22378553987144,
4.99123033162662));
#53546=CARTESIAN_POINT('Ctrl Pts',(-0.297150388856748,2.2247554693234,4.99116439414858));
#53547=CARTESIAN_POINT('Ctrl Pts',(-0.296595765151285,2.22606452698728,
4.99107560225768));
#53548=CARTESIAN_POINT('Ctrl Pts',(-0.2964506528227,2.22640539274288,4.99105250013645));
#53549=CARTESIAN_POINT('Ctrl Pts',(-0.296221327926977,2.22694150510257,
4.99101619508998));
#53550=CARTESIAN_POINT('Ctrl Pts',(-0.296137509920641,2.22713691853733,
4.99100296812664));
#53551=CARTESIAN_POINT('Ctrl Pts',(-0.295975409014389,2.2275138108057,4.99097746967704));
#53552=CARTESIAN_POINT('Ctrl Pts',(-0.295897153164332,2.22769529919646,
4.99096519670665));
#53553=CARTESIAN_POINT('Ctrl Pts',(-0.295710049611672,2.22812812806948,
4.99093594013195));
#53554=CARTESIAN_POINT('Ctrl Pts',(-0.295601048504267,2.22837940165166,
4.99091896605956));
#53555=CARTESIAN_POINT('Ctrl Pts',(-0.29527475277289,2.22912897240887,4.99086836135098));
#53556=CARTESIAN_POINT('Ctrl Pts',(-0.295056516169467,2.22962686224932,
4.99083478817932));
#53557=CARTESIAN_POINT('Ctrl Pts',(-0.293211738371326,2.23380678250297,
4.99055325076726));
#53558=CARTESIAN_POINT('Ctrl Pts',(-0.291517514121243,2.23745879807833,
4.99030934973404));
#53559=CARTESIAN_POINT('Ctrl Pts',(-0.28592472370122,2.24894561104576,4.98954588004797));
#53560=CARTESIAN_POINT('Ctrl Pts',(-0.281775085198949,2.25665429690691,
4.98903901052657));
#53561=CARTESIAN_POINT('Ctrl Pts',(-0.265187406427254,2.28467168360347,
4.98718285014188));
#53562=CARTESIAN_POINT('Ctrl Pts',(-0.250825608139067,2.30375125909199,
4.98588500129471));
#53563=CARTESIAN_POINT('Ctrl Pts',(-0.230231663522013,2.32559508367137,
4.98416616410154));
#53564=CARTESIAN_POINT('Ctrl Pts',(-0.225840953701362,2.32999047411652,
4.98380685017447));
#53565=CARTESIAN_POINT('Ctrl Pts',(-0.220106859677583,2.33540807054301,
4.98334423219237));
#53566=CARTESIAN_POINT('Ctrl Pts',(-0.218878614581359,2.33655050473622,
4.98324551208478));
#53567=CARTESIAN_POINT('Ctrl Pts',(-0.212895445199329,2.34202916553444,
4.982766268601));
#53568=CARTESIAN_POINT('Ctrl Pts',(-0.208020543743614,2.3462316635459,4.98238074990235));
#53569=CARTESIAN_POINT('Ctrl Pts',(-0.202223643370219,2.35093392368583,
4.9819264460974));
#53570=CARTESIAN_POINT('Ctrl Pts',(-0.201420827684218,2.35157878712385,
4.98186361936357));
#53571=CARTESIAN_POINT('Ctrl Pts',(-0.200221358958731,2.35253284133606,
4.98176987903078));
#53572=CARTESIAN_POINT('Ctrl Pts',(-0.199827045020115,2.35284497347296,
4.98173908317434));
#53573=CARTESIAN_POINT('Ctrl Pts',(-0.199123155569262,2.35339948525176,
4.98168414502061));
#53574=CARTESIAN_POINT('Ctrl Pts',(-0.198813863387272,2.35364222426988,
4.98166001710579));
#53575=CARTESIAN_POINT('Ctrl Pts',(-0.198161536298619,2.35415225805923,
4.98160915415914));
#53576=CARTESIAN_POINT('Ctrl Pts',(-0.197818403251213,2.35441942551036,
4.98158241413985));
#53577=CARTESIAN_POINT('Ctrl Pts',(-0.196912100179739,2.35512214190885,
4.98151182459335));
#53578=CARTESIAN_POINT('Ctrl Pts',(-0.196348028149831,2.35555651883297,
4.98146792882462));
#53579=CARTESIAN_POINT('Ctrl Pts',(-0.193801739109052,2.35750394180115,
4.98126994540544));
#53580=CARTESIAN_POINT('Ctrl Pts',(-0.191803483185973,2.35899578645299,
4.98111502752843));
#53581=CARTESIAN_POINT('Ctrl Pts',(-0.176928058707613,2.3698348146456,4.97996483696135));
#53582=CARTESIAN_POINT('Ctrl Pts',(-0.163393651115211,2.37823864586887,
4.97893335115944));
#53583=CARTESIAN_POINT('Ctrl Pts',(-0.121165639349065,2.40031250055532,
4.97576467543245));
#53584=CARTESIAN_POINT('Ctrl Pts',(-0.0910191242563905,2.41077996187976,
4.97355041953272));
#53585=CARTESIAN_POINT('Ctrl Pts',(-0.0583117413782876,2.41695946677943,
4.97144431421122));
#53586=CARTESIAN_POINT('Ctrl Pts',(-0.056791483864932,2.41723538634693,
4.97134711446894));
#53587=CARTESIAN_POINT('Ctrl Pts',(-0.0548493320747358,2.41757346879647,
4.97122387469924));
#53588=CARTESIAN_POINT('Ctrl Pts',(-0.0544292514864776,2.41764573647393,
4.97119727403627));
#53589=CARTESIAN_POINT('Ctrl Pts',(-0.053761414671408,2.41775926265107,
4.97115507454749));
#53590=CARTESIAN_POINT('Ctrl Pts',(-0.0535137533180082,2.41780106499959,
4.97113944484968));
#53591=CARTESIAN_POINT('Ctrl Pts',(-0.0530508054601922,2.41787864869009,
4.97111026556675));
#53592=CARTESIAN_POINT('Ctrl Pts',(-0.0528355330996498,2.41791450060592,
4.9710967120665));
#53593=CARTESIAN_POINT('Ctrl Pts',(-0.0523515286224808,2.41799460254804,
4.97106627275392));
#53594=CARTESIAN_POINT('Ctrl Pts',(-0.0520827773663643,2.41803873050608,
4.97104939400537));
#53595=CARTESIAN_POINT('Ctrl Pts',(-0.0512848511968853,2.41816870848262,
4.97099934866596));
#53596=CARTESIAN_POINT('Ctrl Pts',(-0.0507555143419635,2.4182535793883,
4.97096623765473));
#53597=CARTESIAN_POINT('Ctrl Pts',(-0.0464817112175732,2.41892788301294,
4.97069960020094));
#53598=CARTESIAN_POINT('Ctrl Pts',(-0.0427271268090138,2.41945256258654,
4.97046967135441));
#53599=CARTESIAN_POINT('Ctrl Pts',(-0.0290514684207105,2.42111820708981,
4.96964497791762));
#53600=CARTESIAN_POINT('Ctrl Pts',(-0.019087289661456,2.42186426015096,
4.9690684034992));
#53601=CARTESIAN_POINT('Ctrl Pts',(0.0225361987648381,2.42304052415228,
4.96670299882422));
#53602=CARTESIAN_POINT('Ctrl Pts',(0.0541331972883655,2.41926902255556,
4.96499186891994));
#53603=CARTESIAN_POINT('Ctrl Pts',(0.0900702326479179,2.40948312028369,
4.96278263195383));
#53604=CARTESIAN_POINT('Ctrl Pts',(0.0954265477058944,2.40787370250556,
4.96244678978236));
#53605=CARTESIAN_POINT('Ctrl Pts',(0.10166385252573,2.40582116776102,4.96204700758918));
#53606=CARTESIAN_POINT('Ctrl Pts',(0.102588264797286,2.40551231309757,4.96198753078389));
#53607=CARTESIAN_POINT('Ctrl Pts',(0.103983286084491,2.40503917827812,4.96189742744099));
#53608=CARTESIAN_POINT('Ctrl Pts',(0.104454944084816,2.40487798989324,4.96186690319567));
#53609=CARTESIAN_POINT('Ctrl Pts',(0.105297483412978,2.40458786874787,4.96181226817832));
#53610=CARTESIAN_POINT('Ctrl Pts',(0.105668507407683,2.40445935088537,4.96178817119696));
#53611=CARTESIAN_POINT('Ctrl Pts',(0.106452312766385,2.40418624562274,4.96173718508696));
#53612=CARTESIAN_POINT('Ctrl Pts',(0.10686503620849,2.40404149544515,4.96171029059445));
#53613=CARTESIAN_POINT('Ctrl Pts',(0.107959305193172,2.40365521054573,4.96163885860543));
#53614=CARTESIAN_POINT('Ctrl Pts',(0.108640331808949,2.40341222249637,4.96159427285685));
#53615=CARTESIAN_POINT('Ctrl Pts',(0.111770688938348,2.40228343089694,4.96138873156491));
#53616=CARTESIAN_POINT('Ctrl Pts',(0.114209986591381,2.40137026698525,4.9612268660532));
#53617=CARTESIAN_POINT('Ctrl Pts',(0.132647455058963,2.39421211295628,4.95999012594554));
#53618=CARTESIAN_POINT('Ctrl Pts',(0.148131934769037,2.3867278776924,4.9588728290175));
#53619=CARTESIAN_POINT('Ctrl Pts',(0.189113194512018,2.3627115362149,4.95570245111312));
#53620=CARTESIAN_POINT('Ctrl Pts',(0.212985217171318,2.34375908173166,4.95359301430377));
#53621=CARTESIAN_POINT('Ctrl Pts',(0.234924769645321,2.32062171719677,4.95157537334494));
#53622=CARTESIAN_POINT('Ctrl Pts',(0.235985663713025,2.31948657417719,4.95147762625543));
#53623=CARTESIAN_POINT('Ctrl Pts',(0.237327728052484,2.31802960252633,4.95135378925536));
#53624=CARTESIAN_POINT('Ctrl Pts',(0.237616501121513,2.31771485130814,4.95132713216683));
#53625=CARTESIAN_POINT('Ctrl Pts',(0.238074220426648,2.31721395991472,4.9512848632618));
#53626=CARTESIAN_POINT('Ctrl Pts',(0.238243574847161,2.31702819599921,4.95126922040223));
#53627=CARTESIAN_POINT('Ctrl Pts',(0.238558607954501,2.31668182483127,4.95124011530601));
#53628=CARTESIAN_POINT('Ctrl Pts',(0.238704340814863,2.31652126989736,4.95122664896153));
#53629=CARTESIAN_POINT('Ctrl Pts',(0.239028435933346,2.31616348709024,4.95119669555889));
#53630=CARTESIAN_POINT('Ctrl Pts',(0.239206715734693,2.31596618597456,4.95118021481238));
#53631=CARTESIAN_POINT('Ctrl Pts',(0.239727800298777,2.31538806820237,4.95113203208205));
#53632=CARTESIAN_POINT('Ctrl Pts',(0.240069943345522,2.31500665215448,4.95110038011802));
#53633=CARTESIAN_POINT('Ctrl Pts',(0.240844396508689,2.3141391497589,4.95102869557715));
#53634=CARTESIAN_POINT('Ctrl Pts',(0.241276149017725,2.31365256544504,4.95098870402498));
#53635=CARTESIAN_POINT('Ctrl Pts',(0.255837842019844,2.29714112953975,4.94963882967666));
#53636=CARTESIAN_POINT('Ctrl Pts',(0.268343427761699,2.27974911802647,4.94844310701638));
#53637=CARTESIAN_POINT('Ctrl Pts',(0.290487159757172,2.24142897747541,4.94596843700238));
#53638=CARTESIAN_POINT('Ctrl Pts',(0.299793301913102,2.22045244646608,4.94469378482681));
#53639=CARTESIAN_POINT('Ctrl Pts',(0.306907861206409,2.19833039312343,4.94331874786958));
#53640=CARTESIAN_POINT('Ctrl Pts',(0.307015917992102,2.19799248736597,4.94329773922019));
#53641=CARTESIAN_POINT('Ctrl Pts',(0.308869314849948,2.19216354830406,4.94293523702275));
#53642=CARTESIAN_POINT('Ctrl Pts',(0.310467557689133,2.18662714662972,4.94258938599066));
#53643=CARTESIAN_POINT('Ctrl Pts',(0.312163835300871,2.18009920665505,4.9421787714325));
#53644=CARTESIAN_POINT('Ctrl Pts',(0.31240683133674,2.17914616021652,4.94211875478632));
#53645=CARTESIAN_POINT('Ctrl Pts',(0.312766857644355,2.1777066196658,4.94202799284582));
#53646=CARTESIAN_POINT('Ctrl Pts',(0.312887125325678,2.177220934866,4.94199735210328));
#53647=CARTESIAN_POINT('Ctrl Pts',(0.313099805080128,2.17635340222543,4.94194258737468));
#53648=CARTESIAN_POINT('Ctrl Pts',(0.313192651098484,2.17597166095557,4.94191847743297));
#53649=CARTESIAN_POINT('Ctrl Pts',(0.313387129071949,2.17516563909467,4.94186754563762));
#53650=CARTESIAN_POINT('Ctrl Pts',(0.313488597887623,2.17474132029835,4.94184071858365));
#53651=CARTESIAN_POINT('Ctrl Pts',(0.313754825874647,2.17361793737006,4.94176965439154));
#53652=CARTESIAN_POINT('Ctrl Pts',(0.3139181096242,2.17291852918753,4.94172536988332));
#53653=CARTESIAN_POINT('Ctrl Pts',(0.314651739773671,2.16972796735458,4.94152316304693));
#53654=CARTESIAN_POINT('Ctrl Pts',(0.31519476699923,2.16723068514589,4.94136436641353));
#53655=CARTESIAN_POINT('Ctrl Pts',(0.317431347067279,2.15632173864572,4.94066822734824));
#53656=CARTESIAN_POINT('Ctrl Pts',(0.318818152565558,2.14785145346323,4.94012121866955));
#53657=CARTESIAN_POINT('Ctrl Pts',(0.321629972427538,2.12498712042102,4.93862639135604));
#53658=CARTESIAN_POINT('Ctrl Pts',(0.322426885125518,2.11053666742506,4.93766171497881));
#53659=CARTESIAN_POINT('Ctrl Pts',(0.322118612248737,2.08517567533685,4.93595025601389));
#53660=CARTESIAN_POINT('Ctrl Pts',(0.321432353448473,2.07428222323742,4.93520946009156));
#53661=CARTESIAN_POINT('Ctrl Pts',(0.318559899753805,2.04912194627197,4.93350583779406));
#53662=CARTESIAN_POINT('Ctrl Pts',(0.315965351473869,2.03492317229471,4.9325498529394));
#53663=CARTESIAN_POINT('Ctrl Pts',(0.312211581362928,2.02008827536237,4.93158776963432));
#53664=CARTESIAN_POINT('Ctrl Pts',(0.311991462736948,2.01923315968619,4.93153244718585));
#53665=CARTESIAN_POINT('Ctrl Pts',(0.311689306878116,2.01807901533772,4.9314579703632));
#53666=CARTESIAN_POINT('Ctrl Pts',(0.311610351183128,2.01777919492188,4.93143864047791));
#53667=CARTESIAN_POINT('Ctrl Pts',(0.311476273151781,2.01727302431225,4.93140603698993));
#53668=CARTESIAN_POINT('Ctrl Pts',(0.311421378339076,2.01706661494332,4.93139275020344));
#53669=CARTESIAN_POINT('Ctrl Pts',(0.311311329296443,2.01665447075513,4.93136623717617));
#53670=CARTESIAN_POINT('Ctrl Pts',(0.311256176734703,2.0164487376626,4.93135301103546));
#53671=CARTESIAN_POINT('Ctrl Pts',(0.311129591912441,2.01597840888347,4.93132279400105));
#53672=CARTESIAN_POINT('Ctrl Pts',(0.311058026175602,2.01571384994894,4.93130581100523));
#53673=CARTESIAN_POINT('Ctrl Pts',(0.310841818368519,2.01491861475394,4.93125480326497));
#53674=CARTESIAN_POINT('Ctrl Pts',(0.310696154181569,2.01438821372391,4.93122083776021));
#53675=CARTESIAN_POINT('Ctrl Pts',(0.310359140540996,2.01317324870739,4.93114315596628));
#53676=CARTESIAN_POINT('Ctrl Pts',(0.310166882007339,2.0124889367837,4.9310994913013));
#53677=CARTESIAN_POINT('Ctrl Pts',(0.3095296218116,2.01024919953733,4.93095685115454));
#53678=CARTESIAN_POINT('Ctrl Pts',(0.309075163547145,2.00869645962982,4.93085839574877));
#53679=CARTESIAN_POINT('Ctrl Pts',(0.307172379495514,2.00237229765838,4.93045891718404));
#53680=CARTESIAN_POINT('Ctrl Pts',(0.305625028726907,1.99763112468333,4.93016297582191));
#53681=CARTESIAN_POINT('Ctrl Pts',(0.298446854704317,1.97725300163685,4.92889879734349));
#53682=CARTESIAN_POINT('Ctrl Pts',(0.29172090269926,1.96202768642256,4.92797351204341));
#53683=CARTESIAN_POINT('Ctrl Pts',(0.271449038642051,1.92432310109351,4.92558069045999));
#53684=CARTESIAN_POINT('Ctrl Pts',(0.256285466088191,1.90285931328351,4.924108867789));
#53685=CARTESIAN_POINT('Ctrl Pts',(0.237656837394638,1.88232412738319,4.92242765980989));
#53686=CARTESIAN_POINT('Ctrl Pts',(0.236611623555963,1.88118844329193,4.92233372892197));
#53687=CARTESIAN_POINT('Ctrl Pts',(0.235182587814837,1.87965792707016,4.92220582218965));
#53688=CARTESIAN_POINT('Ctrl Pts',(0.234805840942989,1.87925649326101,4.92217214938553));
#53689=CARTESIAN_POINT('Ctrl Pts',(0.23416590652874,1.87857811804576,4.92211503384966));
#53690=CARTESIAN_POINT('Ctrl Pts',(0.233903250839194,1.87830067471143,4.92209161405256));
#53691=CARTESIAN_POINT('Ctrl Pts',(0.233396625760517,1.87776742888401,4.92204648407902));
#53692=CARTESIAN_POINT('Ctrl Pts',(0.233152727485863,1.87751155929903,4.92202477699577));
#53693=CARTESIAN_POINT('Ctrl Pts',(0.232576548693942,1.87690908766511,4.92197354183132));
#53694=CARTESIAN_POINT('Ctrl Pts',(0.232243914259228,1.87656282660576,4.92194399840028));
#53695=CARTESIAN_POINT('Ctrl Pts',(0.231272526633299,1.87555615803756,4.92185782447984));
#53696=CARTESIAN_POINT('Ctrl Pts',(0.230631725549644,1.8748977412103,4.9218011046692));
#53697=CARTESIAN_POINT('Ctrl Pts',(0.226008115444792,1.87018749492261,4.92139274397734));
#53698=CARTESIAN_POINT('Ctrl Pts',(0.221921805314116,1.86623909346406,4.92103654449244));
#53699=CARTESIAN_POINT('Ctrl Pts',(0.208276177960231,1.85373437244721,4.91986095935454));
#53700=CARTESIAN_POINT('Ctrl Pts',(0.198310988337186,1.84564117916157,4.919023077544));
#53701=CARTESIAN_POINT('Ctrl Pts',(0.166979342514135,1.82315787851648,4.91645524053457));
#53702=CARTESIAN_POINT('Ctrl Pts',(0.144346563418404,1.81071179923744,4.91467843008413));
#53703=CARTESIAN_POINT('Ctrl Pts',(0.119867772167208,1.80084565593393,4.9129509756304));
#53704=CARTESIAN_POINT('Ctrl Pts',(0.119259704409608,1.80060272664195,4.91290818688716));
#53705=CARTESIAN_POINT('Ctrl Pts',(0.118107154228722,1.80014633942668,4.91282732028419));
#53706=CARTESIAN_POINT('Ctrl Pts',(0.117562823543743,1.79993250731083,4.91278922782771));
#53707=CARTESIAN_POINT('Ctrl Pts',(0.116104641530133,1.79936425933894,4.91268745518606));
#53708=CARTESIAN_POINT('Ctrl Pts',(0.115189743210504,1.7990125260885,4.91262388522602));
#53709=CARTESIAN_POINT('Ctrl Pts',(0.114031636473136,1.79857334511165,4.91254378762926));
#53710=CARTESIAN_POINT('Ctrl Pts',(0.113789918209831,1.79848201229681,4.91252709016359));
#53711=CARTESIAN_POINT('Ctrl Pts',(0.109546616859029,1.79688451781218,4.9122343310971));
#53712=CARTESIAN_POINT('Ctrl Pts',(0.105515314470069,1.79545775395595,4.91196181916322));
#53713=CARTESIAN_POINT('Ctrl Pts',(0.100939315151927,1.79393999399408,4.91165971645277));
#53714=CARTESIAN_POINT('Ctrl Pts',(0.100421614059181,1.79376974013052,4.91162564187411));
#53715=CARTESIAN_POINT('Ctrl Pts',(0.0996388310344936,1.79351450856575,
4.91157427878358));
#53716=CARTESIAN_POINT('Ctrl Pts',(0.0993740700341939,1.79342856082816,
4.91155693364632));
#53717=CARTESIAN_POINT('Ctrl Pts',(0.0989140740047226,1.7932798936513,4.9115268461984));
#53718=CARTESIAN_POINT('Ctrl Pts',(0.0987188904218197,1.79321701750391,
4.9115140946151));
#53719=CARTESIAN_POINT('Ctrl Pts',(0.098326416285836,1.79309099981352,4.91148848412391));
#53720=CARTESIAN_POINT('Ctrl Pts',(0.0981291250528937,1.79302786225508,
4.91147562549983));
#53721=CARTESIAN_POINT('Ctrl Pts',(0.0976511473070049,1.7928754066882,4.91144450991313));
#53722=CARTESIAN_POINT('Ctrl Pts',(0.0973703980071717,1.79278628288943,
4.9114262644739));
#53723=CARTESIAN_POINT('Ctrl Pts',(0.0964694179139788,1.79250162610258,
4.91136780911793));
#53724=CARTESIAN_POINT('Ctrl Pts',(0.0958487122960348,1.79230758392387,
4.91132768655093));
#53725=CARTESIAN_POINT('Ctrl Pts',(0.0943896870109544,1.79185631348505,
4.91123371426582));
#53726=CARTESIAN_POINT('Ctrl Pts',(0.0935508916661377,1.79160062376468,
4.91117995205819));
#53727=CARTESIAN_POINT('Ctrl Pts',(0.0906499029710511,1.79072924102489,
4.91099488685064));
#53728=CARTESIAN_POINT('Ctrl Pts',(0.0885825422377806,1.79013076785538,
4.91086452117648));
#53729=CARTESIAN_POINT('Ctrl Pts',(0.0796508718086383,1.78764186488825,
4.91030720788724));
#53730=CARTESIAN_POINT('Ctrl Pts',(0.0727304956507097,1.78595835325802,
4.90989034566553));
#53731=CARTESIAN_POINT('Ctrl Pts',(0.0557793061854829,1.78242516294654,
4.90889292126009));
#53732=CARTESIAN_POINT('Ctrl Pts',(0.0457054754876024,1.78081958425325,
4.90831986355142));
#53733=CARTESIAN_POINT('Ctrl Pts',(0.0126161561991393,1.77714479862516,
4.9064563309362));
#53734=CARTESIAN_POINT('Ctrl Pts',(-0.0105450421554305,1.77707068013885,
4.90517593918929));
#53735=CARTESIAN_POINT('Ctrl Pts',(-0.0340603516362207,1.77952945658949,
4.9037844805471));
#53736=CARTESIAN_POINT('Ctrl Pts',(-0.0346059736006281,1.77958791637398,
4.90375214751362));
#53737=CARTESIAN_POINT('Ctrl Pts',(-0.0370285748449317,1.77985374229101,
4.9036083722892));
#53738=CARTESIAN_POINT('Ctrl Pts',(-0.0389038331065797,1.78007620713922,
4.90349650885488));
#53739=CARTESIAN_POINT('Ctrl Pts',(-0.0457185701542494,1.78094545235103,
4.90308777707625));
#53740=CARTESIAN_POINT('Ctrl Pts',(-0.0506446370890009,1.78169023169552,
4.90278806349461));
#53741=CARTESIAN_POINT('Ctrl Pts',(-0.0563944995492054,1.78269640900079,
4.9024325737323));
#53742=CARTESIAN_POINT('Ctrl Pts',(-0.0572371347822403,1.78284732569291,
4.90238033452974));
#53743=CARTESIAN_POINT('Ctrl Pts',(-0.0585849977047262,1.78309427563108,
4.90229654169261));
#53744=CARTESIAN_POINT('Ctrl Pts',(-0.0590906181149852,1.78318816477316,
4.90226505635006));
#53745=CARTESIAN_POINT('Ctrl Pts',(-0.0599851499888794,1.7833564872005,
4.90220925971586));
#53746=CARTESIAN_POINT('Ctrl Pts',(-0.0603741539823994,1.78343042795322,
4.90218496416936));
#53747=CARTESIAN_POINT('Ctrl Pts',(-0.061180671074282,1.78358526903079,
4.90213452710143));
#53748=CARTESIAN_POINT('Ctrl Pts',(-0.061598162073709,1.78366627920217,
4.90210838211758));
#53749=CARTESIAN_POINT('Ctrl Pts',(-0.0626719243003144,1.78387683886596,
4.90204104447265));
#53750=CARTESIAN_POINT('Ctrl Pts',(-0.0633279523224707,1.78400760524223,
4.90199981301688));
#53751=CARTESIAN_POINT('Ctrl Pts',(-0.0660465977404793,1.78455832027943,
4.90182856580469));
#53752=CARTESIAN_POINT('Ctrl Pts',(-0.0681054465392296,1.78499642193805,
4.9016979707848));
#53753=CARTESIAN_POINT('Ctrl Pts',(-0.0819021885258003,1.78807380619137,
4.90081656257755));
#53754=CARTESIAN_POINT('Ctrl Pts',(-0.0934872709603142,1.79134811145348,
4.90004535706683));
#53755=CARTESIAN_POINT('Ctrl Pts',(-0.118037164213278,1.79979579047846,
4.89834238871617));
#53756=CARTESIAN_POINT('Ctrl Pts',(-0.130904235254047,1.80517910128837,
4.8974060981435));
#53757=CARTESIAN_POINT('Ctrl Pts',(-0.156012751790007,1.81765248781097,
4.89551012055536));
#53758=CARTESIAN_POINT('Ctrl Pts',(-0.168218820636678,1.8247500149342,4.89455235768706));
#53759=CARTESIAN_POINT('Ctrl Pts',(-0.187449868611456,1.83769088207898,
4.89301814238897));
#53760=CARTESIAN_POINT('Ctrl Pts',(-0.19476223326193,1.84307348380651,4.89242838634614));
#53761=CARTESIAN_POINT('Ctrl Pts',(-0.202397233178494,1.84920715798605,
4.89181377737325));
#53762=CARTESIAN_POINT('Ctrl Pts',(-0.202954644578776,1.84965803014506,
4.89176891387104));
#53763=CARTESIAN_POINT('Ctrl Pts',(-0.203730781650267,1.85029011853364,
4.8917064622363));
#53764=CARTESIAN_POINT('Ctrl Pts',(-0.203950774068478,1.85046976525445,
4.89168876242783));
#53765=CARTESIAN_POINT('Ctrl Pts',(-0.20433031942275,1.85078054080631,4.89165822912815));
#53766=CARTESIAN_POINT('Ctrl Pts',(-0.204489983837239,1.85091153220795,
4.89164538569328));
#53767=CARTESIAN_POINT('Ctrl Pts',(-0.204810273912798,1.85117481914578,
4.89161962389364));
#53768=CARTESIAN_POINT('Ctrl Pts',(-0.204970897090989,1.85130711656083,
4.89160670577159));
#53769=CARTESIAN_POINT('Ctrl Pts',(-0.205299163985142,1.85157802792428,
4.89158030719383));
#53770=CARTESIAN_POINT('Ctrl Pts',(-0.205466795978473,1.8517166564306,4.89156682778007));
#53771=CARTESIAN_POINT('Ctrl Pts',(-0.206024825204633,1.85217908828728,
4.89152195981218));
#53772=CARTESIAN_POINT('Ctrl Pts',(-0.206414600923051,1.85250364564947,
4.89149062600046));
#53773=CARTESIAN_POINT('Ctrl Pts',(-0.209158625115843,1.85479952340239,
4.89127006377298));
#53774=CARTESIAN_POINT('Ctrl Pts',(-0.211485461943075,1.85680356655684,
4.89108318069101));
#53775=CARTESIAN_POINT('Ctrl Pts',(-0.218456199692757,1.86298299943317,
4.89052250082994));
#53776=CARTESIAN_POINT('Ctrl Pts',(-0.223007936643175,1.86726057393529,
4.89015525580672));
#53777=CARTESIAN_POINT('Ctrl Pts',(-0.231209344535718,1.87542968286756,
4.88948499572229));
#53778=CARTESIAN_POINT('Ctrl Pts',(-0.234892137846137,1.8792846267259,4.88918056091153));
#53779=CARTESIAN_POINT('Ctrl Pts',(-0.2588322070827,1.90562200977954,4.88716418725922));
#53780=CARTESIAN_POINT('Ctrl Pts',(-0.275930231567867,1.93076811539111,
4.88552213332932));
#53781=CARTESIAN_POINT('Ctrl Pts',(-0.289433127595241,1.95826159141789,
4.88370980546362));
#53782=CARTESIAN_POINT('Ctrl Pts',(-0.289595244123922,1.95859311757843,
4.88368795218456));
#53783=CARTESIAN_POINT('Ctrl Pts',(-0.292279880270452,1.96410714284778,
4.88332448532333));
#53784=CARTESIAN_POINT('Ctrl Pts',(-0.294663360651078,1.96935584767068,
4.8829785127219));
#53785=CARTESIAN_POINT('Ctrl Pts',(-0.297287267483676,1.97557161183215,
4.88256776650722));
#53786=CARTESIAN_POINT('Ctrl Pts',(-0.297665659860272,1.97647956405412,
4.88250774327529));
#53787=CARTESIAN_POINT('Ctrl Pts',(-0.298230257399003,1.97785197678372,
4.88241697330308));
#53788=CARTESIAN_POINT('Ctrl Pts',(-0.298419549601623,1.97831516768709,
4.88238633114226));
#53789=CARTESIAN_POINT('Ctrl Pts',(-0.298755537806978,1.97914281732393,
4.88233156483162));
#53790=CARTESIAN_POINT('Ctrl Pts',(-0.298902647857488,1.97950710777665,
4.88230745472925));
#53791=CARTESIAN_POINT('Ctrl Pts',(-0.299211711218769,1.98027649426032,
4.88225652358116));
#53792=CARTESIAN_POINT('Ctrl Pts',(-0.299373508694214,1.98068165167838,
4.88222969733709));
#53793=CARTESIAN_POINT('Ctrl Pts',(-0.29979946855865,1.98175461941225,4.88215863756179));
#53794=CARTESIAN_POINT('Ctrl Pts',(-0.300062221155235,1.9824229835366,4.88211435667104));
#53795=CARTESIAN_POINT('Ctrl Pts',(-0.301249592477169,1.98547320476046,
4.88191218954603));
#53796=CARTESIAN_POINT('Ctrl Pts',(-0.302148079004301,1.98786507437551,
4.88175342942669));
#53797=CARTESIAN_POINT('Ctrl Pts',(-0.30593919039407,1.99833392497667,4.88105739941803));
#53798=CARTESIAN_POINT('Ctrl Pts',(-0.30853685196925,2.00651327541375,4.8805104656047));
#53799=CARTESIAN_POINT('Ctrl Pts',(-0.318435690733512,2.04261773638176,
4.87808123122172));
#53800=CARTESIAN_POINT('Ctrl Pts',(-0.322292289400603,2.07134562550872,
4.87609432867143));
#53801=CARTESIAN_POINT('Ctrl Pts',(-0.322274941730377,2.10019379804403,
4.87417052639597));
#53802=CARTESIAN_POINT('',(-0.322274997047983,2.09995637979558,4.62467682828221));
#53803=CARTESIAN_POINT('Ctrl Pts',(-0.322274941450803,2.10019426240285,
4.87417049542921));
#53804=CARTESIAN_POINT('Ctrl Pts',(-0.322268128655327,2.11149646618101,
4.87341678409002));
#53805=CARTESIAN_POINT('Ctrl Pts',(-0.321666760855951,2.12279221049134,
4.87267666953879));
#53806=CARTESIAN_POINT('Ctrl Pts',(-0.320424902963008,2.13448569369698,
4.87193935096571));
#53807=CARTESIAN_POINT('Ctrl Pts',(-0.320376031233745,2.13493680187771,
4.87191095211947));
#53808=CARTESIAN_POINT('Ctrl Pts',(-0.320294868028792,2.13567148149227,
4.87186477682651));
#53809=CARTESIAN_POINT('Ctrl Pts',(-0.320263152514294,2.13595511396919,
4.87184696857217));
#53810=CARTESIAN_POINT('Ctrl Pts',(-0.320206675156625,2.13645418820485,
4.87181566618503));
#53811=CARTESIAN_POINT('Ctrl Pts',(-0.320182072613328,2.13666964726079,
4.87180216311917));
#53812=CARTESIAN_POINT('Ctrl Pts',(-0.320133378167099,2.1370923081101,4.87177569573478));
#53813=CARTESIAN_POINT('Ctrl Pts',(-0.320109302509417,2.13729951186743,
4.87176273048878));
#53814=CARTESIAN_POINT('Ctrl Pts',(-0.320060901577437,2.13771256916723,
4.87173690464753));
#53815=CARTESIAN_POINT('Ctrl Pts',(-0.320036578926151,2.13791842219309,
4.8717240439309));
#53816=CARTESIAN_POINT('Ctrl Pts',(-0.319978115060117,2.13840916341201,
4.87169340820454));
#53817=CARTESIAN_POINT('Ctrl Pts',(-0.319943791889473,2.13869403034452,
4.87167564353179));
#53818=CARTESIAN_POINT('Ctrl Pts',(-0.319820330693305,2.13970730693732,
4.87161252013109));
#53819=CARTESIAN_POINT('Ctrl Pts',(-0.319729084340935,2.14043546464048,
4.87156727967688));
#53820=CARTESIAN_POINT('Ctrl Pts',(-0.318336874951251,2.15124604585586,
4.87089733286547));
#53821=CARTESIAN_POINT('Ctrl Pts',(-0.316561887017375,2.16126289887626,
4.8702986931919));
#53822=CARTESIAN_POINT('Ctrl Pts',(-0.313962964170089,2.17273917804128,
4.86962136279284));
#53823=CARTESIAN_POINT('Ctrl Pts',(-0.313598303937198,2.17429559055922,
4.86952968879505));
#53824=CARTESIAN_POINT('Ctrl Pts',(-0.308532015426681,2.19521700439227,
4.86829915195087));
#53825=CARTESIAN_POINT('Ctrl Pts',(-0.302055595949303,2.21410856289424,
4.86720559521908));
#53826=CARTESIAN_POINT('Ctrl Pts',(-0.288420639419096,2.24439985878511,
4.86532880260235));
#53827=CARTESIAN_POINT('Ctrl Pts',(-0.282222028776344,2.25616804327379,
4.86456601735192));
#53828=CARTESIAN_POINT('Ctrl Pts',(-0.272308552442702,2.2724606763237,4.86343522251373));
#53829=CARTESIAN_POINT('Ctrl Pts',(-0.269169583373027,2.27731994114857,
4.86308784788229));
#53830=CARTESIAN_POINT('Ctrl Pts',(-0.265380204734901,2.282853423421,4.86267932171832));
#53831=CARTESIAN_POINT('Ctrl Pts',(-0.264855436120933,2.28361270503775,
4.86262297646148));
#53832=CARTESIAN_POINT('Ctrl Pts',(-0.264052222736889,2.28476425706182,
4.86253707624422));
#53833=CARTESIAN_POINT('Ctrl Pts',(-0.26377614634954,2.28515818003233,4.86250761177816));
#53834=CARTESIAN_POINT('Ctrl Pts',(-0.263295605950863,2.28584058905837,
4.86245643010016));
#53835=CARTESIAN_POINT('Ctrl Pts',(-0.263091546647212,2.28612936021965,
4.86243472843184));
#53836=CARTESIAN_POINT('Ctrl Pts',(-0.262666258801115,2.28672910260028,
4.86238956606743));
#53837=CARTESIAN_POINT('Ctrl Pts',(-0.262444952403878,2.28704001771347,
4.86236610239837));
#53838=CARTESIAN_POINT('Ctrl Pts',(-0.261903921812844,2.28779726515785,
4.86230883103157));
#53839=CARTESIAN_POINT('Ctrl Pts',(-0.26158360915885,2.28824317378112,4.86227500066798));
#53840=CARTESIAN_POINT('Ctrl Pts',(-0.260364349747404,2.28993138876847,
4.86214651446085));
#53841=CARTESIAN_POINT('Ctrl Pts',(-0.259457690959584,2.29116807665078,
4.86205156024783));
#53842=CARTESIAN_POINT('Ctrl Pts',(-0.258188081013857,2.29287416207649,
4.86191939145064));
#53843=CARTESIAN_POINT('Ctrl Pts',(-0.257832597204343,2.29334911270965,
4.86188247014929));
#53844=CARTESIAN_POINT('Ctrl Pts',(-0.236716853230922,2.32139940111636,
4.85969434212092));
#53845=CARTESIAN_POINT('Ctrl Pts',(-0.211666025758102,2.34545629989079,
4.85734672268934));
#53846=CARTESIAN_POINT('Ctrl Pts',(-0.175988098028588,2.37012624668841,
4.85442776457839));
#53847=CARTESIAN_POINT('Ctrl Pts',(-0.168479501207194,2.37487211219895,
4.85383542130252));
#53848=CARTESIAN_POINT('Ctrl Pts',(-0.157159769817998,2.38138846941071,
4.85298332544006));
#53849=CARTESIAN_POINT('Ctrl Pts',(-0.153495025439052,2.38340420751134,
4.85271349829144));
#53850=CARTESIAN_POINT('Ctrl Pts',(-0.148531186383487,2.38600994680659,
4.85235704602735));
#53851=CARTESIAN_POINT('Ctrl Pts',(-0.14726607644514,2.38666340174567,4.85226697134025));
#53852=CARTESIAN_POINT('Ctrl Pts',(-0.145143175727789,2.3877421600609,4.85211716236207));
#53853=CARTESIAN_POINT('Ctrl Pts',(-0.144287759498379,2.38817205737353,
4.85205715818387));
#53854=CARTESIAN_POINT('Ctrl Pts',(-0.143122279916794,2.3887512892182,4.85197590675229));
#53855=CARTESIAN_POINT('Ctrl Pts',(-0.142813885492725,2.38890394276794,
4.85195445467657));
#53856=CARTESIAN_POINT('Ctrl Pts',(-0.142322137422816,2.38914637556452,
4.85192032499414));
#53857=CARTESIAN_POINT('Ctrl Pts',(-0.142138943045734,2.38923647448601,
4.85190762732413));
#53858=CARTESIAN_POINT('Ctrl Pts',(-0.141757448412948,2.38942365174824,
4.85188122031524));
#53859=CARTESIAN_POINT('Ctrl Pts',(-0.141559134511655,2.38952070013796,
4.85186751294768));
#53860=CARTESIAN_POINT('Ctrl Pts',(-0.141101270043214,2.38974418125038,
4.85183591116737));
#53861=CARTESIAN_POINT('Ctrl Pts',(-0.1408416483862,2.38987046944743,4.85181802585306));
#53862=CARTESIAN_POINT('Ctrl Pts',(-0.140010570155516,2.39027335209213,
4.85176087975923));
#53863=CARTESIAN_POINT('Ctrl Pts',(-0.139438461309851,2.39054860903778,
4.85172170211838));
#53864=CARTESIAN_POINT('Ctrl Pts',(-0.134286039308753,2.39300885418631,
4.85137028360454));
#53865=CARTESIAN_POINT('Ctrl Pts',(-0.129655215699195,2.39508720923257,
4.85106448456639));
#53866=CARTESIAN_POINT('Ctrl Pts',(-0.124777432473551,2.39713938616822,
4.85075078170711));
#53867=CARTESIAN_POINT('Ctrl Pts',(-0.124577853788275,2.39722311621589,
4.85073796079745));
#53868=CARTESIAN_POINT('Ctrl Pts',(-0.120528645131049,2.39891710204929,
4.85047813139925));
#53869=CARTESIAN_POINT('Ctrl Pts',(-0.116648025050203,2.40045270722893,
4.8502344541806));
#53870=CARTESIAN_POINT('Ctrl Pts',(-0.0973425337813854,2.40766165707349,
4.84904328892021));
#53871=CARTESIAN_POINT('Ctrl Pts',(-0.0815283744665412,2.41222500997753,
4.84813226904585));
#53872=CARTESIAN_POINT('Ctrl Pts',(-0.0634174388931679,2.4159804528886,
4.84709737643731));
#53873=CARTESIAN_POINT('Ctrl Pts',(-0.0613966437774145,2.4163793138569,
4.84698203834633));
#53874=CARTESIAN_POINT('Ctrl Pts',(-0.0569698697425441,2.41720905310331,
4.84672946753446));
#53875=CARTESIAN_POINT('Ctrl Pts',(-0.0545625397841204,2.41763198598952,
4.84659217424934));
#53876=CARTESIAN_POINT('Ctrl Pts',(-0.049199147629875,2.41851148346717,
4.84628609520719));
#53877=CARTESIAN_POINT('Ctrl Pts',(-0.0462410873781094,2.41895435826742,
4.84611715067794));
#53878=CARTESIAN_POINT('Ctrl Pts',(-0.0394372929907041,2.41987637016344,
4.84572768648321));
#53879=CARTESIAN_POINT('Ctrl Pts',(-0.0355882665178808,2.42032743618227,
4.84550671726191));
#53880=CARTESIAN_POINT('Ctrl Pts',(-0.0197746804476762,2.4218920901358,
4.84459424930391));
#53881=CARTESIAN_POINT('Ctrl Pts',(-0.00776167628994374,2.4224054320035,
4.84388978840217));
#53882=CARTESIAN_POINT('Ctrl Pts',(0.00635418966876181,2.42221921712871,
4.84303653023704));
#53883=CARTESIAN_POINT('Ctrl Pts',(0.00845697275531886,2.42217088462533,
4.84290877476047));
#53884=CARTESIAN_POINT('Ctrl Pts',(0.0112274795880952,2.4220800623233,4.84273954849792));
#53885=CARTESIAN_POINT('Ctrl Pts',(0.0118957911237079,2.42205607118482,
4.84269865789764));
#53886=CARTESIAN_POINT('Ctrl Pts',(0.0129889325340823,2.42201342220907,
4.84263165915507));
#53887=CARTESIAN_POINT('Ctrl Pts',(0.0134138110157763,2.42199600327094,
4.84260558989657));
#53888=CARTESIAN_POINT('Ctrl Pts',(0.0142342726536967,2.42196073970551,
4.84255519348863));
#53889=CARTESIAN_POINT('Ctrl Pts',(0.0146298600493643,2.42194300679221,
4.84253086988713));
#53890=CARTESIAN_POINT('Ctrl Pts',(0.0155392175825932,2.4219005637038,4.84247489833979));
#53891=CARTESIAN_POINT('Ctrl Pts',(0.0160529622635845,2.42187535257235,
4.84244323473672));
#53892=CARTESIAN_POINT('Ctrl Pts',(0.0174218916145037,2.42180488919129,
4.84235874979769));
#53893=CARTESIAN_POINT('Ctrl Pts',(0.0182769556424048,2.42175745816472,
4.8423058602328));
#53894=CARTESIAN_POINT('Ctrl Pts',(0.0241106936887208,2.4214105271917,4.84194419742778));
#53895=CARTESIAN_POINT('Ctrl Pts',(0.0290817875505189,2.42099890603712,
4.84163192225173));
#53896=CARTESIAN_POINT('Ctrl Pts',(0.0354452542983857,2.42032296737841,
4.84122663125795));
#53897=CARTESIAN_POINT('Ctrl Pts',(0.0368483816991462,2.42016459227723,
4.84113691936874));
#53898=CARTESIAN_POINT('Ctrl Pts',(0.0615720046078876,2.41720928771899,
4.83955001167512));
#53899=CARTESIAN_POINT('Ctrl Pts',(0.0845152488114976,2.41188084254682,
4.83797290926765));
#53900=CARTESIAN_POINT('Ctrl Pts',(0.117922385920848,2.40016268419484,4.83557709613835));
#53901=CARTESIAN_POINT('Ctrl Pts',(0.12894585453008,2.39559485409365,4.83477050991965));
#53902=CARTESIAN_POINT('Ctrl Pts',(0.145281319472512,2.38773771426922,4.83357135995942));
#53903=CARTESIAN_POINT('Ctrl Pts',(0.150793000920482,2.38488793481828,4.83316613614821));
#53904=CARTESIAN_POINT('Ctrl Pts',(0.158002113638956,2.38089261685851,4.83263846629668));
#53905=CARTESIAN_POINT('Ctrl Pts',(0.159775532780996,2.37988767341365,4.83250885714809));
#53906=CARTESIAN_POINT('Ctrl Pts',(0.162268400156727,2.37844362410543,4.8323270738612));
#53907=CARTESIAN_POINT('Ctrl Pts',(0.162995802000475,2.37801844194476,4.83227408012897));
#53908=CARTESIAN_POINT('Ctrl Pts',(0.164265118212909,2.37726980511566,4.8321817040103));
#53909=CARTESIAN_POINT('Ctrl Pts',(0.164807761611215,2.37694760446531,4.83214224392933));
#53910=CARTESIAN_POINT('Ctrl Pts',(0.165598491076305,2.37647495284844,4.83208479351402));
#53911=CARTESIAN_POINT('Ctrl Pts',(0.165847321711147,2.37632576007698,4.83206672199443));
#53912=CARTESIAN_POINT('Ctrl Pts',(0.166274265406379,2.37606899062516,4.83203572781));
#53913=CARTESIAN_POINT('Ctrl Pts',(0.166452476047773,2.37596157728889,4.83202279440428));
#53914=CARTESIAN_POINT('Ctrl Pts',(0.166807339571422,2.37574722071598,4.83199704855406));
#53915=CARTESIAN_POINT('Ctrl Pts',(0.166983993388746,2.37564028047446,4.83198423595731));
#53916=CARTESIAN_POINT('Ctrl Pts',(0.167403304812929,2.37538589249596,4.83195383248506));
#53917=CARTESIAN_POINT('Ctrl Pts',(0.167645871068165,2.3752382934174,4.83193625158671));
#53918=CARTESIAN_POINT('Ctrl Pts',(0.168372146672137,2.37479504586338,4.83188363240171));
#53919=CARTESIAN_POINT('Ctrl Pts',(0.168855274556989,2.37449843947065,4.83184865654926));
#53920=CARTESIAN_POINT('Ctrl Pts',(0.173524394531838,2.37161493813981,4.83151087488642));
#53921=CARTESIAN_POINT('Ctrl Pts',(0.177651679100235,2.36893359304684,4.8312141415317));
#53922=CARTESIAN_POINT('Ctrl Pts',(0.1821138842968,2.36588708250768,4.83089351143413));
#53923=CARTESIAN_POINT('Ctrl Pts',(0.182510962329631,2.36561467604989,4.83086498117166));
#53924=CARTESIAN_POINT('Ctrl Pts',(0.183958819967914,2.36461662621113,4.83076095201303));
#53925=CARTESIAN_POINT('Ctrl Pts',(0.185005906809195,2.36388562076396,4.83068571870046));
#53926=CARTESIAN_POINT('Ctrl Pts',(0.208035144533708,2.34760371203934,4.82903042001129));
#53927=CARTESIAN_POINT('Ctrl Pts',(0.227988780203923,2.32936356013473,4.82757509403875));
#53928=CARTESIAN_POINT('Ctrl Pts',(0.255361709097943,2.29719496307759,4.82517797169339));
#53929=CARTESIAN_POINT('Ctrl Pts',(0.264436702590681,2.28484749174768,4.8242905871659));
#53930=CARTESIAN_POINT('Ctrl Pts',(0.273899678817082,2.26984134581946,4.82322038231216));
#53931=CARTESIAN_POINT('Ctrl Pts',(0.27517636809393,2.26776496280401,4.82307250538115));
#53932=CARTESIAN_POINT('Ctrl Pts',(0.276792354679387,2.26506867243317,4.82288066978062));
#53933=CARTESIAN_POINT('Ctrl Pts',(0.27715336030624,2.26446181649937,4.82283750557514));
#53934=CARTESIAN_POINT('Ctrl Pts',(0.277732808280146,2.26348042946233,4.82276771982976));
#53935=CARTESIAN_POINT('Ctrl Pts',(0.277952495676334,2.26310663308631,4.8227411436195));
#53936=CARTESIAN_POINT('Ctrl Pts',(0.278370111697928,2.26239276880576,4.82269039670057));
#53937=CARTESIAN_POINT('Ctrl Pts',(0.278568173299315,2.26205277927151,4.82266623087303));
#53938=CARTESIAN_POINT('Ctrl Pts',(0.279019188405874,2.26127530346146,4.82261097624568));
#53939=CARTESIAN_POINT('Ctrl Pts',(0.279271736067242,2.26083758402379,4.82257987283894));
#53940=CARTESIAN_POINT('Ctrl Pts',(0.280041894192321,2.2594954513706,4.82248451783246));
#53941=CARTESIAN_POINT('Ctrl Pts',(0.280556144690441,2.25858912682247,4.82242014533502));
#53942=CARTESIAN_POINT('Ctrl Pts',(0.284345061306474,2.25183536390115,4.82194057465915));
#53943=CARTESIAN_POINT('Ctrl Pts',(0.287440797539427,2.24588991967462,4.82151902166383));
#53944=CARTESIAN_POINT('Ctrl Pts',(0.291198620017513,2.23808828514821,4.82096605773868));
#53945=CARTESIAN_POINT('Ctrl Pts',(0.292032343852998,2.23631625243464,4.8208404768697));
#53946=CARTESIAN_POINT('Ctrl Pts',(0.303391096256598,2.21159134502695,4.81908849040367));
#53947=CARTESIAN_POINT('Ctrl Pts',(0.311197726987942,2.18748931346215,4.8173730224208));
#53948=CARTESIAN_POINT('Ctrl Pts',(0.318041263535512,2.15300241744209,4.8149999249504));
#53949=CARTESIAN_POINT('Ctrl Pts',(0.319521535311326,2.14319159989958,4.81433498082942));
#53950=CARTESIAN_POINT('Ctrl Pts',(0.321197690317714,2.12707023000438,4.81327295667407));
#53951=CARTESIAN_POINT('Ctrl Pts',(0.321664965062384,2.12079462817901,4.81286709042574));
#53952=CARTESIAN_POINT('Ctrl Pts',(0.321981371918348,2.11377365039208,4.81242432537052));
#53953=CARTESIAN_POINT('Ctrl Pts',(0.322011988022272,2.11303828601411,4.81237808949803));
#53954=CARTESIAN_POINT('Ctrl Pts',(0.322061679753676,2.1117375487786,4.81229655856279));
#53955=CARTESIAN_POINT('Ctrl Pts',(0.322081786338681,2.11117222169169,4.81226120791357));
#53956=CARTESIAN_POINT('Ctrl Pts',(0.322109531414066,2.11032968042448,4.81220865136003));
#53957=CARTESIAN_POINT('Ctrl Pts',(0.322118300630859,2.11005250842005,4.81219138250199));
#53958=CARTESIAN_POINT('Ctrl Pts',(0.322133135297717,2.10956366095423,4.81216096246701));
#53959=CARTESIAN_POINT('Ctrl Pts',(0.322139349874116,2.10935199076667,4.81214780288536));
#53960=CARTESIAN_POINT('Ctrl Pts',(0.322151364572573,2.10892853925314,4.81212150143145));
#53961=CARTESIAN_POINT('Ctrl Pts',(0.322157164473211,2.10871675905122,4.81210835960547));
#53962=CARTESIAN_POINT('Ctrl Pts',(0.322172430330033,2.10813849845567,4.81207250933764));
#53963=CARTESIAN_POINT('Ctrl Pts',(0.322181479834903,2.1077720059466,4.81204982436566));
#53964=CARTESIAN_POINT('Ctrl Pts',(0.322213438525605,2.10638158367025,4.81196389596481));
#53965=CARTESIAN_POINT('Ctrl Pts',(0.322232092321038,2.10535754809489,4.81190088861712));
#53966=CARTESIAN_POINT('Ctrl Pts',(0.322485255830175,2.08653158537324,4.81074738667012));
#53967=CARTESIAN_POINT('Ctrl Pts',(0.32124911896349,2.06873754545673,4.80973572988078));
#53968=CARTESIAN_POINT('Ctrl Pts',(0.313838026920968,2.02042553719714,4.8069925051278));
#53969=CARTESIAN_POINT('Ctrl Pts',(0.304712742059126,1.99056349005026,4.80528361107469));
#53970=CARTESIAN_POINT('Ctrl Pts',(0.290591778881093,1.96063826586778,4.80328269644488));
#53971=CARTESIAN_POINT('Ctrl Pts',(0.289710533985563,1.95881543603725,4.80315968384702));
#53972=CARTESIAN_POINT('Ctrl Pts',(0.288519695560239,1.95641032271227,4.80299582767971));
#53973=CARTESIAN_POINT('Ctrl Pts',(0.288225393876434,1.95582048528183,4.80295551871572));
#53974=CARTESIAN_POINT('Ctrl Pts',(0.287739218182699,1.95485353268535,4.80288923191766));
#53975=CARTESIAN_POINT('Ctrl Pts',(0.287548406463915,1.95447588312698,4.80286329137894));
#53976=CARTESIAN_POINT('Ctrl Pts',(0.28717720473359,1.95374479096842,4.80281297210186));
#53977=CARTESIAN_POINT('Ctrl Pts',(0.286996904477842,1.95339130344565,4.80278859655356));
#53978=CARTESIAN_POINT('Ctrl Pts',(0.286579069856641,1.95257584259151,4.80273225809954));
#53979=CARTESIAN_POINT('Ctrl Pts',(0.286341070946028,1.95211410969283,4.80270027886447));
#53980=CARTESIAN_POINT('Ctrl Pts',(0.285575090363893,1.95063684031922,4.80259770940755));
#53981=CARTESIAN_POINT('Ctrl Pts',(0.285042818939824,1.94962354897512,4.80252696775815));
#53982=CARTESIAN_POINT('Ctrl Pts',(0.280080937216537,1.94029855970708,4.80187233642857));
#53983=CARTESIAN_POINT('Ctrl Pts',(0.27529477503627,1.93218272322465,4.80127575448553));
#53984=CARTESIAN_POINT('Ctrl Pts',(0.254228450564688,1.89979271928812,4.79877854827676));
#53985=CARTESIAN_POINT('Ctrl Pts',(0.235039651075048,1.87757943941959,4.79676927091829));
#53986=CARTESIAN_POINT('Ctrl Pts',(0.205004019701675,1.85109880084923,4.79409378790848));
#53987=CARTESIAN_POINT('Ctrl Pts',(0.196523941432936,1.8443501457477,4.79338179226732));
#53988=CARTESIAN_POINT('Ctrl Pts',(0.186902877453307,1.83745572055375,4.79263323342299));
#53989=CARTESIAN_POINT('Ctrl Pts',(0.186083784810643,1.83687453684134,4.79256995503804));
#53990=CARTESIAN_POINT('Ctrl Pts',(0.184852203585605,1.83600930083761,4.79247549940798));
#53991=CARTESIAN_POINT('Ctrl Pts',(0.18444175719958,1.83572237207105,4.79244413435826));
#53992=CARTESIAN_POINT('Ctrl Pts',(0.183780242123295,1.83526222168505,4.79239376870911));
#53993=CARTESIAN_POINT('Ctrl Pts',(0.183529595407413,1.83508839913382,4.79237472791721));
#53994=CARTESIAN_POINT('Ctrl Pts',(0.183059261097417,1.83476321197031,4.79233907865184));
#53995=CARTESIAN_POINT('Ctrl Pts',(0.18283963189247,1.8346117639976,4.79232246452709));
#53996=CARTESIAN_POINT('Ctrl Pts',(0.182441750354263,1.83433812833652,4.79229242597892));
#53997=CARTESIAN_POINT('Ctrl Pts',(0.182263562946289,1.83421584706511,4.79227899513823));
#53998=CARTESIAN_POINT('Ctrl Pts',(0.181911687228781,1.83397489230373,4.79225251538646));
#53999=CARTESIAN_POINT('Ctrl Pts',(0.181738006293539,1.83385621002112,4.792239465858));
#54000=CARTESIAN_POINT('Ctrl Pts',(0.181317706356923,1.83356960758188,4.79220793583064));
#54001=CARTESIAN_POINT('Ctrl Pts',(0.181070969573557,1.83340185930513,4.792189467079));
#54002=CARTESIAN_POINT('Ctrl Pts',(0.180157314519947,1.832782548594,4.79212122799425));
#54003=CARTESIAN_POINT('Ctrl Pts',(0.179488929885066,1.83233313915921,4.79207160258001));
#54004=CARTESIAN_POINT('Ctrl Pts',(0.166933218304063,1.82395908937581,4.79114475263217));
#54005=CARTESIAN_POINT('Ctrl Pts',(0.154531818082685,1.81682987901813,4.79031900275228));
#54006=CARTESIAN_POINT('Ctrl Pts',(0.12489229302803,1.8023204021336,4.78845002941961));
#54007=CARTESIAN_POINT('Ctrl Pts',(0.107403620836295,1.79557313929471,4.78742062358528));
#54008=CARTESIAN_POINT('Ctrl Pts',(0.0744499114832903,1.78605502365687,
4.7854756855256));
#54009=CARTESIAN_POINT('Ctrl Pts',(0.0591794655796977,1.78282192188091,
4.78457270493879));
#54010=CARTESIAN_POINT('Ctrl Pts',(0.0412949831052748,1.78037213550469,
4.78348391645955));
#54011=CARTESIAN_POINT('Ctrl Pts',(0.0388499836119388,1.78006574793495,
4.78333443680278));
#54012=CARTESIAN_POINT('Ctrl Pts',(0.035697405382869,1.77970736286322,4.78314081112966));
#54013=CARTESIAN_POINT('Ctrl Pts',(0.0349927906499727,1.77962961631108,
4.7830974781047));
#54014=CARTESIAN_POINT('Ctrl Pts',(0.0338561977097987,1.7795080000561,4.78302748526975));
#54015=CARTESIAN_POINT('Ctrl Pts',(0.0334243746457255,1.77946267716843,
4.78300087128325));
#54016=CARTESIAN_POINT('Ctrl Pts',(0.0326012015240472,1.77937796084627,
4.78295009573004));
#54017=CARTESIAN_POINT('Ctrl Pts',(0.0322098680723235,1.77933841089321,
4.78292593913988));
#54018=CARTESIAN_POINT('Ctrl Pts',(0.0313167529035856,1.7792497999923,4.78287076642416));
#54019=CARTESIAN_POINT('Ctrl Pts',(0.0308149274061844,1.77920120003069,
4.78283973584789));
#54020=CARTESIAN_POINT('Ctrl Pts',(0.0292814555914005,1.77905632028465,
4.78274482018136));
#54021=CARTESIAN_POINT('Ctrl Pts',(0.0282494647856454,1.77896383865685,
4.78268081581378));
#54022=CARTESIAN_POINT('Ctrl Pts',(0.0206681939859864,1.77832128287119,
4.78220965879185));
#54023=CARTESIAN_POINT('Ctrl Pts',(0.0141043110404413,1.77796672617015,
4.78179639903181));
#54024=CARTESIAN_POINT('Ctrl Pts',(0.00703368274073614,1.77780137502898,
4.78134504303566));
#54025=CARTESIAN_POINT('Ctrl Pts',(0.00653279515968749,1.77779083003571,
4.78131303558347));
#54026=CARTESIAN_POINT('Ctrl Pts',(-0.0190737884633688,1.77731147828438,
4.77967504165991));
#54027=CARTESIAN_POINT('Ctrl Pts',(-0.0441447003268799,1.7797773806324,
4.7779777608863));
#54028=CARTESIAN_POINT('Ctrl Pts',(-0.0867273544029329,1.78906413278301,
4.77503097228658));
#54029=CARTESIAN_POINT('Ctrl Pts',(-0.104414975911622,1.79454878027021,
4.77378988504117));
#54030=CARTESIAN_POINT('Ctrl Pts',(-0.122191856685247,1.80178728036398,
4.77258567868829));
#54031=CARTESIAN_POINT('Ctrl Pts',(-0.122846121692588,1.80205620261458,
4.77254142421478));
#54032=CARTESIAN_POINT('Ctrl Pts',(-0.123781282844102,1.80244418555649,
4.77247826926928));
#54033=CARTESIAN_POINT('Ctrl Pts',(-0.124062897676875,1.80256149187852,
4.77245926368818));
#54034=CARTESIAN_POINT('Ctrl Pts',(-0.124549765577342,1.80276510787446,
4.77242642893027));
#54035=CARTESIAN_POINT('Ctrl Pts',(-0.12475509620438,1.8028512305688,4.77241258833444));
#54036=CARTESIAN_POINT('Ctrl Pts',(-0.125150757770159,1.80301766697324,
4.77238593204706));
#54037=CARTESIAN_POINT('Ctrl Pts',(-0.12534110031677,1.80309795071026,4.77237311454903));
#54038=CARTESIAN_POINT('Ctrl Pts',(-0.125793163755688,1.80328913674417,
4.77234268732114));
#54039=CARTESIAN_POINT('Ctrl Pts',(-0.126054815903675,1.80340020261198,
4.77232508760511));
#54040=CARTESIAN_POINT('Ctrl Pts',(-0.126838980215234,1.80373428906069,
4.77227237500421));
#54041=CARTESIAN_POINT('Ctrl Pts',(-0.127361053463563,1.80395834676073,
4.77223732486269));
#54042=CARTESIAN_POINT('Ctrl Pts',(-0.132434029451511,1.8061514146326,4.77189714943663));
#54043=CARTESIAN_POINT('Ctrl Pts',(-0.136939812009465,1.80822395961091,
4.77159819081554));
#54044=CARTESIAN_POINT('Ctrl Pts',(-0.151369038822595,1.81526897803176,
4.77064555783122));
#54045=CARTESIAN_POINT('Ctrl Pts',(-0.161084547826962,1.82065048447673,
4.77001141832463));
#54046=CARTESIAN_POINT('Ctrl Pts',(-0.17818285015979,1.83131070310796,4.76887503486144));
#54047=CARTESIAN_POINT('Ctrl Pts',(-0.185657024213084,1.83641976409258,
4.76837059430449));
#54048=CARTESIAN_POINT('Ctrl Pts',(-0.200010987435166,1.84714541917724,
4.76736856006734));
#54049=CARTESIAN_POINT('Ctrl Pts',(-0.206893265007696,1.8527450632355,4.76687145972178));
#54050=CARTESIAN_POINT('Ctrl Pts',(-0.224731240007123,1.86852542544296,
4.76551830727427));
#54051=CARTESIAN_POINT('Ctrl Pts',(-0.235222832762577,1.87919524049093,
4.76465064307751));
#54052=CARTESIAN_POINT('Ctrl Pts',(-0.2459659922425,1.89175874405818,4.7636532497755));
#54053=CARTESIAN_POINT('Ctrl Pts',(-0.246987604121375,1.89297146745341,
4.76355721978287));
#54054=CARTESIAN_POINT('Ctrl Pts',(-0.248762236370317,1.89510990937155,
4.76338828617161));
#54055=CARTESIAN_POINT('Ctrl Pts',(-0.249519147959675,1.89603236966802,
4.76331554166465));
#54056=CARTESIAN_POINT('Ctrl Pts',(-0.250607453805062,1.89737382927089,
4.76320993133883));
#54057=CARTESIAN_POINT('Ctrl Pts',(-0.250942962845622,1.89778948998671,
4.76317723151798));
#54058=CARTESIAN_POINT('Ctrl Pts',(-0.251526479257595,1.89851609480964,
4.76312011126511));
#54059=CARTESIAN_POINT('Ctrl Pts',(-0.251774947992806,1.89882666831957,
4.76309570941787));
#54060=CARTESIAN_POINT('Ctrl Pts',(-0.25225377927961,1.89942746010993,4.76304852996609));
#54061=CARTESIAN_POINT('Ctrl Pts',(-0.252484217631362,1.89971761743953,
4.76302575544581));
#54062=CARTESIAN_POINT('Ctrl Pts',(-0.253029288393582,1.90040638106119,
4.76297172032097));
#54063=CARTESIAN_POINT('Ctrl Pts',(-0.253343479359646,1.90080533398885,
4.76294044217932));
#54064=CARTESIAN_POINT('Ctrl Pts',(-0.254443992338109,1.90220955720428,
4.7628304213289));
#54065=CARTESIAN_POINT('Ctrl Pts',(-0.255225276624635,1.9032187443009,4.76275147902246));
#54066=CARTESIAN_POINT('Ctrl Pts',(-0.266526580048867,1.91799719448045,
4.76159722340893));
#54067=CARTESIAN_POINT('Ctrl Pts',(-0.27592353813765,1.93258595602232,4.76047766022678));
#54068=CARTESIAN_POINT('Ctrl Pts',(-0.293697794153064,1.96577640500607,
4.75797478464817));
#54069=CARTESIAN_POINT('Ctrl Pts',(-0.301576948587302,1.98456328165682,
4.75658403687646));
#54070=CARTESIAN_POINT('Ctrl Pts',(-0.3101888433781,2.01215023269976,4.75464910060457));
#54071=CARTESIAN_POINT('Ctrl Pts',(-0.312416526892854,2.02043470224888,
4.75408163622111));
#54072=CARTESIAN_POINT('Ctrl Pts',(-0.31525265901204,2.03295454173911,4.75325326273716));
#54073=CARTESIAN_POINT('Ctrl Pts',(-0.316111618806432,2.03712885140085,
4.75298185759566));
#54074=CARTESIAN_POINT('Ctrl Pts',(-0.3169878380855,2.04186060468506,4.75268052334854));
#54075=CARTESIAN_POINT('Ctrl Pts',(-0.317086705653594,2.04240225794249,
4.75264612206017));
#54076=CARTESIAN_POINT('Ctrl Pts',(-0.317232928903758,2.04321514068883,
4.75259463678681));
#54077=CARTESIAN_POINT('Ctrl Pts',(-0.317281325300182,2.04348617828385,
4.75257749387181));
#54078=CARTESIAN_POINT('Ctrl Pts',(-0.317363899786889,2.04395207519724,
4.75254806737087));
#54079=CARTESIAN_POINT('Ctrl Pts',(-0.31739824576466,2.044146903855,4.75253577416445));
#54080=CARTESIAN_POINT('Ctrl Pts',(-0.317469029612501,2.04455060131008,
4.75251032754907));
#54081=CARTESIAN_POINT('Ctrl Pts',(-0.3175054406621,2.0447594738552,4.75249717571326));
#54082=CARTESIAN_POINT('Ctrl Pts',(-0.317604386025712,2.0453304051715,4.75246126499654));
#54083=CARTESIAN_POINT('Ctrl Pts',(-0.317666507592022,2.04569253661826,
4.75243852972371));
#54084=CARTESIAN_POINT('Ctrl Pts',(-0.317900383443802,2.04707002479976,
4.75235220640011));
#54085=CARTESIAN_POINT('Ctrl Pts',(-0.318067892457474,2.04808611049339,
4.75228885722561));
#54086=CARTESIAN_POINT('Ctrl Pts',(-0.320907561612405,2.06584097587976,
4.7511873216208));
#54087=CARTESIAN_POINT('Ctrl Pts',(-0.322260290453718,2.08276679870848,
4.750220556137));
#54088=CARTESIAN_POINT('Ctrl Pts',(-0.32229447047123,2.12248874906482,4.74798769927676));
#54089=CARTESIAN_POINT('Ctrl Pts',(-0.3199017979713,2.14519145954743,4.74673518061688));
#54090=CARTESIAN_POINT('Ctrl Pts',(-0.314698395215594,2.16950171021866,
4.7452914527566));
#54091=CARTESIAN_POINT('Ctrl Pts',(-0.314239786475283,2.17154665620285,
4.74516924563928));
#54092=CARTESIAN_POINT('Ctrl Pts',(-0.313345478981616,2.17535981926996,
4.74493982652879));
#54093=CARTESIAN_POINT('Ctrl Pts',(-0.312914673320171,2.1771291034513,4.74483275304375));
#54094=CARTESIAN_POINT('Ctrl Pts',(-0.310863981700725,2.18525104352628,
4.74433818362047));
#54095=CARTESIAN_POINT('Ctrl Pts',(-0.309065572852634,2.1915566378076,4.74394557163244));
#54096=CARTESIAN_POINT('Ctrl Pts',(-0.306762017828688,2.19878923037657,
4.74348360007954));
#54097=CARTESIAN_POINT('Ctrl Pts',(-0.306443057872553,2.19977424448834,
4.74342043168156));
#54098=CARTESIAN_POINT('Ctrl Pts',(-0.305961779027517,2.20123645311741,
4.74332627989157));
#54099=CARTESIAN_POINT('Ctrl Pts',(-0.305803076107235,2.20171483817156,
4.7432954157721));
#54100=CARTESIAN_POINT('Ctrl Pts',(-0.305518534580197,2.20256585857512,
4.74324040104798));
#54101=CARTESIAN_POINT('Ctrl Pts',(-0.305393134550463,2.20293864038615,
4.74321626497472));
#54102=CARTESIAN_POINT('Ctrl Pts',(-0.305127837524803,2.20372254812007,
4.74316543111873));
#54103=CARTESIAN_POINT('Ctrl Pts',(-0.304987791397928,2.20413362241062,
4.74313872844051));
#54104=CARTESIAN_POINT('Ctrl Pts',(-0.304616837482741,2.20521530775314,
4.74306834254177));
#54105=CARTESIAN_POINT('Ctrl Pts',(-0.304384546993899,2.20588543904636,
4.74302461356063));
#54106=CARTESIAN_POINT('Ctrl Pts',(-0.303334191026098,2.20888357555696,
4.74282841531693));
#54107=CARTESIAN_POINT('Ctrl Pts',(-0.302491634034368,2.21120285637565,
4.74267513409293));
#54108=CARTESIAN_POINT('Ctrl Pts',(-0.296117965925828,2.22813885352821,
4.74154447449076));
#54109=CARTESIAN_POINT('Ctrl Pts',(-0.289557610523375,2.24234351633138,
4.74053220514915));
#54110=CARTESIAN_POINT('Ctrl Pts',(-0.266454111670279,2.28410269655956,
4.73736134912195));
#54111=CARTESIAN_POINT('Ctrl Pts',(-0.24680636084669,2.30970968101141,4.73512042852325));
#54112=CARTESIAN_POINT('Ctrl Pts',(-0.222612535317334,2.33303887158884,
4.73299451931738));
#54113=CARTESIAN_POINT('Ctrl Pts',(-0.221517979475821,2.33407956239844,
4.73289952506346));
#54114=CARTESIAN_POINT('Ctrl Pts',(-0.220104178893503,2.33540498909725,
4.73277838162719));
#54115=CARTESIAN_POINT('Ctrl Pts',(-0.219791650930607,2.33569681509194,
4.73275169888468));
#54116=CARTESIAN_POINT('Ctrl Pts',(-0.219296223276313,2.3361575831369,4.73270955468023));
#54117=CARTESIAN_POINT('Ctrl Pts',(-0.219113708422816,2.33632693540628,
4.73269406174996));
#54118=CARTESIAN_POINT('Ctrl Pts',(-0.218786697378166,2.33662965862673,
4.73266636232387));
#54119=CARTESIAN_POINT('Ctrl Pts',(-0.21864227641429,2.33676310788666,4.73265414979793));
#54120=CARTESIAN_POINT('Ctrl Pts',(-0.21830293274274,2.3370760962415,4.73262550251671));
#54121=CARTESIAN_POINT('Ctrl Pts',(-0.218107910957724,2.33725552687358,
4.73260907614257));
#54122=CARTESIAN_POINT('Ctrl Pts',(-0.21754352502898,2.33777350859236,4.73256164574526));
#54123=CARTESIAN_POINT('Ctrl Pts',(-0.217173590299353,2.33811144104149,
4.73253068890219));
#54124=CARTESIAN_POINT('Ctrl Pts',(-0.214655043948123,2.34040136125284,
4.73232081526259));
#54125=CARTESIAN_POINT('Ctrl Pts',(-0.212480843920028,2.34232518393617,
4.73214399038355));
#54126=CARTESIAN_POINT('Ctrl Pts',(-0.205576265880877,2.34827024933106,
4.73159484729011));
#54127=CARTESIAN_POINT('Ctrl Pts',(-0.200755281736487,2.35218454576287,
4.73122926383669));
#54128=CARTESIAN_POINT('Ctrl Pts',(-0.184258546457667,2.36480561303203,
4.73002521544727));
#54129=CARTESIAN_POINT('Ctrl Pts',(-0.172105993366381,2.37286041799107,
4.72921310604732));
#54130=CARTESIAN_POINT('Ctrl Pts',(-0.136465703089263,2.3931514549812,4.72692080766496));
#54131=CARTESIAN_POINT('Ctrl Pts',(-0.111962445982215,2.40335591723922,
4.72543634664687));
#54132=CARTESIAN_POINT('Ctrl Pts',(-0.0849414614765147,2.4108837508264,
4.72373618032123));
#54133=CARTESIAN_POINT('Ctrl Pts',(-0.0833901321576499,2.41130345985668,
4.72363840181915));
#54134=CARTESIAN_POINT('Ctrl Pts',(-0.0812339868929345,2.41186952732937,
4.72350224756173));
#54135=CARTESIAN_POINT('Ctrl Pts',(-0.0806317708512905,2.41202576852561,
4.72346419191757));
#54136=CARTESIAN_POINT('Ctrl Pts',(-0.0796672802145586,2.41227302094876,
4.72340319793779));
#54137=CARTESIAN_POINT('Ctrl Pts',(-0.0793052911839022,2.41236514840421,
4.72338029572481));
#54138=CARTESIAN_POINT('Ctrl Pts',(-0.0785591904951232,2.41255365306523,
4.72333307033914));
#54139=CARTESIAN_POINT('Ctrl Pts',(-0.0781750598429435,2.41264995197831,
4.72330874468141));
#54140=CARTESIAN_POINT('Ctrl Pts',(-0.0772827692325008,2.41287189585916,
4.72325221159709));
#54141=CARTESIAN_POINT('Ctrl Pts',(-0.0767744797801339,2.41299701098905,
4.72321998714346));
#54142=CARTESIAN_POINT('Ctrl Pts',(-0.0751624768244624,2.41338964158503,
4.72311772293767));
#54143=CARTESIAN_POINT('Ctrl Pts',(-0.0740576621192644,2.41365255937694,
4.72304753532863));
#54144=CARTESIAN_POINT('Ctrl Pts',(-0.0540452197870818,2.41830338047471,
4.72177430657084));
#54145=CARTESIAN_POINT('Ctrl Pts',(-0.0347843170496422,2.42097933122551,
4.72051511248661));
#54146=CARTESIAN_POINT('Ctrl Pts',(0.0145843283142795,2.42334155036074,
4.71721364217749));
#54147=CARTESIAN_POINT('Ctrl Pts',(0.0446242229580015,2.42057947129813,
4.71512719575121));
#54148=CARTESIAN_POINT('Ctrl Pts',(0.075351629882844,2.41334596602037,4.71312983752989));
#54149=CARTESIAN_POINT('Ctrl Pts',(0.0768529593083725,2.41298112629895,
4.71303264223228));
#54150=CARTESIAN_POINT('Ctrl Pts',(0.0787650941151597,2.41250186760287,
4.71290940731139));
#54151=CARTESIAN_POINT('Ctrl Pts',(0.0791783429142083,2.41239741888273,
4.71288280710551));
#54152=CARTESIAN_POINT('Ctrl Pts',(0.0798347677233625,2.41223012117625,
4.71284060817787));
#54153=CARTESIAN_POINT('Ctrl Pts',(0.0800780777510664,2.4121678077123,4.71282497858551));
#54154=CARTESIAN_POINT('Ctrl Pts',(0.080532667481871,2.41205081753032,4.71279579939799));
#54155=CARTESIAN_POINT('Ctrl Pts',(0.0807439629013194,2.41199621104831,
4.71278224588794));
#54156=CARTESIAN_POINT('Ctrl Pts',(0.0812188228869276,2.41187297511796,
4.71275180642207));
#54157=CARTESIAN_POINT('Ctrl Pts',(0.0814823554000284,2.41180422633416,
4.71273492753036));
#54158=CARTESIAN_POINT('Ctrl Pts',(0.0822643721400682,2.41159915935127,
4.71268488134413));
#54159=CARTESIAN_POINT('Ctrl Pts',(0.0827826069644153,2.41146188053434,
4.71265176963212));
#54160=CARTESIAN_POINT('Ctrl Pts',(0.086962590227864,2.41034344612227,4.71238511030734));
#54161=CARTESIAN_POINT('Ctrl Pts',(0.0906073014049481,2.40929899232091,
4.7121551609534));
#54162=CARTESIAN_POINT('Ctrl Pts',(0.10378384929359,2.40527010435142,4.71133034939099));
#54163=CARTESIAN_POINT('Ctrl Pts',(0.113194752466662,2.40190711793694,4.71075368353714));
#54164=CARTESIAN_POINT('Ctrl Pts',(0.151532163623229,2.38616189760132,4.70839939133914));
#54165=CARTESIAN_POINT('Ctrl Pts',(0.178721359323029,2.37001732351581,4.70669857777219));
#54166=CARTESIAN_POINT('Ctrl Pts',(0.20762171962464,2.34655161823008,4.70449235536249));
#54167=CARTESIAN_POINT('Ctrl Pts',(0.212003047743296,2.34279452269041,4.7041459639046));
#54168=CARTESIAN_POINT('Ctrl Pts',(0.21701046944905,2.33826162106833,4.70373476409637));
#54169=CARTESIAN_POINT('Ctrl Pts',(0.217736949909935,2.33759790515667,4.70367471820302));
#54170=CARTESIAN_POINT('Ctrl Pts',(0.218828301502073,2.3365916324509,4.70358392059871));
#54171=CARTESIAN_POINT('Ctrl Pts',(0.219195437626998,2.33625153164183,4.70355327356264));
#54172=CARTESIAN_POINT('Ctrl Pts',(0.219843467654706,2.33564841063624,4.70349899661171));
#54173=CARTESIAN_POINT('Ctrl Pts',(0.220124686106478,2.33538573930958,4.70347538166765));
#54174=CARTESIAN_POINT('Ctrl Pts',(0.220715455426778,2.33483194828122,4.70342564370211));
#54175=CARTESIAN_POINT('Ctrl Pts',(0.221024902104478,2.33454071894824,4.70339951598795));
#54176=CARTESIAN_POINT('Ctrl Pts',(0.221656081702871,2.33394433888966,4.70334606952108));
#54177=CARTESIAN_POINT('Ctrl Pts',(0.221977762518819,2.33363913456095,4.70331874848007));
#54178=CARTESIAN_POINT('Ctrl Pts',(0.222768752800128,2.33288555064095,4.70325136483833));
#54179=CARTESIAN_POINT('Ctrl Pts',(0.22323733803676,2.33243641672047,4.70321126953441));
#54180=CARTESIAN_POINT('Ctrl Pts',(0.224528197274878,2.33119163791149,4.7031003223998));
#54181=CARTESIAN_POINT('Ctrl Pts',(0.22534758975252,2.33039303060238,4.70302934137892));
#54182=CARTESIAN_POINT('Ctrl Pts',(0.232253276749586,2.3235904335203,4.7024263637213));
#54183=CARTESIAN_POINT('Ctrl Pts',(0.238102183101612,2.31735131611586,4.70188396789753));
#54184=CARTESIAN_POINT('Ctrl Pts',(0.24889836449907,2.30487554958358,4.7008180169498));
#54185=CARTESIAN_POINT('Ctrl Pts',(0.253876372178593,2.29867349867532,4.70029617891608));
#54186=CARTESIAN_POINT('Ctrl Pts',(0.277825862088175,2.26646341172295,4.69762991055377));
#54187=CARTESIAN_POINT('Ctrl Pts',(0.293052819310045,2.23790304731271,4.69538241483096));
#54188=CARTESIAN_POINT('Ctrl Pts',(0.304295683437239,2.2061487541136,4.69325189515312));
#54189=CARTESIAN_POINT('Ctrl Pts',(0.304785952355911,2.20473272846598,4.69315765127834));
#54190=CARTESIAN_POINT('Ctrl Pts',(0.305403001215232,2.20290949524154,4.69303733001132));
#54191=CARTESIAN_POINT('Ctrl Pts',(0.305538863947283,2.20250541441762,4.69301072775747));
#54192=CARTESIAN_POINT('Ctrl Pts',(0.305752715163683,2.2018651787608,4.69296868172219));
#54193=CARTESIAN_POINT('Ctrl Pts',(0.305831232171156,2.20162920300588,4.69295320671902));
#54194=CARTESIAN_POINT('Ctrl Pts',(0.305971352977167,2.20120644970894,4.69292552306731));
#54195=CARTESIAN_POINT('Ctrl Pts',(0.30603305850721,2.20101970800992,4.69291330843054));
#54196=CARTESIAN_POINT('Ctrl Pts',(0.306177627519708,2.20058084540187,4.69288463550763));
#54197=CARTESIAN_POINT('Ctrl Pts',(0.306260350424772,2.20032867892214,4.69286818565203));
#54198=CARTESIAN_POINT('Ctrl Pts',(0.306498909342499,2.19959842892441,4.69282062100725));
#54199=CARTESIAN_POINT('Ctrl Pts',(0.30665393894006,2.19912007976689,4.69278955381309));
#54200=CARTESIAN_POINT('Ctrl Pts',(0.307708205853703,2.19584095481054,4.6925771886934));
#54201=CARTESIAN_POINT('Ctrl Pts',(0.30857021693016,2.19302822832906,4.69239803991428));
#54202=CARTESIAN_POINT('Ctrl Pts',(0.311153591107174,2.18416742683443,4.69184193452161));
#54203=CARTESIAN_POINT('Ctrl Pts',(0.312736629787916,2.17808024210419,4.69147187046152));
#54204=CARTESIAN_POINT('Ctrl Pts',(0.317590849055811,2.15688632271318,4.69021227830414));
#54205=CARTESIAN_POINT('Ctrl Pts',(0.319953291456941,2.14159273671054,4.68935269184683));
#54206=CARTESIAN_POINT('Ctrl Pts',(0.323285875256329,2.10071660916601,4.68705991796746));
#54207=CARTESIAN_POINT('Ctrl Pts',(0.322325396691778,2.07509317366343,4.68562001907203));
#54208=CARTESIAN_POINT('Ctrl Pts',(0.318113695042522,2.04835551336149,4.68397845132261));
#54209=CARTESIAN_POINT('Ctrl Pts',(0.317867126552376,2.04685900162257,4.68388613893577));
#54210=CARTESIAN_POINT('Ctrl Pts',(0.317517356945999,2.04482570949266,4.68376010711967));
#54211=CARTESIAN_POINT('Ctrl Pts',(0.317423337497217,2.04428735241179,4.68372667943307));
#54212=CARTESIAN_POINT('Ctrl Pts',(0.317261459833271,2.04337415040534,4.68366987728087));
#54213=CARTESIAN_POINT('Ctrl Pts',(0.317194305312372,2.0429991805915,4.68364652522996));
#54214=CARTESIAN_POINT('Ctrl Pts',(0.317057959777484,2.04224557227749,4.68359953492941));
#54215=CARTESIAN_POINT('Ctrl Pts',(0.316988754933454,2.04186693691577,4.68357589627299));
#54216=CARTESIAN_POINT('Ctrl Pts',(0.316830292203949,2.04100864807557,4.68352224535904));
#54217=CARTESIAN_POINT('Ctrl Pts',(0.316740623250193,2.04052907232254,4.68349222004913));
#54218=CARTESIAN_POINT('Ctrl Pts',(0.316551036549072,2.03952769939121,4.68342942617512));
#54219=CARTESIAN_POINT('Ctrl Pts',(0.316450916901234,2.03900594235374,4.68339665124279));
#54220=CARTESIAN_POINT('Ctrl Pts',(0.316185721577719,2.03764215070368,4.68331083319887));
#54221=CARTESIAN_POINT('Ctrl Pts',(0.316018573161058,2.03680052774827,4.68325772399474));
#54222=CARTESIAN_POINT('Ctrl Pts',(0.315513609655335,2.03431004175316,4.68310011901254));
#54223=CARTESIAN_POINT('Ctrl Pts',(0.315166240409126,2.03266316590817,4.68299531862604));
#54224=CARTESIAN_POINT('Ctrl Pts',(0.312969347932007,2.02263727424979,4.68235369661809));
#54225=CARTESIAN_POINT('Ctrl Pts',(0.310798841185253,2.01433284144608,4.68180666570732));
#54226=CARTESIAN_POINT('Ctrl Pts',(0.304088306439989,1.99229431219967,4.68031177326691));
#54227=CARTESIAN_POINT('Ctrl Pts',(0.298951291259274,1.97876361516742,4.67934705270825));
#54228=CARTESIAN_POINT('Ctrl Pts',(0.282631438468832,1.94318806109096,4.67670590825821));
#54229=CARTESIAN_POINT('Ctrl Pts',(0.26979444527191,1.92200651886549,4.67501311919923));
#54230=CARTESIAN_POINT('Ctrl Pts',(0.253807897984132,1.90139315664724,4.67336477728538));
#54231=CARTESIAN_POINT('Ctrl Pts',(0.25294455753177,1.90029477150287,4.67327696293238));
#54232=CARTESIAN_POINT('Ctrl Pts',(0.251815549208849,1.89887745781029,4.67316371214626));
#54233=CARTESIAN_POINT('Ctrl Pts',(0.251556386683429,1.89855340131047,4.67313782253891));
#54234=CARTESIAN_POINT('Ctrl Pts',(0.251157867475305,1.89805706169818,4.67309817650121));
#54235=CARTESIAN_POINT('Ctrl Pts',(0.251018959006343,1.89788442181567,4.6730843879994));
#54236=CARTESIAN_POINT('Ctrl Pts',(0.250743084396651,1.89754227912291,4.67305706461617));
#54237=CARTESIAN_POINT('Ctrl Pts',(0.250606125232967,1.89737277302457,4.67304352945788));
#54238=CARTESIAN_POINT('Ctrl Pts',(0.250300828460356,1.89699570863196,4.67301342397207));
#54239=CARTESIAN_POINT('Ctrl Pts',(0.250132405010795,1.89678822128987,4.67299686001929));
#54240=CARTESIAN_POINT('Ctrl Pts',(0.249640806380492,1.89618413912813,4.67294864107108));
#54241=CARTESIAN_POINT('Ctrl Pts',(0.24931694279469,1.89578810172452,4.67291703571754));
#54242=CARTESIAN_POINT('Ctrl Pts',(0.246998859199979,1.8929671615086,4.67269195038114));
#54243=CARTESIAN_POINT('Ctrl Pts',(0.244970153439424,1.89057063633793,4.67250092433542));
#54244=CARTESIAN_POINT('Ctrl Pts',(0.240124849356564,1.88501360590962,4.6720573931713));
#54245=CARTESIAN_POINT('Ctrl Pts',(0.237280316945324,1.8818781359135,4.67180667961306));
#54246=CARTESIAN_POINT('Ctrl Pts',(0.224836253359085,1.86869293375816,4.67074576451726));
#54247=CARTESIAN_POINT('Ctrl Pts',(0.214653291626464,1.85921311260342,4.6699655944049));
#54248=CARTESIAN_POINT('Ctrl Pts',(0.189962177871301,1.83904222265235,4.66818205537132));
#54249=CARTESIAN_POINT('Ctrl Pts',(0.175107478445908,1.82885075209964,4.66718238465805));
#54250=CARTESIAN_POINT('Ctrl Pts',(0.149540783323748,1.81429107839264,4.66548187218267));
#54251=CARTESIAN_POINT('Ctrl Pts',(0.139307003016006,1.80916405371986,4.66480640465326));
#54252=CARTESIAN_POINT('Ctrl Pts',(0.127722463865901,1.804112200744,4.66403815130503));
#54253=CARTESIAN_POINT('Ctrl Pts',(0.126619117153392,1.80363836848408,4.6639649499326));
#54254=CARTESIAN_POINT('Ctrl Pts',(0.125069213822046,1.80298299761466,4.66386207025725));
#54255=CARTESIAN_POINT('Ctrl Pts',(0.124624849307177,1.802796273773,4.66383256826626));
#54256=CARTESIAN_POINT('Ctrl Pts',(0.123814248011677,1.8024577932902,4.66377873985155));
#54257=CARTESIAN_POINT('Ctrl Pts',(0.123448146313705,1.80230571393808,4.66375442442804));
#54258=CARTESIAN_POINT('Ctrl Pts',(0.122711693234474,1.8020013820337,4.66370550240214));
#54259=CARTESIAN_POINT('Ctrl Pts',(0.122341336872543,1.80184914345883,4.66368089537897));
#54260=CARTESIAN_POINT('Ctrl Pts',(0.121439686066852,1.8014804740226,4.6636209768788));
#54261=CARTESIAN_POINT('Ctrl Pts',(0.120908097023008,1.80126477139569,4.66358564085488));
#54262=CARTESIAN_POINT('Ctrl Pts',(0.119772473233747,1.80080749759525,4.66351013132357));
#54263=CARTESIAN_POINT('Ctrl Pts',(0.119168278073462,1.80056633400566,4.66346994422556));
#54264=CARTESIAN_POINT('Ctrl Pts',(0.117496005380549,1.79990471193144,4.66335867722148));
#54265=CARTESIAN_POINT('Ctrl Pts',(0.116426413159749,1.79948813090781,4.66328746718483));
#54266=CARTESIAN_POINT('Ctrl Pts',(0.113023060331444,1.7981835019318,4.6630607340252));
#54267=CARTESIAN_POINT('Ctrl Pts',(0.110681237370315,1.79731687559112,4.66290449843538));
#54268=CARTESIAN_POINT('Ctrl Pts',(0.100986540465924,1.79385675916467,4.66225668070163));
#54269=CARTESIAN_POINT('Ctrl Pts',(0.093551312552428,1.79150348360915,4.66175732456876));
#54270=CARTESIAN_POINT('Ctrl Pts',(0.0715980601253098,1.78542183067228,
4.66027533106316));
#54271=CARTESIAN_POINT('Ctrl Pts',(0.0568975592974022,1.78243379874549,
4.65927250163564));
#54272=CARTESIAN_POINT('Ctrl Pts',(0.0220662687796256,1.77785053960165,
4.65689884413128));
#54273=CARTESIAN_POINT('Ctrl Pts',(0.00188482287959766,1.77710102166971,
4.65552432948218));
#54274=CARTESIAN_POINT('Ctrl Pts',(-0.0193298806421376,1.77830335269784,
4.65415121043592));
#54275=CARTESIAN_POINT('Ctrl Pts',(-0.0204239669655363,1.77837096086944,
4.65408060692298));
#54276=CARTESIAN_POINT('Ctrl Pts',(-0.0248880044125756,1.77866968293866,
4.6537934517719));
#54277=CARTESIAN_POINT('Ctrl Pts',(-0.0282547203627233,1.77894819975883,
4.6535790181372));
#54278=CARTESIAN_POINT('Ctrl Pts',(-0.0321783322720964,1.77933498916711,
4.65333209109713));
#54279=CARTESIAN_POINT('Ctrl Pts',(-0.0327399281691189,1.7793918414088,
4.65329681918501));
#54280=CARTESIAN_POINT('Ctrl Pts',(-0.0335780185733662,1.7794789091958,
4.65324429105903));
#54281=CARTESIAN_POINT('Ctrl Pts',(-0.0338546242406436,1.77950800727545,
4.65322697233886));
#54282=CARTESIAN_POINT('Ctrl Pts',(-0.03434871986902,1.77956063144022,4.65319606846604));
#54283=CARTESIAN_POINT('Ctrl Pts',(-0.0345662233157622,1.77958402086294,
4.65318247560642));
#54284=CARTESIAN_POINT('Ctrl Pts',(-0.0350295433034604,1.77963432164187,
4.65315354438992));
#54285=CARTESIAN_POINT('Ctrl Pts',(-0.0352753520119601,1.77966129438462,
4.65313820959209));
#54286=CARTESIAN_POINT('Ctrl Pts',(-0.0359385536488279,1.77973484052807,
4.65309687371149));
#54287=CARTESIAN_POINT('Ctrl Pts',(-0.0363558887958978,1.77978194716013,
4.6530709027797));
#54288=CARTESIAN_POINT('Ctrl Pts',(-0.0383975142120484,1.78001643800371,
4.65294404529832));
#54289=CARTESIAN_POINT('Ctrl Pts',(-0.0400204918343865,1.78021537006362,
4.65284380076537));
#54290=CARTESIAN_POINT('Ctrl Pts',(-0.049325616557849,1.78142787200496,
4.65227214793176));
#54291=CARTESIAN_POINT('Ctrl Pts',(-0.0569713964816663,1.78270597476258,
4.6518145057367));
#54292=CARTESIAN_POINT('Ctrl Pts',(-0.0812282180897502,1.78766612484256,
4.65038024451293));
#54293=CARTESIAN_POINT('Ctrl Pts',(-0.0975973483235727,1.7923877288741,
4.64943805181323));
#54294=CARTESIAN_POINT('Ctrl Pts',(-0.122024625474658,1.80158120715939,
4.64797754801995));
#54295=CARTESIAN_POINT('Ctrl Pts',(-0.130391599172382,1.8051410389746,4.64746710085284));
#54296=CARTESIAN_POINT('Ctrl Pts',(-0.15237497237863,1.81561300539085,4.64607882133509));
#54297=CARTESIAN_POINT('Ctrl Pts',(-0.165667816522649,1.82314593541205,
4.64518785555756));
#54298=CARTESIAN_POINT('Ctrl Pts',(-0.17941734706603,1.83228344354583,4.64418482875963));
#54299=CARTESIAN_POINT('Ctrl Pts',(-0.18045466953299,1.83298155269204,4.64410863651903));
#54300=CARTESIAN_POINT('Ctrl Pts',(-0.181903857228763,1.83396914514694,
4.64400145070112));
#54301=CARTESIAN_POINT('Ctrl Pts',(-0.182319155955958,1.83425359009852,
4.64397064804889));
#54302=CARTESIAN_POINT('Ctrl Pts',(-0.183038048838936,1.83474845005943,
4.64391717769331));
#54303=CARTESIAN_POINT('Ctrl Pts',(-0.183341951638912,1.8349584167795,4.64389452706873));
#54304=CARTESIAN_POINT('Ctrl Pts',(-0.18396641346124,1.83539144598389,4.64384788783974));
#54305=CARTESIAN_POINT('Ctrl Pts',(-0.184286929253606,1.83561456953063,
4.64382389692861));
#54306=CARTESIAN_POINT('Ctrl Pts',(-0.185035784543128,1.83613790029041,
4.64376772094007));
#54307=CARTESIAN_POINT('Ctrl Pts',(-0.185463799363721,1.83643856817608,
4.64373551826451));
#54308=CARTESIAN_POINT('Ctrl Pts',(-0.186364826648522,1.83707479513318,
4.64366752627649));
#54309=CARTESIAN_POINT('Ctrl Pts',(-0.186837668654765,1.83741059135866,
4.64363172791377));
#54310=CARTESIAN_POINT('Ctrl Pts',(-0.188102954524015,1.83831430184366,
4.64353561749699));
#54311=CARTESIAN_POINT('Ctrl Pts',(-0.188893727364413,1.83888453540806,
4.64347521605263));
#54312=CARTESIAN_POINT('Ctrl Pts',(-0.191300675919869,1.8406368638681,4.64329033370659));
#54313=CARTESIAN_POINT('Ctrl Pts',(-0.192908409267721,1.84183042329919,
4.64316540885032));
#54314=CARTESIAN_POINT('Ctrl Pts',(-0.218547981896928,1.86123811387354,
4.64114973258302));
#54315=CARTESIAN_POINT('Ctrl Pts',(-0.239913090764258,1.88271828066298,
4.63911568429291));
#54316=CARTESIAN_POINT('Ctrl Pts',(-0.266864060205434,1.91871410395949,
4.63607667084967));
#54317=CARTESIAN_POINT('Ctrl Pts',(-0.274921624118765,1.93118296334252,
4.63508149240349));
#54318=CARTESIAN_POINT('Ctrl Pts',(-0.283702852571273,1.94707858855951,
4.63391632864756));
#54319=CARTESIAN_POINT('Ctrl Pts',(-0.28526802820553,1.95001859827816,4.63370495753369));
#54320=CARTESIAN_POINT('Ctrl Pts',(-0.287040612557722,1.95347638274788,
4.63346160636504));
#54321=CARTESIAN_POINT('Ctrl Pts',(-0.287292530313309,1.95397094225035,
4.63342692424446));
#54322=CARTESIAN_POINT('Ctrl Pts',(-0.287669637322058,1.95471602353945,
4.63337486265846));
#54323=CARTESIAN_POINT('Ctrl Pts',(-0.287795778063445,1.95496605851223,
4.63335742372047));
#54324=CARTESIAN_POINT('Ctrl Pts',(-0.28801996285247,1.95541187957668,4.63332638677494));
#54325=CARTESIAN_POINT('Ctrl Pts',(-0.288118133220805,1.95560760103276,
4.63331278079689));
#54326=CARTESIAN_POINT('Ctrl Pts',(-0.288326224425396,1.95602352794442,
4.63328390862952));
#54327=CARTESIAN_POINT('Ctrl Pts',(-0.288436092189978,1.9562437586742,4.63326864582177));
#54328=CARTESIAN_POINT('Ctrl Pts',(-0.288730431567737,1.956835459939,4.63322770477675));
#54329=CARTESIAN_POINT('Ctrl Pts',(-0.288914439332306,1.95720716266549,
4.63320205570511));
#54330=CARTESIAN_POINT('Ctrl Pts',(-0.289794484686172,1.95899355309227,
4.63307911712227));
#54331=CARTESIAN_POINT('Ctrl Pts',(-0.2904808675845,1.96041301196285,4.63298242273095));
#54332=CARTESIAN_POINT('Ctrl Pts',(-0.296113634762158,1.97228322572427,
4.6321815850503));
#54333=CARTESIAN_POINT('Ctrl Pts',(-0.300505323576294,1.98298943380868,
4.63150912491742));
#54334=CARTESIAN_POINT('Ctrl Pts',(-0.316198905427581,2.02800535365237,
4.62879278800612));
#54335=CARTESIAN_POINT('Ctrl Pts',(-0.322270110159706,2.06385104911035,
4.62685414642446));
#54336=CARTESIAN_POINT('Ctrl Pts',(-0.322274997047983,2.09995637979558,
4.62467682828221));
#54337=CARTESIAN_POINT('',(-0.322274981579892,2.09989103817067,4.37437734492394));
#54338=CARTESIAN_POINT('Ctrl Pts',(-0.322274997069199,2.09995653682505,
4.62467681881261));
#54339=CARTESIAN_POINT('Ctrl Pts',(-0.322275187530063,2.10136878465242,
4.62459165372713));
#54340=CARTESIAN_POINT('Ctrl Pts',(-0.32226609503044,2.10278100557306,4.62450620683319));
#54341=CARTESIAN_POINT('Ctrl Pts',(-0.322232983422061,2.10532569039139,
4.62435170814883));
#54342=CARTESIAN_POINT('Ctrl Pts',(-0.32221227553972,2.10645817494858,4.62428276038247));
#54343=CARTESIAN_POINT('Ctrl Pts',(-0.322173630227217,2.10809850660617,
4.62418261114945));
#54344=CARTESIAN_POINT('Ctrl Pts',(-0.322160460884536,2.10860646623495,
4.6241515587642));
#54345=CARTESIAN_POINT('Ctrl Pts',(-0.322135120840432,2.10950210443448,
4.62409673688665));
#54346=CARTESIAN_POINT('Ctrl Pts',(-0.322123451457929,2.10988979708164,
4.62407298312027));
#54347=CARTESIAN_POINT('Ctrl Pts',(-0.322099172786788,2.11065072674517,
4.62402631543877));
#54348=CARTESIAN_POINT('Ctrl Pts',(-0.322086614572444,2.11102396487159,
4.62400340315945));
#54349=CARTESIAN_POINT('Ctrl Pts',(-0.322060358722216,2.11176593015203,
4.62395781214256));
#54350=CARTESIAN_POINT('Ctrl Pts',(-0.322046676527055,2.11213465733939,
4.6239351339217));
#54351=CARTESIAN_POINT('Ctrl Pts',(-0.322012892473588,2.11300478819637,
4.62388156669676));
#54352=CARTESIAN_POINT('Ctrl Pts',(-0.321992252750884,2.11350616892771,
4.62385066087302));
#54353=CARTESIAN_POINT('Ctrl Pts',(-0.321916489087427,2.11524764065199,
4.62374317488986));
#54354=CARTESIAN_POINT('Ctrl Pts',(-0.321855371998147,2.11648744791126,
4.62366640705546));
#54355=CARTESIAN_POINT('Ctrl Pts',(-0.321651256538203,2.12019265743169,
4.62343623491896));
#54356=CARTESIAN_POINT('Ctrl Pts',(-0.321487083791414,2.12265675738753,
4.62328216975928));
#54357=CARTESIAN_POINT('Ctrl Pts',(-0.318546131365999,2.16027467452957,
4.62091450096085));
#54358=CARTESIAN_POINT('Ctrl Pts',(-0.310045951090214,2.19473598291975,
4.61849722897432));
#54359=CARTESIAN_POINT('Ctrl Pts',(-0.29159527079729,2.2377182288673,4.61536523362758));
#54360=CARTESIAN_POINT('Ctrl Pts',(-0.286481409072725,2.24806274287713,
4.61460517481756));
#54361=CARTESIAN_POINT('Ctrl Pts',(-0.28005108146272,2.25948368493022,4.61377588403408));
#54362=CARTESIAN_POINT('Ctrl Pts',(-0.279268660410145,2.26084983537447,
4.61367685685382));
#54363=CARTESIAN_POINT('Ctrl Pts',(-0.278267592175472,2.26256843055088,
4.61355255255379));
#54364=CARTESIAN_POINT('Ctrl Pts',(-0.27805825091827,2.26292623044731,4.61352668813877));
#54365=CARTESIAN_POINT('Ctrl Pts',(-0.277723546463401,2.2634957733816,4.61348554238852));
#54366=CARTESIAN_POINT('Ctrl Pts',(-0.277598631012643,2.26370777695252,
4.61347023205442));
#54367=CARTESIAN_POINT('Ctrl Pts',(-0.277362094851295,2.26410817138233,
4.61344132741317));
#54368=CARTESIAN_POINT('Ctrl Pts',(-0.277250525864528,2.2642965899917,4.61342772995435));
#54369=CARTESIAN_POINT('Ctrl Pts',(-0.276995786057336,2.26472579824611,
4.61339676581713));
#54370=CARTESIAN_POINT('Ctrl Pts',(-0.27685249350869,2.26496651460459,4.61337940724632));
#54371=CARTESIAN_POINT('Ctrl Pts',(-0.276424168679889,2.26568392521232,
4.61332769407639));
#54372=CARTESIAN_POINT('Ctrl Pts',(-0.276138215920658,2.26616007289104,
4.61329339937088));
#54373=CARTESIAN_POINT('Ctrl Pts',(-0.274125147743464,2.26949253799383,
4.61305355308458));
#54374=CARTESIAN_POINT('Ctrl Pts',(-0.272354899408359,2.27232274355462,
4.61285076224998));
#54375=CARTESIAN_POINT('Ctrl Pts',(-0.262479003959397,2.28757946177137,
4.61175965348516));
#54376=CARTESIAN_POINT('Ctrl Pts',(-0.253565700416985,2.29946383299502,
4.61091687257788));
#54377=CARTESIAN_POINT('Ctrl Pts',(-0.224126862767211,2.33353750605077,
4.60838825886458));
#54378=CARTESIAN_POINT('Ctrl Pts',(-0.201280413452453,2.35349289627581,
4.60672957473035));
#54379=CARTESIAN_POINT('Ctrl Pts',(-0.174341401341979,2.37105374395786,
4.6047957642201));
#54380=CARTESIAN_POINT('Ctrl Pts',(-0.172681322207265,2.37211434551246,
4.60467675632164));
#54381=CARTESIAN_POINT('Ctrl Pts',(-0.17019517415967,2.37367079901421,4.6044987185447));
#54382=CARTESIAN_POINT('Ctrl Pts',(-0.169376416229719,2.37417828713108,
4.60444011605323));
#54383=CARTESIAN_POINT('Ctrl Pts',(-0.16806520488208,2.37498289639412,4.6043463091766));
#54384=CARTESIAN_POINT('Ctrl Pts',(-0.167574205708521,2.37528238587998,
4.60431119159643));
#54385=CARTESIAN_POINT('Ctrl Pts',(-0.166638219094032,2.37584986749199,
4.60424426419851));
#54386=CARTESIAN_POINT('Ctrl Pts',(-0.166193379814277,2.37611810146945,
4.60421246334414));
#54387=CARTESIAN_POINT('Ctrl Pts',(-0.165413510654871,2.37658578803669,
4.60415672354022));
#54388=CARTESIAN_POINT('Ctrl Pts',(-0.165078762823075,2.37678571081919,
4.60413280181023));
#54389=CARTESIAN_POINT('Ctrl Pts',(-0.164425417875467,2.3771743037915,4.6040861195305));
#54390=CARTESIAN_POINT('Ctrl Pts',(-0.164106856655065,2.37736303344685,
4.60406336119257));
#54391=CARTESIAN_POINT('Ctrl Pts',(-0.163351497476454,2.37780878450867,
4.60400940486667));
#54392=CARTESIAN_POINT('Ctrl Pts',(-0.162914418063582,2.37806532480751,
4.60397818946346));
#54393=CARTESIAN_POINT('Ctrl Pts',(-0.161379668751497,2.37896127305236,
4.60386859936239));
#54394=CARTESIAN_POINT('Ctrl Pts',(-0.160278835930207,2.37959521460155,
4.6037900271237));
#54395=CARTESIAN_POINT('Ctrl Pts',(-0.144586359620438,2.38850898051737,
4.60267037159344));
#54396=CARTESIAN_POINT('Ctrl Pts',(-0.12937612332373,2.39564218873458,4.60158790867995));
#54397=CARTESIAN_POINT('Ctrl Pts',(-0.106102971298018,2.40441573548338,
4.59993711829214));
#54398=CARTESIAN_POINT('Ctrl Pts',(-0.0984192432931792,2.40698603034381,
4.59939331988942));
#54399=CARTESIAN_POINT('Ctrl Pts',(-0.0805222913351933,2.41223173500415,
4.59813452148875));
#54400=CARTESIAN_POINT('Ctrl Pts',(-0.0702577968750717,2.41470039527728,
4.59741815471573));
#54401=CARTESIAN_POINT('Ctrl Pts',(-0.0456798702669214,2.41934886356838,
4.59573493947132));
#54402=CARTESIAN_POINT('Ctrl Pts',(-0.0313022276549956,2.42107729352348,
4.59477528233938));
#54403=CARTESIAN_POINT('Ctrl Pts',(-0.0158851986191007,2.42188473097346,
4.59380395953406));
#54404=CARTESIAN_POINT('Ctrl Pts',(-0.0149147208572632,2.42193115836829,
4.59374306185069));
#54405=CARTESIAN_POINT('Ctrl Pts',(-0.013597795183024,2.42198819185932,
4.59366077112828));
#54406=CARTESIAN_POINT('Ctrl Pts',(-0.0132515311714041,2.42200262833551,
4.59363916663381));
#54407=CARTESIAN_POINT('Ctrl Pts',(-0.0126744555465138,2.42202575541378,
4.59360321600057));
#54408=CARTESIAN_POINT('Ctrl Pts',(-0.012443657731343,2.42203475644143,
4.59358885240479));
#54409=CARTESIAN_POINT('Ctrl Pts',(-0.0119906035835674,2.42205193760481,
4.59356068578388));
#54410=CARTESIAN_POINT('Ctrl Pts',(-0.0117683485032361,2.42206013578722,
4.5935468817782));
#54411=CARTESIAN_POINT('Ctrl Pts',(-0.0112795133407785,2.4220776604413,
4.59351655061084));
#54412=CARTESIAN_POINT('Ctrl Pts',(-0.0110129292292425,2.42208688605334,
4.59350002914122));
#54413=CARTESIAN_POINT('Ctrl Pts',(-0.0100878985711194,2.42211774857295,
4.5934427673555));
#54414=CARTESIAN_POINT('Ctrl Pts',(-0.00942939163363354,2.42213769763063,
4.59340212134454));
#54415=CARTESIAN_POINT('Ctrl Pts',(-0.00293933082998487,2.42231439224278,
4.59300264061024));
#54416=CARTESIAN_POINT('Ctrl Pts',(0.00289584677027582,2.42231480201296,
4.5926523374891));
#54417=CARTESIAN_POINT('Ctrl Pts',(0.0377133692223503,2.42137148476953,
4.59059807276249));
#54418=CARTESIAN_POINT('Ctrl Pts',(0.0664627189404521,2.41667813564588,
4.58903984646069));
#54419=CARTESIAN_POINT('Ctrl Pts',(0.101267702356863,2.40604029852649,4.58696676273227));
#54420=CARTESIAN_POINT('Ctrl Pts',(0.108259755867507,2.40363732871762,4.58654103316248));
#54421=CARTESIAN_POINT('Ctrl Pts',(0.120500130013859,2.39895409747222,4.58577381460868));
#54422=CARTESIAN_POINT('Ctrl Pts',(0.125782010324904,2.39677047322707,4.58543527649251));
#54423=CARTESIAN_POINT('Ctrl Pts',(0.132939740478171,2.39358592488311,4.58496475094986));
#54424=CARTESIAN_POINT('Ctrl Pts',(0.134868069820154,2.39270509613726,4.58483679810572));
#54425=CARTESIAN_POINT('Ctrl Pts',(0.137708281537022,2.39137371001142,4.58464650784085));
#54426=CARTESIAN_POINT('Ctrl Pts',(0.138626972506996,2.39093774616984,4.584584670991));
#54427=CARTESIAN_POINT('Ctrl Pts',(0.140081926274201,2.39023884345766,4.58448627741105));
#54428=CARTESIAN_POINT('Ctrl Pts',(0.140619553124763,2.38997874679325,4.58444981912336));
#54429=CARTESIAN_POINT('Ctrl Pts',(0.141637797910818,2.38948263596219,4.58438057640223));
#54430=CARTESIAN_POINT('Ctrl Pts',(0.142118557249825,2.38924691528244,4.58434780225779));
#54431=CARTESIAN_POINT('Ctrl Pts',(0.142950862924263,2.38883625223199,4.58429092024555));
#54432=CARTESIAN_POINT('Ctrl Pts',(0.143302682127653,2.38866186292447,4.58426683174087));
#54433=CARTESIAN_POINT('Ctrl Pts',(0.14398216390915,2.38832350987764,4.58422022273971));
#54434=CARTESIAN_POINT('Ctrl Pts',(0.14430986749189,2.38815962939814,4.58419770518633));
#54435=CARTESIAN_POINT('Ctrl Pts',(0.145076569375989,2.38777457545933,4.58414493149331));
#54436=CARTESIAN_POINT('Ctrl Pts',(0.145515341620354,2.38755295618641,4.58411465973887));
#54437=CARTESIAN_POINT('Ctrl Pts',(0.147031208403229,2.38678294970945,4.58400983302295));
#54438=CARTESIAN_POINT('Ctrl Pts',(0.148105713754767,2.3862295127654,4.58393510054501));
#54439=CARTESIAN_POINT('Ctrl Pts',(0.160238942053434,2.37989353379258,4.58308632162054));
#54440=CARTESIAN_POINT('Ctrl Pts',(0.170954556217832,2.37348012732697,4.58228975546083));
#54441=CARTESIAN_POINT('Ctrl Pts',(0.194569085765799,2.35741551657576,4.58042121090629));
#54442=CARTESIAN_POINT('Ctrl Pts',(0.207170680760043,2.34738653331393,4.57933814398522));
#54443=CARTESIAN_POINT('Ctrl Pts',(0.223237535552025,2.33250808194978,4.57785638931334));
#54444=CARTESIAN_POINT('Ctrl Pts',(0.227397372423332,2.32844133047175,4.57746259728413));
#54445=CARTESIAN_POINT('Ctrl Pts',(0.234344543051893,2.32127171913313,4.5767894830817));
#54446=CARTESIAN_POINT('Ctrl Pts',(0.237185938327672,2.31822321284495,4.57650943546035));
#54447=CARTESIAN_POINT('Ctrl Pts',(0.247158038847169,2.30709930416308,4.57551141629466));
#54448=CARTESIAN_POINT('Ctrl Pts',(0.253942762687946,2.29872177298631,4.57480334133327));
#54449=CARTESIAN_POINT('Ctrl Pts',(0.261189986599597,2.28879424474817,4.5740260321682));
#54450=CARTESIAN_POINT('Ctrl Pts',(0.262075612528277,2.28756292139651,4.57393065804701));
#54451=CARTESIAN_POINT('Ctrl Pts',(0.263189102947726,2.28599150287744,4.5738102988537));
#54452=CARTESIAN_POINT('Ctrl Pts',(0.26342503834332,2.28565719008773,4.57378477035259));
#54453=CARTESIAN_POINT('Ctrl Pts',(0.263801145807956,2.2851220976922,4.57374403487827));
#54454=CARTESIAN_POINT('Ctrl Pts',(0.263941725881553,2.28492160750756,4.57372879989495));
#54455=CARTESIAN_POINT('Ctrl Pts',(0.264207721919452,2.28454133237403,4.57369995646709));
#54456=CARTESIAN_POINT('Ctrl Pts',(0.264333181912522,2.28436158118365,4.57368634505427));
#54457=CARTESIAN_POINT('Ctrl Pts',(0.26461973645995,2.28395013002444,4.57365523971034));
#54458=CARTESIAN_POINT('Ctrl Pts',(0.264780709897111,2.28371834673756,4.57363775416373));
#54459=CARTESIAN_POINT('Ctrl Pts',(0.265274374010635,2.28300553049639,4.57358409266247));
#54460=CARTESIAN_POINT('Ctrl Pts',(0.265606062165876,2.28252379968764,4.57354798503256));
#54461=CARTESIAN_POINT('Ctrl Pts',(0.268084063511809,2.27890378956677,4.57327780876737));
#54462=CARTESIAN_POINT('Ctrl Pts',(0.270176114122937,2.27572848792521,4.57304733335643));
#54463=CARTESIAN_POINT('Ctrl Pts',(0.285609168738636,2.25137690133295,4.57132259907083));
#54464=CARTESIAN_POINT('Ctrl Pts',(0.296500475998486,2.22874542623796,4.56995645758664));
#54465=CARTESIAN_POINT('Ctrl Pts',(0.311093954214909,2.18643339276941,4.56744356382087));
#54466=CARTESIAN_POINT('Ctrl Pts',(0.315798718087328,2.16723981550127,4.56631753744043));
#54467=CARTESIAN_POINT('Ctrl Pts',(0.318992085717201,2.14591956323552,4.56501967609921));
#54468=CARTESIAN_POINT('Ctrl Pts',(0.319248899449333,2.1440987190766,4.56490849628523));
#54469=CARTESIAN_POINT('Ctrl Pts',(0.31961022762356,2.14136806075941,4.56474122114416));
#54470=CARTESIAN_POINT('Ctrl Pts',(0.319726472657586,2.14045981596039,4.5646854940741));
#54471=CARTESIAN_POINT('Ctrl Pts',(0.319906999619618,2.13899994400357,4.56459577232617));
#54472=CARTESIAN_POINT('Ctrl Pts',(0.319973729609344,2.13844862015373,4.56456185471717));
#54473=CARTESIAN_POINT('Ctrl Pts',(0.32009838123621,2.1373959444762,4.56449702778116));
#54474=CARTESIAN_POINT('Ctrl Pts',(0.320156550933138,2.13689462323059,4.56446612635752));
#54475=CARTESIAN_POINT('Ctrl Pts',(0.32025731941996,2.13600798888557,4.56441142301896));
#54476=CARTESIAN_POINT('Ctrl Pts',(0.320300401116058,2.13562273078256,4.56438763637306));
#54477=CARTESIAN_POINT('Ctrl Pts',(0.320383726791296,2.13486521799335,4.56434083198357));
#54478=CARTESIAN_POINT('Ctrl Pts',(0.320424017374704,2.13449296893601,4.56431781574675));
#54479=CARTESIAN_POINT('Ctrl Pts',(0.320518986771833,2.13360100940536,4.56426262672786));
#54480=CARTESIAN_POINT('Ctrl Pts',(0.3205730502568,2.13308123574199,4.56423043461548));
#54481=CARTESIAN_POINT('Ctrl Pts',(0.320733701462322,2.13149933104821,4.564132361899));
#54482=CARTESIAN_POINT('Ctrl Pts',(0.320836275679614,2.13043680788569,4.56406635515123));
#54483=CARTESIAN_POINT('Ctrl Pts',(0.321923602454403,2.11855684670442,4.56332680818932));
#54484=CARTESIAN_POINT('Ctrl Pts',(0.322366031817001,2.1076979461868,4.5626362645731));
#54485=CARTESIAN_POINT('Ctrl Pts',(0.321975340975053,2.06787519781979,4.56004703924851));
#54486=CARTESIAN_POINT('Ctrl Pts',(0.317787518208194,2.03908385862853,4.55805023089022));
#54487=CARTESIAN_POINT('Ctrl Pts',(0.307144261411345,2.00193127254364,4.55547810368107));
#54488=CARTESIAN_POINT('Ctrl Pts',(0.304056578824144,1.99273999194857,4.55484387331992));
#54489=CARTESIAN_POINT('Ctrl Pts',(0.300043891779038,1.98236974819069,4.55414123143897));
#54490=CARTESIAN_POINT('Ctrl Pts',(0.299519932477342,1.98104192602815,4.55405151534968));
#54491=CARTESIAN_POINT('Ctrl Pts',(0.298837680397546,1.97934604525443,4.55393729392506));
#54492=CARTESIAN_POINT('Ctrl Pts',(0.298687510632921,1.97897476702282,4.55391230986944));
#54493=CARTESIAN_POINT('Ctrl Pts',(0.29844514215234,1.97837873638653,4.55387223888141));
#54494=CARTESIAN_POINT('Ctrl Pts',(0.298353381346516,1.97815380811325,4.55385712551486));
#54495=CARTESIAN_POINT('Ctrl Pts',(0.298178157377616,1.97772567585418,4.55382837498));
#54496=CARTESIAN_POINT('Ctrl Pts',(0.298094741464879,1.97752245514518,4.55381473514727));
#54497=CARTESIAN_POINT('Ctrl Pts',(0.297904112858937,1.97705938758681,4.55378367084896));
#54498=CARTESIAN_POINT('Ctrl Pts',(0.297796768091028,1.97679959596341,4.55376625454502));
#54499=CARTESIAN_POINT('Ctrl Pts',(0.297461283843121,1.97599067037787,4.5537120593778));
#54500=CARTESIAN_POINT('Ctrl Pts',(0.29723196268716,1.97544202318043,4.553675351975));
#54501=CARTESIAN_POINT('Ctrl Pts',(0.295439620695161,1.9711870104725,4.55339103449133));
#54502=CARTESIAN_POINT('Ctrl Pts',(0.293808765264527,1.96750936326479,4.55314745171547));
#54503=CARTESIAN_POINT('Ctrl Pts',(0.285988003195334,1.95072833928226,4.55204168513106));
#54504=CARTESIAN_POINT('Ctrl Pts',(0.278986976188894,1.93801998498287,4.55122006229704));
#54505=CARTESIAN_POINT('Ctrl Pts',(0.254900776914848,1.90052289926077,4.54871910649744));
#54506=CARTESIAN_POINT('Ctrl Pts',(0.235189227775424,1.87762336639573,4.54706431017389));
#54507=CARTESIAN_POINT('Ctrl Pts',(0.211223847348802,1.85658889443726,4.54514425815119));
#54508=CARTESIAN_POINT('Ctrl Pts',(0.209847550212254,1.85540137886105,4.54503433727265));
#54509=CARTESIAN_POINT('Ctrl Pts',(0.207768880582198,1.85363828979879,4.54486879580796));
#54510=CARTESIAN_POINT('Ctrl Pts',(0.20707398633711,1.8530539246155,4.54481353435915));
#54511=CARTESIAN_POINT('Ctrl Pts',(0.205952554088424,1.85211892779933,4.54472447403346));
#54512=CARTESIAN_POINT('Ctrl Pts',(0.20552756483114,1.85176643945768,4.54469075069432));
#54513=CARTESIAN_POINT('Ctrl Pts',(0.204713720689455,1.85109495555024,4.54462622330877));
#54514=CARTESIAN_POINT('Ctrl Pts',(0.204325020442008,1.85077577443616,4.54459542690181));
#54515=CARTESIAN_POINT('Ctrl Pts',(0.203635702488499,1.85021243769995,4.54454085184358));
#54516=CARTESIAN_POINT('Ctrl Pts',(0.203335388177042,1.8499679110183,4.54451708824976));
#54517=CARTESIAN_POINT('Ctrl Pts',(0.20274315640915,1.84948746732515,4.54447025080113));
#54518=CARTESIAN_POINT('Ctrl Pts',(0.202451266054904,1.84925151771381,4.54444717831058));
#54519=CARTESIAN_POINT('Ctrl Pts',(0.201749397842952,1.84868618687107,4.54439172760249));
#54520=CARTESIAN_POINT('Ctrl Pts',(0.201339025612784,1.84835729901414,4.54435932964721));
#54521=CARTESIAN_POINT('Ctrl Pts',(0.19984501305444,1.84716593479695,4.54424146359948));
#54522=CARTESIAN_POINT('Ctrl Pts',(0.198756632859906,1.84630945116549,4.54415575655851));
#54523=CARTESIAN_POINT('Ctrl Pts',(0.180772483103976,1.83234387677761,4.54274201784886));
#54524=CARTESIAN_POINT('Ctrl Pts',(0.162622125117904,1.82094407394239,4.5413452554332));
#54525=CARTESIAN_POINT('Ctrl Pts',(0.129714878429536,1.80458240197122,4.53887761804258));
#54526=CARTESIAN_POINT('Ctrl Pts',(0.115477669790181,1.79873200633156,4.5378300129434));
#54527=CARTESIAN_POINT('Ctrl Pts',(0.0915294864427441,1.79083919181348,
4.53613860571807));
#54528=CARTESIAN_POINT('Ctrl Pts',(0.0820444181801044,1.78818787806282,
4.53548629660424));
#54529=CARTESIAN_POINT('Ctrl Pts',(0.0687877575405258,1.78512929270441,
4.53461122360926));
#54530=CARTESIAN_POINT('Ctrl Pts',(0.0651086824127195,1.78434800739767,
4.53437220990488));
#54531=CARTESIAN_POINT('Ctrl Pts',(0.0608912901534426,1.78352928612848,
4.53410324614969));
#54532=CARTESIAN_POINT('Ctrl Pts',(0.0603657410783373,1.78342861899918,
4.53406981803239));
#54533=CARTESIAN_POINT('Ctrl Pts',(0.0595725244416208,1.78327872818386,
4.53401950093834));
#54534=CARTESIAN_POINT('Ctrl Pts',(0.0593050445592811,1.78322853446007,
4.53400255691538));
#54535=CARTESIAN_POINT('Ctrl Pts',(0.0588229788532426,1.78313870479148,
4.53397206202357));
#54536=CARTESIAN_POINT('Ctrl Pts',(0.058608416822605,1.78309894805966,4.53395850426682));
#54537=CARTESIAN_POINT('Ctrl Pts',(0.0581466913976274,1.78301387877959,
4.53392936144607));
#54538=CARTESIAN_POINT('Ctrl Pts',(0.0578995160846108,1.78296863750561,
4.53391378053407));
#54539=CARTESIAN_POINT('Ctrl Pts',(0.0572323372415175,1.782847327952,4.53387177795912));
#54540=CARTESIAN_POINT('Ctrl Pts',(0.0568122332340528,1.78277180457398,
4.53384538742762));
#54541=CARTESIAN_POINT('Ctrl Pts',(0.0548649124117083,1.78242572113924,
4.53372331894553));
#54542=CARTESIAN_POINT('Ctrl Pts',(0.0533358720597281,1.7821653477266,4.53362821210427));
#54543=CARTESIAN_POINT('Ctrl Pts',(0.0204327649374402,1.77680655960813,
4.53159639272886));
#54544=CARTESIAN_POINT('Ctrl Pts',(-0.0115285967771731,1.77636535368129,
4.52989783877908));
#54545=CARTESIAN_POINT('Ctrl Pts',(-0.055322460813225,1.782267164628,4.52739423577715));
#54546=CARTESIAN_POINT('Ctrl Pts',(-0.0674963361952112,1.78462890314258,
4.52668068021975));
#54547=CARTESIAN_POINT('Ctrl Pts',(-0.0849204757361831,1.78906441778081,
4.52561362809984));
#54548=CARTESIAN_POINT('Ctrl Pts',(-0.0903006157187279,1.79058407210571,
4.52527773327316));
#54549=CARTESIAN_POINT('Ctrl Pts',(-0.0965119185732252,1.79251428951246,
4.5248815070195));
#54550=CARTESIAN_POINT('Ctrl Pts',(-0.0973843920833234,1.79278949768575,
4.52482565573068));
#54551=CARTESIAN_POINT('Ctrl Pts',(-0.0987121433231434,1.7932145405961,
4.52474035793878));
#54552=CARTESIAN_POINT('Ctrl Pts',(-0.0991682831903105,1.79336168382565,
4.52471100000876));
#54553=CARTESIAN_POINT('Ctrl Pts',(-0.0999601383356593,1.79361907496038,
4.52465993957367));
#54554=CARTESIAN_POINT('Ctrl Pts',(-0.100296004564026,1.7937288587687,4.52463825239425));
#54555=CARTESIAN_POINT('Ctrl Pts',(-0.100994954344315,1.7939585958718,4.52459305813245));
#54556=CARTESIAN_POINT('Ctrl Pts',(-0.101358006145582,1.7940786433869,4.52456954796843));
#54557=CARTESIAN_POINT('Ctrl Pts',(-0.102244476148977,1.79437351676707,
4.52451205644772));
#54558=CARTESIAN_POINT('Ctrl Pts',(-0.10276765921128,1.79454904097303,4.5244780520548));
#54559=CARTESIAN_POINT('Ctrl Pts',(-0.104760965577773,1.79522348203908,
4.52434821375438));
#54560=CARTESIAN_POINT('Ctrl Pts',(-0.1062279091361,1.79573166941937,4.5242520733434));
#54561=CARTESIAN_POINT('Ctrl Pts',(-0.130484381856795,1.80433153773056,
4.52265242544909));
#54562=CARTESIAN_POINT('Ctrl Pts',(-0.152290713152085,1.81495072102985,
4.52105963881474));
#54563=CARTESIAN_POINT('Ctrl Pts',(-0.184708505815811,1.83552652170552,
4.51846897725457));
#54564=CARTESIAN_POINT('Ctrl Pts',(-0.196198824550928,1.84393460792379,
4.51750103030015));
#54565=CARTESIAN_POINT('Ctrl Pts',(-0.215112060873255,1.85979711464196,
4.51585364986379));
#54566=CARTESIAN_POINT('Ctrl Pts',(-0.22279666352885,1.86690705752968,4.51516680767203));
#54567=CARTESIAN_POINT('Ctrl Pts',(-0.230812284088111,1.87508260176963,
4.51444289900769));
#54568=CARTESIAN_POINT('Ctrl Pts',(-0.231498886629132,1.87578935783409,
4.514380828236));
#54569=CARTESIAN_POINT('Ctrl Pts',(-0.232681906574711,1.8770183301956,4.51427378975466));
#54570=CARTESIAN_POINT('Ctrl Pts',(-0.233179829686016,1.87753907811186,
4.51422871017536));
#54571=CARTESIAN_POINT('Ctrl Pts',(-0.233887663234675,1.87828434635492,
4.51416459206058));
#54572=CARTESIAN_POINT('Ctrl Pts',(-0.234099000715582,1.87850749911003,
4.51414544396624));
#54573=CARTESIAN_POINT('Ctrl Pts',(-0.234463158984647,1.87889311984239,
4.51411244261688));
#54574=CARTESIAN_POINT('Ctrl Pts',(-0.234616130666335,1.87905544449699,
4.51409857762197));
#54575=CARTESIAN_POINT('Ctrl Pts',(-0.234910064101439,1.87936799904045,
4.51407193226462));
#54576=CARTESIAN_POINT('Ctrl Pts',(-0.235051050040951,1.87951820497192,
4.5140591499858));
#54577=CARTESIAN_POINT('Ctrl Pts',(-0.235384741871708,1.87987440292686,
4.5140288918353));
#54578=CARTESIAN_POINT('Ctrl Pts',(-0.235577321912191,1.88008051338068,
4.51401142571908));
#54579=CARTESIAN_POINT('Ctrl Pts',(-0.236250706344075,1.88080310836149,
4.51395033929737));
#54580=CARTESIAN_POINT('Ctrl Pts',(-0.236730089302662,1.88132092374223,
4.51390682752149));
#54581=CARTESIAN_POINT('Ctrl Pts',(-0.242925121458277,1.88805686023063,
4.51334414602258));
#54582=CARTESIAN_POINT('Ctrl Pts',(-0.2483964780876,1.89449640429394,4.51284294273553));
#54583=CARTESIAN_POINT('Ctrl Pts',(-0.269186200550787,1.92101038419349,
4.51088651071572));
#54584=CARTESIAN_POINT('Ctrl Pts',(-0.282376156885098,1.94263926276705,
4.50951674486301));
#54585=CARTESIAN_POINT('Ctrl Pts',(-0.297782674136048,1.97621260265667,
4.50741908689142));
#54586=CARTESIAN_POINT('Ctrl Pts',(-0.302076273279367,1.98709416902304,
4.50674429327485));
#54587=CARTESIAN_POINT('Ctrl Pts',(-0.307496400373257,2.00337167708153,
4.50572550675659));
#54588=CARTESIAN_POINT('Ctrl Pts',(-0.309091358748421,2.00860199404576,
4.5053968543759));
#54589=CARTESIAN_POINT('Ctrl Pts',(-0.310795565517467,2.01474673239587,
4.50500838373934));
#54590=CARTESIAN_POINT('Ctrl Pts',(-0.311034973908767,2.0156243627495,4.50495284492084));
#54591=CARTESIAN_POINT('Ctrl Pts',(-0.311394568008039,2.01696490285246,
4.50486792407217));
#54592=CARTESIAN_POINT('Ctrl Pts',(-0.311517445796499,2.01742709098192,
4.50483862937747));
#54593=CARTESIAN_POINT('Ctrl Pts',(-0.311729305006143,2.01823117442838,
4.50478763621584));
#54594=CARTESIAN_POINT('Ctrl Pts',(-0.311818754102739,2.01857294661352,
4.50476595293384));
#54595=CARTESIAN_POINT('Ctrl Pts',(-0.312004001758485,2.01928553294174,
4.50472072509327));
#54596=CARTESIAN_POINT('Ctrl Pts',(-0.312099701600884,2.01965637197343,
4.5046971773791));
#54597=CARTESIAN_POINT('Ctrl Pts',(-0.31233218626508,2.02056393869788,4.50463952201286));
#54598=CARTESIAN_POINT('Ctrl Pts',(-0.312468248508577,2.02110084867259,
4.50460539106698));
#54599=CARTESIAN_POINT('Ctrl Pts',(-0.312983662586338,2.02315694936466,
4.50447459862682));
#54600=CARTESIAN_POINT('Ctrl Pts',(-0.3133533198935,2.02467852729999,4.50437762494992));
#54601=CARTESIAN_POINT('Ctrl Pts',(-0.319425494415398,2.05049130998662,
4.50272925164632));
#54602=CARTESIAN_POINT('Ctrl Pts',(-0.322297879207263,2.07535592345029,
4.50108236478238));
#54603=CARTESIAN_POINT('Ctrl Pts',(-0.322252709050149,2.12430402355982,
4.49777687468305));
#54604=CARTESIAN_POINT('Ctrl Pts',(-0.319548251603004,2.14823505406213,
4.49613367791463));
#54605=CARTESIAN_POINT('Ctrl Pts',(-0.313902454782349,2.17299549645883,
4.49452912794629));
#54606=CARTESIAN_POINT('Ctrl Pts',(-0.31358586537667,2.17434378805043,4.49444208125366));
#54607=CARTESIAN_POINT('Ctrl Pts',(-0.313163453274868,2.17609203773674,
4.49432967518207));
#54608=CARTESIAN_POINT('Ctrl Pts',(-0.313065544632058,2.17649386539296,
4.49430387092083));
#54609=CARTESIAN_POINT('Ctrl Pts',(-0.312914051216105,2.17711044783589,
4.49426432571514));
#54610=CARTESIAN_POINT('Ctrl Pts',(-0.312861018745365,2.17732533584948,
4.49425055296658));
#54611=CARTESIAN_POINT('Ctrl Pts',(-0.312755303230623,2.17775180685073,
4.49422323806932));
#54612=CARTESIAN_POINT('Ctrl Pts',(-0.312702627192136,2.17796338958157,
4.49420969569517));
#54613=CARTESIAN_POINT('Ctrl Pts',(-0.312584755136581,2.1784348024938,4.49417954329042));
#54614=CARTESIAN_POINT('Ctrl Pts',(-0.31251945003005,2.17869460426357,4.4941629397082));
#54615=CARTESIAN_POINT('Ctrl Pts',(-0.312327854277337,2.17945282523058,
4.4941145223147));
#54616=CARTESIAN_POINT('Ctrl Pts',(-0.312200693939053,2.1799510269304,4.49408275870935));
#54617=CARTESIAN_POINT('Ctrl Pts',(-0.31127472970468,2.18354296829767,4.49385409476724));
#54618=CARTESIAN_POINT('Ctrl Pts',(-0.310431112203309,2.18662511963994,
4.49365973584894));
#54619=CARTESIAN_POINT('Ctrl Pts',(-0.307942611817073,2.19521311597016,
4.49312207033707));
#54620=CARTESIAN_POINT('Ctrl Pts',(-0.306196062322751,2.20068847643272,
4.49278378386813));
#54621=CARTESIAN_POINT('Ctrl Pts',(-0.301532736499007,2.21406146455074,
4.49196212952329));
#54622=CARTESIAN_POINT('Ctrl Pts',(-0.298451155384507,2.22189721584668,
4.49148466461904));
#54623=CARTESIAN_POINT('Ctrl Pts',(-0.28515399750154,2.25217059518616,4.48962451458178));
#54624=CARTESIAN_POINT('Ctrl Pts',(-0.272686498978403,2.2735243920923,4.48827108571912));
#54625=CARTESIAN_POINT('Ctrl Pts',(-0.256379259867567,2.29528785044138,
4.48668170716075));
#54626=CARTESIAN_POINT('Ctrl Pts',(-0.254827101037764,2.29730893924557,
4.48653199021396));
#54627=CARTESIAN_POINT('Ctrl Pts',(-0.249302626687654,2.30432850648377,
4.48600415617149));
#54628=CARTESIAN_POINT('Ctrl Pts',(-0.245206098789032,2.30922690733415,
4.4856216105108));
#54629=CARTESIAN_POINT('Ctrl Pts',(-0.240284634971525,2.3147685401397,4.48517050701104));
#54630=CARTESIAN_POINT('Ctrl Pts',(-0.239598596882237,2.31553362607924,
4.48510780838867));
#54631=CARTESIAN_POINT('Ctrl Pts',(-0.238571596637828,2.316667998351,4.48501421506202));
#54632=CARTESIAN_POINT('Ctrl Pts',(-0.238233406189017,2.3170397945143,4.4849834374572));
#54633=CARTESIAN_POINT('Ctrl Pts',(-0.237629043917199,2.31770109731778,
4.48492851142747));
#54634=CARTESIAN_POINT('Ctrl Pts',(-0.237363208713023,2.31799091135561,
4.48490437732318));
#54635=CARTESIAN_POINT('Ctrl Pts',(-0.236801991521736,2.31860050765711,
4.48485348030516));
#54636=CARTESIAN_POINT('Ctrl Pts',(-0.236506490945261,2.31892017923071,
4.48482671236027));
#54637=CARTESIAN_POINT('Ctrl Pts',(-0.23572498777887,2.31976217778918,4.48475600111385));
#54638=CARTESIAN_POINT('Ctrl Pts',(-0.235237898824132,2.32028348915368,
4.48471201133277));
#54639=CARTESIAN_POINT('Ctrl Pts',(-0.233031629605031,2.32262910615578,
4.48451312617098));
#54640=CARTESIAN_POINT('Ctrl Pts',(-0.231292968485754,2.32443489359354,
4.48435739175576));
#54641=CARTESIAN_POINT('Ctrl Pts',(-0.223579583352869,2.3322612510759,4.48367065009848));
#54642=CARTESIAN_POINT('Ctrl Pts',(-0.217390038820479,2.33806442041225,
4.48313018379167));
#54643=CARTESIAN_POINT('Ctrl Pts',(-0.200214722962118,2.35293877490139,
4.48165676651));
#54644=CARTESIAN_POINT('Ctrl Pts',(-0.188845205068137,2.36153656040124,
4.48070746905897));
#54645=CARTESIAN_POINT('Ctrl Pts',(-0.155942505368941,2.38315121774945,
4.47805228586352));
#54646=CARTESIAN_POINT('Ctrl Pts',(-0.13339620331319,2.39444581406517,4.47632715146045));
#54647=CARTESIAN_POINT('Ctrl Pts',(-0.108498678045123,2.4034650340022,4.47465463986337));
#54648=CARTESIAN_POINT('Ctrl Pts',(-0.107229336516695,2.40391587576309,
4.47456999580508));
#54649=CARTESIAN_POINT('Ctrl Pts',(-0.105570817886753,2.40449326002815,
4.47446024770178));
#54650=CARTESIAN_POINT('Ctrl Pts',(-0.105184198018649,2.40462703012608,
4.47443472398899));
#54651=CARTESIAN_POINT('Ctrl Pts',(-0.104588877874785,2.40483174184533,
4.47439551556005));
#54652=CARTESIAN_POINT('Ctrl Pts',(-0.104380359588049,2.40490320553337,
4.47438179988561));
#54653=CARTESIAN_POINT('Ctrl Pts',(-0.103965557906558,2.4050448915779,4.47435455069314));
#54654=CARTESIAN_POINT('Ctrl Pts',(-0.103759277718189,2.40511511826951,
4.47434101701871));
#54655=CARTESIAN_POINT('Ctrl Pts',(-0.103298268426545,2.40527154417185,
4.4743108096053));
#54656=CARTESIAN_POINT('Ctrl Pts',(-0.103043503258766,2.40535763356827,
4.47429414248433));
#54657=CARTESIAN_POINT('Ctrl Pts',(-0.102295414053347,2.40560938254398,
4.47424527754099));
#54658=CARTESIAN_POINT('Ctrl Pts',(-0.101801793203356,2.40577416722936,
4.4742131315385));
#54659=CARTESIAN_POINT('Ctrl Pts',(-0.0981122153388935,2.40699592852565,
4.47397356550991));
#54660=CARTESIAN_POINT('Ctrl Pts',(-0.0949001221484285,2.40800401933534,
4.47376897620937));
#54661=CARTESIAN_POINT('Ctrl Pts',(-0.0839914687636972,2.41124074924305,
4.47308567521436));
#54662=CARTESIAN_POINT('Ctrl Pts',(-0.0762273130646911,2.4132328016951,
4.47261850980601));
#54663=CARTESIAN_POINT('Ctrl Pts',(-0.0391905778975258,2.4212763381231,
4.47044554647348));
#54664=CARTESIAN_POINT('Ctrl Pts',(-0.00924472785627596,2.42352602791262,
4.46883609786955));
#54665=CARTESIAN_POINT('Ctrl Pts',(0.0301083332534404,2.42100740481181,
4.46653927602263));
#54666=CARTESIAN_POINT('Ctrl Pts',(0.0396003521912912,2.41997507797706,
4.46597263872235));
#54667=CARTESIAN_POINT('Ctrl Pts',(0.0501516498871189,2.41835086161297,
4.465323462058));
#54668=CARTESIAN_POINT('Ctrl Pts',(0.0512704282328862,2.41817259815009,
4.46525438655756));
#54669=CARTESIAN_POINT('Ctrl Pts',(0.0528597967512131,2.41791075150287,
4.46515590436989));
#54670=CARTESIAN_POINT('Ctrl Pts',(0.0533311857580323,2.41783201326401,
4.46512665161407));
#54671=CARTESIAN_POINT('Ctrl Pts',(0.0541959564767994,2.41768558868351,
4.465072905447));
#54672=CARTESIAN_POINT('Ctrl Pts',(0.0545893915174747,2.41761821938784,
4.46504842215948));
#54673=CARTESIAN_POINT('Ctrl Pts',(0.055386815898049,2.41748014812923,4.4649987355163));
#54674=CARTESIAN_POINT('Ctrl Pts',(0.0557907973796482,2.41740940558961,
4.46497353091056));
#54675=CARTESIAN_POINT('Ctrl Pts',(0.0567857764561705,2.4172332132924,4.46491137191246));
#54676=CARTESIAN_POINT('Ctrl Pts',(0.0573766148008803,2.41712688326559,
4.46487438953699));
#54677=CARTESIAN_POINT('Ctrl Pts',(0.0595356592593219,2.41673210033206,
4.4647389858631));
#54678=CARTESIAN_POINT('Ctrl Pts',(0.0611019957969733,2.41643366456019,
4.4646402467365));
#54679=CARTESIAN_POINT('Ctrl Pts',(0.0701600580862758,2.41463806064984,
4.46406624199894));
#54680=CARTESIAN_POINT('Ctrl Pts',(0.0775983221806385,2.41288660461245,
4.46358288508447));
#54681=CARTESIAN_POINT('Ctrl Pts',(0.0919936168366696,2.40895212227722,
4.46262287294023));
#54682=CARTESIAN_POINT('Ctrl Pts',(0.0989527974004637,2.40679402052957,
4.46214723261885));
#54683=CARTESIAN_POINT('Ctrl Pts',(0.128649744806816,2.39646918363126,4.46006939889688));
#54684=CARTESIAN_POINT('Ctrl Pts',(0.150500257436267,2.38599694141076,4.45840914776875));
#54685=CARTESIAN_POINT('Ctrl Pts',(0.180046294304361,2.36750521033777,4.45608800343556));
#54686=CARTESIAN_POINT('Ctrl Pts',(0.188830652553895,2.36137854744795,4.45538816864679));
#54687=CARTESIAN_POINT('Ctrl Pts',(0.197880281213324,2.35437200776909,4.45466971185274));
#54688=CARTESIAN_POINT('Ctrl Pts',(0.198464277207677,2.3539166294824,4.45462336044449));
#54689=CARTESIAN_POINT('Ctrl Pts',(0.199273157668604,2.35328139916858,4.45455918361392));
#54690=CARTESIAN_POINT('Ctrl Pts',(0.199499372824427,2.35310325714273,4.45454123819974));
#54691=CARTESIAN_POINT('Ctrl Pts',(0.199888149776683,2.35279625439183,4.45451040179857));
#54692=CARTESIAN_POINT('Ctrl Pts',(0.200050825934099,2.35266753986083,4.45449750037733));
#54693=CARTESIAN_POINT('Ctrl Pts',(0.200383778747172,2.35240357391829,4.45447109797611));
#54694=CARTESIAN_POINT('Ctrl Pts',(0.20055404256886,2.35226830740556,4.4544575981957));
#54695=CARTESIAN_POINT('Ctrl Pts',(0.200952656417856,2.35195096903396,4.45442599692546));
#54696=CARTESIAN_POINT('Ctrl Pts',(0.201180896832849,2.35176875832733,4.45440790542132));
#54697=CARTESIAN_POINT('Ctrl Pts',(0.201662895029652,2.35138289174255,4.45436970519287));
#54698=CARTESIAN_POINT('Ctrl Pts',(0.201916592956766,2.3511791611251,4.45434960183096));
#54699=CARTESIAN_POINT('Ctrl Pts',(0.202598398843979,2.35062994044679,4.4542955818674));
#54700=CARTESIAN_POINT('Ctrl Pts',(0.203025933783631,2.3502837359561,4.45426171567616));
#54701=CARTESIAN_POINT('Ctrl Pts',(0.213880728340614,2.34144774533698,4.45340201371961));
#54702=CARTESIAN_POINT('Ctrl Pts',(0.223768893485688,2.33231349890859,4.45262186816909));
#54703=CARTESIAN_POINT('Ctrl Pts',(0.255183806318814,2.29942066912169,4.45003877443414));
#54704=CARTESIAN_POINT('Ctrl Pts',(0.273730340374863,2.27308705072218,4.44830741820548));
#54705=CARTESIAN_POINT('Ctrl Pts',(0.290429522192716,2.23978244713345,4.44609339193743));
#54706=CARTESIAN_POINT('Ctrl Pts',(0.292656017105525,2.23505884182629,4.44577945773601));
#54707=CARTESIAN_POINT('Ctrl Pts',(0.295118138897196,2.22948828324147,4.44540858022175));
#54708=CARTESIAN_POINT('Ctrl Pts',(0.295466364161317,2.22869172090325,4.44535553171109));
#54709=CARTESIAN_POINT('Ctrl Pts',(0.296017055693599,2.22741800118514,4.44527067863244));
#54710=CARTESIAN_POINT('Ctrl Pts',(0.296221602870952,2.22694174362727,4.44523894506001));
#54711=CARTESIAN_POINT('Ctrl Pts',(0.29658070369808,2.22610003671187,4.44518284962745));
#54712=CARTESIAN_POINT('Ctrl Pts',(0.2967357334264,2.22573479061281,4.4451585040221));
#54713=CARTESIAN_POINT('Ctrl Pts',(0.297054992033892,2.22497874630301,4.44510810129153));
#54714=CARTESIAN_POINT('Ctrl Pts',(0.297219125100246,2.22458790868957,4.44508204097011));
#54715=CARTESIAN_POINT('Ctrl Pts',(0.29763764068907,2.22358579545913,4.44501520957049));
#54716=CARTESIAN_POINT('Ctrl Pts',(0.297890910535101,2.22297405988396,4.44497440087338));
#54717=CARTESIAN_POINT('Ctrl Pts',(0.298919354571821,2.22046818563054,4.44480718324378));
#54718=CARTESIAN_POINT('Ctrl Pts',(0.299678348858594,2.21856749639668,4.44468022919748));
#54719=CARTESIAN_POINT('Ctrl Pts',(0.304579666821558,2.20594574807542,4.44383624186085));
#54720=CARTESIAN_POINT('Ctrl Pts',(0.308163565718999,2.1950180963027,4.44310064696179));
#54721=CARTESIAN_POINT('Ctrl Pts',(0.319705909018979,2.1522235003017,4.44019971276318));
#54722=CARTESIAN_POINT('Ctrl Pts',(0.323360473012411,2.11940908314164,4.43790971082713));
#54723=CARTESIAN_POINT('Ctrl Pts',(0.321786569198625,2.08155592580723,4.43545177812395));
#54724=CARTESIAN_POINT('Ctrl Pts',(0.321457300508331,2.07650551018429,4.43512820494653));
#54725=CARTESIAN_POINT('Ctrl Pts',(0.320952975646236,2.07083210197153,4.43477118094128));
#54726=CARTESIAN_POINT('Ctrl Pts',(0.320894880489813,2.07019975598632,4.43473147849955));
#54727=CARTESIAN_POINT('Ctrl Pts',(0.320807628880947,2.06927990268041,4.43467386070206));
#54728=CARTESIAN_POINT('Ctrl Pts',(0.32077995459967,2.06899226135075,4.4346558627857));
#54729=CARTESIAN_POINT('Ctrl Pts',(0.320730832246723,2.06848879707,4.43462439505245));
#54730=CARTESIAN_POINT('Ctrl Pts',(0.320709553215465,2.06827295883453,4.43461091572398));
#54731=CARTESIAN_POINT('Ctrl Pts',(0.320664846116422,2.06782412511059,4.43458290871706));
#54732=CARTESIAN_POINT('Ctrl Pts',(0.320641382065921,2.06759113443115,4.43456838313801));
#54733=CARTESIAN_POINT('Ctrl Pts',(0.320580442822337,2.06699257126501,4.43453109903687));
#54734=CARTESIAN_POINT('Ctrl Pts',(0.320542596118838,2.06662703566607,4.43450836145497));
#54735=CARTESIAN_POINT('Ctrl Pts',(0.320458871388904,2.06583167808654,4.43445895422118));
#54736=CARTESIAN_POINT('Ctrl Pts',(0.320412753586477,2.0654018812878,4.43443229790286));
#54737=CARTESIAN_POINT('Ctrl Pts',(0.320276748932008,2.06415797771096,4.43435526963409));
#54738=CARTESIAN_POINT('Ctrl Pts',(0.320184622327838,2.06334411198364,4.43430501961294));
#54739=CARTESIAN_POINT('Ctrl Pts',(0.319210546791,2.05502288943818,4.43379268426282));
#54740=CARTESIAN_POINT('Ctrl Pts',(0.318067751716315,2.04754774194699,4.4333443976989));
#54741=CARTESIAN_POINT('Ctrl Pts',(0.31512367707776,2.03197885260587,4.43242301783707));
#54742=CARTESIAN_POINT('Ctrl Pts',(0.313270967515525,2.023900567361,4.43195199141336));
#54743=CARTESIAN_POINT('Ctrl Pts',(0.304536883868285,1.991589926744,4.43006592967774));
#54744=CARTESIAN_POINT('Ctrl Pts',(0.295138258999131,1.96813331643806,4.4286841869479));
#54745=CARTESIAN_POINT('Ctrl Pts',(0.28169330484156,1.94341525150783,4.42703826527747));
#54746=CARTESIAN_POINT('Ctrl Pts',(0.280246266328384,1.94083992054523,4.42686441923744));
#54747=CARTESIAN_POINT('Ctrl Pts',(0.275827611325756,1.93322305471463,4.42634269655314));
#54748=CARTESIAN_POINT('Ctrl Pts',(0.272753991311786,1.92824239691003,4.42599149944224));
#54749=CARTESIAN_POINT('Ctrl Pts',(0.269004041470019,1.9225204767946,4.42557501257402));
#54750=CARTESIAN_POINT('Ctrl Pts',(0.268457643341898,1.92169506686144,4.4255146091281));
#54751=CARTESIAN_POINT('Ctrl Pts',(0.267628188795722,1.92045451653725,4.42542333125281));
#54752=CARTESIAN_POINT('Ctrl Pts',(0.267347946596122,1.92003749413758,4.42539256259399));
#54753=CARTESIAN_POINT('Ctrl Pts',(0.266846234064971,1.9192946647454,4.42533760309664));
#54754=CARTESIAN_POINT('Ctrl Pts',(0.266625138903693,1.91896860458324,4.42531342644442));
#54755=CARTESIAN_POINT('Ctrl Pts',(0.26615757632399,1.91828178108096,4.42526238862274));
#54756=CARTESIAN_POINT('Ctrl Pts',(0.265910972184482,1.91792111217748,4.42523552231068));
#54757=CARTESIAN_POINT('Ctrl Pts',(0.265257198688153,1.91696910194844,4.42516443405522));
#54758=CARTESIAN_POINT('Ctrl Pts',(0.264848787064476,1.91637862032262,4.42512016499919));
#54759=CARTESIAN_POINT('Ctrl Pts',(0.26298561063822,1.91370398754606,4.42491883559167));
#54760=CARTESIAN_POINT('Ctrl Pts',(0.261508226866333,1.91163577211601,4.42476091336106));
#54761=CARTESIAN_POINT('Ctrl Pts',(0.254956597043167,1.90268968375777,4.42406779465087));
#54762=CARTESIAN_POINT('Ctrl Pts',(0.249634736505242,1.89599827562939,4.42352302341793));
#54763=CARTESIAN_POINT('Ctrl Pts',(0.24050585607852,1.88541291029464,4.42261623387618));
#54764=CARTESIAN_POINT('Ctrl Pts',(0.236854784251018,1.88138963388034,4.42226012244768));
#54765=CARTESIAN_POINT('Ctrl Pts',(0.230367087010454,1.87459394533332,4.42163880562299));
#54766=CARTESIAN_POINT('Ctrl Pts',(0.227577665743222,1.87177798354352,4.42137510890594));
#54767=CARTESIAN_POINT('Ctrl Pts',(0.211598483321895,1.85623107254909,4.41988460608222));
#54768=CARTESIAN_POINT('Ctrl Pts',(0.197393770619289,1.84459272900576,4.41863209166605));
#54769=CARTESIAN_POINT('Ctrl Pts',(0.172130132608163,1.8272660942492,4.41658197186032));
#54770=CARTESIAN_POINT('Ctrl Pts',(0.161591580632492,1.82089284451229,4.41577255006289));
#54771=CARTESIAN_POINT('Ctrl Pts',(0.150023218241999,1.8147723387325,4.41495063754112));
#54772=CARTESIAN_POINT('Ctrl Pts',(0.149332016418205,1.81440985019381,4.41490177406642));
#54773=CARTESIAN_POINT('Ctrl Pts',(0.14837827955385,1.81391408903499,4.41483469532006));
#54774=CARTESIAN_POINT('Ctrl Pts',(0.148116875795505,1.81377866361448,4.41481634562381));
#54775=CARTESIAN_POINT('Ctrl Pts',(0.147669296514933,1.81354756362365,4.4147849881801));
#54776=CARTESIAN_POINT('Ctrl Pts',(0.14748321332103,1.81345171222247,4.41477196923512));
#54777=CARTESIAN_POINT('Ctrl Pts',(0.147105261952016,1.81325749526824,4.41474556345939));
#54778=CARTESIAN_POINT('Ctrl Pts',(0.146913388685245,1.81315914109081,4.41473217740209));
#54779=CARTESIAN_POINT('Ctrl Pts',(0.14646853124635,1.81293167076412,4.41470118658725));
#54780=CARTESIAN_POINT('Ctrl Pts',(0.146215475433979,1.81280269666855,4.41468359095198));
#54781=CARTESIAN_POINT('Ctrl Pts',(0.145681391537066,1.81253138080525,4.41464652438819));
#54782=CARTESIAN_POINT('Ctrl Pts',(0.145400324331815,1.81238911608194,4.41462705834358));
#54783=CARTESIAN_POINT('Ctrl Pts',(0.144648598620156,1.81201000684936,4.41457510288657));
#54784=CARTESIAN_POINT('Ctrl Pts',(0.144177564655171,1.81177390281764,4.41454265961742));
#54785=CARTESIAN_POINT('Ctrl Pts',(0.142739533054601,1.81105750211353,4.41444394800241));
#54786=CARTESIAN_POINT('Ctrl Pts',(0.141770687159321,1.81058090298048,4.41437790410398));
#54787=CARTESIAN_POINT('Ctrl Pts',(0.138221168679432,1.80885690828808,4.41413755668986));
#54788=CARTESIAN_POINT('Ctrl Pts',(0.135626197375761,1.80763904643118,4.41396495003369));
#54789=CARTESIAN_POINT('Ctrl Pts',(0.126642533147847,1.80356822979324,4.41337684640274));
#54790=CARTESIAN_POINT('Ctrl Pts',(0.120177050737953,1.80088862382197,4.41296984152715));
#54791=CARTESIAN_POINT('Ctrl Pts',(0.0847615380862129,1.78754473360271,
4.41080099533721));
#54792=CARTESIAN_POINT('Ctrl Pts',(0.0544823634979874,1.78086887746603,
4.40914501070586));
#54793=CARTESIAN_POINT('Ctrl Pts',(0.0209445314662134,1.7783943163197,4.40718131347243));
#54794=CARTESIAN_POINT('Ctrl Pts',(0.0181722671549749,1.7782257666651,4.40701819627046));
#54795=CARTESIAN_POINT('Ctrl Pts',(0.0141491157124072,1.7780333216021,4.40678013542227));
#54796=CARTESIAN_POINT('Ctrl Pts',(0.0128996799294585,1.77798084269795,
4.4067060155409));
#54797=CARTESIAN_POINT('Ctrl Pts',(0.00656572131066864,1.77775172542638,
4.40632926464961));
#54798=CARTESIAN_POINT('Ctrl Pts',(0.00147805479965953,1.77768824091122,
4.40602335184442));
#54799=CARTESIAN_POINT('Ctrl Pts',(-0.00446655842054763,1.77775481172251,
4.40566137815842));
#54800=CARTESIAN_POINT('Ctrl Pts',(-0.00532429485811365,1.7777678424274,
4.40560903983186));
#54801=CARTESIAN_POINT('Ctrl Pts',(-0.00669482120962326,1.77779413705707,
4.40552523237389));
#54802=CARTESIAN_POINT('Ctrl Pts',(-0.00720765327246761,1.77780520104246,
4.40549383269388));
#54803=CARTESIAN_POINT('Ctrl Pts',(-0.00811388734251212,1.77782691711509,
4.40543827416123));
#54804=CARTESIAN_POINT('Ctrl Pts',(-0.00850730129608764,1.77783706556179,
4.40541413125278));
#54805=CARTESIAN_POINT('Ctrl Pts',(-0.00932182339267204,1.77785956987869,
4.40536409609776));
#54806=CARTESIAN_POINT('Ctrl Pts',(-0.00974292766759119,1.77787203091338,
4.4053382005767));
#54807=CARTESIAN_POINT('Ctrl Pts',(-0.0108234410920633,1.77790612542731,
4.40527168380189));
#54808=CARTESIAN_POINT('Ctrl Pts',(-0.0114828080472422,1.77792895811133,
4.40523102475855));
#54809=CARTESIAN_POINT('Ctrl Pts',(-0.014193643489848,1.77803116464757,
4.40506358065614));
#54810=CARTESIAN_POINT('Ctrl Pts',(-0.0162443651213139,1.77812811439979,
4.40493624190347));
#54811=CARTESIAN_POINT('Ctrl Pts',(-0.0298764253930816,1.77890318985903,
4.40408517331389));
#54812=CARTESIAN_POINT('Ctrl Pts',(-0.0414135041611636,1.78018657168362,
4.40334237160816));
#54813=CARTESIAN_POINT('Ctrl Pts',(-0.0618461876082502,1.78358366573439,
4.40198574524155));
#54814=CARTESIAN_POINT('Ctrl Pts',(-0.0707691234933321,1.78545912929497,
4.40137909932707));
#54815=CARTESIAN_POINT('Ctrl Pts',(-0.0821953293102451,1.78837157324676,
4.40058672004942));
#54816=CARTESIAN_POINT('Ctrl Pts',(-0.0847822030411975,1.7890653986954,
4.40040629262924));
#54817=CARTESIAN_POINT('Ctrl Pts',(-0.0895568653694782,1.79041002603614,
4.40007152438889));
#54818=CARTESIAN_POINT('Ctrl Pts',(-0.0917469827105972,1.79105198630164,
4.39991727997557));
#54819=CARTESIAN_POINT('Ctrl Pts',(-0.0958291656182346,1.79229577845136,
4.39962861686701));
#54820=CARTESIAN_POINT('Ctrl Pts',(-0.0977228552277498,1.79289194006671,
4.39949423555541));
#54821=CARTESIAN_POINT('Ctrl Pts',(-0.118423162978865,1.79961955482423,
4.39802061865691));
#54822=CARTESIAN_POINT('Ctrl Pts',(-0.136634588979585,1.80745323094136,
4.39667887427147));
#54823=CARTESIAN_POINT('Ctrl Pts',(-0.155895771020906,1.81793214827442,
4.39528414492368));
#54824=CARTESIAN_POINT('Ctrl Pts',(-0.157767271604775,1.81897463992516,
4.39514892738152));
#54825=CARTESIAN_POINT('Ctrl Pts',(-0.160006977809383,1.82025166185578,
4.39498759895547));
#54826=CARTESIAN_POINT('Ctrl Pts',(-0.160385222006933,1.82046834488869,
4.39496037066216));
#54827=CARTESIAN_POINT('Ctrl Pts',(-0.161002284248947,1.82082350332021,
4.39491598016177));
#54828=CARTESIAN_POINT('Ctrl Pts',(-0.161241364498036,1.82096151841016,
4.39489878831537));
#54829=CARTESIAN_POINT('Ctrl Pts',(-0.161659881438182,1.82120383533108,
4.39486870654485));
#54830=CARTESIAN_POINT('Ctrl Pts',(-0.161839393179539,1.82130800241799,
4.39485580801692));
#54831=CARTESIAN_POINT('Ctrl Pts',(-0.162225806844437,1.821532729821,4.39482805188359));
#54832=CARTESIAN_POINT('Ctrl Pts',(-0.162432674537413,1.82165334704583,
4.39481319810085));
#54833=CARTESIAN_POINT('Ctrl Pts',(-0.162977671823719,1.82197193013445,
4.39477407960757));
#54834=CARTESIAN_POINT('Ctrl Pts',(-0.163315576474736,1.82217028303146,
4.39474984002556));
#54835=CARTESIAN_POINT('Ctrl Pts',(-0.164056412161959,1.82260697843853,
4.39469672581033));
#54836=CARTESIAN_POINT('Ctrl Pts',(-0.16445918814923,1.82284558415538,4.39466786806795));
#54837=CARTESIAN_POINT('Ctrl Pts',(-0.165647719278523,1.8235531767693,4.39458276593566));
#54838=CARTESIAN_POINT('Ctrl Pts',(-0.166432006372451,1.82402463827811,
4.39452667704528));
#54839=CARTESIAN_POINT('Ctrl Pts',(-0.169162714998928,1.82568203415616,
4.39433158888757));
#54840=CARTESIAN_POINT('Ctrl Pts',(-0.171098605387895,1.82688530172058,
4.39419364168322));
#54841=CARTESIAN_POINT('Ctrl Pts',(-0.180054863384314,1.8325847422329,4.39355632571406));
#54842=CARTESIAN_POINT('Ctrl Pts',(-0.186912378454082,1.83733203584922,
4.39307088697199));
#54843=CARTESIAN_POINT('Ctrl Pts',(-0.214988641288412,1.85842560678748,
4.39106025797942));
#54844=CARTESIAN_POINT('Ctrl Pts',(-0.2343105539658,1.87711664615387,4.38960940869498));
#54845=CARTESIAN_POINT('Ctrl Pts',(-0.252607669201272,1.89985920467212,
4.38792777434474));
#54846=CARTESIAN_POINT('Ctrl Pts',(-0.254095812546078,1.9017519478463,4.38778845887559));
#54847=CARTESIAN_POINT('Ctrl Pts',(-0.261683017159232,1.91162776060205,
4.38706430365587));
#54848=CARTESIAN_POINT('Ctrl Pts',(-0.267427041060778,1.91987546425222,
4.38646847932064));
#54849=CARTESIAN_POINT('Ctrl Pts',(-0.273336076576221,1.92926725471254,
4.38579363179422));
#54850=CARTESIAN_POINT('Ctrl Pts',(-0.27389162129599,1.9301598963303,4.38572952870617));
#54851=CARTESIAN_POINT('Ctrl Pts',(-0.274715372125618,1.93149804058435,
4.38563348280659));
#54852=CARTESIAN_POINT('Ctrl Pts',(-0.274986887969283,1.93194150587066,
4.38560166104879));
#54853=CARTESIAN_POINT('Ctrl Pts',(-0.275452373532967,1.93270592904141,
4.38554682152066));
#54854=CARTESIAN_POINT('Ctrl Pts',(-0.275646859058124,1.93302657291559,
4.3855238225981));
#54855=CARTESIAN_POINT('Ctrl Pts',(-0.276046835904073,1.93368860896503,
4.38547634440509));
#54856=CARTESIAN_POINT('Ctrl Pts',(-0.276252254557321,1.93403004413321,
4.38545186254307));
#54857=CARTESIAN_POINT('Ctrl Pts',(-0.27672848620391,1.93482494281015,4.38539487561855));
#54858=CARTESIAN_POINT('Ctrl Pts',(-0.276998818122395,1.9352786918826,4.38536235318719));
#54859=CARTESIAN_POINT('Ctrl Pts',(-0.277855087040688,1.93672399827022,
4.38525878246725));
#54860=CARTESIAN_POINT('Ctrl Pts',(-0.278436819706205,1.93771802468459,
4.38518758256341));
#54861=CARTESIAN_POINT('Ctrl Pts',(-0.290061833012129,1.95782860533378,
4.38374766923735));
#54862=CARTESIAN_POINT('Ctrl Pts',(-0.299114980480026,1.9780227663809,4.38230575172274));
#54863=CARTESIAN_POINT('Ctrl Pts',(-0.313616405766477,2.02195357590079,
4.37919979833315));
#54864=CARTESIAN_POINT('Ctrl Pts',(-0.318589153887707,2.04570886986425,
4.37753747090088));
#54865=CARTESIAN_POINT('Ctrl Pts',(-0.320986583694565,2.07117793557682,
4.3758874634548));
#54866=CARTESIAN_POINT('Ctrl Pts',(-0.321107623629924,2.07255929128988,
4.37579839930321));
#54867=CARTESIAN_POINT('Ctrl Pts',(-0.321455123307179,2.07684285985011,
4.37552361944549));
#54868=CARTESIAN_POINT('Ctrl Pts',(-0.321651187999729,2.07974749065067,
4.37533929403666));
#54869=CARTESIAN_POINT('Ctrl Pts',(-0.321834175319448,2.08314242069002,
4.37512649291554));
#54870=CARTESIAN_POINT('Ctrl Pts',(-0.321859364856429,2.08363040485127,
4.37509596868315));
#54871=CARTESIAN_POINT('Ctrl Pts',(-0.321897798115476,2.08440936083387,
4.37504734719406));
#54872=CARTESIAN_POINT('Ctrl Pts',(-0.321911757277751,2.08470029446399,
4.37502921051265));
#54873=CARTESIAN_POINT('Ctrl Pts',(-0.321935546127147,2.08521054562655,
4.37499744254248));
#54874=CARTESIAN_POINT('Ctrl Pts',(-0.321945546126175,2.08542985411713,
4.37498380173922));
#54875=CARTESIAN_POINT('Ctrl Pts',(-0.321964675993694,2.08585902540057,
4.37495713323466));
#54876=CARTESIAN_POINT('Ctrl Pts',(-0.321973824784277,2.08606888716867,
4.37494410449256));
#54877=CARTESIAN_POINT('Ctrl Pts',(-0.321993022699707,2.08651938561134,
4.37491616183459));
#54878=CARTESIAN_POINT('Ctrl Pts',(-0.322003007280448,2.0867600251201,4.37490125146639));
#54879=CARTESIAN_POINT('Ctrl Pts',(-0.322026432696717,2.08734030778371,
4.37486533335715));
#54880=CARTESIAN_POINT('Ctrl Pts',(-0.322039606005793,2.08767996231985,
4.37484434014324));
#54881=CARTESIAN_POINT('Ctrl Pts',(-0.322098762712622,2.0892701940173,4.37474619238116));
#54882=CARTESIAN_POINT('Ctrl Pts',(-0.322137999888886,2.09052103270796,
4.37466939859012));
#54883=CARTESIAN_POINT('Ctrl Pts',(-0.322238911436358,2.09447230018914,
4.37442801115635));
#54884=CARTESIAN_POINT('Ctrl Pts',(-0.322273924581758,2.09717335249639,
4.37426476447746));
#54885=CARTESIAN_POINT('Ctrl Pts',(-0.322274975605568,2.09987460689646,
4.37410298671292));
#54886=CARTESIAN_POINT('',(-0.203129159293197,2.35019936105002,4.35670055803058));
#54887=CARTESIAN_POINT('Ctrl Pts',(-0.203129159293197,2.35019936105002,
4.35670055803058));
#54888=CARTESIAN_POINT('Ctrl Pts',(-0.216614563769107,2.33925097628028,
4.35777896221699));
#54889=CARTESIAN_POINT('Ctrl Pts',(-0.229260010381491,2.32717006691284,
4.3588573664034));
#54890=CARTESIAN_POINT('Ctrl Pts',(-0.240866999069484,2.31411273755725,
4.35993577058981));
#54891=CARTESIAN_POINT('Ctrl Pts',(-0.252452758994495,2.30107928958534,
4.36101220241392));
#54892=CARTESIAN_POINT('Ctrl Pts',(-0.263003251354075,2.28707351158869,
4.36208863423803));
#54893=CARTESIAN_POINT('Ctrl Pts',(-0.272355508139451,2.27228944486271,
4.36316506606214));
#54894=CARTESIAN_POINT('Ctrl Pts',(-0.281706384805359,2.25750755983242,
4.36424133903641));
#54895=CARTESIAN_POINT('Ctrl Pts',(-0.289858909139876,2.2419482646331,4.36531761201069));
#54896=CARTESIAN_POINT('Ctrl Pts',(-0.296692758115266,2.2258355391253,4.36639388498496));
#54897=CARTESIAN_POINT('Ctrl Pts',(-0.303525842065698,2.20972461737952,
4.36747003747432));
#54898=CARTESIAN_POINT('Ctrl Pts',(-0.309040250270101,2.19306113470876,
4.36854618996367));
#54899=CARTESIAN_POINT('Ctrl Pts',(-0.313164036280824,2.17608851427977,
4.36962234245303));
#54900=CARTESIAN_POINT('Ctrl Pts',(-0.317296249751049,2.15908120823156,
4.37070069419121));
#54901=CARTESIAN_POINT('Ctrl Pts',(-0.320032030726004,2.14176429471861,
4.37177904592939));
#54902=CARTESIAN_POINT('Ctrl Pts',(-0.321350696853865,2.1243906797063,4.37285739766757));
#54903=CARTESIAN_POINT('Ctrl Pts',(-0.321970254428679,2.11622791996345,
4.37336404675303));
#54904=CARTESIAN_POINT('Ctrl Pts',(-0.322277741048769,2.10805268328092,
4.37387069583848));
#54905=CARTESIAN_POINT('Ctrl Pts',(-0.322274981579892,2.09989103817067,
4.37437734492394));
#54906=CARTESIAN_POINT('',(-0.30265674053785,1.98927478592477,4.3567));
#54907=CARTESIAN_POINT('Origin',(0.,2.1,4.3567));
#54908=CARTESIAN_POINT('',(-0.322274978099547,2.0998811894946,4.4747226550683));
#54909=CARTESIAN_POINT('Ctrl Pts',(-0.302656740537849,1.98927478592477,
4.35670000000001));
#54910=CARTESIAN_POINT('Ctrl Pts',(-0.296404879462199,1.97218592399522,
4.35782329269583));
#54911=CARTESIAN_POINT('Ctrl Pts',(-0.288694193033434,1.95560777832229,
4.35894658539165));
#54912=CARTESIAN_POINT('Ctrl Pts',(-0.279632519152931,1.9397912928172,4.36006987808747));
#54913=CARTESIAN_POINT('Ctrl Pts',(-0.270577330574803,1.92398612693056,
4.36119236685978));
#54914=CARTESIAN_POINT('Ctrl Pts',(-0.260173420581183,1.90894216953555,
4.36231485563208));
#54915=CARTESIAN_POINT('Ctrl Pts',(-0.248574373589272,1.89488550412099,
4.36343734440438));
#54916=CARTESIAN_POINT('Ctrl Pts',(-0.23696239461704,1.88081316668436,4.36456108465904));
#54917=CARTESIAN_POINT('Ctrl Pts',(-0.224153067988682,1.86773088506809,
4.3656848249137));
#54918=CARTESIAN_POINT('Ctrl Pts',(-0.21034067269066,1.85583207205482,4.36680856516836));
#54919=CARTESIAN_POINT('Ctrl Pts',(-0.196522621340862,1.84392838658454,
4.36793276558456));
#54920=CARTESIAN_POINT('Ctrl Pts',(-0.181701252710663,1.83320958091786,
4.36905696600076));
#54921=CARTESIAN_POINT('Ctrl Pts',(-0.166103519464854,1.8238283207018,4.37018116641696));
#54922=CARTESIAN_POINT('Ctrl Pts',(-0.150460516351211,1.81441983291341,
4.37130862964087));
#54923=CARTESIAN_POINT('Ctrl Pts',(-0.134037286039767,1.80635699061725,
4.37243609286478));
#54924=CARTESIAN_POINT('Ctrl Pts',(-0.117086170482513,1.79974676636755,
4.37356355608868));
#54925=CARTESIAN_POINT('Ctrl Pts',(-0.102017415490227,1.79387058380445,
4.37456581856672));
#54926=CARTESIAN_POINT('Ctrl Pts',(-0.086532162885214,1.7891417213372,4.37556808104475));
#54927=CARTESIAN_POINT('Ctrl Pts',(-0.070816614222938,1.78560187218274,
4.37657034352279));
#54928=CARTESIAN_POINT('Ctrl Pts',(-0.0537834963462461,1.78176524711737,
4.37765663425935));
#54929=CARTESIAN_POINT('Ctrl Pts',(-0.036373093928319,1.77930248748307,
4.37874292499591));
#54930=CARTESIAN_POINT('Ctrl Pts',(-0.0188326652239015,1.77827572931847,
4.37982921573246));
#54931=CARTESIAN_POINT('Ctrl Pts',(-0.00132981533986302,1.77725117089261,
4.380913179187));
#54932=CARTESIAN_POINT('Ctrl Pts',(0.0163017347981785,1.77765663538176,
4.38199714264153));
#54933=CARTESIAN_POINT('Ctrl Pts',(0.0338062062375431,1.77950301710496,
4.38308110609606));
#54934=CARTESIAN_POINT('Ctrl Pts',(0.0517843956155461,1.781399366869,4.38419440450852));
#54935=CARTESIAN_POINT('Ctrl Pts',(0.0696276570204186,1.78481592139951,
4.38530770292098));
#54936=CARTESIAN_POINT('Ctrl Pts',(0.0870607697616642,1.78970723825151,
4.38642100133344));
#54937=CARTESIAN_POINT('Ctrl Pts',(0.104020876238972,1.79446584079458,4.38750409302777));
#54938=CARTESIAN_POINT('Ctrl Pts',(0.120592055650822,1.80061981374593,4.3885871847221));
#54939=CARTESIAN_POINT('Ctrl Pts',(0.136534628114959,1.80807625833018,4.38967027641643));
#54940=CARTESIAN_POINT('Ctrl Pts',(0.153144142439005,1.81584463594973,4.39079867818795));
#54941=CARTESIAN_POINT('Ctrl Pts',(0.169070369245532,1.82502664665808,4.39192707995948));
#54942=CARTESIAN_POINT('Ctrl Pts',(0.184070819008737,1.83546435171332,4.393055481731));
#54943=CARTESIAN_POINT('Ctrl Pts',(0.199071268771941,1.84590205676856,4.39418388350253));
#54944=CARTESIAN_POINT('Ctrl Pts',(0.213145247532986,1.85759478899131,4.39531228527405));
#54945=CARTESIAN_POINT('Ctrl Pts',(0.226090844627291,1.87033915091876,4.39644068704558));
#54946=CARTESIAN_POINT('Ctrl Pts',(0.238695992515106,1.88274835581375,4.39753941359356));
#54947=CARTESIAN_POINT('Ctrl Pts',(0.250315384053979,1.89623671552766,4.39863814014154));
#54948=CARTESIAN_POINT('Ctrl Pts',(0.260762804773581,1.91062224187721,4.39973686668952));
#54949=CARTESIAN_POINT('Ctrl Pts',(0.271190233577476,1.92498024045335,4.40083349074262));
#54950=CARTESIAN_POINT('Ctrl Pts',(0.280449643884497,1.94023141810416,4.40193011479572));
#54951=CARTESIAN_POINT('Ctrl Pts',(0.288394111067946,1.95615976805383,4.40302673884883));
#54952=CARTESIAN_POINT('Ctrl Pts',(0.296413922667818,1.9722391806492,4.40413376315879));
#54953=CARTESIAN_POINT('Ctrl Pts',(0.303093248446507,1.98900802855614,4.40524078746875));
#54954=CARTESIAN_POINT('Ctrl Pts',(0.308327722020033,2.00621731791563,4.40634781177871));
#54955=CARTESIAN_POINT('Ctrl Pts',(0.313510317810215,2.02325604957294,4.40744386460004));
#54956=CARTESIAN_POINT('Ctrl Pts',(0.317276412305712,2.04072576159458,4.40853991742137));
#54957=CARTESIAN_POINT('Ctrl Pts',(0.319574828048716,2.05836942346504,4.4096359702427));
#54958=CARTESIAN_POINT('Ctrl Pts',(0.321907754503758,2.07627800491584,4.41074848029698));
#54959=CARTESIAN_POINT('Ctrl Pts',(0.322728416857932,2.09436499939892,4.41186099035126));
#54960=CARTESIAN_POINT('Ctrl Pts',(0.32203798925476,2.11235755241749,4.41297350040554));
#54961=CARTESIAN_POINT('Ctrl Pts',(0.321347561651589,2.13035010543605,4.41408601045981));
#54962=CARTESIAN_POINT('Ctrl Pts',(0.319146197115451,2.14824740746737,4.41519852051409));
#54963=CARTESIAN_POINT('Ctrl Pts',(0.315489363474537,2.16578477908629,4.41631103056837));
#54964=CARTESIAN_POINT('Ctrl Pts',(0.311876365368133,2.18311192510176,4.41741020463921));
#54965=CARTESIAN_POINT('Ctrl Pts',(0.306820812234803,2.2001926869356,4.41850937871005));
#54966=CARTESIAN_POINT('Ctrl Pts',(0.300375610800813,2.21677186331064,4.41960855278089));
#54967=CARTESIAN_POINT('Ctrl Pts',(0.29394238844351,2.23332022556338,4.42070568392248));
#54968=CARTESIAN_POINT('Ctrl Pts',(0.286124863992888,2.24936812040546,4.42180281506408));
#54969=CARTESIAN_POINT('Ctrl Pts',(0.277025776962371,2.26467511810651,4.42289994620567));
#54970=CARTESIAN_POINT('Ctrl Pts',(0.267846619944137,2.28011681405958,4.4240067318628));
#54971=CARTESIAN_POINT('Ctrl Pts',(0.257363532542741,2.29480376905319,4.42511351751992));
#54972=CARTESIAN_POINT('Ctrl Pts',(0.245729626709979,2.30851409108733,4.42622030317704));
#54973=CARTESIAN_POINT('Ctrl Pts',(0.234201794628709,2.32209940735701,4.42731699756229));
#54974=CARTESIAN_POINT('Ctrl Pts',(0.221544601532698,2.33472527546789,4.42841369194754));
#54975=CARTESIAN_POINT('Ctrl Pts',(0.207946939793699,2.34620975987039,4.42951038633278));
#54976=CARTESIAN_POINT('Ctrl Pts',(0.194161599012098,2.35785275660235,4.43062221762585));
#54977=CARTESIAN_POINT('Ctrl Pts',(0.179410229651956,2.36832207423201,4.43173404891891));
#54978=CARTESIAN_POINT('Ctrl Pts',(0.163922416644867,2.37747183090596,4.43284588021197));
#54979=CARTESIAN_POINT('Ctrl Pts',(0.148434603637777,2.38662158757992,4.43395771150504));
#54980=CARTESIAN_POINT('Ctrl Pts',(0.132211106067836,2.39445147857908,4.4350695427981));
#54981=CARTESIAN_POINT('Ctrl Pts',(0.115503787987989,2.40086550248479,4.43618137409116));
#54982=CARTESIAN_POINT('Ctrl Pts',(0.0990367795359562,2.40718727030906,
4.43727721336426));
#54983=CARTESIAN_POINT('Ctrl Pts',(0.081996347123964,2.4121733903919,4.43837305263736));
#54984=CARTESIAN_POINT('Ctrl Pts',(0.0646237538508256,2.41572922902897,
4.43946889191047));
#54985=CARTESIAN_POINT('Ctrl Pts',(0.0472848784563243,2.41927816625911,
4.44056260430619));
#54986=CARTESIAN_POINT('Ctrl Pts',(0.0296158596789326,2.42140211334889,
4.44165631670191));
#54987=CARTESIAN_POINT('Ctrl Pts',(0.011872857537185,2.42205622316437,4.44275002909764));
#54988=CARTESIAN_POINT('Ctrl Pts',(-0.00610961883994167,2.42271916138707,
4.44385850314066));
#54989=CARTESIAN_POINT('Ctrl Pts',(-0.0241672924948265,2.42187210391943,
4.44496697718369));
#54990=CARTESIAN_POINT('Ctrl Pts',(-0.042028264297906,2.41952277011992,
4.44607545122672));
#54991=CARTESIAN_POINT('Ctrl Pts',(-0.0596422300846304,2.41720592613055,
4.44716859577028));
#54992=CARTESIAN_POINT('Ctrl Pts',(-0.0770641265237543,2.41342829230801,
4.44826174031385));
#54993=CARTESIAN_POINT('Ctrl Pts',(-0.0940399066885015,2.40824936589557,
4.44935488485742));
#54994=CARTESIAN_POINT('Ctrl Pts',(-0.111372771670244,2.40296150098531,
4.45047102365017));
#54995=CARTESIAN_POINT('Ctrl Pts',(-0.128239712338758,2.39621289405118,
4.45158716244293));
#54996=CARTESIAN_POINT('Ctrl Pts',(-0.144389702293705,2.38811940145803,
4.45270330123568));
#54997=CARTESIAN_POINT('Ctrl Pts',(-0.160539692248653,2.38002590886489,
4.45381944002844));
#54998=CARTESIAN_POINT('Ctrl Pts',(-0.175972035610441,2.37058802489359,
4.4549355788212));
#54999=CARTESIAN_POINT('Ctrl Pts',(-0.190466496365977,2.3599686315444,4.45605171761395));
#55000=CARTESIAN_POINT('Ctrl Pts',(-0.204594111146087,2.34961800857428,
4.45713960761353));
#55001=CARTESIAN_POINT('Ctrl Pts',(-0.217923393648165,2.33807715066765,
4.4582274976131));
#55002=CARTESIAN_POINT('Ctrl Pts',(-0.230246003460366,2.3254949079592,4.45931538761268));
#55003=CARTESIAN_POINT('Ctrl Pts',(-0.242545064567707,2.31293671011825,
4.46040119863703));
#55004=CARTESIAN_POINT('Ctrl Pts',(-0.253840676982854,2.29934158552362,
4.46148700966138));
#55005=CARTESIAN_POINT('Ctrl Pts',(-0.263958165993931,2.28489797789625,
4.46257282068573));
#55006=CARTESIAN_POINT('Ctrl Pts',(-0.274073351784462,2.27045765831928,
4.46365838452797));
#55007=CARTESIAN_POINT('Ctrl Pts',(-0.283010453362923,2.25516985310587,
4.46474394837021));
#55008=CARTESIAN_POINT('Ctrl Pts',(-0.290635823550638,2.23925513884249,
4.46582951221245));
#55009=CARTESIAN_POINT('Ctrl Pts',(-0.298259388333677,2.22334419259285,
4.46691481903346));
#55010=CARTESIAN_POINT('Ctrl Pts',(-0.304571509155866,2.20680734850197,
4.46800012585447));
#55011=CARTESIAN_POINT('Ctrl Pts',(-0.309485782603731,2.18988729604987,
4.46908543267548));
#55012=CARTESIAN_POINT('Ctrl Pts',(-0.31441066678873,2.17293071037861,4.47017308285518));
#55013=CARTESIAN_POINT('Ctrl Pts',(-0.317931490025487,2.15559003286069,
4.47126073303488));
#55014=CARTESIAN_POINT('Ctrl Pts',(-0.32001248200996,2.13812068969503,4.47234838321458));
#55015=CARTESIAN_POINT('Ctrl Pts',(-0.321526706831123,2.12540919766228,
4.47313980716582));
#55016=CARTESIAN_POINT('Ctrl Pts',(-0.322279678047781,2.11262985771029,
4.47393123111706));
#55017=CARTESIAN_POINT('Ctrl Pts',(-0.322274978099547,2.0998811894946,4.4747226550683));
#55018=CARTESIAN_POINT('',(-0.322274995052385,2.09994352890236,4.72441933817791));
#55019=CARTESIAN_POINT('Ctrl Pts',(-0.322274984171188,2.09989899277133,
4.47499672223609));
#55020=CARTESIAN_POINT('Ctrl Pts',(-0.322273429072572,2.09493727479805,
4.4753190331803));
#55021=CARTESIAN_POINT('Ctrl Pts',(-0.322157288520209,2.08997587454079,
4.47563692052927));
#55022=CARTESIAN_POINT('Ctrl Pts',(-0.32189880254931,2.08442135331536,4.47598643353917));
#55023=CARTESIAN_POINT('Ctrl Pts',(-0.321869337429171,2.0838240007594,4.47602393855795));
#55024=CARTESIAN_POINT('Ctrl Pts',(-0.321820232419069,2.08288179528726,
4.47608296095535));
#55025=CARTESIAN_POINT('Ctrl Pts',(-0.32180170090614,2.08253688964145,4.4761045384053));
#55026=CARTESIAN_POINT('Ctrl Pts',(-0.321769318457598,2.08195175283111,
4.47614109585607));
#55027=CARTESIAN_POINT('Ctrl Pts',(-0.321755752949808,2.08171150713891,
4.47615609161978));
#55028=CARTESIAN_POINT('Ctrl Pts',(-0.321730105701105,2.08126615564203,
4.47618386351632));
#55029=CARTESIAN_POINT('Ctrl Pts',(-0.321718096881468,2.08106104600555,
4.47619664372542));
#55030=CARTESIAN_POINT('Ctrl Pts',(-0.321693417195328,2.08064631666016,
4.47622246409026));
#55031=CARTESIAN_POINT('Ctrl Pts',(-0.321680737662999,2.08043669908492,
4.47623550361519));
#55032=CARTESIAN_POINT('Ctrl Pts',(-0.321650685303944,2.07994780398357,
4.47626589056541));
#55033=CARTESIAN_POINT('Ctrl Pts',(-0.32163315366901,2.07966853709335,4.47628322893535));
#55034=CARTESIAN_POINT('Ctrl Pts',(-0.321578713976487,2.0788190448839,4.47633591222419));
#55035=CARTESIAN_POINT('Ctrl Pts',(-0.321540652791955,2.07824889068717,
4.47637119260462));
#55036=CARTESIAN_POINT('Ctrl Pts',(-0.321258436483804,2.07418401106051,
4.47662217694601));
#55037=CARTESIAN_POINT('Ctrl Pts',(-0.32095881712453,2.07069320152637,4.47683484267544));
#55038=CARTESIAN_POINT('Ctrl Pts',(-0.320499294592935,2.06620054785817,
4.47710563012839));
#55039=CARTESIAN_POINT('Ctrl Pts',(-0.320391522006456,2.06519377243649,
4.47716612289197));
#55040=CARTESIAN_POINT('Ctrl Pts',(-0.320124646487641,2.06280704580368,
4.4773091175874));
#55041=CARTESIAN_POINT('Ctrl Pts',(-0.319961361917081,2.06142757289138,
4.47739143708493));
#55042=CARTESIAN_POINT('Ctrl Pts',(-0.317109083622791,2.03859631139614,
4.47874907546743));
#55043=CARTESIAN_POINT('Ctrl Pts',(-0.31227681142198,2.01746528692992,4.47993814989359));
#55044=CARTESIAN_POINT('Ctrl Pts',(-0.297966718749578,1.97505017629298,
4.48244714670141));
#55045=CARTESIAN_POINT('Ctrl Pts',(-0.288231033890626,1.95398885226982,
4.48376561588582));
#55046=CARTESIAN_POINT('Ctrl Pts',(-0.275733533737731,1.93316619672375,
4.48524244698808));
#55047=CARTESIAN_POINT('Ctrl Pts',(-0.275136137255755,1.93218282130435,
4.48531260848586));
#55048=CARTESIAN_POINT('Ctrl Pts',(-0.274257707511894,1.93075413522918,
4.48541515868244));
#55049=CARTESIAN_POINT('Ctrl Pts',(-0.27398082402183,1.93030627314239,4.48544739485242));
#55050=CARTESIAN_POINT('Ctrl Pts',(-0.273493376315486,1.92952212412634,
4.48550399324385));
#55051=CARTESIAN_POINT('Ctrl Pts',(-0.27328328577089,1.92918554286353,4.48552833795757));
#55052=CARTESIAN_POINT('Ctrl Pts',(-0.272874444355994,1.9285332322881,4.48557561846849));
#55053=CARTESIAN_POINT('Ctrl Pts',(-0.272675765644358,1.92821745827761,
4.48559855157041));
#55054=CARTESIAN_POINT('Ctrl Pts',(-0.272200589289356,1.92746512860334,
4.48565329808707));
#55055=CARTESIAN_POINT('Ctrl Pts',(-0.271923589736859,1.92702889259477,
4.48568513008761));
#55056=CARTESIAN_POINT('Ctrl Pts',(-0.271084245857539,1.92571404109614,
4.48578133984946));
#55057=CARTESIAN_POINT('Ctrl Pts',(-0.270518687710994,1.92483749436224,
4.48584583711899));
#55058=CARTESIAN_POINT('Ctrl Pts',(-0.264558489828369,1.9156976240433,4.48652215719101));
#55059=CARTESIAN_POINT('Ctrl Pts',(-0.258791805671756,1.90768430292009,
4.48714796730868));
#55060=CARTESIAN_POINT('Ctrl Pts',(-0.234716198265635,1.87727652148885,
4.48965945756845));
#55061=CARTESIAN_POINT('Ctrl Pts',(-0.213795990968193,1.85712577176646,
4.49164875303043));
#55062=CARTESIAN_POINT('Ctrl Pts',(-0.183586135610912,1.83499029574287,
4.49415043452161));
#55063=CARTESIAN_POINT('Ctrl Pts',(-0.176487091884017,1.83020992720397,
4.49471436695229));
#55064=CARTESIAN_POINT('Ctrl Pts',(-0.16724144964405,1.82450626449113,4.49541179000964));
#55065=CARTESIAN_POINT('Ctrl Pts',(-0.165264447753006,1.82331576881747,
4.49555883752627));
#55066=CARTESIAN_POINT('Ctrl Pts',(-0.162478947992507,1.82167892802945,
4.49576294005663));
#55067=CARTESIAN_POINT('Ctrl Pts',(-0.161681113409922,1.82121469683959,
4.49582105017541));
#55068=CARTESIAN_POINT('Ctrl Pts',(-0.160473232347745,1.82051880367673,
4.49590848614731));
#55069=CARTESIAN_POINT('Ctrl Pts',(-0.160064662739322,1.82028460688197,
4.49593796883971));
#55070=CARTESIAN_POINT('Ctrl Pts',(-0.159313690036746,1.81985632490354,
4.49599198735746));
#55071=CARTESIAN_POINT('Ctrl Pts',(-0.158971442788583,1.81966197027282,
4.49601654022928));
#55072=CARTESIAN_POINT('Ctrl Pts',(-0.158420205062174,1.8193502686648,4.49605597983617));
#55073=CARTESIAN_POINT('Ctrl Pts',(-0.158211439573286,1.81923252777519,
4.49607089198801));
#55074=CARTESIAN_POINT('Ctrl Pts',(-0.157820996831486,1.81901289714336,
4.49609873538693));
#55075=CARTESIAN_POINT('Ctrl Pts',(-0.157639353556617,1.81891095143494,
4.49611167019485));
#55076=CARTESIAN_POINT('Ctrl Pts',(-0.157216061234975,1.81867392165739,
4.49614176966104));
#55077=CARTESIAN_POINT('Ctrl Pts',(-0.156974337243435,1.81853897301005,
4.49615892548677));
#55078=CARTESIAN_POINT('Ctrl Pts',(-0.156351449984595,1.8181922821646,4.49620305022385));
#55079=CARTESIAN_POINT('Ctrl Pts',(-0.155970028786825,1.81798100087157,
4.4962299895395));
#55080=CARTESIAN_POINT('Ctrl Pts',(-0.153731161948265,1.81674675285051,
4.49638765529263));
#55081=CARTESIAN_POINT('Ctrl Pts',(-0.151864029219147,1.81574133369301,
4.49651727847567));
#55082=CARTESIAN_POINT('Ctrl Pts',(-0.133210569991579,1.8059330239884,4.49779520521927));
#55083=CARTESIAN_POINT('Ctrl Pts',(-0.115685945269864,1.79860753928493,
4.49886054912733));
#55084=CARTESIAN_POINT('Ctrl Pts',(-0.0958487973092332,1.79230270555119,
4.50002506625158));
#55085=CARTESIAN_POINT('Ctrl Pts',(-0.0940760399937242,1.79175607763204,
4.50012876922808));
#55086=CARTESIAN_POINT('Ctrl Pts',(-0.0902724485436537,1.7906191133431,
4.50035065485709));
#55087=CARTESIAN_POINT('Ctrl Pts',(-0.088240325712086,1.7900334003384,4.50046882658662));
#55088=CARTESIAN_POINT('Ctrl Pts',(-0.0838379982918046,1.78881133085156,
4.50072425673073));
#55089=CARTESIAN_POINT('Ctrl Pts',(-0.0814659975071729,1.78818196181416,
4.50086152785652));
#55090=CARTESIAN_POINT('Ctrl Pts',(-0.0762568713917799,1.78686330720148,
4.50116255987996));
#55091=CARTESIAN_POINT('Ctrl Pts',(-0.0734171113129211,1.78618536310497,
4.50132639265848));
#55092=CARTESIAN_POINT('Ctrl Pts',(-0.0512738315672547,1.7812160521037,
4.50260372406697));
#55093=CARTESIAN_POINT('Ctrl Pts',(-0.031624580851592,1.77867162528165,
4.50373981570125));
#55094=CARTESIAN_POINT('Ctrl Pts',(-0.0102723125877482,1.77788479691748,
4.50503521350223));
#55095=CARTESIAN_POINT('Ctrl Pts',(-0.00867649551879349,1.77783786264474,
4.5051323690496));
#55096=CARTESIAN_POINT('Ctrl Pts',(-0.00647980535113511,1.77778958946529,
4.50526659622268));
#55097=CARTESIAN_POINT('Ctrl Pts',(-0.00587916056410101,1.77777807027193,
4.50530334853987));
#55098=CARTESIAN_POINT('Ctrl Pts',(-0.00486822641532941,1.77776151012307,
4.50536529165778));
#55099=CARTESIAN_POINT('Ctrl Pts',(-0.00445795161193327,1.77775557312569,
4.50539045431464));
#55100=CARTESIAN_POINT('Ctrl Pts',(-0.00364843140309706,1.77774540501589,
4.50544015063562));
#55101=CARTESIAN_POINT('Ctrl Pts',(-0.00324918718173291,1.77774113228578,
4.50546468294935));
#55102=CARTESIAN_POINT('Ctrl Pts',(-0.00237200160275339,1.77773337486801,
4.50551863373672));
#55103=CARTESIAN_POINT('Ctrl Pts',(-0.00189405898876175,1.77773021146533,
4.50554806223401));
#55104=CARTESIAN_POINT('Ctrl Pts',(-0.000238787662817182,1.77772293794388,
4.50565009784488));
#55105=CARTESIAN_POINT('Ctrl Pts',(0.000938544586681608,1.77772421620278,
4.5057228736675));
#55106=CARTESIAN_POINT('Ctrl Pts',(0.0126705599419939,1.77780124202494,
4.50645013273548));
#55107=CARTESIAN_POINT('Ctrl Pts',(0.0232143808413407,1.77838900303163,
4.50712063283737));
#55108=CARTESIAN_POINT('Ctrl Pts',(0.0492137169969657,1.78112349321522,
4.50881827390047));
#55109=CARTESIAN_POINT('Ctrl Pts',(0.064577608017244,1.78387683625848,4.50986148372357));
#55110=CARTESIAN_POINT('Ctrl Pts',(0.0946031864249646,1.79153833225944,
4.51195559625379));
#55111=CARTESIAN_POINT('Ctrl Pts',(0.109234244934967,1.7964110092605,4.51300343283825));
#55112=CARTESIAN_POINT('Ctrl Pts',(0.12926124482282,1.80471685903077,4.51443735080164));
#55113=CARTESIAN_POINT('Ctrl Pts',(0.134990194753682,1.8072915083247,4.51484732751742));
#55114=CARTESIAN_POINT('Ctrl Pts',(0.142387251647469,1.8108792387982,4.51537312621331));
#55115=CARTESIAN_POINT('Ctrl Pts',(0.144126236527113,1.8117421772867,4.51549647230797));
#55116=CARTESIAN_POINT('Ctrl Pts',(0.146582072772296,1.81298862033187,4.5156701764144));
#55117=CARTESIAN_POINT('Ctrl Pts',(0.147305395143184,1.81335918519505,4.51572127722593));
#55118=CARTESIAN_POINT('Ctrl Pts',(0.14840861895822,1.81392965600966,4.51579911536518));
#55119=CARTESIAN_POINT('Ctrl Pts',(0.14878952920448,1.81412758808173,4.51582597194781));
#55120=CARTESIAN_POINT('Ctrl Pts',(0.149493707965175,1.81449528861242,4.51587558494555));
#55121=CARTESIAN_POINT('Ctrl Pts',(0.14981708495877,1.81466484618385,4.51589835439699));
#55122=CARTESIAN_POINT('Ctrl Pts',(0.150346248052047,1.81494345199662,4.51593558954295));
#55123=CARTESIAN_POINT('Ctrl Pts',(0.150552204228655,1.81505217378326,4.51595007590823));
#55124=CARTESIAN_POINT('Ctrl Pts',(0.150949392889979,1.81526239573457,4.51597800122498));
#55125=CARTESIAN_POINT('Ctrl Pts',(0.151140640615144,1.81536386516929,4.51599144205147));
#55126=CARTESIAN_POINT('Ctrl Pts',(0.151586931768654,1.81560122845572,4.51602279514631));
#55127=CARTESIAN_POINT('Ctrl Pts',(0.151841895716483,1.81573727320361,4.51604069778581));
#55128=CARTESIAN_POINT('Ctrl Pts',(0.15265736176679,1.81617380322568,4.5160979283893));
#55129=CARTESIAN_POINT('Ctrl Pts',(0.153217161984782,1.81647560710487,4.51613717290932));
#55130=CARTESIAN_POINT('Ctrl Pts',(0.158258887874711,1.81921303471953,4.5164902647909));
#55131=CARTESIAN_POINT('Ctrl Pts',(0.162683595728975,1.82175325649428,4.51679760408254));
#55132=CARTESIAN_POINT('Ctrl Pts',(0.167433248370488,1.82463208689165,4.51712678488508));
#55133=CARTESIAN_POINT('Ctrl Pts',(0.167819580790366,1.82486736191966,4.51715355479696));
#55134=CARTESIAN_POINT('Ctrl Pts',(0.192055871337686,1.83969721484594,4.51883269213715));
#55135=CARTESIAN_POINT('Ctrl Pts',(0.213908211452221,1.85733426529815,4.52034026122556));
#55136=CARTESIAN_POINT('Ctrl Pts',(0.243831900989314,1.8887087619504,4.52280023365836));
#55137=CARTESIAN_POINT('Ctrl Pts',(0.253640194960309,1.90058951255121,4.52369215267718));
#55138=CARTESIAN_POINT('Ctrl Pts',(0.263980035772892,1.91511706693387,4.5247677908075));
#55139=CARTESIAN_POINT('Ctrl Pts',(0.265375582445543,1.91712584119527,4.52491617885086));
#55140=CARTESIAN_POINT('Ctrl Pts',(0.267145037090441,1.91973573532518,4.52510860594292));
#55141=CARTESIAN_POINT('Ctrl Pts',(0.267540043399601,1.92032250801508,4.52515184499288));
#55142=CARTESIAN_POINT('Ctrl Pts',(0.268174319801933,1.92127143980358,4.52522173536099));
#55143=CARTESIAN_POINT('Ctrl Pts',(0.268414797074188,1.92163279242019,4.52524834117387));
#55144=CARTESIAN_POINT('Ctrl Pts',(0.268872018326673,1.92232285342988,4.52529913377999));
#55145=CARTESIAN_POINT('Ctrl Pts',(0.269088891529336,1.9226514756033,4.52532331566262));
#55146=CARTESIAN_POINT('Ctrl Pts',(0.269582789506912,1.92340285762271,4.52537859183644));
#55147=CARTESIAN_POINT('Ctrl Pts',(0.269859422537255,1.92382587262208,4.52540970071205));
#55148=CARTESIAN_POINT('Ctrl Pts',(0.270702959103565,1.92512241996806,4.5255050185312));
#55149=CARTESIAN_POINT('Ctrl Pts',(0.271266620592019,1.92599804432972,4.52556934810237));
#55150=CARTESIAN_POINT('Ctrl Pts',(0.275411781158541,1.93250647161751,4.5260472057192));
#55151=CARTESIAN_POINT('Ctrl Pts',(0.278821521692072,1.93824623788067,4.52646703391546));
#55152=CARTESIAN_POINT('Ctrl Pts',(0.282338608137678,1.94460874914244,4.52693120093886));
#55153=CARTESIAN_POINT('Ctrl Pts',(0.282625354636898,1.94513089592826,4.52696928421607));
#55154=CARTESIAN_POINT('Ctrl Pts',(0.284963396136583,1.94941643697788,4.52728178022675));
#55155=CARTESIAN_POINT('Ctrl Pts',(0.286940797829966,1.95321947514137,4.52755863460151));
#55156=CARTESIAN_POINT('Ctrl Pts',(0.301071213224542,1.98177322304823,4.52963367474962));
#55157=CARTESIAN_POINT('Ctrl Pts',(0.310077764914263,2.00795189407541,4.53153000844516));
#55158=CARTESIAN_POINT('Ctrl Pts',(0.317760004095797,2.04522883458338,4.53407014202454));
#55159=CARTESIAN_POINT('Ctrl Pts',(0.319375124750885,2.05560541692728,4.53475915640031));
#55160=CARTESIAN_POINT('Ctrl Pts',(0.320585116538556,2.06702525761937,4.53548524260158));
#55161=CARTESIAN_POINT('Ctrl Pts',(0.320684642660192,2.0680076477637,4.53554744368912));
#55162=CARTESIAN_POINT('Ctrl Pts',(0.320827258125165,2.06948294182772,4.53564044721951));
#55163=CARTESIAN_POINT('Ctrl Pts',(0.320873728940259,2.06997550201573,4.53567143062338));
#55164=CARTESIAN_POINT('Ctrl Pts',(0.320946794833823,2.07076950086914,4.53572126378663));
#55165=CARTESIAN_POINT('Ctrl Pts',(0.320974099721045,2.07107087101923,4.53574015256685));
#55166=CARTESIAN_POINT('Ctrl Pts',(0.321025765019208,2.07165019105327,4.53577641188889));
#55167=CARTESIAN_POINT('Ctrl Pts',(0.321050189003121,2.07192813479736,4.53579378597075));
#55168=CARTESIAN_POINT('Ctrl Pts',(0.321092794384865,2.072420311015,4.5358245117469));
#55169=CARTESIAN_POINT('Ctrl Pts',(0.321111122356962,2.07263452996741,4.53583787172114));
#55170=CARTESIAN_POINT('Ctrl Pts',(0.321147282533309,2.07306221185723,4.53586451770843));
#55171=CARTESIAN_POINT('Ctrl Pts',(0.321165116224875,2.0732756734519,4.53587780377392));
#55172=CARTESIAN_POINT('Ctrl Pts',(0.321213828891136,2.0738658344423,4.53591449963487));
#55173=CARTESIAN_POINT('Ctrl Pts',(0.321244258151676,2.07424257217133,4.53593788402296));
#55174=CARTESIAN_POINT('Ctrl Pts',(0.321360996281057,2.07572027075689,4.53602944836725));
#55175=CARTESIAN_POINT('Ctrl Pts',(0.321442310019689,2.0768216351914,4.53609735070477));
#55176=CARTESIAN_POINT('Ctrl Pts',(0.322866683562374,2.09756586122998,4.53737020625869));
#55177=CARTESIAN_POINT('Ctrl Pts',(0.322412765451218,2.11729400059599,4.53847928736019));
#55178=CARTESIAN_POINT('Ctrl Pts',(0.318285467855231,2.15314316759343,4.5404992695517));
#55179=CARTESIAN_POINT('Ctrl Pts',(0.315171292177117,2.1692594025311,4.54140942897139));
#55180=CARTESIAN_POINT('Ctrl Pts',(0.309294688855034,2.19073292954909,4.54268546926145));
#55181=CARTESIAN_POINT('Ctrl Pts',(0.307589917170555,2.19635406947532,4.54302543240003));
#55182=CARTESIAN_POINT('Ctrl Pts',(0.303401872052834,2.20891642579411,4.5438019245872));
#55183=CARTESIAN_POINT('Ctrl Pts',(0.300832208524172,2.21582509775483,4.54424077320023));
#55184=CARTESIAN_POINT('Ctrl Pts',(0.297434067949031,2.22408298909304,4.54478229419096));
#55185=CARTESIAN_POINT('Ctrl Pts',(0.296829492135799,2.22552237021234,4.5448773173132));
#55186=CARTESIAN_POINT('Ctrl Pts',(0.295979786774727,2.22750488776175,4.54500909465397));
#55187=CARTESIAN_POINT('Ctrl Pts',(0.295743566719805,2.22805183840413,4.54504554525152));
#55188=CARTESIAN_POINT('Ctrl Pts',(0.295342401668063,2.22897367618259,4.54510714119497));
#55189=CARTESIAN_POINT('Ctrl Pts',(0.295178255578197,2.22934891109889,4.54513225920044));
#55190=CARTESIAN_POINT('Ctrl Pts',(0.294852143655695,2.23009054341848,4.54518199379408));
#55191=CARTESIAN_POINT('Ctrl Pts',(0.294690209042942,2.23045695380928,4.54520660927791));
#55192=CARTESIAN_POINT('Ctrl Pts',(0.294331918435954,2.23126358889178,4.54526089577067));
#55193=CARTESIAN_POINT('Ctrl Pts',(0.294135257366237,2.23170367629269,4.54529057720867));
#55194=CARTESIAN_POINT('Ctrl Pts',(0.293445449579098,2.23323807435634,4.54539428707664));
#55195=CARTESIAN_POINT('Ctrl Pts',(0.292947181853805,2.23433005962283,4.54546849143462));
#55196=CARTESIAN_POINT('Ctrl Pts',(0.287654945151131,2.24575884081851,4.54624934514555));
#55197=CARTESIAN_POINT('Ctrl Pts',(0.282322642950932,2.25583606772135,4.54697469429424));
#55198=CARTESIAN_POINT('Ctrl Pts',(0.262322469519647,2.28922447973946,4.5495104820285));
#55199=CARTESIAN_POINT('Ctrl Pts',(0.245209377628064,2.31092883693061,4.55140397180431));
#55200=CARTESIAN_POINT('Ctrl Pts',(0.218054649140363,2.33753633856572,4.55394146292063));
#55201=CARTESIAN_POINT('Ctrl Pts',(0.210202416086392,2.34451244356362,4.55463064573098));
#55202=CARTESIAN_POINT('Ctrl Pts',(0.201253644195357,2.35171237762961,4.55535686228635));
#55203=CARTESIAN_POINT('Ctrl Pts',(0.200481572377854,2.35232774233007,4.55541905704884));
#55204=CARTESIAN_POINT('Ctrl Pts',(0.199318475409572,2.35324605747116,4.55551204616128));
#55205=CARTESIAN_POINT('Ctrl Pts',(0.19892956934423,2.35355166477946,4.55554302159676));
#55206=CARTESIAN_POINT('Ctrl Pts',(0.198301694463696,2.3540427229659,4.55559283927684));
#55207=CARTESIAN_POINT('Ctrl Pts',(0.198063167304039,2.35422873338466,4.5556117205588));
#55208=CARTESIAN_POINT('Ctrl Pts',(0.197606777482922,2.35458360728011,4.55564776229534));
#55209=CARTESIAN_POINT('Ctrl Pts',(0.197388959546763,2.35475252747195,4.55566492675871));
#55210=CARTESIAN_POINT('Ctrl Pts',(0.197000773153382,2.3550527735061,4.55569545049949));
#55211=CARTESIAN_POINT('Ctrl Pts',(0.196830489941176,2.35518420822371,4.55570881755598));
#55212=CARTESIAN_POINT('Ctrl Pts',(0.196491025074465,2.35544568546526,4.55573542010897));
#55213=CARTESIAN_POINT('Ctrl Pts',(0.196321846496122,2.35557572996395,4.55574865576223));
#55214=CARTESIAN_POINT('Ctrl Pts',(0.195855732115731,2.35593328770389,4.55578506138897));
#55215=CARTESIAN_POINT('Ctrl Pts',(0.195558527953201,2.3561604530478,4.55580820661613));
#55216=CARTESIAN_POINT('Ctrl Pts',(0.194404023995219,2.35703970754884,4.55589785579956));
#55217=CARTESIAN_POINT('Ctrl Pts',(0.193543840227857,2.35768802414824,4.5559640965188));
#55218=CARTESIAN_POINT('Ctrl Pts',(0.192556592926056,2.35842437579343,4.55603951158739));
#55219=CARTESIAN_POINT('Ctrl Pts',(0.192432711236372,2.35851663607969,4.55604896387689));
#55220=CARTESIAN_POINT('Ctrl Pts',(0.176345220602216,2.37047974535436,4.55727504247922));
#55221=CARTESIAN_POINT('Ctrl Pts',(0.159314025071371,2.38084912082708,4.55839404301133));
#55222=CARTESIAN_POINT('Ctrl Pts',(0.123860509620407,2.3981646991722,4.56060192419195));
#55223=CARTESIAN_POINT('Ctrl Pts',(0.105544873422519,2.40512920851287,4.56168752404402));
#55224=CARTESIAN_POINT('Ctrl Pts',(0.0784877550954512,2.41268795239035,
4.56331861799718));
#55225=CARTESIAN_POINT('Ctrl Pts',(0.0701765878628224,2.41465745008404,
4.56382269244057));
#55226=CARTESIAN_POINT('Ctrl Pts',(0.0601589745572409,2.41661468814422,
4.56443808780219));
#55227=CARTESIAN_POINT('Ctrl Pts',(0.0585179834362899,2.41692208572791,
4.56453913935081));
#55228=CARTESIAN_POINT('Ctrl Pts',(0.0556504919857703,2.41743620655454,
4.56471617541852));
#55229=CARTESIAN_POINT('Ctrl Pts',(0.0544250360756299,2.41764860753722,
4.56479197898809));
#55230=CARTESIAN_POINT('Ctrl Pts',(0.0526624736373075,2.41794360309979,
4.56490122499572));
#55231=CARTESIAN_POINT('Ctrl Pts',(0.0521263292292006,2.41803194285645,
4.56493448492785));
#55232=CARTESIAN_POINT('Ctrl Pts',(0.0511957384668416,2.41818285857508,
4.56499226568274));
#55233=CARTESIAN_POINT('Ctrl Pts',(0.0508013932965448,2.41824605820809,
4.5650167666638));
#55234=CARTESIAN_POINT('Ctrl Pts',(0.0500430867522277,2.41836614266802,
4.56506391186514));
#55235=CARTESIAN_POINT('Ctrl Pts',(0.0496791430923102,2.41842313683033,
4.56508655257814));
#55236=CARTESIAN_POINT('Ctrl Pts',(0.0488217516405681,2.41855589999861,
4.56513992304476));
#55237=CARTESIAN_POINT('Ctrl Pts',(0.0483282249879684,2.41863114650362,
4.56517066930899));
#55238=CARTESIAN_POINT('Ctrl Pts',(0.0468705708701003,2.41884992607259,
4.56526155609528));
#55239=CARTESIAN_POINT('Ctrl Pts',(0.0459059712172327,2.41899023110956,
4.56532179868413));
#55240=CARTESIAN_POINT('Ctrl Pts',(0.0373567378187211,2.4201941720082,4.56585662154304));
#55241=CARTESIAN_POINT('Ctrl Pts',(0.0297376352563984,2.42099141814585,
4.56633957241109));
#55242=CARTESIAN_POINT('Ctrl Pts',(0.0164784128669503,2.42190272585278,
4.56719198240653));
#55243=CARTESIAN_POINT('Ctrl Pts',(0.010850083851793,2.42214154155815,4.56755750914741));
#55244=CARTESIAN_POINT('Ctrl Pts',(-0.0195724645750351,2.42263424223003,
4.56955242233473));
#55245=CARTESIAN_POINT('Ctrl Pts',(-0.044325918813064,2.42017325086526,
4.57125300857453));
#55246=CARTESIAN_POINT('Ctrl Pts',(-0.0771812358358951,2.41302123406358,
4.57350370546215));
#55247=CARTESIAN_POINT('Ctrl Pts',(-0.0857340532573378,2.41078760200592,
4.57408795793851));
#55248=CARTESIAN_POINT('Ctrl Pts',(-0.0979308668506281,2.40706035852617,
4.57490912655983));
#55249=CARTESIAN_POINT('Ctrl Pts',(-0.101655884504313,2.40584735252556,
4.57515824850686));
#55250=CARTESIAN_POINT('Ctrl Pts',(-0.105868682425279,2.40439002881244,
4.57543734981006));
#55251=CARTESIAN_POINT('Ctrl Pts',(-0.106378862062687,2.40421210573421,
4.57547110513695));
#55252=CARTESIAN_POINT('Ctrl Pts',(-0.1071463820999,2.40394226934598,4.57552181738757));
#55253=CARTESIAN_POINT('Ctrl Pts',(-0.107404053759997,2.40385131154815,
4.57553883065291));
#55254=CARTESIAN_POINT('Ctrl Pts',(-0.107865550050935,2.40368774350185,
4.57556928020374));
#55255=CARTESIAN_POINT('Ctrl Pts',(-0.108069416789901,2.40361525586942,
4.57558272374858));
#55256=CARTESIAN_POINT('Ctrl Pts',(-0.108478292294501,2.40346941054224,
4.57560967084974));
#55257=CARTESIAN_POINT('Ctrl Pts',(-0.108683298832308,2.40339605071521,
4.5756231742007));
#55258=CARTESIAN_POINT('Ctrl Pts',(-0.109260566270517,2.40318882034475,
4.57566117635787));
#55259=CARTESIAN_POINT('Ctrl Pts',(-0.109632656885098,2.4030544714603,4.57568564659828));
#55260=CARTESIAN_POINT('Ctrl Pts',(-0.111166901631901,2.4024973139853,4.57578644584669));
#55261=CARTESIAN_POINT('Ctrl Pts',(-0.112326884428536,2.40206849577114,
4.57586242131542));
#55262=CARTESIAN_POINT('Ctrl Pts',(-0.133710823667689,2.39402314489708,
4.5772591602468));
#55263=CARTESIAN_POINT('Ctrl Pts',(-0.153124142202206,2.38439673994208,
4.5784655144129));
#55264=CARTESIAN_POINT('Ctrl Pts',(-0.180830571058473,2.36699199969083,
4.58029457413922));
#55265=CARTESIAN_POINT('Ctrl Pts',(-0.189919716259851,2.3606049020487,4.58091404916114));
#55266=CARTESIAN_POINT('Ctrl Pts',(-0.208035118612865,2.34642300458966,
4.58221957665366));
#55267=CARTESIAN_POINT('Ctrl Pts',(-0.216994636469219,2.33857115186426,
4.58290627110753));
#55268=CARTESIAN_POINT('Ctrl Pts',(-0.229429862357396,2.32639211731332,
4.5839397048306));
#55269=CARTESIAN_POINT('Ctrl Pts',(-0.233261516908457,2.32244215351955,
4.58427042418844));
#55270=CARTESIAN_POINT('Ctrl Pts',(-0.237607693179668,2.31772595285347,
4.58466112546756));
#55271=CARTESIAN_POINT('Ctrl Pts',(-0.23822251863537,2.31705307644062,4.58471677159636));
#55272=CARTESIAN_POINT('Ctrl Pts',(-0.239155897709731,2.31602282610005,
4.58480182954323));
#55273=CARTESIAN_POINT('Ctrl Pts',(-0.239476526683884,2.31566733171502,
4.58483115362675));
#55274=CARTESIAN_POINT('Ctrl Pts',(-0.240032502258556,2.31504813045852,
4.58488218646046));
#55275=CARTESIAN_POINT('Ctrl Pts',(-0.240268209950572,2.31478474768886,
4.58490387997611));
#55276=CARTESIAN_POINT('Ctrl Pts',(-0.240758418379112,2.31423516584687,
4.58494911794823));
#55277=CARTESIAN_POINT('Ctrl Pts',(-0.241012843059035,2.31394889993752,
4.58497266554279));
#55278=CARTESIAN_POINT('Ctrl Pts',(-0.241633761859633,2.31324776011363,
4.58503030125001));
#55279=CARTESIAN_POINT('Ctrl Pts',(-0.241999697497565,2.31283239525246,
4.58506441260506));
#55280=CARTESIAN_POINT('Ctrl Pts',(-0.243394687857498,2.31124072570819,
4.58519500327344));
#55281=CARTESIAN_POINT('Ctrl Pts',(-0.244416237815886,2.31005789875355,
4.58529179347486));
#55282=CARTESIAN_POINT('Ctrl Pts',(-0.262445993604225,2.28887210903096,
4.58702105726295));
#55283=CARTESIAN_POINT('Ctrl Pts',(-0.276951741692165,2.26687637185957,
4.58876020289764));
#55284=CARTESIAN_POINT('Ctrl Pts',(-0.294170264108086,2.23221293817648,
4.59137692502761));
#55285=CARTESIAN_POINT('Ctrl Pts',(-0.299061372503493,2.22074235227141,
4.59222284591545));
#55286=CARTESIAN_POINT('Ctrl Pts',(-0.307044154341661,2.19853495494782,
4.59379613557797));
#55287=CARTESIAN_POINT('Ctrl Pts',(-0.310266642655159,2.18786308314059,
4.59452540731873));
#55288=CARTESIAN_POINT('Ctrl Pts',(-0.313100194145897,2.17635410698771,
4.59526905477803));
#55289=CARTESIAN_POINT('Ctrl Pts',(-0.313267899292191,2.17566309882598,
4.59531354140973));
#55290=CARTESIAN_POINT('Ctrl Pts',(-0.313504456451249,2.17467412485468,
4.59537697297875));
#55291=CARTESIAN_POINT('Ctrl Pts',(-0.313575171988812,2.17437661360702,
4.59539602424065));
#55292=CARTESIAN_POINT('Ctrl Pts',(-0.31369669186866,2.17386210667814,4.59542891724439));
#55293=CARTESIAN_POINT('Ctrl Pts',(-0.313747694693875,2.17364515848125,
4.59544277049775));
#55294=CARTESIAN_POINT('Ctrl Pts',(-0.313845525207081,2.17322707545613,
4.59546943527407));
#55295=CARTESIAN_POINT('Ctrl Pts',(-0.313892384510236,2.1730259489459,4.5954822486356));
#55296=CARTESIAN_POINT('Ctrl Pts',(-0.314003180742505,2.17254831941527,
4.59551264399341));
#55297=CARTESIAN_POINT('Ctrl Pts',(-0.314066945951606,2.17227177615401,
4.59553021603536));
#55298=CARTESIAN_POINT('Ctrl Pts',(-0.314290128697797,2.1712979817325,4.59559200017891));
#55299=CARTESIAN_POINT('Ctrl Pts',(-0.314447591796843,2.17060027784849,
4.59563610049465));
#55300=CARTESIAN_POINT('Ctrl Pts',(-0.316547933216148,2.1611474338762,4.59623140901051));
#55301=CARTESIAN_POINT('Ctrl Pts',(-0.318127068217185,2.15231448505691,
4.59676235231723));
#55302=CARTESIAN_POINT('Ctrl Pts',(-0.321279572688121,2.12913249526383,
4.59811708324573));
#55303=CARTESIAN_POINT('Ctrl Pts',(-0.322261603439283,2.11472339687742,
4.59892147974423));
#55304=CARTESIAN_POINT('Ctrl Pts',(-0.322299026505738,2.07400756785731,
4.60119725886281));
#55305=CARTESIAN_POINT('Ctrl Pts',(-0.319106828542065,2.04781913843993,
4.60267310959814));
#55306=CARTESIAN_POINT('Ctrl Pts',(-0.312368014685267,2.02068928395737,
4.60436678591414));
#55307=CARTESIAN_POINT('Ctrl Pts',(-0.311952714799364,2.01907120510316,
4.60446839672546));
#55308=CARTESIAN_POINT('Ctrl Pts',(-0.311362874120434,2.01684510702386,
4.60460903767301));
#55309=CARTESIAN_POINT('Ctrl Pts',(-0.311199090208047,2.01623424416204,
4.60464771926073));
#55310=CARTESIAN_POINT('Ctrl Pts',(-0.310935168011888,2.01526135469867,
4.60470946771727));
#55311=CARTESIAN_POINT('Ctrl Pts',(-0.310836192490293,2.0148990120487,4.60473249681103));
#55312=CARTESIAN_POINT('Ctrl Pts',(-0.310631776091599,2.01415577184085,
4.60477979934079));
#55313=CARTESIAN_POINT('Ctrl Pts',(-0.310526267584728,2.0137748936574,4.6048040749418));
#55314=CARTESIAN_POINT('Ctrl Pts',(-0.310281018652486,2.0128958509323,4.60486018306977));
#55315=CARTESIAN_POINT('Ctrl Pts',(-0.310140778941195,2.01239782791733,
4.60489203179511));
#55316=CARTESIAN_POINT('Ctrl Pts',(-0.309697752560719,2.01083893898023,
4.60499191439398));
#55317=CARTESIAN_POINT('Ctrl Pts',(-0.309390719785355,2.00977929724539,
4.60506008647354));
#55318=CARTESIAN_POINT('Ctrl Pts',(-0.304901515995812,1.99457843748915,
4.60604208251637));
#55319=CARTESIAN_POINT('Ctrl Pts',(-0.299759637922862,1.98074108866683,
4.60698767135027));
#55320=CARTESIAN_POINT('Ctrl Pts',(-0.286766629181926,1.95198390853262,
4.60906713271287));
#55321=CARTESIAN_POINT('Ctrl Pts',(-0.278655926364474,1.93722821147532,
4.61020604344051));
#55322=CARTESIAN_POINT('Ctrl Pts',(-0.259274656885136,1.90769674605257,
4.6125951384316));
#55323=CARTESIAN_POINT('Ctrl Pts',(-0.247801096856571,1.89312157228115,
4.61384048601969));
#55324=CARTESIAN_POINT('Ctrl Pts',(-0.234428109079249,1.87885363507568,
4.61507192906011));
#55325=CARTESIAN_POINT('Ctrl Pts',(-0.233714610064458,1.87809972023885,
4.61513703212251));
#55326=CARTESIAN_POINT('Ctrl Pts',(-0.232742862269487,1.87708281469978,
4.61522487493555));
#55327=CARTESIAN_POINT('Ctrl Pts',(-0.232487796699551,1.87681681105292,
4.61524785575522));
#55328=CARTESIAN_POINT('Ctrl Pts',(-0.232085083044099,1.87639826717924,
4.61528401846936));
#55329=CARTESIAN_POINT('Ctrl Pts',(-0.231937740557124,1.87624543535846,
4.6152972240691));
#55330=CARTESIAN_POINT('Ctrl Pts',(-0.231652795611825,1.87595045849294,
4.61532271309303));
#55331=CARTESIAN_POINT('Ctrl Pts',(-0.231515214329933,1.87580829565245,
4.61533499794245));
#55332=CARTESIAN_POINT('Ctrl Pts',(-0.231186110477615,1.87546885840849,
4.61536433146544));
#55333=CARTESIAN_POINT('Ctrl Pts',(-0.230994466437707,1.87527170249685,
4.61538137047583));
#55334=CARTESIAN_POINT('Ctrl Pts',(-0.230419757571968,1.87468197632246,
4.61543234139994));
#55335=CARTESIAN_POINT('Ctrl Pts',(-0.230035940138853,1.87429013595239,
4.61546621461641));
#55336=CARTESIAN_POINT('Ctrl Pts',(-0.226716140520434,1.87091820647289,
4.61575777720764));
#55337=CARTESIAN_POINT('Ctrl Pts',(-0.223723221455666,1.86799439499913,
4.6160110738012));
#55338=CARTESIAN_POINT('Ctrl Pts',(-0.214381593815384,1.85921740940135,
4.61677617419931));
#55339=CARTESIAN_POINT('Ctrl Pts',(-0.207853577369733,1.85356007302027,
4.61727608034494));
#55340=CARTESIAN_POINT('Ctrl Pts',(-0.184251942007615,1.83471223975982,
4.61899762475195));
#55341=CARTESIAN_POINT('Ctrl Pts',(-0.166089431374551,1.8229788198299,4.62017786115513));
#55342=CARTESIAN_POINT('Ctrl Pts',(-0.132535560478973,1.80579667449252,
4.62232136031678));
#55343=CARTESIAN_POINT('Ctrl Pts',(-0.11765119019602,1.7995347634027,4.62326037122781));
#55344=CARTESIAN_POINT('Ctrl Pts',(-0.101164914717352,1.794012370056,4.6243166338652));
#55345=CARTESIAN_POINT('Ctrl Pts',(-0.0999654141651552,1.79361839880892,
4.62439356419384));
#55346=CARTESIAN_POINT('Ctrl Pts',(-0.0982824005210525,1.79307655519359,
4.62450162589741));
#55347=CARTESIAN_POINT('Ctrl Pts',(-0.0978007965386315,1.79292275334075,
4.62453256220524));
#55348=CARTESIAN_POINT('Ctrl Pts',(-0.0969660799568446,1.79265834664908,
4.62458620574611));
#55349=CARTESIAN_POINT('Ctrl Pts',(-0.0966131341034557,1.79254721522886,
4.62460889564694));
#55350=CARTESIAN_POINT('Ctrl Pts',(-0.09587990092875,1.79231773068773,4.62465604933553));
#55351=CARTESIAN_POINT('Ctrl Pts',(-0.0954995841951934,1.79219947422466,
4.62468051624962));
#55352=CARTESIAN_POINT('Ctrl Pts',(-0.0946061665433012,1.79192348835285,
4.62473801411775));
#55353=CARTESIAN_POINT('Ctrl Pts',(-0.0940928899854948,1.7917663356716,
4.62477106389711));
#55354=CARTESIAN_POINT('Ctrl Pts',(-0.0924241912953026,1.7912599775936,
4.62487856689298));
#55355=CARTESIAN_POINT('Ctrl Pts',(-0.0912672098014756,1.79091598403735,
4.62495319024206));
#55356=CARTESIAN_POINT('Ctrl Pts',(-0.0760782504437914,1.78649272367566,
4.62593405077409));
#55357=CARTESIAN_POINT('Ctrl Pts',(-0.061788615253312,1.78336650396834,
4.62687142269172));
#55358=CARTESIAN_POINT('Ctrl Pts',(-0.0306958863038654,1.77874931602146,
4.62894295983905));
#55359=CARTESIAN_POINT('Ctrl Pts',(-0.013887026758127,1.77758519350702,
4.63008269858988));
#55360=CARTESIAN_POINT('Ctrl Pts',(0.0214220791628359,1.77790669745729,
4.6324708735153));
#55361=CARTESIAN_POINT('Ctrl Pts',(0.0398635927146037,1.77966568542667,
4.63371446601899));
#55362=CARTESIAN_POINT('Ctrl Pts',(0.0590672106276965,1.78318254397015,
4.63494377210031));
#55363=CARTESIAN_POINT('Ctrl Pts',(0.0600791442978562,1.78337288128574,
4.63500834915202));
#55364=CARTESIAN_POINT('Ctrl Pts',(0.0614509764940646,1.78363772641091,
4.6350956039724));
#55365=CARTESIAN_POINT('Ctrl Pts',(0.0618116711996511,1.78370800204677,
4.63511851862635));
#55366=CARTESIAN_POINT('Ctrl Pts',(0.0623803427114498,1.78381980858071,
4.63515460214095));
#55367=CARTESIAN_POINT('Ctrl Pts',(0.062588398669669,1.78386092782553,4.63516779452849));
#55368=CARTESIAN_POINT('Ctrl Pts',(0.0629905290240198,1.78394081559652,
4.63519327469142));
#55369=CARTESIAN_POINT('Ctrl Pts',(0.0631846068119249,1.78397955722021,
4.63520556386088));
#55370=CARTESIAN_POINT('Ctrl Pts',(0.0636487278928227,1.78407264927036,
4.63523493302334));
#55371=CARTESIAN_POINT('Ctrl Pts',(0.0639187370909483,1.78412716712025,
4.63525200328792));
#55372=CARTESIAN_POINT('Ctrl Pts',(0.064728604533257,1.78429176928048,4.63530315782323));
#55373=CARTESIAN_POINT('Ctrl Pts',(0.0652682542201548,1.78440289261378,
4.63533718276731));
#55374=CARTESIAN_POINT('Ctrl Pts',(0.0699864197292205,1.78538706505165,
4.63563414586314));
#55375=CARTESIAN_POINT('Ctrl Pts',(0.0741477362072086,1.78634172207099,
4.63589250816159));
#55376=CARTESIAN_POINT('Ctrl Pts',(0.0866041041611286,1.7894611455429,4.63665851176773));
#55377=CARTESIAN_POINT('Ctrl Pts',(0.0948333957680858,1.79187453699471,
4.6371546834383));
#55378=CARTESIAN_POINT('Ctrl Pts',(0.121871621331492,1.80099013403117,4.63878085445742));
#55379=CARTESIAN_POINT('Ctrl Pts',(0.140153026986773,1.8091103756087,4.63987617315425));
#55380=CARTESIAN_POINT('Ctrl Pts',(0.164519052022037,1.8227669117983,4.64145749701418));
#55381=CARTESIAN_POINT('Ctrl Pts',(0.17132462644364,1.8269202220289,4.64191331240111));
#55382=CARTESIAN_POINT('Ctrl Pts',(0.186236716628233,1.83679778107081,4.64295356414291));
#55383=CARTESIAN_POINT('Ctrl Pts',(0.19424653956578,1.84265242526862,4.64354173476242));
#55384=CARTESIAN_POINT('Ctrl Pts',(0.202786776778855,1.84952088143951,4.64420813967507));
#55385=CARTESIAN_POINT('Ctrl Pts',(0.203597164951073,1.85017914407529,4.64427178102764));
#55386=CARTESIAN_POINT('Ctrl Pts',(0.20480391789763,1.8511691378325,4.644367164899));
#55387=CARTESIAN_POINT('Ctrl Pts',(0.205202711991843,1.85149790797758,4.64439878752968));
#55388=CARTESIAN_POINT('Ctrl Pts',(0.20588793309469,1.85206558579343,4.64445329802884));
#55389=CARTESIAN_POINT('Ctrl Pts',(0.206174740260987,1.85230403471518,4.64447616720529));
#55390=CARTESIAN_POINT('Ctrl Pts',(0.206759501683683,1.85279191946094,4.64452290347942));
#55391=CARTESIAN_POINT('Ctrl Pts',(0.207057419982652,1.85304139729833,4.64454677227234));
#55392=CARTESIAN_POINT('Ctrl Pts',(0.207745912683269,1.8536200651365,4.64460206836851));
#55393=CARTESIAN_POINT('Ctrl Pts',(0.208136156306218,1.85394964545194,4.64463351164323));
#55394=CARTESIAN_POINT('Ctrl Pts',(0.20895482807744,1.85464439613383,4.6446996883537));
#55395=CARTESIAN_POINT('Ctrl Pts',(0.209383085895758,1.8550097637461,4.64473442986127));
#55396=CARTESIAN_POINT('Ctrl Pts',(0.210519143736123,1.85598414472606,4.64482692085497));
#55397=CARTESIAN_POINT('Ctrl Pts',(0.211225254064813,1.85659511196311,4.64488475112242));
#55398=CARTESIAN_POINT('Ctrl Pts',(0.226687429799513,1.87009182522492,4.64615871340064));
#55399=CARTESIAN_POINT('Ctrl Pts',(0.240237970170727,1.88429088100175,4.64743212855514));
#55400=CARTESIAN_POINT('Ctrl Pts',(0.270803958182613,1.92279597791174,4.65072014737897));
#55401=CARTESIAN_POINT('Ctrl Pts',(0.285917071594265,1.9483835019075,4.65277360865473));
#55402=CARTESIAN_POINT('Ctrl Pts',(0.297897221732843,1.97703416707449,4.65473729202593));
#55403=CARTESIAN_POINT('Ctrl Pts',(0.298456848714247,1.9783987646595,4.6548300391783));
#55404=CARTESIAN_POINT('Ctrl Pts',(0.299165215498802,1.98016040270523,4.65494872468456));
#55405=CARTESIAN_POINT('Ctrl Pts',(0.299322555661424,1.98055393300142,4.65497517072323));
#55406=CARTESIAN_POINT('Ctrl Pts',(0.299570806395052,1.98117841449606,4.65501702970987));
#55407=CARTESIAN_POINT('Ctrl Pts',(0.29966222656197,1.98140916056131,4.65503247339567));
#55408=CARTESIAN_POINT('Ctrl Pts',(0.299825665835762,1.98182307979224,4.65506013482778));
#55409=CARTESIAN_POINT('Ctrl Pts',(0.299897783174249,1.98200621198075,4.65507235848008));
#55410=CARTESIAN_POINT('Ctrl Pts',(0.300067076222544,1.98243726653436,4.65510109585825));
#55411=CARTESIAN_POINT('Ctrl Pts',(0.300164112315517,1.98268524299252,4.65511760104362));
#55412=CARTESIAN_POINT('Ctrl Pts',(0.300444940144499,1.9834055300544,4.65516546595973));
#55413=CARTESIAN_POINT('Ctrl Pts',(0.300627926301566,1.9838781570236,4.65519677718011));
#55414=CARTESIAN_POINT('Ctrl Pts',(0.301895846891044,1.98717609867468,4.65541460765242));
#55415=CARTESIAN_POINT('Ctrl Pts',(0.302942096851317,1.99001626194707,4.6555988496368));
#55416=CARTESIAN_POINT('Ctrl Pts',(0.306066871507953,1.99888191474616,4.65616484819768));
#55417=CARTESIAN_POINT('Ctrl Pts',(0.308006882444144,2.00495491315872,4.6565396150681));
#55418=CARTESIAN_POINT('Ctrl Pts',(0.314128170108212,2.02627974410496,4.65782373099043));
#55419=CARTESIAN_POINT('Ctrl Pts',(0.317366622463534,2.04177907990649,4.6587020689851));
#55420=CARTESIAN_POINT('Ctrl Pts',(0.322762261479198,2.08229228629075,4.66098751549565));
#55421=CARTESIAN_POINT('Ctrl Pts',(0.323161917841359,2.10742696744241,4.66240212454196));
#55422=CARTESIAN_POINT('Ctrl Pts',(0.320497480109653,2.13383428389503,4.66401208311936));
#55423=CARTESIAN_POINT('Ctrl Pts',(0.320337709099968,2.135314947768,4.66410273651061));
#55424=CARTESIAN_POINT('Ctrl Pts',(0.320105751795304,2.13733333013961,4.66422685081282));
#55425=CARTESIAN_POINT('Ctrl Pts',(0.320042460144643,2.13787206847587,4.66426003135707));
#55426=CARTESIAN_POINT('Ctrl Pts',(0.319932530391134,2.1387878324401,4.66431652282108));
#55427=CARTESIAN_POINT('Ctrl Pts',(0.319886585078825,2.13916494136957,4.66433981185553));
#55428=CARTESIAN_POINT('Ctrl Pts',(0.319792647454913,2.1399247671823,4.66438678905129));
#55429=CARTESIAN_POINT('Ctrl Pts',(0.319744634643312,2.14030748088862,4.66441047782506));
#55430=CARTESIAN_POINT('Ctrl Pts',(0.31963403662193,2.14117643261107,4.66446432497043));
#55431=CARTESIAN_POINT('Ctrl Pts',(0.31957102884465,2.14166261500123,4.66449449664035));
#55432=CARTESIAN_POINT('Ctrl Pts',(0.319436910891427,2.14267929319894,4.66455768269616));
#55433=CARTESIAN_POINT('Ctrl Pts',(0.31936558804735,2.14320975900721,4.66459070372861));
#55434=CARTESIAN_POINT('Ctrl Pts',(0.319175221626972,2.14459939312543,4.66467734689045));
#55435=CARTESIAN_POINT('Ctrl Pts',(0.319054030966084,2.14545825852875,4.66473103683525));
#55436=CARTESIAN_POINT('Ctrl Pts',(0.318683923880575,2.14800676115965,4.6648907714494));
#55437=CARTESIAN_POINT('Ctrl Pts',(0.318425044839465,2.14969490009154,4.66499713056754));
#55438=CARTESIAN_POINT('Ctrl Pts',(0.315434455823464,2.1682127658467,4.66616999668355));
#55439=CARTESIAN_POINT('Ctrl Pts',(0.31138518744132,2.18479962864227,4.66727885149815));
#55440=CARTESIAN_POINT('Ctrl Pts',(0.297230501974381,2.22769610971411,4.67029278758103));
#55441=CARTESIAN_POINT('Ctrl Pts',(0.284958865483838,2.25313622796883,4.672241951265));
#55442=CARTESIAN_POINT('Ctrl Pts',(0.267546094463786,2.27970394409235,4.67428443061787));
#55443=CARTESIAN_POINT('Ctrl Pts',(0.265499628615286,2.28271390248755,4.6745157356746));
#55444=CARTESIAN_POINT('Ctrl Pts',(0.263069784324188,2.28616067701977,4.67477990000651));
#55445=CARTESIAN_POINT('Ctrl Pts',(0.262735787982972,2.2866317626185,4.67481598887121));
#55446=CARTESIAN_POINT('Ctrl Pts',(0.262237506826088,2.28733057540571,4.6748694970489));
#55447=CARTESIAN_POINT('Ctrl Pts',(0.262074190014144,2.28755898644978,4.67488698230461));
#55448=CARTESIAN_POINT('Ctrl Pts',(0.261782900219347,2.28796525420165,4.6749180748701));
#55449=CARTESIAN_POINT('Ctrl Pts',(0.261655044443343,2.28814319374556,4.67493169024392));
#55450=CARTESIAN_POINT('Ctrl Pts',(0.261383359098157,2.28852049130286,4.67496055395379));
#55451=CARTESIAN_POINT('Ctrl Pts',(0.261239483285007,2.28871981461537,4.6749757989636));
#55452=CARTESIAN_POINT('Ctrl Pts',(0.260853150421691,2.28925374576728,4.67501662735212));
#55453=CARTESIAN_POINT('Ctrl Pts',(0.260610276632537,2.28958805365819,4.67504218185907));
#55454=CARTESIAN_POINT('Ctrl Pts',(0.259448110138156,2.29118128503546,4.67516392946409));
#55455=CARTESIAN_POINT('Ctrl Pts',(0.258520314224159,2.29243402237016,4.67525954140931));
#55456=CARTESIAN_POINT('Ctrl Pts',(0.250781443599317,2.30272628208356,4.67604455355918));
#55457=CARTESIAN_POINT('Ctrl Pts',(0.243506784677752,2.31140904268779,4.67670357887331));
#55458=CARTESIAN_POINT('Ctrl Pts',(0.233014739499046,2.32266987799107,4.67758142280991));
#55459=CARTESIAN_POINT('Ctrl Pts',(0.23018379125078,2.3255951395105,4.67781175694168));
#55460=CARTESIAN_POINT('Ctrl Pts',(0.214761491605272,2.34093860104124,4.67903711657215));
#55461=CARTESIAN_POINT('Ctrl Pts',(0.201219721161123,2.35235794525604,4.68001284188649));
#55462=CARTESIAN_POINT('Ctrl Pts',(0.173682591858064,2.37194677357373,4.68193448394837));
#55463=CARTESIAN_POINT('Ctrl Pts',(0.159875810243121,2.38028611346861,4.68287249711085));
#55464=CARTESIAN_POINT('Ctrl Pts',(0.14437829177132,2.38812788553139,4.68392766341475));
#55465=CARTESIAN_POINT('Ctrl Pts',(0.143248459144363,2.3886912683776,4.68400459154756));
#55466=CARTESIAN_POINT('Ctrl Pts',(0.141661602715333,2.38947093383952,4.68411265091945));
#55467=CARTESIAN_POINT('Ctrl Pts',(0.141207325774261,2.38969280689186,4.68414358710722));
#55468=CARTESIAN_POINT('Ctrl Pts',(0.140419655457845,2.39007521939989,4.68419723071261));
#55469=CARTESIAN_POINT('Ctrl Pts',(0.140086503264321,2.39023625574714,4.68421992079886));
#55470=CARTESIAN_POINT('Ctrl Pts',(0.139401403631416,2.39056595913233,4.68426658354593));
#55471=CARTESIAN_POINT('Ctrl Pts',(0.139049425773298,2.3907345612942,4.68429055841434));
#55472=CARTESIAN_POINT('Ctrl Pts',(0.138226718983486,2.39112681324392,4.68434660041197));
#55473=CARTESIAN_POINT('Ctrl Pts',(0.137755753100695,2.39134996089424,4.68437868487787));
#55474=CARTESIAN_POINT('Ctrl Pts',(0.136761938317653,2.39181789037348,4.68444639494943));
#55475=CARTESIAN_POINT('Ctrl Pts',(0.136238969293794,2.39206241140081,4.68448202945224));
#55476=CARTESIAN_POINT('Ctrl Pts',(0.134836996976981,2.3927133370451,4.68457756995864));
#55477=CARTESIAN_POINT('Ctrl Pts',(0.133956819288346,2.39311718470795,4.68463756395158));
#55478=CARTESIAN_POINT('Ctrl Pts',(0.131267936224006,2.39433627124205,4.68482088614121));
#55479=CARTESIAN_POINT('Ctrl Pts',(0.12945353735844,2.39513876910877,4.68494464951488));
#55480=CARTESIAN_POINT('Ctrl Pts',(0.0999151119131207,2.40787865824408,
4.68696077727994));
#55481=CARTESIAN_POINT('Ctrl Pts',(0.0706616876727685,2.4158771888731,4.68899680475839));
#55482=CARTESIAN_POINT('Ctrl Pts',(0.0260240969215149,2.42156456831388,
4.69203793276011));
#55483=CARTESIAN_POINT('Ctrl Pts',(0.0112023207511253,2.4224214970483,4.69303316923491));
#55484=CARTESIAN_POINT('Ctrl Pts',(-0.00695842717649646,2.4222170935713,
4.69419847524837));
#55485=CARTESIAN_POINT('Ctrl Pts',(-0.0102891855150253,2.42212794027649,
4.69440992858046));
#55486=CARTESIAN_POINT('Ctrl Pts',(-0.0141728397428451,2.42196368507066,
4.69465337243868));
#55487=CARTESIAN_POINT('Ctrl Pts',(-0.0147275039674132,2.42193879003388,
4.69468806703854));
#55488=CARTESIAN_POINT('Ctrl Pts',(-0.0155619406349865,2.42189917693679,
4.6947401472688));
#55489=CARTESIAN_POINT('Ctrl Pts',(-0.0158417591231338,2.42188552744451,
4.69475759241391));
#55490=CARTESIAN_POINT('Ctrl Pts',(-0.0163403256655439,2.42186055576958,
4.69478864039519));
#55491=CARTESIAN_POINT('Ctrl Pts',(-0.0165590798269971,2.42184937545304,
4.69480225120741));
#55492=CARTESIAN_POINT('Ctrl Pts',(-0.0170236935492711,2.42182515454647,
4.69483113373689));
#55493=CARTESIAN_POINT('Ctrl Pts',(-0.017269548905499,2.42181205527838,
4.69484640206994));
#55494=CARTESIAN_POINT('Ctrl Pts',(-0.0179296832100263,2.42177612439762,
4.69488735817403));
#55495=CARTESIAN_POINT('Ctrl Pts',(-0.0183439352442097,2.42175277437296,
4.69491301675766));
#55496=CARTESIAN_POINT('Ctrl Pts',(-0.0203327488817649,2.42163681810002,
4.69503600394895));
#55497=CARTESIAN_POINT('Ctrl Pts',(-0.0219066964851299,2.42153345132637,
4.69513273696171));
#55498=CARTESIAN_POINT('Ctrl Pts',(-0.0350170550928157,2.42057573002211,
4.69593396012065));
#55499=CARTESIAN_POINT('Ctrl Pts',(-0.0465019223588754,2.4191122484282,
4.69660673674212));
#55500=CARTESIAN_POINT('Ctrl Pts',(-0.0657090124969458,2.41560539687204,
4.69771919109732));
#55501=CARTESIAN_POINT('Ctrl Pts',(-0.0734782777856998,2.41388754536831,
4.69816558584579));
#55502=CARTESIAN_POINT('Ctrl Pts',(-0.0908731623428266,2.40936005653806,
4.69917135699064));
#55503=CARTESIAN_POINT('Ctrl Pts',(-0.100447052820797,2.40638531697912,
4.69972949918874));
#55504=CARTESIAN_POINT('Ctrl Pts',(-0.128265513933019,2.39629742999938,
4.70139718930113));
#55505=CARTESIAN_POINT('Ctrl Pts',(-0.146015461841703,2.38796444472437,
4.70252435249028));
#55506=CARTESIAN_POINT('Ctrl Pts',(-0.164015571338357,2.37741979672301,
4.70379142741676));
#55507=CARTESIAN_POINT('Ctrl Pts',(-0.165128528534599,2.37675877627077,
4.70387029084024));
#55508=CARTESIAN_POINT('Ctrl Pts',(-0.166675245351863,2.37582748113571,
4.7039806283394));
#55509=CARTESIAN_POINT('Ctrl Pts',(-0.167112400493743,2.37556284647834,
4.70401189626538));
#55510=CARTESIAN_POINT('Ctrl Pts',(-0.16786622551124,2.37510406018809,4.70406595821423));
#55511=CARTESIAN_POINT('Ctrl Pts',(-0.168183193461786,2.37491039819273,
4.70408873425139));
#55512=CARTESIAN_POINT('Ctrl Pts',(-0.168831757256897,2.37451259533248,
4.70413542818665));
#55513=CARTESIAN_POINT('Ctrl Pts',(-0.169163319262705,2.37430840065258,
4.70415934803914));
#55514=CARTESIAN_POINT('Ctrl Pts',(-0.169933336135604,2.37383225357167,
4.70421501319779));
#55515=CARTESIAN_POINT('Ctrl Pts',(-0.17037150870673,2.37355984873948,4.70424677515324));
#55516=CARTESIAN_POINT('Ctrl Pts',(-0.171292476621976,2.37298422685196,
4.7043137160109));
#55517=CARTESIAN_POINT('Ctrl Pts',(-0.171775124849703,2.37268077881185,
4.70434890339712));
#55518=CARTESIAN_POINT('Ctrl Pts',(-0.173060744986607,2.37186772268018,
4.70444291582998));
#55519=CARTESIAN_POINT('Ctrl Pts',(-0.173862266021968,2.37135584112599,
4.70450182521601));
#55520=CARTESIAN_POINT('Ctrl Pts',(-0.176288355197909,2.36979128744708,
4.70468104698536));
#55521=CARTESIAN_POINT('Ctrl Pts',(-0.177905692503867,2.3687275335206,4.70480177206373));
#55522=CARTESIAN_POINT('Ctrl Pts',(-0.204629980063425,2.35080345996794,
4.70681770899292));
#55523=CARTESIAN_POINT('Ctrl Pts',(-0.227245378051158,2.33050924126038,
4.70885731178849));
#55524=CARTESIAN_POINT('Ctrl Pts',(-0.256249319694636,2.29600477968466,
4.71190371340892));
#55525=CARTESIAN_POINT('Ctrl Pts',(-0.265006514246938,2.28399245517173,
4.71290030552239));
#55526=CARTESIAN_POINT('Ctrl Pts',(-0.274681802839067,2.26858897876081,
4.71406749375441));
#55527=CARTESIAN_POINT('Ctrl Pts',(-0.276414764126198,2.26573236529977,
4.71427954070437));
#55528=CARTESIAN_POINT('Ctrl Pts',(-0.278383866661579,2.26236966217774,
4.71452359260699));
#55529=CARTESIAN_POINT('Ctrl Pts',(-0.278663423404615,2.2618894094144,4.71455831674827));
#55530=CARTESIAN_POINT('Ctrl Pts',(-0.279082100035496,2.26116586364756,
4.71461043272201));
#55531=CARTESIAN_POINT('Ctrl Pts',(-0.279222145190115,2.26092311146118,
4.71462788418872));
#55532=CARTESIAN_POINT('Ctrl Pts',(-0.279471088676323,2.26049029317157,
4.71465893921821));
#55533=CARTESIAN_POINT('Ctrl Pts',(-0.279580109807511,2.26030029884351,
4.71467255077093));
#55534=CARTESIAN_POINT('Ctrl Pts',(-0.279811225277397,2.25989657413593,
4.71470143037109));
#55535=CARTESIAN_POINT('Ctrl Pts',(-0.27993326814201,2.25968281560628,4.71471669504349));
#55536=CARTESIAN_POINT('Ctrl Pts',(-0.280260240178963,2.25910859601858,
4.71475763110251));
#55537=CARTESIAN_POINT('Ctrl Pts',(-0.280464719663853,2.25874787740508,
4.71478327335133));
#55538=CARTESIAN_POINT('Ctrl Pts',(-0.281442251445843,2.25701564689641,
4.7149060651389));
#55539=CARTESIAN_POINT('Ctrl Pts',(-0.282205960011085,2.25563884682263,
4.71500262137186));
#55540=CARTESIAN_POINT('Ctrl Pts',(-0.288477484608659,2.24413470796355,
4.71580126160416));
#55541=CARTESIAN_POINT('Ctrl Pts',(-0.293449001894129,2.23372291856966,
4.71647184744707));
#55542=CARTESIAN_POINT('Ctrl Pts',(-0.311817612255427,2.18926600017448,
4.71921301145395));
#55543=CARTESIAN_POINT('Ctrl Pts',(-0.319927756985202,2.15333862351635,
4.72117565196667));
#55544=CARTESIAN_POINT('Ctrl Pts',(-0.321945817749436,2.11471374155642,
4.72351278071896));
#55545=CARTESIAN_POINT('Ctrl Pts',(-0.322035026497539,2.11261131002231,
4.72364056323453));
#55546=CARTESIAN_POINT('Ctrl Pts',(-0.322126306221127,2.10981334754542,
4.72381142215885));
#55547=CARTESIAN_POINT('Ctrl Pts',(-0.322146726029427,2.10911843442186,
4.72385392318663));
#55548=CARTESIAN_POINT('Ctrl Pts',(-0.322175041291975,2.10803548533588,
4.72392026093351));
#55549=CARTESIAN_POINT('Ctrl Pts',(-0.322184484673896,2.10764748908873,
4.72394404912277));
#55550=CARTESIAN_POINT('Ctrl Pts',(-0.32220194332813,2.10687263171224,4.72399159796329));
#55551=CARTESIAN_POINT('Ctrl Pts',(-0.322209962787825,2.10648577129614,
4.72401535844456));
#55552=CARTESIAN_POINT('Ctrl Pts',(-0.322224409897198,2.10572250097408,
4.72406227920662));
#55553=CARTESIAN_POINT('Ctrl Pts',(-0.322230874755522,2.10534609234585,
4.72408543828096));
#55554=CARTESIAN_POINT('Ctrl Pts',(-0.322243969803928,2.10449700154428,
4.7241377252403));
#55555=CARTESIAN_POINT('Ctrl Pts',(-0.322250219521799,2.10402431512527,
4.72416686500768));
#55556=CARTESIAN_POINT('Ctrl Pts',(-0.3222686839118,2.10234895229109,4.72427026000821));
#55557=CARTESIAN_POINT('Ctrl Pts',(-0.322275205798636,2.10114623701008,
4.72434469321685));
#55558=CARTESIAN_POINT('Ctrl Pts',(-0.322274995052385,2.09994352890236,
4.72441933817791));
#55559=CARTESIAN_POINT('',(-0.322274937371842,2.10020091534284,4.97494943677011));
#55560=CARTESIAN_POINT('Ctrl Pts',(-0.322274995069378,2.0999436259616,4.72441933215401));
#55561=CARTESIAN_POINT('Ctrl Pts',(-0.322274547943088,2.09738752696416,
4.7245779740387));
#55562=CARTESIAN_POINT('Ctrl Pts',(-0.322243690626771,2.09483157014679,
4.72473756644637));
#55563=CARTESIAN_POINT('Ctrl Pts',(-0.321335065755551,2.05692969309682,
4.72711886872579));
#55564=CARTESIAN_POINT('Ctrl Pts',(-0.314676157708159,2.02196848964178,
4.72954509116856));
#55565=CARTESIAN_POINT('Ctrl Pts',(-0.298601357054798,1.97824230550722,
4.73266195050605));
#55566=CARTESIAN_POINT('Ctrl Pts',(-0.294169496817719,1.96789371210595,
4.73340268415641));
#55567=CARTESIAN_POINT('Ctrl Pts',(-0.288752555336678,1.9568770158005,4.73417929989949));
#55568=CARTESIAN_POINT('Ctrl Pts',(-0.288295759312503,1.9559590959222,4.73424391317211));
#55569=CARTESIAN_POINT('Ctrl Pts',(-0.28750009264393,1.95437917257349,4.73435494116238));
#55570=CARTESIAN_POINT('Ctrl Pts',(-0.2871632999874,1.95371613958796,4.73440147898744));
#55571=CARTESIAN_POINT('Ctrl Pts',(-0.28668221313438,1.95277710340268,4.73446730283752));
#55572=CARTESIAN_POINT('Ctrl Pts',(-0.286539812508352,1.95250014081441,
4.73448670644769));
#55573=CARTESIAN_POINT('Ctrl Pts',(-0.28629435605936,1.95202443637072,4.73452001465143));
#55574=CARTESIAN_POINT('Ctrl Pts',(-0.286191494392835,1.95182559505374,
4.73453393154702));
#55575=CARTESIAN_POINT('Ctrl Pts',(-0.285993950484522,1.95144469709913,
4.73456057940287));
#55576=CARTESIAN_POINT('Ctrl Pts',(-0.285899301700763,1.95126262399343,
4.73457331246777));
#55577=CARTESIAN_POINT('Ctrl Pts',(-0.28567567681513,1.95083344544871,4.73460331533039));
#55578=CARTESIAN_POINT('Ctrl Pts',(-0.285546553653665,1.95058641621874,
4.73462057577588));
#55579=CARTESIAN_POINT('Ctrl Pts',(-0.285163434367359,1.9498557702661,4.734671602424));
#55580=CARTESIAN_POINT('Ctrl Pts',(-0.284908527335595,1.94937262836942,
4.73470531135803));
#55581=CARTESIAN_POINT('Ctrl Pts',(-0.282632449248504,1.94508507864646,
4.73500418561647));
#55582=CARTESIAN_POINT('Ctrl Pts',(-0.280536294570565,1.94132068168172,
4.73526470628351));
#55583=CARTESIAN_POINT('Ctrl Pts',(-0.278246628046583,1.93739604882048,
4.73553551695539));
#55584=CARTESIAN_POINT('Ctrl Pts',(-0.278127867869703,1.93719299746828,
4.73554952578012));
#55585=CARTESIAN_POINT('Ctrl Pts',(-0.277944061789395,1.93687952131825,
4.73557114973181));
#55586=CARTESIAN_POINT('Ctrl Pts',(-0.277879172390624,1.93676900539128,
4.73557877262503));
#55587=CARTESIAN_POINT('Ctrl Pts',(-0.265493573508929,1.91570334818976,
4.7370316737817));
#55588=CARTESIAN_POINT('Ctrl Pts',(-0.250840055453509,1.89620681532173,
4.73835956307186));
#55589=CARTESIAN_POINT('Ctrl Pts',(-0.219493124091191,1.86306596888579,
4.74092149802996));
#55590=CARTESIAN_POINT('Ctrl Pts',(-0.203358906735829,1.84908184896662,
4.74214082725452));
#55591=CARTESIAN_POINT('Ctrl Pts',(-0.185189197729576,1.83624435840432,
4.74349138570597));
#55592=CARTESIAN_POINT('Ctrl Pts',(-0.184411203423234,1.83569981942645,
4.74354916423492));
#55593=CARTESIAN_POINT('Ctrl Pts',(-0.183162783934418,1.83483421303547,
4.74364180484366));
#55594=CARTESIAN_POINT('Ctrl Pts',(-0.182693890665827,1.83451093750973,
4.74367658297569));
#55595=CARTESIAN_POINT('Ctrl Pts',(-0.18179888319161,1.83389737405409,4.74374293574978));
#55596=CARTESIAN_POINT('Ctrl Pts',(-0.181372924060936,1.83360686217973,
4.74377450178129));
#55597=CARTESIAN_POINT('Ctrl Pts',(-0.180624074078974,1.83309876154052,
4.74382997371869));
#55598=CARTESIAN_POINT('Ctrl Pts',(-0.180301481812524,1.83288073285114,
4.74385386292528));
#55599=CARTESIAN_POINT('Ctrl Pts',(-0.179670254216398,1.83245577290588,
4.74390059410385));
#55600=CARTESIAN_POINT('Ctrl Pts',(-0.179361654428296,1.83224878969363,
4.74392343406777));
#55601=CARTESIAN_POINT('Ctrl Pts',(-0.178627371745863,1.83175813271335,
4.74397776477584));
#55602=CARTESIAN_POINT('Ctrl Pts',(-0.178201371029061,1.83147493848653,
4.74400927349607));
#55603=CARTESIAN_POINT('Ctrl Pts',(-0.176692369059128,1.83047696546601,
4.74412084530581));
#55604=CARTESIAN_POINT('Ctrl Pts',(-0.175605737973411,1.82976772187624,
4.74420111543285));
#55605=CARTESIAN_POINT('Ctrl Pts',(-0.157489377820834,1.81809859475036,
4.74553827735376));
#55606=CARTESIAN_POINT('Ctrl Pts',(-0.139471499948845,1.80876344994324,
4.74685647753258));
#55607=CARTESIAN_POINT('Ctrl Pts',(-0.100979544123374,1.79321560880284,
4.74963667777787));
#55608=CARTESIAN_POINT('Ctrl Pts',(-0.0805193728849704,1.78722188406425,
4.7510956986516));
#55609=CARTESIAN_POINT('Ctrl Pts',(-0.0517850699502814,1.78181292845422,
4.75302784297435));
#55610=CARTESIAN_POINT('Ctrl Pts',(-0.04389927028912,1.78062939387546,4.75354584820889));
#55611=CARTESIAN_POINT('Ctrl Pts',(-0.0347137491669791,1.77959752312098,
4.75412910121221));
#55612=CARTESIAN_POINT('Ctrl Pts',(-0.0334496425227513,1.77946308619111,
4.75420892755528));
#55613=CARTESIAN_POINT('Ctrl Pts',(-0.0318026092067258,1.77929777491508,
4.75431233263403));
#55614=CARTESIAN_POINT('Ctrl Pts',(-0.0314203989883882,1.77926010279693,
4.75433628658921));
#55615=CARTESIAN_POINT('Ctrl Pts',(-0.0307999376527302,1.77920006744461,
4.75437510276674));
#55616=CARTESIAN_POINT('Ctrl Pts',(-0.0305617287982219,1.77917728630798,
4.75438998853751));
#55617=CARTESIAN_POINT('Ctrl Pts',(-0.0301036265495518,1.77913399047732,
4.75441858329381));
#55618=CARTESIAN_POINT('Ctrl Pts',(-0.0298837380949415,1.7791134365603,
4.75443229442039));
#55619=CARTESIAN_POINT('Ctrl Pts',(-0.0293763572658202,1.77906653554926,
4.75446389936115));
#55620=CARTESIAN_POINT('Ctrl Pts',(-0.0290888495932546,1.77904034863949,
4.75448178408523));
#55621=CARTESIAN_POINT('Ctrl Pts',(-0.0281693468069803,1.77895784371366,
4.75453890635953));
#55622=CARTESIAN_POINT('Ctrl Pts',(-0.0275372154203691,1.77890300531529,
4.75457806089332));
#55623=CARTESIAN_POINT('Ctrl Pts',(-0.0218635453144588,1.77842768333002,
4.75492848888543));
#55624=CARTESIAN_POINT('Ctrl Pts',(-0.0168125786775542,1.77812407106975,
4.75523336089768));
#55625=CARTESIAN_POINT('Ctrl Pts',(-0.0105768964562659,1.77789644902548,
4.7556032965631));
#55626=CARTESIAN_POINT('Ctrl Pts',(-0.00939732711859988,1.77785987737585,
4.75567299116233));
#55627=CARTESIAN_POINT('Ctrl Pts',(0.0236689207366504,1.77701645939498,
4.75761939655843));
#55628=CARTESIAN_POINT('Ctrl Pts',(0.0555020713937053,1.7809410735263,4.75931959009532));
#55629=CARTESIAN_POINT('Ctrl Pts',(0.0977623471692265,1.79267829686755,
4.76184549427587));
#55630=CARTESIAN_POINT('Ctrl Pts',(0.109093487027939,1.79651578830825,4.76254896510335));
#55631=CARTESIAN_POINT('Ctrl Pts',(0.121135349328311,1.80135564116716,4.76333620574593));
#55632=CARTESIAN_POINT('Ctrl Pts',(0.122084420615296,1.80174235948617,4.76339852203811));
#55633=CARTESIAN_POINT('Ctrl Pts',(0.123586707155374,1.80236286837052,4.76349759883531));
#55634=CARTESIAN_POINT('Ctrl Pts',(0.124141146611156,1.80259369202969,4.76353425912491));
#55635=CARTESIAN_POINT('Ctrl Pts',(0.125190972817312,1.80303420175775,4.76360385612501));
#55636=CARTESIAN_POINT('Ctrl Pts',(0.125686486637661,1.80324358124593,4.76363678235485));
#55637=CARTESIAN_POINT('Ctrl Pts',(0.126543417496122,1.80360820889033,4.76369385812731));
#55638=CARTESIAN_POINT('Ctrl Pts',(0.126905079899416,1.80376288037739,4.76371798799422));
#55639=CARTESIAN_POINT('Ctrl Pts',(0.127602783897303,1.80406277831003,4.76376461867095));
#55640=CARTESIAN_POINT('Ctrl Pts',(0.127938863182336,1.80420791605282,4.76378711642586));
#55641=CARTESIAN_POINT('Ctrl Pts',(0.128724131392164,1.80454862727937,4.76383976846701));
#55642=CARTESIAN_POINT('Ctrl Pts',(0.129173122177034,1.8047446526344,4.7638699381659));
#55643=CARTESIAN_POINT('Ctrl Pts',(0.130695925320206,1.80541363322174,4.76397248411289));
#55644=CARTESIAN_POINT('Ctrl Pts',(0.131767591425263,1.80589142450702,4.76404502586968));
#55645=CARTESIAN_POINT('Ctrl Pts',(0.143118691695756,1.8110266888249,4.76481743173806));
#55646=CARTESIAN_POINT('Ctrl Pts',(0.153148163358532,1.81621465226782,4.76553564155586));
#55647=CARTESIAN_POINT('Ctrl Pts',(0.18124070703955,1.83266956877606,4.7676559135239));
#55648=CARTESIAN_POINT('Ctrl Pts',(0.198485828572135,1.84521199137991,4.76909893007554));
#55649=CARTESIAN_POINT('Ctrl Pts',(0.218240208679316,1.86280959470392,4.77088674085388));
#55650=CARTESIAN_POINT('Ctrl Pts',(0.222029278360146,1.86635266157439,4.77123637371201));
#55651=CARTESIAN_POINT('Ctrl Pts',(0.231768501317145,1.87591053250826,4.77215013439335));
#55652=CARTESIAN_POINT('Ctrl Pts',(0.237570621916372,1.88207122988262,4.77271015816524));
#55653=CARTESIAN_POINT('Ctrl Pts',(0.246029783771259,1.89179308984146,4.77354261721365));
#55654=CARTESIAN_POINT('Ctrl Pts',(0.248866656728988,1.89519237319296,4.77382477416132));
#55655=CARTESIAN_POINT('Ctrl Pts',(0.251979726887251,1.89908284973005,4.77413680249407));
#55656=CARTESIAN_POINT('Ctrl Pts',(0.252325577625095,1.89951736503658,4.77417150206428));
#55657=CARTESIAN_POINT('Ctrl Pts',(0.252841844430484,1.90016943752902,4.77422334848586));
#55658=CARTESIAN_POINT('Ctrl Pts',(0.253013104371194,1.90038632058323,4.77424055547313));
#55659=CARTESIAN_POINT('Ctrl Pts',(0.253306610247418,1.90075900008808,4.77427005839593));
#55660=CARTESIAN_POINT('Ctrl Pts',(0.253428991500558,1.90091468886734,4.77428236408162));
#55661=CARTESIAN_POINT('Ctrl Pts',(0.253681914753753,1.90123705935169,4.77430780431052));
#55662=CARTESIAN_POINT('Ctrl Pts',(0.253812435649459,1.90140375643383,4.77432093733637));
#55663=CARTESIAN_POINT('Ctrl Pts',(0.254167918921418,1.90185869106997,4.77435671906143));
#55664=CARTESIAN_POINT('Ctrl Pts',(0.25439255606977,1.90214718416767,4.77437934445946));
#55665=CARTESIAN_POINT('Ctrl Pts',(0.255240196448918,1.90323960720513,4.77446477504665));
#55666=CARTESIAN_POINT('Ctrl Pts',(0.255859892270745,1.90404611346424,4.77452734770043));
#55667=CARTESIAN_POINT('Ctrl Pts',(0.267643829345911,1.9195335862945,4.77571972799984));
#55668=CARTESIAN_POINT('Ctrl Pts',(0.27753313523343,1.93514575471937,4.77676487777652));
#55669=CARTESIAN_POINT('Ctrl Pts',(0.29379133191771,1.96646582358621,4.77874347161244));
#55670=CARTESIAN_POINT('Ctrl Pts',(0.300365881084286,1.98199558572142,4.77967607794931));
#55671=CARTESIAN_POINT('Ctrl Pts',(0.310244164514636,2.01159171432753,4.78145894755035));
#55672=CARTESIAN_POINT('Ctrl Pts',(0.313875044148507,2.02550274275552,4.78229889245078));
#55673=CARTESIAN_POINT('Ctrl Pts',(0.316745730245191,2.04055054206694,4.78322877664618));
#55674=CARTESIAN_POINT('Ctrl Pts',(0.316921266267282,2.04149353340299,4.78328713222741));
#55675=CARTESIAN_POINT('Ctrl Pts',(0.317195022981206,2.04300156211961,4.7833805922474));
#55676=CARTESIAN_POINT('Ctrl Pts',(0.317295950610439,2.04356610730783,4.78341561074861));
#55677=CARTESIAN_POINT('Ctrl Pts',(0.317485243078731,2.044641488338,4.78348237612829));
#55678=CARTESIAN_POINT('Ctrl Pts',(0.317573883333443,2.04515227437982,4.78351411416085));
#55679=CARTESIAN_POINT('Ctrl Pts',(0.317722575851088,2.04602155482355,4.78356817200388));
#55680=CARTESIAN_POINT('Ctrl Pts',(0.317783254983974,2.04637994219333,4.78359047185833));
#55681=CARTESIAN_POINT('Ctrl Pts',(0.317903871892142,2.04709973471263,4.78363528546525));
#55682=CARTESIAN_POINT('Ctrl Pts',(0.317963800007859,2.0474611409114,4.7836577994882));
#55683=CARTESIAN_POINT('Ctrl Pts',(0.318102602501957,2.0483071478249,4.78371053327904));
#55684=CARTESIAN_POINT('Ctrl Pts',(0.318180985784851,2.04879182716364,4.78374076858309));
#55685=CARTESIAN_POINT('Ctrl Pts',(0.318443867997036,2.05044125465171,4.78384374607425));
#55686=CARTESIAN_POINT('Ctrl Pts',(0.318623079619836,2.05160682507111,4.78391665564451));
#55687=CARTESIAN_POINT('Ctrl Pts',(0.3204852304953,2.06417697187075,4.78470451103431));
#55688=CARTESIAN_POINT('Ctrl Pts',(0.321561292627095,2.07566169388501,4.78543861549542));
#55689=CARTESIAN_POINT('Ctrl Pts',(0.323072952801183,2.11362736853598,4.78791544009857));
#55690=CARTESIAN_POINT('Ctrl Pts',(0.320863191711508,2.14010385172059,4.78973224530757));
#55691=CARTESIAN_POINT('Ctrl Pts',(0.313122989998399,2.1770939750261,4.79226121142413));
#55692=CARTESIAN_POINT('Ctrl Pts',(0.310219724754215,2.18805264762559,4.79300736399185));
#55693=CARTESIAN_POINT('Ctrl Pts',(0.306429352962278,2.19981626285489,4.79378925525127));
#55694=CARTESIAN_POINT('Ctrl Pts',(0.306109046731703,2.20079427693285,4.79385411240761));
#55695=CARTESIAN_POINT('Ctrl Pts',(0.305548521924831,2.20247844984597,4.793965521861));
#55696=CARTESIAN_POINT('Ctrl Pts',(0.305310528760909,2.20318533319857,4.79401219837646));
#55697=CARTESIAN_POINT('Ctrl Pts',(0.304969566324361,2.20418654644486,4.79407818365519));
#55698=CARTESIAN_POINT('Ctrl Pts',(0.304868622981311,2.20448155611217,4.79409761078358));
#55699=CARTESIAN_POINT('Ctrl Pts',(0.30469444485817,2.20498819479714,4.7941309468645));
#55700=CARTESIAN_POINT('Ctrl Pts',(0.304621417477834,2.20519989443491,4.79414486817189));
#55701=CARTESIAN_POINT('Ctrl Pts',(0.304481076289535,2.20560535915375,4.79417151544452));
#55702=CARTESIAN_POINT('Ctrl Pts',(0.304413798251961,2.20579913579435,4.79418424353182));
#55703=CARTESIAN_POINT('Ctrl Pts',(0.304254765406981,2.20625578040847,4.7942142217656));
#55704=CARTESIAN_POINT('Ctrl Pts',(0.304162854693844,2.20651859447494,4.79423146259749));
#55705=CARTESIAN_POINT('Ctrl Pts',(0.303890019737201,2.20729551981103,4.79428239311764));
#55706=CARTESIAN_POINT('Ctrl Pts',(0.303708130637591,2.20780929487872,4.79431602584079));
#55707=CARTESIAN_POINT('Ctrl Pts',(0.302088659480754,2.21234712755753,4.79461268370196));
#55708=CARTESIAN_POINT('Ctrl Pts',(0.300572395077036,2.21634291934177,4.79487113964616));
#55709=CARTESIAN_POINT('Ctrl Pts',(0.298879635831992,2.22054960372375,4.79514146905773));
#55710=CARTESIAN_POINT('Ctrl Pts',(0.298781960745809,2.22079148813868,4.79515700674482));
#55711=CARTESIAN_POINT('Ctrl Pts',(0.298608901267073,2.22121856164141,4.79518442962557));
#55712=CARTESIAN_POINT('Ctrl Pts',(0.298533638147916,2.22140379935112,4.79519632042079));
#55713=CARTESIAN_POINT('Ctrl Pts',(0.288243589254833,2.24666225465086,4.79681724708452));
#55714=CARTESIAN_POINT('Ctrl Pts',(0.274908960551781,2.27035150890766,4.7982823088134));
#55715=CARTESIAN_POINT('Ctrl Pts',(0.248655272503861,2.30571704761376,4.80077010726724));
#55716=CARTESIAN_POINT('Ctrl Pts',(0.237485478497587,2.31851654493557,4.80174798534859));
#55717=CARTESIAN_POINT('Ctrl Pts',(0.224143846496643,2.33156772791971,4.80287291557645));
#55718=CARTESIAN_POINT('Ctrl Pts',(0.222916913683114,2.33274906220982,4.80297598299758));
#55719=CARTESIAN_POINT('Ctrl Pts',(0.221052375225113,2.33451603860636,4.80313206757275));
#55720=CARTESIAN_POINT('Ctrl Pts',(0.220421666608549,2.33510894032972,4.80318477299008));
#55721=CARTESIAN_POINT('Ctrl Pts',(0.21939765974554,2.33606382236053,4.80327019926381));
#55722=CARTESIAN_POINT('Ctrl Pts',(0.219005833382308,2.33642738053874,4.80330285268552));
#55723=CARTESIAN_POINT('Ctrl Pts',(0.218252907105572,2.33712250946958,4.80336553465834));
#55724=CARTESIAN_POINT('Ctrl Pts',(0.217891951249932,2.33745423460845,4.80339555652448));
#55725=CARTESIAN_POINT('Ctrl Pts',(0.217245818113449,2.33804532916167,4.80344924808123));
#55726=CARTESIAN_POINT('Ctrl Pts',(0.216960929132252,2.33830501348366,4.80347290435363));
#55727=CARTESIAN_POINT('Ctrl Pts',(0.216394139896661,2.33881979898669,4.80351993523174));
#55728=CARTESIAN_POINT('Ctrl Pts',(0.216112252737284,2.33907491374995,4.80354330920985));
#55729=CARTESIAN_POINT('Ctrl Pts',(0.215426295066431,2.33969351767809,4.8036001492532));
#55730=CARTESIAN_POINT('Ctrl Pts',(0.215021756246044,2.34005648368256,4.80363363726486));
#55731=CARTESIAN_POINT('Ctrl Pts',(0.213500134666006,2.34141480221091,4.80375947633488));
#55732=CARTESIAN_POINT('Ctrl Pts',(0.212377056454096,2.34240338281396,4.80385211023167));
#55733=CARTESIAN_POINT('Ctrl Pts',(0.192193098774542,2.35992220858378,4.80551272578128));
#55734=CARTESIAN_POINT('Ctrl Pts',(0.171267145774927,2.37416196981549,4.80717858195709));
#55735=CARTESIAN_POINT('Ctrl Pts',(0.134973045136161,2.39307008041397,4.80994275748884));
#55736=CARTESIAN_POINT('Ctrl Pts',(0.120533535663463,2.3992983334101,4.81101174144656));
#55737=CARTESIAN_POINT('Ctrl Pts',(0.0996979530953711,2.40653192623375,
4.81247102143551));
#55738=CARTESIAN_POINT('Ctrl Pts',(0.0936380881739768,2.4084370655673,4.81288583197488));
#55739=CARTESIAN_POINT('Ctrl Pts',(0.0846564720144243,2.41097161295694,
4.81348286928738));
#55740=CARTESIAN_POINT('Ctrl Pts',(0.0817762387361333,2.41174141633265,
4.8136716819946));
#55741=CARTESIAN_POINT('Ctrl Pts',(0.0783961997869921,2.41259473168522,
4.81388984402913));
#55742=CARTESIAN_POINT('Ctrl Pts',(0.0779064910381102,2.41271713909021,
4.81392136845973));
#55743=CARTESIAN_POINT('Ctrl Pts',(0.0771584243834943,2.41290225925904,
4.81396939490895));
#55744=CARTESIAN_POINT('Ctrl Pts',(0.0769002759501127,2.41296580302451,
4.81398594472511));
#55745=CARTESIAN_POINT('Ctrl Pts',(0.076432352612189,2.4130803694059,4.81401590018309));
#55746=CARTESIAN_POINT('Ctrl Pts',(0.0762226058937506,2.41313150046699,
4.81402931206462));
#55747=CARTESIAN_POINT('Ctrl Pts',(0.0757970786081907,2.41323478060272,
4.81405648989239));
#55748=CARTESIAN_POINT('Ctrl Pts',(0.0755812964742037,2.41328691726399,
4.81407025507855));
#55749=CARTESIAN_POINT('Ctrl Pts',(0.0749603002214063,2.41343628166926,
4.81410982265611));
#55750=CARTESIAN_POINT('Ctrl Pts',(0.0745549492616168,2.41353294694683,
4.81413559250593));
#55751=CARTESIAN_POINT('Ctrl Pts',(0.0727755942865998,2.41395362932403,
4.8142484654288));
#55752=CARTESIAN_POINT('Ctrl Pts',(0.0713996304504149,2.41426940899893,
4.81433510075792));
#55753=CARTESIAN_POINT('Ctrl Pts',(0.0458100076429556,2.41996541149745,
4.81593503546628));
#55754=CARTESIAN_POINT('Ctrl Pts',(0.0210527262711037,2.42254245797922,
4.81729979469515));
#55755=CARTESIAN_POINT('Ctrl Pts',(-0.0181377052763326,2.42208537688345,
4.81949260754807));
#55756=CARTESIAN_POINT('Ctrl Pts',(-0.0324888165575953,2.4209554488909,
4.82030169016366));
#55757=CARTESIAN_POINT('Ctrl Pts',(-0.0551670736788468,2.41763300957231,
4.82163243785005));
#55758=CARTESIAN_POINT('Ctrl Pts',(-0.0635652816464482,2.41605944195539,
4.82213668544881));
#55759=CARTESIAN_POINT('Ctrl Pts',(-0.0735190890367058,2.41378162801453,
4.82275232407146));
#55760=CARTESIAN_POINT('Ctrl Pts',(-0.075144647552223,2.41339631190449,
4.82285343992258));
#55761=CARTESIAN_POINT('Ctrl Pts',(-0.0779756927401721,2.41270195953203,
4.82303058133914));
#55762=CARTESIAN_POINT('Ctrl Pts',(-0.0791825313281298,2.41239854483979,
4.82310642569914));
#55763=CARTESIAN_POINT('Ctrl Pts',(-0.0809139239891755,2.41195257325496,
4.82321572256215));
#55764=CARTESIAN_POINT('Ctrl Pts',(-0.0814399322665852,2.41181566426723,
4.82324899236324));
#55765=CARTESIAN_POINT('Ctrl Pts',(-0.0823518991976577,2.41157583327347,
4.8233067871556));
#55766=CARTESIAN_POINT('Ctrl Pts',(-0.0827380186489511,2.41147352287031,
4.82333129228985));
#55767=CARTESIAN_POINT('Ctrl Pts',(-0.0834798861566364,2.41127547278139,
4.82337844328639));
#55768=CARTESIAN_POINT('Ctrl Pts',(-0.0838356624413832,2.41117984036449,
4.8234010856368));
#55769=CARTESIAN_POINT('Ctrl Pts',(-0.0846731491461758,2.41095318401872,
4.82345445661156));
#55770=CARTESIAN_POINT('Ctrl Pts',(-0.0851547196179992,2.41082165072596,
4.82348520173893));
#55771=CARTESIAN_POINT('Ctrl Pts',(-0.0865755000462562,2.41043003748887,
4.82357607526605));
#55772=CARTESIAN_POINT('Ctrl Pts',(-0.0875138318464044,2.41016681735112,
4.82363630566708));
#55773=CARTESIAN_POINT('Ctrl Pts',(-0.0958083217458707,2.40779941808609,
4.82417064160083));
#55774=CARTESIAN_POINT('Ctrl Pts',(-0.103088020073232,2.40543830847302,
4.82465309972509));
#55775=CARTESIAN_POINT('Ctrl Pts',(-0.131813020240103,2.3949776981861,4.82661371616162));
#55776=CARTESIAN_POINT('Ctrl Pts',(-0.152448508420773,2.38486076554084,
4.82815789406693));
#55777=CARTESIAN_POINT('Ctrl Pts',(-0.181669467611517,2.36644429523975,
4.83049503711453));
#55778=CARTESIAN_POINT('Ctrl Pts',(-0.191163510464489,2.35971695566081,
4.83128033285603));
#55779=CARTESIAN_POINT('Ctrl Pts',(-0.204205464423418,2.34937219174579,
4.8323788449472));
#55780=CARTESIAN_POINT('Ctrl Pts',(-0.208064178027766,2.34616186775728,
4.83270648303304));
#55781=CARTESIAN_POINT('Ctrl Pts',(-0.214583399585041,2.34047521713428,
4.83326243420519));
#55782=CARTESIAN_POINT('Ctrl Pts',(-0.217279858907874,2.33804165835473,
4.83349312998607));
#55783=CARTESIAN_POINT('Ctrl Pts',(-0.220322711220529,2.33520068086404,
4.83375374112989));
#55784=CARTESIAN_POINT('Ctrl Pts',(-0.220709790269944,2.3348374881637,4.83378689854286));
#55785=CARTESIAN_POINT('Ctrl Pts',(-0.221293365339988,2.33428720769479,
4.83383689341249));
#55786=CARTESIAN_POINT('Ctrl Pts',(-0.22149052290109,2.33410082763464,4.83385378485063));
#55787=CARTESIAN_POINT('Ctrl Pts',(-0.221845843194195,2.33376408002005,
4.83388422817723));
#55788=CARTESIAN_POINT('Ctrl Pts',(-0.222004088137277,2.33361380117925,
4.83389778682475));
#55789=CARTESIAN_POINT('Ctrl Pts',(-0.222321074933184,2.33331215865124,
4.83392494755549));
#55790=CARTESIAN_POINT('Ctrl Pts',(-0.222479814201102,2.33316079431946,
4.83393854946002));
#55791=CARTESIAN_POINT('Ctrl Pts',(-0.222930173794775,2.3327304795077,4.83397714123216));
#55792=CARTESIAN_POINT('Ctrl Pts',(-0.223221426184596,2.33245114191241,
4.83400210106155));
#55793=CARTESIAN_POINT('Ctrl Pts',(-0.224449032432517,2.33126932068924,
4.83410731775268));
#55794=CARTESIAN_POINT('Ctrl Pts',(-0.225380460588576,2.33036170465509,
4.83418718125985));
#55795=CARTESIAN_POINT('Ctrl Pts',(-0.250771147196566,2.30531871838263,
4.83636600503686));
#55796=CARTESIAN_POINT('Ctrl Pts',(-0.271224248489784,2.2774270288178,4.83818434348403));
#55797=CARTESIAN_POINT('Ctrl Pts',(-0.293188683860187,2.23451005768142,
4.84093381071334));
#55798=CARTESIAN_POINT('Ctrl Pts',(-0.298691174732031,2.22180341126569,
4.84173989535427));
#55799=CARTESIAN_POINT('Ctrl Pts',(-0.304134261484152,2.20662451764932,
4.842713452436));
#55800=CARTESIAN_POINT('Ctrl Pts',(-0.304885415788433,2.20445726203305,
4.84285267810548));
#55801=CARTESIAN_POINT('Ctrl Pts',(-0.305832599472033,2.20162713184336,
4.84303483420693));
#55802=CARTESIAN_POINT('Ctrl Pts',(-0.306049733622719,2.20097134922485,
4.84307706648878));
#55803=CARTESIAN_POINT('Ctrl Pts',(-0.306398679645331,2.19990600506856,
4.84314571527919));
#55804=CARTESIAN_POINT('Ctrl Pts',(-0.306531783527915,2.19949686639042,
4.84317208915837));
#55805=CARTESIAN_POINT('Ctrl Pts',(-0.306785370610973,2.19871204414177,
4.84322269950382));
#55806=CARTESIAN_POINT('Ctrl Pts',(-0.306905984103844,2.19833640322185,
4.8432469316295));
#55807=CARTESIAN_POINT('Ctrl Pts',(-0.307179105977551,2.19748039029691,
4.84330217151592));
#55808=CARTESIAN_POINT('Ctrl Pts',(-0.307331177604268,2.19699988097611,
4.84333319356386));
#55809=CARTESIAN_POINT('Ctrl Pts',(-0.307800303592523,2.19550537911362,
4.84342972444637));
#55810=CARTESIAN_POINT('Ctrl Pts',(-0.308113469068286,2.19449018185342,
4.84349536061404));
#55811=CARTESIAN_POINT('Ctrl Pts',(-0.310498057020221,2.18662208312165,
4.84400458072169));
#55812=CARTESIAN_POINT('Ctrl Pts',(-0.312345487444632,2.17970390166747,
4.84445543271626));
#55813=CARTESIAN_POINT('Ctrl Pts',(-0.31950725476006,2.14878813394352,4.84648616264434));
#55814=CARTESIAN_POINT('Ctrl Pts',(-0.322295837656254,2.12429352717107,
4.84814582981022));
#55815=CARTESIAN_POINT('Ctrl Pts',(-0.322265261789212,2.08844506048664,
4.85057028780775));
#55816=CARTESIAN_POINT('Ctrl Pts',(-0.321663418753319,2.0771726175823,4.85133039379503));
#55817=CARTESIAN_POINT('Ctrl Pts',(-0.31966821847208,2.05839177309774,4.85257245571714));
#55818=CARTESIAN_POINT('Ctrl Pts',(-0.318597266857262,2.05085920061318,
4.85306388510344));
#55819=CARTESIAN_POINT('Ctrl Pts',(-0.317139531205371,2.0426923346232,4.85358433770952));
#55820=CARTESIAN_POINT('Ctrl Pts',(-0.317016231029612,2.04201413923544,
4.85362746337546));
#55821=CARTESIAN_POINT('Ctrl Pts',(-0.316839910972375,2.04106168939858,
4.85368789149017));
#55822=CARTESIAN_POINT('Ctrl Pts',(-0.316788710151355,2.04078710644104,
4.85370529636091));
#55823=CARTESIAN_POINT('Ctrl Pts',(-0.316699247274855,2.0403107667193,4.85373546167032));
#55824=CARTESIAN_POINT('Ctrl Pts',(-0.316661149349566,2.04010897991143,
4.85374823148886));
#55825=CARTESIAN_POINT('Ctrl Pts',(-0.316581137717659,2.03968740654789,
4.85377489163569));
#55826=CARTESIAN_POINT('Ctrl Pts',(-0.316539188019205,2.03946762737182,
4.85378877980809));
#55827=CARTESIAN_POINT('Ctrl Pts',(-0.31643842938532,2.0389427105068,4.85382192516007));
#55828=CARTESIAN_POINT('Ctrl Pts',(-0.316379407720406,2.03863761278658,
4.85384117012793));
#55829=CARTESIAN_POINT('Ctrl Pts',(-0.316178398267344,2.03760654453316,
4.85390614131245));
#55830=CARTESIAN_POINT('Ctrl Pts',(-0.316034350960006,2.03688097074001,
4.85395175058863));
#55831=CARTESIAN_POINT('Ctrl Pts',(-0.315686045254178,2.03515762419322,
4.85405982776758));
#55832=CARTESIAN_POINT('Ctrl Pts',(-0.31547955146576,2.03416030423277,4.8541221723812));
#55833=CARTESIAN_POINT('Ctrl Pts',(-0.312964366910576,2.02229607512246,
4.85486161767935));
#55834=CARTESIAN_POINT('Ctrl Pts',(-0.310099710828364,2.01155328689114,
4.85550912136439));
#55835=CARTESIAN_POINT('Ctrl Pts',(-0.297780652426222,1.97339905809882,
4.85779789265055));
#55836=CARTESIAN_POINT('Ctrl Pts',(-0.285196755739902,1.94714701531693,
4.85936438115177));
#55837=CARTESIAN_POINT('Ctrl Pts',(-0.264134978644012,1.91511812636728,
4.86159914486023));
#55838=CARTESIAN_POINT('Ctrl Pts',(-0.258660770473499,1.90753396594059,
4.86215458182131));
#55839=CARTESIAN_POINT('Ctrl Pts',(-0.252156573781885,1.89930235740854,
4.86279258404127));
#55840=CARTESIAN_POINT('Ctrl Pts',(-0.251443361930493,1.89840953114887,
4.86286226477275));
#55841=CARTESIAN_POINT('Ctrl Pts',(-0.250399203620586,1.89711657522875,
4.86296388398589));
#55842=CARTESIAN_POINT('Ctrl Pts',(-0.250072009158192,1.8967134154664,4.86299567138536));
#55843=CARTESIAN_POINT('Ctrl Pts',(-0.249492997884153,1.89600348740729,
4.86305182597509));
#55844=CARTESIAN_POINT('Ctrl Pts',(-0.249241585388863,1.89569638952329,
4.86307617677848));
#55845=CARTESIAN_POINT('Ctrl Pts',(-0.248720769463517,1.89506261014191,
4.86312655516956));
#55846=CARTESIAN_POINT('Ctrl Pts',(-0.248451288315194,1.89473599376372,
4.86315258588599));
#55847=CARTESIAN_POINT('Ctrl Pts',(-0.247760010890798,1.89390150783462,
4.86321926867271));
#55848=CARTESIAN_POINT('Ctrl Pts',(-0.247337297829863,1.89339440336402,
4.86325995807122));
#55849=CARTESIAN_POINT('Ctrl Pts',(-0.245607411054075,1.89133207556412,
4.86342612373572));
#55850=CARTESIAN_POINT('Ctrl Pts',(-0.244287125542864,1.88978795694985,
4.86355213689264));
#55851=CARTESIAN_POINT('Ctrl Pts',(-0.235490870777365,1.87969522536101,
4.86438655768729));
#55852=CARTESIAN_POINT('Ctrl Pts',(-0.227582937952363,1.87153534418111,
4.86511309085673));
#55853=CARTESIAN_POINT('Ctrl Pts',(-0.195678319830756,1.84191734953361,
4.86796076437346));
#55854=CARTESIAN_POINT('Ctrl Pts',(-0.168953727629281,1.82368343088164,
4.8702016052494));
#55855=CARTESIAN_POINT('Ctrl Pts',(-0.134698442587637,1.80716588646477,
4.87268038720507));
#55856=CARTESIAN_POINT('Ctrl Pts',(-0.129353278372291,1.80476580715939,
4.87305623874594));
#55857=CARTESIAN_POINT('Ctrl Pts',(-0.123336330879813,1.80225890397114,
4.87346495857367));
#55858=CARTESIAN_POINT('Ctrl Pts',(-0.122726622223432,1.80200706888379,
4.87350621293542));
#55859=CARTESIAN_POINT('Ctrl Pts',(-0.121869100873056,1.80165595508512,
4.87356400324145));
#55860=CARTESIAN_POINT('Ctrl Pts',(-0.121621936810504,1.80155511166799,
4.87358063321549));
#55861=CARTESIAN_POINT('Ctrl Pts',(-0.121168517609294,1.80137077256667,
4.87361109087047));
#55862=CARTESIAN_POINT('Ctrl Pts',(-0.120962300846453,1.80128718321444,
4.87362492425928));
#55863=CARTESIAN_POINT('Ctrl Pts',(-0.12054181084276,1.80111724567625,4.87365309280054));
#55864=CARTESIAN_POINT('Ctrl Pts',(-0.120327531281979,1.8010309142908,4.87366742691741));
#55865=CARTESIAN_POINT('Ctrl Pts',(-0.119791611534497,1.80081566634908,
4.87370322637883));
#55866=CARTESIAN_POINT('Ctrl Pts',(-0.119469854925936,1.80068703759638,
4.87372467421235));
#55867=CARTESIAN_POINT('Ctrl Pts',(-0.118245975170635,1.80020005466924,
4.87380608562438));
#55868=CARTESIAN_POINT('Ctrl Pts',(-0.117342430262574,1.79984525327537,
4.87386583657852));
#55869=CARTESIAN_POINT('Ctrl Pts',(-0.096995564250157,1.79196142400602,
4.87520375984501));
#55870=CARTESIAN_POINT('Ctrl Pts',(-0.0768651435166155,1.7863314655387,
4.87637331379111));
#55871=CARTESIAN_POINT('Ctrl Pts',(-0.0332567888343984,1.77859019553519,
4.87885051167343));
#55872=CARTESIAN_POINT('Ctrl Pts',(-0.00980932474648738,1.77702333968839,
4.8801534401622));
#55873=CARTESIAN_POINT('Ctrl Pts',(0.0139488372131563,1.77802682172866,
4.88156073206936));
#55874=CARTESIAN_POINT('Ctrl Pts',(0.0142977297635525,1.77804212619036,
4.88158141594368));
#55875=CARTESIAN_POINT('Ctrl Pts',(0.0203749903211787,1.77831860822223,
4.8819420125137));
#55876=CARTESIAN_POINT('Ctrl Pts',(0.0260951100757931,1.77873204799749,
4.88228624451177));
#55877=CARTESIAN_POINT('Ctrl Pts',(0.032778429286154,1.77939476741297,4.88269511973009));
#55878=CARTESIAN_POINT('Ctrl Pts',(0.0337555038563629,1.77949616770693,
4.88275506263294));
#55879=CARTESIAN_POINT('Ctrl Pts',(0.0352293743224789,1.77965593964246,
4.88284574085923));
#55880=CARTESIAN_POINT('Ctrl Pts',(0.0357265290834473,1.77971100403432,
4.88287637195565));
#55881=CARTESIAN_POINT('Ctrl Pts',(0.0366140320804729,1.77981139510296,
4.88293113320139));
#55882=CARTESIAN_POINT('Ctrl Pts',(0.0370044302345017,1.77985627884971,
4.88295524934095));
#55883=CARTESIAN_POINT('Ctrl Pts',(0.037828421228792,1.77995253974591,4.88300620848894));
#55884=CARTESIAN_POINT('Ctrl Pts',(0.0382619933879894,1.78000408420302,
4.88303305672985));
#55885=CARTESIAN_POINT('Ctrl Pts',(0.0394095694647336,1.78014287740532,
4.88310420991677));
#55886=CARTESIAN_POINT('Ctrl Pts',(0.0401233853250986,1.78023163543497,
4.88314856241899));
#55887=CARTESIAN_POINT('Ctrl Pts',(0.0433811805793674,1.78064779971001,
4.883351416637));
#55888=CARTESIAN_POINT('Ctrl Pts',(0.0459214354545084,1.78100317272342,
4.88351079937893));
#55889=CARTESIAN_POINT('Ctrl Pts',(0.0569570318977422,1.78268156086102,
4.88420864086914));
#55890=CARTESIAN_POINT('Ctrl Pts',(0.065401087692953,1.78431380999952,4.88475680122686));
#55891=CARTESIAN_POINT('Ctrl Pts',(0.0878737946854206,1.78959814530528,
4.88625498031525));
#55892=CARTESIAN_POINT('Ctrl Pts',(0.101737249171859,1.793861846152,4.88722192190025));
#55893=CARTESIAN_POINT('Ctrl Pts',(0.135926778861214,1.80695633384551,4.88969259580636));
#55894=CARTESIAN_POINT('Ctrl Pts',(0.155719355249845,1.81697652314565,4.89120658296429));
#55895=CARTESIAN_POINT('Ctrl Pts',(0.177370872869418,1.83090183886975,4.89286155542775));
#55896=CARTESIAN_POINT('Ctrl Pts',(0.18037870556673,1.83290868197584,4.89309131771158));
#55897=CARTESIAN_POINT('Ctrl Pts',(0.183826325482239,1.83529376669032,4.89335391664071));
#55898=CARTESIAN_POINT('Ctrl Pts',(0.184299494311144,1.83562298832504,4.89338994020404));
#55899=CARTESIAN_POINT('Ctrl Pts',(0.185001669839254,1.83611434955825,4.89344337043796));
#55900=CARTESIAN_POINT('Ctrl Pts',(0.185231348924223,1.83627551928286,4.8934608427724));
#55901=CARTESIAN_POINT('Ctrl Pts',(0.185639992611315,1.83656306870964,4.89349192099115));
#55902=CARTESIAN_POINT('Ctrl Pts',(0.18581903871964,1.83668933087549,4.89350553491112));
#55903=CARTESIAN_POINT('Ctrl Pts',(0.186194756266568,1.83695485855592,4.89353409666998));
#55904=CARTESIAN_POINT('Ctrl Pts',(0.186391399687352,1.8370941616814,4.89354904180288));
#55905=CARTESIAN_POINT('Ctrl Pts',(0.186913734512173,1.83746506672604,4.89358873096248));
#55906=CARTESIAN_POINT('Ctrl Pts',(0.187239152993307,1.83769705505105,4.89361344838351));
#55907=CARTESIAN_POINT('Ctrl Pts',(0.187954110498187,1.83820875120506,4.89366773526208));
#55908=CARTESIAN_POINT('Ctrl Pts',(0.188343459285105,1.83848872500367,4.89369728661286));
#55909=CARTESIAN_POINT('Ctrl Pts',(0.189499239362217,1.83932374601552,4.89378497868441));
#55910=CARTESIAN_POINT('Ctrl Pts',(0.190263860468096,1.83988130678276,4.89384295186516));
#55911=CARTESIAN_POINT('Ctrl Pts',(0.198864769113692,1.84621129423566,4.89449474605051));
#55912=CARTESIAN_POINT('Ctrl Pts',(0.206439006730695,1.85233312630594,4.89506575189868));
#55913=CARTESIAN_POINT('Ctrl Pts',(0.235457423415743,1.87804492827192,4.89729303033909));
#55914=CARTESIAN_POINT('Ctrl Pts',(0.254487949032189,1.90014927149583,4.89885814034142));
#55915=CARTESIAN_POINT('Ctrl Pts',(0.271396762730176,1.92619257382369,4.90065781662078));
#55916=CARTESIAN_POINT('Ctrl Pts',(0.272476614457511,1.92789038793251,4.90077489168021));
#55917=CARTESIAN_POINT('Ctrl Pts',(0.274882271260998,1.93175211030656,4.90104074660629));
#55918=CARTESIAN_POINT('Ctrl Pts',(0.276198546578949,1.93392177197681,4.90118980989194));
#55919=CARTESIAN_POINT('Ctrl Pts',(0.280757448272113,1.94164048492708,4.90171939884683));
#55920=CARTESIAN_POINT('Ctrl Pts',(0.283859403515536,1.94727046441732,4.90210442863076));
#55921=CARTESIAN_POINT('Ctrl Pts',(0.287260497011978,1.95390536437986,4.90255821890697));
#55922=CARTESIAN_POINT('Ctrl Pts',(0.287725767507003,1.9548238367552,4.90262103696446));
#55923=CARTESIAN_POINT('Ctrl Pts',(0.288411766273436,1.95619429187825,4.90271477325147));
#55924=CARTESIAN_POINT('Ctrl Pts',(0.288635853713503,1.9566445935449,4.90274557379243));
#55925=CARTESIAN_POINT('Ctrl Pts',(0.289033283495843,1.95744793463144,4.90280052440996));
#55926=CARTESIAN_POINT('Ctrl Pts',(0.289207035847639,1.95780077101729,4.90282466010733));
#55927=CARTESIAN_POINT('Ctrl Pts',(0.289571640620388,1.9585446011121,4.90287554367883));
#55928=CARTESIAN_POINT('Ctrl Pts',(0.289762347868402,1.95893566474493,4.9029022965523));
#55929=CARTESIAN_POINT('Ctrl Pts',(0.29026324199799,1.95996809812808,4.90297292965072));
#55930=CARTESIAN_POINT('Ctrl Pts',(0.290572093748385,1.96061010969693,4.90301685619378));
#55931=CARTESIAN_POINT('Ctrl Pts',(0.291953819240987,1.9635068574753,4.90321507413395));
#55932=CARTESIAN_POINT('Ctrl Pts',(0.293002572165233,1.96577294361475,4.90337019803546));
#55933=CARTESIAN_POINT('Ctrl Pts',(0.300553045159915,1.98259782097038,4.90452265563934));
#55934=CARTESIAN_POINT('Ctrl Pts',(0.305991679295684,1.99760683553069,4.90555635586953));
#55935=CARTESIAN_POINT('Ctrl Pts',(0.318073317936753,2.04067516462421,4.90853125377937));
#55936=CARTESIAN_POINT('Ctrl Pts',(0.322099627098489,2.06931079529919,4.91052896425579));
#55937=CARTESIAN_POINT('Ctrl Pts',(0.322293940540496,2.10226162305399,4.91265505538569));
#55938=CARTESIAN_POINT('Ctrl Pts',(0.322237854692327,2.10642402756504,4.91292020236123));
#55939=CARTESIAN_POINT('Ctrl Pts',(0.322083375255219,2.1111250913408,4.9132149238937));
#55940=CARTESIAN_POINT('Ctrl Pts',(0.322064246802898,2.11166572820254,4.91324874687412));
#55941=CARTESIAN_POINT('Ctrl Pts',(0.32203325103478,2.11248350083632,4.9132997979569));
#55942=CARTESIAN_POINT('Ctrl Pts',(0.322022387203129,2.11276067030295,4.91331708171227));
#55943=CARTESIAN_POINT('Ctrl Pts',(0.322002877802161,2.11324251786208,4.91334709518598));
#55944=CARTESIAN_POINT('Ctrl Pts',(0.321994394914889,2.11344720179584,4.91335983405732));
#55945=CARTESIAN_POINT('Ctrl Pts',(0.321976417707225,2.11387120236315,4.91338620044791));
#55946=CARTESIAN_POINT('Ctrl Pts',(0.321966894474799,2.11409051727788,4.91339982626128));
#55947=CARTESIAN_POINT('Ctrl Pts',(0.321943664635465,2.11461316615525,4.91343226907822));
#55948=CARTESIAN_POINT('Ctrl Pts',(0.321929753358055,2.11491649183373,4.91345107452457));
#55949=CARTESIAN_POINT('Ctrl Pts',(0.321899290027875,2.11556082462684,4.9134909732681));
#55950=CARTESIAN_POINT('Ctrl Pts',(0.321882624731105,2.1159018263813,4.91351206022582));
#55951=CARTESIAN_POINT('Ctrl Pts',(0.321835717218445,2.11683133998055,4.91356946292282));
#55952=CARTESIAN_POINT('Ctrl Pts',(0.321804402497657,2.11741979990875,4.91360571968249));
#55953=CARTESIAN_POINT('Ctrl Pts',(0.321701412792414,2.11926002788214,4.91371884817332));
#55954=CARTESIAN_POINT('Ctrl Pts',(0.321624045793445,2.12051148337365,4.91379541489961));
#55955=CARTESIAN_POINT('Ctrl Pts',(0.320123871491914,2.14267647295589,4.9151455171179));
#55956=CARTESIAN_POINT('Ctrl Pts',(0.316671021991063,2.1634059458373,4.91631539996858));
#55957=CARTESIAN_POINT('Ctrl Pts',(0.30416033530231,2.20995006885759,4.9190095336928));
#55958=CARTESIAN_POINT('Ctrl Pts',(0.293790381414986,2.23523860195805,4.92053236685435));
#55959=CARTESIAN_POINT('Ctrl Pts',(0.279521873082247,2.26041081259793,4.92228499936186));
#55960=CARTESIAN_POINT('Ctrl Pts',(0.278665838976018,2.26189334866414,4.92238911129845));
#55961=CARTESIAN_POINT('Ctrl Pts',(0.277474157852359,2.2639197229722,4.92253266741629));
#55962=CARTESIAN_POINT('Ctrl Pts',(0.277148634100527,2.26446950617699,4.92257174382178));
#55963=CARTESIAN_POINT('Ctrl Pts',(0.276628496067899,2.26534204799168,4.92263396535432));
#55964=CARTESIAN_POINT('Ctrl Pts',(0.276434945627879,2.26566544149166,4.92265707164365));
#55965=CARTESIAN_POINT('Ctrl Pts',(0.276057875014385,2.26629296871717,4.92270199574014));
#55966=CARTESIAN_POINT('Ctrl Pts',(0.275874418336761,2.2665971401556,4.92272381120328));
#55967=CARTESIAN_POINT('Ctrl Pts',(0.275435318834114,2.26732245359808,4.92277592753903));
#55968=CARTESIAN_POINT('Ctrl Pts',(0.275179213030766,2.26774331298386,4.92280624535523));
#55969=CARTESIAN_POINT('Ctrl Pts',(0.274411543463086,2.26899833717915,4.92289688769907));
#55970=CARTESIAN_POINT('Ctrl Pts',(0.273897147919139,2.26983075540977,4.92295731628401));
#55971=CARTESIAN_POINT('Ctrl Pts',(0.269465085201235,2.2769304097023,4.92347537566626));
#55972=CARTESIAN_POINT('Ctrl Pts',(0.265336967146784,2.28306305288221,4.92394079015998));
#55973=CARTESIAN_POINT('Ctrl Pts',(0.25733055427579,2.29411680371633,4.92481456216514));
#55974=CARTESIAN_POINT('Ctrl Pts',(0.253512465989989,2.29907729438206,4.92522054433851));
#55975=CARTESIAN_POINT('Ctrl Pts',(0.229418085230222,2.32856297125221,4.92771881997399));
#55976=CARTESIAN_POINT('Ctrl Pts',(0.205749159318426,2.35008116908336,4.92993498557596));
#55977=CARTESIAN_POINT('Ctrl Pts',(0.178597806776332,2.36826245160499,4.93205933604973));
#55978=CARTESIAN_POINT('Ctrl Pts',(0.177879215421006,2.36873947286963,4.93211527549247));
#55979=CARTESIAN_POINT('Ctrl Pts',(0.177031379824794,2.36929739957222,4.93218093515087));
#55980=CARTESIAN_POINT('Ctrl Pts',(0.176903989608042,2.36938110052481,4.93219079171582));
#55981=CARTESIAN_POINT('Ctrl Pts',(0.176281323502011,2.36978958725832,4.93223892501936));
#55982=CARTESIAN_POINT('Ctrl Pts',(0.175785208840704,2.37011309996359,4.93227713897255));
#55983=CARTESIAN_POINT('Ctrl Pts',(0.172033118376223,2.37254509505325,4.93256510292587));
#55984=CARTESIAN_POINT('Ctrl Pts',(0.1687400240406,2.37459612210321,4.93281190831192));
#55985=CARTESIAN_POINT('Ctrl Pts',(0.164905471058264,2.37688934170053,4.9330918218446));
#55986=CARTESIAN_POINT('Ctrl Pts',(0.164399587554018,2.37719000262882,4.93312860246759));
#55987=CARTESIAN_POINT('Ctrl Pts',(0.163649232140557,2.37763318338571,4.93318293591792));
#55988=CARTESIAN_POINT('Ctrl Pts',(0.163405395117226,2.37777676746829,4.93320055767154));
#55989=CARTESIAN_POINT('Ctrl Pts',(0.162972193694406,2.37803109147877,4.93323180278278));
#55990=CARTESIAN_POINT('Ctrl Pts',(0.16278290536923,2.37814195919908,4.93324543450341));
#55991=CARTESIAN_POINT('Ctrl Pts',(0.16238659063629,2.3783735408355,4.93327393153319));
#55992=CARTESIAN_POINT('Ctrl Pts',(0.16217954336044,2.37849421676593,4.93328879434037));
#55993=CARTESIAN_POINT('Ctrl Pts',(0.161632407778791,2.3788122935003,4.93332800496262));
#55994=CARTESIAN_POINT('Ctrl Pts',(0.161292091125194,2.37900930377969,4.9333523273292));
#55995=CARTESIAN_POINT('Ctrl Pts',(0.160543749364406,2.3794406942097,4.93340566712659));
#55996=CARTESIAN_POINT('Ctrl Pts',(0.160135568931605,2.37967480510382,4.93343466733614));
#55997=CARTESIAN_POINT('Ctrl Pts',(0.158926096305574,2.38036497925462,4.93352032456823));
#55998=CARTESIAN_POINT('Ctrl Pts',(0.158123350016578,2.3808185034968,4.93357682318576));
#55999=CARTESIAN_POINT('Ctrl Pts',(0.155307865814115,2.38239325525237,4.93377378738386));
#56000=CARTESIAN_POINT('Ctrl Pts',(0.153285007730874,2.38349636836024,4.9339131753335));
#56001=CARTESIAN_POINT('Ctrl Pts',(0.143727730534213,2.38857597279667,4.93456262951908));
#56002=CARTESIAN_POINT('Ctrl Pts',(0.136048807342316,2.39227469719597,4.93505813523177));
#56003=CARTESIAN_POINT('Ctrl Pts',(0.101801745661704,2.40712785768207,4.93719304753925));
#56004=CARTESIAN_POINT('Ctrl Pts',(0.0739545566416514,2.41499518762634,
4.93874921222989));
#56005=CARTESIAN_POINT('Ctrl Pts',(0.0355731158524276,2.42046042553011,
4.9410035141464));
#56006=CARTESIAN_POINT('Ctrl Pts',(0.0256560087534891,2.4214063929849,4.94159402708941));
#56007=CARTESIAN_POINT('Ctrl Pts',(0.0146678372804947,2.42194273162756,
4.94226296312359));
#56008=CARTESIAN_POINT('Ctrl Pts',(0.0136237293338335,2.42198860516654,
4.94232666906711));
#56009=CARTESIAN_POINT('Ctrl Pts',(0.0120627116730934,2.42204958315988,
4.94242213388536));
#56010=CARTESIAN_POINT('Ctrl Pts',(0.0115459516608255,2.42206852379841,
4.94245377258649));
#56011=CARTESIAN_POINT('Ctrl Pts',(0.0106563176493978,2.42209898740388,
4.94250830329072));
#56012=CARTESIAN_POINT('Ctrl Pts',(0.0102834639957898,2.42211110685414,
4.94253117656916));
#56013=CARTESIAN_POINT('Ctrl Pts',(0.00951430126319144,2.42213477131627,
4.94257840150632));
#56014=CARTESIAN_POINT('Ctrl Pts',(0.00911799037340792,2.42214623243005,
4.94260275575507));
#56015=CARTESIAN_POINT('Ctrl Pts',(0.00819614545506967,2.42217118926649,
4.94265945604237));
#56016=CARTESIAN_POINT('Ctrl Pts',(0.0076705986699563,2.42218413043557,
4.94269181939801));
#56017=CARTESIAN_POINT('Ctrl Pts',(0.00599829233637522,2.42222121555949,
4.94279492396209));
#56018=CARTESIAN_POINT('Ctrl Pts',(0.00485144411905283,2.42224052306163,
4.94286581645272));
#56019=CARTESIAN_POINT('Ctrl Pts',(-0.0183774249295346,2.42250755496071,
4.9443055311557));
#56020=CARTESIAN_POINT('Ctrl Pts',(-0.0404223272764245,2.42049107446837,
4.94574808159247));
#56021=CARTESIAN_POINT('Ctrl Pts',(-0.0643358711676005,2.41579635396005,
4.94738540654633));
#56022=CARTESIAN_POINT('Ctrl Pts',(-0.0665828307877071,2.41533025221395,
4.94753990778047));
#56023=CARTESIAN_POINT('Ctrl Pts',(-0.0707411789875144,2.41442123023292,
4.94782694680699));
#56024=CARTESIAN_POINT('Ctrl Pts',(-0.0726538807611539,2.41398477345302,
4.94795941364434));
#56025=CARTESIAN_POINT('Ctrl Pts',(-0.0906458012331739,2.40970601789076,
4.94920922434033));
#56026=CARTESIAN_POINT('Ctrl Pts',(-0.106411610203028,2.40464913410129,
4.95033431165134));
#56027=CARTESIAN_POINT('Ctrl Pts',(-0.128772903870237,2.39552788300091,
4.95192261183336));
#56028=CARTESIAN_POINT('Ctrl Pts',(-0.135721989468169,2.39240170012366,
4.95241481061547));
#56029=CARTESIAN_POINT('Ctrl Pts',(-0.143172776405399,2.38872687298559,
4.95293600480697));
#56030=CARTESIAN_POINT('Ctrl Pts',(-0.143790213867807,2.38841987709633,
4.95297914523595));
#56031=CARTESIAN_POINT('Ctrl Pts',(-0.144656409135474,2.38798572353584,
4.95303959060412));
#56032=CARTESIAN_POINT('Ctrl Pts',(-0.144905988589138,2.38786022326276,
4.95305699804221));
#56033=CARTESIAN_POINT('Ctrl Pts',(-0.145338757143185,2.38764190145123,
4.95308716657351));
#56034=CARTESIAN_POINT('Ctrl Pts',(-0.145522020748349,2.38754922930911,
4.95309993705138));
#56035=CARTESIAN_POINT('Ctrl Pts',(-0.14589015847889,2.3873626285457,4.95312558013461));
#56036=CARTESIAN_POINT('Ctrl Pts',(-0.146075030331999,2.38726869676218,
4.95313845246242));
#56037=CARTESIAN_POINT('Ctrl Pts',(-0.146521737729971,2.38704118589238,
4.95316954381583));
#56038=CARTESIAN_POINT('Ctrl Pts',(-0.146783482308285,2.3869074264445,4.95318775143665));
#56039=CARTESIAN_POINT('Ctrl Pts',(-0.147622961103616,2.38647697774722,
4.95324611644008));
#56040=CARTESIAN_POINT('Ctrl Pts',(-0.1481999862815,2.38617889773293,4.95328618666301));
#56041=CARTESIAN_POINT('Ctrl Pts',(-0.149551259978411,2.38547567295452,
4.95337992023138));
#56042=CARTESIAN_POINT('Ctrl Pts',(-0.150324773973997,2.38506911719797,
4.95343349712333));
#56043=CARTESIAN_POINT('Ctrl Pts',(-0.152988342000505,2.38365530073962,
4.95361774609478));
#56044=CARTESIAN_POINT('Ctrl Pts',(-0.15487004916085,2.38263232448624,4.9537474901944));
#56045=CARTESIAN_POINT('Ctrl Pts',(-0.162762212164817,2.37823931880452,
4.95429046856925));
#56046=CARTESIAN_POINT('Ctrl Pts',(-0.168674362870796,2.37469552090784,
4.95469430417393));
#56047=CARTESIAN_POINT('Ctrl Pts',(-0.179591400865977,2.36766625739586,
4.95544310770418));
#56048=CARTESIAN_POINT('Ctrl Pts',(-0.18461969152328,2.36422314723462,4.95578931756166));
#56049=CARTESIAN_POINT('Ctrl Pts',(-0.208382651068145,2.34694176439733,
4.95744652111076));
#56050=CARTESIAN_POINT('Ctrl Pts',(-0.225676777211939,2.33124347392579,
4.95872327563729));
#56051=CARTESIAN_POINT('Ctrl Pts',(-0.243510518413488,2.31113193993891,
4.96027835107427));
#56052=CARTESIAN_POINT('Ctrl Pts',(-0.245847687628171,2.3084058105027,4.96048750253086));
#56053=CARTESIAN_POINT('Ctrl Pts',(-0.249426807870841,2.30408703493889,
4.96081680344968));
#56054=CARTESIAN_POINT('Ctrl Pts',(-0.250700201293458,2.3025207622361,4.96093582178142));
#56055=CARTESIAN_POINT('Ctrl Pts',(-0.255625107782704,2.29634550081298,
4.9614036739144));
#56056=CARTESIAN_POINT('Ctrl Pts',(-0.259164738971889,2.29164911354047,
4.96175650744875));
#56057=CARTESIAN_POINT('Ctrl Pts',(-0.263147745531854,2.2860521959901,4.96217469634275));
#56058=CARTESIAN_POINT('Ctrl Pts',(-0.26371800117585,2.28524300643413,4.96223510156464));
#56059=CARTESIAN_POINT('Ctrl Pts',(-0.26457170138322,2.28401967907161,4.96232634352333));
#56060=CARTESIAN_POINT('Ctrl Pts',(-0.26485792528649,2.28360748042186,4.96235707408239));
#56061=CARTESIAN_POINT('Ctrl Pts',(-0.265366673574097,2.28287115343142,
4.9624119463717));
#56062=CARTESIAN_POINT('Ctrl Pts',(-0.265589570266834,2.28254728254462,
4.96243607387539));
#56063=CARTESIAN_POINT('Ctrl Pts',(-0.266058238527429,2.28186362798819,
4.96248698809765));
#56064=CARTESIAN_POINT('Ctrl Pts',(-0.266303874046762,2.28150375240767,
4.96251377991105));
#56065=CARTESIAN_POINT('Ctrl Pts',(-0.266950802510136,2.28055181041424,
4.96258462536978));
#56066=CARTESIAN_POINT('Ctrl Pts',(-0.267350853876713,2.27995890676172,
4.9626287258372));
#56067=CARTESIAN_POINT('Ctrl Pts',(-0.269153972644418,2.27726727810525,
4.96282882397911));
#56068=CARTESIAN_POINT('Ctrl Pts',(-0.270534292955428,2.27515348877182,
4.96298567365845));
#56069=CARTESIAN_POINT('Ctrl Pts',(-0.27646299142556,2.26583712897176,4.96367587801448));
#56070=CARTESIAN_POINT('Ctrl Pts',(-0.280749260932982,2.25847261461545,
4.96421877064474));
#56071=CARTESIAN_POINT('Ctrl Pts',(-0.298757239437896,2.22450342002641,
4.96671262057183));
#56072=CARTESIAN_POINT('Ctrl Pts',(-0.309022719174845,2.19623639185006,
4.96877833908566));
#56073=CARTESIAN_POINT('Ctrl Pts',(-0.315558407868929,2.16547067616215,
4.97086902698191));
#56074=CARTESIAN_POINT('Ctrl Pts',(-0.315865786832819,2.16397126731309,
4.97097049201869));
#56075=CARTESIAN_POINT('Ctrl Pts',(-0.31784894469439,2.15393440094963,4.97164660841912));
#56076=CARTESIAN_POINT('Ctrl Pts',(-0.31918926896389,2.14533336180689,4.97221121623603));
#56077=CARTESIAN_POINT('Ctrl Pts',(-0.320260804481919,2.13598190569201,
4.97280187248485));
#56078=CARTESIAN_POINT('Ctrl Pts',(-0.320339353353755,2.13527575853472,
4.97284633134776));
#56079=CARTESIAN_POINT('Ctrl Pts',(-0.320445921569804,2.1342880015794,4.97290831526014));
#56080=CARTESIAN_POINT('Ctrl Pts',(-0.320475905508153,2.13400661249329,
4.97292594978955));
#56081=CARTESIAN_POINT('Ctrl Pts',(-0.320527107307109,2.13352001886538,
4.97295640376962));
#56082=CARTESIAN_POINT('Ctrl Pts',(-0.32054849876368,2.13331483339738,4.97296923303459));
#56083=CARTESIAN_POINT('Ctrl Pts',(-0.320591059542951,2.13290275699368,
4.9729949729349));
#56084=CARTESIAN_POINT('Ctrl Pts',(-0.320612225587194,2.1326958664191,4.973007883319));
#56085=CARTESIAN_POINT('Ctrl Pts',(-0.320655156004477,2.13227218653559,
4.97303429580221));
#56086=CARTESIAN_POINT('Ctrl Pts',(-0.320676900863282,2.13205539501295,
4.97304779680586));
#56087=CARTESIAN_POINT('Ctrl Pts',(-0.320726893598553,2.13155183640301,
4.97307912465446));
#56088=CARTESIAN_POINT('Ctrl Pts',(-0.320754976805667,2.13126505259401,
4.97309694222366));
#56089=CARTESIAN_POINT('Ctrl Pts',(-0.320826916153189,2.13052011344701,
4.9731431628323));
#56090=CARTESIAN_POINT('Ctrl Pts',(-0.320870175738407,2.13006189915664,
4.97317153271127));
#56091=CARTESIAN_POINT('Ctrl Pts',(-0.32181409468499,2.1198295138048,4.97380374020075));
#56092=CARTESIAN_POINT('Ctrl Pts',(-0.322268816889106,2.11001837458985,
4.9743830666047));
#56093=CARTESIAN_POINT('Ctrl Pts',(-0.322274937371842,2.10020091534284,
4.97494943677011));
#56094=CARTESIAN_POINT('',(-0.322021731191934,2.09973199008727,5.22472278440197));
#56095=CARTESIAN_POINT('Ctrl Pts',(-0.322274937078364,2.10020138554251,
4.97494940964423));
#56096=CARTESIAN_POINT('Ctrl Pts',(-0.322285045080913,2.08402566684362,
4.97588258911077));
#56097=CARTESIAN_POINT('Ctrl Pts',(-0.321077299150837,2.06787059725422,
4.97677927466193));
#56098=CARTESIAN_POINT('Ctrl Pts',(-0.314995452800083,2.02760098425642,
4.97905824022963));
#56099=CARTESIAN_POINT('Ctrl Pts',(-0.308569406782582,2.00383133143984,
4.98044985199316));
#56100=CARTESIAN_POINT('Ctrl Pts',(-0.299083168913247,1.97995099337579,
4.98201236551914));
#56101=CARTESIAN_POINT('Ctrl Pts',(-0.298651617283599,1.97888139136204,
4.98208269263931));
#56102=CARTESIAN_POINT('Ctrl Pts',(-0.298014570617035,1.97732657602321,
4.98218543030167));
#56103=CARTESIAN_POINT('Ctrl Pts',(-0.297813609123736,1.97683950525542,
4.98221768735976));
#56104=CARTESIAN_POINT('Ctrl Pts',(-0.297459266665263,1.97598662312765,
4.98227429953891));
#56105=CARTESIAN_POINT('Ctrl Pts',(-0.297306402710333,1.97562059706895,
4.98229863707631));
#56106=CARTESIAN_POINT('Ctrl Pts',(-0.297008598236242,1.97491120310649,
4.98234588680405));
#56107=CARTESIAN_POINT('Ctrl Pts',(-0.296863736989732,1.97456780240623,
4.98236879626946));
#56108=CARTESIAN_POINT('Ctrl Pts',(-0.296516977586349,1.9737497577096,4.98242345954799));
#56109=CARTESIAN_POINT('Ctrl Pts',(-0.29631453545269,1.9732753467164,4.98245523185294));
#56110=CARTESIAN_POINT('Ctrl Pts',(-0.295700521480166,1.97184595754359,
4.98255117746212));
#56111=CARTESIAN_POINT('Ctrl Pts',(-0.295285468521383,1.97089249037709,
4.98261546947633));
#56112=CARTESIAN_POINT('Ctrl Pts',(-0.290926355204326,1.96100963677147,
4.98328493776214));
#56113=CARTESIAN_POINT('Ctrl Pts',(-0.2865835314591,1.95226269427122,4.98390380151509));
#56114=CARTESIAN_POINT('Ctrl Pts',(-0.269002211865862,1.92055337908637,
4.98625051312027));
#56115=CARTESIAN_POINT('Ctrl Pts',(-0.253345668210878,1.89905508372831,
4.98806199798688));
#56116=CARTESIAN_POINT('Ctrl Pts',(-0.231727110796095,1.87596847033774,
4.99018778715869));
#56117=CARTESIAN_POINT('Ctrl Pts',(-0.228125502853717,1.8723020890074,4.99053127295136));
#56118=CARTESIAN_POINT('Ctrl Pts',(-0.219891384771832,1.8643114613683,4.99129062357023));
#56119=CARTESIAN_POINT('Ctrl Pts',(-0.215215694283978,1.8600343265057,4.99170457842632));
#56120=CARTESIAN_POINT('Ctrl Pts',(-0.208106270461783,1.8539059937815,4.9923053726836));
#56121=CARTESIAN_POINT('Ctrl Pts',(-0.205767634006069,1.8519472593076,4.99249863541314));
#56122=CARTESIAN_POINT('Ctrl Pts',(-0.203008678567032,1.84970236029569,
4.99272124499645));
#56123=CARTESIAN_POINT('Ctrl Pts',(-0.202615163983639,1.84938370494463,
4.99275287033279));
#56124=CARTESIAN_POINT('Ctrl Pts',(-0.202051548841236,1.84892950284937,
4.99279798443158));
#56125=CARTESIAN_POINT('Ctrl Pts',(-0.201882062134013,1.84879320089258,
4.99281152745962));
#56126=CARTESIAN_POINT('Ctrl Pts',(-0.201550025902481,1.84852672895536,
4.99283801321791));
#56127=CARTESIAN_POINT('Ctrl Pts',(-0.201387487766252,1.84839654461164,
4.99285095698887));
#56128=CARTESIAN_POINT('Ctrl Pts',(-0.201063352672803,1.84813744508352,
4.9928767265649));
#56129=CARTESIAN_POINT('Ctrl Pts',(-0.20090175815639,1.8480085280662,4.99288955251658));
#56130=CARTESIAN_POINT('Ctrl Pts',(-0.200517398105693,1.84770249768361,
4.99292000952176));
#56131=CARTESIAN_POINT('Ctrl Pts',(-0.200294521334867,1.84752552338336,
4.99293763052492));
#56132=CARTESIAN_POINT('Ctrl Pts',(-0.199625109026554,1.84699542383421,
4.99299043666155));
#56133=CARTESIAN_POINT('Ctrl Pts',(-0.199177868935805,1.84664318392328,
4.9930255587589));
#56134=CARTESIAN_POINT('Ctrl Pts',(-0.194800624192822,1.84321448263786,
4.99336779169078));
#56135=CARTESIAN_POINT('Ctrl Pts',(-0.190800324775829,1.84022831586212,
4.99366865473377));
#56136=CARTESIAN_POINT('Ctrl Pts',(-0.186472322953587,1.83715146963094,
4.99398362557414));
#56137=CARTESIAN_POINT('Ctrl Pts',(-0.186212361882987,1.83696723886878,
4.99400250457603));
#56138=CARTESIAN_POINT('Ctrl Pts',(-0.184431822847895,1.83570935842939,
4.99413154346191));
#56139=CARTESIAN_POINT('Ctrl Pts',(-0.182902211796027,1.83464849408067,
4.9942410609518));
#56140=CARTESIAN_POINT('Ctrl Pts',(-0.170434786230683,1.82616071882682,
4.99512368523359));
#56141=CARTESIAN_POINT('Ctrl Pts',(-0.159057739484304,1.81939946929525,
4.99586745403962));
#56142=CARTESIAN_POINT('Ctrl Pts',(-0.13746713155384,1.80830478646286,4.99722617819139));
#56143=CARTESIAN_POINT('Ctrl Pts',(-0.127384300725526,1.80376268755188,
4.99784129090588));
#56144=CARTESIAN_POINT('Ctrl Pts',(-0.101031843765891,1.79348612395394,
4.99943781658683));
#56145=CARTESIAN_POINT('Ctrl Pts',(-0.0845012519627029,1.78852350216596,
5.00043034144248));
#56146=CARTESIAN_POINT('Ctrl Pts',(-0.0651026808327272,1.7843583852689,
5.00162606144927));
#56147=CARTESIAN_POINT('Ctrl Pts',(-0.0625442860651763,1.78384149597908,
5.00178431716365));
#56148=CARTESIAN_POINT('Ctrl Pts',(-0.0592688166274296,1.78322104416558,
5.0019877296404));
#56149=CARTESIAN_POINT('Ctrl Pts',(-0.0585572342652978,1.78308873515493,
5.00203196816155));
#56150=CARTESIAN_POINT('Ctrl Pts',(-0.0574146976721475,1.7828802755536,
5.00210307783264));
#56151=CARTESIAN_POINT('Ctrl Pts',(-0.056984020711297,1.78280260322265,
5.00212990048609));
#56152=CARTESIAN_POINT('Ctrl Pts',(-0.0561665108796347,1.78265688450705,
5.00218084983699));
#56153=CARTESIAN_POINT('Ctrl Pts',(-0.0557797088943821,1.78258866754848,
5.00220497105818));
#56154=CARTESIAN_POINT('Ctrl Pts',(-0.05490175715466,1.78243548508362,5.00225975449271));
#56155=CARTESIAN_POINT('Ctrl Pts',(-0.0544105339023778,1.78235095172698,
5.00229043038341));
#56156=CARTESIAN_POINT('Ctrl Pts',(-0.0529586595425619,1.78210456899808,
5.00238116889875));
#56157=CARTESIAN_POINT('Ctrl Pts',(-0.0519974748410022,1.78194593659375,
5.00244133350966));
#56158=CARTESIAN_POINT('Ctrl Pts',(-0.0455260274660343,1.78090801858261,
5.00284705095586));
#56159=CARTESIAN_POINT('Ctrl Pts',(-0.0399947413692446,1.78016765930278,
5.00319698100972));
#56160=CARTESIAN_POINT('Ctrl Pts',(-0.0325023336891928,1.7793621973218,
5.003675625501));
#56161=CARTESIAN_POINT('Ctrl Pts',(-0.0305555478140931,1.77917082359186,
5.00380041271909));
#56162=CARTESIAN_POINT('Ctrl Pts',(-0.0048009350987952,1.7768756204169,
5.00545684222292));
#56163=CARTESIAN_POINT('Ctrl Pts',(0.0191640134420057,1.77740923559079,
5.00706951958968));
#56164=CARTESIAN_POINT('Ctrl Pts',(0.0535259227642527,1.78201842300329,
5.00941478483482));
#56165=CARTESIAN_POINT('Ctrl Pts',(0.0641286817172353,1.78398600873702,
5.01014172067818));
#56166=CARTESIAN_POINT('Ctrl Pts',(0.0795297220992006,1.78765125519509,
5.01118703679555));
#56167=CARTESIAN_POINT('Ctrl Pts',(0.0844181516588503,1.78893682889579,
5.0115171786066));
#56168=CARTESIAN_POINT('Ctrl Pts',(0.0916596000014079,1.79102450830991,
5.01200182180603));
#56169=CARTESIAN_POINT('Ctrl Pts',(0.0940366823353032,1.7917396555413,5.0121601912217));
#56170=CARTESIAN_POINT('Ctrl Pts',(0.0973345286285136,1.79277351449441,
5.01237867326754));
#56171=CARTESIAN_POINT('Ctrl Pts',(0.0982624009441628,1.79306902327,5.01244000804325));
#56172=CARTESIAN_POINT('Ctrl Pts',(0.0996548334102818,1.79351944665416,
5.01253183071055));
#56173=CARTESIAN_POINT('Ctrl Pts',(0.100120393080221,1.79367121862601,5.01256249441605));
#56174=CARTESIAN_POINT('Ctrl Pts',(0.100971991974085,1.79395098780339,5.01261851379667));
#56175=CARTESIAN_POINT('Ctrl Pts',(0.101358137245699,1.79407865545512,5.01264388839978));
#56176=CARTESIAN_POINT('Ctrl Pts',(0.101974146494986,1.79428361528847,5.01268432432849));
#56177=CARTESIAN_POINT('Ctrl Pts',(0.102204165083954,1.7943604360118,5.01269941342867));
#56178=CARTESIAN_POINT('Ctrl Pts',(0.102641565350218,1.7945070662561,5.01272808785687));
#56179=CARTESIAN_POINT('Ctrl Pts',(0.102848960970675,1.79457682679176,5.01274167589739));
#56180=CARTESIAN_POINT('Ctrl Pts',(0.103319718082555,1.79473570667262,5.01277250052962));
#56181=CARTESIAN_POINT('Ctrl Pts',(0.103583034892043,1.79482495546117,5.01278972930331));
#56182=CARTESIAN_POINT('Ctrl Pts',(0.104379841921049,1.79509617590237,5.01284182609504));
#56183=CARTESIAN_POINT('Ctrl Pts',(0.104912974113302,1.7952792077608,5.01287663148807));
#56184=CARTESIAN_POINT('Ctrl Pts',(0.108620466812036,1.79656292605023,5.0131183310444));
#56185=CARTESIAN_POINT('Ctrl Pts',(0.111778073282456,1.79771184583542,5.01332242958655));
#56186=CARTESIAN_POINT('Ctrl Pts',(0.137235139330595,1.80742806616125,5.01495803001313));
#56187=CARTESIAN_POINT('Ctrl Pts',(0.158539998096427,1.81840238153108,5.01626889402307));
#56188=CARTESIAN_POINT('Ctrl Pts',(0.197976332303377,1.84462369416768,5.01892183769232));
#56189=CARTESIAN_POINT('Ctrl Pts',(0.216034177682866,1.85970710688899,5.02025711030116));
#56190=CARTESIAN_POINT('Ctrl Pts',(0.233091693737246,1.87744492204922,5.02175356272773));
#56191=CARTESIAN_POINT('Ctrl Pts',(0.233885045666559,1.87827881073132,5.02182374491815));
#56192=CARTESIAN_POINT('Ctrl Pts',(0.235034730272235,1.87950027586249,5.02192630967003));
#56193=CARTESIAN_POINT('Ctrl Pts',(0.235394613413208,1.87988451042756,5.02195853948149));
#56194=CARTESIAN_POINT('Ctrl Pts',(0.236023954099939,1.88055974388594,5.02201512010935));
#56195=CARTESIAN_POINT('Ctrl Pts',(0.236293819689449,1.88085036233963,5.02203945340265));
#56196=CARTESIAN_POINT('Ctrl Pts',(0.236816341037455,1.88141515320515,5.02208670687443));
#56197=CARTESIAN_POINT('Ctrl Pts',(0.23706905894509,1.88168926751126,5.02210962435014));
#56198=CARTESIAN_POINT('Ctrl Pts',(0.237739473036178,1.88241897917038,5.02217058915443));
#56199=CARTESIAN_POINT('Ctrl Pts',(0.23815633363553,1.88287533902027,5.02220867185819));
#56200=CARTESIAN_POINT('Ctrl Pts',(0.239635076218769,1.88450358059975,5.02234439114973));
#56201=CARTESIAN_POINT('Ctrl Pts',(0.240689629006266,1.88568206123985,5.02244233604848));
#56202=CARTESIAN_POINT('Ctrl Pts',(0.259141142097004,1.90660988922329,5.02417685142317));
#56203=CARTESIAN_POINT('Ctrl Pts',(0.274059139456869,1.9284049288921,5.02592064059716));
#56204=CARTESIAN_POINT('Ctrl Pts',(0.293787468080232,1.96648934222579,5.02882061511528));
#56205=CARTESIAN_POINT('Ctrl Pts',(0.300267564250743,1.98178148318281,5.0299482434542));
#56206=CARTESIAN_POINT('Ctrl Pts',(0.307094746972246,2.00213363090361,5.03135562599535));
#56207=CARTESIAN_POINT('Ctrl Pts',(0.30854212526078,2.00679714375217,5.03167191579786));
#56208=CARTESIAN_POINT('Ctrl Pts',(0.310320612606232,2.01302396104813,5.03208448085106));
#56209=CARTESIAN_POINT('Ctrl Pts',(0.310746809413888,2.01455917464978,5.0321854199144));
#56210=CARTESIAN_POINT('Ctrl Pts',(0.311344605301387,2.01677616675163,5.03233000337358));
#56211=CARTESIAN_POINT('Ctrl Pts',(0.311525378488111,2.01745541659061,5.03237414205912));
#56212=CARTESIAN_POINT('Ctrl Pts',(0.311842432005389,2.01866261308421,5.03245229818241));
#56213=CARTESIAN_POINT('Ctrl Pts',(0.311979596768773,2.01919032162126,5.03248636504559));
#56214=CARTESIAN_POINT('Ctrl Pts',(0.312180118579282,2.01996990167836,5.03253654463823));
#56215=CARTESIAN_POINT('Ctrl Pts',(0.312244510550553,2.02022150223443,5.03255271693116));
#56216=CARTESIAN_POINT('Ctrl Pts',(0.312361825730554,2.02068220895086,5.0325822883727));
#56217=CARTESIAN_POINT('Ctrl Pts',(0.312414843192067,2.02089129058684,5.03259569299979));
#56218=CARTESIAN_POINT('Ctrl Pts',(0.312519471399414,2.02130565189407,5.03262222722457));
#56219=CARTESIAN_POINT('Ctrl Pts',(0.312571089637877,2.02151092846271,5.03263535724331));
#56220=CARTESIAN_POINT('Ctrl Pts',(0.312711262192331,2.02207070106962,5.03267112078711));
#56221=CARTESIAN_POINT('Ctrl Pts',(0.312799416272429,2.02242529847646,5.03269373105243));
#56222=CARTESIAN_POINT('Ctrl Pts',(0.313130266685761,2.02376586886925,5.03277904370457));
#56223=CARTESIAN_POINT('Ctrl Pts',(0.313368909141737,2.0247528504716,5.03284151438046));
#56224=CARTESIAN_POINT('Ctrl Pts',(0.31775834800345,2.04328986196905,5.03400872135404));
#56225=CARTESIAN_POINT('Ctrl Pts',(0.32043413285657,2.06115956095556,5.03503251121383));
#56226=CARTESIAN_POINT('Ctrl Pts',(0.321702277965392,2.08073103206813,5.03613286385662));
#56227=CARTESIAN_POINT('Ctrl Pts',(0.321792475893252,2.08230109426493,5.03622098277257));
#56228=CARTESIAN_POINT('Ctrl Pts',(0.322671373706601,2.09984125062288,5.03720423402327));
#56229=CARTESIAN_POINT('Ctrl Pts',(0.322281959900942,2.1158479015747,5.03809191552928));
#56230=CARTESIAN_POINT('Ctrl Pts',(0.319277074930664,2.14619171240716,5.03983607345623));
#56231=CARTESIAN_POINT('Ctrl Pts',(0.316875384936777,2.16050975003607,5.04068567357673));
#56232=CARTESIAN_POINT('Ctrl Pts',(0.313263205060972,2.1756871980551,5.04163473331104));
#56233=CARTESIAN_POINT('Ctrl Pts',(0.313002831729384,2.17675685556859,5.04170187709708));
#56234=CARTESIAN_POINT('Ctrl Pts',(0.312612150057299,2.17832679294692,5.04180080945977));
#56235=CARTESIAN_POINT('Ctrl Pts',(0.312486108524085,2.17882813477021,5.04183246028464));
#56236=CARTESIAN_POINT('Ctrl Pts',(0.312261592242,2.17971216836523,5.04188837430691));
#56237=CARTESIAN_POINT('Ctrl Pts',(0.312163618613665,2.18009498727615,5.04191262126205));
#56238=CARTESIAN_POINT('Ctrl Pts',(0.311971106357432,2.18084148454154,5.04195996986228));
#56239=CARTESIAN_POINT('Ctrl Pts',(0.311876635219036,2.18120517980618,5.04198306929006));
#56240=CARTESIAN_POINT('Ctrl Pts',(0.31164807551653,2.18207880763858,5.0420386312419));
#56241=CARTESIAN_POINT('Ctrl Pts',(0.311513371500428,2.18258857673849,5.04207111366669));
#56242=CARTESIAN_POINT('Ctrl Pts',(0.311097370856156,2.18414737706962,5.04217063004478));
#56243=CARTESIAN_POINT('Ctrl Pts',(0.310812023904342,2.18519531073634,5.04223779526339));
#56244=CARTESIAN_POINT('Ctrl Pts',(0.307401108742523,2.19747662277672,5.04302807715991));
#56245=CARTESIAN_POINT('Ctrl Pts',(0.303673786495036,2.20853252481737,5.0437708343792));
#56246=CARTESIAN_POINT('Ctrl Pts',(0.289255985146281,2.24469216422925,5.04630973299465));
#56247=CARTESIAN_POINT('Ctrl Pts',(0.275981755803391,2.26863738590936,5.0481853382273));
#56248=CARTESIAN_POINT('Ctrl Pts',(0.253661686238835,2.29906426559523,5.05070377191487));
#56249=CARTESIAN_POINT('Ctrl Pts',(0.247059235152875,2.30720187155542,5.05139128886121));
#56250=CARTESIAN_POINT('Ctrl Pts',(0.239413697998304,2.31573879830375,5.05211587425953));
#56251=CARTESIAN_POINT('Ctrl Pts',(0.238752494286659,2.31647030838679,5.05217798906159));
#56252=CARTESIAN_POINT('Ctrl Pts',(0.237754891682736,2.3175638556859,5.05227087026417));
#56253=CARTESIAN_POINT('Ctrl Pts',(0.237421007742963,2.31792816456326,5.05230181723936));
#56254=CARTESIAN_POINT('Ctrl Pts',(0.23688152300107,2.31851409810551,5.05235159516165));
#56255=CARTESIAN_POINT('Ctrl Pts',(0.23667644760993,2.31873620221328,5.05237046505801));
#56256=CARTESIAN_POINT('Ctrl Pts',(0.236283789201891,2.31916026683631,5.05240649491942));
#56257=CARTESIAN_POINT('Ctrl Pts',(0.236096259156231,2.31936227572936,5.05242365886563));
#56258=CARTESIAN_POINT('Ctrl Pts',(0.235761926266498,2.3197214964769,5.05245418124618));
#56259=CARTESIAN_POINT('Ctrl Pts',(0.235615225219009,2.31987880192731,5.05246754745773));
#56260=CARTESIAN_POINT('Ctrl Pts',(0.235322598288376,2.32019195248919,5.05249415615056));
#56261=CARTESIAN_POINT('Ctrl Pts',(0.235176675583811,2.32034779887298,5.05250739877382));
#56262=CARTESIAN_POINT('Ctrl Pts',(0.234774322725495,2.32077665933305,5.05254384099689));
#56263=CARTESIAN_POINT('Ctrl Pts',(0.234517570276904,2.32104937265749,5.05256701577288));
#56264=CARTESIAN_POINT('Ctrl Pts',(0.233444142118669,2.32218555458504,5.05266357452925));
#56265=CARTESIAN_POINT('Ctrl Pts',(0.232623155139511,2.3230449639695,5.05273663027835));
#56266=CARTESIAN_POINT('Ctrl Pts',(0.218533372782861,2.33763173342188,5.05397733815393));
#56267=CARTESIAN_POINT('Ctrl Pts',(0.204073050422405,2.3501601476604,5.05505520457786));
#56268=CARTESIAN_POINT('Ctrl Pts',(0.175155981008347,2.37102741479991,5.0570524258703));
#56269=CARTESIAN_POINT('Ctrl Pts',(0.160998725708501,2.37966920374122,5.05797113804771));
#56270=CARTESIAN_POINT('Ctrl Pts',(0.140343932853513,2.39018708462406,5.05929804833022));
#56271=CARTESIAN_POINT('Ctrl Pts',(0.13435639512478,2.39300736378414,5.05968102060005));
#56272=CARTESIAN_POINT('Ctrl Pts',(0.121124344038216,2.39874909985578,5.06052824351389));
#56273=CARTESIAN_POINT('Ctrl Pts',(0.113852095929765,2.40159545122321,5.0609944560831));
#56274=CARTESIAN_POINT('Ctrl Pts',(0.10554948159414,2.40450199200812,5.0615300147376));
#56275=CARTESIAN_POINT('Ctrl Pts',(0.104613361828836,2.40482486889071,5.06159044383869));
#56276=CARTESIAN_POINT('Ctrl Pts',(0.103207043588835,2.40530268071623,5.06168129791067));
#56277=CARTESIAN_POINT('Ctrl Pts',(0.102737945945071,2.40546085699733,5.06171161562632));
#56278=CARTESIAN_POINT('Ctrl Pts',(0.101931307225233,2.40573078133177,5.06176376993145));
#56279=CARTESIAN_POINT('Ctrl Pts',(0.101593941276093,2.40584305311827,5.06178558918454));
#56280=CARTESIAN_POINT('Ctrl Pts',(0.100899451990349,2.40607289584898,5.06183051897494));
#56281=CARTESIAN_POINT('Ctrl Pts',(0.100542307411169,2.40619040057439,5.06185363165984));
#56282=CARTESIAN_POINT('Ctrl Pts',(0.0996830626629651,2.40647143666381,
5.06190925583489));
#56283=CARTESIAN_POINT('Ctrl Pts',(0.0991807658248759,2.40663435906262,
5.06194178732419));
#56284=CARTESIAN_POINT('Ctrl Pts',(0.0976410772466343,2.40712958546628,
5.06204155240271));
#56285=CARTESIAN_POINT('Ctrl Pts',(0.0966024072354025,2.40745786232287,
5.06210891815628));
#56286=CARTESIAN_POINT('Ctrl Pts',(0.084285899739606,2.41128198362624,5.06290854171715));
#56287=CARTESIAN_POINT('Ctrl Pts',(0.0728271702375305,2.41416035920824,
5.06366094794572));
#56288=CARTESIAN_POINT('Ctrl Pts',(0.0346019510344244,2.42155855938874,
5.0662017146396));
#56289=CARTESIAN_POINT('Ctrl Pts',(0.00742329798941937,2.42332917726726,
5.06806759087787));
#56290=CARTESIAN_POINT('Ctrl Pts',(-0.0300907877523687,2.42103760141242,
5.07057580847388));
#56291=CARTESIAN_POINT('Ctrl Pts',(-0.0404957642956893,2.41989176032202,
5.0712625553953));
#56292=CARTESIAN_POINT('Ctrl Pts',(-0.0523008765267065,2.41800632049263,
5.07201841007402));
#56293=CARTESIAN_POINT('Ctrl Pts',(-0.0537725429164855,2.41776078328165,
5.07211221664668));
#56294=CARTESIAN_POINT('Ctrl Pts',(-0.0556433804115265,2.41743527753573,
5.07223088488691));
#56295=CARTESIAN_POINT('Ctrl Pts',(-0.0560441464761551,2.41736476625156,
5.07225627162892));
#56296=CARTESIAN_POINT('Ctrl Pts',(-0.0566854172699531,2.41725068767852,
5.07229683754336));
#56297=CARTESIAN_POINT('Ctrl Pts',(-0.0569260061898422,2.41720760581012,
5.07231204430483));
#56298=CARTESIAN_POINT('Ctrl Pts',(-0.0573824715228527,2.41712533125735,
5.0723408716858));
#56299=CARTESIAN_POINT('Ctrl Pts',(-0.0575983551238477,2.41708619214727,
5.07235449519227));
#56300=CARTESIAN_POINT('Ctrl Pts',(-0.0580928781320035,2.41699601476829,
5.07238567908276));
#56301=CARTESIAN_POINT('Ctrl Pts',(-0.058371489918554,2.41694482963885,
5.07240323094593));
#56302=CARTESIAN_POINT('Ctrl Pts',(-0.0592302010320829,2.4167859009375,
5.07245727628635));
#56303=CARTESIAN_POINT('Ctrl Pts',(-0.0598100763818755,2.41667693083535,
5.07249370003249));
#56304=CARTESIAN_POINT('Ctrl Pts',(-0.0642341636128275,2.41583297163124,
5.07277106087828));
#56305=CARTESIAN_POINT('Ctrl Pts',(-0.0680652047929457,2.41502956208742,
5.0730081875616));
#56306=CARTESIAN_POINT('Ctrl Pts',(-0.0991596439612118,2.4079149709497,
5.07491485403923));
#56307=CARTESIAN_POINT('Ctrl Pts',(-0.125513030189108,2.39814627749829,
5.07642607198489));
#56308=CARTESIAN_POINT('Ctrl Pts',(-0.165231814284946,2.37721014769211,
5.07896246564542));
#56309=CARTESIAN_POINT('Ctrl Pts',(-0.179542591847503,2.36816293869034,
5.07993725185203));
#56310=CARTESIAN_POINT('Ctrl Pts',(-0.195144269511299,2.3564889039339,5.08111176575143));
#56311=CARTESIAN_POINT('Ctrl Pts',(-0.197193102325694,2.35491709154408,
5.08126835171411));
#56312=CARTESIAN_POINT('Ctrl Pts',(-0.199789545535448,2.35287513325113,
5.08146990713136));
#56313=CARTESIAN_POINT('Ctrl Pts',(-0.200354809388862,2.35242750615471,
5.0815139788756));
#56314=CARTESIAN_POINT('Ctrl Pts',(-0.201260250690224,2.35170553847089,
5.08158488393191));
#56315=CARTESIAN_POINT('Ctrl Pts',(-0.201601382816849,2.35143239458783,
5.0816116692467));
#56316=CARTESIAN_POINT('Ctrl Pts',(-0.202248150215842,2.35091236662254,
5.08166258879869));
#56317=CARTESIAN_POINT('Ctrl Pts',(-0.202553891895389,2.35066561564306,
5.08168671765172));
#56318=CARTESIAN_POINT('Ctrl Pts',(-0.203247320558231,2.35010388207035,
5.08174157481916));
#56319=CARTESIAN_POINT('Ctrl Pts',(-0.203634727298463,2.34978855653204,
5.08177231695273));
#56320=CARTESIAN_POINT('Ctrl Pts',(-0.204779362116287,2.34885246076335,
5.08186342887907));
#56321=CARTESIAN_POINT('Ctrl Pts',(-0.205534490851644,2.34822914295706,
5.08192390191535));
#56322=CARTESIAN_POINT('Ctrl Pts',(-0.210646742006857,2.34396993652484,
5.08233581711139));
#56323=CARTESIAN_POINT('Ctrl Pts',(-0.214909776044909,2.34022314916051,
5.08269178983913));
#56324=CARTESIAN_POINT('Ctrl Pts',(-0.219976533234906,2.33552711785698,
5.08313079215456));
#56325=CARTESIAN_POINT('Ctrl Pts',(-0.220876761198919,2.33468309422648,
5.08320942332677));
#56326=CARTESIAN_POINT('Ctrl Pts',(-0.226198130864565,2.32963621597357,
5.08367800649076));
#56327=CARTESIAN_POINT('Ctrl Pts',(-0.230503834916903,2.32531391566893,
5.08407283026291));
#56328=CARTESIAN_POINT('Ctrl Pts',(-0.251979375367832,2.30249544232156,
5.08612418117315));
#56329=CARTESIAN_POINT('Ctrl Pts',(-0.267055321515111,2.28215159696037,
5.08785533599168));
#56330=CARTESIAN_POINT('Ctrl Pts',(-0.284020248806697,2.25255364193745,
5.09013874298989));
#56331=CARTESIAN_POINT('Ctrl Pts',(-0.288118235529243,2.24466521202856,
5.09072619161299));
#56332=CARTESIAN_POINT('Ctrl Pts',(-0.293519304037409,2.23312570164678,
5.09154620641875));
#56333=CARTESIAN_POINT('Ctrl Pts',(-0.295090686226717,2.22960526404774,
5.09179129964355));
#56334=CARTESIAN_POINT('Ctrl Pts',(-0.296809184386449,2.22556183142715,
5.09206636977017));
#56335=CARTESIAN_POINT('Ctrl Pts',(-0.297018519677702,2.22506584036391,
5.09210000219524));
#56336=CARTESIAN_POINT('Ctrl Pts',(-0.297332086313077,2.22431765977784,
5.09215056814716));
#56337=CARTESIAN_POINT('Ctrl Pts',(-0.297437240494103,2.22406586175295,
5.09216755751857));
#56338=CARTESIAN_POINT('Ctrl Pts',(-0.297625961574288,2.22361233877598,
5.09219810612257));
#56339=CARTESIAN_POINT('Ctrl Pts',(-0.297709643081217,2.22341066290273,
5.09221167233033));
#56340=CARTESIAN_POINT('Ctrl Pts',(-0.297889059914329,2.22297701648203,
5.09224080307109));
#56341=CARTESIAN_POINT('Ctrl Pts',(-0.297984728986997,2.22274501982174,
5.09225636351185));
#56342=CARTESIAN_POINT('Ctrl Pts',(-0.298241726796195,2.22211973111332,
5.09229823815228));
#56343=CARTESIAN_POINT('Ctrl Pts',(-0.298402549229552,2.22172622949794,
5.09232452156681));
#56344=CARTESIAN_POINT('Ctrl Pts',(-0.299139804960049,2.21991206470504,
5.09244538471539));
#56345=CARTESIAN_POINT('Ctrl Pts',(-0.299706886859887,2.21848758737001,
5.09253940710168));
#56346=CARTESIAN_POINT('Ctrl Pts',(-0.311864296941188,2.18730307825963,
5.09457973190748));
#56347=CARTESIAN_POINT('Ctrl Pts',(-0.318979528599732,2.15598244022577,
5.09628545726322));
#56348=CARTESIAN_POINT('Ctrl Pts',(-0.321969437543412,2.11614891405994,
5.09854943707508));
#56349=CARTESIAN_POINT('Ctrl Pts',(-0.322270950202066,2.10815656070147,
5.09900739530887));
#56350=CARTESIAN_POINT('Ctrl Pts',(-0.322279716646284,2.09067528164424,
5.10002592410256));
#56351=CARTESIAN_POINT('Ctrl Pts',(-0.321865625026729,2.08119418185082,
5.10058925107366));
#56352=CARTESIAN_POINT('Ctrl Pts',(-0.320933513765265,2.07060321553701,
5.10123579416297));
#56353=CARTESIAN_POINT('Ctrl Pts',(-0.320826858603185,2.06946120598247,
5.10130573314836));
#56354=CARTESIAN_POINT('Ctrl Pts',(-0.320662991998946,2.06780230437277,
5.10140765999625));
#56355=CARTESIAN_POINT('Ctrl Pts',(-0.320610621314186,2.06728493409842,
5.1014394954748));
#56356=CARTESIAN_POINT('Ctrl Pts',(-0.320516059384775,2.066372794886,5.10149570614405));
#56357=CARTESIAN_POINT('Ctrl Pts',(-0.320474390321553,2.06597797194295,
5.10152006484342));
#56358=CARTESIAN_POINT('Ctrl Pts',(-0.320386805594868,2.06516252798548,
5.10157043149906));
#56359=CARTESIAN_POINT('Ctrl Pts',(-0.320340790950744,2.06474191857204,
5.10159644252975));
#56360=CARTESIAN_POINT('Ctrl Pts',(-0.320221019099625,2.06366670256384,
5.10166301694102));
#56361=CARTESIAN_POINT('Ctrl Pts',(-0.320146083147756,2.06301223160768,
5.10170361741313));
#56362=CARTESIAN_POINT('Ctrl Pts',(-0.319833205707336,2.06035184133243,
5.10186897457095));
#56363=CARTESIAN_POINT('Ctrl Pts',(-0.319578417977619,2.05834798416497,
5.10199426158106));
#56364=CARTESIAN_POINT('Ctrl Pts',(-0.315110225282228,2.02566511415882,
5.1040500691332));
#56365=CARTESIAN_POINT('Ctrl Pts',(-0.306516127007977,1.99575475164704,
5.10613370126422));
#56366=CARTESIAN_POINT('Ctrl Pts',(-0.287853086921499,1.95436104566144,
5.10920349140419));
#56367=CARTESIAN_POINT('Ctrl Pts',(-0.281031677762897,1.9415974197239,5.11017512544206));
#56368=CARTESIAN_POINT('Ctrl Pts',(-0.271216533664863,1.92587535603576,
5.11137033799005));
#56369=CARTESIAN_POINT('Ctrl Pts',(-0.268991779029281,1.92245781789046,
5.11162998218112));
#56370=CARTESIAN_POINT('Ctrl Pts',(-0.26640072138197,1.91863815030557,5.11191917492675));
#56371=CARTESIAN_POINT('Ctrl Pts',(-0.266097685937063,1.91819382181492,
5.11195280004526));
#56372=CARTESIAN_POINT('Ctrl Pts',(-0.265637133960592,1.91752215154401,
5.11200360322074));
#56373=CARTESIAN_POINT('Ctrl Pts',(-0.265480436609093,1.91729425325081,
5.11202083617721));
#56374=CARTESIAN_POINT('Ctrl Pts',(-0.2652072772758,1.91689806776479,5.11205078606386));
#56375=CARTESIAN_POINT('Ctrl Pts',(-0.265090948321882,1.91672968972943,
5.11206351205307));
#56376=CARTESIAN_POINT('Ctrl Pts',(-0.264846753241866,1.91637695335379,
5.11209016605967));
#56377=CARTESIAN_POINT('Ctrl Pts',(-0.264718855019159,1.91619261777585,
5.11210409178066));
#56378=CARTESIAN_POINT('Ctrl Pts',(-0.264411480430327,1.91575059496508,
5.11213747699517));
#56379=CARTESIAN_POINT('Ctrl Pts',(-0.264231819082923,1.91549303529349,
5.11215692381319));
#56380=CARTESIAN_POINT('Ctrl Pts',(-0.263616616120723,1.9146138315163,5.11222328758627));
#56381=CARTESIAN_POINT('Ctrl Pts',(-0.263179250656773,1.91399345761182,
5.11227008066282));
#56382=CARTESIAN_POINT('Ctrl Pts',(-0.262130447270882,1.91251690447786,
5.11238138716638));
#56383=CARTESIAN_POINT('Ctrl Pts',(-0.261516996229678,1.91166215662917,
5.11244576723247));
#56384=CARTESIAN_POINT('Ctrl Pts',(-0.25396362616563,1.90124578291539,5.11322988744973));
#56385=CARTESIAN_POINT('Ctrl Pts',(-0.246506309745506,1.89206859775676,
5.11391622223745));
#56386=CARTESIAN_POINT('Ctrl Pts',(-0.217350367933014,1.85996829302401,
5.11638458808503));
#56387=CARTESIAN_POINT('Ctrl Pts',(-0.192827395105979,1.83985757320203,
5.11808734392856));
#56388=CARTESIAN_POINT('Ctrl Pts',(-0.165100649834053,1.82322650957429,
5.11999929621495));
#56389=CARTESIAN_POINT('Ctrl Pts',(-0.164427243152219,1.8228259188302,5.12004571186467));
#56390=CARTESIAN_POINT('Ctrl Pts',(-0.159018062486628,1.81963479878462,
5.12041840638111));
#56391=CARTESIAN_POINT('Ctrl Pts',(-0.154213293777334,1.81696352759643,
5.12074860954042));
#56392=CARTESIAN_POINT('Ctrl Pts',(-0.148559776674896,1.81400708203306,
5.12113705437957));
#56393=CARTESIAN_POINT('Ctrl Pts',(-0.147775102054241,1.81360084573901,
5.12119096569368));
#56394=CARTESIAN_POINT('Ctrl Pts',(-0.14652381581915,1.81295954990248,5.12127693562017));
#56395=CARTESIAN_POINT('Ctrl Pts',(-0.146058282230693,1.8127223872608,5.12130892019706));
#56396=CARTESIAN_POINT('Ctrl Pts',(-0.145237615255287,1.81230681501058,
5.12136530508642));
#56397=CARTESIAN_POINT('Ctrl Pts',(-0.144882723817743,1.81212792787193,
5.12138968858301));
#56398=CARTESIAN_POINT('Ctrl Pts',(-0.144150179515521,1.8117603781812,5.12144002040104));
#56399=CARTESIAN_POINT('Ctrl Pts',(-0.143772485195432,1.8115718003755,5.12146597163043));
#56400=CARTESIAN_POINT('Ctrl Pts',(-0.142808385927782,1.81109280253147,
5.1215322164389));
#56401=CARTESIAN_POINT('Ctrl Pts',(-0.142221467024086,1.81080342645902,
5.12157254639289));
#56402=CARTESIAN_POINT('Ctrl Pts',(-0.139850669662212,1.80964348477773,
5.12173546560285));
#56403=CARTESIAN_POINT('Ctrl Pts',(-0.138059676498706,1.80878763560113,
5.12185856564488));
#56404=CARTESIAN_POINT('Ctrl Pts',(-0.126350141681476,1.80332438175122,
5.12266368052197));
#56405=CARTESIAN_POINT('Ctrl Pts',(-0.116211501170433,1.79920834159235,
5.1233624795124));
#56406=CARTESIAN_POINT('Ctrl Pts',(-0.0770503066071499,1.7855855831329,
5.12606999354659));
#56407=CARTESIAN_POINT('Ctrl Pts',(-0.046943100351864,1.77970468702387,
5.12818630696107));
#56408=CARTESIAN_POINT('Ctrl Pts',(-0.0153677196784037,1.77808975162365,
5.13026843510386));
#56409=CARTESIAN_POINT('Ctrl Pts',(-0.0142737823858288,1.77803939059718,
5.13034037735279));
#56410=CARTESIAN_POINT('Ctrl Pts',(-0.0116690858419834,1.77793278103843,
5.13051118243553));
#56411=CARTESIAN_POINT('Ctrl Pts',(-0.010158132163823,1.77788158451176,
5.13060987108058));
#56412=CARTESIAN_POINT('Ctrl Pts',(-0.00849108474651263,1.7778368404287,
5.13071828295553));
#56413=CARTESIAN_POINT('Ctrl Pts',(-0.00833531671228995,1.7778327726155,
5.13072840835777));
#56414=CARTESIAN_POINT('Ctrl Pts',(-0.00805012154474173,1.7778255318473,
5.13074693852835));
#56415=CARTESIAN_POINT('Ctrl Pts',(-0.00792069541683257,1.77782232391028,
5.13075534465113));
#56416=CARTESIAN_POINT('Ctrl Pts',(-0.00680945594168689,1.77779545091379,
5.1308274913965));
#56417=CARTESIAN_POINT('Ctrl Pts',(-0.00582752944657534,1.77777619565147,
5.13089105916989));
#56418=CARTESIAN_POINT('Ctrl Pts',(-0.000655327699106262,1.77769842097698,
5.1312248790249));
#56419=CARTESIAN_POINT('Ctrl Pts',(0.00353594717595642,1.77771714514683,
5.1314918759806));
#56420=CARTESIAN_POINT('Ctrl Pts',(0.0082676932618976,1.77783061197874,
5.13178845024824));
#56421=CARTESIAN_POINT('Ctrl Pts',(0.00880945400669028,1.77784497076702,
5.13182233456962));
#56422=CARTESIAN_POINT('Ctrl Pts',(0.00962869562767096,1.77786875202025,
5.13187346248299));
#56423=CARTESIAN_POINT('Ctrl Pts',(0.00990620140697552,1.7778771664728,
5.13189076196259));
#56424=CARTESIAN_POINT('Ctrl Pts',(0.0103885174154802,1.77789241498503,
5.13192079513109));
#56425=CARTESIAN_POINT('Ctrl Pts',(0.0105933320553065,1.77789908579023,
5.13193353800224));
#56426=CARTESIAN_POINT('Ctrl Pts',(0.0110221318756865,1.77791346122156,
5.13196019395179));
#56427=CARTESIAN_POINT('Ctrl Pts',(0.0112461152896326,1.77792120413692,
5.1319741047886));
#56428=CARTESIAN_POINT('Ctrl Pts',(0.0117826324977038,1.77794031142885,
5.13200739551768));
#56429=CARTESIAN_POINT('Ctrl Pts',(0.0120951592698433,1.77795189714061,
5.13202676291682));
#56430=CARTESIAN_POINT('Ctrl Pts',(0.0131585098058498,1.7779928667846,5.13209257627652));
#56431=CARTESIAN_POINT('Ctrl Pts',(0.0139092547403826,1.77802442191818,
5.13213890112612));
#56432=CARTESIAN_POINT('Ctrl Pts',(0.0156975597044053,1.77810585399429,
5.13224892836011));
#56433=CARTESIAN_POINT('Ctrl Pts',(0.0167350097324752,1.77815812247363,
5.13231250142758));
#56434=CARTESIAN_POINT('Ctrl Pts',(0.0292834884766979,1.77885117658798,
5.13307853371981));
#56435=CARTESIAN_POINT('Ctrl Pts',(0.0407537751593051,1.78010426418285,
5.13374915848192));
#56436=CARTESIAN_POINT('Ctrl Pts',(0.0726210816245385,1.78532814360564,
5.13558938850359));
#56437=CARTESIAN_POINT('Ctrl Pts',(0.092736571261693,1.79065846965798,5.13672705814357));
#56438=CARTESIAN_POINT('Ctrl Pts',(0.119255394257325,1.80050714583129,5.13833211620569));
#56439=CARTESIAN_POINT('Ctrl Pts',(0.126216437450541,1.80337360179638,5.13876353147201));
#56440=CARTESIAN_POINT('Ctrl Pts',(0.141770288126491,1.8104251319774,5.13975826371954));
#56441=CARTESIAN_POINT('Ctrl Pts',(0.150289691357093,1.81475379026526,5.14032539026622));
#56442=CARTESIAN_POINT('Ctrl Pts',(0.159603974827992,1.82001952376744,5.14097604735303));
#56443=CARTESIAN_POINT('Ctrl Pts',(0.160601167524356,1.82059033519116,5.141046109356));
#56444=CARTESIAN_POINT('Ctrl Pts',(0.162045520927383,1.82142739621505,5.14114818270856));
#56445=CARTESIAN_POINT('Ctrl Pts',(0.162495130696303,1.82168942002301,5.14118004105223));
#56446=CARTESIAN_POINT('Ctrl Pts',(0.163286687866008,1.82215329610949,5.14123627840878));
#56447=CARTESIAN_POINT('Ctrl Pts',(0.163628901384876,1.82235469403137,5.14126064088062));
#56448=CARTESIAN_POINT('Ctrl Pts',(0.164327457883124,1.82276754536333,5.14131047318749));
#56449=CARTESIAN_POINT('Ctrl Pts',(0.164683766902341,1.82297905452023,5.14133594502139));
#56450=CARTESIAN_POINT('Ctrl Pts',(0.165585756467785,1.82351684119085,5.14140056439152));
#56451=CARTESIAN_POINT('Ctrl Pts',(0.166130879387406,1.82384404631657,5.1414397457614));
#56452=CARTESIAN_POINT('Ctrl Pts',(0.167307801958041,1.82455522942232,5.14152461800237));
#56453=CARTESIAN_POINT('Ctrl Pts',(0.16793925458826,1.824939772071,5.14157032945591));
#56454=CARTESIAN_POINT('Ctrl Pts',(0.169738432072969,1.82604394193958,5.14170107762166));
#56455=CARTESIAN_POINT('Ctrl Pts',(0.170902882731435,1.82676884941304,5.14178630844597));
#56456=CARTESIAN_POINT('Ctrl Pts',(0.181936421360456,1.83373570460249,5.14259977101199));
#56457=CARTESIAN_POINT('Ctrl Pts',(0.191462885565185,1.84050155263272,5.14334754010476));
#56458=CARTESIAN_POINT('Ctrl Pts',(0.218837672325478,1.86227280956496,5.14563850887266));
#56459=CARTESIAN_POINT('Ctrl Pts',(0.235446867315453,1.87871126883502,5.14723100970842));
#56460=CARTESIAN_POINT('Ctrl Pts',(0.258964221731378,1.90765990091767,5.14973802926356));
#56461=CARTESIAN_POINT('Ctrl Pts',(0.267075657761865,1.91909151874405,5.15066512796842));
#56462=CARTESIAN_POINT('Ctrl Pts',(0.274880006191671,1.93176524669219,5.15160086912769));
#56463=CARTESIAN_POINT('Ctrl Pts',(0.275338367135858,1.93251646752497,5.15165600397935));
#56464=CARTESIAN_POINT('Ctrl Pts',(0.275953856730147,1.93353456673698,5.1517302707603));
#56465=CARTESIAN_POINT('Ctrl Pts',(0.276113680676089,1.93379979885345,5.15174957692328));
#56466=CARTESIAN_POINT('Ctrl Pts',(0.276383062739164,1.93424830665128,5.15178215290319));
#56467=CARTESIAN_POINT('Ctrl Pts',(0.276492821015366,1.93443146088517,5.15179543584986));
#56468=CARTESIAN_POINT('Ctrl Pts',(0.27670373915598,1.93478421576785,5.15182098031268));
#56469=CARTESIAN_POINT('Ctrl Pts',(0.276804924396527,1.93495379903676,5.15183324343165));
#56470=CARTESIAN_POINT('Ctrl Pts',(0.277045192114745,1.93535732259782,5.15186238299627));
#56471=CARTESIAN_POINT('Ctrl Pts',(0.277184134030369,1.93559134591149,5.15187925014069));
#56472=CARTESIAN_POINT('Ctrl Pts',(0.277595271819646,1.93628583809265,5.15192921045948));
#56473=CARTESIAN_POINT('Ctrl Pts',(0.277866619623585,1.93674681180957,5.1519622483578));
#56474=CARTESIAN_POINT('Ctrl Pts',(0.280031522978218,1.94044564865951,5.15222637213945));
#56475=CARTESIAN_POINT('Ctrl Pts',(0.281869665871285,1.94371583787578,5.15245393640567));
#56476=CARTESIAN_POINT('Ctrl Pts',(0.288300240432539,1.95563900236441,5.15326510037742));
#56477=CARTESIAN_POINT('Ctrl Pts',(0.292555032621645,1.9644687736137,5.15383121011053));
#56478=CARTESIAN_POINT('Ctrl Pts',(0.308502694031347,2.00182954216195,5.15614063547757));
#56479=CARTESIAN_POINT('Ctrl Pts',(0.316473918900532,2.03176751124718,5.15780730371048));
#56480=CARTESIAN_POINT('Ctrl Pts',(0.32083882184001,2.06890692824254,5.16001497058225));
#56481=CARTESIAN_POINT('Ctrl Pts',(0.321405891622924,2.07545265401265,5.1604083568191));
#56482=CARTESIAN_POINT('Ctrl Pts',(0.321830377040606,2.08304541903164,5.1608711804083));
#56483=CARTESIAN_POINT('Ctrl Pts',(0.321883228015103,2.08408029883549,5.16093440096425));
#56484=CARTESIAN_POINT('Ctrl Pts',(0.321954378170445,2.08561916828983,5.16102862197144));
#56485=CARTESIAN_POINT('Ctrl Pts',(0.321976487207062,2.08612298212779,5.16105950293105));
#56486=CARTESIAN_POINT('Ctrl Pts',(0.322013740584781,2.08701996492306,5.1611145437547));
#56487=CARTESIAN_POINT('Ctrl Pts',(0.322029347648736,2.08741311449356,5.16113868906402));
#56488=CARTESIAN_POINT('Ctrl Pts',(0.322058106416754,2.08817265327619,5.16118537673314));
#56489=CARTESIAN_POINT('Ctrl Pts',(0.322071352961083,2.08853903846443,5.16120791608106));
#56490=CARTESIAN_POINT('Ctrl Pts',(0.322105694241859,2.08953599376847,5.16126929693301));
#56491=CARTESIAN_POINT('Ctrl Pts',(0.322125562422325,2.09016660208763,5.16130817682191));
#56492=CARTESIAN_POINT('Ctrl Pts',(0.322195463509988,2.09261350260604,5.16145925332203));
#56493=CARTESIAN_POINT('Ctrl Pts',(0.322231986721765,2.09443011972202,5.1615718723004));
#56494=CARTESIAN_POINT('Ctrl Pts',(0.322418580025097,2.11045169821216,5.16256927685574));
#56495=CARTESIAN_POINT('Ctrl Pts',(0.321644624980028,2.12464984545561,5.16348311104624));
#56496=CARTESIAN_POINT('Ctrl Pts',(0.317895137290635,2.15560800605637,5.16554116404712));
#56497=CARTESIAN_POINT('Ctrl Pts',(0.314524023080926,2.1722781253663,5.16669284883827));
#56498=CARTESIAN_POINT('Ctrl Pts',(0.305867290901938,2.20255160394687,5.16882154949197));
#56499=CARTESIAN_POINT('Ctrl Pts',(0.300941197331393,2.21621576799354,5.16979665749187));
#56500=CARTESIAN_POINT('Ctrl Pts',(0.293498400759003,2.23317642903458,5.17099055628135));
#56501=CARTESIAN_POINT('Ctrl Pts',(0.291817628276304,2.23682013008512,5.17124597609863));
#56502=CARTESIAN_POINT('Ctrl Pts',(0.289810189033462,2.24096660295828,5.17153461194444));
#56503=CARTESIAN_POINT('Ctrl Pts',(0.289549740657808,2.24150080040618,5.17157175826703));
#56504=CARTESIAN_POINT('Ctrl Pts',(0.289163938571284,2.24228658143442,5.17162633776634));
#56505=CARTESIAN_POINT('Ctrl Pts',(0.289039732947551,2.2425387224771,5.1716438419173));
#56506=CARTESIAN_POINT('Ctrl Pts',(0.288817844182879,2.24298768053485,5.17167499250948));
#56507=CARTESIAN_POINT('Ctrl Pts',(0.288720289587857,2.24318456021731,5.17168864699748));
#56508=CARTESIAN_POINT('Ctrl Pts',(0.288514395659611,2.24359901879592,5.17171737908938));
#56509=CARTESIAN_POINT('Ctrl Pts',(0.28840601179599,2.24381657436767,5.17173245379939));
#56510=CARTESIAN_POINT('Ctrl Pts',(0.288118224759445,2.24439260672437,5.17177234929841));
#56511=CARTESIAN_POINT('Ctrl Pts',(0.287938397974384,2.24475087319692,5.17179714348035));
#56512=CARTESIAN_POINT('Ctrl Pts',(0.287113923596844,2.24638584645943,5.17191021057851));
#56513=CARTESIAN_POINT('Ctrl Pts',(0.286461437160134,2.24765861426111,5.17199799820846));
#56514=CARTESIAN_POINT('Ctrl Pts',(0.281308353988924,2.25754771049502,5.17267860771744));
#56515=CARTESIAN_POINT('Ctrl Pts',(0.276427986163082,2.26596168141894,5.17324894535946));
#56516=CARTESIAN_POINT('Ctrl Pts',(0.256734256922605,2.29662861870966,5.17534279486634));
#56517=CARTESIAN_POINT('Ctrl Pts',(0.239553610959685,2.31723146585915,5.17678939251239));
#56518=CARTESIAN_POINT('Ctrl Pts',(0.219924291886246,2.33557270801519,5.17833301241377));
#56519=CARTESIAN_POINT('Ctrl Pts',(0.219822727252329,2.33566748504275,5.17834099644943));
#56520=CARTESIAN_POINT('Ctrl Pts',(0.218761212821919,2.33665677477419,5.17842441294535));
#56521=CARTESIAN_POINT('Ctrl Pts',(0.21779587763854,2.33754547545778,5.17850001910827));
#56522=CARTESIAN_POINT('Ctrl Pts',(0.20825912408366,2.34621813914642,5.17924465101702));
#56523=CARTESIAN_POINT('Ctrl Pts',(0.199280421179306,2.35353994164118,5.17992804960406));
#56524=CARTESIAN_POINT('Ctrl Pts',(0.188967432666075,2.36106301668377,5.18070401411057));
#56525=CARTESIAN_POINT('Ctrl Pts',(0.188003012540059,2.36175839338033,5.18077649114619));
#56526=CARTESIAN_POINT('Ctrl Pts',(0.18663717401669,2.36273176297626,5.18087902101642));
#56527=CARTESIAN_POINT('Ctrl Pts',(0.186238929871124,2.36301421063864,5.18090890255137));
#56528=CARTESIAN_POINT('Ctrl Pts',(0.185541300035437,2.36350661342546,5.18096122490166));
#56529=CARTESIAN_POINT('Ctrl Pts',(0.185242195240774,2.36371696653493,5.18098365042736));
#56530=CARTESIAN_POINT('Ctrl Pts',(0.184613714848363,2.36415736469812,5.18103075590447));
#56531=CARTESIAN_POINT('Ctrl Pts',(0.184284265967452,2.36438730368329,5.18105543985585));
#56532=CARTESIAN_POINT('Ctrl Pts',(0.183506759316075,2.36492780547902,5.18111367452699));
#56533=CARTESIAN_POINT('Ctrl Pts',(0.183058342826739,2.3652378478768,5.18114724498544));
#56534=CARTESIAN_POINT('Ctrl Pts',(0.181568867564697,2.36626211875618,5.18125870369161));
#56535=CARTESIAN_POINT('Ctrl Pts',(0.180524408533545,2.36697136064405,5.18133678068782));
#56536=CARTESIAN_POINT('Ctrl Pts',(0.178050651552201,2.36863001571106,5.18152152569188));
#56537=CARTESIAN_POINT('Ctrl Pts',(0.176617896146414,2.36957417984018,5.18162838867972));
#56538=CARTESIAN_POINT('Ctrl Pts',(0.171574758600473,2.37284006835595,5.18200409272662));
#56539=CARTESIAN_POINT('Ctrl Pts',(0.167925718551589,2.37510098307525,5.18227516160093));
#56540=CARTESIAN_POINT('Ctrl Pts',(0.158555985024941,2.38065050428849,5.18296949346351));
#56541=CARTESIAN_POINT('Ctrl Pts',(0.152777652720028,2.38383742727995,5.1833961552431));
#56542=CARTESIAN_POINT('Ctrl Pts',(0.135213363206224,2.39283288197974,5.184688131128));
#56543=CARTESIAN_POINT('Ctrl Pts',(0.123166561089593,2.39810014522031,5.18556838158964));
#56544=CARTESIAN_POINT('Ctrl Pts',(0.100782104942607,2.40629840500096,5.18717882015782));
#56545=CARTESIAN_POINT('Ctrl Pts',(0.0905540495958589,2.40947651557396,
5.18790546814082));
#56546=CARTESIAN_POINT('Ctrl Pts',(0.0668971765186751,2.41555381744271,
5.18954572938213));
#56547=CARTESIAN_POINT('Ctrl Pts',(0.0534012488364664,2.41811609645066,
5.19045283985469));
#56548=CARTESIAN_POINT('Ctrl Pts',(0.0390165034065126,2.41990542714555,
5.19136308624037));
#56549=CARTESIAN_POINT('Ctrl Pts',(0.0382511872849979,2.41999783836065,
5.19141134528465));
#56550=CARTESIAN_POINT('Ctrl Pts',(0.0371944704604102,2.42012159076548,
5.19147773921923));
#56551=CARTESIAN_POINT('Ctrl Pts',(0.0369033554559773,2.42015528086354,
5.19149600495293));
#56552=CARTESIAN_POINT('Ctrl Pts',(0.0364045807530623,2.42021231361684,
5.1915272565701));
#56553=CARTESIAN_POINT('Ctrl Pts',(0.0361969442689838,2.42023585139364,
5.19154025348698));
#56554=CARTESIAN_POINT('Ctrl Pts',(0.0357693584790864,2.42028390155794,
5.19156699123645));
#56555=CARTESIAN_POINT('Ctrl Pts',(0.03554940732181,2.42030838927893,5.19158073056709));
#56556=CARTESIAN_POINT('Ctrl Pts',(0.0350345376077072,2.42036517416729,
5.19161285815161));
#56557=CARTESIAN_POINT('Ctrl Pts',(0.0347395985056996,2.42039729078439,
5.19163123614439));
#56558=CARTESIAN_POINT('Ctrl Pts',(0.0337879300774918,2.42049959067515,
5.1916904528953));
#56559=CARTESIAN_POINT('Ctrl Pts',(0.0331310238048297,2.42056816298829,
5.19173120115618));
#56560=CARTESIAN_POINT('Ctrl Pts',(0.0168108740217263,2.4222210688014,5.1927404946942));
#56561=CARTESIAN_POINT('Ctrl Pts',(0.00105012008026275,2.42265782422649,
5.19364574104255));
#56562=CARTESIAN_POINT('Ctrl Pts',(-0.0334936255536876,2.42108251990121,
5.19559734031623));
#56563=CARTESIAN_POINT('Ctrl Pts',(-0.0521941154928808,2.41857744682543,
5.19663424528499));
#56564=CARTESIAN_POINT('Ctrl Pts',(-0.0765884891096376,2.41310291992299,
5.19805736687232));
#56565=CARTESIAN_POINT('Ctrl Pts',(-0.0825677460721462,2.41157951951921,
5.19841174866557));
#56566=CARTESIAN_POINT('Ctrl Pts',(-0.0979066214174795,2.40719893041556,
5.19934000960093));
#56567=CARTESIAN_POINT('Ctrl Pts',(-0.107185806087738,2.40408561813031,
5.19992047626176));
#56568=CARTESIAN_POINT('Ctrl Pts',(-0.117278766227451,2.40017986144128,
5.20057855681905));
#56569=CARTESIAN_POINT('Ctrl Pts',(-0.118247289734139,2.39979966086297,
5.20064198161484));
#56570=CARTESIAN_POINT('Ctrl Pts',(-0.119693295871762,2.39922392409437,
5.20073709339893));
#56571=CARTESIAN_POINT('Ctrl Pts',(-0.120172184200983,2.39903191797291,
5.20076866144768));
#56572=CARTESIAN_POINT('Ctrl Pts',(-0.120996245324255,2.39869921858108,
5.20082310272895));
#56573=CARTESIAN_POINT('Ctrl Pts',(-0.121341639935803,2.3985590745218,5.20084595737828));
#56574=CARTESIAN_POINT('Ctrl Pts',(-0.122054071500556,2.39826856452117,
5.2008931740433));
#56575=CARTESIAN_POINT('Ctrl Pts',(-0.122421075419096,2.39811811961439,
5.20091753870167));
#56576=CARTESIAN_POINT('Ctrl Pts',(-0.123147036590687,2.39781896173692,
5.2009658160954));
#56577=CARTESIAN_POINT('Ctrl Pts',(-0.123506004520981,2.39767027637351,
5.20098972785973));
#56578=CARTESIAN_POINT('Ctrl Pts',(-0.124690891944273,2.39717698092486,
5.20106878874426));
#56579=CARTESIAN_POINT('Ctrl Pts',(-0.125515639377708,2.39682958203525,
5.20112403252878));
#56580=CARTESIAN_POINT('Ctrl Pts',(-0.13112391867334,2.39443971783413,5.20150115728883));
#56581=CARTESIAN_POINT('Ctrl Pts',(-0.135858607999843,2.39228524256525,
5.20182684583936));
#56582=CARTESIAN_POINT('Ctrl Pts',(-0.1439124217978,2.38838246093822,5.2023939968143));
#56583=CARTESIAN_POINT('Ctrl Pts',(-0.147257067590164,2.38668900068895,
5.2026335381937));
#56584=CARTESIAN_POINT('Ctrl Pts',(-0.161135482297279,2.3793551467279,5.20364452524249));
#56585=CARTESIAN_POINT('Ctrl Pts',(-0.171380001700075,2.37319001940358,
5.20443296575815));
#56586=CARTESIAN_POINT('Ctrl Pts',(-0.205159586133253,2.35021261077742,
5.20716906570496));
#56587=CARTESIAN_POINT('Ctrl Pts',(-0.22676542242463,2.33081238797812,5.20917293808333));
#56588=CARTESIAN_POINT('Ctrl Pts',(-0.246483878120763,2.30762756286976,
5.21109840967081));
#56589=CARTESIAN_POINT('Ctrl Pts',(-0.24746484543768,2.30645739882126,5.21119445853409));
#56590=CARTESIAN_POINT('Ctrl Pts',(-0.248707834553097,2.30495308926973,
5.2113164473278));
#56591=CARTESIAN_POINT('Ctrl Pts',(-0.248977542574868,2.30462536271829,
5.21134293423166));
#56592=CARTESIAN_POINT('Ctrl Pts',(-0.249405587347312,2.30410313942243,
5.211384997083));
#56593=CARTESIAN_POINT('Ctrl Pts',(-0.249564344672945,2.30390899046178,
5.21140060355169));
#56594=CARTESIAN_POINT('Ctrl Pts',(-0.249860907797609,2.30354544962497,
5.21142976740907));
#56595=CARTESIAN_POINT('Ctrl Pts',(-0.249998767015926,2.30337610429794,
5.21144332864786));
#56596=CARTESIAN_POINT('Ctrl Pts',(-0.25030864763161,2.30299465786778,5.21147382135945));
#56597=CARTESIAN_POINT('Ctrl Pts',(-0.250480571219786,2.30278247864338,
5.21149074567707));
#56598=CARTESIAN_POINT('Ctrl Pts',(-0.250991273783402,2.30215055543887,
5.21154104079314));
#56599=CARTESIAN_POINT('Ctrl Pts',(-0.251329271014511,2.30173017652534,
5.2115743551942));
#56600=CARTESIAN_POINT('Ctrl Pts',(-0.254094267568999,2.29827351836931,
5.21184713112828));
#56601=CARTESIAN_POINT('Ctrl Pts',(-0.256467338468236,2.29519424298539,
5.21208280714787));
#56602=CARTESIAN_POINT('Ctrl Pts',(-0.264064411276896,2.28495851690477,
5.21284531377718));
#56603=CARTESIAN_POINT('Ctrl Pts',(-0.269049428639147,2.27762909967955,
5.21335870854257));
#56604=CARTESIAN_POINT('Ctrl Pts',(-0.284019051411226,2.25354027504166,
5.21497575069274));
#56605=CARTESIAN_POINT('Ctrl Pts',(-0.29278742907882,2.23607722545153,5.21604669004016));
#56606=CARTESIAN_POINT('Ctrl Pts',(-0.300792637237424,2.2157177855621,5.2172834079808));
#56607=CARTESIAN_POINT('Ctrl Pts',(-0.301637256681434,2.21349793680584,
5.21741806057806));
#56608=CARTESIAN_POINT('Ctrl Pts',(-0.304631272000374,2.20535944513291,
5.2179114739331));
#56609=CARTESIAN_POINT('Ctrl Pts',(-0.30663154489143,2.19938769776535,5.21827306740836));
#56610=CARTESIAN_POINT('Ctrl Pts',(-0.31129230346613,2.18398907768822,5.21920922880558));
#56611=CARTESIAN_POINT('Ctrl Pts',(-0.313700180163125,2.17449316125589,
5.21979020794796));
#56612=CARTESIAN_POINT('Ctrl Pts',(-0.315881528741162,2.16388363264929,
5.22044884215179));
#56613=CARTESIAN_POINT('Ctrl Pts',(-0.316086178221075,2.16286323741401,
5.22051228143699));
#56614=CARTESIAN_POINT('Ctrl Pts',(-0.316384897315462,2.16133545988705,
5.22060741141829));
#56615=CARTESIAN_POINT('Ctrl Pts',(-0.316482697994233,2.16082880694437,
5.22063898311141));
#56616=CARTESIAN_POINT('Ctrl Pts',(-0.316649052538471,2.15995575119867,
5.22069342900424));
#56617=CARTESIAN_POINT('Ctrl Pts',(-0.316718188492703,2.15958945922992,
5.22071628461343));
#56618=CARTESIAN_POINT('Ctrl Pts',(-0.316859576463072,2.1588331687754,5.22076350169901));
#56619=CARTESIAN_POINT('Ctrl Pts',(-0.316931744286872,2.15844315533578,
5.22078786581536));
#56620=CARTESIAN_POINT('Ctrl Pts',(-0.317073178982807,2.15767083966702,
5.2208361416299));
#56621=CARTESIAN_POINT('Ctrl Pts',(-0.317142474875327,2.15728854340972,
5.22086005235616));
#56622=CARTESIAN_POINT('Ctrl Pts',(-0.317301096401533,2.15640434146702,
5.22091538800589));
#56623=CARTESIAN_POINT('Ctrl Pts',(-0.31738992259949,2.15590234826415,5.22094682877375));
#56624=CARTESIAN_POINT('Ctrl Pts',(-0.317616246264796,2.15460537188408,
5.22102812563903));
#56625=CARTESIAN_POINT('Ctrl Pts',(-0.31775194961828,2.15381008292821,5.22107803865954));
#56626=CARTESIAN_POINT('Ctrl Pts',(-0.320822267103388,2.13539982626745,
5.22223496737217));
#56627=CARTESIAN_POINT('Ctrl Pts',(-0.322290159470362,2.11757536368981,
5.22338921839787));
#56628=CARTESIAN_POINT('Ctrl Pts',(-0.322274881976907,2.09972418888649,
5.22457701413596));
#56629=CARTESIAN_POINT('',(-0.322324149694691,2.09995053291872,5.34972264852953));
#56630=CARTESIAN_POINT('Ctrl Pts',(-0.322021731191934,2.09973199008727,
5.22472278440197));
#56631=CARTESIAN_POINT('Ctrl Pts',(-0.322284766309565,2.06580495458856,
5.22681356126889));
#56632=CARTESIAN_POINT('Ctrl Pts',(-0.301715959323295,1.92471043066922,
5.23552778597674));
#56633=CARTESIAN_POINT('Ctrl Pts',(-0.0967559193787474,1.73141707993042,
5.25086545852553));
#56634=CARTESIAN_POINT('Ctrl Pts',(0.257535391016418,1.81912529612678,5.27073580204831));
#56635=CARTESIAN_POINT('Ctrl Pts',(0.375573040431588,2.16449781548873,5.29060614557111));
#56636=CARTESIAN_POINT('Ctrl Pts',(0.149073554903257,2.45070236972446,5.31047648909389));
#56637=CARTESIAN_POINT('Ctrl Pts',(-0.211166715081224,2.41547992794995,
5.33018196904799));
#56638=CARTESIAN_POINT('Ctrl Pts',(-0.322574663534915,2.20410493244714,
5.34326400116115));
#56639=CARTESIAN_POINT('Ctrl Pts',(-0.322798140628015,2.09995147753102,
5.34972258543339));
#56640=CARTESIAN_POINT('',(-0.322274866580731,2.10029324967485,5.47472265506957));
#56641=CARTESIAN_POINT('Ctrl Pts',(-0.322274996188514,2.09995043496114,
5.34972265507269));
#56642=CARTESIAN_POINT('Ctrl Pts',(-0.322274588015624,2.0972964691886,5.34988749542828));
#56643=CARTESIAN_POINT('Ctrl Pts',(-0.322241396999529,2.09464278843267,
5.35005233578388));
#56644=CARTESIAN_POINT('Ctrl Pts',(-0.32217544030333,2.091989925696,5.35021717613947));
#56645=CARTESIAN_POINT('Ctrl Pts',(-0.321736399743732,2.07433115247729,
5.351314435495));
#56646=CARTESIAN_POINT('Ctrl Pts',(-0.319839819770441,2.0566532640631,5.35241169485053));
#56647=CARTESIAN_POINT('Ctrl Pts',(-0.316490882531739,2.03921598154711,
5.35350895420606));
#56648=CARTESIAN_POINT('Ctrl Pts',(-0.313148351723602,2.02181205610285,
5.35460411453274));
#56649=CARTESIAN_POINT('Ctrl Pts',(-0.308359059551374,2.00464858611462,
5.35569927485942));
#56650=CARTESIAN_POINT('Ctrl Pts',(-0.302179881901054,1.98797993662176,
5.3567944351861));
#56651=CARTESIAN_POINT('Ctrl Pts',(-0.295929630339874,1.97111956159919,
5.35790219222578));
#56652=CARTESIAN_POINT('Ctrl Pts',(-0.288257459219722,1.95476626028155,
5.35900994926546));
#56653=CARTESIAN_POINT('Ctrl Pts',(-0.27927412115275,1.93916735132642,5.36011770630514));
#56654=CARTESIAN_POINT('Ctrl Pts',(-0.270397237075894,1.92375329193248,
5.36121233624707));
#56655=CARTESIAN_POINT('Ctrl Pts',(-0.260240559951294,1.90907648271744,
5.362306966189));
#56656=CARTESIAN_POINT('Ctrl Pts',(-0.248956461332729,1.89534942954957,
5.36340159613092));
#56657=CARTESIAN_POINT('Ctrl Pts',(-0.237469379779092,1.88137544859101,
5.36451591671948));
#56658=CARTESIAN_POINT('Ctrl Pts',(-0.224814399824077,1.8683864042059,5.36563023730803));
#56659=CARTESIAN_POINT('Ctrl Pts',(-0.211192980042452,1.85656889926349,
5.36674455789659));
#56660=CARTESIAN_POINT('Ctrl Pts',(-0.197571560260828,1.84475139432108,
5.36785887848515));
#56661=CARTESIAN_POINT('Ctrl Pts',(-0.182984409865951,1.83410587602989,
5.3689731990737));
#56662=CARTESIAN_POINT('Ctrl Pts',(-0.167664373286722,1.82477312348651,
5.37008751966226));
#56663=CARTESIAN_POINT('Ctrl Pts',(-0.152578900007102,1.8155832636327,5.37118477901779));
#56664=CARTESIAN_POINT('Ctrl Pts',(-0.136688361908179,1.80760858161357,
5.37228203837332));
#56665=CARTESIAN_POINT('Ctrl Pts',(-0.120213942326157,1.80098531190692,
5.37337929772885));
#56666=CARTESIAN_POINT('Ctrl Pts',(-0.103771037883913,1.7943747123444,5.37447445805553));
#56667=CARTESIAN_POINT('Ctrl Pts',(-0.0867471546266051,1.78911073852328,
5.37556961838221));
#56668=CARTESIAN_POINT('Ctrl Pts',(-0.0693869551783361,1.78528326057218,
5.37666477870889));
#56669=CARTESIAN_POINT('Ctrl Pts',(-0.0518270758797871,1.78141175834436,
5.37777253574857));
#56670=CARTESIAN_POINT('Ctrl Pts',(-0.0339238424814607,1.77901031969905,
5.37888029278825));
#56671=CARTESIAN_POINT('Ctrl Pts',(-0.0159451573288649,1.77811969991508,
5.37998804982793));
#56672=CARTESIAN_POINT('Ctrl Pts',(0.0018204775347214,1.77723963411773,
5.38108267976986));
#56673=CARTESIAN_POINT('Ctrl Pts',(0.0196589943490197,1.77783472807192,
5.38217730971178));
#56674=CARTESIAN_POINT('Ctrl Pts',(0.0373092328999541,1.77989189831337,
5.38327193965371));
#56675=CARTESIAN_POINT('Ctrl Pts',(0.0552769710888044,1.7819860737661,5.38438626024227));
#56676=CARTESIAN_POINT('Ctrl Pts',(0.0730487614792567,1.78559540306911,
5.38550058083083));
#56677=CARTESIAN_POINT('Ctrl Pts',(0.0903586518712053,1.79065150775053,
5.38661490141938));
#56678=CARTESIAN_POINT('Ctrl Pts',(0.107668542263155,1.79570761243196,5.38772922200794));
#56679=CARTESIAN_POINT('Ctrl Pts',(0.12451577272566,1.80221013825458,5.38884354259649));
#56680=CARTESIAN_POINT('Ctrl Pts',(0.140655930777141,1.81003951172234,5.38995786318505));
#56681=CARTESIAN_POINT('Ctrl Pts',(0.15654896874447,1.81774901056286,5.39105512254058));
#56682=CARTESIAN_POINT('Ctrl Pts',(0.171856059564678,1.82679322003641,5.39215238189611));
#56683=CARTESIAN_POINT('Ctrl Pts',(0.186342924313215,1.83705991141821,5.39324964125164));
#56684=CARTESIAN_POINT('Ctrl Pts',(0.200802076063112,1.84730696288418,5.39434480157832));
#56685=CARTESIAN_POINT('Ctrl Pts',(0.214443455109349,1.85877146458573,5.395439961905));
#56686=CARTESIAN_POINT('Ctrl Pts',(0.227059056739523,1.87129634813244,5.39653512223168));
#56687=CARTESIAN_POINT('Ctrl Pts',(0.239819765080723,1.88396529493596,5.39764287927136));
#56688=CARTESIAN_POINT('Ctrl Pts',(0.2515302814194,1.89771871199369,5.39875063631104));
#56689=CARTESIAN_POINT('Ctrl Pts',(0.262011317607084,1.91235340378573,5.39985839335072));
#56690=CARTESIAN_POINT('Ctrl Pts',(0.272368151842847,1.9268146721439,5.40095302329265));
#56691=CARTESIAN_POINT('Ctrl Pts',(0.281524097664492,1.94213575157908,5.40204765323458));
#56692=CARTESIAN_POINT('Ctrl Pts',(0.289348785140309,1.95808997159176,5.4031422831765));
#56693=CARTESIAN_POINT('Ctrl Pts',(0.297314226262783,1.97433118257415,5.40425660376506));
#56694=CARTESIAN_POINT('Ctrl Pts',(0.30389962881623,1.99122781729556,5.40537092435362));
#56695=CARTESIAN_POINT('Ctrl Pts',(0.309018521912682,2.00851924388211,5.40648524494217));
#56696=CARTESIAN_POINT('Ctrl Pts',(0.314137415009134,2.02581067046866,5.40759956553073));
#56697=CARTESIAN_POINT('Ctrl Pts',(0.317789685133248,2.04349605820179,5.40871388611929));
#56698=CARTESIAN_POINT('Ctrl Pts',(0.319943566928859,2.06130517339696,5.40982820670784));
#56699=CARTESIAN_POINT('Ctrl Pts',(0.322064470890616,2.07884161529912,5.41092546606337));
#56700=CARTESIAN_POINT('Ctrl Pts',(0.322745942476812,2.09660788533131,5.4120227254189));
#56701=CARTESIAN_POINT('Ctrl Pts',(0.321955526193629,2.11434624614258,5.41311998477443));
#56702=CARTESIAN_POINT('Ctrl Pts',(0.32116662195641,2.1320506739271,5.41421514510111));
#56703=CARTESIAN_POINT('Ctrl Pts',(0.318911388622714,2.14972653159111,5.41531030542779));
#56704=CARTESIAN_POINT('Ctrl Pts',(0.315209295398185,2.16711390109046,5.41640546575447));
#56705=CARTESIAN_POINT('Ctrl Pts',(0.311464620092556,2.18470126295445,5.41751322279415));
#56706=CARTESIAN_POINT('Ctrl Pts',(0.306239614873689,2.20199264792342,5.41862097983383));
#56707=CARTESIAN_POINT('Ctrl Pts',(0.299608078258493,2.21872731390566,5.41972873687351));
#56708=CARTESIAN_POINT('Ctrl Pts',(0.293055126410787,2.23526367142464,5.42082336681544));
#56709=CARTESIAN_POINT('Ctrl Pts',(0.285129167417892,2.25125573173565,5.42191799675736));
#56710=CARTESIAN_POINT('Ctrl Pts',(0.275950218294543,2.26647117662885,5.42301262669929));
#56711=CARTESIAN_POINT('Ctrl Pts',(0.266606154517656,2.28196032310577,5.42412694728785));
#56712=CARTESIAN_POINT('Ctrl Pts',(0.255963958912909,2.29664390115781,5.4252412678764));
#56713=CARTESIAN_POINT('Ctrl Pts',(0.244195967172233,2.31030811977149,5.42635558846496));
#56714=CARTESIAN_POINT('Ctrl Pts',(0.232427975431557,2.32397233838516,5.42746990905352));
#56715=CARTESIAN_POINT('Ctrl Pts',(0.219534824590082,2.33661665243179,5.42858422964207));
#56716=CARTESIAN_POINT('Ctrl Pts',(0.205726536806876,2.34806807065491,5.42969855023063));
#56717=CARTESIAN_POINT('Ctrl Pts',(0.192129666113152,2.35934415754447,5.43079580958616));
#56718=CARTESIAN_POINT('Ctrl Pts',(0.177560361058981,2.36953435404003,5.43189306894169));
#56719=CARTESIAN_POINT('Ctrl Pts',(0.162217763078438,2.37847185309619,5.43299032829722));
#56720=CARTESIAN_POINT('Ctrl Pts',(0.14690451509214,2.38739225494716,5.4340854886239));
#56721=CARTESIAN_POINT('Ctrl Pts',(0.130821538939885,2.39506427551764,5.43518064895058));
#56722=CARTESIAN_POINT('Ctrl Pts',(0.114197917399677,2.40136358653058,5.43627580927726));
#56723=CARTESIAN_POINT('Ctrl Pts',(0.0973830882486234,2.40773535324795,
5.43738356631694));
#56724=CARTESIAN_POINT('Ctrl Pts',(0.0800157924402915,2.41270221442863,
5.43849132335662));
#56725=CARTESIAN_POINT('Ctrl Pts',(0.0623552150644683,2.41618507678141,
5.4395990803963));
#56726=CARTESIAN_POINT('Ctrl Pts',(0.0449039183497231,2.41962666665933,
5.44069371033823));
#56727=CARTESIAN_POINT('Ctrl Pts',(0.027167042896384,2.42161916963324,5.44178834028015));
#56728=CARTESIAN_POINT('Ctrl Pts',(0.00940489339345394,2.42213774011323,
5.44288297022208));
#56729=CARTESIAN_POINT('Ctrl Pts',(-0.00867676884691561,2.42266563884899,
5.44399729081064));
#56730=CARTESIAN_POINT('Ctrl Pts',(-0.026783796946607,2.42166597635755,
5.4451116113992));
#56731=CARTESIAN_POINT('Ctrl Pts',(-0.0446431431697494,2.41916792663569,
5.44622593198775));
#56732=CARTESIAN_POINT('Ctrl Pts',(-0.0625024893928918,2.41666987691383,
5.44734025257631));
#56733=CARTESIAN_POINT('Ctrl Pts',(-0.0801133505468911,2.41267368050409,
5.44845457316486));
#56734=CARTESIAN_POINT('Ctrl Pts',(-0.0972165836964554,2.40726228450526,
5.44956889375342));
#56735=CARTESIAN_POINT('Ctrl Pts',(-0.114057951230964,2.40193374176166,
5.45066615310895));
#56736=CARTESIAN_POINT('Ctrl Pts',(-0.13051267897008,2.39519974670589,5.45176341246448));
#56737=CARTESIAN_POINT('Ctrl Pts',(-0.146332713706938,2.38713744535355,
5.45286067182001));
#56738=CARTESIAN_POINT('Ctrl Pts',(-0.162122485125355,2.37909056697576,
5.45395583214669));
#56739=CARTESIAN_POINT('Ctrl Pts',(-0.177279262975971,2.36972071603058,
5.45505099247337));
#56740=CARTESIAN_POINT('Ctrl Pts',(-0.191574503170435,2.3591532082765,5.45614615280005));
#56741=CARTESIAN_POINT('Ctrl Pts',(-0.206034169553102,2.34846415132176,
5.45725390983973));
#56742=CARTESIAN_POINT('Ctrl Pts',(-0.219611626390578,2.33655006975797,
5.45836166687941));
#56743=CARTESIAN_POINT('Ctrl Pts',(-0.232100069055215,2.32358607642151,
5.45946942391909));
#56744=CARTESIAN_POINT('Ctrl Pts',(-0.244440521680733,2.31077570847554,
5.46056405386101));
#56745=CARTESIAN_POINT('Ctrl Pts',(-0.255717145023625,2.29694080388856,
5.46165868380294));
#56746=CARTESIAN_POINT('Ctrl Pts',(-0.265768140835497,2.28228678213695,
5.46275331374487));
#56747=CARTESIAN_POINT('Ctrl Pts',(-0.275999938029845,2.26736915790842,
5.46386763433343));
#56748=CARTESIAN_POINT('Ctrl Pts',(-0.284961065392298,2.25160330911764,
5.46498195492198));
#56749=CARTESIAN_POINT('Ctrl Pts',(-0.292528247268615,2.23523461160129,
5.46609627551054));
#56750=CARTESIAN_POINT('Ctrl Pts',(-0.300095429144934,2.21886591408494,
5.46721059609909));
#56751=CARTESIAN_POINT('Ctrl Pts',(-0.306268433004919,2.20189517339176,
5.46832491668765));
#56752=CARTESIAN_POINT('Ctrl Pts',(-0.310976723501059,2.18458518230486,
5.46943923727621));
#56753=CARTESIAN_POINT('Ctrl Pts',(-0.316842100935001,2.16302117065645,
5.47082740795931));
#56754=CARTESIAN_POINT('Ctrl Pts',(-0.320466759043346,2.14082296958456,
5.47221557864242));
#56755=CARTESIAN_POINT('Ctrl Pts',(-0.321749112810183,2.11840337009517,
5.47360374932553));
#56756=CARTESIAN_POINT('Ctrl Pts',(-0.32209365089258,2.11237975475911,5.47397671790688));
#56757=CARTESIAN_POINT('Ctrl Pts',(-0.322269364165322,2.10634028175669,
5.47434968648822));
#56758=CARTESIAN_POINT('Ctrl Pts',(-0.322274866580731,2.10029324967485,
5.47472265506957));
#56759=CARTESIAN_POINT('',(-0.322274952656718,2.09975862400584,5.72487098172704));
#56760=CARTESIAN_POINT('Ctrl Pts',(-0.322274869645138,2.1002898623972,5.47466220412381));
#56761=CARTESIAN_POINT('Ctrl Pts',(-0.322295039416003,2.07786470363518,
5.47591876512393));
#56762=CARTESIAN_POINT('Ctrl Pts',(-0.319974701019861,2.05550143112443,
5.47719494582332));
#56763=CARTESIAN_POINT('Ctrl Pts',(-0.31511241078133,2.0324226576908,5.47862363347245));
#56764=CARTESIAN_POINT('Ctrl Pts',(-0.314866454738616,2.03128577841999,
5.47869428649189));
#56765=CARTESIAN_POINT('Ctrl Pts',(-0.314472000395494,2.02950909306706,
5.47880514099861));
#56766=CARTESIAN_POINT('Ctrl Pts',(-0.314327690013433,2.0288683595453,5.47884520864498));
#56767=CARTESIAN_POINT('Ctrl Pts',(-0.314081940527683,2.02779259177882,
5.47891263327804));
#56768=CARTESIAN_POINT('Ctrl Pts',(-0.3139815532966,2.02735731727185,5.47893995649529));
#56769=CARTESIAN_POINT('Ctrl Pts',(-0.313781840838838,2.02649952126034,
5.47899388589563));
#56770=CARTESIAN_POINT('Ctrl Pts',(-0.313682566348333,2.02607698882368,
5.47902049039843));
#56771=CARTESIAN_POINT('Ctrl Pts',(-0.313491653720592,2.02527173529575,
5.47907126952667));
#56772=CARTESIAN_POINT('Ctrl Pts',(-0.313400167479033,2.02488897870412,
5.47909543921964));
#56773=CARTESIAN_POINT('Ctrl Pts',(-0.313189697854583,2.02401550325668,
5.47915067215672));
#56774=CARTESIAN_POINT('Ctrl Pts',(-0.313070262025087,2.02352489543324,
5.47918174993945));
#56775=CARTESIAN_POINT('Ctrl Pts',(-0.312701435295801,2.02202520643533,
5.47927691768361));
#56776=CARTESIAN_POINT('Ctrl Pts',(-0.312448316870483,2.02101705683022,
5.47934112781115));
#56777=CARTESIAN_POINT('Ctrl Pts',(-0.310542503289915,2.01357890521393,
5.47981662985734));
#56778=CARTESIAN_POINT('Ctrl Pts',(-0.308696451843209,2.00720052787361,
5.48023415560076));
#56779=CARTESIAN_POINT('Ctrl Pts',(-0.306086022594601,1.99912411889603,
5.48077599848467));
#56780=CARTESIAN_POINT('Ctrl Pts',(-0.305502048030464,1.99736913210421,
5.48089454325521));
#56781=CARTESIAN_POINT('Ctrl Pts',(-0.300225244363447,1.98195523596384,
5.48194281753255));
#56782=CARTESIAN_POINT('Ctrl Pts',(-0.294634795383065,1.96862262230926,
5.48290000506907));
#56783=CARTESIAN_POINT('Ctrl Pts',(-0.285867025182904,1.95111186864262,
5.4842173697174));
#56784=CARTESIAN_POINT('Ctrl Pts',(-0.283454410104206,1.94656849169576,
5.48456486695539));
#56785=CARTESIAN_POINT('Ctrl Pts',(-0.278571130692444,1.93788104162778,
5.48523905315639));
#56786=CARTESIAN_POINT('Ctrl Pts',(-0.276114066707337,1.93373077887201,
5.48556560446138));
#56787=CARTESIAN_POINT('Ctrl Pts',(-0.267446515115443,1.9198126166023,5.48667350921797));
#56788=CARTESIAN_POINT('Ctrl Pts',(-0.260802985595397,1.9103240359307,5.48745106172768));
#56789=CARTESIAN_POINT('Ctrl Pts',(-0.251070460141749,1.89790481434811,
5.48848148880088));
#56790=CARTESIAN_POINT('Ctrl Pts',(-0.248413401897396,1.89464755786082,
5.48875298747842));
#56791=CARTESIAN_POINT('Ctrl Pts',(-0.244191156615343,1.88967348648262,
5.48916835237233));
#56792=CARTESIAN_POINT('Ctrl Pts',(-0.242669936333266,1.887920142379,5.48931491930548));
#56793=CARTESIAN_POINT('Ctrl Pts',(-0.240904976852216,1.88592972500554,
5.48948132529066));
#56794=CARTESIAN_POINT('Ctrl Pts',(-0.240679699471364,1.88567647638853,
5.48950249817451));
#56795=CARTESIAN_POINT('Ctrl Pts',(-0.240250549294356,1.88519557132406,
5.48954270425292));
#56796=CARTESIAN_POINT('Ctrl Pts',(-0.240046751602167,1.88496784877108,
5.48956174297938));
#56797=CARTESIAN_POINT('Ctrl Pts',(-0.239693804421044,1.88457459436594,
5.48959462040412));
#56798=CARTESIAN_POINT('Ctrl Pts',(-0.239544806859487,1.88440892695135,
5.48960847058834));
#56799=CARTESIAN_POINT('Ctrl Pts',(-0.239257355483712,1.88408998139295,
5.48963513462629));
#56800=CARTESIAN_POINT('Ctrl Pts',(-0.239118926426719,1.88393668216679,
5.4896479503082));
#56801=CARTESIAN_POINT('Ctrl Pts',(-0.238789843609458,1.88357295260691,
5.48967835755085));
#56802=CARTESIAN_POINT('Ctrl Pts',(-0.23859905854623,1.88336264053352,5.48969593913818));
#56803=CARTESIAN_POINT('Ctrl Pts',(-0.2380266477082,1.88273331637492,5.48974854956863));
#56804=CARTESIAN_POINT('Ctrl Pts',(-0.23764419177435,1.88231505573409,5.489783516024));
#56805=CARTESIAN_POINT('Ctrl Pts',(-0.233936589356397,1.87828177180005,
5.49012072819342));
#56806=CARTESIAN_POINT('Ctrl Pts',(-0.230530093007673,1.87474196312295,
5.49041692418063));
#56807=CARTESIAN_POINT('Ctrl Pts',(-0.213017856733913,1.85735797837242,
5.49188133070462));
#56808=CARTESIAN_POINT('Ctrl Pts',(-0.197739266187922,1.84475282556504,
5.49297726249604));
#56809=CARTESIAN_POINT('Ctrl Pts',(-0.174691618674529,1.82905739518009,
5.49453626283725));
#56810=CARTESIAN_POINT('Ctrl Pts',(-0.167812732251578,1.82474386706052,
5.49499075892837));
#56811=CARTESIAN_POINT('Ctrl Pts',(-0.152286048325084,1.81580613145408,
5.49600530570774));
#56812=CARTESIAN_POINT('Ctrl Pts',(-0.143575614649371,1.81130774670117,
5.49656723894533));
#56813=CARTESIAN_POINT('Ctrl Pts',(-0.129697927002537,1.80492437166496,
5.49746281379729));
#56814=CARTESIAN_POINT('Ctrl Pts',(-0.124664300869996,1.80276274522428,
5.49778766088663));
#56815=CARTESIAN_POINT('Ctrl Pts',(-0.11767006635181,1.79996807908464,5.49824027529802));
#56816=CARTESIAN_POINT('Ctrl Pts',(-0.115754676201834,1.79922391597172,
5.49836434768622));
#56817=CARTESIAN_POINT('Ctrl Pts',(-0.112467638040274,1.79798289139977,
5.49857754291374));
#56818=CARTESIAN_POINT('Ctrl Pts',(-0.111099477821311,1.79747692747115,
5.49866636074617));
#56819=CARTESIAN_POINT('Ctrl Pts',(-0.109307685550258,1.79682809285152,
5.49878279885299));
#56820=CARTESIAN_POINT('Ctrl Pts',(-0.108887109562394,1.7966767849762,5.49881013815319));
#56821=CARTESIAN_POINT('Ctrl Pts',(-0.108057329994095,1.79638020879685,
5.49886409489106));
#56822=CARTESIAN_POINT('Ctrl Pts',(-0.107648144806369,1.79623489158147,
5.49889071063728));
#56823=CARTESIAN_POINT('Ctrl Pts',(-0.106867596877025,1.79595946454169,
5.49894149830139));
#56824=CARTESIAN_POINT('Ctrl Pts',(-0.106496286811176,1.79582920692924,
5.49896566525841));
#56825=CARTESIAN_POINT('Ctrl Pts',(-0.105648294629428,1.79553346969367,
5.49902087388109));
#56826=CARTESIAN_POINT('Ctrl Pts',(-0.105171461435552,1.79536842919721,
5.49905193003896));
#56827=CARTESIAN_POINT('Ctrl Pts',(-0.103712842552697,1.79486740799666,
5.49914696738483));
#56828=CARTESIAN_POINT('Ctrl Pts',(-0.102729827265973,1.79453505117183,
5.49921106825836));
#56829=CARTESIAN_POINT('Ctrl Pts',(-0.0954821775133347,1.79212356725776,
5.49968407946031));
#56830=CARTESIAN_POINT('Ctrl Pts',(-0.0891569879735945,1.79023272417629,
5.50009915048292));
#56831=CARTESIAN_POINT('Ctrl Pts',(-0.0810052264134533,1.78806619968929,
5.50063751076568));
#56832=CARTESIAN_POINT('Ctrl Pts',(-0.0792279247514117,1.78761005424845,
5.50075508955459));
#56833=CARTESIAN_POINT('Ctrl Pts',(-0.0752122807052728,1.7866159100921,
5.50102120425307));
#56834=CARTESIAN_POINT('Ctrl Pts',(-0.0729718900094262,1.78608667146019,
5.50116999219249));
#56835=CARTESIAN_POINT('Ctrl Pts',(-0.0664200754710443,1.78461289036432,
5.50160601784391));
#56836=CARTESIAN_POINT('Ctrl Pts',(-0.0620947977488439,1.78373288378242,
5.50189501680985));
#56837=CARTESIAN_POINT('Ctrl Pts',(-0.0491804405426671,1.78138049933143,
5.50276091374107));
#56838=CARTESIAN_POINT('Ctrl Pts',(-0.0405485689226521,1.78016738635559,
5.50334370992194));
#56839=CARTESIAN_POINT('Ctrl Pts',(-0.00797611926683815,1.77692952782993,
5.50554898081245));
#56840=CARTESIAN_POINT('Ctrl Pts',(0.0161181246918636,1.77723307199857,
5.50719833123795));
#56841=CARTESIAN_POINT('Ctrl Pts',(0.042996590793723,1.78059139142204,5.50893232954168));
#56842=CARTESIAN_POINT('Ctrl Pts',(0.0460318940539969,1.78101468298175,
5.50912649934827));
#56843=CARTESIAN_POINT('Ctrl Pts',(0.0495659346278239,1.78155902441389,
5.50935028950308));
#56844=CARTESIAN_POINT('Ctrl Pts',(0.0500708568414377,1.78163802659319,
5.5093822087016));
#56845=CARTESIAN_POINT('Ctrl Pts',(0.0508394651533864,1.78176015995089,
5.5094307117353));
#56846=CARTESIAN_POINT('Ctrl Pts',(0.0511032861045851,1.78180241804483,
5.50944734483163));
#56847=CARTESIAN_POINT('Ctrl Pts',(0.0515614476923745,1.7818763895743,5.50947620351358));
#56848=CARTESIAN_POINT('Ctrl Pts',(0.0517558113507193,1.78190795295927,
5.50948843763293));
#56849=CARTESIAN_POINT('Ctrl Pts',(0.0521632878405286,1.78197450783408,
5.50951406824309));
#56850=CARTESIAN_POINT('Ctrl Pts',(0.0523763937597191,1.78200953529534,
5.50952746261199));
#56851=CARTESIAN_POINT('Ctrl Pts',(0.0529711104062391,1.78210790081363,
5.50956481441183));
#56852=CARTESIAN_POINT('Ctrl Pts',(0.0533526441683417,1.78217171204132,
5.5095887448618));
#56853=CARTESIAN_POINT('Ctrl Pts',(0.0548871891364662,1.7824312045983,5.50968486800382));
#56854=CARTESIAN_POINT('Ctrl Pts',(0.0560392645927981,1.78263247761223,
5.50975674678841));
#56855=CARTESIAN_POINT('Ctrl Pts',(0.0765077279115629,1.78632334783021,
5.51102909510853));
#56856=CARTESIAN_POINT('Ctrl Pts',(0.0954699152458125,1.7915648854506,5.51213467515926));
#56857=CARTESIAN_POINT('Ctrl Pts',(0.125460328708668,1.80288861042201,5.51392904866884));
#56858=CARTESIAN_POINT('Ctrl Pts',(0.136817650594346,1.80794453532368,5.51461996365921));
#56859=CARTESIAN_POINT('Ctrl Pts',(0.157552125344653,1.81865036391846,5.51594149064312));
#56860=CARTESIAN_POINT('Ctrl Pts',(0.16698835011805,1.82414650456605,5.5165683155795));
#56861=CARTESIAN_POINT('Ctrl Pts',(0.181939144824755,1.83390323392207,5.51762012449362));
#56862=CARTESIAN_POINT('Ctrl Pts',(0.18762678391317,1.83788262103993,5.51803515410984));
#56863=CARTESIAN_POINT('Ctrl Pts',(0.194048595074708,1.84269183340754,5.51852322293015));
#56864=CARTESIAN_POINT('Ctrl Pts',(0.194912659816613,1.8433457484398,5.5185893123363));
#56865=CARTESIAN_POINT('Ctrl Pts',(0.19609925589007,1.84425319993321,5.51868065715743));
#56866=CARTESIAN_POINT('Ctrl Pts',(0.196424632452732,1.84450301827929,5.51870576598485));
#56867=CARTESIAN_POINT('Ctrl Pts',(0.19707381415707,1.84500342151033,5.51875598522046));
#56868=CARTESIAN_POINT('Ctrl Pts',(0.197397620497288,1.84525400358905,5.51878109548911));
#56869=CARTESIAN_POINT('Ctrl Pts',(0.198037357830995,1.84575102542282,5.518830827297));
#56870=CARTESIAN_POINT('Ctrl Pts',(0.19835330854856,1.84599743868267,5.51885544775638));
#56871=CARTESIAN_POINT('Ctrl Pts',(0.199048614515774,1.84654180350524,5.51890976041343));
#56872=CARTESIAN_POINT('Ctrl Pts',(0.199427761483535,1.84684001845344,5.51893946307942));
#56873=CARTESIAN_POINT('Ctrl Pts',(0.200749692709195,1.84788458518436,5.51904332708928));
#56874=CARTESIAN_POINT('Ctrl Pts',(0.201688959393291,1.84863535430274,5.51911766507012));
#56875=CARTESIAN_POINT('Ctrl Pts',(0.211554417011902,1.85661184850422,5.51990423461445));
#56876=CARTESIAN_POINT('Ctrl Pts',(0.22009146974321,1.86430368066689,5.52063546820119));
#56877=CARTESIAN_POINT('Ctrl Pts',(0.232070027442631,1.87631555881756,5.52174109823591));
#56878=CARTESIAN_POINT('Ctrl Pts',(0.235841094106152,1.88029519713349,5.52210202317852));
#56879=CARTESIAN_POINT('Ctrl Pts',(0.252357779804051,1.89864083490154,5.52374070465222));
#56880=CARTESIAN_POINT('Ctrl Pts',(0.263905081720795,1.91403228004728,5.52505158731254));
#56881=CARTESIAN_POINT('Ctrl Pts',(0.277753991620937,1.93640167190296,5.52681986889858));
#56882=CARTESIAN_POINT('Ctrl Pts',(0.281294573733258,1.94256726513338,5.52729395957921));
#56883=CARTESIAN_POINT('Ctrl Pts',(0.287948678308964,1.95509712106857,5.52822484751959));
#56884=CARTESIAN_POINT('Ctrl Pts',(0.291062250707027,1.96145733498274,5.5286814642977));
#56885=CARTESIAN_POINT('Ctrl Pts',(0.294260508014744,1.96857529804747,5.52917116638926));
#56886=CARTESIAN_POINT('Ctrl Pts',(0.294554754441885,1.96923610773584,5.52921642971607));
#56887=CARTESIAN_POINT('Ctrl Pts',(0.294972547887366,1.97018294149415,5.52928099442377));
#56888=CARTESIAN_POINT('Ctrl Pts',(0.29509790618423,1.97046815660263,5.52930040568847));
#56889=CARTESIAN_POINT('Ctrl Pts',(0.295312642258065,1.97095865361975,5.52933372296816));
#56890=CARTESIAN_POINT('Ctrl Pts',(0.295402219895857,1.97116384733002,5.52934764130235));
#56891=CARTESIAN_POINT('Ctrl Pts',(0.2955734775248,1.97155726136999,5.52937428897157));
#56892=CARTESIAN_POINT('Ctrl Pts',(0.295655191478141,1.97174546606261,5.52938702041693));
#56893=CARTESIAN_POINT('Ctrl Pts',(0.295847450587662,1.97218944001578,5.52941701526175));
#56894=CARTESIAN_POINT('Ctrl Pts',(0.295957844097497,1.97244527534732,5.52943426932124));
#56895=CARTESIAN_POINT('Ctrl Pts',(0.296283518378198,1.97320271959478,5.52948526465528));
#56896=CARTESIAN_POINT('Ctrl Pts',(0.296497858076163,1.97370473584789,5.52951894876024));
#56897=CARTESIAN_POINT('Ctrl Pts',(0.298387981115609,1.97816302432943,5.52981709633304));
#56898=CARTESIAN_POINT('Ctrl Pts',(0.299985865234027,1.9821521279428,5.53007693996119));
#56899=CARTESIAN_POINT('Ctrl Pts',(0.301532487609039,1.98624877479189,5.53033794780547));
#56900=CARTESIAN_POINT('Ctrl Pts',(0.301561358511304,1.98632533539577,5.53034282361473));
#56901=CARTESIAN_POINT('Ctrl Pts',(0.301945366214564,1.98734483279348,5.53040772358156));
#56902=CARTESIAN_POINT('Ctrl Pts',(0.302296112262658,1.98828943006488,5.5304675440082));
#56903=CARTESIAN_POINT('Ctrl Pts',(0.302743891859443,1.98951290246778,5.53054464211683));
#56904=CARTESIAN_POINT('Ctrl Pts',(0.302844976545546,1.98979027737278,5.53056209572466));
#56905=CARTESIAN_POINT('Ctrl Pts',(0.303592262984062,1.99184961195699,5.53069149214904));
#56906=CARTESIAN_POINT('Ctrl Pts',(0.304223125769417,1.99363713709346,5.53080277885917));
#56907=CARTESIAN_POINT('Ctrl Pts',(0.30637900156563,1.99992186768926,5.53119078535168));
#56908=CARTESIAN_POINT('Ctrl Pts',(0.307820405502191,2.00444725779309,5.53146435081629));
#56909=CARTESIAN_POINT('Ctrl Pts',(0.313773653113842,2.02467335495098,5.53266793579159));
#56910=CARTESIAN_POINT('Ctrl Pts',(0.317188058125169,2.04067221641019,5.53357049460153));
#56911=CARTESIAN_POINT('Ctrl Pts',(0.321054278317949,2.06929567536191,5.53519182435985));
#56912=CARTESIAN_POINT('Ctrl Pts',(0.322006106270631,2.08181656449784,5.53590303811867));
#56913=CARTESIAN_POINT('Ctrl Pts',(0.322338286338671,2.10079584545927,5.53700936454063));
#56914=CARTESIAN_POINT('Ctrl Pts',(0.322258096219163,2.10723294464565,5.53738938925162));
#56915=CARTESIAN_POINT('Ctrl Pts',(0.321835752299973,2.11718597211689,5.5379867600805));
#56916=CARTESIAN_POINT('Ctrl Pts',(0.321628457296497,2.12070611132324,5.53819992446199));
#56917=CARTESIAN_POINT('Ctrl Pts',(0.321303752563177,2.12501409880645,5.53846333773981));
#56918=CARTESIAN_POINT('Ctrl Pts',(0.321241125094297,2.12580593111411,5.53851185972658));
#56919=CARTESIAN_POINT('Ctrl Pts',(0.321144266226192,2.12697554032314,5.53858368915228));
#56920=CARTESIAN_POINT('Ctrl Pts',(0.321112293814993,2.12735350552724,5.53860692558892));
#56921=CARTESIAN_POINT('Ctrl Pts',(0.321049057875516,2.12808566346722,5.53865198459456));
#56922=CARTESIAN_POINT('Ctrl Pts',(0.321017875294259,2.12843986278171,5.53867380458778));
#56923=CARTESIAN_POINT('Ctrl Pts',(0.32095251725464,2.12916845264115,5.53871873316167));
#56924=CARTESIAN_POINT('Ctrl Pts',(0.320918272742553,2.12954283635068,5.53874184388517));
#56925=CARTESIAN_POINT('Ctrl Pts',(0.320834363764139,2.13044282143607,5.53879745885791));
#56926=CARTESIAN_POINT('Ctrl Pts',(0.320784062814432,2.13096836107868,5.53882998309175));
#56927=CARTESIAN_POINT('Ctrl Pts',(0.320626066032162,2.13257739977866,5.53892971137704));
#56928=CARTESIAN_POINT('Ctrl Pts',(0.320514171124259,2.13366047024979,5.53899704745965));
#56929=CARTESIAN_POINT('Ctrl Pts',(0.319126221929996,2.14646003292185,5.53979530860743));
#56930=CARTESIAN_POINT('Ctrl Pts',(0.317214025059591,2.15809719954957,5.54054630763282));
#56931=CARTESIAN_POINT('Ctrl Pts',(0.314392653969702,2.17085247937803,5.54139873219072));
#56932=CARTESIAN_POINT('Ctrl Pts',(0.314108708655933,2.17210085842848,5.54148246953287));
#56933=CARTESIAN_POINT('Ctrl Pts',(0.307715381607373,2.19945471301917,5.54332400606755));
#56934=CARTESIAN_POINT('Ctrl Pts',(0.298379292015336,2.22469767921069,5.54517058108146));
#56935=CARTESIAN_POINT('Ctrl Pts',(0.281603260167049,2.25701283143421,5.54759307076845));
#56936=CARTESIAN_POINT('Ctrl Pts',(0.276798542339603,2.2653361160755,5.54822150001533));
#56937=CARTESIAN_POINT('Ctrl Pts',(0.270875548856404,2.27461263169682,5.54891693542782));
#56938=CARTESIAN_POINT('Ctrl Pts',(0.270114733885519,2.27578727150623,5.54900489812689));
#56939=CARTESIAN_POINT('Ctrl Pts',(0.269120787197656,2.27730015838857,5.54911802608913));
#56940=CARTESIAN_POINT('Ctrl Pts',(0.268894642009926,2.27764294460887,5.54914364736011));
#56941=CARTESIAN_POINT('Ctrl Pts',(0.268532393220227,2.27818975718383,5.5491844996308));
#56942=CARTESIAN_POINT('Ctrl Pts',(0.268396711813417,2.27839406061448,5.54919975890493));
#56943=CARTESIAN_POINT('Ctrl Pts',(0.268139306283006,2.27878069278044,5.5492286279143));
#56944=CARTESIAN_POINT('Ctrl Pts',(0.268017630345328,2.27896305068184,5.54924224066575));
#56945=CARTESIAN_POINT('Ctrl Pts',(0.267739131897342,2.27937952022521,5.54927332164872));
#56946=CARTESIAN_POINT('Ctrl Pts',(0.267582188607598,2.27961355006454,5.54929078155951));
#56947=CARTESIAN_POINT('Ctrl Pts',(0.267099895655398,2.28033069794003,5.54934426834693));
#56948=CARTESIAN_POINT('Ctrl Pts',(0.266773540765566,2.28081314343429,5.54938022756913));
#56949=CARTESIAN_POINT('Ctrl Pts',(0.264338631138373,2.28439169045772,5.54964680676294));
#56950=CARTESIAN_POINT('Ctrl Pts',(0.2621774385234,2.28745186342891,5.54987394035509));
#56951=CARTESIAN_POINT('Ctrl Pts',(0.259261333730675,2.29143183373422,5.55016923247058));
#56952=CARTESIAN_POINT('Ctrl Pts',(0.258554098592807,2.29238597744342,5.55024001611934));
#56953=CARTESIAN_POINT('Ctrl Pts',(0.257006213827043,2.29445030409225,5.55039319247933));
#56954=CARTESIAN_POINT('Ctrl Pts',(0.256163607684727,2.29555899602032,5.5504754803148));
#56955=CARTESIAN_POINT('Ctrl Pts',(0.254379999302698,2.29787453945384,5.55064746651978));
#56956=CARTESIAN_POINT('Ctrl Pts',(0.253437532002508,2.2990802223354,5.55073709053411));
#56957=CARTESIAN_POINT('Ctrl Pts',(0.250009880001951,2.30340137003331,5.55105874574034));
#56958=CARTESIAN_POINT('Ctrl Pts',(0.247475480406074,2.30647747109506,5.5512885654422));
#56959=CARTESIAN_POINT('Ctrl Pts',(0.228932302030499,2.32815198966563,5.55292027719812));
#56960=CARTESIAN_POINT('Ctrl Pts',(0.210902487277469,2.34491542995423,5.55425524586823));
#56961=CARTESIAN_POINT('Ctrl Pts',(0.180767606197172,2.36711486715365,5.55639719107328));
#56962=CARTESIAN_POINT('Ctrl Pts',(0.169943035446717,2.37412877452456,5.55715056787063));
#56963=CARTESIAN_POINT('Ctrl Pts',(0.157463177791235,2.38119145992263,5.55801681056844));
#56964=CARTESIAN_POINT('Ctrl Pts',(0.156193023137833,2.381898969331,5.5581049390324));
#56965=CARTESIAN_POINT('Ctrl Pts',(0.153949719159728,2.38312873268272,5.55826054958932));
#56966=CARTESIAN_POINT('Ctrl Pts',(0.152978585097126,2.38365462759139,5.55832790118789));
#56967=CARTESIAN_POINT('Ctrl Pts',(0.151550044107019,2.38441875061441,5.55842696405328));
#56968=CARTESIAN_POINT('Ctrl Pts',(0.151094730660062,2.38466089287393,5.55845853626862));
#56969=CARTESIAN_POINT('Ctrl Pts',(0.150288265126148,2.38508730286089,5.55851445575335));
#56970=CARTESIAN_POINT('Ctrl Pts',(0.149937349604948,2.3852720176924,5.55853878713094));
#56971=CARTESIAN_POINT('Ctrl Pts',(0.149255803872446,2.38562916462576,5.55858604231771));
#56972=CARTESIAN_POINT('Ctrl Pts',(0.148925213398252,2.38580167159569,5.55860896343416));
#56973=CARTESIAN_POINT('Ctrl Pts',(0.14813599489041,2.38621175626834,5.55866368224964));
#56974=CARTESIAN_POINT('Ctrl Pts',(0.147677094712553,2.38644880537485,5.5586954985269));
#56975=CARTESIAN_POINT('Ctrl Pts',(0.146037041604601,2.38729100130721,5.55880920529237));
#56976=CARTESIAN_POINT('Ctrl Pts',(0.144852735260972,2.387889947646,5.55889131335468));
#56977=CARTESIAN_POINT('Ctrl Pts',(0.123358872762979,2.39859396291889,5.56038157408449));
#56978=CARTESIAN_POINT('Ctrl Pts',(0.102046377603564,2.40653208142139,5.56186769253266));
#56979=CARTESIAN_POINT('Ctrl Pts',(0.0658924549141328,2.41580680735454,
5.56437939030894));
#56980=CARTESIAN_POINT('Ctrl Pts',(0.051471858556127,2.41847511877644,5.56537709262186));
#56981=CARTESIAN_POINT('Ctrl Pts',(0.0252655019948851,2.42149721532713,
5.5671444763503));
#56982=CARTESIAN_POINT('Ctrl Pts',(0.0135450624519604,2.42220397259656,
5.56791842020518));
#56983=CARTESIAN_POINT('Ctrl Pts',(0.000221912068356351,2.42227884137083,
5.56876152563732));
#56984=CARTESIAN_POINT('Ctrl Pts',(-0.00136723884647932,2.42227601794867,
5.56886149261588));
#56985=CARTESIAN_POINT('Ctrl Pts',(-0.00337230365008466,2.42225762400849,
5.56898681551018));
#56986=CARTESIAN_POINT('Ctrl Pts',(-0.00378826013363588,2.42225300270642,
5.56901277025045));
#56987=CARTESIAN_POINT('Ctrl Pts',(-0.00445063106545653,2.42224436107115,
5.56905402959807));
#56988=CARTESIAN_POINT('Ctrl Pts',(-0.00469705007615137,2.42224086345557,
5.56906936346601));
#56989=CARTESIAN_POINT('Ctrl Pts',(-0.00516243649555589,2.42223372392391,
5.56909829307104));
#56990=CARTESIAN_POINT('Ctrl Pts',(-0.00538140240343053,2.42223014150282,
5.5691118920063));
#56991=CARTESIAN_POINT('Ctrl Pts',(-0.00588007284775842,2.42222147449788,
5.56914283369319));
#56992=CARTESIAN_POINT('Ctrl Pts',(-0.00615977402736211,2.42221624892242,
5.5691601683964));
#56993=CARTESIAN_POINT('Ctrl Pts',(-0.00701159420103367,2.42219922506018,
5.56921289976747));
#56994=CARTESIAN_POINT('Ctrl Pts',(-0.00758369280629195,2.42218626708462,
5.56924823153866));
#56995=CARTESIAN_POINT('Ctrl Pts',(-0.0116853252403361,2.42208243451034,
5.56950096066145));
#56996=CARTESIAN_POINT('Ctrl Pts',(-0.0152133617157631,2.42193508283617,
5.56971526595571));
#56997=CARTESIAN_POINT('Ctrl Pts',(-0.0510842193015345,2.41984586426108,
5.57186925757705));
#56998=CARTESIAN_POINT('Ctrl Pts',(-0.0829654846381817,2.41309486697978,
5.57359321169757));
#56999=CARTESIAN_POINT('Ctrl Pts',(-0.127066442583779,2.39653213187297,
5.57628469362726));
#57000=CARTESIAN_POINT('Ctrl Pts',(-0.140454032552032,2.39043030645595,
5.57714452415153));
#57001=CARTESIAN_POINT('Ctrl Pts',(-0.15443994632272,2.38286204756227,5.57811115292283));
#57002=CARTESIAN_POINT('Ctrl Pts',(-0.155499145147346,2.38228115553036,
5.57818479329279));
#57003=CARTESIAN_POINT('Ctrl Pts',(-0.15702440872034,2.38143347178752,5.57829147529698));
#57004=CARTESIAN_POINT('Ctrl Pts',(-0.157493120678105,2.3811714439802,5.57832434619832));
#57005=CARTESIAN_POINT('Ctrl Pts',(-0.158308361753162,2.3807130151585,5.57838167302838));
#57006=CARTESIAN_POINT('Ctrl Pts',(-0.158655186683821,2.38051714032545,
5.57840611000084));
#57007=CARTESIAN_POINT('Ctrl Pts',(-0.15932347086983,2.38013808050322,5.57845329100383));
#57008=CARTESIAN_POINT('Ctrl Pts',(-0.159644979734389,2.37995498381324,
5.57847603182433));
#57009=CARTESIAN_POINT('Ctrl Pts',(-0.160404918846401,2.37952046985351,
5.57852988387269));
#57010=CARTESIAN_POINT('Ctrl Pts',(-0.160843073409277,2.37926857465325,
5.57856101233922));
#57011=CARTESIAN_POINT('Ctrl Pts',(-0.162372849968561,2.37838431124759,
5.57866997327037));
#57012=CARTESIAN_POINT('Ctrl Pts',(-0.163461339086637,2.37774657100877,
5.57874800025504));
#57013=CARTESIAN_POINT('Ctrl Pts',(-0.178340752657707,2.36891103558384,
5.5798215333238));
#57014=CARTESIAN_POINT('Ctrl Pts',(-0.191502307695084,2.35970231571622,
5.58085476216332));
#57015=CARTESIAN_POINT('Ctrl Pts',(-0.2103070685247,2.34433604229763,5.58246300907199));
#57016=CARTESIAN_POINT('Ctrl Pts',(-0.21648912836491,2.3388757217534,5.58301579169205));
#57017=CARTESIAN_POINT('Ctrl Pts',(-0.233515297686581,2.3226330013751,5.58460288321765));
#57018=CARTESIAN_POINT('Ctrl Pts',(-0.243811198661628,2.31130774121618,
5.58564413352071));
#57019=CARTESIAN_POINT('Ctrl Pts',(-0.259296612193892,2.29162878138581,
5.58731113280887));
#57020=CARTESIAN_POINT('Ctrl Pts',(-0.264978226450914,2.28369241399321,
5.58794973818881));
#57021=CARTESIAN_POINT('Ctrl Pts',(-0.271071994922174,2.27430778224615,
5.58865684087102));
#57022=CARTESIAN_POINT('Ctrl Pts',(-0.271844443778486,2.27310062955182,
5.58874691699477));
#57023=CARTESIAN_POINT('Ctrl Pts',(-0.272822787754532,2.27154901056902,
5.58886153546993));
#57024=CARTESIAN_POINT('Ctrl Pts',(-0.273036111798481,2.27120928188474,
5.58888656052523));
#57025=CARTESIAN_POINT('Ctrl Pts',(-0.273377704766443,2.27066301670217,
5.5889266847581));
#57026=CARTESIAN_POINT('Ctrl Pts',(-0.273506374407568,2.27045673319825,
5.58894181048111));
#57027=CARTESIAN_POINT('Ctrl Pts',(-0.273750877682042,2.27006375529491,
5.58897057541734));
#57028=CARTESIAN_POINT('Ctrl Pts',(-0.273866752865476,2.26987708960266,
5.58898421731618));
#57029=CARTESIAN_POINT('Ctrl Pts',(-0.274130370536744,2.2694514517753,5.58901527496823));
#57030=CARTESIAN_POINT('Ctrl Pts',(-0.274277991268687,2.26921240517888,
5.58903268258323));
#57031=CARTESIAN_POINT('Ctrl Pts',(-0.274736576057089,2.26846762852597,
5.58908681017239));
#57032=CARTESIAN_POINT('Ctrl Pts',(-0.275046457640657,2.26796122837524,
5.58912345895247));
#57033=CARTESIAN_POINT('Ctrl Pts',(-0.277432197536317,2.26403820840733,
5.58940620301845));
#57034=CARTESIAN_POINT('Ctrl Pts',(-0.279445831974639,2.26058389893638,
5.58964832050689));
#57035=CARTESIAN_POINT('Ctrl Pts',(-0.281631774391969,2.25666829822584,
5.58991620644255));
#57036=CARTESIAN_POINT('Ctrl Pts',(-0.281867813153797,2.25624323322828,
5.58994520163774));
#57037=CARTESIAN_POINT('Ctrl Pts',(-0.282171692339081,2.25569306958657,
5.58998262181291));
#57038=CARTESIAN_POINT('Ctrl Pts',(-0.282240411817415,2.25556846020985,
5.58999109012269));
#57039=CARTESIAN_POINT('Ctrl Pts',(-0.288542184469433,2.24412350464023,
5.59076822119098));
#57040=CARTESIAN_POINT('Ctrl Pts',(-0.294089414241081,2.23243737516183,
5.59150318956021));
#57041=CARTESIAN_POINT('Ctrl Pts',(-0.310538650271962,2.19161492203197,
5.59397735034514));
#57042=CARTESIAN_POINT('Ctrl Pts',(-0.317923142611618,2.16125577184274,
5.59568122426102));
#57043=CARTESIAN_POINT('Ctrl Pts',(-0.321103356018776,2.12759105351112,
5.59771772940258));
#57044=CARTESIAN_POINT('Ctrl Pts',(-0.321325593972288,2.1248695281943,5.59788322444787));
#57045=CARTESIAN_POINT('Ctrl Pts',(-0.321563749271872,2.12141194838804,
5.59809467219416));
#57046=CARTESIAN_POINT('Ctrl Pts',(-0.321611769132162,2.12067816048703,
5.59813961491862));
#57047=CARTESIAN_POINT('Ctrl Pts',(-0.321684520013776,2.11950484555407,
5.59821158855182));
#57048=CARTESIAN_POINT('Ctrl Pts',(-0.321710862805945,2.11906541807021,
5.59823856883306));
#57049=CARTESIAN_POINT('Ctrl Pts',(-0.321758978611058,2.11823428677734,
5.59828964676918));
#57050=CARTESIAN_POINT('Ctrl Pts',(-0.321780936916443,2.11784259415342,
5.59831373856303));
#57051=CARTESIAN_POINT('Ctrl Pts',(-0.321828934879923,2.11695748901073,
5.59836822415722));
#57052=CARTESIAN_POINT('Ctrl Pts',(-0.3218545550857,2.116464055568,5.59839863105959));
#57053=CARTESIAN_POINT('Ctrl Pts',(-0.321917255910508,2.11520035084856,
5.5984765872401));
#57054=CARTESIAN_POINT('Ctrl Pts',(-0.321952706550846,2.1144300050905,5.59852418752623));
#57055=CARTESIAN_POINT('Ctrl Pts',(-0.32214014786984,2.11001160262876,5.59879766296652));
#57056=CARTESIAN_POINT('Ctrl Pts',(-0.322232893435412,2.10636142117186,
5.59902538734719));
#57057=CARTESIAN_POINT('Ctrl Pts',(-0.322268819383934,2.1020901311049,5.59929408196456));
#57058=CARTESIAN_POINT('Ctrl Pts',(-0.322272246117975,2.10146968315857,
5.59933316725188));
#57059=CARTESIAN_POINT('Ctrl Pts',(-0.322274729611917,2.10052722618315,
5.5993926211616));
#57060=CARTESIAN_POINT('Ctrl Pts',(-0.322275095528039,2.10020521956859,
5.59941294943006));
#57061=CARTESIAN_POINT('Ctrl Pts',(-0.322271684120159,2.09079133210786,
5.6000076823408));
#57062=CARTESIAN_POINT('Ctrl Pts',(-0.321883651494965,2.08170444921664,
5.60059378601718));
#57063=CARTESIAN_POINT('Ctrl Pts',(-0.318099653150887,2.03728234170793,
5.60351711798254));
#57064=CARTESIAN_POINT('Ctrl Pts',(-0.309267229173563,2.00266449487461,
5.60600990815023));
#57065=CARTESIAN_POINT('Ctrl Pts',(-0.294100133651789,1.96820096658294,
5.60840486522824));
#57066=CARTESIAN_POINT('Ctrl Pts',(-0.293207011460761,1.9662258512745,5.60854167595591));
#57067=CARTESIAN_POINT('Ctrl Pts',(-0.292108909905293,1.96386127116063,
5.60870479395439));
#57068=CARTESIAN_POINT('Ctrl Pts',(-0.291923002579937,1.96346308445623,
5.60873223942929));
#57069=CARTESIAN_POINT('Ctrl Pts',(-0.291618151489236,1.96281360621666,
5.60877696635384));
#57070=CARTESIAN_POINT('Ctrl Pts',(-0.291499696754035,1.96256208779605,
5.60879427780816));
#57071=CARTESIAN_POINT('Ctrl Pts',(-0.29128743039153,1.96211288530184,5.60882517783779));
#57072=CARTESIAN_POINT('Ctrl Pts',(-0.291193743007796,1.96191514370491,
5.60883877409607));
#57073=CARTESIAN_POINT('Ctrl Pts',(-0.290993653015017,1.96149393230199,
5.60886772248641));
#57074=CARTESIAN_POINT('Ctrl Pts',(-0.290887194655796,1.96127049026808,
5.60888307103652));
#57075=CARTESIAN_POINT('Ctrl Pts',(-0.290599072890201,1.96066755051505,
5.60892446722927));
#57076=CARTESIAN_POINT('Ctrl Pts',(-0.290416922765928,1.96028828388406,
5.60895048458479));
#57077=CARTESIAN_POINT('Ctrl Pts',(-0.289520027814286,1.95843013362637,
5.60907784905689));
#57078=CARTESIAN_POINT('Ctrl Pts',(-0.288794710214921,1.95695633816627,
5.60917854804987));
#57079=CARTESIAN_POINT('Ctrl Pts',(-0.284575686806505,1.9485464828899,5.60975168573835));
#57080=CARTESIAN_POINT('Ctrl Pts',(-0.280843136534661,1.94173236770354,
5.61021030464034));
#57081=CARTESIAN_POINT('Ctrl Pts',(-0.268909142489587,1.92170010365539,
5.61156089960037));
#57082=CARTESIAN_POINT('Ctrl Pts',(-0.259993622897372,1.90893362416738,
5.61242554942837));
#57083=CARTESIAN_POINT('Ctrl Pts',(-0.240018087235018,1.88433140560677,
5.61419730733332));
#57084=CARTESIAN_POINT('Ctrl Pts',(-0.228919360810158,1.87258519057617,
5.61510269000134));
#57085=CARTESIAN_POINT('Ctrl Pts',(-0.209729049058428,1.85510961442861,
5.61661280011476));
#57086=CARTESIAN_POINT('Ctrl Pts',(-0.202172048187132,1.8488346990185,5.61719528319366));
#57087=CARTESIAN_POINT('Ctrl Pts',(-0.193510220840325,1.8422868753659,5.61785554221577));
#57088=CARTESIAN_POINT('Ctrl Pts',(-0.192676429016835,1.84166290657392,
5.61791902393836));
#57089=CARTESIAN_POINT('Ctrl Pts',(-0.191424867564646,1.84073572913391,
5.61801420721487));
#57090=CARTESIAN_POINT('Ctrl Pts',(-0.191009364358687,1.84042946085453,
5.61804578957989));
#57091=CARTESIAN_POINT('Ctrl Pts',(-0.190292505518085,1.83990371599445,
5.61810024897742));
#57092=CARTESIAN_POINT('Ctrl Pts',(-0.189991500655529,1.83968376100095,
5.61812310739805));
#57093=CARTESIAN_POINT('Ctrl Pts',(-0.189369485804514,1.83923088608776,
5.61817032571903));
#57094=CARTESIAN_POINT('Ctrl Pts',(-0.189048426260731,1.83899803554266,
5.61819468825139));
#57095=CARTESIAN_POINT('Ctrl Pts',(-0.188300119670472,1.83845742638522,
5.6182514488994));
#57096=CARTESIAN_POINT('Ctrl Pts',(-0.187872547495064,1.8381501216853,5.61828386444611));
#57097=CARTESIAN_POINT('Ctrl Pts',(-0.186507523867209,1.83717411629757,
5.61838729925704));
#57098=CARTESIAN_POINT('Ctrl Pts',(-0.185567248635086,1.83650939716588,
5.61845847117841));
#57099=CARTESIAN_POINT('Ctrl Pts',(-0.165216861119755,1.8222858316003,5.61999726991051));
#57100=CARTESIAN_POINT('Ctrl Pts',(-0.14437894263507,1.81090476902241,5.62155045089508));
#57101=CARTESIAN_POINT('Ctrl Pts',(-0.100697226864652,1.79295566204286,
5.62473192888082));
#57102=CARTESIAN_POINT('Ctrl Pts',(-0.0779901020985928,1.78641775892956,
5.62634890546494));
#57103=CARTESIAN_POINT('Ctrl Pts',(-0.0513527190731283,1.78182376753071,
5.62808492019714));
#57104=CARTESIAN_POINT('Ctrl Pts',(-0.0479237049567799,1.78128925718876,
5.6283052979047));
#57105=CARTESIAN_POINT('Ctrl Pts',(-0.0439228096747885,1.78073163889518,
5.62855831144904));
#57106=CARTESIAN_POINT('Ctrl Pts',(-0.0433588476256891,1.78065456014429,
5.62859388099007));
#57107=CARTESIAN_POINT('Ctrl Pts',(-0.0425180110532875,1.78054190841317,
5.62864676870856));
#57108=CARTESIAN_POINT('Ctrl Pts',(-0.0422412935829531,1.78050520088414,
5.62866415062883));
#57109=CARTESIAN_POINT('Ctrl Pts',(-0.0417474617536401,1.78044034517424,
5.62869512850483));
#57110=CARTESIAN_POINT('Ctrl Pts',(-0.0415303665944644,1.78041205872747,
5.62870873229801));
#57111=CARTESIAN_POINT('Ctrl Pts',(-0.0410684664279713,1.78035235398053,
5.62873764531517));
#57112=CARTESIAN_POINT('Ctrl Pts',(-0.04082365481761,1.78032099576474,5.62875295106238));
#57113=CARTESIAN_POINT('Ctrl Pts',(-0.0401645054337035,1.78023733404486,
5.62879411238003));
#57114=CARTESIAN_POINT('Ctrl Pts',(-0.0397500998336552,1.78018555441733,
5.62881993825236));
#57115=CARTESIAN_POINT('Ctrl Pts',(-0.0377402231692326,1.77993838894242,
5.62894494661227));
#57116=CARTESIAN_POINT('Ctrl Pts',(-0.036143370007888,1.77975413137111,
5.62904350954445));
#57117=CARTESIAN_POINT('Ctrl Pts',(-0.0226233437624814,1.77829650008731,
5.62987211979563));
#57118=CARTESIAN_POINT('Ctrl Pts',(-0.0106375794744982,1.77767738433408,
5.63056812075044));
#57119=CARTESIAN_POINT('Ctrl Pts',(0.0292505477647775,1.77784523171065,
5.63283706223557));
#57120=CARTESIAN_POINT('Ctrl Pts',(0.0570108113776403,1.78158341673356,
5.63434997488827));
#57121=CARTESIAN_POINT('Ctrl Pts',(0.0930871735592631,1.79131627596256,
5.63652722643062));
#57122=CARTESIAN_POINT('Ctrl Pts',(0.102116670787986,1.79418465984062,5.63708963085385));
#57123=CARTESIAN_POINT('Ctrl Pts',(0.112082515384229,1.79784110172805,5.63773517514946));
#57124=CARTESIAN_POINT('Ctrl Pts',(0.113156719533934,1.79824174107257,5.63780508413283));
#57125=CARTESIAN_POINT('Ctrl Pts',(0.114714921317338,1.79883238425544,5.63790697524715));
#57126=CARTESIAN_POINT('Ctrl Pts',(0.115200641417765,1.79901784412022,5.63793880514564));
#57127=CARTESIAN_POINT('Ctrl Pts',(0.116056449915167,1.79934698792746,5.63799500930376));
#57128=CARTESIAN_POINT('Ctrl Pts',(0.116426726497803,1.79949018220701,5.63801936708417));
#57129=CARTESIAN_POINT('Ctrl Pts',(0.117191125786115,1.79978741744612,5.63806973508912));
#57130=CARTESIAN_POINT('Ctrl Pts',(0.117585211404007,1.79994155112205,5.63809574839436));
#57131=CARTESIAN_POINT('Ctrl Pts',(0.118592166048454,1.80033767679874,5.63816233533064));
#57132=CARTESIAN_POINT('Ctrl Pts',(0.119204596382314,1.80058077218477,5.63820294608055));
#57133=CARTESIAN_POINT('Ctrl Pts',(0.121692708438512,1.80157723597374,5.6383683965021));
#57134=CARTESIAN_POINT('Ctrl Pts',(0.123561996595663,1.80234635215689,5.6384937672534));
#57135=CARTESIAN_POINT('Ctrl Pts',(0.153976087073731,1.81519605743917,5.64055147676102));
#57136=CARTESIAN_POINT('Ctrl Pts',(0.180632608726762,1.83131271353187,5.64263724661702));
#57137=CARTESIAN_POINT('Ctrl Pts',(0.218323451649387,1.86227581723676,5.64593491201262));
#57138=CARTESIAN_POINT('Ctrl Pts',(0.231117783291788,1.87469431377972,5.64712971177108));
#57139=CARTESIAN_POINT('Ctrl Pts',(0.243540059172243,1.88892985330789,5.64832011129109));
#57140=CARTESIAN_POINT('Ctrl Pts',(0.244253613387702,1.88975599967063,5.64838860131622));
#57141=CARTESIAN_POINT('Ctrl Pts',(0.245207392567154,1.89087168592748,5.64848028122478));
#57142=CARTESIAN_POINT('Ctrl Pts',(0.245451317709631,1.89115803162573,5.64850373971649));
#57143=CARTESIAN_POINT('Ctrl Pts',(0.245833111200154,1.89160781497218,5.6485404746464));
#57144=CARTESIAN_POINT('Ctrl Pts',(0.245971318198467,1.89177096271804,5.64855377609165));
#57145=CARTESIAN_POINT('Ctrl Pts',(0.246236806859725,1.89208499443579,5.64857933425364));
#57146=CARTESIAN_POINT('Ctrl Pts',(0.246364111307641,1.89223585667622,5.64859159261534));
#57147=CARTESIAN_POINT('Ctrl Pts',(0.246662670320094,1.89259032453136,5.64862034849148));
#57148=CARTESIAN_POINT('Ctrl Pts',(0.246833811213905,1.89279402506132,5.64863683756304));
#57149=CARTESIAN_POINT('Ctrl Pts',(0.247334050469771,1.89339093432121,5.64868505162227));
#57150=CARTESIAN_POINT('Ctrl Pts',(0.247662464839708,1.89378471913909,5.6487167265097));
#57151=CARTESIAN_POINT('Ctrl Pts',(0.2484057286578,1.89468026531379,5.64878846646553));
#57152=CARTESIAN_POINT('Ctrl Pts',(0.248820001803071,1.89518250513845,5.64882849043117));
#57153=CARTESIAN_POINT('Ctrl Pts',(0.263077815607167,1.9125749219,5.65020743692388));
#57154=CARTESIAN_POINT('Ctrl Pts',(0.275172887664815,1.93083052747052,5.65142712721316));
#57155=CARTESIAN_POINT('Ctrl Pts',(0.295568074914054,1.96967074543919,5.65387957986407));
#57156=CARTESIAN_POINT('Ctrl Pts',(0.303780200765764,1.99016526284765,5.65510798192187));
#57157=CARTESIAN_POINT('Ctrl Pts',(0.311612463255215,2.01753530250231,5.65678963381482));
#57158=CARTESIAN_POINT('Ctrl Pts',(0.313199901941567,2.02378605010888,5.65717590930341));
#57159=CARTESIAN_POINT('Ctrl Pts',(0.314822314881139,2.03108593897024,5.65763104627727));
#57160=CARTESIAN_POINT('Ctrl Pts',(0.315041081815506,2.03209304538884,5.65769392484574));
#57161=CARTESIAN_POINT('Ctrl Pts',(0.315359463626633,2.03359339253839,5.65778773402111));
#57162=CARTESIAN_POINT('Ctrl Pts',(0.315462761528865,2.03408585206891,5.65781854666922));
#57163=CARTESIAN_POINT('Ctrl Pts',(0.315644749385013,2.03496368311615,5.65787351085414));
#57164=CARTESIAN_POINT('Ctrl Pts',(0.315723888129888,2.03534896141504,5.65789764798533));
#57165=CARTESIAN_POINT('Ctrl Pts',(0.315889061429835,2.03616062577541,5.65794852633307));
#57166=CARTESIAN_POINT('Ctrl Pts',(0.315974938382422,2.03658704277768,5.65797527253255));
#57167=CARTESIAN_POINT('Ctrl Pts',(0.316199098944816,2.03771186037276,5.6580458692332));
#57168=CARTESIAN_POINT('Ctrl Pts',(0.316335931405178,2.03841054472757,5.65808976596633));
#57169=CARTESIAN_POINT('Ctrl Pts',(0.316941336482345,2.04155706770522,5.65828766340539));
#57170=CARTESIAN_POINT('Ctrl Pts',(0.317383809385245,2.04400978580732,5.65844249331573));
#57171=CARTESIAN_POINT('Ctrl Pts',(0.32043777427336,2.06213971196706,5.65959141615244));
#57172=CARTESIAN_POINT('Ctrl Pts',(0.32191443786841,2.07798346376891,5.66062163362133));
#57173=CARTESIAN_POINT('Ctrl Pts',(0.32272480736288,2.12057617880755,5.66345439825226));
#57174=CARTESIAN_POINT('Ctrl Pts',(0.319910808831705,2.14724052951334,5.66530113995622));
#57175=CARTESIAN_POINT('Ctrl Pts',(0.313577984584291,2.17437304659382,5.66712043648747));
#57176=CARTESIAN_POINT('Ctrl Pts',(0.313310150769913,2.17549339023988,5.6671954287632));
#57177=CARTESIAN_POINT('Ctrl Pts',(0.311827501636082,2.18155146561861,5.66760015246425));
#57178=CARTESIAN_POINT('Ctrl Pts',(0.310501875523857,2.18646169578967,5.66792537074629));
#57179=CARTESIAN_POINT('Ctrl Pts',(0.308880426357622,2.19194814593583,5.66828399507165));
#57180=CARTESIAN_POINT('Ctrl Pts',(0.308698545359132,2.1925569415948,5.66832372269519));
#57181=CARTESIAN_POINT('Ctrl Pts',(0.308431357950041,2.19344172782026,5.6683813593692));
#57182=CARTESIAN_POINT('Ctrl Pts',(0.308347480500788,2.19371814304244,5.66839935122224));
#57183=CARTESIAN_POINT('Ctrl Pts',(0.308198811824424,2.19420571532244,5.66843106145133));
#57184=CARTESIAN_POINT('Ctrl Pts',(0.308134175070046,2.19441691884663,5.66844478892069));
#57185=CARTESIAN_POINT('Ctrl Pts',(0.30800935594309,2.19482327764441,5.66847118411638));
#57186=CARTESIAN_POINT('Ctrl Pts',(0.307949205411923,2.19501844146495,5.66848385368565));
#57187=CARTESIAN_POINT('Ctrl Pts',(0.307787191206201,2.19554234138585,5.66851784454146));
#57188=CARTESIAN_POINT('Ctrl Pts',(0.307684986031808,2.19587097288192,5.66853914569239));
#57189=CARTESIAN_POINT('Ctrl Pts',(0.307296060059555,2.19711450116972,5.668619672563));
#57190=CARTESIAN_POINT('Ctrl Pts',(0.307005779755647,2.19802829243136,5.66867869121788));
#57191=CARTESIAN_POINT('Ctrl Pts',(0.306273711829903,2.20029766584284,5.66882490653003));
#57192=CARTESIAN_POINT('Ctrl Pts',(0.305826993786587,2.20165165208551,5.66891182686689));
#57193=CARTESIAN_POINT('Ctrl Pts',(0.302633307000184,2.21111995416262,5.66951772033062));
#57194=CARTESIAN_POINT('Ctrl Pts',(0.299572489523979,2.21912561921818,5.67002006997595));
#57195=CARTESIAN_POINT('Ctrl Pts',(0.290050709682761,2.24133272623132,5.67141015765725));
#57196=CARTESIAN_POINT('Ctrl Pts',(0.282872964539985,2.25520081274931,5.67227496391193));
#57197=CARTESIAN_POINT('Ctrl Pts',(0.266578006325859,2.28176852374226,5.67401900742099));
#57198=CARTESIAN_POINT('Ctrl Pts',(0.257486302370868,2.29443347500778,5.67489617462869));
#57199=CARTESIAN_POINT('Ctrl Pts',(0.241762138362382,2.31329077274653,5.67632983483744));
#57200=CARTESIAN_POINT('Ctrl Pts',(0.235723185319355,2.31994645311042,5.67686409547644));
#57201=CARTESIAN_POINT('Ctrl Pts',(0.228699589142733,2.32706543064022,5.67747231382474));
#57202=CARTESIAN_POINT('Ctrl Pts',(0.227981231297449,2.32778667653042,5.67753437368575));
#57203=CARTESIAN_POINT('Ctrl Pts',(0.226897667255206,2.32886433668427,5.67762776975596));
#57204=CARTESIAN_POINT('Ctrl Pts',(0.226535007248728,2.32922331141897,5.67765899292806));
#57205=CARTESIAN_POINT('Ctrl Pts',(0.225907023032041,2.32984196832012,5.67771299836074));
#57206=CARTESIAN_POINT('Ctrl Pts',(0.225642099081592,2.33010205687184,5.67773576272422));
#57207=CARTESIAN_POINT('Ctrl Pts',(0.225092591286237,2.33063967348047,5.67778294270911));
#57208=CARTESIAN_POINT('Ctrl Pts',(0.224807942317624,2.33091713384641,5.6778073612343));
#57209=CARTESIAN_POINT('Ctrl Pts',(0.22414105027979,2.331564782197,5.67786452169802));
#57210=CARTESIAN_POINT('Ctrl Pts',(0.223758403101919,2.33193455070415,5.67789728182263));
#57211=CARTESIAN_POINT('Ctrl Pts',(0.222523215724299,2.3331222639505,5.67800291356466));
#57212=CARTESIAN_POINT('Ctrl Pts',(0.221667100290692,2.33393646161901,5.67807594715105));
#57213=CARTESIAN_POINT('Ctrl Pts',(0.208875399421384,2.34596858172557,5.67916458227217));
#57214=CARTESIAN_POINT('Ctrl Pts',(0.196108035538481,2.35626346296337,5.68021959986638));
#57215=CARTESIAN_POINT('Ctrl Pts',(0.163663320877388,2.37857593095105,5.68282873056233));
#57216=CARTESIAN_POINT('Ctrl Pts',(0.143372160346033,2.38954194220059,5.68440759184431));
#57217=CARTESIAN_POINT('Ctrl Pts',(0.118369341016072,2.39977661305382,5.68620824855694));
#57218=CARTESIAN_POINT('Ctrl Pts',(0.114622699869233,2.40122907817368,5.6864742988123));
#57219=CARTESIAN_POINT('Ctrl Pts',(0.108358362013218,2.40352377324617,5.68691188641338));
#57220=CARTESIAN_POINT('Ctrl Pts',(0.105855718431158,2.40440562291175,5.68708481488433));
#57221=CARTESIAN_POINT('Ctrl Pts',(0.10309639820632,2.40533977099777,5.68727320542469));
#57222=CARTESIAN_POINT('Ctrl Pts',(0.102850298155727,2.40542275495817,5.68728998795915));
#57223=CARTESIAN_POINT('Ctrl Pts',(0.0985518700657273,2.40686638336472,
5.68758276666533));
#57224=CARTESIAN_POINT('Ctrl Pts',(0.0944727170032536,2.40814665092759,
5.68785521477102));
#57225=CARTESIAN_POINT('Ctrl Pts',(0.0898458584428837,2.40949829474201,
5.68815726206931));
#57226=CARTESIAN_POINT('Ctrl Pts',(0.0893222638756283,2.40964981174545,
5.68819134288011));
#57227=CARTESIAN_POINT('Ctrl Pts',(0.0885306261060259,2.409876719668,5.68824271681912));
#57228=CARTESIAN_POINT('Ctrl Pts',(0.0882628687613149,2.40995309185485,
5.68826006658954));
#57229=CARTESIAN_POINT('Ctrl Pts',(0.0877976794361183,2.41008512571158,
5.6882901627852));
#57230=CARTESIAN_POINT('Ctrl Pts',(0.0876002932395677,2.41014094590495,
5.68830291848679));
#57231=CARTESIAN_POINT('Ctrl Pts',(0.0871873081877042,2.41025731105677,
5.68832957627332));
#57232=CARTESIAN_POINT('Ctrl Pts',(0.0869716996354782,2.41031781972045,
5.68834347615774));
#57233=CARTESIAN_POINT('Ctrl Pts',(0.0864617969686547,2.4104603463013,5.68837630778164));
#57234=CARTESIAN_POINT('Ctrl Pts',(0.0861674479696204,2.41054217084451,
5.688395228182));
#57235=CARTESIAN_POINT('Ctrl Pts',(0.0852298445650234,2.41080137460705,
5.68845539518268));
#57236=CARTESIAN_POINT('Ctrl Pts',(0.0845861501278494,2.41097717615213,
5.68849655045149));
#57237=CARTESIAN_POINT('Ctrl Pts',(0.0770385627496673,2.41301335448509,
5.68897739244752));
#57238=CARTESIAN_POINT('Ctrl Pts',(0.0700745191519581,2.41464564256456,
5.68940421491959));
#57239=CARTESIAN_POINT('Ctrl Pts',(0.0504960057673272,2.41855219743501,
5.69057213112692));
#57240=CARTESIAN_POINT('Ctrl Pts',(0.0377913431119163,2.42030799737302,
5.69129370016153));
#57241=CARTESIAN_POINT('Ctrl Pts',(0.00197268669316696,2.42309666171127,
5.69330539212059));
#57242=CARTESIAN_POINT('Ctrl Pts',(-0.0211936361763739,2.42240669334756,
5.69458529650879));
#57243=CARTESIAN_POINT('Ctrl Pts',(-0.0515550368994546,2.41821392003696,
5.6963865526067));
#57244=CARTESIAN_POINT('Ctrl Pts',(-0.0589847213401951,2.41692082523618,
5.69683679066854));
#57245=CARTESIAN_POINT('Ctrl Pts',(-0.0673114676605211,2.41516865917588,
5.69735450050088));
#57246=CARTESIAN_POINT('Ctrl Pts',(-0.0682602083284834,2.41496453980095,
5.69741368029993));
#57247=CARTESIAN_POINT('Ctrl Pts',(-0.0696945380990065,2.4146491619938,
5.69750344635019));
#57248=CARTESIAN_POINT('Ctrl Pts',(-0.0701808208012834,2.41454105641631,
5.69753393153673));
#57249=CARTESIAN_POINT('Ctrl Pts',(-0.0710260278052374,2.41435110072193,
5.69758700842962));
#57250=CARTESIAN_POINT('Ctrl Pts',(-0.0713850670894342,2.41426976206071,
5.69760958368488));
#57251=CARTESIAN_POINT('Ctrl Pts',(-0.0721335860859953,2.41409883970402,
5.69765670795708));
#57252=CARTESIAN_POINT('Ctrl Pts',(-0.0725230399259975,2.41400914639972,
5.69768126046333));
#57253=CARTESIAN_POINT('Ctrl Pts',(-0.0734428991119554,2.41379549533252,
5.69773933187717));
#57254=CARTESIAN_POINT('Ctrl Pts',(-0.073973157767019,2.41367091711715,
5.69777287069511));
#57255=CARTESIAN_POINT('Ctrl Pts',(-0.0757201339037588,2.4132558088181,
5.69788357678611));
#57256=CARTESIAN_POINT('Ctrl Pts',(-0.0769354642836219,2.41295954163662,
5.69796092864064));
#57257=CARTESIAN_POINT('Ctrl Pts',(-0.0908184268523851,2.40948946824201,
5.69884844593346));
#57258=CARTESIAN_POINT('Ctrl Pts',(-0.103281950967356,2.40555601452187,
5.69968330975698));
#57259=CARTESIAN_POINT('Ctrl Pts',(-0.127037177113129,2.3964392077659,5.70135166033467));
#57260=CARTESIAN_POINT('Ctrl Pts',(-0.138336641184565,2.39133756838317,
5.70218156951798));
#57261=CARTESIAN_POINT('Ctrl Pts',(-0.159755809498103,2.38013942817263,
5.70381385362561));
#57262=CARTESIAN_POINT('Ctrl Pts',(-0.16989078355478,2.37411155634012,5.70461431947547));
#57263=CARTESIAN_POINT('Ctrl Pts',(-0.187894537828682,2.36202079688238,
5.70606813003992));
#57264=CARTESIAN_POINT('Ctrl Pts',(-0.195858016562943,2.35612287662011,
5.7067237176934));
#57265=CARTESIAN_POINT('Ctrl Pts',(-0.20616813639496,2.3477244125013,5.70757729963383));
#57266=CARTESIAN_POINT('Ctrl Pts',(-0.208764590572189,2.34554028793596,
5.70779268181104));
#57267=CARTESIAN_POINT('Ctrl Pts',(-0.211753026051544,2.34294474927109,
5.70804058857714));
#57268=CARTESIAN_POINT('Ctrl Pts',(-0.212178885652864,2.34257290808132,
5.70807591609431));
#57269=CARTESIAN_POINT('Ctrl Pts',(-0.212812969749657,2.34201630734162,
5.70812851435845));
#57270=CARTESIAN_POINT('Ctrl Pts',(-0.213021934032479,2.34183239802683,
5.70814584783501));
#57271=CARTESIAN_POINT('Ctrl Pts',(-0.213394757707541,2.34150341799366,
5.70817677215883));
#57272=CARTESIAN_POINT('Ctrl Pts',(-0.213558707444492,2.34135845126153,
5.7081903707374));
#57273=CARTESIAN_POINT('Ctrl Pts',(-0.213876001819698,2.34107731856288,
5.70821668733534));
#57274=CARTESIAN_POINT('Ctrl Pts',(-0.214029363411063,2.34094117389576,
5.70822940685426));
#57275=CARTESIAN_POINT('Ctrl Pts',(-0.214364328487292,2.34064324102714,
5.70825718764066));
#57276=CARTESIAN_POINT('Ctrl Pts',(-0.214545879185266,2.34048139326237,
5.70827224442213));
#57277=CARTESIAN_POINT('Ctrl Pts',(-0.215281099969483,2.33982446762575,
5.70833321877181));
#57278=CARTESIAN_POINT('Ctrl Pts',(-0.215833246773317,2.33932767681374,
5.70837900861677));
#57279=CARTESIAN_POINT('Ctrl Pts',(-0.223635443495532,2.33225873547486,
5.70902611064433));
#57280=CARTESIAN_POINT('Ctrl Pts',(-0.230585042190231,2.32536085141049,
5.70960329324905));
#57281=CARTESIAN_POINT('Ctrl Pts',(-0.24165130376895,2.31332805169386,5.71054599300962));
#57282=CARTESIAN_POINT('Ctrl Pts',(-0.24594370640364,2.30836484860853,5.71091830974663));
#57283=CARTESIAN_POINT('Ctrl Pts',(-0.265923845083845,2.28378388563311,
5.71270282061998));
#57284=CARTESIAN_POINT('Ctrl Pts',(-0.279432359874984,2.26251008316921,
5.71407907431262));
#57285=CARTESIAN_POINT('Ctrl Pts',(-0.29423414796575,2.23178842069122,5.7160702635909));
#57286=CARTESIAN_POINT('Ctrl Pts',(-0.297793879060483,2.22353422313462,
5.71660464149274));
#57287=CARTESIAN_POINT('Ctrl Pts',(-0.301367622035029,2.21419180520443,
5.71721298623936));
#57288=CARTESIAN_POINT('Ctrl Pts',(-0.30172682978468,2.21323926941554,5.71727504970301));
#57289=CARTESIAN_POINT('Ctrl Pts',(-0.302259309349847,2.21180673476348,
5.71736845030554));
#57290=CARTESIAN_POINT('Ctrl Pts',(-0.302435966416557,2.21132799396412,
5.71739967439195));
#57291=CARTESIAN_POINT('Ctrl Pts',(-0.302739182661009,2.2105002295976,5.71745368097865));
#57292=CARTESIAN_POINT('Ctrl Pts',(-0.302866277512642,2.21015140218419,
5.71747644558001));
#57293=CARTESIAN_POINT('Ctrl Pts',(-0.30312820201904,2.20942863781447,5.71752362565372));
#57294=CARTESIAN_POINT('Ctrl Pts',(-0.303262943118027,2.20905466960388,
5.71754804402917));
#57295=CARTESIAN_POINT('Ctrl Pts',(-0.303576432152048,2.20817952024651,
5.7176052034412));
#57296=CARTESIAN_POINT('Ctrl Pts',(-0.303754631016065,2.20767814490327,
5.71763796266186));
#57297=CARTESIAN_POINT('Ctrl Pts',(-0.304324470392052,2.2060621893944,5.71774358860175));
#57298=CARTESIAN_POINT('Ctrl Pts',(-0.304711220734981,2.20494590605264,
5.71781661726496));
#57299=CARTESIAN_POINT('Ctrl Pts',(-0.310290095914531,2.18855267073059,
5.71889007753343));
#57300=CARTESIAN_POINT('Ctrl Pts',(-0.3143330827811,2.1729115014575,5.71992871658828));
#57301=CARTESIAN_POINT('Ctrl Pts',(-0.320587101506358,2.13813140654909,
5.72226851870401));
#57302=CARTESIAN_POINT('Ctrl Pts',(-0.322289269816695,2.1189626625909,5.72357815247994));
#57303=CARTESIAN_POINT('Ctrl Pts',(-0.322274909898337,2.09975901240904,
5.72487103019784));
#57304=CARTESIAN_POINT('',(-0.322274982545603,2.10010606710754,5.97444230798123));
#57305=CARTESIAN_POINT('Ctrl Pts',(-0.322274909611437,2.09975862903993,
5.724871056008));
#57306=CARTESIAN_POINT('Ctrl Pts',(-0.322264020214785,2.085219268876,5.7258499121261));
#57307=CARTESIAN_POINT('Ctrl Pts',(-0.321269222642355,2.07069492405067,
5.7268157023856));
#57308=CARTESIAN_POINT('Ctrl Pts',(-0.319195443610201,2.05554779287244,
5.72777898760693));
#57309=CARTESIAN_POINT('Ctrl Pts',(-0.319091896698514,2.0548104942833,5.7278257642248));
#57310=CARTESIAN_POINT('Ctrl Pts',(-0.318928349001282,2.05367456073724,
5.7278976518244));
#57311=CARTESIAN_POINT('Ctrl Pts',(-0.318870154632419,2.05327567433946,
5.72792286117238));
#57312=CARTESIAN_POINT('Ctrl Pts',(-0.318772580783095,2.05261553877446,
5.72796452348555));
#57313=CARTESIAN_POINT('Ctrl Pts',(-0.31873362840297,2.05235422840359,5.72798100023831));
#57314=CARTESIAN_POINT('Ctrl Pts',(-0.318663139620769,2.05188531236647,
5.72801054013422));
#57315=CARTESIAN_POINT('Ctrl Pts',(-0.318631721622433,2.05167768946372,
5.72802360996504));
#57316=CARTESIAN_POINT('Ctrl Pts',(-0.318570404651505,2.05127514192537,
5.72804893144045));
#57317=CARTESIAN_POINT('Ctrl Pts',(-0.318540529715395,2.05108021419087,
5.72806118441127));
#57318=CARTESIAN_POINT('Ctrl Pts',(-0.318477770839417,2.05067322067429,
5.72808674964826));
#57319=CARTESIAN_POINT('Ctrl Pts',(-0.318444854103606,2.05046116096334,
5.72810005998056));
#57320=CARTESIAN_POINT('Ctrl Pts',(-0.318363327599387,2.0499393812093,5.72813278580853));
#57321=CARTESIAN_POINT('Ctrl Pts',(-0.318314477530252,2.04962969813026,
5.7281521876118));
#57322=CARTESIAN_POINT('Ctrl Pts',(-0.318122668337188,2.04842515414412,
5.72822757134989));
#57323=CARTESIAN_POINT('Ctrl Pts',(-0.317976385209643,2.047530815421,5.72828336638451));
#57324=CARTESIAN_POINT('Ctrl Pts',(-0.315432598807844,2.03238017349651,
5.72922577782891));
#57325=CARTESIAN_POINT('Ctrl Pts',(-0.312081916676324,2.01829833798893,
5.73006006792826));
#57326=CARTESIAN_POINT('Ctrl Pts',(-0.306976563440437,2.00184596680618,
5.73103477195394));
#57327=CARTESIAN_POINT('Ctrl Pts',(-0.306122915064667,1.99921515026202,
5.73119061816042));
#57328=CARTESIAN_POINT('Ctrl Pts',(-0.304541249977357,1.99454629253937,
5.7314676554991));
#57329=CARTESIAN_POINT('Ctrl Pts',(-0.303826375874321,1.99250399645486,
5.7315889983304));
#57330=CARTESIAN_POINT('Ctrl Pts',(-0.301630030894537,1.98642633230106,
5.73195095261844));
#57331=CARTESIAN_POINT('Ctrl Pts',(-0.300088333785187,1.98241324180227,
5.73219108413579));
#57332=CARTESIAN_POINT('Ctrl Pts',(-0.295022319998671,1.96997543517858,
5.73294180271045));
#57333=CARTESIAN_POINT('Ctrl Pts',(-0.291220029513777,1.96166907638582,
5.73345270318302));
#57334=CARTESIAN_POINT('Ctrl Pts',(-0.27997183669563,1.93962261910464,5.73485597204474));
#57335=CARTESIAN_POINT('Ctrl Pts',(-0.271872288473323,1.92624587230503,
5.73576052391397));
#57336=CARTESIAN_POINT('Ctrl Pts',(-0.261408150838758,1.911497902633,5.73685120325654));
#57337=CARTESIAN_POINT('Ctrl Pts',(-0.259957515463289,1.9095023578399,5.73700086137625));
#57338=CARTESIAN_POINT('Ctrl Pts',(-0.258060482504202,1.90695475611422,
5.73719469596328));
#57339=CARTESIAN_POINT('Ctrl Pts',(-0.257634947752474,1.90638720987205,
5.73723805739455));
#57340=CARTESIAN_POINT('Ctrl Pts',(-0.256945809489131,1.90547438391682,
5.73730809102925));
#57341=CARTESIAN_POINT('Ctrl Pts',(-0.256683373954672,1.90512822200512,
5.73733471733814));
#57342=CARTESIAN_POINT('Ctrl Pts',(-0.256181905454801,1.90446953753993,
5.73738551304584));
#57343=CARTESIAN_POINT('Ctrl Pts',(-0.25594299829978,1.90415691982754,5.73740967745715));
#57344=CARTESIAN_POINT('Ctrl Pts',(-0.255396596907795,1.90344464343799,
5.73746486335632));
#57345=CARTESIAN_POINT('Ctrl Pts',(-0.255088736498328,1.90304526811376,
5.737495899293));
#57346=CARTESIAN_POINT('Ctrl Pts',(-0.254145495548868,1.90182755969468,
5.73759081479355));
#57347=CARTESIAN_POINT('Ctrl Pts',(-0.253507109766786,1.90101157254281,
5.73765481359475));
#57348=CARTESIAN_POINT('Ctrl Pts',(-0.248794707925047,1.89504764492045,
5.73812550881994));
#57349=CARTESIAN_POINT('Ctrl Pts',(-0.244568429261714,1.89002250660112,
5.73853829834352));
#57350=CARTESIAN_POINT('Ctrl Pts',(-0.239852900918646,1.88475126002786,
5.73898964479482));
#57351=CARTESIAN_POINT('Ctrl Pts',(-0.239513013314509,1.88437312183531,
5.73902212719018));
#57352=CARTESIAN_POINT('Ctrl Pts',(-0.222452284321282,1.8654825053648,5.7406500978203));
#57353=CARTESIAN_POINT('Ctrl Pts',(-0.203641755261037,1.84897588595725,
5.74233559596896));
#57354=CARTESIAN_POINT('Ctrl Pts',(-0.177549458293191,1.83095872620241,
5.74447972759449));
#57355=CARTESIAN_POINT('Ctrl Pts',(-0.171858026096936,1.82728798940623,
5.74493644773138));
#57356=CARTESIAN_POINT('Ctrl Pts',(-0.15969252041563,1.81997394975125,5.74588490190476));
#57357=CARTESIAN_POINT('Ctrl Pts',(-0.153199251541654,1.81636944053919,
5.74637550297007));
#57358=CARTESIAN_POINT('Ctrl Pts',(-0.142437215140867,1.81087281898544,
5.7471572673649));
#57359=CARTESIAN_POINT('Ctrl Pts',(-0.138241813160883,1.80884352349147,
5.7474545593267));
#57360=CARTESIAN_POINT('Ctrl Pts',(-0.133494983877891,1.80667325780593,
5.74778144830025));
#57361=CARTESIAN_POINT('Ctrl Pts',(-0.132985745640435,1.80644203319553,
5.74781639612182));
#57362=CARTESIAN_POINT('Ctrl Pts',(-0.132272460729269,1.80612039614442,
5.74786517582073));
#57363=CARTESIAN_POINT('Ctrl Pts',(-0.132068921944593,1.80602886997733,
5.74787907582819));
#57364=CARTESIAN_POINT('Ctrl Pts',(-0.131660609538261,1.80584577202053,
5.74790692088508));
#57365=CARTESIAN_POINT('Ctrl Pts',(-0.131455834728225,1.80575420230832,
5.74792086581216));
#57366=CARTESIAN_POINT('Ctrl Pts',(-0.131064006674325,1.80557947815676,
5.74794751079608));
#57367=CARTESIAN_POINT('Ctrl Pts',(-0.130876970049189,1.80549628824191,
5.74796021306663));
#57368=CARTESIAN_POINT('Ctrl Pts',(-0.130436870970177,1.80530104358354,
5.74799006303583));
#57369=CARTESIAN_POINT('Ctrl Pts',(-0.130183742689964,1.80518913628904,
5.74800720161665));
#57370=CARTESIAN_POINT('Ctrl Pts',(-0.129437617781264,1.80486042492366,
5.74805763217225));
#57371=CARTESIAN_POINT('Ctrl Pts',(-0.128944218399221,1.80464452904267,
5.74809086874667));
#57372=CARTESIAN_POINT('Ctrl Pts',(-0.124692690825109,1.8027968799296,5.74837631593897));
#57373=CARTESIAN_POINT('Ctrl Pts',(-0.120904092192029,1.80123560112782,
5.74862432923978));
#57374=CARTESIAN_POINT('Ctrl Pts',(-0.116712896374063,1.79960120459046,
5.74889286326565));
#57375=CARTESIAN_POINT('Ctrl Pts',(-0.116338980714718,1.79945619614954,
5.74891676987989));
#57376=CARTESIAN_POINT('Ctrl Pts',(-0.107420720490024,1.79601673793573,
5.74948578492848));
#57377=CARTESIAN_POINT('Ctrl Pts',(-0.0987393731918041,1.79308698671092,
5.75001391482371));
#57378=CARTESIAN_POINT('Ctrl Pts',(-0.0731892849765471,1.78566108793362,
5.75152548454611));
#57379=CARTESIAN_POINT('Ctrl Pts',(-0.0560661024676764,1.78216002814846,
5.75248713534905));
#57380=CARTESIAN_POINT('Ctrl Pts',(-0.0361929644712237,1.77975346287182,
5.75361603242056));
#57381=CARTESIAN_POINT('Ctrl Pts',(-0.0336390536165905,1.7794751350974,
5.7537613102101));
#57382=CARTESIAN_POINT('Ctrl Pts',(-0.0278258770146788,1.7789118519331,
5.75409280333765));
#57383=CARTESIAN_POINT('Ctrl Pts',(-0.0245650802082596,1.77864593609912,
5.75427932937292));
#57384=CARTESIAN_POINT('Ctrl Pts',(-0.0089746082849849,1.77761322139547,
5.75517531778487));
#57385=CARTESIAN_POINT('Ctrl Pts',(0.00338707621833142,1.77750619676307,
5.75589873554261));
#57386=CARTESIAN_POINT('Ctrl Pts',(0.0178607208586101,1.77821319323672,
5.75677439859087));
#57387=CARTESIAN_POINT('Ctrl Pts',(0.0199968357020707,1.77833887307228,
5.75690435203885));
#57388=CARTESIAN_POINT('Ctrl Pts',(0.0228031314669913,1.77853204507372,
5.75707607027264));
#57389=CARTESIAN_POINT('Ctrl Pts',(0.0234746108622119,1.77858038099205,
5.75711723314175));
#57390=CARTESIAN_POINT('Ctrl Pts',(0.0245710600039138,1.77866276220894,
5.75718457131871));
#57391=CARTESIAN_POINT('Ctrl Pts',(0.0249961246925882,1.77869554760556,
5.75721070700293));
#57392=CARTESIAN_POINT('Ctrl Pts',(0.0258156727782518,1.77876039579559,
5.75726115721789));
#57393=CARTESIAN_POINT('Ctrl Pts',(0.026210164840199,1.77879234204766,5.75728546804184));
#57394=CARTESIAN_POINT('Ctrl Pts',(0.0271152304769176,1.77886731334499,
5.75734130444039));
#57395=CARTESIAN_POINT('Ctrl Pts',(0.0276257613239366,1.77891082941257,
5.75737284539908));
#57396=CARTESIAN_POINT('Ctrl Pts',(0.0289823249762215,1.77902971801466,
5.75745677468915));
#57397=CARTESIAN_POINT('Ctrl Pts',(0.0298281630306431,1.77910721767719,
5.75750922980785));
#57398=CARTESIAN_POINT('Ctrl Pts',(0.0355108900033,1.77965055823793,5.75786249190126));
#57399=CARTESIAN_POINT('Ctrl Pts',(0.0403367945243799,1.78022237883874,
5.75816661937243));
#57400=CARTESIAN_POINT('Ctrl Pts',(0.0467085879788301,1.78112389788232,
5.75857393098527));
#57401=CARTESIAN_POINT('Ctrl Pts',(0.0482677884194959,1.78135618450388,
5.75867405959665));
#57402=CARTESIAN_POINT('Ctrl Pts',(0.0719039902823701,1.78505492229719,
5.76019893461121));
#57403=CARTESIAN_POINT('Ctrl Pts',(0.0935600316628738,1.79079651517814,
5.76169542593593));
#57404=CARTESIAN_POINT('Ctrl Pts',(0.127061324020658,1.80352276349304,5.76412026410933));
#57405=CARTESIAN_POINT('Ctrl Pts',(0.13936521000401,1.80910362186993,5.76503510033277));
#57406=CARTESIAN_POINT('Ctrl Pts',(0.155727752179207,1.81780258964203,5.76625869693939));
#57407=CARTESIAN_POINT('Ctrl Pts',(0.160116439268343,1.82026933903393,5.76658753318001));
#57408=CARTESIAN_POINT('Ctrl Pts',(0.166592007020732,1.82411142333808,5.76707180206359));
#57409=CARTESIAN_POINT('Ctrl Pts',(0.168723458823988,1.8254097619282,5.76723104332797));
#57410=CARTESIAN_POINT('Ctrl Pts',(0.171668649034083,1.8272510195755,5.76745062920414));
#57411=CARTESIAN_POINT('Ctrl Pts',(0.172495261860654,1.82777304307551,5.76751220932676));
#57412=CARTESIAN_POINT('Ctrl Pts',(0.173918737159818,1.82868108488885,5.76761814977272));
#57413=CARTESIAN_POINT('Ctrl Pts',(0.174516716215791,1.82906532776999,5.76766262169365));
#57414=CARTESIAN_POINT('Ctrl Pts',(0.175369504301298,1.82961729782662,5.76772599249199));
#57415=CARTESIAN_POINT('Ctrl Pts',(0.175625348563394,1.82978340980375,5.7677449976804));
#57416=CARTESIAN_POINT('Ctrl Pts',(0.176068531828038,1.83007205066311,5.76777790714728));
#57417=CARTESIAN_POINT('Ctrl Pts',(0.176255979434251,1.83019441175523,5.76779182269803));
#57418=CARTESIAN_POINT('Ctrl Pts',(0.176615038472122,1.83042933036116,5.76781847075867));
#57419=CARTESIAN_POINT('Ctrl Pts',(0.176786669606336,1.83054185632248,5.76783120536785));
#57420=CARTESIAN_POINT('Ctrl Pts',(0.177191235769833,1.83080765363453,5.76786121585116));
#57421=CARTESIAN_POINT('Ctrl Pts',(0.177424080046902,1.83096106379139,5.76787848236141));
#57422=CARTESIAN_POINT('Ctrl Pts',(0.178112808169605,1.8314161173708,5.76792953873331));
#57423=CARTESIAN_POINT('Ctrl Pts',(0.178568126892339,1.83171862064108,5.76796327123243));
#57424=CARTESIAN_POINT('Ctrl Pts',(0.182613911540048,1.83442140955377,5.76826283957173));
#57425=CARTESIAN_POINT('Ctrl Pts',(0.186156770692396,1.83689262732509,5.76852400698594));
#57426=CARTESIAN_POINT('Ctrl Pts',(0.189832962423795,1.8395682935528,5.76879498156927));
#57427=CARTESIAN_POINT('Ctrl Pts',(0.19001669596465,1.83970231925575,5.76880852463292));
#57428=CARTESIAN_POINT('Ctrl Pts',(0.190331989504498,1.8399328240392,5.76883176521534));
#57429=CARTESIAN_POINT('Ctrl Pts',(0.190463618150189,1.84002920855929,5.76884146774175));
#57430=CARTESIAN_POINT('Ctrl Pts',(0.192557291080573,1.84156473533348,5.76899579708992));
#57431=CARTESIAN_POINT('Ctrl Pts',(0.194503099910967,1.84302599135101,5.76913925340138));
#57432=CARTESIAN_POINT('Ctrl Pts',(0.199620658817928,1.84696058861459,5.76951716220704));
#57433=CARTESIAN_POINT('Ctrl Pts',(0.202763038178625,1.84947155110292,5.76974985090437));
#57434=CARTESIAN_POINT('Ctrl Pts',(0.225789296172022,1.86858813005397,5.77146645239087));
#57435=CARTESIAN_POINT('Ctrl Pts',(0.243653415116403,1.88747846755907,5.77287144592799));
#57436=CARTESIAN_POINT('Ctrl Pts',(0.262432066876406,1.91285660377111,5.77468258066731));
#57437=CARTESIAN_POINT('Ctrl Pts',(0.265679589454469,1.9174963246509,5.77501058313047));
#57438=CARTESIAN_POINT('Ctrl Pts',(0.272842445818083,1.92832649312977,5.77577214957779));
#57439=CARTESIAN_POINT('Ctrl Pts',(0.276672215041648,1.93456945252373,5.77620826617175));
#57440=CARTESIAN_POINT('Ctrl Pts',(0.281053451903209,1.94228965952567,5.77674659322142));
#57441=CARTESIAN_POINT('Ctrl Pts',(0.281811236515871,1.94364776573232,5.77684125427333));
#57442=CARTESIAN_POINT('Ctrl Pts',(0.282845231187349,1.94553283625092,5.77697261062435));
#57443=CARTESIAN_POINT('Ctrl Pts',(0.283129865036585,1.9460551754719,5.77700900484827));
#57444=CARTESIAN_POINT('Ctrl Pts',(0.283607932464402,1.94693830051208,5.77707053202901));
#57445=CARTESIAN_POINT('Ctrl Pts',(0.283802128513008,1.94729867369306,5.77709563778086));
#57446=CARTESIAN_POINT('Ctrl Pts',(0.284185069719855,1.9480125585161,5.77714536895957));
#57447=CARTESIAN_POINT('Ctrl Pts',(0.284373843201527,1.94836605419304,5.77716999332281));
#57448=CARTESIAN_POINT('Ctrl Pts',(0.284788501857637,1.94914603832949,5.77722432467714));
#57449=CARTESIAN_POINT('Ctrl Pts',(0.285014089031827,1.94957268336064,5.77725404216285));
#57450=CARTESIAN_POINT('Ctrl Pts',(0.28579906497395,1.95106538521777,5.77735801118651));
#57451=CARTESIAN_POINT('Ctrl Pts',(0.286353432503831,1.95213405851747,5.77743243983861));
#57452=CARTESIAN_POINT('Ctrl Pts',(0.29216026547678,1.96348321814778,5.77822284688498));
#57453=CARTESIAN_POINT('Ctrl Pts',(0.296862095679574,1.97403455187322,5.77895803127679));
#57454=CARTESIAN_POINT('Ctrl Pts',(0.301797820013975,1.98693191307256,5.77985828991696));
#57455=CARTESIAN_POINT('Ctrl Pts',(0.30258581472433,1.989057939372,5.78000672355907));
#57456=CARTESIAN_POINT('Ctrl Pts',(0.306168918568508,1.99904746098387,5.78070423647146));
#57457=CARTESIAN_POINT('Ctrl Pts',(0.308680197622661,2.00700890725271,5.78126045979066));
#57458=CARTESIAN_POINT('Ctrl Pts',(0.315345814615061,2.03140455036122,5.78296014253687));
#57459=CARTESIAN_POINT('Ctrl Pts',(0.318515844734172,2.0480772342913,5.78411679298052));
#57460=CARTESIAN_POINT('Ctrl Pts',(0.321480516982876,2.0751528316532,5.78593347850045));
#57461=CARTESIAN_POINT('Ctrl Pts',(0.322110149726099,2.08543283351798,5.7866087320004));
#57462=CARTESIAN_POINT('Ctrl Pts',(0.322259612980905,2.0967028530805,5.78732127092103));
#57463=CARTESIAN_POINT('Ctrl Pts',(0.322268124840648,2.09767941712541,5.78738278437888));
#57464=CARTESIAN_POINT('Ctrl Pts',(0.322275158787201,2.09936608214417,5.78748861377938));
#57465=CARTESIAN_POINT('Ctrl Pts',(0.322275773283339,2.1000761609614,5.78753304106816));
#57466=CARTESIAN_POINT('Ctrl Pts',(0.32227329686296,2.10109122249819,5.78759636378561));
#57467=CARTESIAN_POINT('Ctrl Pts',(0.322272119894244,2.1013962013366,5.78761536527523));
#57468=CARTESIAN_POINT('Ctrl Pts',(0.322269328447923,2.10192501137883,5.78764827017607));
#57469=CARTESIAN_POINT('Ctrl Pts',(0.322267913701746,2.10214884307118,5.78766218485182));
#57470=CARTESIAN_POINT('Ctrl Pts',(0.32226475467842,2.10257791442516,5.78768883303995));
#57471=CARTESIAN_POINT('Ctrl Pts',(0.322263047536509,2.102783153571,5.78770156864816));
#57472=CARTESIAN_POINT('Ctrl Pts',(0.32225855812668,2.10326728099141,5.78773158406687));
#57473=CARTESIAN_POINT('Ctrl Pts',(0.322255609887789,2.10354616809737,5.78774885450597));
#57474=CARTESIAN_POINT('Ctrl Pts',(0.322245808608929,2.1043719044401,5.78779993014431));
#57475=CARTESIAN_POINT('Ctrl Pts',(0.322237925581,2.10491874395003,5.78783367792004));
#57476=CARTESIAN_POINT('Ctrl Pts',(0.322155284597172,2.10979093748329,5.78813369825474));
#57477=CARTESIAN_POINT('Ctrl Pts',(0.321994830511464,2.11411465318918,5.78839528687277));
#57478=CARTESIAN_POINT('Ctrl Pts',(0.321744450091459,2.11848477858142,5.78865614477654));
#57479=CARTESIAN_POINT('Ctrl Pts',(0.321741533357088,2.11853547725027,5.78865917055703));
#57480=CARTESIAN_POINT('Ctrl Pts',(0.321675956172566,2.11967066033943,5.7887269094025));
#57481=CARTESIAN_POINT('Ctrl Pts',(0.321607824100771,2.12075483544003,5.78879138459255));
#57482=CARTESIAN_POINT('Ctrl Pts',(0.319592037439303,2.15043359813829,5.79055083800215));
#57483=CARTESIAN_POINT('Ctrl Pts',(0.313843979427069,2.17864470165379,5.79209291094241));
#57484=CARTESIAN_POINT('Ctrl Pts',(0.299036769110684,2.22128215275347,5.79465792259777));
#57485=CARTESIAN_POINT('Ctrl Pts',(0.292450916738611,2.23639902505667,5.79561639975298));
#57486=CARTESIAN_POINT('Ctrl Pts',(0.28418397398593,2.25199359293855,5.79668944121871));
#57487=CARTESIAN_POINT('Ctrl Pts',(0.283622477448984,2.25303879766774,5.79676177512135));
#57488=CARTESIAN_POINT('Ctrl Pts',(0.282800378582326,2.25454903957084,5.79686690375821));
#57489=CARTESIAN_POINT('Ctrl Pts',(0.282544369400296,2.25501657676963,5.79689953466767));
#57490=CARTESIAN_POINT('Ctrl Pts',(0.282095350755949,2.25583179020305,5.79695658125485));
#57491=CARTESIAN_POINT('Ctrl Pts',(0.281902855005901,2.25617974930586,5.79698097851482));
#57492=CARTESIAN_POINT('Ctrl Pts',(0.281529518718597,2.25685166037853,5.79702818294984));
#57493=CARTESIAN_POINT('Ctrl Pts',(0.281348761713098,2.25717565827489,5.79705098710138));
#57494=CARTESIAN_POINT('Ctrl Pts',(0.280918528383279,2.25794370977834,5.79710514550435));
#57495=CARTESIAN_POINT('Ctrl Pts',(0.28066855860949,2.25838748451468,5.79713651746574));
#57496=CARTESIAN_POINT('Ctrl Pts',(0.279784449916111,2.25994838956708,5.79724714536905));
#57497=CARTESIAN_POINT('Ctrl Pts',(0.279144691188368,2.26106230795778,5.79732660377483));
#57498=CARTESIAN_POINT('Ctrl Pts',(0.269354828356038,2.27787442160478,5.79853369159408));
#57499=CARTESIAN_POINT('Ctrl Pts',(0.258901495141235,2.29277226205717,5.7997101645988));
#57500=CARTESIAN_POINT('Ctrl Pts',(0.232144611744198,2.32477706708822,5.80248977170565));
#57501=CARTESIAN_POINT('Ctrl Pts',(0.215104426518439,2.34113455490837,5.80411004221691));
#57502=CARTESIAN_POINT('Ctrl Pts',(0.190243796952678,2.36024883379797,5.80618075224492));
#57503=CARTESIAN_POINT('Ctrl Pts',(0.183881431769681,2.36478255149144,5.80668791401487));
#57504=CARTESIAN_POINT('Ctrl Pts',(0.176664087766309,2.36953973833608,5.80723328033171));
#57505=CARTESIAN_POINT('Ctrl Pts',(0.175966326557108,2.36999578219339,5.80728570426058));
#57506=CARTESIAN_POINT('Ctrl Pts',(0.174899792244733,2.37068695860006,5.80736536704225));
#57507=CARTESIAN_POINT('Ctrl Pts',(0.17453230328793,2.37092405208418,5.80739273172469));
#57508=CARTESIAN_POINT('Ctrl Pts',(0.173852631104433,2.37136060053063,5.80744318576719));
#57509=CARTESIAN_POINT('Ctrl Pts',(0.173540585064222,2.37156026624145,5.80746628892765));
#57510=CARTESIAN_POINT('Ctrl Pts',(0.17303052537325,2.37188539472137,5.80750395228057));
#57511=CARTESIAN_POINT('Ctrl Pts',(0.172832718999569,2.37201117958238,5.8075185339523));
#57512=CARTESIAN_POINT('Ctrl Pts',(0.172448269763176,2.37225506177614,5.80754682640895));
#57513=CARTESIAN_POINT('Ctrl Pts',(0.17226164327628,2.37237318271634,5.80756053872138));
#57514=CARTESIAN_POINT('Ctrl Pts',(0.171830691427337,2.37264532368112,5.80759215244075));
#57515=CARTESIAN_POINT('Ctrl Pts',(0.171586279576572,2.37279920766786,5.80761004474133));
#57516=CARTESIAN_POINT('Ctrl Pts',(0.170803708464042,2.37329045396174,5.80766721535858));
#57517=CARTESIAN_POINT('Ctrl Pts',(0.17026475434948,2.37362655663183,5.80770641046022));
#57518=CARTESIAN_POINT('Ctrl Pts',(0.165407627397522,2.37663565180014,5.80805807585713));
#57519=CARTESIAN_POINT('Ctrl Pts',(0.161027535321424,2.37920799945013,5.80836409484753));
#57520=CARTESIAN_POINT('Ctrl Pts',(0.156401960934109,2.38177943082283,5.80867781143872));
#57521=CARTESIAN_POINT('Ctrl Pts',(0.156215639853434,2.38188276798077,5.80869043238856));
#57522=CARTESIAN_POINT('Ctrl Pts',(0.155336867165052,2.38236901287315,5.80874988480085));
#57523=CARTESIAN_POINT('Ctrl Pts',(0.154643103782922,2.38274955739266,5.80879660545504));
#57524=CARTESIAN_POINT('Ctrl Pts',(0.151923850567915,2.38422812574864,5.80897891784714));
#57525=CARTESIAN_POINT('Ctrl Pts',(0.14988797096674,2.38530699339266,5.80911365639485));
#57526=CARTESIAN_POINT('Ctrl Pts',(0.12098121698274,2.40023063584287,5.8110045253961));
#57527=CARTESIAN_POINT('Ctrl Pts',(0.0923034097621147,2.41025036243928,
5.81262513990115));
#57528=CARTESIAN_POINT('Ctrl Pts',(0.0519879773275619,2.41823969953699,
5.81499633121213));
#57529=CARTESIAN_POINT('Ctrl Pts',(0.0412297780674123,2.41981138772159,
5.81563587608256));
#57530=CARTESIAN_POINT('Ctrl Pts',(0.0284451823997788,2.4210232957224,5.81641264057607));
#57531=CARTESIAN_POINT('Ctrl Pts',(0.0264752030585762,2.42119176227135,
5.81653278789971));
#57532=CARTESIAN_POINT('Ctrl Pts',(0.0238523243728455,2.42139176899382,
5.81669340008371));
#57533=CARTESIAN_POINT('Ctrl Pts',(0.0232006712699923,2.42143946770376,
5.81673335699306));
#57534=CARTESIAN_POINT('Ctrl Pts',(0.0221279762260744,2.42151470623572,
5.81679921918326));
#57535=CARTESIAN_POINT('Ctrl Pts',(0.0217070150997383,2.42154340165906,
5.81682508813054));
#57536=CARTESIAN_POINT('Ctrl Pts',(0.0208893446200458,2.42159752631441,
5.81687537974956));
#57537=CARTESIAN_POINT('Ctrl Pts',(0.0204926420069347,2.42162304841464,
5.81689979945853));
#57538=CARTESIAN_POINT('Ctrl Pts',(0.0195738867001377,2.42168045035464,
5.81695640207538));
#57539=CARTESIAN_POINT('Ctrl Pts',(0.0190518026564808,2.42171179336684,
5.81698860177151));
#57540=CARTESIAN_POINT('Ctrl Pts',(0.0176455946837466,2.42179277921376,
5.81707542595115));
#57541=CARTESIAN_POINT('Ctrl Pts',(0.0167613433665243,2.42184004895187,
5.8171301247436));
#57542=CARTESIAN_POINT('Ctrl Pts',(0.0103496192081794,2.42215630731137,
5.81752750017183));
#57543=CARTESIAN_POINT('Ctrl Pts',(0.00481651662403091,2.42228651226943,
5.81787450419063));
#57544=CARTESIAN_POINT('Ctrl Pts',(-0.0324581831251064,2.42220359095218,
5.82024159450783));
#57545=CARTESIAN_POINT('Ctrl Pts',(-0.0640106748623482,2.41744366170526,
5.82241406808191));
#57546=CARTESIAN_POINT('Ctrl Pts',(-0.107201007305519,2.40421996711594,
5.82544508123735));
#57547=CARTESIAN_POINT('Ctrl Pts',(-0.119796447190444,2.39948414250967,
5.82633258724156));
#57548=CARTESIAN_POINT('Ctrl Pts',(-0.132741382378724,2.39366895970823,
5.82722330863282));
#57549=CARTESIAN_POINT('Ctrl Pts',(-0.133421031590975,2.39336080318858,
5.82727000871046));
#57550=CARTESIAN_POINT('Ctrl Pts',(-0.134383195337325,2.3929205177089,5.82733602140956));
#57551=CARTESIAN_POINT('Ctrl Pts',(-0.134666591300461,2.39279033808068,
5.82735545252891));
#57552=CARTESIAN_POINT('Ctrl Pts',(-0.135153171401869,2.39256596869687,
5.82738879334182));
#57553=CARTESIAN_POINT('Ctrl Pts',(-0.135356446763625,2.39247197831617,
5.8274027153992));
#57554=CARTESIAN_POINT('Ctrl Pts',(-0.135745706610365,2.3922914997595,5.82742936257808));
#57555=CARTESIAN_POINT('Ctrl Pts',(-0.135931706222862,2.39220504605283,
5.8274420898246));
#57556=CARTESIAN_POINT('Ctrl Pts',(-0.136369942710466,2.39200084218755,
5.82747206389522));
#57557=CARTESIAN_POINT('Ctrl Pts',(-0.136622110292285,2.39188294245079,
5.8274893014111));
#57558=CARTESIAN_POINT('Ctrl Pts',(-0.137367354364829,2.39153332981585,
5.82754021568627));
#57559=CARTESIAN_POINT('Ctrl Pts',(-0.137859999542672,2.39130069168305,
5.82757383553164));
#57560=CARTESIAN_POINT('Ctrl Pts',(-0.14220612006825,2.38923486106908,5.82787012221538));
#57561=CARTESIAN_POINT('Ctrl Pts',(-0.14602364610149,2.38732644241518,5.82812823243293));
#57562=CARTESIAN_POINT('Ctrl Pts',(-0.150605634383394,2.38492093922282,
5.82843676202643));
#57563=CARTESIAN_POINT('Ctrl Pts',(-0.151407132993402,2.38449583271017,
5.82849068343335));
#57564=CARTESIAN_POINT('Ctrl Pts',(-0.152306920463536,2.38401371533267,
5.82855117543504));
#57565=CARTESIAN_POINT('Ctrl Pts',(-0.152406978451895,2.38396003492989,
5.82855790167054));
#57566=CARTESIAN_POINT('Ctrl Pts',(-0.152746443308193,2.38377768332541,
5.82858071973117));
#57567=CARTESIAN_POINT('Ctrl Pts',(-0.152985716365899,2.38364876182674,
5.8285967998963));
#57568=CARTESIAN_POINT('Ctrl Pts',(-0.154159151280926,2.38301459261448,
5.8286756452471));
#57569=CARTESIAN_POINT('Ctrl Pts',(-0.155090984649795,2.38250502665968,
5.82873821192304));
#57570=CARTESIAN_POINT('Ctrl Pts',(-0.16133909018262,2.37904806617456,5.82915754318643));
#57571=CARTESIAN_POINT('Ctrl Pts',(-0.166573837786884,2.37595523042498,
5.82950795214966));
#57572=CARTESIAN_POINT('Ctrl Pts',(-0.182698062355121,2.36580246082704,
5.8305941161091));
#57573=CARTESIAN_POINT('Ctrl Pts',(-0.193250753000684,2.35823187385438,
5.83131544589907));
#57574=CARTESIAN_POINT('Ctrl Pts',(-0.214556289678984,2.34090777790732,
5.83285156777277));
#57575=CARTESIAN_POINT('Ctrl Pts',(-0.225164608822422,2.33102340738084,
5.83366603698555));
#57576=CARTESIAN_POINT('Ctrl Pts',(-0.240957268727839,2.3141840227594,5.83500588071417));
#57577=CARTESIAN_POINT('Ctrl Pts',(-0.246588786853342,2.30767559288076,
5.83551362870343));
#57578=CARTESIAN_POINT('Ctrl Pts',(-0.253554251096458,2.29894223581908,
5.83618701341247));
#57579=CARTESIAN_POINT('Ctrl Pts',(-0.255131541249635,2.29691538160539,
5.83634275524099));
#57580=CARTESIAN_POINT('Ctrl Pts',(-0.257119550015415,2.29429675887561,
5.83654337128035));
#57581=CARTESIAN_POINT('Ctrl Pts',(-0.257552771892464,2.29372212880045,
5.83658735807068));
#57582=CARTESIAN_POINT('Ctrl Pts',(-0.258245785832869,2.29279647411495,
5.83665815889976));
#57583=CARTESIAN_POINT('Ctrl Pts',(-0.258506797096817,2.29244636183457,
5.83668492519471));
#57584=CARTESIAN_POINT('Ctrl Pts',(-0.259001320849695,2.2917802018914,5.83673582966921));
#57585=CARTESIAN_POINT('Ctrl Pts',(-0.259234968672806,2.29146425529176,
5.83675996251163));
#57586=CARTESIAN_POINT('Ctrl Pts',(-0.25976463716848,2.29074527246748,5.83681485772809));
#57587=CARTESIAN_POINT('Ctrl Pts',(-0.260060298267402,2.29034197370139,
5.83684563399438));
#57588=CARTESIAN_POINT('Ctrl Pts',(-0.260933612543216,2.28914488956945,
5.83693693860547));
#57589=CARTESIAN_POINT('Ctrl Pts',(-0.261508574736918,2.28834915638252,
5.83699757084551));
#57590=CARTESIAN_POINT('Ctrl Pts',(-0.265410423022274,2.28289678895216,
5.83741263047262));
#57591=CARTESIAN_POINT('Ctrl Pts',(-0.26861621239145,2.27815513384584,5.83777166713408));
#57592=CARTESIAN_POINT('Ctrl Pts',(-0.272655307532565,2.27182390450379,
5.83824900997595));
#57593=CARTESIAN_POINT('Ctrl Pts',(-0.273604133659034,2.27030898017297,
5.83836307488627));
#57594=CARTESIAN_POINT('Ctrl Pts',(-0.287692186786489,2.2473939743284,5.84008619600989));
#57595=CARTESIAN_POINT('Ctrl Pts',(-0.298296778850963,2.22454078346523,
5.84178554796992));
#57596=CARTESIAN_POINT('Ctrl Pts',(-0.311798248017079,2.18349214116606,
5.84470636232775));
#57597=CARTESIAN_POINT('Ctrl Pts',(-0.315997054805826,2.16584168270886,
5.84592088773631));
#57598=CARTESIAN_POINT('Ctrl Pts',(-0.3187961248048,2.14723035896621,5.84710166407308));
#57599=CARTESIAN_POINT('Ctrl Pts',(-0.318899025334597,2.14653050248745,
5.84714591882361));
#57600=CARTESIAN_POINT('Ctrl Pts',(-0.319043014388169,2.14552827364399,
5.84720907806441));
#57601=CARTESIAN_POINT('Ctrl Pts',(-0.319085978136598,2.1452261792477,5.84722808765476));
#57602=CARTESIAN_POINT('Ctrl Pts',(-0.319159560840155,2.14470346695913,
5.8472609308248));
#57603=CARTESIAN_POINT('Ctrl Pts',(-0.319190380198436,2.1444828778724,5.84727477582552));
#57604=CARTESIAN_POINT('Ctrl Pts',(-0.319249355064044,2.14405754903072,
5.84730144175229));
#57605=CARTESIAN_POINT('Ctrl Pts',(-0.319277542253672,2.14385281460139,
5.84731426448387));
#57606=CARTESIAN_POINT('Ctrl Pts',(-0.319344049930595,2.14336628042638,
5.84734470589697));
#57607=CARTESIAN_POINT('Ctrl Pts',(-0.319382194458872,2.14308445622464,
5.84736231455225));
#57608=CARTESIAN_POINT('Ctrl Pts',(-0.319495469860674,2.14223912343266,
5.84741505934774));
#57609=CARTESIAN_POINT('Ctrl Pts',(-0.319569483301295,2.14167546237286,
5.84745013265542));
#57610=CARTESIAN_POINT('Ctrl Pts',(-0.320275505848948,2.13618614926962,
5.84779078692209));
#57611=CARTESIAN_POINT('Ctrl Pts',(-0.320795117685735,2.13124637773909,
5.84809018271486));
#57612=CARTESIAN_POINT('Ctrl Pts',(-0.321909745541444,2.1176315495383,5.84890057323159));
#57613=CARTESIAN_POINT('Ctrl Pts',(-0.322268267235593,2.10894103123165,
5.84940145333319));
#57614=CARTESIAN_POINT('Ctrl Pts',(-0.322299152829136,2.06848972625361,
5.85169907108656));
#57615=CARTESIAN_POINT('Ctrl Pts',(-0.317630088314807,2.03690627870991,
5.85341581292444));
#57616=CARTESIAN_POINT('Ctrl Pts',(-0.306832050915311,2.00128242650799,
5.85562514977907));
#57617=CARTESIAN_POINT('Ctrl Pts',(-0.305113297466253,1.99609168936067,
5.8559536093269));
#57618=CARTESIAN_POINT('Ctrl Pts',(-0.302964947794916,1.99011736218584,
5.85634017055159));
#57619=CARTESIAN_POINT('Ctrl Pts',(-0.302663063079958,1.98928855565854,
5.85639398950238));
#57620=CARTESIAN_POINT('Ctrl Pts',(-0.302177111718614,1.98797124796551,
5.85647983961475));
#57621=CARTESIAN_POINT('Ctrl Pts',(-0.301995252659374,1.9874819325835,5.85651179706453));
#57622=CARTESIAN_POINT('Ctrl Pts',(-0.301672873057565,1.98662094031251,
5.85656815022161));
#57623=CARTESIAN_POINT('Ctrl Pts',(-0.301532852127135,1.98624907648614,
5.85659252917215));
#57624=CARTESIAN_POINT('Ctrl Pts',(-0.301242591101558,1.98548251097197,
5.8566428671562));
#57625=CARTESIAN_POINT('Ctrl Pts',(-0.301092262221968,1.98508784392319,
5.85666882912773));
#57626=CARTESIAN_POINT('Ctrl Pts',(-0.300706746866104,1.98408167850595,
5.85673513318695));
#57627=CARTESIAN_POINT('Ctrl Pts',(-0.3004704714884,1.98347060189718,5.85677551177803));
#57628=CARTESIAN_POINT('Ctrl Pts',(-0.299508568914852,1.98100521960543,
5.85693886693759));
#57629=CARTESIAN_POINT('Ctrl Pts',(-0.298767638616338,1.97915696774651,
5.85706235775706));
#57630=CARTESIAN_POINT('Ctrl Pts',(-0.293825020448678,1.96715096315554,
5.85787138303386));
#57631=CARTESIAN_POINT('Ctrl Pts',(-0.289123547575297,1.95720806471087,
5.85857387747085));
#57632=CARTESIAN_POINT('Ctrl Pts',(-0.269376055747928,1.92043609502304,
5.86130005562987));
#57633=CARTESIAN_POINT('Ctrl Pts',(-0.251029430650001,1.89557288765733,
5.86343291900502));
#57634=CARTESIAN_POINT('Ctrl Pts',(-0.228344419024603,1.87257431339062,
5.86555761256718));
#57635=CARTESIAN_POINT('Ctrl Pts',(-0.227239172108488,1.871469968172,5.86566000864408));
#57636=CARTESIAN_POINT('Ctrl Pts',(-0.225557483889891,1.86981391538576,
5.86581406949147));
#57637=CARTESIAN_POINT('Ctrl Pts',(-0.224986965718934,1.86925625172414,
5.86586603698184));
#57638=CARTESIAN_POINT('Ctrl Pts',(-0.223645323170776,1.86795454485823,
5.86598753670674));
#57639=CARTESIAN_POINT('Ctrl Pts',(-0.222872542196176,1.86721221290131,
5.86605697687923));
#57640=CARTESIAN_POINT('Ctrl Pts',(-0.218950415745593,1.8634820592006,5.86640661482323));
#57641=CARTESIAN_POINT('Ctrl Pts',(-0.215744444940642,1.86055405630005,
5.86668337796792));
#57642=CARTESIAN_POINT('Ctrl Pts',(-0.212028799627972,1.85729580959307,
5.86699305726811));
#57643=CARTESIAN_POINT('Ctrl Pts',(-0.211576389154281,1.85690132151947,
5.8670305804367));
#57644=CARTESIAN_POINT('Ctrl Pts',(-0.210906440268504,1.85632043347992,
5.86708587341841));
#57645=CARTESIAN_POINT('Ctrl Pts',(-0.210689754539812,1.85613305878076,
5.86710371519191));
#57646=CARTESIAN_POINT('Ctrl Pts',(-0.210305837499724,1.85580196774247,
5.86713525202897));
#57647=CARTESIAN_POINT('Ctrl Pts',(-0.210138708336134,1.85565813394977,
5.86714895586355));
#57648=CARTESIAN_POINT('Ctrl Pts',(-0.209789110889789,1.85535788928486,
5.86717756894567));
#57649=CARTESIAN_POINT('Ctrl Pts',(-0.209606615653896,1.85520151132388,
5.86719247574261));
#57650=CARTESIAN_POINT('Ctrl Pts',(-0.209128514739989,1.85479275903371,
5.86723145149828));
#57651=CARTESIAN_POINT('Ctrl Pts',(-0.208832625994621,1.85454071412225,
5.86725549600962));
#57652=CARTESIAN_POINT('Ctrl Pts',(-0.207535015911361,1.85343942437933,
5.86736060971929));
#57653=CARTESIAN_POINT('Ctrl Pts',(-0.206528546636458,1.85259575621504,
5.86744127339747));
#57654=CARTESIAN_POINT('Ctrl Pts',(-0.199034289112397,1.84639133344262,
5.86803576079662));
#57655=CARTESIAN_POINT('Ctrl Pts',(-0.192343265210407,1.84127988152837,
5.86853268383402));
#57656=CARTESIAN_POINT('Ctrl Pts',(-0.172410707253764,1.82725416838901,
5.86994254398031));
#57657=CARTESIAN_POINT('Ctrl Pts',(-0.158697585376564,1.81905359487004,
5.87082832345679));
#57658=CARTESIAN_POINT('Ctrl Pts',(-0.122365344702224,1.80083907820688,
5.87310132157554));
#57659=CARTESIAN_POINT('Ctrl Pts',(-0.0991038509970655,1.79234969146709,
5.87449610614019));
#57660=CARTESIAN_POINT('Ctrl Pts',(-0.0735756788442157,1.78623215193834,
5.87608759994219));
#57661=CARTESIAN_POINT('Ctrl Pts',(-0.0720455067440576,1.78587727268379,
5.87618318314318));
#57662=CARTESIAN_POINT('Ctrl Pts',(-0.0699715425688329,1.78541222755775,
5.87631300857094));
#57663=CARTESIAN_POINT('Ctrl Pts',(-0.0694299531255458,1.7852922547147,
5.87634693602148));
#57664=CARTESIAN_POINT('Ctrl Pts',(-0.0685136230434926,1.78509174987352,
5.87640438235838));
#57665=CARTESIAN_POINT('Ctrl Pts',(-0.0681390422193349,1.7850104867402,
5.87642787777476));
#57666=CARTESIAN_POINT('Ctrl Pts',(-0.0674188622620702,1.78485559262965,
5.87647307470548));
#57667=CARTESIAN_POINT('Ctrl Pts',(-0.0670732850402093,1.78478186137555,
5.87649477297386));
#57668=CARTESIAN_POINT('Ctrl Pts',(-0.0662599227253543,1.78460972308465,
5.87654586799627));
#57669=CARTESIAN_POINT('Ctrl Pts',(-0.0657920394986536,1.78451178838659,
5.87657527981746));
#57670=CARTESIAN_POINT('Ctrl Pts',(-0.0644345674962926,1.7842308010358,
5.87666067032801));
#57671=CARTESIAN_POINT('Ctrl Pts',(-0.0635444260407747,1.78405046859499,
5.87671673582982));
#57672=CARTESIAN_POINT('Ctrl Pts',(-0.0573281479795498,1.78281845441331,
5.8771087841462));
#57673=CARTESIAN_POINT('Ctrl Pts',(-0.0519772175502979,1.78189779555488,
5.87744892169057));
#57674=CARTESIAN_POINT('Ctrl Pts',(-0.0353289799955228,1.7794646311759,
5.87851628863267));
#57675=CARTESIAN_POINT('Ctrl Pts',(-0.0239738266270041,1.77841600389988,
5.87925754506346));
#57676=CARTESIAN_POINT('Ctrl Pts',(0.018012418676957,1.77677477758248,5.88204191822955));
#57677=CARTESIAN_POINT('Ctrl Pts',(0.0486242682877354,1.77994606354785,
5.88417367464612));
#57678=CARTESIAN_POINT('Ctrl Pts',(0.0818523072166536,1.78827162418953,
5.88637615380775));
#57679=CARTESIAN_POINT('Ctrl Pts',(0.0853621925889448,1.78921441584519,
5.8866071062415));
#57680=CARTESIAN_POINT('Ctrl Pts',(0.0894103936000768,1.79037556570785,
5.88687091148799));
#57681=CARTESIAN_POINT('Ctrl Pts',(0.089964805825962,1.79053620160119,5.88690698411782));
#57682=CARTESIAN_POINT('Ctrl Pts',(0.0907882267240392,1.79077718013067,
5.88696047294389));
#57683=CARTESIAN_POINT('Ctrl Pts',(0.0910575629599759,1.7908563850427,5.88697795501326));
#57684=CARTESIAN_POINT('Ctrl Pts',(0.0915369200238509,1.79099803252306,
5.88700904406568));
#57685=CARTESIAN_POINT('Ctrl Pts',(0.0917469805518384,1.7910603372942,5.88702265910571));
#57686=CARTESIAN_POINT('Ctrl Pts',(0.0921926135113602,1.79119300836335,
5.88705152439189));
#57687=CARTESIAN_POINT('Ctrl Pts',(0.0924281683354561,1.7912634298162,5.88706677130715));
#57688=CARTESIAN_POINT('Ctrl Pts',(0.0930595400778105,1.79145297200373,
5.88710761003534));
#57689=CARTESIAN_POINT('Ctrl Pts',(0.0934552104642061,1.7915725853196,5.88713317295116));
#57690=CARTESIAN_POINT('Ctrl Pts',(0.0953433396208922,1.79214734401817,
5.88725501983132));
#57691=CARTESIAN_POINT('Ctrl Pts',(0.0968327427997494,1.79261257286985,
5.88735072149524));
#57692=CARTESIAN_POINT('Ctrl Pts',(0.109116192116552,1.79654756305845,5.88813701557171));
#57693=CARTESIAN_POINT('Ctrl Pts',(0.119724892893234,1.80057432513179,5.88879712845626));
#57694=CARTESIAN_POINT('Ctrl Pts',(0.154338764754285,1.81584756205429,5.89095481441185));
#57695=CARTESIAN_POINT('Ctrl Pts',(0.177165699417369,1.82949036538013,5.89239272813096));
#57696=CARTESIAN_POINT('Ctrl Pts',(0.207131200685941,1.85283629229838,5.89458779526385));
#57697=CARTESIAN_POINT('Ctrl Pts',(0.215811174433609,1.8603779557243,5.89526624350565));
#57698=CARTESIAN_POINT('Ctrl Pts',(0.224933673498165,1.86920254664458,5.89603777573693));
#57699=CARTESIAN_POINT('Ctrl Pts',(0.225793362954381,1.87004352774241,5.89611108865486));
#57700=CARTESIAN_POINT('Ctrl Pts',(0.226991266162491,1.8712285563584,5.89621410497054));
#57701=CARTESIAN_POINT('Ctrl Pts',(0.227333452548888,1.87156858865708,5.89624363146771));
#57702=CARTESIAN_POINT('Ctrl Pts',(0.227958460820005,1.87219245772562,5.89629774513913));
#57703=CARTESIAN_POINT('Ctrl Pts',(0.228241519733373,1.87247605654785,5.89632232174967));
#57704=CARTESIAN_POINT('Ctrl Pts',(0.228806972048985,1.87304470447661,5.89637155628299));
#57705=CARTESIAN_POINT('Ctrl Pts',(0.229089363454994,1.87332975454683,5.89639621422717));
#57706=CARTESIAN_POINT('Ctrl Pts',(0.229776626207071,1.87402608392546,5.89645639592029));
#57707=CARTESIAN_POINT('Ctrl Pts',(0.230180925434693,1.87443792371881,5.89649194469645));
#57708=CARTESIAN_POINT('Ctrl Pts',(0.231041927645179,1.87531970998233,5.89656796252592));
#57709=CARTESIAN_POINT('Ctrl Pts',(0.231498307273205,1.87578996728089,5.8966084454966));
#57710=CARTESIAN_POINT('Ctrl Pts',(0.232758231222888,1.87709615104065,5.89672073440696));
#57711=CARTESIAN_POINT('Ctrl Pts',(0.233558697347007,1.87793502095114,5.89679267348119));
#57712=CARTESIAN_POINT('Ctrl Pts',(0.240359800043001,1.88513986991649,5.89740907570609));
#57713=CARTESIAN_POINT('Ctrl Pts',(0.246102940801926,1.89174288096354,5.89796443249822));
#57714=CARTESIAN_POINT('Ctrl Pts',(0.256582180659106,1.90483066873755,5.89904868377395));
#57715=CARTESIAN_POINT('Ctrl Pts',(0.26135864552966,1.91127499845539,5.8995755344524));
#57716=CARTESIAN_POINT('Ctrl Pts',(0.283874691551311,1.94414959819888,5.90222464073648));
#57717=CARTESIAN_POINT('Ctrl Pts',(0.297869860329996,1.9729264630263,5.90444531093781));
#57718=CARTESIAN_POINT('Ctrl Pts',(0.307885441082755,2.00476279266951,5.90655707004294));
#57719=CARTESIAN_POINT('Ctrl Pts',(0.308339222323259,2.00624236193462,5.90665442845457));
#57720=CARTESIAN_POINT('Ctrl Pts',(0.308904484862313,2.00813391895601,5.90677784722743));
#57721=CARTESIAN_POINT('Ctrl Pts',(0.309025820114343,2.00854290556724,5.9068044700906));
#57722=CARTESIAN_POINT('Ctrl Pts',(0.309217339881436,2.00919319687889,5.90684670022106));
#57723=CARTESIAN_POINT('Ctrl Pts',(0.309288054330192,2.00943434300957,5.90686233842063));
#57724=CARTESIAN_POINT('Ctrl Pts',(0.309419673174766,2.00988513365147,5.90689153070262));
#57725=CARTESIAN_POINT('Ctrl Pts',(0.30948064615236,2.01009475575843,5.90690508870986));
#57726=CARTESIAN_POINT('Ctrl Pts',(0.30961721589297,2.01056606103152,5.90693553457582));
#57727=CARTESIAN_POINT('Ctrl Pts',(0.309692693751389,2.01082777755908,5.90695241537429));
#57728=CARTESIAN_POINT('Ctrl Pts',(0.309915706927583,2.0116047654323,5.90700245555047));
#57729=CARTESIAN_POINT('Ctrl Pts',(0.310062289654226,2.01212031270614,5.90703555938568));
#57730=CARTESIAN_POINT('Ctrl Pts',(0.311233043082511,2.01627737444864,5.90730171069016));
#57731=CARTESIAN_POINT('Ctrl Pts',(0.312194366312396,2.01993648878598,5.90753117559));
#57732=CARTESIAN_POINT('Ctrl Pts',(0.315448704243452,2.03327500415194,5.90835310477475));
#57733=CARTESIAN_POINT('Ctrl Pts',(0.317357915125968,2.04304300496929,5.908927525144));
#57734=CARTESIAN_POINT('Ctrl Pts',(0.323474489300776,2.08443147440125,5.91130455419184));
#57735=CARTESIAN_POINT('Ctrl Pts',(0.323428723733039,2.11649360942277,5.91302786343218));
#57736=CARTESIAN_POINT('Ctrl Pts',(0.317868565371912,2.15338648361829,5.91524277950933));
#57737=CARTESIAN_POINT('Ctrl Pts',(0.316925993521362,2.15872351131321,5.91556838657768));
#57738=CARTESIAN_POINT('Ctrl Pts',(0.315674596854227,2.16489605684914,5.91595186670328));
#57739=CARTESIAN_POINT('Ctrl Pts',(0.315496301924824,2.1657573778473,5.9160055343774));
#57740=CARTESIAN_POINT('Ctrl Pts',(0.315206728141049,2.16712798151037,5.91609118821949));
#57741=CARTESIAN_POINT('Ctrl Pts',(0.315097734921821,2.16763774692533,5.91612310120431));
#57742=CARTESIAN_POINT('Ctrl Pts',(0.314905188607795,2.16852772691989,5.91617891548017));
#57743=CARTESIAN_POINT('Ctrl Pts',(0.314822182301013,2.16890805974657,5.91620279920292));
#57744=CARTESIAN_POINT('Ctrl Pts',(0.314656638070723,2.16966003642676,5.9162500837104));
#57745=CARTESIAN_POINT('Ctrl Pts',(0.314574130317158,2.17003168632963,5.91627348349224));
#57746=CARTESIAN_POINT('Ctrl Pts',(0.314359788162189,2.17098915250499,5.91633384601408));
#57747=CARTESIAN_POINT('Ctrl Pts',(0.314226975117556,2.17157474615695,5.91637084013599));
#57748=CARTESIAN_POINT('Ctrl Pts',(0.313938373811275,2.1728309485022,5.91645036356686));
#57749=CARTESIAN_POINT('Ctrl Pts',(0.313782071901832,2.173501435035,5.91649290926483));
#57750=CARTESIAN_POINT('Ctrl Pts',(0.313337678769559,2.17538049034476,5.91661243003385));
#57751=CARTESIAN_POINT('Ctrl Pts',(0.31304474765444,2.17658789171759,5.91668956070578));
#57752=CARTESIAN_POINT('Ctrl Pts',(0.312074267648776,2.18048940537081,5.91693988521061));
#57753=CARTESIAN_POINT('Ctrl Pts',(0.31136887834961,2.18317640123909,5.9171139725925));
#57754=CARTESIAN_POINT('Ctrl Pts',(0.308434964303101,2.19379162805344,5.91780858288632));
#57755=CARTESIAN_POINT('Ctrl Pts',(0.305937793093243,2.20164174404664,5.91833763227893));
#57756=CARTESIAN_POINT('Ctrl Pts',(0.292873761551843,2.23784591173306,5.92085023836029));
#57757=CARTESIAN_POINT('Ctrl Pts',(0.278650657881394,2.26471161897201,5.92294598742858));
#57758=CARTESIAN_POINT('Ctrl Pts',(0.259556998880454,2.29104062154919,5.92509110524389));
#57759=CARTESIAN_POINT('Ctrl Pts',(0.258201452457649,2.29286877709352,5.92524047255357));
#57760=CARTESIAN_POINT('Ctrl Pts',(0.256403751806235,2.29524031783795,5.92543463936345));
#57761=CARTESIAN_POINT('Ctrl Pts',(0.255979059670027,2.29579679945235,5.92548022991581));
#57762=CARTESIAN_POINT('Ctrl Pts',(0.255339445515972,2.29662925909837,5.92554846927776));
#57763=CARTESIAN_POINT('Ctrl Pts',(0.255125884345274,2.29690627493564,5.92557118364002));
#57764=CARTESIAN_POINT('Ctrl Pts',(0.251828345878157,2.30116922834889,5.92592082487133));
#57765=CARTESIAN_POINT('Ctrl Pts',(0.248651518977412,2.30508291828741,5.92624308811138));
#57766=CARTESIAN_POINT('Ctrl Pts',(0.244973027077439,2.30940342284844,5.92659877879941));
#57767=CARTESIAN_POINT('Ctrl Pts',(0.244560640765067,2.30988489822024,5.92663841571429));
#57768=CARTESIAN_POINT('Ctrl Pts',(0.243958454311387,2.3105837873148,5.92669594528991));
#57769=CARTESIAN_POINT('Ctrl Pts',(0.243769781844406,2.31080216405658,5.92671392032301));
#57770=CARTESIAN_POINT('Ctrl Pts',(0.243436220036271,2.31118719460483,5.92674561107171));
#57771=CARTESIAN_POINT('Ctrl Pts',(0.243291452535744,2.31135395315641,5.92675933584449));
#57772=CARTESIAN_POINT('Ctrl Pts',(0.242989423724844,2.31170114044945,5.92678790897882));
#57773=CARTESIAN_POINT('Ctrl Pts',(0.242832133132022,2.31188154244571,5.92680275505514));
#57774=CARTESIAN_POINT('Ctrl Pts',(0.24242178418731,2.31235112865637,5.92684139777665));
#57775=CARTESIAN_POINT('Ctrl Pts',(0.242168408380421,2.31264003686119,5.92686517073903));
#57776=CARTESIAN_POINT('Ctrl Pts',(0.241073367799878,2.31388414565622,5.92696753955987));
#57777=CARTESIAN_POINT('Ctrl Pts',(0.240226548890328,2.31483482436609,5.9270457556523));
#57778=CARTESIAN_POINT('Ctrl Pts',(0.234023987108327,2.32171557960394,5.92761201688977));
#57779=CARTESIAN_POINT('Ctrl Pts',(0.228454476739092,2.3274502157832,5.92808481359217));
#57780=CARTESIAN_POINT('Ctrl Pts',(0.210101142790094,2.34499249367169,5.9295569879299));
#57781=CARTESIAN_POINT('Ctrl Pts',(0.196571768656621,2.35597546165371,5.93051999921938));
#57782=CARTESIAN_POINT('Ctrl Pts',(0.173825972315789,2.371568235032,5.93206343206742));
#57783=CARTESIAN_POINT('Ctrl Pts',(0.165163190686127,2.37692215798706,5.93263559221807));
#57784=CARTESIAN_POINT('Ctrl Pts',(0.144015181940963,2.38864664301284,5.93401997305151));
#57785=CARTESIAN_POINT('Ctrl Pts',(0.131340469967132,2.39463004051628,5.93484056814862));
#57786=CARTESIAN_POINT('Ctrl Pts',(0.117173716331366,2.40022160003568,5.93576604321558));
#57787=CARTESIAN_POINT('Ctrl Pts',(0.116026893538369,2.4006666739717,5.93584101174342));
#57788=CARTESIAN_POINT('Ctrl Pts',(0.114410437430141,2.40128338387601,5.93594675986202));
#57789=CARTESIAN_POINT('Ctrl Pts',(0.113942899939969,2.4014605134036,5.9359773553303));
#57790=CARTESIAN_POINT('Ctrl Pts',(0.113129961134235,2.40176633904944,5.93603057058695));
#57791=CARTESIAN_POINT('Ctrl Pts',(0.112784746772811,2.4018955322344,5.93605317370996));
#57792=CARTESIAN_POINT('Ctrl Pts',(0.112072584229157,2.40216066027659,5.93609981418559));
#57793=CARTESIAN_POINT('Ctrl Pts',(0.111705608700279,2.40229651955883,5.93612385401888));
#57794=CARTESIAN_POINT('Ctrl Pts',(0.110873656708889,2.4026027976063,5.93617836780097));
#57795=CARTESIAN_POINT('Ctrl Pts',(0.11040853387257,2.40277281336821,5.93620885512825));
#57796=CARTESIAN_POINT('Ctrl Pts',(0.109408374517544,2.40313578922414,5.93627443482322));
#57797=CARTESIAN_POINT('Ctrl Pts',(0.108873216004177,2.40332840611025,5.93630953851775));
#57798=CARTESIAN_POINT('Ctrl Pts',(0.107444924188173,2.40383821713495,5.93640326526189));
#57799=CARTESIAN_POINT('Ctrl Pts',(0.106550901832313,2.40415288789266,5.93646197197736));
#57800=CARTESIAN_POINT('Ctrl Pts',(0.103835164873879,2.4050953078456,5.93664042954428));
#57801=CARTESIAN_POINT('Ctrl Pts',(0.102009221814378,2.40571065853003,5.93676058897178));
#57802=CARTESIAN_POINT('Ctrl Pts',(0.0954059974970812,2.40787022905597,
5.93719579981648));
#57803=CARTESIAN_POINT('Ctrl Pts',(0.0905985056734264,2.4093190723698,5.93751393583382));
#57804=CARTESIAN_POINT('Ctrl Pts',(0.0739521978342939,2.41391444836124,
5.93862030998128));
#57805=CARTESIAN_POINT('Ctrl Pts',(0.0619700678904657,2.41649780896726,
5.93942544001448));
#57806=CARTESIAN_POINT('Ctrl Pts',(0.0248501533739732,2.42231204160706,
5.94193624169357));
#57807=CARTESIAN_POINT('Ctrl Pts',(-0.000544646142155328,2.42326811623638,
5.94368350304947));
#57808=CARTESIAN_POINT('Ctrl Pts',(-0.0271344272948742,2.42113349204407,
5.94542052101855));
#57809=CARTESIAN_POINT('Ctrl Pts',(-0.0284789599432046,2.42101704910268,
5.94550808000024));
#57810=CARTESIAN_POINT('Ctrl Pts',(-0.0342047096750918,2.42048491531657,
5.94587967553323));
#57811=CARTESIAN_POINT('Ctrl Pts',(-0.0385781520544983,2.41998792802032,
5.94616031979644));
#57812=CARTESIAN_POINT('Ctrl Pts',(-0.0435451644099679,2.41932016339867,
5.94647438325466));
#57813=CARTESIAN_POINT('Ctrl Pts',(-0.0441498007895482,2.41923712691536,
5.94651253518693));
#57814=CARTESIAN_POINT('Ctrl Pts',(-0.0450355919893432,2.4191129138967,
5.94656830803236));
#57815=CARTESIAN_POINT('Ctrl Pts',(-0.0453169294817579,2.41907308295328,
5.94658600442564));
#57816=CARTESIAN_POINT('Ctrl Pts',(-0.0458161543058124,2.41900173055541,
5.9466173742618));
#57817=CARTESIAN_POINT('Ctrl Pts',(-0.0460340621991443,2.4189703578882,
5.94663105616374));
#57818=CARTESIAN_POINT('Ctrl Pts',(-0.0464909019615065,2.41890410778745,
5.94665971721381));
#57819=CARTESIAN_POINT('Ctrl Pts',(-0.0467298262391742,2.418869185199,5.94667469372496));
#57820=CARTESIAN_POINT('Ctrl Pts',(-0.0473582496228737,2.4187766096347,
5.94671405147865));
#57821=CARTESIAN_POINT('Ctrl Pts',(-0.0477476842309654,2.41871851109095,
5.94673840738548));
#57822=CARTESIAN_POINT('Ctrl Pts',(-0.0494824750020427,2.418456452074,5.94684675594786));
#57823=CARTESIAN_POINT('Ctrl Pts',(-0.050826663443067,2.41824468202518,
5.94693031156555));
#57824=CARTESIAN_POINT('Ctrl Pts',(-0.0609843379672103,2.41657839232637,
5.94755898448899));
#57825=CARTESIAN_POINT('Ctrl Pts',(-0.0697361589562724,2.41476637080739,
5.9480850830531));
#57826=CARTESIAN_POINT('Ctrl Pts',(-0.0938645701930585,2.40871466333967,
5.9495200011912));
#57827=CARTESIAN_POINT('Ctrl Pts',(-0.10901879296144,2.40369435939589,5.95040413247739));
#57828=CARTESIAN_POINT('Ctrl Pts',(-0.131595136689005,2.39430642033264,
5.95177210032367));
#57829=CARTESIAN_POINT('Ctrl Pts',(-0.139317700866998,2.39073032217292,
5.95224955800796));
#57830=CARTESIAN_POINT('Ctrl Pts',(-0.161162083675026,2.3795444138845,5.95364541554557));
#57831=CARTESIAN_POINT('Ctrl Pts',(-0.174867317973763,2.37118187371701,
5.95457930833665));
#57832=CARTESIAN_POINT('Ctrl Pts',(-0.188917100596259,2.36109978106376,
5.95562988868433));
#57833=CARTESIAN_POINT('Ctrl Pts',(-0.189937538679195,2.36035840278169,
5.95570674514527));
#57834=CARTESIAN_POINT('Ctrl Pts',(-0.191360686204609,2.35931162486902,
5.95581472010645));
#57835=CARTESIAN_POINT('Ctrl Pts',(-0.19176707857674,2.35901123254883,5.95584564396108));
#57836=CARTESIAN_POINT('Ctrl Pts',(-0.19246976678205,2.35848926744706,5.95589927206847));
#57837=CARTESIAN_POINT('Ctrl Pts',(-0.192766391550058,2.35826813740253,
5.95592195901416));
#57838=CARTESIAN_POINT('Ctrl Pts',(-0.193375195427103,2.35781264863979,
5.95596862370062));
#57839=CARTESIAN_POINT('Ctrl Pts',(-0.193687330747948,2.3575782326028,5.95599260366396));
#57840=CARTESIAN_POINT('Ctrl Pts',(-0.194413626711849,2.35703071205162,
5.95604853016788));
#57841=CARTESIAN_POINT('Ctrl Pts',(-0.194827457271954,2.35671717331907,
5.95608049373833));
#57842=CARTESIAN_POINT('Ctrl Pts',(-0.195699183691634,2.35605338792739,
5.95614803171647));
#57843=CARTESIAN_POINT('Ctrl Pts',(-0.196156900599818,2.35570291024317,
5.95618361518185));
#57844=CARTESIAN_POINT('Ctrl Pts',(-0.197379406211927,2.35476161327594,
5.95627898108646));
#57845=CARTESIAN_POINT('Ctrl Pts',(-0.198142477397575,2.35416858227091,
5.95633885109385));
#57846=CARTESIAN_POINT('Ctrl Pts',(-0.200459525043095,2.35235108204038,
5.95652170360012));
#57847=CARTESIAN_POINT('Ctrl Pts',(-0.202004881376879,2.35111574503841,
5.95664511866774));
#57848=CARTESIAN_POINT('Ctrl Pts',(-0.207573036532313,2.34657997783755,
5.95709520444008));
#57849=CARTESIAN_POINT('Ctrl Pts',(-0.211526951680161,2.34319661724007,
5.95742519671695));
#57850=CARTESIAN_POINT('Ctrl Pts',(-0.220319556615638,2.33529611781992,
5.95818340135166));
#57851=CARTESIAN_POINT('Ctrl Pts',(-0.225104365213146,2.33072274578182,
5.95861375920701));
#57852=CARTESIAN_POINT('Ctrl Pts',(-0.241371378174606,2.31418660010616,
5.9601398951498));
#57853=CARTESIAN_POINT('Ctrl Pts',(-0.252067788547602,2.30148892782995,
5.96126140185053));
#57854=CARTESIAN_POINT('Ctrl Pts',(-0.272876410845914,2.27252257399,5.96367445293564));
#57855=CARTESIAN_POINT('Ctrl Pts',(-0.282615679658572,2.25605811756274,
5.96496147068477));
#57856=CARTESIAN_POINT('Ctrl Pts',(-0.291331894598258,2.23779768631007,
5.96623694079903));
#57857=CARTESIAN_POINT('Ctrl Pts',(-0.291817507543199,2.23676628804718,
5.96630848695744));
#57858=CARTESIAN_POINT('Ctrl Pts',(-0.29245894457534,2.2353849623668,5.96640362463533));
#57859=CARTESIAN_POINT('Ctrl Pts',(-0.292619624844501,2.23503731875548,
5.96642751080922));
#57860=CARTESIAN_POINT('Ctrl Pts',(-0.292869620597625,2.23449389302969,
5.96646475824669));
#57861=CARTESIAN_POINT('Ctrl Pts',(-0.292959359670112,2.23429830793281,
5.96647814570673));
#57862=CARTESIAN_POINT('Ctrl Pts',(-0.293130906524664,2.23392343372899,
5.96650376991083));
#57863=CARTESIAN_POINT('Ctrl Pts',(-0.29321274516041,2.23374416076038,5.96651600849295));
#57864=CARTESIAN_POINT('Ctrl Pts',(-0.293405776274511,2.2333202845306,5.96654490919947));
#57865=CARTESIAN_POINT('Ctrl Pts',(-0.293516827189713,2.23307561751243,
5.96656156247198));
#57866=CARTESIAN_POINT('Ctrl Pts',(-0.293841166598091,2.23235865288243,
5.96661027980416));
#57867=CARTESIAN_POINT('Ctrl Pts',(-0.29405362331227,2.23188597653412,5.96664229265333));
#57868=CARTESIAN_POINT('Ctrl Pts',(-0.295609461174895,2.22840208009805,
5.96687748651993));
#57869=CARTESIAN_POINT('Ctrl Pts',(-0.296907761050969,2.22537077485921,
5.96707795654666));
#57870=CARTESIAN_POINT('Ctrl Pts',(-0.301031421160604,2.21531920085007,
5.96773074998102));
#57871=CARTESIAN_POINT('Ctrl Pts',(-0.30365624534299,2.2082189302946,5.96817291655553));
#57872=CARTESIAN_POINT('Ctrl Pts',(-0.316779669352195,2.1684678262965,5.97057872956467));
#57873=CARTESIAN_POINT('Ctrl Pts',(-0.32226369604783,2.13439903461908,5.9724110985191));
#57874=CARTESIAN_POINT('Ctrl Pts',(-0.322274982545603,2.10010606710754,
5.97444230798123));
#57875=CARTESIAN_POINT('',(-0.322274999303774,2.10002118378279,6.22472265507673));
#57876=CARTESIAN_POINT('Ctrl Pts',(-0.322274982642247,2.10010577305737,
5.97444232539814));
#57877=CARTESIAN_POINT('Ctrl Pts',(-0.322276324034467,2.09601874782303,
5.9746844044184));
#57878=CARTESIAN_POINT('Ctrl Pts',(-0.32219991927052,2.09193217407,5.97492868233561));
#57879=CARTESIAN_POINT('Ctrl Pts',(-0.321968486419485,2.08579873707773,
5.97529915987549));
#57880=CARTESIAN_POINT('Ctrl Pts',(-0.321871590513878,2.08375004504883,
5.97542355104126));
#57881=CARTESIAN_POINT('Ctrl Pts',(-0.321720677281781,2.08109629533517,
5.97558555916811));
#57882=CARTESIAN_POINT('Ctrl Pts',(-0.321684493673447,2.08049023929307,
5.97562261760034));
#57883=CARTESIAN_POINT('Ctrl Pts',(-0.321619995793277,2.0794589296274,5.9756857815322));
#57884=CARTESIAN_POINT('Ctrl Pts',(-0.321592550045636,2.07903362171208,
5.9757118597827));
#57885=CARTESIAN_POINT('Ctrl Pts',(-0.321539924274289,2.07824253809059,
5.97576042174362));
#57886=CARTESIAN_POINT('Ctrl Pts',(-0.321514963530535,2.07787674808591,
5.97578289854142));
#57887=CARTESIAN_POINT('Ctrl Pts',(-0.32146332831164,2.07713860159609,5.97582830072277));
#57888=CARTESIAN_POINT('Ctrl Pts',(-0.321436630956802,2.07676624732297,
5.97585122679096));
#57889=CARTESIAN_POINT('Ctrl Pts',(-0.321373136224455,2.07590173211162,
5.97590450967321));
#57890=CARTESIAN_POINT('Ctrl Pts',(-0.321335855217238,2.07540960859504,
5.97593488163286));
#57891=CARTESIAN_POINT('Ctrl Pts',(-0.321237566908938,2.0741505683697,5.97601269003489));
#57892=CARTESIAN_POINT('Ctrl Pts',(-0.321174943834661,2.07338378416154,
5.97606017715736));
#57893=CARTESIAN_POINT('Ctrl Pts',(-0.320801147318777,2.06900038282241,
5.97633222167329));
#57894=CARTESIAN_POINT('Ctrl Pts',(-0.320431643059886,2.06538912342834,
5.97655860628214));
#57895=CARTESIAN_POINT('Ctrl Pts',(-0.319933724434097,2.06121969950897,
5.97682271708887));
#57896=CARTESIAN_POINT('Ctrl Pts',(-0.319864719108417,2.06065459112596,
5.97685857187485));
#57897=CARTESIAN_POINT('Ctrl Pts',(-0.319748312806751,2.05972184856381,
5.97691784870096));
#57898=CARTESIAN_POINT('Ctrl Pts',(-0.319701774090159,2.05935410638641,
5.97694124391604));
#57899=CARTESIAN_POINT('Ctrl Pts',(-0.31937029412024,2.05677059219032,5.97710577797865));
#57900=CARTESIAN_POINT('Ctrl Pts',(-0.319062960076768,2.05455779962926,
5.97724760611613));
#57901=CARTESIAN_POINT('Ctrl Pts',(-0.313541684992787,2.01762700297687,
5.97962996163393));
#57902=CARTESIAN_POINT('Ctrl Pts',(-0.3027114338086,1.98398948036205,5.9820637321409));
#57903=CARTESIAN_POINT('Ctrl Pts',(-0.283770011806913,1.94710680351185,
5.98480784499535));
#57904=CARTESIAN_POINT('Ctrl Pts',(-0.280692524035074,1.94152770761205,
5.98522406235335));
#57905=CARTESIAN_POINT('Ctrl Pts',(-0.275908613697531,1.93343226725783,
5.9858258589934));
#57906=CARTESIAN_POINT('Ctrl Pts',(-0.274328902530941,1.93084318642345,
5.98601798574393));
#57907=CARTESIAN_POINT('Ctrl Pts',(-0.272442611369619,1.92784757838102,
5.98623953002309));
#57908=CARTESIAN_POINT('Ctrl Pts',(-0.272171398524418,1.92741911289836,
5.98627119964388));
#57909=CARTESIAN_POINT('Ctrl Pts',(-0.271756191037942,1.92676657598484,
5.98631940142748));
#57910=CARTESIAN_POINT('Ctrl Pts',(-0.271612929613146,1.92654204246659,
5.9863359819238));
#57911=CARTESIAN_POINT('Ctrl Pts',(-0.271363315196208,1.9261518894814,5.98636478268045));
#57912=CARTESIAN_POINT('Ctrl Pts',(-0.271257089111903,1.92598619028251,
5.98637701136242));
#57913=CARTESIAN_POINT('Ctrl Pts',(-0.271016593562798,1.92561180310387,
5.98640463428518));
#57914=CARTESIAN_POINT('Ctrl Pts',(-0.270882235106954,1.92540317326044,
5.98642002244607));
#57915=CARTESIAN_POINT('Ctrl Pts',(-0.270517860199896,1.92483881026177,
5.98646163615303));
#57916=CARTESIAN_POINT('Ctrl Pts',(-0.270287382090383,1.92448337353619,
5.98648783086211));
#57917=CARTESIAN_POINT('Ctrl Pts',(-0.269252307263618,1.92289398468269,
5.98660490806167));
#57918=CARTESIAN_POINT('Ctrl Pts',(-0.268439940157357,1.92166507815052,
5.9866952790142));
#57919=CARTESIAN_POINT('Ctrl Pts',(-0.25113644077913,1.89587540757211,5.98858953312115));
#57920=CARTESIAN_POINT('Ctrl Pts',(-0.231346571480411,1.87369093856763,
5.9901848308886));
#57921=CARTESIAN_POINT('Ctrl Pts',(-0.199261171030816,1.84639972738477,
5.99255832918909));
#57922=CARTESIAN_POINT('Ctrl Pts',(-0.189254396342781,1.83884708486307,
5.9932735083687));
#57923=CARTESIAN_POINT('Ctrl Pts',(-0.174621996600138,1.82908678676636,
5.99430748533453));
#57924=CARTESIAN_POINT('Ctrl Pts',(-0.170344497993436,1.82637697707623,
5.99460835091578));
#57925=CARTESIAN_POINT('Ctrl Pts',(-0.164343236446771,1.82277042811039,
5.99502950813506));
#57926=CARTESIAN_POINT('Ctrl Pts',(-0.162672414698106,1.82178673622255,
5.99514666159192));
#57927=CARTESIAN_POINT('Ctrl Pts',(-0.160168014144757,1.82034254979135,
5.99532215834626));
#57928=CARTESIAN_POINT('Ctrl Pts',(-0.159341085644919,1.81987056454653,
5.99538008869582));
#57929=CARTESIAN_POINT('Ctrl Pts',(-0.15801529474266,1.81912161384015,5.99547294491671));
#57930=CARTESIAN_POINT('Ctrl Pts',(-0.157517763060367,1.81884229425774,
5.99550778631902));
#57931=CARTESIAN_POINT('Ctrl Pts',(-0.15656908219843,1.81831300323682,5.99557421295439));
#57932=CARTESIAN_POINT('Ctrl Pts',(-0.156118069137033,1.81806279044802,
5.99560578943013));
#57933=CARTESIAN_POINT('Ctrl Pts',(-0.155325380996444,1.81762550862425,
5.99566128211725));
#57934=CARTESIAN_POINT('Ctrl Pts',(-0.154983962907371,1.81743797388755,
5.99568518162244));
#57935=CARTESIAN_POINT('Ctrl Pts',(-0.154316466633623,1.81707290409603,
5.9957319038689));
#57936=CARTESIAN_POINT('Ctrl Pts',(-0.153990419873345,1.81689531254961,
5.99575472454909));
#57937=CARTESIAN_POINT('Ctrl Pts',(-0.153215461963583,1.81647494237105,
5.9958089625517));
#57938=CARTESIAN_POINT('Ctrl Pts',(-0.152766280586222,1.81623266643378,
5.99584039770692));
#57939=CARTESIAN_POINT('Ctrl Pts',(-0.151179197877049,1.81538149862372,
5.99595146014532));
#57940=CARTESIAN_POINT('Ctrl Pts',(-0.15003822793166,1.81477838216951,5.99603129198993));
#57941=CARTESIAN_POINT('Ctrl Pts',(-0.132088242759602,1.80542753419985,
5.99728712469225));
#57942=CARTESIAN_POINT('Ctrl Pts',(-0.114546607542374,1.79817374912461,
5.99851644517375));
#57943=CARTESIAN_POINT('Ctrl Pts',(-0.0885519162482108,1.790018321513,6.00033540371106));
#57944=CARTESIAN_POINT('Ctrl Pts',(-0.0805387328308302,1.7878404464921,
6.00089522664238));
#57945=CARTESIAN_POINT('Ctrl Pts',(-0.0700805066005682,1.78542756800238,
6.00162115754897));
#57946=CARTESIAN_POINT('Ctrl Pts',(-0.0677042208196777,1.78490758366534,
6.00178578218591));
#57947=CARTESIAN_POINT('Ctrl Pts',(-0.0572538547405641,1.7827444872967,
6.00250796394472));
#57948=CARTESIAN_POINT('Ctrl Pts',(-0.0491241569203728,1.78138441992741,
6.00306516658279));
#57949=CARTESIAN_POINT('Ctrl Pts',(-0.0298165801534796,1.77891097887452,
6.00436737920277));
#57950=CARTESIAN_POINT('Ctrl Pts',(-0.0186137921955024,1.7780671312962,
6.00510652825681));
#57951=CARTESIAN_POINT('Ctrl Pts',(-0.00636478906222278,1.77778622938642,
6.00588160057922));
#57952=CARTESIAN_POINT('Ctrl Pts',(-0.0053407838913757,1.77776762948839,
6.00594614217272));
#57953=CARTESIAN_POINT('Ctrl Pts',(-0.00357374939333483,1.77774395893557,
6.00605705802779));
#57954=CARTESIAN_POINT('Ctrl Pts',(-0.00283076616661024,1.77773657595665,
6.00610355507108));
#57955=CARTESIAN_POINT('Ctrl Pts',(-0.00177644796941559,1.77772974575061,
6.00616933145193));
#57956=CARTESIAN_POINT('Ctrl Pts',(-0.00146513624856991,1.77772818007296,
6.00618872814567));
#57957=CARTESIAN_POINT('Ctrl Pts',(-0.000929972888969344,1.77772626404852,
6.00622202816027));
#57958=CARTESIAN_POINT('Ctrl Pts',(-0.000706122669313682,1.77772569583411,
6.0062359437676));
#57959=CARTESIAN_POINT('Ctrl Pts',(-0.000277042723912563,1.77772505373371,
6.00626259182007));
#57960=CARTESIAN_POINT('Ctrl Pts',(-7.18138411814191E-5,1.77772494265461,
6.00627532636474));
#57961=CARTESIAN_POINT('Ctrl Pts',(0.000412249114008256,1.77772514304749,
6.00630533652925));
#57962=CARTESIAN_POINT('Ctrl Pts',(0.000691083487634166,1.77772562035113,
6.0063226027857));
#57963=CARTESIAN_POINT('Ctrl Pts',(0.00151654134169048,1.77772810465847,
6.00637365791319));
#57964=CARTESIAN_POINT('Ctrl Pts',(0.00206316422157728,1.77773114052335,
6.00640738942561));
#57965=CARTESIAN_POINT('Ctrl Pts',(0.00692806608651488,1.77777053776774,
6.00670692860615));
#57966=CARTESIAN_POINT('Ctrl Pts',(0.0112454701613375,1.77789230330704,
6.00696806884825));
#57967=CARTESIAN_POINT('Ctrl Pts',(0.0164168488414262,1.77814226794955,
6.00727662576614));
#57968=CARTESIAN_POINT('Ctrl Pts',(0.0172741636417999,1.77818714148329,
6.00732763878128));
#57969=CARTESIAN_POINT('Ctrl Pts',(0.0185942290903376,1.77826152661565,
6.00740598555378));
#57970=CARTESIAN_POINT('Ctrl Pts',(0.0190571062794627,1.77828861177145,
6.00743341947004));
#57971=CARTESIAN_POINT('Ctrl Pts',(0.019972969561048,1.77834418687623,6.00748762836247));
#57972=CARTESIAN_POINT('Ctrl Pts',(0.0204259569467413,1.77837263500097,
6.00751440495122));
#57973=CARTESIAN_POINT('Ctrl Pts',(0.0213271736906037,1.77843114408072,
6.00756760944102));
#57974=CARTESIAN_POINT('Ctrl Pts',(0.0217754032444151,1.77846118546392,
6.00759403804401));
#57975=CARTESIAN_POINT('Ctrl Pts',(0.0529236028462803,1.78061424101814,
6.00942838566713));
#57976=CARTESIAN_POINT('Ctrl Pts',(0.0831638781695995,1.7871224273202,6.01107389418862));
#57977=CARTESIAN_POINT('Ctrl Pts',(0.120068433768491,1.80080384500296,6.01333364628619));
#57978=CARTESIAN_POINT('Ctrl Pts',(0.127989261555435,1.80410559385301,6.01383350366518));
#57979=CARTESIAN_POINT('Ctrl Pts',(0.138838225390564,1.80914508937148,6.01454494020172));
#57980=CARTESIAN_POINT('Ctrl Pts',(0.141885172347559,1.81061923276612,6.01474777655643));
#57981=CARTESIAN_POINT('Ctrl Pts',(0.146193261950573,1.81278792595278,6.01503917722958));
#57982=CARTESIAN_POINT('Ctrl Pts',(0.147473908477938,1.81344338860694,6.01512638915847));
#57983=CARTESIAN_POINT('Ctrl Pts',(0.149429029706652,1.81446063945195,6.01526045566602));
#57984=CARTESIAN_POINT('Ctrl Pts',(0.150106686725002,1.81481629793079,6.01530709500402));
#57985=CARTESIAN_POINT('Ctrl Pts',(0.151218177784307,1.81540470714947,6.01538387702229));
#57986=CARTESIAN_POINT('Ctrl Pts',(0.151652759340992,1.81563604555936,6.01541396973184));
#57987=CARTESIAN_POINT('Ctrl Pts',(0.152491958167897,1.81608524255208,6.01547221991599));
#57988=CARTESIAN_POINT('Ctrl Pts',(0.152896643139389,1.81630297267008,6.015500372781));
#57989=CARTESIAN_POINT('Ctrl Pts',(0.153637709376501,1.81670373010934,6.01555204303792));
#57990=CARTESIAN_POINT('Ctrl Pts',(0.153974233251077,1.81688649313543,6.01557555097874));
#57991=CARTESIAN_POINT('Ctrl Pts',(0.154710508175788,1.8172880583337,6.01562708062456));
#57992=CARTESIAN_POINT('Ctrl Pts',(0.155110122002998,1.81750710920528,6.0156551111789));
#57993=CARTESIAN_POINT('Ctrl Pts',(0.156195902452067,1.81810528517933,6.01573144407577));
#57994=CARTESIAN_POINT('Ctrl Pts',(0.156881149212739,1.81848606572505,6.01577980564082));
#57995=CARTESIAN_POINT('Ctrl Pts',(0.160143880351032,1.82031472509501,6.01601097528115));
#57996=CARTESIAN_POINT('Ctrl Pts',(0.162702683139745,1.82179548642315,6.01619496376859));
#57997=CARTESIAN_POINT('Ctrl Pts',(0.166321641004864,1.8239567559912,6.01645913442091));
#57998=CARTESIAN_POINT('Ctrl Pts',(0.167398791104794,1.82460863213639,6.01653826908407));
#57999=CARTESIAN_POINT('Ctrl Pts',(0.16902587199492,1.82560639178278,6.01665858084509));
#58000=CARTESIAN_POINT('Ctrl Pts',(0.169578631078597,1.82594765918583,6.01669959035282));
#58001=CARTESIAN_POINT('Ctrl Pts',(0.197679134913713,1.84341417103175,6.01879137377047));
#58002=CARTESIAN_POINT('Ctrl Pts',(0.222480638524965,1.86459661297245,6.02100870830197));
#58003=CARTESIAN_POINT('Ctrl Pts',(0.246773618830178,1.89266918962849,6.02350159681502));
#58004=CARTESIAN_POINT('Ctrl Pts',(0.249772337884942,1.89629171369737,6.02381564995278));
#58005=CARTESIAN_POINT('Ctrl Pts',(0.256642968683991,1.90497151389146,6.0245483023688));
#58006=CARTESIAN_POINT('Ctrl Pts',(0.26044657521795,1.9100807629944,6.02496439237164));
#58007=CARTESIAN_POINT('Ctrl Pts',(0.265835920540655,1.91778680039788,6.02556621974879));
#58008=CARTESIAN_POINT('Ctrl Pts',(0.267540171836522,1.92029845616658,6.02575849527237));
#58009=CARTESIAN_POINT('Ctrl Pts',(0.269487578956976,1.92325759520918,6.02598019128351));
#58010=CARTESIAN_POINT('Ctrl Pts',(0.269765399328139,1.92368192889831,6.02601186734955));
#58011=CARTESIAN_POINT('Ctrl Pts',(0.27018759697553,1.92433011352077,6.02606007691514));
#58012=CARTESIAN_POINT('Ctrl Pts',(0.270332698764096,1.92455348805066,6.02607665877204));
#58013=CARTESIAN_POINT('Ctrl Pts',(0.270594917326387,1.92495825366348,6.02610664780295));
#58014=CARTESIAN_POINT('Ctrl Pts',(0.270712128305197,1.92513958185835,6.02612006128768));
#58015=CARTESIAN_POINT('Ctrl Pts',(0.270949306270022,1.9255073119196,6.0261472208323));
#58016=CARTESIAN_POINT('Ctrl Pts',(0.271069262646378,1.92569371895769,6.026160966173));
#58017=CARTESIAN_POINT('Ctrl Pts',(0.271413305684466,1.92622956108312,6.02620041505129));
#58018=CARTESIAN_POINT('Ctrl Pts',(0.271636910702271,1.92657930719593,6.02622608635646));
#58019=CARTESIAN_POINT('Ctrl Pts',(0.272610473426049,1.92810858333926,6.02633800306861));
#58020=CARTESIAN_POINT('Ctrl Pts',(0.273353443216009,1.92929257604979,6.02642379039984));
#58021=CARTESIAN_POINT('Ctrl Pts',(0.287073461453989,1.95147599294181,6.02801585110701));
#58022=CARTESIAN_POINT('Ctrl Pts',(0.297605399935614,1.97389683781789,6.0293748431283));
#58023=CARTESIAN_POINT('Ctrl Pts',(0.31008047671043,2.01100449842006,6.03156493642414));
#58024=CARTESIAN_POINT('Ctrl Pts',(0.313759281967147,2.02499885855254,6.03237789128311));
#58025=CARTESIAN_POINT('Ctrl Pts',(0.318105113879117,2.04761754092978,6.03371481961574));
#58026=CARTESIAN_POINT('Ctrl Pts',(0.31938672821074,2.05610371082636,6.03422120728117));
#58027=CARTESIAN_POINT('Ctrl Pts',(0.32051292859904,2.06630325241381,6.03483981821183));
#58028=CARTESIAN_POINT('Ctrl Pts',(0.320684530268572,2.06797750667553,6.0349416777637));
#58029=CARTESIAN_POINT('Ctrl Pts',(0.320923811497116,2.07050730269682,6.03509609153991));
#58030=CARTESIAN_POINT('Ctrl Pts',(0.321001202462517,2.07136191390072,6.03514834202492));
#58031=CARTESIAN_POINT('Ctrl Pts',(0.32112098689032,2.07274619760191,6.03523312052977));
#58032=CARTESIAN_POINT('Ctrl Pts',(0.321165485515884,2.07327568757455,6.0352655825102));
#58033=CARTESIAN_POINT('Ctrl Pts',(0.321248311683141,2.0742913306554,6.03532791598354));
#58034=CARTESIAN_POINT('Ctrl Pts',(0.321286845675813,2.07477746582335,6.0353577809155));
#58035=CARTESIAN_POINT('Ctrl Pts',(0.321353853909911,2.07564790153094,6.03541130761905));
#58036=CARTESIAN_POINT('Ctrl Pts',(0.321382742606543,2.07603216999382,6.03543495632493));
#58037=CARTESIAN_POINT('Ctrl Pts',(0.321438830393111,2.07679656964346,6.03548203616105));
#58038=CARTESIAN_POINT('Ctrl Pts',(0.321466044554084,2.07717669915171,6.03550546677965));
#58039=CARTESIAN_POINT('Ctrl Pts',(0.321530664410971,2.07810236367373,6.03556256811849));
#58040=CARTESIAN_POINT('Ctrl Pts',(0.321567355950908,2.07864794590456,6.03559626120986));
#58041=CARTESIAN_POINT('Ctrl Pts',(0.321700661992337,2.08070844703493,6.03572365460019));
#58042=CARTESIAN_POINT('Ctrl Pts',(0.321787959928929,2.0822239301215,6.03581764676955));
#58043=CARTESIAN_POINT('Ctrl Pts',(0.323158692612482,2.10935732344249,6.03750593866038));
#58044=CARTESIAN_POINT('Ctrl Pts',(0.321389671727212,2.13503189134735,6.03920166358152));
#58045=CARTESIAN_POINT('Ctrl Pts',(0.313724772733462,2.17532928979751,6.04197348407867));
#58046=CARTESIAN_POINT('Ctrl Pts',(0.309772761142307,2.19021420937721,6.04301977850816));
#58047=CARTESIAN_POINT('Ctrl Pts',(0.30226002210517,2.21207054388735,6.04454815713027));
#58048=CARTESIAN_POINT('Ctrl Pts',(0.299484852913449,2.21928860857097,6.04505129930937));
#58049=CARTESIAN_POINT('Ctrl Pts',(0.295814209527044,2.22789752806881,6.04564372284205));
#58050=CARTESIAN_POINT('Ctrl Pts',(0.295164552344143,2.2293897660107,6.04574612443588));
#58051=CARTESIAN_POINT('Ctrl Pts',(0.294333279016621,2.23126032299449,6.04587406658077));
#58052=CARTESIAN_POINT('Ctrl Pts',(0.29416220613545,2.23164326042592,6.04590023639711));
#58053=CARTESIAN_POINT('Ctrl Pts',(0.293889111114884,2.23225137846412,6.04594175823122));
#58054=CARTESIAN_POINT('Ctrl Pts',(0.293787577336947,2.23247677585536,6.04595714015285));
#58055=CARTESIAN_POINT('Ctrl Pts',(0.293595663647149,2.2329015041803,6.04598610965021));
#58056=CARTESIAN_POINT('Ctrl Pts',(0.293505340767425,2.23310085825089,6.04599970054055));
#58057=CARTESIAN_POINT('Ctrl Pts',(0.29329962404224,2.23355367355041,6.04603055651584));
#58058=CARTESIAN_POINT('Ctrl Pts',(0.293184104910394,2.2338070768361,6.04604781372093));
#58059=CARTESIAN_POINT('Ctrl Pts',(0.292832826822641,2.23457500315665,6.04610008043174));
#58060=CARTESIAN_POINT('Ctrl Pts',(0.292596039246178,2.23508905865577,6.04613502670821));
#58061=CARTESIAN_POINT('Ctrl Pts',(0.290924605397629,2.23869265675996,6.0463797318912));
#58062=CARTESIAN_POINT('Ctrl Pts',(0.289442341057997,2.24176005259815,6.0465866157625));
#58063=CARTESIAN_POINT('Ctrl Pts',(0.276673061714968,2.26714910657841,6.04829189798559));
#58064=CARTESIAN_POINT('Ctrl Pts',(0.262869620789346,2.28811362617499,6.04965855111715));
#58065=CARTESIAN_POINT('Ctrl Pts',(0.232677628683257,2.32406013908515,6.05229237088171));
#58066=CARTESIAN_POINT('Ctrl Pts',(0.216903551347983,2.33936261254836,6.05354461256304));
#58067=CARTESIAN_POINT('Ctrl Pts',(0.19895236730321,2.35353508372282,6.05493302203375));
#58068=CARTESIAN_POINT('Ctrl Pts',(0.198202064817772,2.35412206634907,6.05499098159017));
#58069=CARTESIAN_POINT('Ctrl Pts',(0.196998069755074,2.35505540952141,6.05508387928737));
#58070=CARTESIAN_POINT('Ctrl Pts',(0.196546036534835,2.35540390938515,6.05511873285867));
#58071=CARTESIAN_POINT('Ctrl Pts',(0.195683308370511,2.356065392192,6.05518520761916));
#58072=CARTESIAN_POINT('Ctrl Pts',(0.195272781971566,2.35637859284553,6.05521682010577));
#58073=CARTESIAN_POINT('Ctrl Pts',(0.194551285978017,2.35692630158305,6.05527234572342));
#58074=CARTESIAN_POINT('Ctrl Pts',(0.194240639878214,2.35716123568374,6.05529624205379));
#58075=CARTESIAN_POINT('Ctrl Pts',(0.193633016628128,2.35761903726646,6.05534296276148));
#58076=CARTESIAN_POINT('Ctrl Pts',(0.193336078578046,2.3578419558739,6.0553657850865));
#58077=CARTESIAN_POINT('Ctrl Pts',(0.192630003943509,2.35837011780096,6.05542003100266));
#58078=CARTESIAN_POINT('Ctrl Pts',(0.192220527000308,2.3586749025064,6.05545147243882));
#58079=CARTESIAN_POINT('Ctrl Pts',(0.190772753070647,2.35974718367091,6.05556257812688));
#58080=CARTESIAN_POINT('Ctrl Pts',(0.189730580083967,2.3605094041341,6.05564244714957));
#58081=CARTESIAN_POINT('Ctrl Pts',(0.173247512178866,2.37241335235415,6.0569040280374));
#58082=CARTESIAN_POINT('Ctrl Pts',(0.15685648537718,2.382169353956,6.05813960272788));
#58083=CARTESIAN_POINT('Ctrl Pts',(0.119684304392901,2.40005053932184,6.06089426569416));
#58084=CARTESIAN_POINT('Ctrl Pts',(0.098724491135488,2.40758428832935,6.06241991181727));
#58085=CARTESIAN_POINT('Ctrl Pts',(0.0710101032122141,2.41441822708487,
6.06430826499847));
#58086=CARTESIAN_POINT('Ctrl Pts',(0.0648195163537652,2.41575258956753,
6.06472174196745));
#58087=CARTESIAN_POINT('Ctrl Pts',(0.05567603529061,2.41744315343383,6.0653165470208));
#58088=CARTESIAN_POINT('Ctrl Pts',(0.0527514027849231,2.4179422394241,6.0655044342247));
#58089=CARTESIAN_POINT('Ctrl Pts',(0.0493221151375749,2.41847881988596,
6.06572165091937));
#58090=CARTESIAN_POINT('Ctrl Pts',(0.0488238733228427,2.41855558252769,
6.06575313424284));
#58091=CARTESIAN_POINT('Ctrl Pts',(0.0480627397245179,2.41867102045701,
6.06580111103935));
#58092=CARTESIAN_POINT('Ctrl Pts',(0.0477999797004034,2.41871053978619,
6.06581765215867));
#58093=CARTESIAN_POINT('Ctrl Pts',(0.0473425580156136,2.41877875798385,
6.0658464096939));
#58094=CARTESIAN_POINT('Ctrl Pts',(0.0471479194930042,2.41880760346854,
6.06585863444783));
#58095=CARTESIAN_POINT('Ctrl Pts',(0.0467072948921429,2.41887249181483,
6.06588628192731));
#58096=CARTESIAN_POINT('Ctrl Pts',(0.0464612939664794,2.41890842823027,
6.06590169850582));
#58097=CARTESIAN_POINT('Ctrl Pts',(0.0457939625917339,2.41900512507688,
6.06594346836437));
#58098=CARTESIAN_POINT('Ctrl Pts',(0.045372551070656,2.41906533570641,6.06596979041004));
#58099=CARTESIAN_POINT('Ctrl Pts',(0.0434736757502484,2.41933280599869,
6.06608815407462));
#58100=CARTESIAN_POINT('Ctrl Pts',(0.0419948721830814,2.41953064388627,
6.06617967033556));
#58101=CARTESIAN_POINT('Ctrl Pts',(0.00853123491329284,2.4237711584285,
6.0682366874628));
#58102=CARTESIAN_POINT('Ctrl Pts',(-0.0238853703800827,2.42300288438291,
6.06995659374557));
#58103=CARTESIAN_POINT('Ctrl Pts',(-0.072591374857377,2.41446366609711,
6.07276110104687));
#58104=CARTESIAN_POINT('Ctrl Pts',(-0.0892624662103829,2.41014349417944,
6.07375989293959));
#58105=CARTESIAN_POINT('Ctrl Pts',(-0.106618269922248,2.40413007230692,
6.07487666012262));
#58106=CARTESIAN_POINT('Ctrl Pts',(-0.107726438239217,2.40373931390203,
6.07494830081459));
#58107=CARTESIAN_POINT('Ctrl Pts',(-0.109332175599828,2.40316321164182,
6.0750526042093));
#58108=CARTESIAN_POINT('Ctrl Pts',(-0.109831471566688,2.40298268162148,
6.07508510669631));
#58109=CARTESIAN_POINT('Ctrl Pts',(-0.110703619843708,2.40266490056629,
6.07514200375382));
#58110=CARTESIAN_POINT('Ctrl Pts',(-0.111076669707779,2.40252819195184,
6.07516638019371));
#58111=CARTESIAN_POINT('Ctrl Pts',(-0.111798115605101,2.40226229510442,
6.0752135989404));
#58112=CARTESIAN_POINT('Ctrl Pts',(-0.112146543078011,2.40213319342386,
6.07523643832512));
#58113=CARTESIAN_POINT('Ctrl Pts',(-0.112974078990658,2.40182494055626,
6.07529076623788));
#58114=CARTESIAN_POINT('Ctrl Pts',(-0.113452984627335,2.40164525114762,
6.07532227273767));
#58115=CARTESIAN_POINT('Ctrl Pts',(-0.115145050046982,2.40100577442701,
6.07543382708968));
#58116=CARTESIAN_POINT('Ctrl Pts',(-0.116355846731803,2.40053980708236,
6.07551408189172));
#58117=CARTESIAN_POINT('Ctrl Pts',(-0.136351290076403,2.39270574499538,
6.07684665428916));
#58118=CARTESIAN_POINT('Ctrl Pts',(-0.154402304294605,2.38359827180811,
6.07815981129278));
#58119=CARTESIAN_POINT('Ctrl Pts',(-0.180215954593104,2.36737580437865,
6.08020128533362));
#58120=CARTESIAN_POINT('Ctrl Pts',(-0.188682130013069,2.36147017666878,
6.08089989494506));
#58121=CARTESIAN_POINT('Ctrl Pts',(-0.205208739096896,2.3487207126804,6.08231211659649));
#58122=CARTESIAN_POINT('Ctrl Pts',(-0.213245753435008,2.34186543318844,
6.08302486799576));
#58123=CARTESIAN_POINT('Ctrl Pts',(-0.227032239669349,2.32888369114118,
6.08427850967839));
#58124=CARTESIAN_POINT('Ctrl Pts',(-0.232906681989655,2.32290331266854,
6.08482398972139));
#58125=CARTESIAN_POINT('Ctrl Pts',(-0.239422553371044,2.31573069357209,
6.08543567064522));
#58126=CARTESIAN_POINT('Ctrl Pts',(-0.240297375151487,2.31475582144961,
6.08551793974294));
#58127=CARTESIAN_POINT('Ctrl Pts',(-0.241423824373539,2.31348504264521,
6.08562402943166));
#58128=CARTESIAN_POINT('Ctrl Pts',(-0.241680878315509,2.31319399491729,
6.08564824966583));
#58129=CARTESIAN_POINT('Ctrl Pts',(-0.242096118861859,2.31272212525919,
6.08568739099263));
#58130=CARTESIAN_POINT('Ctrl Pts',(-0.242254629426003,2.31254159090714,
6.08570233636578));
#58131=CARTESIAN_POINT('Ctrl Pts',(-0.242558253511869,2.31219499973033,
6.08573097111408));
#58132=CARTESIAN_POINT('Ctrl Pts',(-0.242703398001503,2.31202897173744,
6.08574466278412));
#58133=CARTESIAN_POINT('Ctrl Pts',(-0.243036808975878,2.31164679839394,
6.08577612131313));
#58134=CARTESIAN_POINT('Ctrl Pts',(-0.243224958136835,2.3114305501304,6.08579387935271));
#58135=CARTESIAN_POINT('Ctrl Pts',(-0.243806779978318,2.31076003178779,
6.08584881138185));
#58136=CARTESIAN_POINT('Ctrl Pts',(-0.244199473255355,2.31030490778423,
6.08588591275705));
#58137=CARTESIAN_POINT('Ctrl Pts',(-0.247432273563176,2.30653689024694,
6.08619158415615));
#58138=CARTESIAN_POINT('Ctrl Pts',(-0.250206267961081,2.30316752958681,
6.08645540300492));
#58139=CARTESIAN_POINT('Ctrl Pts',(-0.253417410859009,2.29910162918703,
6.08676407404153));
#58140=CARTESIAN_POINT('Ctrl Pts',(-0.25392125269123,2.29845866151078,6.08681260498745));
#58141=CARTESIAN_POINT('Ctrl Pts',(-0.254498918147973,2.29771568406699,
6.0868683705174));
#58142=CARTESIAN_POINT('Ctrl Pts',(-0.25457513041202,2.29761754486977,6.08687573024442));
#58143=CARTESIAN_POINT('Ctrl Pts',(-0.254837199113164,2.2972796735276,6.08690104660015));
#58144=CARTESIAN_POINT('Ctrl Pts',(-0.255022774353042,2.29703972239507,
6.08691898860585));
#58145=CARTESIAN_POINT('Ctrl Pts',(-0.272519743352753,2.27434979452356,
6.08861211490864));
#58146=CARTESIAN_POINT('Ctrl Pts',(-0.286795492931976,2.24971173398175,
6.09013876506786));
#58147=CARTESIAN_POINT('Ctrl Pts',(-0.304046051141138,2.2081408845776,6.09269533336683));
#58148=CARTESIAN_POINT('Ctrl Pts',(-0.309225792538832,2.19229160802325,
6.09366408858299));
#58149=CARTESIAN_POINT('Ctrl Pts',(-0.313434583055251,2.1749754102828,6.09474757643626));
#58150=CARTESIAN_POINT('Ctrl Pts',(-0.313705243810199,2.17383474758697,
6.09481905284651));
#58151=CARTESIAN_POINT('Ctrl Pts',(-0.314089316520008,2.17217588399112,
6.09492316056475));
#58152=CARTESIAN_POINT('Ctrl Pts',(-0.314207684440214,2.17165883068618,
6.09495563250657));
#58153=CARTESIAN_POINT('Ctrl Pts',(-0.314412462385804,2.17075405933997,
6.09501249404458));
#58154=CARTESIAN_POINT('Ctrl Pts',(-0.314499433304771,2.17036646833032,
6.09503686557836));
#58155=CARTESIAN_POINT('Ctrl Pts',(-0.314666401092002,2.16961587333682,
6.09508408791751));
#58156=CARTESIAN_POINT('Ctrl Pts',(-0.314746486996248,2.16925288960298,
6.09510693582506));
#58157=CARTESIAN_POINT('Ctrl Pts',(-0.31493539689231,2.16838957220406,6.09516130464812));
#58158=CARTESIAN_POINT('Ctrl Pts',(-0.315043656579309,2.167889117289,6.09519284359864));
#58159=CARTESIAN_POINT('Ctrl Pts',(-0.315422653256835,2.16611668967211,
6.09530462216546));
#58160=CARTESIAN_POINT('Ctrl Pts',(-0.3156868805191,2.1648433514663,6.09538506982508));
#58161=CARTESIAN_POINT('Ctrl Pts',(-0.320174180133562,2.14254089876369,
6.09679672931513));
#58162=CARTESIAN_POINT('Ctrl Pts',(-0.322294390262843,2.12114782869986,
6.0981971628962));
#58163=CARTESIAN_POINT('Ctrl Pts',(-0.322252498381139,2.07514179083036,
6.10128594209211));
#58164=CARTESIAN_POINT('Ctrl Pts',(-0.319421715827119,2.05065997744838,
6.10297727197978));
#58165=CARTESIAN_POINT('Ctrl Pts',(-0.313587547175297,2.02566810382857,
6.10463535462289));
#58166=CARTESIAN_POINT('Ctrl Pts',(-0.313332547194403,2.02460042792881,
6.10470604126003));
#58167=CARTESIAN_POINT('Ctrl Pts',(-0.312278628154533,2.02028540029798,
6.10499106618463));
#58168=CARTESIAN_POINT('Ctrl Pts',(-0.311434605938142,2.01704912657215,
6.10520332941835));
#58169=CARTESIAN_POINT('Ctrl Pts',(-0.310391688961403,2.01329080772112,
6.10544760274731));
#58170=CARTESIAN_POINT('Ctrl Pts',(-0.310241670753992,2.01275557129131,
6.10548233755754));
#58171=CARTESIAN_POINT('Ctrl Pts',(-0.310013924409518,2.01195103147772,
6.10553446640724));
#58172=CARTESIAN_POINT('Ctrl Pts',(-0.309937229503655,2.01168144048583,
6.10555192012439));
#58173=CARTESIAN_POINT('Ctrl Pts',(-0.309799968195203,2.0112013326895,6.10558297764037));
#58174=CARTESIAN_POINT('Ctrl Pts',(-0.309739538902464,2.01099077771695,
6.10559658943409));
#58175=CARTESIAN_POINT('Ctrl Pts',(-0.309610757202732,2.01054378039886,
6.10562546793786));
#58176=CARTESIAN_POINT('Ctrl Pts',(-0.309542348802191,2.0103073553742,6.10564073127614));
#58177=CARTESIAN_POINT('Ctrl Pts',(-0.309357993143648,2.00967293013661,
6.10568166003039));
#58178=CARTESIAN_POINT('Ctrl Pts',(-0.309241548198942,2.00927507319344,
6.10570729632664));
#58179=CARTESIAN_POINT('Ctrl Pts',(-0.308679484388917,2.00736832693394,
6.1058300169887));
#58180=CARTESIAN_POINT('Ctrl Pts',(-0.308223577986725,2.00586245622988,
6.10592650888078));
#58181=CARTESIAN_POINT('Ctrl Pts',(-0.304339793046374,1.99336496555509,
6.10672421156539));
#58182=CARTESIAN_POINT('Ctrl Pts',(-0.300335754018257,1.98255964340394,
6.10739400217946));
#58183=CARTESIAN_POINT('Ctrl Pts',(-0.288099967351573,1.95428924479531,
6.10914954923612));
#58184=CARTESIAN_POINT('Ctrl Pts',(-0.278864724840168,1.93731094009641,
6.11020925435597));
#58185=CARTESIAN_POINT('Ctrl Pts',(-0.257997196607783,1.90600307688698,
6.11233577532785));
#58186=CARTESIAN_POINT('Ctrl Pts',(-0.246546215926454,1.89164411839782,
6.11339596981487));
#58187=CARTESIAN_POINT('Ctrl Pts',(-0.233053395332642,1.87740407849933,
6.11458755156693));
#58188=CARTESIAN_POINT('Ctrl Pts',(-0.232163328989578,1.8764759119415,6.11466590073906));
#58189=CARTESIAN_POINT('Ctrl Pts',(-0.230912850802078,1.87518743223455,
6.11477563323072));
#58190=CARTESIAN_POINT('Ctrl Pts',(-0.230557095112029,1.87482260064643,
6.11480681337896));
#58191=CARTESIAN_POINT('Ctrl Pts',(-0.229940785522465,1.87419355971777,
6.11486076451862));
#58192=CARTESIAN_POINT('Ctrl Pts',(-0.229680637073817,1.87392895304547,
6.11488351769808));
#58193=CARTESIAN_POINT('Ctrl Pts',(-0.229140783950723,1.87338174200713,
6.11493069355465));
#58194=CARTESIAN_POINT('Ctrl Pts',(-0.228861012213215,1.87309920491146,
6.11495511916866));
#58195=CARTESIAN_POINT('Ctrl Pts',(-0.228205124685474,1.87243928156132,
6.11501232932334));
#58196=CARTESIAN_POINT('Ctrl Pts',(-0.227828595302568,1.87206230968517,
6.11504513214394));
#58197=CARTESIAN_POINT('Ctrl Pts',(-0.226611480104256,1.87084979286035,
6.11515103813267));
#58198=CARTESIAN_POINT('Ctrl Pts',(-0.225767226719683,1.87001795803512,
6.11522430445236));
#58199=CARTESIAN_POINT('Ctrl Pts',(-0.223792376335082,1.86809351035422,
6.11539524481828));
#58200=CARTESIAN_POINT('Ctrl Pts',(-0.222658341224862,1.86700448376102,
6.11549307299862));
#58201=CARTESIAN_POINT('Ctrl Pts',(-0.210819650012635,1.85580101924174,
6.11651101464629));
#58202=CARTESIAN_POINT('Ctrl Pts',(-0.199443175942011,1.84642480858418,
6.11746246721005));
#58203=CARTESIAN_POINT('Ctrl Pts',(-0.162347505265138,1.81989616912389,
6.12048368240245));
#58204=CARTESIAN_POINT('Ctrl Pts',(-0.134778971525478,1.80563739888518,
6.12263443974411));
#58205=CARTESIAN_POINT('Ctrl Pts',(-0.10231325515177,1.79437717859305,6.12484157555323));
#58206=CARTESIAN_POINT('Ctrl Pts',(-0.0990035264729396,1.79328903617023,
6.12506282975967));
#58207=CARTESIAN_POINT('Ctrl Pts',(-0.0951324524187147,1.79208553640912,
6.12531673954882));
#58208=CARTESIAN_POINT('Ctrl Pts',(-0.094587809726223,1.79191779237569,
6.12535235206415));
#58209=CARTESIAN_POINT('Ctrl Pts',(-0.0937755978687378,1.79166999681326,
6.12540529116005));
#58210=CARTESIAN_POINT('Ctrl Pts',(-0.0935083686859163,1.79158884811361,
6.12542268166413));
#58211=CARTESIAN_POINT('Ctrl Pts',(-0.0930314525777255,1.79144470123993,
6.12545366904471));
#58212=CARTESIAN_POINT('Ctrl Pts',(-0.0928218071158267,1.79138156943168,
6.12546727377751));
#58213=CARTESIAN_POINT('Ctrl Pts',(-0.0923757752453353,1.79124774875767,
6.12549618258839));
#58214=CARTESIAN_POINT('Ctrl Pts',(-0.0921393726370167,1.79117711789698,
6.12551148320236));
#58215=CARTESIAN_POINT('Ctrl Pts',(-0.0915029618571355,1.79098777096134,
6.12555261636274));
#58216=CARTESIAN_POINT('Ctrl Pts',(-0.0911028021387213,1.79086955961731,
6.12557841928132));
#58217=CARTESIAN_POINT('Ctrl Pts',(-0.0891639944751465,1.7903009072697,
6.12570314829454));
#58218=CARTESIAN_POINT('Ctrl Pts',(-0.087622194656767,1.78986116463411,
6.12580145817532));
#58219=CARTESIAN_POINT('Ctrl Pts',(-0.0745794032770317,1.78624620892881,
6.12662620682416));
#58220=CARTESIAN_POINT('Ctrl Pts',(-0.0629121295655456,1.78370004582771,
6.12731893360064));
#58221=CARTESIAN_POINT('Ctrl Pts',(-0.01967727693028,1.77675280710321,6.12981034467774));
#58222=CARTESIAN_POINT('Ctrl Pts',(0.0123483058771805,1.77638983346874,
6.13152979185127));
#58223=CARTESIAN_POINT('Ctrl Pts',(0.0496733722488915,1.78152299729853,
6.13376209380974));
#58224=CARTESIAN_POINT('Ctrl Pts',(0.0554160184057503,1.78247188550634,
6.13411136692855));
#58225=CARTESIAN_POINT('Ctrl Pts',(0.062098464152659,1.78376285768748,6.1345257013214));
#58226=CARTESIAN_POINT('Ctrl Pts',(0.0630664904390666,1.78395448559134,
6.13458591669315));
#58227=CARTESIAN_POINT('Ctrl Pts',(0.0645247807302468,1.78425013149964,
6.13467692719652));
#58228=CARTESIAN_POINT('Ctrl Pts',(0.0650157133332328,1.78435085331722,
6.13470761695353));
#58229=CARTESIAN_POINT('Ctrl Pts',(0.0658912836991643,1.78453261837151,
6.13476244364955));
#58230=CARTESIAN_POINT('Ctrl Pts',(0.0662760127161906,1.78461322114691,
6.13478656645093));
#58231=CARTESIAN_POINT('Ctrl Pts',(0.0670872480887549,1.78478472920762,
6.13483749890691));
#58232=CARTESIAN_POINT('Ctrl Pts',(0.0675137190157128,1.78487579664753,
6.13486431371254));
#58233=CARTESIAN_POINT('Ctrl Pts',(0.0686407959578311,1.78511886257096,
6.13493528455893));
#58234=CARTESIAN_POINT('Ctrl Pts',(0.0693410789654432,1.7852723330672,6.13497948772036));
#58235=CARTESIAN_POINT('Ctrl Pts',(0.0725210370095364,1.78598036502446,
6.13518070432379));
#58236=CARTESIAN_POINT('Ctrl Pts',(0.0749945575184244,1.78656189174418,
6.13533858148531));
#58237=CARTESIAN_POINT('Ctrl Pts',(0.0857612650868999,1.78922789448097,
6.13603191459942));
#58238=CARTESIAN_POINT('Ctrl Pts',(0.0939758539606996,1.7916125603886,6.13657697597359));
#58239=CARTESIAN_POINT('Ctrl Pts',(0.11574516496817,1.79888269075009,6.1380659913772));
#58240=CARTESIAN_POINT('Ctrl Pts',(0.129082476472,1.80435458012504,6.1390266835851));
#58241=CARTESIAN_POINT('Ctrl Pts',(0.1584904971171,1.81878998915011,6.14123700957637));
#58242=CARTESIAN_POINT('Ctrl Pts',(0.174251876602522,1.82827469863625,6.14249019169553));
#58243=CARTESIAN_POINT('Ctrl Pts',(0.190264851916607,1.83987991184667,6.14378919008863));
#58244=CARTESIAN_POINT('Ctrl Pts',(0.191404076532268,1.84071703923454,6.14388174293532));
#58245=CARTESIAN_POINT('Ctrl Pts',(0.193569150051231,1.84233002906218,6.14405784722488));
#58246=CARTESIAN_POINT('Ctrl Pts',(0.19459593395165,1.84310458867143,6.14414145571172));
#58247=CARTESIAN_POINT('Ctrl Pts',(0.195905010449885,1.84410444928828,6.14424814021547));
#58248=CARTESIAN_POINT('Ctrl Pts',(0.196191584954809,1.84432409580013,6.14427150043006));
#58249=CARTESIAN_POINT('Ctrl Pts',(0.197079354728163,1.84500690300454,6.14434388296792));
#58250=CARTESIAN_POINT('Ctrl Pts',(0.197679288094204,1.84547170951711,6.14439281972307));
#58251=CARTESIAN_POINT('Ctrl Pts',(0.201200631414062,1.84821987798304,6.14468016220897));
#58252=CARTESIAN_POINT('Ctrl Pts',(0.204084254296424,1.85055152035375,6.1449158970472));
#58253=CARTESIAN_POINT('Ctrl Pts',(0.2073723218429,1.8533053852159,6.14518457005795));
#58254=CARTESIAN_POINT('Ctrl Pts',(0.207816497727555,1.8536794443926,6.1452208616136));
#58255=CARTESIAN_POINT('Ctrl Pts',(0.208474439840365,1.85423657155294,6.14527461177801));
#58256=CARTESIAN_POINT('Ctrl Pts',(0.208688978099588,1.85441871966698,6.14529213719708));
#58257=CARTESIAN_POINT('Ctrl Pts',(0.209066299364539,1.85473992593625,6.1453229577456));
#58258=CARTESIAN_POINT('Ctrl Pts',(0.209229182371642,1.85487886524237,6.14533626161611));
#58259=CARTESIAN_POINT('Ctrl Pts',(0.209573492832958,1.85517315552479,6.14536438216025));
#58260=CARTESIAN_POINT('Ctrl Pts',(0.209754885581102,1.8553285454949,6.14537919582944));
#58261=CARTESIAN_POINT('Ctrl Pts',(0.210126415708694,1.85564753334101,6.14540953555669));
#58262=CARTESIAN_POINT('Ctrl Pts',(0.210316535243675,1.85581115188232,6.14542506006956));
#58263=CARTESIAN_POINT('Ctrl Pts',(0.210787480414418,1.85621740943749,6.14546351406734));
#58264=CARTESIAN_POINT('Ctrl Pts',(0.211068079185067,1.85646031265279,6.14548642417412));
#58265=CARTESIAN_POINT('Ctrl Pts',(0.211848953993099,1.85713864821505,6.14555017808704));
#58266=CARTESIAN_POINT('Ctrl Pts',(0.21234830987487,1.85757514399296,6.14559094492608));
#58267=CARTESIAN_POINT('Ctrl Pts',(0.216774543820778,1.86146836270738,6.14595231101492));
#58268=CARTESIAN_POINT('Ctrl Pts',(0.22061832218819,1.86501891950113,6.14626622065885));
#58269=CARTESIAN_POINT('Ctrl Pts',(0.228919635561087,1.87307033490035,6.1469489179583));
#58270=CARTESIAN_POINT('Ctrl Pts',(0.233334411963596,1.87761220020752,6.14731522148948));
#58271=CARTESIAN_POINT('Ctrl Pts',(0.257402471648043,1.90387949229667,6.1493507933882));
#58272=CARTESIAN_POINT('Ctrl Pts',(0.274154946726946,1.92807422356698,6.15093270075099));
#58273=CARTESIAN_POINT('Ctrl Pts',(0.291601912712039,1.96246667060929,6.15318173199054));
#58274=CARTESIAN_POINT('Ctrl Pts',(0.295436405075282,1.97090934319422,6.15373250469504));
#58275=CARTESIAN_POINT('Ctrl Pts',(0.29932781992931,1.98056243536318,6.15436545921748));
#58276=CARTESIAN_POINT('Ctrl Pts',(0.299748500421382,1.9816221639291,6.15443498552988));
#58277=CARTESIAN_POINT('Ctrl Pts',(0.300352383037549,1.98316725316324,6.15453642074973));
#58278=CARTESIAN_POINT('Ctrl Pts',(0.300540053984974,1.98365086731954,6.15456817935076));
#58279=CARTESIAN_POINT('Ctrl Pts',(0.300869216756015,1.98450520578921,6.15462430037405));
#58280=CARTESIAN_POINT('Ctrl Pts',(0.301011193422248,1.98487574315788,6.15464864647198));
#58281=CARTESIAN_POINT('Ctrl Pts',(0.301303327870427,1.98564240427087,6.15469903201226));
#58282=CARTESIAN_POINT('Ctrl Pts',(0.301453389587099,1.98603856358196,6.15472507461606));
#58283=CARTESIAN_POINT('Ctrl Pts',(0.301835614107753,1.98705366464322,6.15479182281734));
#58284=CARTESIAN_POINT('Ctrl Pts',(0.302066653615032,1.98767302471025,6.15483256588615));
#58285=CARTESIAN_POINT('Ctrl Pts',(0.303002421146999,1.99020535305112,6.15499922122754));
#58286=CARTESIAN_POINT('Ctrl Pts',(0.303690883495235,1.99212424417632,6.15512567438918));
#58287=CARTESIAN_POINT('Ctrl Pts',(0.314693320219725,2.02373064189522,6.15721161241558));
#58288=CARTESIAN_POINT('Ctrl Pts',(0.320626025351641,2.05475741142396,6.15932935833572));
#58289=CARTESIAN_POINT('Ctrl Pts',(0.322723830933223,2.1034948798078,6.16262606891827));
#58290=CARTESIAN_POINT('Ctrl Pts',(0.322066676492338,2.12088300378392,6.16379047740456));
#58291=CARTESIAN_POINT('Ctrl Pts',(0.319883851859226,2.1392000871647,6.16495250446753));
#58292=CARTESIAN_POINT('Ctrl Pts',(0.319751645760659,2.14026425988876,6.16501977621116));
#58293=CARTESIAN_POINT('Ctrl Pts',(0.319566238746471,2.14169813111846,6.16511007812119));
#58294=CARTESIAN_POINT('Ctrl Pts',(0.319517705201432,2.14206841037539,6.16513336682239));
#58295=CARTESIAN_POINT('Ctrl Pts',(0.319440442900471,2.14265002404014,6.16516989835721));
#58296=CARTESIAN_POINT('Ctrl Pts',(0.319412147986425,2.14286141423722,6.16518316573174));
#58297=CARTESIAN_POINT('Ctrl Pts',(0.319354886969042,2.14328600335469,6.16520979333015));
#58298=CARTESIAN_POINT('Ctrl Pts',(0.319325917435808,2.14349919966461,6.16522315317109));
#58299=CARTESIAN_POINT('Ctrl Pts',(0.319259276128592,2.14398598069271,6.16525363326509));
#58300=CARTESIAN_POINT('Ctrl Pts',(0.319221466239346,2.14425954569449,6.16527074556021));
#58301=CARTESIAN_POINT('Ctrl Pts',(0.319141430067438,2.14483319161268,6.16530659346751));
#58302=CARTESIAN_POINT('Ctrl Pts',(0.319099132057455,2.14513326242987,6.16532532501048));
#58303=CARTESIAN_POINT('Ctrl Pts',(0.318986495932055,2.14592425269514,6.16537464913859));
#58304=CARTESIAN_POINT('Ctrl Pts',(0.318915447437252,2.14641507261807,6.16540520212951));
#58305=CARTESIAN_POINT('Ctrl Pts',(0.31869904851986,2.14788605147193,6.16549661438319));
#58306=CARTESIAN_POINT('Ctrl Pts',(0.318550308793114,2.14886571680875,6.16555728870091));
#58307=CARTESIAN_POINT('Ctrl Pts',(0.316763054360369,2.16028230868027,6.16626212187127));
#58308=CARTESIAN_POINT('Ctrl Pts',(0.314616609181587,2.17063447073129,6.16687947007845));
#58309=CARTESIAN_POINT('Ctrl Pts',(0.30490258971354,2.20811040165076,6.16909479674247));
#58310=CARTESIAN_POINT('Ctrl Pts',(0.29430119535565,2.23431449233291,6.17061649384455));
#58311=CARTESIAN_POINT('Ctrl Pts',(0.27945710958026,2.26052661951239,6.17236261068925));
#58312=CARTESIAN_POINT('Ctrl Pts',(0.27846870563566,2.26223517324694,6.17247746389227));
#58313=CARTESIAN_POINT('Ctrl Pts',(0.276159650424283,2.26614332683492,6.17274269964716));
#58314=CARTESIAN_POINT('Ctrl Pts',(0.274828315617226,2.26833643102073,6.1728934014094));
#58315=CARTESIAN_POINT('Ctrl Pts',(0.27007960422049,2.27595245969209,6.17342366610002));
#58316=CARTESIAN_POINT('Ctrl Pts',(0.266526930772546,2.28128885006375,6.17380768783157));
#58317=CARTESIAN_POINT('Ctrl Pts',(0.262222287329415,2.28735449304122,6.17426038829708));
#58318=CARTESIAN_POINT('Ctrl Pts',(0.261622869962691,2.28819061588986,6.1743231572484));
#58319=CARTESIAN_POINT('Ctrl Pts',(0.260724547062876,2.28943109303871,6.17441683438047));
#58320=CARTESIAN_POINT('Ctrl Pts',(0.260428678015473,2.28983764672363,6.17444762509177));
#58321=CARTESIAN_POINT('Ctrl Pts',(0.259899701467144,2.29056094949178,6.17450256469765));
#58322=CARTESIAN_POINT('Ctrl Pts',(0.259666962819982,2.29087796811468,6.17452669923447));
#58323=CARTESIAN_POINT('Ctrl Pts',(0.25917547098953,2.291544877874,6.17457758706424));
#58324=CARTESIAN_POINT('Ctrl Pts',(0.258916588410107,2.29189467226977,6.17460434536989));
#58325=CARTESIAN_POINT('Ctrl Pts',(0.258231779284392,2.29281605722242,6.17467500809318));
#58326=CARTESIAN_POINT('Ctrl Pts',(0.257804665177576,2.29338675847847,6.1747189588991));
#58327=CARTESIAN_POINT('Ctrl Pts',(0.255870594628274,2.2959532302734,6.17491743807886));
#58328=CARTESIAN_POINT('Ctrl Pts',(0.254342364850452,2.29793279295081,6.17507280165207));
#58329=CARTESIAN_POINT('Ctrl Pts',(0.242875458509469,2.31243412501182,6.1762281480485));
#58330=CARTESIAN_POINT('Ctrl Pts',(0.232041893106022,2.32421678787079,6.17726469585986));
#58331=CARTESIAN_POINT('Ctrl Pts',(0.217556859123327,2.33779227316138,6.17858516935142));
#58332=CARTESIAN_POINT('Ctrl Pts',(0.214685798179649,2.34038751829849,6.17884393306726));
#58333=CARTESIAN_POINT('Ctrl Pts',(0.190799921314123,2.36120946110694,6.18097107783662));
#58334=CARTESIAN_POINT('Ctrl Pts',(0.167552267100266,2.37669726776595,6.1828943681863));
#58335=CARTESIAN_POINT('Ctrl Pts',(0.14125560781912,2.38967272776466,6.18474907791554));
#58336=CARTESIAN_POINT('Ctrl Pts',(0.139902695280505,2.39032855872838,6.18484363868768));
#58337=CARTESIAN_POINT('Ctrl Pts',(0.138159735427634,2.39115845412936,6.18496431306058));
#58338=CARTESIAN_POINT('Ctrl Pts',(0.137773892054862,2.39134123047982,6.18499095516205));
#58339=CARTESIAN_POINT('Ctrl Pts',(0.137162542943741,2.39162934417616,6.18503305317577));
#58340=CARTESIAN_POINT('Ctrl Pts',(0.136937278168955,2.39173518714768,6.18504854042471));
#58341=CARTESIAN_POINT('Ctrl Pts',(0.136517835007061,2.39193167397696,6.18507733148648));
#58342=CARTESIAN_POINT('Ctrl Pts',(0.136323690338754,2.39202238441391,6.18509063936819));
#58343=CARTESIAN_POINT('Ctrl Pts',(0.135886401403803,2.39222616830484,6.18512057254085));
#58344=CARTESIAN_POINT('Ctrl Pts',(0.135643206935435,2.39233913173253,6.18513719091932));
#58345=CARTESIAN_POINT('Ctrl Pts',(0.135134956191531,2.39257444260048,6.18517186224845));
#58346=CARTESIAN_POINT('Ctrl Pts',(0.134869873912707,2.39269673377103,6.18518991171519));
#58347=CARTESIAN_POINT('Ctrl Pts',(0.134178237582412,2.39301466927063,6.1852369185287));
#58348=CARTESIAN_POINT('Ctrl Pts',(0.133751419825575,2.39320974327198,6.18526584113607));
#58349=CARTESIAN_POINT('Ctrl Pts',(0.132487892979433,2.39378389610956,6.18535121255284));
#58350=CARTESIAN_POINT('Ctrl Pts',(0.131649979129677,2.39416033458195,6.18540750421858));
#58351=CARTESIAN_POINT('Ctrl Pts',(0.122366759348874,2.39828327300989,6.18602771841384));
#58352=CARTESIAN_POINT('Ctrl Pts',(0.113764811994164,2.40166892016873,6.18657104877395));
#58353=CARTESIAN_POINT('Ctrl Pts',(0.0783342367324629,2.41388242650221,
6.18872935709145));
#58354=CARTESIAN_POINT('Ctrl Pts',(0.0505460948361024,2.41953671657172,
6.19025251467767));
#58355=CARTESIAN_POINT('Ctrl Pts',(0.0206910924660686,2.42161452727039,
6.19197820487626));
#58356=CARTESIAN_POINT('Ctrl Pts',(0.0190061446707322,2.42171849776017,
6.19207585086633));
#58357=CARTESIAN_POINT('Ctrl Pts',(0.0138822380994547,2.42199427760851,
6.19237366253869));
#58358=CARTESIAN_POINT('Ctrl Pts',(0.0104413441416143,2.4221242128769,6.19257484892087));
#58359=CARTESIAN_POINT('Ctrl Pts',(-0.000136555521104034,2.42235399599426,
6.19319781080413));
#58360=CARTESIAN_POINT('Ctrl Pts',(-0.00727493791641535,2.42227190503922,
6.19362452448265));
#58361=CARTESIAN_POINT('Ctrl Pts',(-0.015464741360703,2.42190548944949,
6.19412336769333));
#58362=CARTESIAN_POINT('Ctrl Pts',(-0.0165249087877676,2.4218528075229,
6.19418812025241));
#58363=CARTESIAN_POINT('Ctrl Pts',(-0.0180878574252477,2.42176739871311,
6.19428384958939));
#58364=CARTESIAN_POINT('Ctrl Pts',(-0.0185908606579843,2.42173872840595,
6.19431469909012));
#58365=CARTESIAN_POINT('Ctrl Pts',(-0.0194876045951519,2.42168550562084,
6.19436977075608));
#58366=CARTESIAN_POINT('Ctrl Pts',(-0.019881372197351,2.42166140939931,
6.19439397855766));
#58367=CARTESIAN_POINT('Ctrl Pts',(-0.0207045761275696,2.42160951686937,
6.19444464046621));
#58368=CARTESIAN_POINT('Ctrl Pts',(-0.0211340027505667,2.42158158333221,
6.19447109883476));
#58369=CARTESIAN_POINT('Ctrl Pts',(-0.0222530168256028,2.42150654210776,
6.19454012491064));
#58370=CARTESIAN_POINT('Ctrl Pts',(-0.022942508260371,2.42145807608265,
6.19458273519188));
#58371=CARTESIAN_POINT('Ctrl Pts',(-0.0259229626274103,2.42123893487744,
6.19476727261138));
#58372=CARTESIAN_POINT('Ctrl Pts',(-0.0282121750117122,2.42104598738231,
6.19490989760952));
#58373=CARTESIAN_POINT('Ctrl Pts',(-0.0443069212725498,2.41951596477287,
6.19591909880909));
#58374=CARTESIAN_POINT('Ctrl Pts',(-0.058013717022465,2.41731352317646,
6.19681296385267));
#58375=CARTESIAN_POINT('Ctrl Pts',(-0.0853943256030159,2.41108042698548,
6.19866772861216));
#58376=CARTESIAN_POINT('Ctrl Pts',(-0.0990292777717138,2.40701200967548,
6.19962775076814));
#58377=CARTESIAN_POINT('Ctrl Pts',(-0.119053531608282,2.39956398881161,
6.20107355519886));
#58378=CARTESIAN_POINT('Ctrl Pts',(-0.125672115479725,2.3968481927999,6.20155742903898));
#58379=CARTESIAN_POINT('Ctrl Pts',(-0.13582566999223,2.39228139149973,6.20230487024037));
#58380=CARTESIAN_POINT('Ctrl Pts',(-0.139425916812929,2.39058121037036,
6.20257092174548));
#58381=CARTESIAN_POINT('Ctrl Pts',(-0.151662645588858,2.38452273563978,
6.20347680230383));
#58382=CARTESIAN_POINT('Ctrl Pts',(-0.160134857578551,2.37984212461508,
6.20410688688518));
#58383=CARTESIAN_POINT('Ctrl Pts',(-0.169004072429104,2.3744072286998,6.2047597472065));
#58384=CARTESIAN_POINT('Ctrl Pts',(-0.16962237869707,2.37402545927299,6.2048052235714));
#58385=CARTESIAN_POINT('Ctrl Pts',(-0.170482029679533,2.37349064853897,
6.20486839335763));
#58386=CARTESIAN_POINT('Ctrl Pts',(-0.17072446415343,2.37333937627609,6.20488620179406));
#58387=CARTESIAN_POINT('Ctrl Pts',(-0.171142188317985,2.37307795564847,
6.20491687496185));
#58388=CARTESIAN_POINT('Ctrl Pts',(-0.171317573109749,2.37296796080814,
6.20492974983965));
#58389=CARTESIAN_POINT('Ctrl Pts',(-0.171677408627946,2.37274180190721,
6.20495615774185));
#58390=CARTESIAN_POINT('Ctrl Pts',(-0.171861847190943,2.37262561989136,
6.20496968945391));
#58391=CARTESIAN_POINT('Ctrl Pts',(-0.17229538727339,2.3723519084127,6.20500148786805));
#58392=CARTESIAN_POINT('Ctrl Pts',(-0.172544391626592,2.37219422369256,
6.20501974423289));
#58393=CARTESIAN_POINT('Ctrl Pts',(-0.173070877623897,2.37185980793827,
6.20505833058906));
#58394=CARTESIAN_POINT('Ctrl Pts',(-0.173348305949448,2.37168299299085,
6.20507865501474));
#58395=CARTESIAN_POINT('Ctrl Pts',(-0.174096244706551,2.3712046929443,6.20513342777145));
#58396=CARTESIAN_POINT('Ctrl Pts',(-0.174566245173121,2.37090240669463,
6.20516782385659));
#58397=CARTESIAN_POINT('Ctrl Pts',(-0.176014790128062,2.36996542307415,
6.20527377008675));
#58398=CARTESIAN_POINT('Ctrl Pts',(-0.176990689963075,2.36932662653336,
6.20534505845735));
#58399=CARTESIAN_POINT('Ctrl Pts',(-0.190327293992514,2.36049306530224,
6.20631837449763));
#58400=CARTESIAN_POINT('Ctrl Pts',(-0.202113182387467,2.35145873517464,
6.20716814245826));
#58401=CARTESIAN_POINT('Ctrl Pts',(-0.231657197921143,2.32538788719773,
6.20938918311929));
#58402=CARTESIAN_POINT('Ctrl Pts',(-0.248158216252713,2.30708025181392,
6.21073517352927));
#58403=CARTESIAN_POINT('Ctrl Pts',(-0.268076790689056,2.2791396122804,6.21273221293303));
#58404=CARTESIAN_POINT('Ctrl Pts',(-0.273370966253454,2.27095160814391,
6.21331054495667));
#58405=CARTESIAN_POINT('Ctrl Pts',(-0.278809954789398,2.26163930603782,
6.21396631955806));
#58406=CARTESIAN_POINT('Ctrl Pts',(-0.279329858391319,2.2607391872492,6.21402968384572));
#58407=CARTESIAN_POINT('Ctrl Pts',(-0.280101160555895,2.25938877446129,
6.21412471963403));
#58408=CARTESIAN_POINT('Ctrl Pts',(-0.280355851257774,2.25894036060636,
6.21415627245991));
#58409=CARTESIAN_POINT('Ctrl Pts',(-0.280792742654014,2.25816684288156,
6.21421069447979));
#58410=CARTESIAN_POINT('Ctrl Pts',(-0.280975458276061,2.2578420297606,6.21423354512098));
#58411=CARTESIAN_POINT('Ctrl Pts',(-0.28135149304452,2.25717083171431,6.21428076003648));
#58412=CARTESIAN_POINT('Ctrl Pts',(-0.281544736823294,2.256824405451,6.21430512696485));
#58413=CARTESIAN_POINT('Ctrl Pts',(-0.281993217969672,2.25601691693269,
6.21436191950979));
#58414=CARTESIAN_POINT('Ctrl Pts',(-0.282247964445309,2.25555558463549,
6.21439436261762));
#58415=CARTESIAN_POINT('Ctrl Pts',(-0.283056882239348,2.25408214855741,
6.21449797208943));
#58416=CARTESIAN_POINT('Ctrl Pts',(-0.28360674522256,2.25306770102113,6.21456929184038));
#58417=CARTESIAN_POINT('Ctrl Pts',(-0.295863117904717,2.23016303361312,
6.21617935198832));
#58418=CARTESIAN_POINT('Ctrl Pts',(-0.305004471569212,2.20700079237407,
6.21781281550682));
#58419=CARTESIAN_POINT('Ctrl Pts',(-0.31783436978374,2.15888022072901,6.22117310277374));
#58420=CARTESIAN_POINT('Ctrl Pts',(-0.321442388459736,2.13406720704661,
6.22288731729675));
#58421=CARTESIAN_POINT('Ctrl Pts',(-0.322180928912625,2.10787908649388,
6.22453982131179));
#58422=CARTESIAN_POINT('Ctrl Pts',(-0.322208166065209,2.10667298951083,
6.22461556572644));
#58423=CARTESIAN_POINT('Ctrl Pts',(-0.322235274014918,2.10507515450673,
6.2247154072277));
#58424=CARTESIAN_POINT('Ctrl Pts',(-0.322241203734308,2.10468354913219,
6.2247398367413));
#58425=CARTESIAN_POINT('Ctrl Pts',(-0.32224930866881,2.10407501515372,6.22477773551545));
#58426=CARTESIAN_POINT('Ctrl Pts',(-0.322251978718531,2.10385809521546,
6.2247912325156));
#58427=CARTESIAN_POINT('Ctrl Pts',(-0.322256864196161,2.10342571607582,
6.22481811045619));
#58428=CARTESIAN_POINT('Ctrl Pts',(-0.322259082556228,2.1032102589536,6.22483149140035));
#58429=CARTESIAN_POINT('Ctrl Pts',(-0.322263047337864,2.1027836208533,6.22485796311304));
#58430=CARTESIAN_POINT('Ctrl Pts',(-0.322264802252337,2.10257244133396,
6.22487105430052));
#58431=CARTESIAN_POINT('Ctrl Pts',(-0.322268314639747,2.10209306824478,
6.22490074427885));
#58432=CARTESIAN_POINT('Ctrl Pts',(-0.322269944911836,2.10182487346972,
6.22491733592495));
#58433=CARTESIAN_POINT('Ctrl Pts',(-0.322273682472704,2.10105110390097,
6.22496515051638));
#58434=CARTESIAN_POINT('Ctrl Pts',(-0.322274934869778,2.10054552339395,
6.22499632600572));
#58435=CARTESIAN_POINT('Ctrl Pts',(-0.322274997525276,2.1000399384962,6.22502743709318));
#58436=CARTESIAN_POINT('',(-0.322274881329742,2.10027656626812,6.34972265506687));
#58437=CARTESIAN_POINT('Ctrl Pts',(-0.322274999303774,2.10002118378279,
6.22472265507673));
#58438=CARTESIAN_POINT('Ctrl Pts',(-0.322276158268471,2.08238951947228,
6.22581786979066));
#58439=CARTESIAN_POINT('Ctrl Pts',(-0.320826057348452,2.06470156024196,
6.22691308450459));
#58440=CARTESIAN_POINT('Ctrl Pts',(-0.317923029073763,2.04721625998887,
6.22800829921852));
#58441=CARTESIAN_POINT('Ctrl Pts',(-0.31502554512302,2.02976435388827,6.22910142224591));
#58442=CARTESIAN_POINT('Ctrl Pts',(-0.310680702994432,2.01251510674329,
6.23019454527331));
#58443=CARTESIAN_POINT('Ctrl Pts',(-0.304938651877089,1.9957234723613,6.2312876683007));
#58444=CARTESIAN_POINT('Ctrl Pts',(-0.299197597929198,1.97893475402875,
6.23238060149542));
#58445=CARTESIAN_POINT('Ctrl Pts',(-0.292060016039921,1.96260424113098,
6.23347353469014));
#58446=CARTESIAN_POINT('Ctrl Pts',(-0.283626232167341,1.94697276042626,
6.23456646788487));
#58447=CARTESIAN_POINT('Ctrl Pts',(-0.275194890595358,1.93134580636999,
6.2356590845821));
#58448=CARTESIAN_POINT('Ctrl Pts',(-0.265468469318602,1.91641816256849,
6.23675170127934));
#58449=CARTESIAN_POINT('Ctrl Pts',(-0.254593111913849,1.9024056605289,6.23784431797657));
#58450=CARTESIAN_POINT('Ctrl Pts',(-0.243691529540873,1.88835936857261,
6.23893956942291));
#58451=CARTESIAN_POINT('Ctrl Pts',(-0.231635973261083,1.87523322977712,
6.24003482086925));
#58452=CARTESIAN_POINT('Ctrl Pts',(-0.218613162004877,1.86321009095988,
6.24113007231559));
#58453=CARTESIAN_POINT('Ctrl Pts',(-0.205721904410726,1.8513084073269,6.2422142597654));
#58454=CARTESIAN_POINT('Ctrl Pts',(-0.191883510059295,1.84048790191718,
6.2432984472152));
#58455=CARTESIAN_POINT('Ctrl Pts',(-0.177308771851876,1.83088520098408,
6.244382634665));
#58456=CARTESIAN_POINT('Ctrl Pts',(-0.162558307939585,1.82116672154669,
6.24547989402053));
#58457=CARTESIAN_POINT('Ctrl Pts',(-0.146960238062366,1.81263413867367,
6.24657715337606));
#58458=CARTESIAN_POINT('Ctrl Pts',(-0.130730780769772,1.80543143653077,
6.24767441273159));
#58459=CARTESIAN_POINT('Ctrl Pts',(-0.114532370010416,1.79824251297131,
6.24876957305827));
#58460=CARTESIAN_POINT('Ctrl Pts',(-0.0977056422412874,1.79237878939909,
6.24986473338495));
#58461=CARTESIAN_POINT('Ctrl Pts',(-0.0804919229730219,1.78793874645976,
6.25095989371163));
#58462=CARTESIAN_POINT('Ctrl Pts',(-0.0630802086934335,1.78344763342115,
6.25206765075131));
#58463=CARTESIAN_POINT('Ctrl Pts',(-0.0452732803213705,1.78041349834926,
6.25317540779099));
#58464=CARTESIAN_POINT('Ctrl Pts',(-0.0273374283460662,1.77888656110897,
6.25428316483067));
#58465=CARTESIAN_POINT('Ctrl Pts',(-0.00961411907978619,1.77737771831872,
6.2553777947726));
#58466=CARTESIAN_POINT('Ctrl Pts',(0.00823428241176009,1.7773405276635,
6.25647242471453));
#58467=CARTESIAN_POINT('Ctrl Pts',(0.0259463163571276,1.77877116522252,
6.25756705465645));
#58468=CARTESIAN_POINT('Ctrl Pts',(0.0439769615409925,1.78022753766925,
6.25868137524501));
#58469=CARTESIAN_POINT('Ctrl Pts',(0.0618654546753276,1.78320505426578,
6.25979569583357));
#58470=CARTESIAN_POINT('Ctrl Pts',(0.0793435882414551,1.78764480053956,
6.26091001642212));
#58471=CARTESIAN_POINT('Ctrl Pts',(0.0968217218075841,1.79208454681334,
6.26202433701068));
#58472=CARTESIAN_POINT('Ctrl Pts',(0.113888723803027,1.79798619566923,6.26313865759923));
#58473=CARTESIAN_POINT('Ctrl Pts',(0.130296099377664,1.80523890671941,6.26425297818779));
#58474=CARTESIAN_POINT('Ctrl Pts',(0.146452263531704,1.8123805723536,6.26535023754332));
#58475=CARTESIAN_POINT('Ctrl Pts',(0.162070129045757,1.82087686749704,6.26644749689885));
#58476=CARTESIAN_POINT('Ctrl Pts',(0.176911588447618,1.83062393295257,6.26754475625438));
#58477=CARTESIAN_POINT('Ctrl Pts',(0.191724656520408,1.84035235252326,6.26863991658106));
#58478=CARTESIAN_POINT('Ctrl Pts',(0.205763592067393,1.85132642698334,6.26973507690774));
#58479=CARTESIAN_POINT('Ctrl Pts',(0.218814956939098,1.86339655487559,6.27083023723442));
#58480=CARTESIAN_POINT('Ctrl Pts',(0.232016440741833,1.87560551535082,6.2719379942741));
#58481=CARTESIAN_POINT('Ctrl Pts',(0.244206807913172,1.88893546741038,6.27304575131378));
#58482=CARTESIAN_POINT('Ctrl Pts',(0.255199684838193,1.90318969416342,6.27415350835346));
#58483=CARTESIAN_POINT('Ctrl Pts',(0.26606229441685,1.91727500605403,6.27524813829539));
#58484=CARTESIAN_POINT('Ctrl Pts',(0.275755227213166,1.93226212961909,6.27634276823731));
#58485=CARTESIAN_POINT('Ctrl Pts',(0.284140165549627,1.9479291548441,6.27743739817924));
#58486=CARTESIAN_POINT('Ctrl Pts',(0.29267593555208,1.96387800486268,6.2785517187678));
#58487=CARTESIAN_POINT('Ctrl Pts',(0.29985575084529,1.98053075370649,6.27966603935635));
#58488=CARTESIAN_POINT('Ctrl Pts',(0.305583962196553,1.99762999622323,6.28078035994491));
#58489=CARTESIAN_POINT('Ctrl Pts',(0.311312173547817,2.01472923873997,6.28189468053347));
#58490=CARTESIAN_POINT('Ctrl Pts',(0.315588638085686,2.03227414875362,6.28300900112202));
#58491=CARTESIAN_POINT('Ctrl Pts',(0.318372037640385,2.04999578744036,6.28412332171058));
#58492=CARTESIAN_POINT('Ctrl Pts',(0.321112820887983,2.06744609217674,6.28522058106611));
#58493=CARTESIAN_POINT('Ctrl Pts',(0.322423216610124,2.08517707120868,6.28631784042164));
#58494=CARTESIAN_POINT('Ctrl Pts',(0.322261659602295,2.10293229865033,6.28741509977716));
#58495=CARTESIAN_POINT('Ctrl Pts',(0.322100411648855,2.12065356079979,6.28851026010384));
#58496=CARTESIAN_POINT('Ctrl Pts',(0.320472742837832,2.13839821396037,6.28960542043052));
#58497=CARTESIAN_POINT('Ctrl Pts',(0.317388902826077,2.15590581354259,6.2907005807572));
#58498=CARTESIAN_POINT('Ctrl Pts',(0.314269591982681,2.17361478839553,6.29180833779688));
#58499=CARTESIAN_POINT('Ctrl Pts',(0.309660395642225,2.191080411281,6.29291609483656));
#58500=CARTESIAN_POINT('Ctrl Pts',(0.303625829483311,2.20803948951921,6.29402385187624));
#58501=CARTESIAN_POINT('Ctrl Pts',(0.297662773896685,2.2247975999731,6.29511848181817));
#58502=CARTESIAN_POINT('Ctrl Pts',(0.290308291730793,2.24106039220014,6.2962131117601));
#58503=CARTESIAN_POINT('Ctrl Pts',(0.281674095040921,2.25659144232007,6.29730774170203));
#58504=CARTESIAN_POINT('Ctrl Pts',(0.272884582924865,2.27240187125833,6.29842206229058));
#58505=CARTESIAN_POINT('Ctrl Pts',(0.262769217289018,2.28745322235227,6.29953638287914));
#58506=CARTESIAN_POINT('Ctrl Pts',(0.251492652336189,2.30152573395452,6.30065070346769));
#58507=CARTESIAN_POINT('Ctrl Pts',(0.24021608738336,2.31559824555678,6.30176502405625));
#58508=CARTESIAN_POINT('Ctrl Pts',(0.227778940438234,2.32869135031448,6.30287934464481));
#58509=CARTESIAN_POINT('Ctrl Pts',(0.21438497380719,2.34062472572595,6.30399366523336));
#58510=CARTESIAN_POINT('Ctrl Pts',(0.201196080642618,2.35237539061337,6.30509092458889));
#58511=CARTESIAN_POINT('Ctrl Pts',(0.186996896892048,2.36307529412683,6.30618818394442));
#58512=CARTESIAN_POINT('Ctrl Pts',(0.171980530035207,2.37255067953283,6.30728544329995));
#58513=CARTESIAN_POINT('Ctrl Pts',(0.156992889100883,2.38200793877093,6.30838060362663));
#58514=CARTESIAN_POINT('Ctrl Pts',(0.141191780478856,2.39024486707358,6.30947576395331));
#58515=CARTESIAN_POINT('Ctrl Pts',(0.124801738967505,2.39712909917355,6.31057092427999));
#58516=CARTESIAN_POINT('Ctrl Pts',(0.108223176520971,2.40409251483585,6.31167868131967));
#58517=CARTESIAN_POINT('Ctrl Pts',(0.0910427268256701,2.40967147727965,
6.31278643835936));
#58518=CARTESIAN_POINT('Ctrl Pts',(0.0735166105016287,2.41377776148948,
6.31389419539904));
#58519=CARTESIAN_POINT('Ctrl Pts',(0.0561981814537302,2.41783538557594,
6.31498882534096));
#58520=CARTESIAN_POINT('Ctrl Pts',(0.0385430204904939,2.42045494857589,
6.31608345528289));
#58521=CARTESIAN_POINT('Ctrl Pts',(0.0208103887975029,2.42160239946726,
6.31717808522482));
#58522=CARTESIAN_POINT('Ctrl Pts',(0.00275877534540055,2.42277049116988,
6.31829240581338));
#58523=CARTESIAN_POINT('Ctrl Pts',(-0.0153723003312898,2.42241287894167,
6.31940672640193));
#58524=CARTESIAN_POINT('Ctrl Pts',(-0.0333089284096789,2.42054904603383,
6.32052104699049));
#58525=CARTESIAN_POINT('Ctrl Pts',(-0.0512455564880679,2.41868521312599,
6.32163536757905));
#58526=CARTESIAN_POINT('Ctrl Pts',(-0.0689869257586935,2.41531537147781,
6.3227496881676));
#58527=CARTESIAN_POINT('Ctrl Pts',(-0.0862711176153947,2.41051323625635,
6.32386400875616));
#58528=CARTESIAN_POINT('Ctrl Pts',(-0.10329067321931,2.40578462596917,6.32496126811169));
#58529=CARTESIAN_POINT('Ctrl Pts',(-0.119973618395755,2.39963774915087,
6.32605852746721));
#58530=CARTESIAN_POINT('Ctrl Pts',(-0.136069322804202,2.39214091636846,
6.32715578682274));
#58531=CARTESIAN_POINT('Ctrl Pts',(-0.152134236545231,2.38465842483382,
6.32825094714942));
#58532=CARTESIAN_POINT('Ctrl Pts',(-0.167613418944239,2.37583136791738,
6.3293461074761));
#58533=CARTESIAN_POINT('Ctrl Pts',(-0.182274030171178,2.36577688678694,
6.33044126780278));
#58534=CARTESIAN_POINT('Ctrl Pts',(-0.197103270143636,2.35560675737187,
6.33154902484246));
#58535=CARTESIAN_POINT('Ctrl Pts',(-0.211094249505374,2.34418112083898,
6.33265678188215));
#58536=CARTESIAN_POINT('Ctrl Pts',(-0.224034090232527,2.33166765427803,
6.33376453892183));
#58537=CARTESIAN_POINT('Ctrl Pts',(-0.23682059178146,2.31930247429337,6.33485916886375));
#58538=CARTESIAN_POINT('Ctrl Pts',(-0.248580224891392,2.30587571563507,
6.33595379880568));
#58539=CARTESIAN_POINT('Ctrl Pts',(-0.25914401608899,2.29158693731638,6.33704842874761));
#58540=CARTESIAN_POINT('Ctrl Pts',(-0.269897833040104,2.27704112666752,
6.33816274933617));
#58541=CARTESIAN_POINT('Ctrl Pts',(-0.279411825147348,2.26160261165204,
6.33927706992472));
#58542=CARTESIAN_POINT('Ctrl Pts',(-0.287554101940797,2.2455122471891,6.34039139051328));
#58543=CARTESIAN_POINT('Ctrl Pts',(-0.295696378734246,2.22942188272616,
6.34150571110184));
#58544=CARTESIAN_POINT('Ctrl Pts',(-0.302466679293908,2.21268046562178,
6.34262003169039));
#58545=CARTESIAN_POINT('Ctrl Pts',(-0.307785203377992,2.19554812508139,
6.34373435227895));
#58546=CARTESIAN_POINT('Ctrl Pts',(-0.314114228816402,2.17516069853496,
6.34506038996159));
#58547=CARTESIAN_POINT('Ctrl Pts',(-0.318421557416576,2.15411748845562,
6.34638642764423));
#58548=CARTESIAN_POINT('Ctrl Pts',(-0.320603011129514,2.13278543700622,
6.34771246532687));
#58549=CARTESIAN_POINT('Ctrl Pts',(-0.321705326679427,2.12200608749046,
6.34838252857354));
#58550=CARTESIAN_POINT('Ctrl Pts',(-0.32226554723971,2.11115331843988,6.3490525918202));
#58551=CARTESIAN_POINT('Ctrl Pts',(-0.322274881329742,2.10027656626812,
6.34972265506687));
#58552=CARTESIAN_POINT('',(-0.32227496222964,2.09984397152879,6.47472265507269));
#58553=CARTESIAN_POINT('Ctrl Pts',(-0.322274881329823,2.10027656617378,
6.34972265507268));
#58554=CARTESIAN_POINT('Ctrl Pts',(-0.322290035910069,2.0826173546965,6.35081055230423));
#58555=CARTESIAN_POINT('Ctrl Pts',(-0.320849399698483,2.0649328324212,6.35189844953578));
#58556=CARTESIAN_POINT('Ctrl Pts',(-0.317966904445043,2.04748121000407,
6.35298634676733));
#58557=CARTESIAN_POINT('Ctrl Pts',(-0.315083192672738,2.03002222236131,
6.35407470313147));
#58558=CARTESIAN_POINT('Ctrl Pts',(-0.310756513550684,2.01279710640944,
6.35516305949561));
#58559=CARTESIAN_POINT('Ctrl Pts',(-0.305052384133251,1.99605665697304,
6.35625141585975));
#58560=CARTESIAN_POINT('Ctrl Pts',(-0.2993465896174,1.97931132081445,6.35734008992714));
#58561=CARTESIAN_POINT('Ctrl Pts',(-0.292262834855402,1.96305165988339,
6.35842876399452));
#58562=CARTESIAN_POINT('Ctrl Pts',(-0.283915241013496,1.94750963458222,
6.35951743806191));
#58563=CARTESIAN_POINT('Ctrl Pts',(-0.275549064599905,1.9319330111915,6.36060853562573));
#58564=CARTESIAN_POINT('Ctrl Pts',(-0.265913864312675,1.91707786596012,
6.36169963318956));
#58565=CARTESIAN_POINT('Ctrl Pts',(-0.255167702714323,1.90314823059852,
6.36279073075338));
#58566=CARTESIAN_POINT('Ctrl Pts',(-0.252495469959852,1.8996843679411,6.36306205243616));
#58567=CARTESIAN_POINT('Ctrl Pts',(-0.249754728417259,1.8962775673472,6.36333337411895));
#58568=CARTESIAN_POINT('Ctrl Pts',(-0.246948266213006,1.89293061684694,
6.36360469580174));
#58569=CARTESIAN_POINT('Ctrl Pts',(-0.235598576509175,1.87939512380717,
6.36470195515727));
#58570=CARTESIAN_POINT('Ctrl Pts',(-0.223097178713936,1.86675313790524,
6.3657992145128));
#58571=CARTESIAN_POINT('Ctrl Pts',(-0.209610004229396,1.85520453077732,
6.36689647386832));
#58572=CARTESIAN_POINT('Ctrl Pts',(-0.196148630361804,1.84367801583699,
6.367991634195));
#58573=CARTESIAN_POINT('Ctrl Pts',(-0.181705762025049,1.83324127421161,
6.36908679452169));
#58574=CARTESIAN_POINT('Ctrl Pts',(-0.166484416736886,1.82405776943574,
6.37018195484837));
#58575=CARTESIAN_POINT('Ctrl Pts',(-0.151087993048431,1.81476863448759,
6.37128971188805));
#58576=CARTESIAN_POINT('Ctrl Pts',(-0.134895678978682,1.80676228458587,
6.37239746892772));
#58577=CARTESIAN_POINT('Ctrl Pts',(-0.118148231707899,1.80016309271656,
6.3735052259674));
#58578=CARTESIAN_POINT('Ctrl Pts',(-0.101599244360684,1.79364210232434,
6.37459985590933));
#58579=CARTESIAN_POINT('Ctrl Pts',(-0.0845089737811362,1.7884953100742,
6.37569448585126));
#58580=CARTESIAN_POINT('Ctrl Pts',(-0.0671290249930131,1.78479392514025,
6.37678911579319));
#58581=CARTESIAN_POINT('Ctrl Pts',(-0.0494364386486706,1.78102595819536,
6.37790343638174));
#58582=CARTESIAN_POINT('Ctrl Pts',(-0.0314444485246837,1.77875613814127,
6.3790177569703));
#58583=CARTESIAN_POINT('Ctrl Pts',(-0.0134269008111419,1.77800482308021,
6.38013207755886));
#58584=CARTESIAN_POINT('Ctrl Pts',(0.00459064690239998,1.77725350801914,
6.38124639814741));
#58585=CARTESIAN_POINT('Ctrl Pts',(0.0226329188654116,1.77802060562909,
6.38236071873597));
#58586=CARTESIAN_POINT('Ctrl Pts',(0.0404300862316696,1.78027107770441,
6.38347503932452));
#58587=CARTESIAN_POINT('Ctrl Pts',(0.0579547632367289,1.78248709306333,
6.38457229868005));
#58588=CARTESIAN_POINT('Ctrl Pts',(0.0753516038425314,1.78615515676448,
6.38566955803558));
#58589=CARTESIAN_POINT('Ctrl Pts',(0.0923627307326406,1.79124394484219,
6.38676681739111));
#58590=CARTESIAN_POINT('Ctrl Pts',(0.109341315775737,1.79632299819956,6.38786197771779));
#58591=CARTESIAN_POINT('Ctrl Pts',(0.125934900594545,1.80281722366599,6.38895713804447));
#58592=CARTESIAN_POINT('Ctrl Pts',(0.141896145071832,1.8106444062425,6.39005229837115));
#58593=CARTESIAN_POINT('Ctrl Pts',(0.15804097839077,1.81856161835178,6.39116005541083));
#58594=CARTESIAN_POINT('Ctrl Pts',(0.173538052919404,1.82784242406768,6.39226781245051));
#58595=CARTESIAN_POINT('Ctrl Pts',(0.188152467412437,1.83835171578699,6.39337556949019));
#58596=CARTESIAN_POINT('Ctrl Pts',(0.202593698760813,1.84873647072182,6.39447019943212));
#58597=CARTESIAN_POINT('Ctrl Pts',(0.216172486101175,1.86032022457424,6.39556482937405));
#58598=CARTESIAN_POINT('Ctrl Pts',(0.228692757139418,1.87292997014804,6.39665945931598));
#58599=CARTESIAN_POINT('Ctrl Pts',(0.24143824788276,1.88576654493111,6.39777377990453));
#58600=CARTESIAN_POINT('Ctrl Pts',(0.253086142572723,1.89966583775454,6.39888810049309));
#58601=CARTESIAN_POINT('Ctrl Pts',(0.263471085861674,1.91440861404723,6.40000242108165));
#58602=CARTESIAN_POINT('Ctrl Pts',(0.273856029150626,1.92915139033992,6.4011167416702));
#58603=CARTESIAN_POINT('Ctrl Pts',(0.282977647562523,1.94473689943903,6.40223106225876));
#58604=CARTESIAN_POINT('Ctrl Pts',(0.290719338618049,1.96091929760573,6.40334538284732));
#58605=CARTESIAN_POINT('Ctrl Pts',(0.298342497541543,1.97685392895477,6.40444264220285));
#58606=CARTESIAN_POINT('Ctrl Pts',(0.304675548068079,1.99346709317499,6.40553990155837));
#58607=CARTESIAN_POINT('Ctrl Pts',(0.309605234297894,2.01052500617297,6.4066371609139));
#58608=CARTESIAN_POINT('Ctrl Pts',(0.314525490165093,2.02755028782334,6.40773232124058));
#58609=CARTESIAN_POINT('Ctrl Pts',(0.31804743640729,2.0450179126251,6.40882748156726));
#58610=CARTESIAN_POINT('Ctrl Pts',(0.320106311193014,2.06267540811474,6.40992264189395));
#58611=CARTESIAN_POINT('Ctrl Pts',(0.322188867492893,2.0805360030023,6.41103039893363));
#58612=CARTESIAN_POINT('Ctrl Pts',(0.322774246336576,2.09859008855908,6.4121381559733));
#58613=CARTESIAN_POINT('Ctrl Pts',(0.321848892327374,2.11656701942543,6.41324591301298));
#58614=CARTESIAN_POINT('Ctrl Pts',(0.320934503910896,2.13433092079134,6.41434054295491));
#58615=CARTESIAN_POINT('Ctrl Pts',(0.318545119212261,2.1520187035724,6.41543517289684));
#58616=CARTESIAN_POINT('Ctrl Pts',(0.314720068304024,2.16937185475184,6.41652980283877));
#58617=CARTESIAN_POINT('Ctrl Pts',(0.310826210831224,2.18703716144127,6.41764412342732));
#58618=CARTESIAN_POINT('Ctrl Pts',(0.305444652426788,2.20435485819457,6.41875844401588));
#58619=CARTESIAN_POINT('Ctrl Pts',(0.298670219605893,2.22106723564023,6.41987276460443));
#58620=CARTESIAN_POINT('Ctrl Pts',(0.291895786784999,2.23777961308589,6.42098708519299));
#58621=CARTESIAN_POINT('Ctrl Pts',(0.283728908549072,2.2538859508512,6.42210140578155));
#58622=CARTESIAN_POINT('Ctrl Pts',(0.274313175686482,2.2691551278259,6.4232157263701));
#58623=CARTESIAN_POINT('Ctrl Pts',(0.265041606015477,2.2841905202065,6.42431298572563));
#58624=CARTESIAN_POINT('Ctrl Pts',(0.254501154771622,2.29850846845181,6.42541024508116));
#58625=CARTESIAN_POINT('Ctrl Pts',(0.242827084341463,2.31188719341957,6.42650750443669));
#58626=CARTESIAN_POINT('Ctrl Pts',(0.231175346106956,2.32524032523152,6.42760266476337));
#58627=CARTESIAN_POINT('Ctrl Pts',(0.218394747565007,2.33765718161538,6.42869782509005));
#58628=CARTESIAN_POINT('Ctrl Pts',(0.204662515333758,2.34894664175734,6.42979298541673));
#58629=CARTESIAN_POINT('Ctrl Pts',(0.190772332723877,2.36036595511428,6.43090074245641));
#58630=CARTESIAN_POINT('Ctrl Pts',(0.175909010485664,2.37063115485541,6.43200849949609));
#58631=CARTESIAN_POINT('Ctrl Pts',(0.160292774302096,2.37958433813706,6.43311625653577));
#58632=CARTESIAN_POINT('Ctrl Pts',(0.144861593010141,2.38843142476762,6.4342108864777));
#58633=CARTESIAN_POINT('Ctrl Pts',(0.128695971448153,2.39599710374989,6.43530551641963));
#58634=CARTESIAN_POINT('Ctrl Pts',(0.112034562068085,2.40217450674604,6.43640014636155));
#58635=CARTESIAN_POINT('Ctrl Pts',(0.0950734405096114,2.40846303136862,
6.43751446695011));
#58636=CARTESIAN_POINT('Ctrl Pts',(0.0775992762138262,2.41331250287217,
6.43862878753866));
#58637=CARTESIAN_POINT('Ctrl Pts',(0.0598800871405084,2.41666315034914,
6.43974310812722));
#58638=CARTESIAN_POINT('Ctrl Pts',(0.0421608980671892,2.42001379782612,
6.44085742871578));
#58639=CARTESIAN_POINT('Ctrl Pts',(0.024197522144825,2.42186559203785,6.44197174930433));
#58640=CARTESIAN_POINT('Ctrl Pts',(0.00626201842926354,2.42221415665702,
6.44308606989289));
#58641=CARTESIAN_POINT('Ctrl Pts',(-0.0113988768733321,2.42255738444381,
6.44418332924842));
#58642=CARTESIAN_POINT('Ctrl Pts',(-0.0291434008242062,2.42144534841178,
6.44528058860395));
#58643=CARTESIAN_POINT('Ctrl Pts',(-0.0467118575758495,2.41887172654033,
6.44637784795948));
#58644=CARTESIAN_POINT('Ctrl Pts',(-0.0642467063228147,2.41630302794115,
6.44747300828616));
#58645=CARTESIAN_POINT('Ctrl Pts',(-0.0816053904080379,2.41227834057728,
6.44856816861284));
#58646=CARTESIAN_POINT('Ctrl Pts',(-0.0985312760586869,2.40684322261254,
6.44966332893952));
#58647=CARTESIAN_POINT('Ctrl Pts',(-0.115651846011373,2.40134558903299,
6.4507710859792));
#58648=CARTESIAN_POINT('Ctrl Pts',(-0.132328794636532,2.39440497967673,
6.45187884301888));
#58649=CARTESIAN_POINT('Ctrl Pts',(-0.148310142254628,2.38612108857862,
6.45298660005856));
#58650=CARTESIAN_POINT('Ctrl Pts',(-0.164102108352333,2.37793536291237,
6.45408123000049));
#58651=CARTESIAN_POINT('Ctrl Pts',(-0.179214209745205,2.3684384576038,6.45517585994242));
#58652=CARTESIAN_POINT('Ctrl Pts',(-0.193427402736963,2.35777318614517,
6.45627048988434));
#58653=CARTESIAN_POINT('Ctrl Pts',(-0.207896268399406,2.346916063465,6.4573848104729));
#58654=CARTESIAN_POINT('Ctrl Pts',(-0.221432871737814,2.33484857981022,
6.45849913106146));
#58655=CARTESIAN_POINT('Ctrl Pts',(-0.233841873338553,2.32176373440785,
6.45961345165001));
#58656=CARTESIAN_POINT('Ctrl Pts',(-0.246250874939294,2.30867888900548,
6.46072777223857));
#58657=CARTESIAN_POINT('Ctrl Pts',(-0.25753179663213,2.29457737057338,6.46184209282713));
#58658=CARTESIAN_POINT('Ctrl Pts',(-0.26753368823998,2.27968556225171,6.46295641341568));
#58659=CARTESIAN_POINT('Ctrl Pts',(-0.277547582711622,2.26477588287585,
6.46407207125511));
#58660=CARTESIAN_POINT('Ctrl Pts',(-0.286340890299472,2.24898295014912,
6.46518772909454));
#58661=CARTESIAN_POINT('Ctrl Pts',(-0.293764094382879,2.23252861002971,
6.46630338693396));
#58662=CARTESIAN_POINT('Ctrl Pts',(-0.301170835693589,2.21611076143852,
6.46741657052895));
#58663=CARTESIAN_POINT('Ctrl Pts',(-0.307213145628115,2.1990350556288,6.46852975412393));
#58664=CARTESIAN_POINT('Ctrl Pts',(-0.311786712349425,2.18154889102457,
6.46964293771892));
#58665=CARTESIAN_POINT('Ctrl Pts',(-0.316353640034259,2.16408810951666,
6.47075450540516));
#58666=CARTESIAN_POINT('Ctrl Pts',(-0.319455832526156,2.14621875250001,
6.47186607309139));
#58667=CARTESIAN_POINT('Ctrl Pts',(-0.321038463309149,2.12820426742712,
6.47297764077763));
#58668=CARTESIAN_POINT('Ctrl Pts',(-0.32186663700003,2.11877748086864,6.47355931220932));
#58669=CARTESIAN_POINT('Ctrl Pts',(-0.322279545747959,2.10931117441553,
6.474140983641));
#58670=CARTESIAN_POINT('Ctrl Pts',(-0.32227496222964,2.09984397152879,6.47472265507269));
#58671=CARTESIAN_POINT('',(-0.322274913684313,2.10027657538795,6.72483363319554));
#58672=CARTESIAN_POINT('Ctrl Pts',(-0.322274953602036,2.09982706704832,
6.47445952331017));
#58673=CARTESIAN_POINT('Ctrl Pts',(-0.322258535437458,2.06923045040549,
6.47642514822576));
#58674=CARTESIAN_POINT('Ctrl Pts',(-0.317884570239021,2.03879330021116,
6.47852897207899));
#58675=CARTESIAN_POINT('Ctrl Pts',(-0.306838273958802,2.00106826228417,
6.48115616092435));
#58676=CARTESIAN_POINT('Ctrl Pts',(-0.304048970120985,1.99280175273676,
6.48173152784109));
#58677=CARTESIAN_POINT('Ctrl Pts',(-0.299669851892031,1.98137662812439,
6.48251722348514));
#58678=CARTESIAN_POINT('Ctrl Pts',(-0.298358508655174,1.97811592673419,
6.48274032867299));
#58679=CARTESIAN_POINT('Ctrl Pts',(-0.296789597914498,1.97439192923526,
6.48299329123514));
#58680=CARTESIAN_POINT('Ctrl Pts',(-0.296583978079407,1.97390718962834,
6.48302618223395));
#58681=CARTESIAN_POINT('Ctrl Pts',(-0.296270956595319,1.97317425721332,
6.48307585650819));
#58682=CARTESIAN_POINT('Ctrl Pts',(-0.296164430304366,1.97292569504783,
6.48309269273285));
#58683=CARTESIAN_POINT('Ctrl Pts',(-0.295979655634586,1.97249604716068,
6.48312177701995));
#58684=CARTESIAN_POINT('Ctrl Pts',(-0.295901553980528,1.97231489949139,
6.48313403404696));
#58685=CARTESIAN_POINT('Ctrl Pts',(-0.295738245746892,1.97193707965653,
6.48315958707906));
#58686=CARTESIAN_POINT('Ctrl Pts',(-0.295653009551372,1.97174042137837,
6.48317288118724));
#58687=CARTESIAN_POINT('Ctrl Pts',(-0.295416618790474,1.97119650469471,
6.48320963251142));
#58688=CARTESIAN_POINT('Ctrl Pts',(-0.295265047562389,1.97084942604879,
6.4832330641785));
#58689=CARTESIAN_POINT('Ctrl Pts',(-0.29466772673854,1.96948818576826,6.48332488864361));
#58690=CARTESIAN_POINT('Ctrl Pts',(-0.294217354368152,1.96847604283693,
6.48339300196234));
#58691=CARTESIAN_POINT('Ctrl Pts',(-0.285824346810446,1.94987290028494,
6.48464228601582));
#58692=CARTESIAN_POINT('Ctrl Pts',(-0.276321100630202,1.93302516984495,
6.48573132495378));
#58693=CARTESIAN_POINT('Ctrl Pts',(-0.2559928205353,1.90352692961752,6.48773743356918));
#58694=CARTESIAN_POINT('Ctrl Pts',(-0.245588722195322,1.89066737900363,
6.48865389446295));
#58695=CARTESIAN_POINT('Ctrl Pts',(-0.229112108465112,1.87322989638084,
6.49002771021757));
#58696=CARTESIAN_POINT('Ctrl Pts',(-0.223791753930463,1.86797784995627,
6.49046104336544));
#58697=CARTESIAN_POINT('Ctrl Pts',(-0.214934076170592,1.85982219755152,
6.49117118992359));
#58698=CARTESIAN_POINT('Ctrl Pts',(-0.21150901550838,1.85680056091025,6.49144323596642));
#58699=CARTESIAN_POINT('Ctrl Pts',(-0.206648876172002,1.85269321663257,
6.49182646327429));
#58700=CARTESIAN_POINT('Ctrl Pts',(-0.205267076805797,1.8515451145531,6.49193511236472));
#58701=CARTESIAN_POINT('Ctrl Pts',(-0.202861230213319,1.84957992699118,
6.49212379498689));
#58702=CARTESIAN_POINT('Ctrl Pts',(-0.201841657451197,1.84875741418385,
6.49220360823545));
#58703=CARTESIAN_POINT('Ctrl Pts',(-0.200384138285469,1.84759619811764,
6.49231750594974));
#58704=CARTESIAN_POINT('Ctrl Pts',(-0.199950280702594,1.84725236435923,
6.49235138491155));
#58705=CARTESIAN_POINT('Ctrl Pts',(-0.199226535766194,1.84668182358617,
6.49240786027095));
#58706=CARTESIAN_POINT('Ctrl Pts',(-0.198937140967943,1.8464544912708,6.49243043169911));
#58707=CARTESIAN_POINT('Ctrl Pts',(-0.198331873373952,1.84598070123244,
6.4924776178057));
#58708=CARTESIAN_POINT('Ctrl Pts',(-0.198015929278044,1.84573433599436,
6.49250223610215));
#58709=CARTESIAN_POINT('Ctrl Pts',(-0.19731868441456,1.84519272976638,6.49255653839377));
#58710=CARTESIAN_POINT('Ctrl Pts',(-0.196937179235094,1.84489775458869,
6.49258623284264));
#58711=CARTESIAN_POINT('Ctrl Pts',(-0.195602738664758,1.84387075880675,
6.49269003865474));
#58712=CARTESIAN_POINT('Ctrl Pts',(-0.194646381290574,1.84314321937085,
6.49276432639079));
#58713=CARTESIAN_POINT('Ctrl Pts',(-0.180235987978609,1.83230735216395,
6.4938821646308));
#58714=CARTESIAN_POINT('Ctrl Pts',(-0.166016803468828,1.82326434614998,
6.49496739069357));
#58715=CARTESIAN_POINT('Ctrl Pts',(-0.144090960856552,1.81162001856537,
6.49661471952838));
#58716=CARTESIAN_POINT('Ctrl Pts',(-0.136886087578603,1.80813118064035,
6.49715183037116));
#58717=CARTESIAN_POINT('Ctrl Pts',(-0.115848529602402,1.79889451791394,
6.49870228580871));
#58718=CARTESIAN_POINT('Ctrl Pts',(-0.101734891721652,1.79383758986947,
6.49972179280312));
#58719=CARTESIAN_POINT('Ctrl Pts',(-0.0800274595650272,1.78772738605329,
6.50122249589078));
#58720=CARTESIAN_POINT('Ctrl Pts',(-0.0726636081286285,1.78593217676732,
6.50172015116792));
#58721=CARTESIAN_POINT('Ctrl Pts',(-0.0620125190637705,1.78373033076195,
6.50241752456368));
#58722=CARTESIAN_POINT('Ctrl Pts',(-0.05877202844937,1.7831121539632,6.50262674672557));
#58723=CARTESIAN_POINT('Ctrl Pts',(-0.0550119404651455,1.78245452193384,
6.50286567132796));
#58724=CARTESIAN_POINT('Ctrl Pts',(-0.0545011960429062,1.78236646292809,
6.50289804337469));
#58725=CARTESIAN_POINT('Ctrl Pts',(-0.0537253352431158,1.78223462086409,
6.50294709254412));
#58726=CARTESIAN_POINT('Ctrl Pts',(-0.053460375936724,1.78218993717891,
6.5029638206315));
#58727=CARTESIAN_POINT('Ctrl Pts',(-0.0530009923093842,1.78211305582627,
6.50299278444998));
#58728=CARTESIAN_POINT('Ctrl Pts',(-0.0528065947318616,1.78208070518534,
6.50300502891636));
#58729=CARTESIAN_POINT('Ctrl Pts',(-0.0523998692832992,1.78201340338304,
6.50303062171758));
#58730=CARTESIAN_POINT('Ctrl Pts',(-0.0521875367374543,1.78197848667289,
6.50304396803739));
#58731=CARTESIAN_POINT('Ctrl Pts',(-0.0515972307284654,1.78188202179442,
6.50308103226511));
#58732=CARTESIAN_POINT('Ctrl Pts',(-0.0512191807084466,1.78182093436617,
6.50310472388172));
#58733=CARTESIAN_POINT('Ctrl Pts',(-0.04971551085765,1.78158071241237,6.50319877832356));
#58734=CARTESIAN_POINT('Ctrl Pts',(-0.0485890356039956,1.78140687320974,
6.50326884406176));
#58735=CARTESIAN_POINT('Ctrl Pts',(-0.0285911448495527,1.7784293045431,
6.50450606799246));
#58736=CARTESIAN_POINT('Ctrl Pts',(-0.00950519058157107,1.77730037052134,
6.50558339937685));
#58737=CARTESIAN_POINT('Ctrl Pts',(0.0261406239477286,1.77835946023586,
6.50758081032869));
#58738=CARTESIAN_POINT('Ctrl Pts',(0.0426472997564674,1.7801294745042,6.50850026678078));
#58739=CARTESIAN_POINT('Ctrl Pts',(0.0652822655045629,1.78434042508229,
6.50981815591815));
#58740=CARTESIAN_POINT('Ctrl Pts',(0.0715835665926123,1.78570948538023,
6.51019113565383));
#58741=CARTESIAN_POINT('Ctrl Pts',(0.0830062286094235,1.78855258482769,
6.51088193881122));
#58742=CARTESIAN_POINT('Ctrl Pts',(0.0881402302758181,1.78996641884462,
6.51119794356894));
#58743=CARTESIAN_POINT('Ctrl Pts',(0.0951629383555637,1.79208890841296,
6.51163896932012));
#58744=CARTESIAN_POINT('Ctrl Pts',(0.0970836986178495,1.79268911450801,
6.51176050624991));
#58745=CARTESIAN_POINT('Ctrl Pts',(0.0999299768158749,1.79360787698679,
6.51194201829872));
#58746=CARTESIAN_POINT('Ctrl Pts',(0.100859892107893,1.79391273230977,6.51200154596951));
#58747=CARTESIAN_POINT('Ctrl Pts',(0.10234016164324,1.79440548905383,6.51209666952114));
#58748=CARTESIAN_POINT('Ctrl Pts',(0.102891425711614,1.79459065450831,6.51213217535216));
#58749=CARTESIAN_POINT('Ctrl Pts',(0.103938687112864,1.79494557899081,6.51219978300012));
#58750=CARTESIAN_POINT('Ctrl Pts',(0.104434777803806,1.79511505836474,6.51223187550116));
#58751=CARTESIAN_POINT('Ctrl Pts',(0.105299999353866,1.79541300336072,6.51228796450383));
#58752=CARTESIAN_POINT('Ctrl Pts',(0.105669315148705,1.79554093178313,6.51231194316407));
#58753=CARTESIAN_POINT('Ctrl Pts',(0.106387095461984,1.79579102922956,6.51235861968455));
#58754=CARTESIAN_POINT('Ctrl Pts',(0.106735584688907,1.79591312600278,6.51238131511682));
#58755=CARTESIAN_POINT('Ctrl Pts',(0.107557869691453,1.79620280965626,6.51243494618325));
#58756=CARTESIAN_POINT('Ctrl Pts',(0.108031483787504,1.79637090603926,6.51246589871753));
#58757=CARTESIAN_POINT('Ctrl Pts',(0.109677097008734,1.7969593092355,6.51257366472926));
#58758=CARTESIAN_POINT('Ctrl Pts',(0.110847040786707,1.79738529555498,6.51265066713543));
#58759=CARTESIAN_POINT('Ctrl Pts',(0.125970494214967,1.80299134069976,6.51365113396894));
#58760=CARTESIAN_POINT('Ctrl Pts',(0.139549262891696,1.80912442907278,6.51460691548829));
#58761=CARTESIAN_POINT('Ctrl Pts',(0.161232773616753,1.82078673270039,6.51623139714973));
#58762=CARTESIAN_POINT('Ctrl Pts',(0.169597284621658,1.82578694934071,6.51688407825055));
#58763=CARTESIAN_POINT('Ctrl Pts',(0.191846725374177,1.84049527943609,6.51868369222193));
#58764=CARTESIAN_POINT('Ctrl Pts',(0.205213832211823,1.85093137361952,6.51983812182962));
#58765=CARTESIAN_POINT('Ctrl Pts',(0.223591584026318,1.86776770935582,6.52148528083735));
#58766=CARTESIAN_POINT('Ctrl Pts',(0.229281610023606,1.87338358233888,6.52200466386139));
#58767=CARTESIAN_POINT('Ctrl Pts',(0.235629694593427,1.8801331230414,6.52258934544858));
#58768=CARTESIAN_POINT('Ctrl Pts',(0.23649646410194,1.88106571955683,6.52266929577331));
#58769=CARTESIAN_POINT('Ctrl Pts',(0.237617638417225,1.88228646985619,6.52277283730607));
#58770=CARTESIAN_POINT('Ctrl Pts',(0.237877070936153,1.88256995970852,6.52279680495517));
#58771=CARTESIAN_POINT('Ctrl Pts',(0.23829726499828,1.88303077083446,6.52283563785442));
#58772=CARTESIAN_POINT('Ctrl Pts',(0.238458336180257,1.88320780729604,6.52285052669038));
#58773=CARTESIAN_POINT('Ctrl Pts',(0.238767640019753,1.88354853091216,6.52287912346315));
#58774=CARTESIAN_POINT('Ctrl Pts',(0.238915901214033,1.88371219050025,6.52289283354896));
#58775=CARTESIAN_POINT('Ctrl Pts',(0.23925752753382,1.88409007798021,6.52292443077763));
#58776=CARTESIAN_POINT('Ctrl Pts',(0.239450773809236,1.88430441397214,6.52294230884464));
#58777=CARTESIAN_POINT('Ctrl Pts',(0.240067585764723,1.88499039151306,6.52299938867727));
#58778=CARTESIAN_POINT('Ctrl Pts',(0.240490051211414,1.88546302705351,6.52303850760051));
#58779=CARTESIAN_POINT('Ctrl Pts',(0.244258333778891,1.88970393187527,6.52338768601719));
#58780=CARTESIAN_POINT('Ctrl Pts',(0.247516957569114,1.89354920079565,6.52369139449247));
#58781=CARTESIAN_POINT('Ctrl Pts',(0.260255767829884,1.90931680336318,6.52489331831766));
#58782=CARTESIAN_POINT('Ctrl Pts',(0.268976405466718,1.92182892003565,6.52575090668255));
#58783=CARTESIAN_POINT('Ctrl Pts',(0.28519040748839,1.94901268437145,6.52752279820172));
#58784=CARTESIAN_POINT('Ctrl Pts',(0.292510850531186,1.96373513391884,6.52843431397889));
#58785=CARTESIAN_POINT('Ctrl Pts',(0.302262763897536,1.98779700759307,6.52992210082112));
#58786=CARTESIAN_POINT('Ctrl Pts',(0.30545303041204,1.99679771049169,6.53047790248133));
#58787=CARTESIAN_POINT('Ctrl Pts',(0.309152562993284,2.00891947100515,6.53123307982606));
#58788=CARTESIAN_POINT('Ctrl Pts',(0.31002243276866,2.01192582602131,6.53142088461074));
#58789=CARTESIAN_POINT('Ctrl Pts',(0.311206592101632,2.01625350740349,6.53169216576253));
#58790=CARTESIAN_POINT('Ctrl Pts',(0.311556545343067,2.01756495310482,6.5317744955639));
#58791=CARTESIAN_POINT('Ctrl Pts',(0.312082893156295,2.01958867119098,6.53190174273652));
#58792=CARTESIAN_POINT('Ctrl Pts',(0.312265160002553,2.02029941131785,6.53194647090718));
#58793=CARTESIAN_POINT('Ctrl Pts',(0.312599963579255,2.02162373987984,6.53202988725153));
#58794=CARTESIAN_POINT('Ctrl Pts',(0.312753125180324,2.02223716786835,6.53206855510158));
#58795=CARTESIAN_POINT('Ctrl Pts',(0.313003454131965,2.02325246411535,6.53213260511041));
#58796=CARTESIAN_POINT('Ctrl Pts',(0.313101655540057,2.02365407765664,6.53215795386647));
#58797=CARTESIAN_POINT('Ctrl Pts',(0.313292756809693,2.02444219318942,6.53220772341406));
#58798=CARTESIAN_POINT('Ctrl Pts',(0.313385714968459,2.02482868039672,6.53223214227674));
#58799=CARTESIAN_POINT('Ctrl Pts',(0.31359930839239,2.02572400876739,6.53228873913749));
#58800=CARTESIAN_POINT('Ctrl Pts',(0.313719420419001,2.02623297251077,6.53232093391327));
#58801=CARTESIAN_POINT('Ctrl Pts',(0.314039521674849,2.0276042949426,6.53240773634923));
#58802=CARTESIAN_POINT('Ctrl Pts',(0.314237196322276,2.02846718440467,6.5324624182604));
#58803=CARTESIAN_POINT('Ctrl Pts',(0.315643664618939,2.03472504656623,6.5328594491829));
#58804=CARTESIAN_POINT('Ctrl Pts',(0.316716943648237,2.0401492351897,6.5332061171858));
#58805=CARTESIAN_POINT('Ctrl Pts',(0.323018217033364,2.07694206435334,6.53557655859086));
#58806=CARTESIAN_POINT('Ctrl Pts',(0.323716403297786,2.10890391905077,6.53775339437791));
#58807=CARTESIAN_POINT('Ctrl Pts',(0.318482233527883,2.15028676631206,6.54055209572546));
#58808=CARTESIAN_POINT('Ctrl Pts',(0.316782394627325,2.16007196335346,6.54121011226145));
#58809=CARTESIAN_POINT('Ctrl Pts',(0.313815489197909,2.17345264175993,6.54209177099681));
#58810=CARTESIAN_POINT('Ctrl Pts',(0.31293271615149,2.17712697391358,6.5423319330912));
#58811=CARTESIAN_POINT('Ctrl Pts',(0.311851162671223,2.1813038441737,6.54260205793298));
#58812=CARTESIAN_POINT('Ctrl Pts',(0.311715551264867,2.1818222332028,6.54263553192139));
#58813=CARTESIAN_POINT('Ctrl Pts',(0.311509061546128,2.18260359783216,6.54268590746918));
#58814=CARTESIAN_POINT('Ctrl Pts',(0.311439142580097,2.18286682249523,6.54270286424847));
#58815=CARTESIAN_POINT('Ctrl Pts',(0.311313093962704,2.18333894612362,6.54273325329548));
#58816=CARTESIAN_POINT('Ctrl Pts',(0.31125708780089,2.183547876743,6.54274669269961));
#58817=CARTESIAN_POINT('Ctrl Pts',(0.311135745278638,2.18399872873202,6.5427756746269));
#58818=CARTESIAN_POINT('Ctrl Pts',(0.311070337288588,2.18424062962062,6.54279121287173));
#58819=CARTESIAN_POINT('Ctrl Pts',(0.310893615555975,2.18489119404949,6.5428329701236));
#58820=CARTESIAN_POINT('Ctrl Pts',(0.31078177773036,2.18529971662458,6.54285915863868));
#58821=CARTESIAN_POINT('Ctrl Pts',(0.310265278141255,2.18717189240875,6.54297902892264));
#58822=CARTESIAN_POINT('Ctrl Pts',(0.3098510712756,2.18863292553078,6.5430721643837));
#58823=CARTESIAN_POINT('Ctrl Pts',(0.300471281894778,2.2208487460776,6.54511782978115));
#58824=CARTESIAN_POINT('Ctrl Pts',(0.286978505556387,2.25010516858085,6.54682814663942));
#58825=CARTESIAN_POINT('Ctrl Pts',(0.260088425521228,2.29105556364028,6.54960532502415));
#58826=CARTESIAN_POINT('Ctrl Pts',(0.249688055047145,2.3044601903934,6.55058818622405));
#58827=CARTESIAN_POINT('Ctrl Pts',(0.237612149603963,2.31772146431123,6.55167646404756));
#58828=CARTESIAN_POINT('Ctrl Pts',(0.236937459741789,2.31845550988153,6.55173710189994));
#58829=CARTESIAN_POINT('Ctrl Pts',(0.235858702922028,2.31961829375068,6.55183380007201));
#58830=CARTESIAN_POINT('Ctrl Pts',(0.235456844062191,2.32004907923247,6.55186976635934));
#58831=CARTESIAN_POINT('Ctrl Pts',(0.234691415113194,2.3208651079101,6.55193816790806));
#58832=CARTESIAN_POINT('Ctrl Pts',(0.234328071608558,2.32125056174142,6.55197059339633));
#58833=CARTESIAN_POINT('Ctrl Pts',(0.23369431536455,2.32191957128155,6.5520270751825));
#58834=CARTESIAN_POINT('Ctrl Pts',(0.23342433199294,2.32220353368691,6.55205111291031));
#58835=CARTESIAN_POINT('Ctrl Pts',(0.232899831868157,2.3227531802419,6.55209776562651));
#58836=CARTESIAN_POINT('Ctrl Pts',(0.23264537654844,2.32301892242809,6.55212037793161));
#58837=CARTESIAN_POINT('Ctrl Pts',(0.23204591774514,2.32364282906568,6.55217360084294));
#58838=CARTESIAN_POINT('Ctrl Pts',(0.231700539930969,2.32400063108384,6.55220422772685));
#58839=CARTESIAN_POINT('Ctrl Pts',(0.23050853290654,2.32522981145031,6.55230980327229));
#58840=CARTESIAN_POINT('Ctrl Pts',(0.229657813119754,2.32609719263374,6.55238493083617));
#58841=CARTESIAN_POINT('Ctrl Pts',(0.219514719096297,2.33632262945309,6.55327813385003));
#58842=CARTESIAN_POINT('Ctrl Pts',(0.209662526328,2.34510536846211,6.5541214233853));
#58843=CARTESIAN_POINT('Ctrl Pts',(0.179920484911499,2.36851074168235,6.55660396240831));
#58844=CARTESIAN_POINT('Ctrl Pts',(0.15885390277515,2.38148642155011,6.55829536378963));
#58845=CARTESIAN_POINT('Ctrl Pts',(0.128516911978139,2.39567312370475,6.56053704943688));
#58846=CARTESIAN_POINT('Ctrl Pts',(0.120364697394606,2.39908453260391,6.56112114291632));
#58847=CARTESIAN_POINT('Ctrl Pts',(0.108405332242408,2.40352073661635,6.5619424633761));
#58848=CARTESIAN_POINT('Ctrl Pts',(0.104703856327779,2.40481742000188,6.56219187496208));
#58849=CARTESIAN_POINT('Ctrl Pts',(0.100466144879292,2.40621564542868,6.5624712701139));
#58850=CARTESIAN_POINT('Ctrl Pts',(0.0999524268810275,2.40638371389958,
6.56250503783142));
#58851=CARTESIAN_POINT('Ctrl Pts',(0.0991783045902107,2.40663482226382,
6.56255576631305));
#58852=CARTESIAN_POINT('Ctrl Pts',(0.0989182167833165,2.40671882354348,
6.56257278345768));
#58853=CARTESIAN_POINT('Ctrl Pts',(0.0984501231351375,2.40686934772098,
6.56260336205983));
#58854=CARTESIAN_POINT('Ctrl Pts',(0.0982421569839919,2.40693598991992,
6.56261693055362));
#58855=CARTESIAN_POINT('Ctrl Pts',(0.0977953665679315,2.40707866210356,
6.56264604413695));
#58856=CARTESIAN_POINT('Ctrl Pts',(0.0975565220298319,2.40715462466311,
6.56266158518031));
#58857=CARTESIAN_POINT('Ctrl Pts',(0.0969136241461207,2.40735826756444,
6.56270335723016));
#58858=CARTESIAN_POINT('Ctrl Pts',(0.0965094054311341,2.40748543031101,
6.56272955770777));
#58859=CARTESIAN_POINT('Ctrl Pts',(0.0946537190578215,2.40806518901736,
6.56284955274681));
#58860=CARTESIAN_POINT('Ctrl Pts',(0.0931992799997537,2.40850831696512,
6.56294279961969));
#58861=CARTESIAN_POINT('Ctrl Pts',(0.0610437557669386,2.41805707192222,
6.56498780904822));
#58862=CARTESIAN_POINT('Ctrl Pts',(0.0291528022426285,2.42254855126251,
6.56669756083612));
#58863=CARTESIAN_POINT('Ctrl Pts',(-0.0185596787889771,2.42212193200753,
6.56940236004781));
#58864=CARTESIAN_POINT('Ctrl Pts',(-0.0342047289446672,2.42083787323481,
6.57031018052081));
#58865=CARTESIAN_POINT('Ctrl Pts',(-0.0521360208321992,2.41803950179141,
6.57140475643834));
#58866=CARTESIAN_POINT('Ctrl Pts',(-0.0545745251660122,2.41763014662507,
6.57155474737915));
#58867=CARTESIAN_POINT('Ctrl Pts',(-0.0577067638734682,2.41706719955389,
6.57174895348593));
#58868=CARTESIAN_POINT('Ctrl Pts',(-0.0584050799225414,2.416939310052,6.57179234973643));
#58869=CARTESIAN_POINT('Ctrl Pts',(-0.0595301196962569,2.41672942598826,
6.57186242608498));
#58870=CARTESIAN_POINT('Ctrl Pts',(-0.0599571127946968,2.41664887345497,
6.57188906018629));
#58871=CARTESIAN_POINT('Ctrl Pts',(-0.0607703984588084,2.41649374256094,
6.57193986184309));
#58872=CARTESIAN_POINT('Ctrl Pts',(-0.0611567202126165,2.41641931985852,
6.57196402439151));
#58873=CARTESIAN_POINT('Ctrl Pts',(-0.0620376499397637,2.41624794015645,
6.57201919360008));
#58874=CARTESIAN_POINT('Ctrl Pts',(-0.0625321677823352,2.4161505300503,
6.57205021467716));
#58875=CARTESIAN_POINT('Ctrl Pts',(-0.0640413036967127,2.41584958117044,
6.57214504069386));
#58876=CARTESIAN_POINT('Ctrl Pts',(-0.0650551642646875,2.41564231666113,
6.5722089645422));
#58877=CARTESIAN_POINT('Ctrl Pts',(-0.0724680185498928,2.41408966731579,
6.57267796594517));
#58878=CARTESIAN_POINT('Ctrl Pts',(-0.0788253440380896,2.41255477578564,
6.57308908740827));
#58879=CARTESIAN_POINT('Ctrl Pts',(-0.0874050759989636,2.41020491052734,
6.57365670544542));
#58880=CARTESIAN_POINT('Ctrl Pts',(-0.0896719671096978,2.40955721875744,
6.57380790384475));
#58881=CARTESIAN_POINT('Ctrl Pts',(-0.115608626024277,2.40183784704886,
6.57555196700301));
#58882=CARTESIAN_POINT('Ctrl Pts',(-0.138394098259906,2.39209272466296,
6.57722910029268));
#58883=CARTESIAN_POINT('Ctrl Pts',(-0.161202130629033,2.37906542832811,
6.57900264634036));
#58884=CARTESIAN_POINT('Ctrl Pts',(-0.162559634867899,2.3782768502201,6.57910855095055));
#58885=CARTESIAN_POINT('Ctrl Pts',(-0.169442264934589,2.37421116034017,
6.57964710563233));
#58886=CARTESIAN_POINT('Ctrl Pts',(-0.17487449945034,2.37077916729813,6.58007752232645));
#58887=CARTESIAN_POINT('Ctrl Pts',(-0.185428670054059,2.36366104693505,
6.580919950602));
#58888=CARTESIAN_POINT('Ctrl Pts',(-0.190552393365375,2.359982183553,6.58133198139306));
#58889=CARTESIAN_POINT('Ctrl Pts',(-0.19800028162625,2.35429598903102,6.58193180361376));
#58890=CARTESIAN_POINT('Ctrl Pts',(-0.200408850120782,2.35240217123401,
6.58212592018641));
#58891=CARTESIAN_POINT('Ctrl Pts',(-0.203185321176402,2.35015427120927,
6.58234949314189));
#58892=CARTESIAN_POINT('Ctrl Pts',(-0.2035797368622,2.34983339427173,6.5823812484604));
#58893=CARTESIAN_POINT('Ctrl Pts',(-0.204179825980537,2.34934282700711,
6.58242955370517));
#58894=CARTESIAN_POINT('Ctrl Pts',(-0.204386048644261,2.34917381451139,
6.58244615228252));
#58895=CARTESIAN_POINT('Ctrl Pts',(-0.204744160587552,2.34887957546118,
6.58247497292661));
#58896=CARTESIAN_POINT('Ctrl Pts',(-0.204896144490074,2.34875446599054,
6.58248720345338));
#58897=CARTESIAN_POINT('Ctrl Pts',(-0.205239296216202,2.34847146393095,
6.58251481531334));
#58898=CARTESIAN_POINT('Ctrl Pts',(-0.205430396120943,2.34831349026966,
6.58253019059712));
#58899=CARTESIAN_POINT('Ctrl Pts',(-0.205946783532397,2.34788561200102,
6.58257173357458));
#58900=CARTESIAN_POINT('Ctrl Pts',(-0.206271724094448,2.34761528654023,
6.58259787061055));
#58901=CARTESIAN_POINT('Ctrl Pts',(-0.2077202289483,2.3464054123774,6.58271436919698));
#58902=CARTESIAN_POINT('Ctrl Pts',(-0.208837935277838,2.34545883105568,
6.58280422536109));
#58903=CARTESIAN_POINT('Ctrl Pts',(-0.231494546378991,2.32600424418803,
6.58462582276576));
#58904=CARTESIAN_POINT('Ctrl Pts',(-0.250504147151153,2.30473377200297,
6.586164726351));
#58905=CARTESIAN_POINT('Ctrl Pts',(-0.278262413253177,2.26392091465782,
6.58893944405263));
#58906=CARTESIAN_POINT('Ctrl Pts',(-0.288324958338725,2.24549417838805,
6.59014109462002));
#58907=CARTESIAN_POINT('Ctrl Pts',(-0.297017964400265,2.22507225552453,
6.59148983028058));
#58908=CARTESIAN_POINT('Ctrl Pts',(-0.297501169991604,2.22391849766322,
6.59156606624788));
#58909=CARTESIAN_POINT('Ctrl Pts',(-0.298185125033141,2.22225834743568,
6.59167582698931));
#58910=CARTESIAN_POINT('Ctrl Pts',(-0.298391330660344,2.22175420358135,
6.5917091668934));
#58911=CARTESIAN_POINT('Ctrl Pts',(-0.298746615801498,2.22087925748714,
6.59176704418544));
#58912=CARTESIAN_POINT('Ctrl Pts',(-0.298896285929663,2.22050869511624,
6.59179156155729));
#58913=CARTESIAN_POINT('Ctrl Pts',(-0.299182501635492,2.21979625147667,
6.59183870836425));
#58914=CARTESIAN_POINT('Ctrl Pts',(-0.299319151535049,2.2194544125402,6.59186133423539));
#58915=CARTESIAN_POINT('Ctrl Pts',(-0.299639336338036,2.21864944969625,
6.59191462408014));
#58916=CARTESIAN_POINT('Ctrl Pts',(-0.299822383334796,2.21818613387922,
6.59194530443323));
#58917=CARTESIAN_POINT('Ctrl Pts',(-0.300358861613304,2.21681896991571,
6.59203586171084));
#58918=CARTESIAN_POINT('Ctrl Pts',(-0.300709282892866,2.21591395356405,
6.59209583963814));
#58919=CARTESIAN_POINT('Ctrl Pts',(-0.303746584613286,2.20796318773336,
6.59262306135422));
#58920=CARTESIAN_POINT('Ctrl Pts',(-0.306189299510039,2.20082725323033,
6.59309841502821));
#58921=CARTESIAN_POINT('Ctrl Pts',(-0.309906926140884,2.18858062828711,
6.59391882785019));
#58922=CARTESIAN_POINT('Ctrl Pts',(-0.311311005847503,2.18351217512201,
6.5942596549374));
#58923=CARTESIAN_POINT('Ctrl Pts',(-0.313297705766731,2.17559215671941,
6.59479406257193));
#58924=CARTESIAN_POINT('Ctrl Pts',(-0.313966813338072,2.17276308130807,
6.59498530914165));
#58925=CARTESIAN_POINT('Ctrl Pts',(-0.319715117439977,2.14690120075679,
6.59673634378382));
#58926=CARTESIAN_POINT('Ctrl Pts',(-0.322289258550463,2.12338728256337,
6.59835561527569));
#58927=CARTESIAN_POINT('Ctrl Pts',(-0.322272956104475,2.09653565802172,
6.60014663846072));
#58928=CARTESIAN_POINT('Ctrl Pts',(-0.322221242681646,2.09326711248847,
6.60036354200454));
#58929=CARTESIAN_POINT('Ctrl Pts',(-0.322093711926189,2.0891591616064,6.60063434088577));
#58930=CARTESIAN_POINT('Ctrl Pts',(-0.32206432218159,2.08831858567874,6.60068965684094));
#58931=CARTESIAN_POINT('Ctrl Pts',(-0.322004108188569,2.08677003044707,
6.60079137646901));
#58932=CARTESIAN_POINT('Ctrl Pts',(-0.321974238931584,2.08606202081072,
6.60083781150307));
#58933=CARTESIAN_POINT('Ctrl Pts',(-0.321892349648388,2.08426195246846,
6.60095567785508));
#58934=CARTESIAN_POINT('Ctrl Pts',(-0.321837107006106,2.08317004116589,
6.60102699546791));
#58935=CARTESIAN_POINT('Ctrl Pts',(-0.321725315800544,2.08116286548787,
6.60115773884758));
#58936=CARTESIAN_POINT('Ctrl Pts',(-0.32167041545863,2.0802475237296,6.60121722680186));
#58937=CARTESIAN_POINT('Ctrl Pts',(-0.321602822166345,2.07919569345824,
6.60128542019758));
#58938=CARTESIAN_POINT('Ctrl Pts',(-0.321593948640068,2.07905897341921,
6.60129428097452));
#58939=CARTESIAN_POINT('Ctrl Pts',(-0.321556524191658,2.07848798525191,
6.60133127301996));
#58940=CARTESIAN_POINT('Ctrl Pts',(-0.321527180665637,2.07805376738307,
6.60135937166211));
#58941=CARTESIAN_POINT('Ctrl Pts',(-0.321215225898136,2.07357250055268,
6.60164901324086));
#58942=CARTESIAN_POINT('Ctrl Pts',(-0.320857083298464,2.06953083586833,
6.60190733662367));
#58943=CARTESIAN_POINT('Ctrl Pts',(-0.320365218657665,2.06496301213095,
6.60219518875027));
#58944=CARTESIAN_POINT('Ctrl Pts',(-0.320306407405511,2.0644293768773,6.60222875345477));
#58945=CARTESIAN_POINT('Ctrl Pts',(-0.320215306413238,2.06362130407119,
6.60227948091063));
#58946=CARTESIAN_POINT('Ctrl Pts',(-0.320183997097856,2.06334676027073,
6.60229669833238));
#58947=CARTESIAN_POINT('Ctrl Pts',(-0.320128891534884,2.06286901176374,
6.60232662878567));
#58948=CARTESIAN_POINT('Ctrl Pts',(-0.320105254876724,2.06266578936656,
6.60233935084768));
#58949=CARTESIAN_POINT('Ctrl Pts',(-0.320055285274006,2.06223969867003,
6.60236600448215));
#58950=CARTESIAN_POINT('Ctrl Pts',(-0.320028913063907,2.06201683541559,
6.60237993374532));
#58951=CARTESIAN_POINT('Ctrl Pts',(-0.319965043463828,2.06148188228979,
6.60241334133741));
#58952=CARTESIAN_POINT('Ctrl Pts',(-0.319927322089582,2.06116981826796,
6.60243280694771));
#58953=CARTESIAN_POINT('Ctrl Pts',(-0.319796734203696,2.06010259016257,
6.60249930143886));
#58954=CARTESIAN_POINT('Ctrl Pts',(-0.319701649116596,2.05934769257635,
6.60254620577905));
#58955=CARTESIAN_POINT('Ctrl Pts',(-0.317380790370106,2.04143386617511,
6.60365631158666));
#58956=CARTESIAN_POINT('Ctrl Pts',(-0.313779010516772,2.02447860488013,
6.60464357552217));
#58957=CARTESIAN_POINT('Ctrl Pts',(-0.301976775891885,1.98490629694215,
6.60696501134263));
#58958=CARTESIAN_POINT('Ctrl Pts',(-0.292577119968493,1.96275893268245,
6.60828353327848));
#58959=CARTESIAN_POINT('Ctrl Pts',(-0.27632343650692,1.93389751449061,6.61021633595446));
#58960=CARTESIAN_POINT('Ctrl Pts',(-0.27150322067352,1.9261303524574,6.61075951804212));
#58961=CARTESIAN_POINT('Ctrl Pts',(-0.265720380824297,1.91764006659532,
6.6113842601));
#58962=CARTESIAN_POINT('Ctrl Pts',(-0.265075935290741,1.91670457022946,
6.61145353242008));
#58963=CARTESIAN_POINT('Ctrl Pts',(-0.264130465538938,1.91534751261913,
6.61155466492517));
#58964=CARTESIAN_POINT('Ctrl Pts',(-0.263833344695421,1.91492323175601,
6.61158637607559));
#58965=CARTESIAN_POINT('Ctrl Pts',(-0.263306876457105,1.91417529284326,
6.61164244183178));
#58966=CARTESIAN_POINT('Ctrl Pts',(-0.263077951375463,1.91385133769661,
6.61166678021621));
#58967=CARTESIAN_POINT('Ctrl Pts',(-0.262603128364511,1.91318203424247,
6.61171717773355));
#58968=CARTESIAN_POINT('Ctrl Pts',(-0.262357146043624,1.91283674699953,
6.61174324008208));
#58969=CARTESIAN_POINT('Ctrl Pts',(-0.261725029852129,1.91195313544969,
6.61181009689063));
#58970=CARTESIAN_POINT('Ctrl Pts',(-0.261337917462433,1.91141551653376,
6.61185092905998));
#58971=CARTESIAN_POINT('Ctrl Pts',(-0.259745921143715,1.90921887890045,
6.61201840020462));
#58972=CARTESIAN_POINT('Ctrl Pts',(-0.258526896249008,1.9075702119671,6.61214558676522));
#58973=CARTESIAN_POINT('Ctrl Pts',(-0.250350834270083,1.89673044630774,
6.61299191475865));
#58974=CARTESIAN_POINT('Ctrl Pts',(-0.242921479923631,1.88790767896034,
6.61372974241548));
#58975=CARTESIAN_POINT('Ctrl Pts',(-0.21250712649406,1.85548790827707,6.61663963451552));
#58976=CARTESIAN_POINT('Ctrl Pts',(-0.18643512863399,1.83507184396763,6.61893723242836));
#58977=CARTESIAN_POINT('Ctrl Pts',(-0.153399672977918,1.81653160745439,
6.6213936917021));
#58978=CARTESIAN_POINT('Ctrl Pts',(-0.149017447459071,1.81420357537402,
6.62171083030969));
#58979=CARTESIAN_POINT('Ctrl Pts',(-0.144074989921747,1.811722536583,6.62205747633366));
#58980=CARTESIAN_POINT('Ctrl Pts',(-0.143566377095639,1.81146890286419,
6.62209302012971));
#58981=CARTESIAN_POINT('Ctrl Pts',(-0.142802288471738,1.81109038975963,
6.62214622205551));
#58982=CARTESIAN_POINT('Ctrl Pts',(-0.142547317389401,1.81096450254575,
6.62216394259694));
#58983=CARTESIAN_POINT('Ctrl Pts',(-0.142106757929065,1.81074770928801,
6.62219450492392));
#58984=CARTESIAN_POINT('Ctrl Pts',(-0.141921248686971,1.81065664427376,
6.62220735668772));
#58985=CARTESIAN_POINT('Ctrl Pts',(-0.141535610414867,1.81046779760793,
6.6222340368884));
#58986=CARTESIAN_POINT('Ctrl Pts',(-0.141335467871401,1.81037004512766,
6.62224786341812));
#58987=CARTESIAN_POINT('Ctrl Pts',(-0.140860870605367,1.8101388541247,6.62228060261706));
#58988=CARTESIAN_POINT('Ctrl Pts',(-0.140586326462323,1.81000559734797,
6.62229950385664));
#58989=CARTESIAN_POINT('Ctrl Pts',(-0.139674574356821,1.80956465503476,
6.62236215067675));
#58990=CARTESIAN_POINT('Ctrl Pts',(-0.139036536613415,1.80925867539049,
6.62240579042705));
#58991=CARTESIAN_POINT('Ctrl Pts',(-0.12167629344045,1.80100355200804,6.623587888039));
#58992=CARTESIAN_POINT('Ctrl Pts',(-0.104298022489748,1.79450671783784,
6.62463905094674));
#58993=CARTESIAN_POINT('Ctrl Pts',(-0.0623097354637593,1.78281409790137,
6.62708428286339));
#58994=CARTESIAN_POINT('Ctrl Pts',(-0.0374643903824467,1.77893034319031,
6.62846567043877));
#58995=CARTESIAN_POINT('Ctrl Pts',(-0.0119401907742147,1.77794590747969,
6.62997025003553));
#58996=CARTESIAN_POINT('Ctrl Pts',(-0.0114598428059394,1.77792845722683,
6.62999859253812));
#58997=CARTESIAN_POINT('Ctrl Pts',(-0.0043846379138922,1.77768727486621,
6.63041647095283));
#58998=CARTESIAN_POINT('Ctrl Pts',(0.00221513620775677,1.77766507862802,
6.63081159301556));
#58999=CARTESIAN_POINT('Ctrl Pts',(0.00984781068270887,1.77787382464165,
6.63127629289522));
#59000=CARTESIAN_POINT('Ctrl Pts',(0.0108848641264693,1.77790719983255,
6.63133959609801));
#59001=CARTESIAN_POINT('Ctrl Pts',(0.0124259545084263,1.77796424752613,
6.63143391660346));
#59002=CARTESIAN_POINT('Ctrl Pts',(0.0129301333053778,1.77798409687565,
6.63146481404263));
#59003=CARTESIAN_POINT('Ctrl Pts',(0.0138274128395668,1.77802153314783,
6.63151987337695));
#59004=CARTESIAN_POINT('Ctrl Pts',(0.0142205327627943,1.7780386561898,6.63154402068141));
#59005=CARTESIAN_POINT('Ctrl Pts',(0.015047406020875,1.77807618951689,6.63159486308492));
#59006=CARTESIAN_POINT('Ctrl Pts',(0.0154811511396879,1.77809675655505,
6.63162156305284));
#59007=CARTESIAN_POINT('Ctrl Pts',(0.0166226138978508,1.77815319407498,
6.63169190761134));
#59008=CARTESIAN_POINT('Ctrl Pts',(0.0173302542044033,1.77819052212011,
6.63173559783877));
#59009=CARTESIAN_POINT('Ctrl Pts',(0.0204938978501519,1.77836786954533,
6.63193128900987));
#59010=CARTESIAN_POINT('Ctrl Pts',(0.0229483208069975,1.77853367015751,
6.63208409663153));
#59011=CARTESIAN_POINT('Ctrl Pts',(0.0408958379445197,1.77995264285547,
6.63320895506484));
#59012=CARTESIAN_POINT('Ctrl Pts',(0.0562798272310379,1.78229693999802,
6.63421550780486));
#59013=CARTESIAN_POINT('Ctrl Pts',(0.0996759653945203,1.79216113708756,
6.63717156661772));
#59014=CARTESIAN_POINT('Ctrl Pts',(0.126922666148529,1.80235826977959,6.63918181129921));
#59015=CARTESIAN_POINT('Ctrl Pts',(0.153117495314163,1.81642143922152,6.64110327697467));
#59016=CARTESIAN_POINT('Ctrl Pts',(0.153794026069427,1.81678777379333,6.64115288408811));
#59017=CARTESIAN_POINT('Ctrl Pts',(0.157714359585299,1.81892878472342,6.64144021118266));
#59018=CARTESIAN_POINT('Ctrl Pts',(0.160928909144305,1.82075685079156,6.64167527713365));
#59019=CARTESIAN_POINT('Ctrl Pts',(0.16461079709705,1.82293539066012,6.64194326977046));
#59020=CARTESIAN_POINT('Ctrl Pts',(0.165109350714285,1.82323220095402,6.64197953100254));
#59021=CARTESIAN_POINT('Ctrl Pts',(0.165848453949092,1.82367492857575,6.64203324497753));
#59022=CARTESIAN_POINT('Ctrl Pts',(0.166089614960133,1.82381981501425,6.64205076440057));
#59023=CARTESIAN_POINT('Ctrl Pts',(0.166518313202314,1.82407813600565,6.642081895075));
#59024=CARTESIAN_POINT('Ctrl Pts',(0.166705924357836,1.82419144602289,6.64209551446522));
#59025=CARTESIAN_POINT('Ctrl Pts',(0.167099207688071,1.82442952211529,6.64212405517522));
#59026=CARTESIAN_POINT('Ctrl Pts',(0.167304855174735,1.82455432672221,6.64213897385418));
#59027=CARTESIAN_POINT('Ctrl Pts',(0.167849442914818,1.82488566436172,6.64217846758175));
#59028=CARTESIAN_POINT('Ctrl Pts',(0.168188143043823,1.82509259430858,6.64220301653856));
#59029=CARTESIAN_POINT('Ctrl Pts',(0.16893231785014,1.82554914041771,6.64225692604055));
#59030=CARTESIAN_POINT('Ctrl Pts',(0.169337624246516,1.82579903107213,6.64228626875434));
#59031=CARTESIAN_POINT('Ctrl Pts',(0.170538942534619,1.82654338036977,6.6423731895107));
#59032=CARTESIAN_POINT('Ctrl Pts',(0.171333361490152,1.82704041868715,6.64243060350788));
#59033=CARTESIAN_POINT('Ctrl Pts',(0.180213610300974,1.83265050250469,6.64307178761961));
#59034=CARTESIAN_POINT('Ctrl Pts',(0.188070955387116,1.83811824545422,6.64363350236649));
#59035=CARTESIAN_POINT('Ctrl Pts',(0.214489214360279,1.8583054220564,6.64554510701098));
#59036=CARTESIAN_POINT('Ctrl Pts',(0.231663114120729,1.8747130369459,6.64683466922115));
#59037=CARTESIAN_POINT('Ctrl Pts',(0.250542492395792,1.89721435963641,6.64850486760126));
#59038=CARTESIAN_POINT('Ctrl Pts',(0.254083828913118,1.90166956822271,6.64883110578064));
#59039=CARTESIAN_POINT('Ctrl Pts',(0.263867026515596,1.91466974084824,6.64977473248237));
#59040=CARTESIAN_POINT('Ctrl Pts',(0.269808047179066,1.92343076709371,6.65040102299436));
#59041=CARTESIAN_POINT('Ctrl Pts',(0.275919907296202,1.93347441651751,6.65111583007051));
#59042=CARTESIAN_POINT('Ctrl Pts',(0.276527163216149,1.93448476462156,6.65118769829599));
#59043=CARTESIAN_POINT('Ctrl Pts',(0.277373085198512,1.93590985354051,6.65128902259934));
#59044=CARTESIAN_POINT('Ctrl Pts',(0.277616396628106,1.93632183750737,6.65131830949718));
#59045=CARTESIAN_POINT('Ctrl Pts',(0.278061261086454,1.9370789441438,6.6513721212519));
#59046=CARTESIAN_POINT('Ctrl Pts',(0.278263091613831,1.93742390335133,6.65139663597726));
#59047=CARTESIAN_POINT('Ctrl Pts',(0.278671020541204,1.93812410121668,6.65144638940773));
#59048=CARTESIAN_POINT('Ctrl Pts',(0.278877082571272,1.93847936011012,6.65147162937053));
#59049=CARTESIAN_POINT('Ctrl Pts',(0.279383141225968,1.939355680066,6.65153388114936));
#59050=CARTESIAN_POINT('Ctrl Pts',(0.279682358944881,1.93987718708582,6.65157092101362));
#59051=CARTESIAN_POINT('Ctrl Pts',(0.280771240981623,1.94178736509621,6.6517065682485));
#59052=CARTESIAN_POINT('Ctrl Pts',(0.281552026293484,1.94318104722937,6.65180549435269));
#59053=CARTESIAN_POINT('Ctrl Pts',(0.2918637822684,1.9619125381584,6.65313465414971));
#59054=CARTESIAN_POINT('Ctrl Pts',(0.299787065605716,1.98008306812772,6.6544230829428));
#59055=CARTESIAN_POINT('Ctrl Pts',(0.313669554506166,2.02208473169073,6.65738506005834));
#59056=CARTESIAN_POINT('Ctrl Pts',(0.318676531929856,2.04610509787584,6.65907000627506));
#59057=CARTESIAN_POINT('Ctrl Pts',(0.321440352670845,2.07613147534416,6.6610336213089));
#59058=CARTESIAN_POINT('Ctrl Pts',(0.321811972000446,2.08181562717994,6.6613987755048));
#59059=CARTESIAN_POINT('Ctrl Pts',(0.322058145387035,2.08816128093234,6.66179694577708));
#59060=CARTESIAN_POINT('Ctrl Pts',(0.322081531968261,2.08881558843204,6.66183788921779));
#59061=CARTESIAN_POINT('Ctrl Pts',(0.322112479369901,2.08976223797089,6.66189695908852));
#59062=CARTESIAN_POINT('Ctrl Pts',(0.322121636314034,2.09005452076652,6.66191517418997));
#59063=CARTESIAN_POINT('Ctrl Pts',(0.322137028731784,2.09056817161309,6.66194714404775));
#59064=CARTESIAN_POINT('Ctrl Pts',(0.322143433868209,2.09078953401528,6.6619609083776));
#59065=CARTESIAN_POINT('Ctrl Pts',(0.322156240369632,2.09124849114401,6.66198941846315));
#59066=CARTESIAN_POINT('Ctrl Pts',(0.322162607055424,2.09148608594818,6.66200416221949));
#59067=CARTESIAN_POINT('Ctrl Pts',(0.322178193742005,2.09209282274428,6.66204177380023));
#59068=CARTESIAN_POINT('Ctrl Pts',(0.322187042198194,2.0924619752037,6.66206462069132));
#59069=CARTESIAN_POINT('Ctrl Pts',(0.322220808277631,2.09397954941442,6.66215839504681));
#59070=CARTESIAN_POINT('Ctrl Pts',(0.322240220687506,2.09512810333524,6.66222901724266));
#59071=CARTESIAN_POINT('Ctrl Pts',(0.322424833033489,2.11110663858217,6.66320694538956));
#59072=CARTESIAN_POINT('Ctrl Pts',(0.321572294807177,2.1259328754125,6.66406005642422));
#59073=CARTESIAN_POINT('Ctrl Pts',(0.317636179035466,2.15688975863748,6.66582242766279));
#59074=CARTESIAN_POINT('Ctrl Pts',(0.314336799815608,2.17294913113394,6.66672643266804));
#59075=CARTESIAN_POINT('Ctrl Pts',(0.304757378828396,2.20641466622414,6.66869333684917));
#59076=CARTESIAN_POINT('Ctrl Pts',(0.298172274796948,2.22367006161451,6.66975912745724));
#59077=CARTESIAN_POINT('Ctrl Pts',(0.289588998660437,2.24142504502064,6.67095699769655));
#59078=CARTESIAN_POINT('Ctrl Pts',(0.289022002074959,2.24258020110023,6.67103539770377));
#59079=CARTESIAN_POINT('Ctrl Pts',(0.288220779409782,2.24418813318997,6.67114519001482));
#59080=CARTESIAN_POINT('Ctrl Pts',(0.287992368980336,2.24464380678333,6.67117637885386));
#59081=CARTESIAN_POINT('Ctrl Pts',(0.287595793671669,2.24543030223995,6.67123034095924));
#59082=CARTESIAN_POINT('Ctrl Pts',(0.287428136144098,2.24576137999518,6.67125309639639));
#59083=CARTESIAN_POINT('Ctrl Pts',(0.287079671705101,2.24644656295273,6.6713002730786));
#59084=CARTESIAN_POINT('Ctrl Pts',(0.286898780676985,2.24680062449059,6.67132469725388));
#59085=CARTESIAN_POINT('Ctrl Pts',(0.286474013425777,2.24762824591477,6.67138189733892));
#59086=CARTESIAN_POINT('Ctrl Pts',(0.286229617952679,2.24810153666108,6.6714146915096));
#59087=CARTESIAN_POINT('Ctrl Pts',(0.285437999652594,2.24962528831241,6.6715205419012));
#59088=CARTESIAN_POINT('Ctrl Pts',(0.284886163545573,2.25067332978498,6.67159376103359));
#59089=CARTESIAN_POINT('Ctrl Pts',(0.279984447835828,2.25985941915393,6.67223922408107));
#59090=CARTESIAN_POINT('Ctrl Pts',(0.27529308552387,2.26780945705125,6.67282362664537));
#59091=CARTESIAN_POINT('Ctrl Pts',(0.26594508137182,2.2822014219522,6.67393219226125));
#59092=CARTESIAN_POINT('Ctrl Pts',(0.261378616761615,2.28869379424179,6.67445292578714));
#59093=CARTESIAN_POINT('Ctrl Pts',(0.24395391162551,2.31161965387523,6.67636543473339));
#59094=CARTESIAN_POINT('Ctrl Pts',(0.229747551353077,2.32696335852053,6.67779353296056));
#59095=CARTESIAN_POINT('Ctrl Pts',(0.210392584851175,2.3441752460367,6.67952672896297));
#59096=CARTESIAN_POINT('Ctrl Pts',(0.20654713192356,2.34743661188732,6.67986173134638));
#59097=CARTESIAN_POINT('Ctrl Pts',(0.201388699498098,2.35160743538036,6.68029749026662));
#59098=CARTESIAN_POINT('Ctrl Pts',(0.200143377555439,2.35259916550958,6.68040167525754));
#59099=CARTESIAN_POINT('Ctrl Pts',(0.194303158707849,2.35717980240808,6.6808853886833));
#59100=CARTESIAN_POINT('Ctrl Pts',(0.189618412515926,2.3606530961014,6.68125944002314));
#59101=CARTESIAN_POINT('Ctrl Pts',(0.184301917989786,2.36437551469702,6.68166638845782));
#59102=CARTESIAN_POINT('Ctrl Pts',(0.183761021906018,2.36475176409661,6.68170759354653));
#59103=CARTESIAN_POINT('Ctrl Pts',(0.182999470483632,2.36527804397849,6.6817653266783));
#59104=CARTESIAN_POINT('Ctrl Pts',(0.182779781593757,2.36542946003816,6.68178194850408));
#59105=CARTESIAN_POINT('Ctrl Pts',(0.182376562742072,2.36570663236852,6.68181239592652));
#59106=CARTESIAN_POINT('Ctrl Pts',(0.182193090199527,2.36583247169365,6.68182622721691));
#59107=CARTESIAN_POINT('Ctrl Pts',(0.181818800492192,2.36608861832693,6.6818543966148));
#59108=CARTESIAN_POINT('Ctrl Pts',(0.181627973458669,2.36621891043587,6.68186873367684));
#59109=CARTESIAN_POINT('Ctrl Pts',(0.18115621237406,2.36654027420806,6.68190411696132));
#59110=CARTESIAN_POINT('Ctrl Pts',(0.180875115170277,2.3667311076183,6.68192514689624));
#59111=CARTESIAN_POINT('Ctrl Pts',(0.179826078021078,2.36744086504932,6.6820034337586));
#59112=CARTESIAN_POINT('Ctrl Pts',(0.179056192895018,2.36795692652046,6.68206049834049));
#59113=CARTESIAN_POINT('Ctrl Pts',(0.177146055461729,2.36922540165571,6.68220114596431));
#59114=CARTESIAN_POINT('Ctrl Pts',(0.176003213337471,2.3699739078248,6.68228447858582));
#59115=CARTESIAN_POINT('Ctrl Pts',(0.17153821047989,2.37285786496532,6.68260702888197));
#59116=CARTESIAN_POINT('Ctrl Pts',(0.168181526489185,2.37493953762409,6.68284304666794));
#59117=CARTESIAN_POINT('Ctrl Pts',(0.160226638593374,2.37967259856458,6.68338945740611));
#59118=CARTESIAN_POINT('Ctrl Pts',(0.15559945994752,2.38227318607562,6.68369745468987));
#59119=CARTESIAN_POINT('Ctrl Pts',(0.139412597132232,2.39085154053913,6.68474861856945));
#59120=CARTESIAN_POINT('Ctrl Pts',(0.127556222363953,2.39624303039463,6.68547379218808));
#59121=CARTESIAN_POINT('Ctrl Pts',(0.111614060275958,2.40235735455902,6.6864282262624));
#59122=CARTESIAN_POINT('Ctrl Pts',(0.107795127994884,2.40373982015107,6.68665532603328));
#59123=CARTESIAN_POINT('Ctrl Pts',(0.0916133909093569,2.4092540342703,6.6876142318097));
#59124=CARTESIAN_POINT('Ctrl Pts',(0.0790327281646841,2.41270570911318,
6.68835215218976));
#59125=CARTESIAN_POINT('Ctrl Pts',(0.0570537308224934,2.41732459719919,
6.6896610448679));
#59126=CARTESIAN_POINT('Ctrl Pts',(0.0477492413629225,2.41885735344982,
6.6902208958949));
#59127=CARTESIAN_POINT('Ctrl Pts',(0.0372546255473993,2.42011650970681,
6.69086367596115));
#59128=CARTESIAN_POINT('Ctrl Pts',(0.0361169583365184,2.42024686131027,
6.69093350163627));
#59129=CARTESIAN_POINT('Ctrl Pts',(0.0344620323983008,2.42042754876007,
6.69103529352009));
#59130=CARTESIAN_POINT('Ctrl Pts',(0.0339452995903808,2.42048270204822,
6.69106710791667));
#59131=CARTESIAN_POINT('Ctrl Pts',(0.0330336200962892,2.42057778017967,
6.69112329398979));
#59132=CARTESIAN_POINT('Ctrl Pts',(0.0326387278411285,2.42061822568947,
6.6911476492208));
#59133=CARTESIAN_POINT('Ctrl Pts',(0.0318226280977629,2.42070028860927,
6.69119802099171));
#59134=CARTESIAN_POINT('Ctrl Pts',(0.0314014115239478,2.42074180601334,
6.69122404062985));
#59135=CARTESIAN_POINT('Ctrl Pts',(0.0303237923561696,2.42084587892096,
6.69129066243472));
#59136=CARTESIAN_POINT('Ctrl Pts',(0.0296672796847925,2.42090724969874,
6.69133130179642));
#59137=CARTESIAN_POINT('Ctrl Pts',(0.0269937487641927,2.42114889696245,
6.69149701209792));
#59138=CARTESIAN_POINT('Ctrl Pts',(0.0249752750714482,2.42131217192448,
6.69162261622494));
#59139=CARTESIAN_POINT('Ctrl Pts',(-0.00838774946760224,2.4236946494542,
6.693707222624));
#59140=CARTESIAN_POINT('Ctrl Pts',(-0.0398832638499902,2.42133618663887,
6.69582444754338));
#59141=CARTESIAN_POINT('Ctrl Pts',(-0.0783202357909937,2.41271530721903,
6.69848659044372));
#59142=CARTESIAN_POINT('Ctrl Pts',(-0.0860435463694925,2.41067899904203,
6.69902414060131));
#59143=CARTESIAN_POINT('Ctrl Pts',(-0.103123955083956,2.40548972772596,
6.70020932019838));
#59144=CARTESIAN_POINT('Ctrl Pts',(-0.112428837767536,2.40218922000245,
6.7008524737216));
#59145=CARTESIAN_POINT('Ctrl Pts',(-0.122244345139656,2.39819126108725,
6.70151769108359));
#59146=CARTESIAN_POINT('Ctrl Pts',(-0.122919221312364,2.397913700866,6.70156335962871));
#59147=CARTESIAN_POINT('Ctrl Pts',(-0.123857547549199,2.39752405868474,
6.70162675330342));
#59148=CARTESIAN_POINT('Ctrl Pts',(-0.124121793275338,2.39741391698577,
6.70164459450796));
#59149=CARTESIAN_POINT('Ctrl Pts',(-0.124577001556301,2.39722346681187,
6.70167530902859));
#59150=CARTESIAN_POINT('Ctrl Pts',(-0.124768033479432,2.39714332629667,
6.70168819255405));
#59151=CARTESIAN_POINT('Ctrl Pts',(-0.125163981208132,2.39697677163485,
6.70171488314916));
#59152=CARTESIAN_POINT('Ctrl Pts',(-0.125368884519984,2.39689032971282,
6.70172868840381));
#59153=CARTESIAN_POINT('Ctrl Pts',(-0.125776123986787,2.39671803209559,
6.70175611200294));
#59154=CARTESIAN_POINT('Ctrl Pts',(-0.12597846236604,2.3966321812555,6.70176973066547));
#59155=CARTESIAN_POINT('Ctrl Pts',(-0.126450733484886,2.39643122935603,
6.70180150187544));
#59156=CARTESIAN_POINT('Ctrl Pts',(-0.126720597705499,2.39631596625084,
6.70181964456846));
#59157=CARTESIAN_POINT('Ctrl Pts',(-0.128260115953721,2.39565592684532,
6.70192307862415));
#59158=CARTESIAN_POINT('Ctrl Pts',(-0.129526439399022,2.39510334813591,
6.70200790072098));
#59159=CARTESIAN_POINT('Ctrl Pts',(-0.132881910086661,2.39361337938705,
6.70223207588046));
#59160=CARTESIAN_POINT('Ctrl Pts',(-0.134964726741288,2.39266182152779,
6.70237062099168));
#59161=CARTESIAN_POINT('Ctrl Pts',(-0.144659581858135,2.38810710504971,
6.70301346580374));
#59162=CARTESIAN_POINT('Ctrl Pts',(-0.152139225106059,2.38422839071104,
6.7035035330709));
#59163=CARTESIAN_POINT('Ctrl Pts',(-0.166729677598269,2.37592098985497,
6.70446422972996));
#59164=CARTESIAN_POINT('Ctrl Pts',(-0.173836777819929,2.37149947106736,
6.70493461024682));
#59165=CARTESIAN_POINT('Ctrl Pts',(-0.199887121818747,2.35385009469461,
6.70669647172027));
#59166=CARTESIAN_POINT('Ctrl Pts',(-0.217560234037594,2.33887690996202,
6.70797574497701));
#59167=CARTESIAN_POINT('Ctrl Pts',(-0.238669612388335,2.31669023517607,
6.70977562260539));
#59168=CARTESIAN_POINT('Ctrl Pts',(-0.243665423848541,2.31105683894828,
6.71022516727129));
#59169=CARTESIAN_POINT('Ctrl Pts',(-0.249076957457928,2.3045061999595,6.71074213040877));
#59170=CARTESIAN_POINT('Ctrl Pts',(-0.249691367760026,2.30375558248127,
6.71080128374122));
#59171=CARTESIAN_POINT('Ctrl Pts',(-0.250616094032689,2.30261539202133,
6.71089101637054));
#59172=CARTESIAN_POINT('Ctrl Pts',(-0.250928914858841,2.30222785009866,
6.71092149470974));
#59173=CARTESIAN_POINT('Ctrl Pts',(-0.251471380539031,2.3015526132297,6.71097456301667));
#59174=CARTESIAN_POINT('Ctrl Pts',(-0.251701433758816,2.30126524630909,
6.71099713654655));
#59175=CARTESIAN_POINT('Ctrl Pts',(-0.252180237198817,2.3006650525851,6.71104426046144));
#59176=CARTESIAN_POINT('Ctrl Pts',(-0.252428898729361,2.30035215608191,
6.7110688143414));
#59177=CARTESIAN_POINT('Ctrl Pts',(-0.253015152701141,2.29961163533312,
6.71112689482671));
#59178=CARTESIAN_POINT('Ctrl Pts',(-0.253352243281556,2.29918361698476,
6.71116044135962));
#59179=CARTESIAN_POINT('Ctrl Pts',(-0.254460152590617,2.29776949444762,
6.7112711985098));
#59180=CARTESIAN_POINT('Ctrl Pts',(-0.255226304829458,2.29677976380397,
6.71134859394398));
#59181=CARTESIAN_POINT('Ctrl Pts',(-0.259652769490427,2.29099222946145,
6.71180049157234));
#59182=CARTESIAN_POINT('Ctrl Pts',(-0.26318330106082,2.28609711046256,6.71218004372892));
#59183=CARTESIAN_POINT('Ctrl Pts',(-0.275331984213955,2.2682151819066,6.7135584033772));
#59184=CARTESIAN_POINT('Ctrl Pts',(-0.283142080295269,2.25470777824621,
6.7145860116383));
#59185=CARTESIAN_POINT('Ctrl Pts',(-0.292412910025094,2.23560181715299,
6.7160119995205));
#59186=CARTESIAN_POINT('Ctrl Pts',(-0.294747514937318,2.230449465473,6.71639380496975));
#59187=CARTESIAN_POINT('Ctrl Pts',(-0.298048129211772,2.2226235787422,6.71696824444314));
#59188=CARTESIAN_POINT('Ctrl Pts',(-0.299116375467834,2.21999426351854,
6.71716032889619));
#59189=CARTESIAN_POINT('Ctrl Pts',(-0.301325466768272,2.21434405896533,
6.71757084737076));
#59190=CARTESIAN_POINT('Ctrl Pts',(-0.302455927953545,2.2113194169866,6.71778924527279));
#59191=CARTESIAN_POINT('Ctrl Pts',(-0.304326815530602,2.20607468465119,
6.71816519606519));
#59192=CARTESIAN_POINT('Ctrl Pts',(-0.305088865559112,2.20386257106296,
6.71832293016905));
#59193=CARTESIAN_POINT('Ctrl Pts',(-0.310348052728714,2.18803845453742,
6.71944461680408));
#59194=CARTESIAN_POINT('Ctrl Pts',(-0.313957232983756,2.17414612796845,
6.72039514285422));
#59195=CARTESIAN_POINT('Ctrl Pts',(-0.316797686513221,2.1591710768528,6.72135363078277));
#59196=CARTESIAN_POINT('Ctrl Pts',(-0.316962188056315,2.15828346167526,
6.72141019770417));
#59197=CARTESIAN_POINT('Ctrl Pts',(-0.317178704001938,2.1570871555029,6.72148609610303));
#59198=CARTESIAN_POINT('Ctrl Pts',(-0.317233999390033,2.15677907386341,
6.7215056115936));
#59199=CARTESIAN_POINT('Ctrl Pts',(-0.317326424413128,2.1562597723572,6.72153845501799));
#59200=CARTESIAN_POINT('Ctrl Pts',(-0.317363792057402,2.15604859595089,
6.7215517965172));
#59201=CARTESIAN_POINT('Ctrl Pts',(-0.317435122519377,2.15564312643118,
6.72157738496654));
#59202=CARTESIAN_POINT('Ctrl Pts',(-0.317469117512383,2.15544884087231,
6.72158963365203));
#59203=CARTESIAN_POINT('Ctrl Pts',(-0.317538950072604,2.1550475697773,6.72161490635898));
#59204=CARTESIAN_POINT('Ctrl Pts',(-0.317574763509821,2.1548405810863,6.72162792894951));
#59205=CARTESIAN_POINT('Ctrl Pts',(-0.317655207364524,2.15437292339899,
6.72165732032001));
#59206=CARTESIAN_POINT('Ctrl Pts',(-0.317699719421908,2.1541122337848,6.72167368234888));
#59207=CARTESIAN_POINT('Ctrl Pts',(-0.317811374478801,2.1534534272156,6.72171497754669));
#59208=CARTESIAN_POINT('Ctrl Pts',(-0.31787809057946,2.15305523690371,6.72173988666838));
#59209=CARTESIAN_POINT('Ctrl Pts',(-0.318065972638084,2.15192079940594,
6.72181071217877));
#59210=CARTESIAN_POINT('Ctrl Pts',(-0.31818533119747,2.15118424950437,6.72185652863981));
#59211=CARTESIAN_POINT('Ctrl Pts',(-0.320931852769821,2.13385479954498,
6.72293068408991));
#59212=CARTESIAN_POINT('Ctrl Pts',(-0.322260476271441,2.11707992411669,
6.72388901335813));
#59213=CARTESIAN_POINT('Ctrl Pts',(-0.322274881577486,2.10027627742869,
6.72483370602588));
#59214=CARTESIAN_POINT('',(-0.322274855983169,2.09970202152027,6.97470119816725));
#59215=CARTESIAN_POINT('Ctrl Pts',(-0.322274881319243,2.10027657850254,
6.72483368909966));
#59216=CARTESIAN_POINT('Ctrl Pts',(-0.322292341980155,2.07993106223288,
6.7259775041476));
#59217=CARTESIAN_POINT('Ctrl Pts',(-0.320383196143773,2.05962956821057,
6.72709872414235));
#59218=CARTESIAN_POINT('Ctrl Pts',(-0.314408027524657,2.02828985983309,
6.72893409671193));
#59219=CARTESIAN_POINT('Ctrl Pts',(-0.311634562382442,2.01706263284682,
6.72961273384056));
#59220=CARTESIAN_POINT('Ctrl Pts',(-0.307665440760797,2.00404495838612,
6.73043554183747));
#59221=CARTESIAN_POINT('Ctrl Pts',(-0.307047721710094,2.00208631485001,
6.73056030725184));
#59222=CARTESIAN_POINT('Ctrl Pts',(-0.306205916898104,1.99950347510119,
6.73072615883518));
#59223=CARTESIAN_POINT('Ctrl Pts',(-0.305998555478583,1.99887384564408,
6.73076669379932));
#59224=CARTESIAN_POINT('Ctrl Pts',(-0.305655368292431,1.9978425173206,6.73083326315196));
#59225=CARTESIAN_POINT('Ctrl Pts',(-0.305520688992642,1.99744043668135,
6.73085925964289));
#59226=CARTESIAN_POINT('Ctrl Pts',(-0.305258496270871,1.99666276854238,
6.73090962407456));
#59227=CARTESIAN_POINT('Ctrl Pts',(-0.305131082178761,1.99628714815867,
6.7309339886917));
#59228=CARTESIAN_POINT('Ctrl Pts',(-0.304835751619087,1.99542176025312,
6.73099021056599));
#59229=CARTESIAN_POINT('Ctrl Pts',(-0.304667348007322,1.99493216121512,
6.73102208391396));
#59230=CARTESIAN_POINT('Ctrl Pts',(-0.304213610614897,1.99362327609867,
6.73110746989048));
#59231=CARTESIAN_POINT('Ctrl Pts',(-0.303926148677729,1.99280473705577,
6.73116105304204));
#59232=CARTESIAN_POINT('Ctrl Pts',(-0.301896082869726,1.98709799843725,
6.73153593476974));
#59233=CARTESIAN_POINT('Ctrl Pts',(-0.300039021659239,1.98225159352048,
6.7318610300894));
#59234=CARTESIAN_POINT('Ctrl Pts',(-0.297424160138748,1.97589161079522,
6.73229698323918));
#59235=CARTESIAN_POINT('Ctrl Pts',(-0.296770233209781,1.97433595655503,
6.73240436742688));
#59236=CARTESIAN_POINT('Ctrl Pts',(-0.295892459109921,1.97229285139125,
6.73254639524188));
#59237=CARTESIAN_POINT('Ctrl Pts',(-0.295679561348259,1.97180070140844,
6.73258068391327));
#59238=CARTESIAN_POINT('Ctrl Pts',(-0.285421723617948,1.94824941523974,
6.73422520285443));
#59239=CARTESIAN_POINT('Ctrl Pts',(-0.272714391273855,1.92644812541136,
6.73592668510302));
#59240=CARTESIAN_POINT('Ctrl Pts',(-0.253385692743078,1.90073587753876,
6.73810112892537));
#59241=CARTESIAN_POINT('Ctrl Pts',(-0.248983097329683,1.89526133038115,
6.73857446766915));
#59242=CARTESIAN_POINT('Ctrl Pts',(-0.237351756600428,1.88172858428139,
6.73976429583988));
#59243=CARTESIAN_POINT('Ctrl Pts',(-0.229888776992585,1.87388172872463,
6.74047327355406));
#59244=CARTESIAN_POINT('Ctrl Pts',(-0.221344368608981,1.86575914393208,
6.74121502202174));
#59245=CARTESIAN_POINT('Ctrl Pts',(-0.22064147300544,1.86509693783851,6.74127555320187));
#59246=CARTESIAN_POINT('Ctrl Pts',(-0.219742810914166,1.86425789038692,
6.74135231217217));
#59247=CARTESIAN_POINT('Ctrl Pts',(-0.219549799208646,1.86407812551204,
6.7413687613954));
#59248=CARTESIAN_POINT('Ctrl Pts',(-0.219202822383161,1.86375575705495,
6.74139826573993));
#59249=CARTESIAN_POINT('Ctrl Pts',(-0.219048938544433,1.86361306679814,
6.74141132750304));
#59250=CARTESIAN_POINT('Ctrl Pts',(-0.218750220566145,1.86333661986971,
6.74143663738265));
#59251=CARTESIAN_POINT('Ctrl Pts',(-0.218605403207598,1.86320284591739,
6.74144888681532));
#59252=CARTESIAN_POINT('Ctrl Pts',(-0.218302518173839,1.86292357279012,
6.74147446317797));
#59253=CARTESIAN_POINT('Ctrl Pts',(-0.218144428248557,1.86277809923107,
6.74148778814097));
#59254=CARTESIAN_POINT('Ctrl Pts',(-0.217754655672758,1.86242015157136,
6.74152058094793));
#59255=CARTESIAN_POINT('Ctrl Pts',(-0.217522806788386,1.86220785762477,
6.74154003498747));
#59256=CARTESIAN_POINT('Ctrl Pts',(-0.216617077183814,1.86138095349516,
6.7416158317742));
#59257=CARTESIAN_POINT('Ctrl Pts',(-0.215940890815322,1.86076885820684,
6.74167198502214));
#59258=CARTESIAN_POINT('Ctrl Pts',(-0.204038278570644,1.85008599691239,
6.7426530360272));
#59259=CARTESIAN_POINT('Ctrl Pts',(-0.192119436851868,1.84081110647185,
6.74352098036951));
#59260=CARTESIAN_POINT('Ctrl Pts',(-0.17009659507384,1.82603078979801,6.74501901412576));
#59261=CARTESIAN_POINT('Ctrl Pts',(-0.160267412040684,1.82016729002085,
6.74565476331232));
#59262=CARTESIAN_POINT('Ctrl Pts',(-0.138480307197349,1.80869563526606,
6.74703380160354));
#59263=CARTESIAN_POINT('Ctrl Pts',(-0.126448068382314,1.80327474235609,
6.74777758986689));
#59264=CARTESIAN_POINT('Ctrl Pts',(-0.106073331073699,1.79556014540796,
6.74904200571659));
#59265=CARTESIAN_POINT('Ctrl Pts',(-0.0979101866706216,1.79283757927498,
6.74954967417675));
#59266=CARTESIAN_POINT('Ctrl Pts',(-0.0871822558279221,1.78973072679797,
6.75022293167715));
#59267=CARTESIAN_POINT('Ctrl Pts',(-0.0847077139084813,1.78904603195827,
6.75037862882173));
#59268=CARTESIAN_POINT('Ctrl Pts',(-0.0815295559684236,1.78820740081492,
6.75057919512504));
#59269=CARTESIAN_POINT('Ctrl Pts',(-0.080833194380414,1.78802614199899,
6.75062317740628));
#59270=CARTESIAN_POINT('Ctrl Pts',(-0.0797132685617597,1.78773863330169,
6.75069397270331));
#59271=CARTESIAN_POINT('Ctrl Pts',(-0.0792900825184149,1.78763090881404,
6.75072073798875));
#59272=CARTESIAN_POINT('Ctrl Pts',(-0.0784856693940366,1.78742788073499,
6.75077164166492));
#59273=CARTESIAN_POINT('Ctrl Pts',(-0.0781044840931819,1.78733241356928,
6.75079577472103));
#59274=CARTESIAN_POINT('Ctrl Pts',(-0.0772377915514198,1.78711703581432,
6.75085067196637));
#59275=CARTESIAN_POINT('Ctrl Pts',(-0.0767521787467464,1.78699755787775,
6.75088145005175));
#59276=CARTESIAN_POINT('Ctrl Pts',(-0.0753123219047789,1.78664685442312,
6.75097276493727));
#59277=CARTESIAN_POINT('Ctrl Pts',(-0.0743573035177538,1.78641886049538,
6.75103340566745));
#59278=CARTESIAN_POINT('Ctrl Pts',(-0.0678261979626444,1.78489118636413,
6.75144863373122));
#59279=CARTESIAN_POINT('Ctrl Pts',(-0.0622176806293128,1.78373601060769,
6.75180783457533));
#59280=CARTESIAN_POINT('Ctrl Pts',(-0.0562352626013929,1.78266910855679,
6.75219409180155));
#59281=CARTESIAN_POINT('Ctrl Pts',(-0.0558887772316407,1.78260790179655,
6.75221647367286));
#59282=CARTESIAN_POINT('Ctrl Pts',(-0.0324493027619221,1.77850688242696,
6.75373132976085));
#59283=CARTESIAN_POINT('Ctrl Pts',(-0.00898823194892534,1.77699901746954,
6.75530395830445));
#59284=CARTESIAN_POINT('Ctrl Pts',(0.0280152198955742,1.77865687080403,
6.75781059379957));
#59285=CARTESIAN_POINT('Ctrl Pts',(0.0415546743414955,1.78012579328335,
6.75873148107395));
#59286=CARTESIAN_POINT('Ctrl Pts',(0.0602374623161578,1.78335936000663,
6.75997838322112));
#59287=CARTESIAN_POINT('Ctrl Pts',(0.065490330798409,1.78440394396361,6.76032620013949));
#59288=CARTESIAN_POINT('Ctrl Pts',(0.0723782998198994,1.78595308678523,
6.76077655527912));
#59289=CARTESIAN_POINT('Ctrl Pts',(0.0740386049570744,1.78634036400982,
6.76088466699732));
#59290=CARTESIAN_POINT('Ctrl Pts',(0.0767649041583947,1.78699914562723,
6.76106137266218));
#59291=CARTESIAN_POINT('Ctrl Pts',(0.077832697882508,1.78726295938607,6.76113037436944));
#59292=CARTESIAN_POINT('Ctrl Pts',(0.0792524377324671,1.78762144837189,
6.76122182316244));
#59293=CARTESIAN_POINT('Ctrl Pts',(0.0796055877380693,1.78771125731494,
6.76124454595599));
#59294=CARTESIAN_POINT('Ctrl Pts',(0.0801570843221477,1.78785250370413,
6.76127999198451));
#59295=CARTESIAN_POINT('Ctrl Pts',(0.0803555340441774,1.78790353132429,
6.76129273893185));
#59296=CARTESIAN_POINT('Ctrl Pts',(0.0807660394355996,1.78800950257269,
6.76131909022812));
#59297=CARTESIAN_POINT('Ctrl Pts',(0.0809780861113127,1.78806447271735,
6.76133269281748));
#59298=CARTESIAN_POINT('Ctrl Pts',(0.0814613381350981,1.78819027503527,
6.76136367223391));
#59299=CARTESIAN_POINT('Ctrl Pts',(0.0817325067575552,1.78826124473545,
6.76138104093861));
#59300=CARTESIAN_POINT('Ctrl Pts',(0.0825596615257031,1.7884788794588,6.76143397687228));
#59301=CARTESIAN_POINT('Ctrl Pts',(0.083115351874641,1.78862667977282,6.76146947846353));
#59302=CARTESIAN_POINT('Ctrl Pts',(0.0871341297739221,1.7897071032596,6.7617258036703));
#59303=CARTESIAN_POINT('Ctrl Pts',(0.0905820022436709,1.79069603653874,
6.76194343533742));
#59304=CARTESIAN_POINT('Ctrl Pts',(0.103475462442264,1.7946283010598,6.76275116110119));
#59305=CARTESIAN_POINT('Ctrl Pts',(0.112801091684172,1.79794868829559,6.7633230028282));
#59306=CARTESIAN_POINT('Ctrl Pts',(0.141635186479585,1.80973723614822,6.76509399090638));
#59307=CARTESIAN_POINT('Ctrl Pts',(0.160466451628482,1.81970807859022,6.76625821981235));
#59308=CARTESIAN_POINT('Ctrl Pts',(0.186006574408517,1.83665427667127,6.76800308841223));
#59309=CARTESIAN_POINT('Ctrl Pts',(0.193602572730806,1.84218720149462,6.76854532625982));
#59310=CARTESIAN_POINT('Ctrl Pts',(0.20628775483523,1.85230416378483,6.76950261112197));
#59311=CARTESIAN_POINT('Ctrl Pts',(0.211492624015434,1.85673322348962,6.76991175343408));
#59312=CARTESIAN_POINT('Ctrl Pts',(0.21726448581017,1.86197007965197,6.77038634432576));
#59313=CARTESIAN_POINT('Ctrl Pts',(0.217973541898985,1.86261921986852,6.77044501806585));
#59314=CARTESIAN_POINT('Ctrl Pts',(0.219038965016669,1.86360341230984,6.77053374863671));
#59315=CARTESIAN_POINT('Ctrl Pts',(0.219397495396707,1.86393612331279,6.77056370558625));
#59316=CARTESIAN_POINT('Ctrl Pts',(0.220014731474875,1.86451153024235,6.7706154484375));
#59317=CARTESIAN_POINT('Ctrl Pts',(0.220273797189978,1.86475384014901,6.77063721776757));
#59318=CARTESIAN_POINT('Ctrl Pts',(0.220808319819621,1.86525544812339,6.770682241432));
#59319=CARTESIAN_POINT('Ctrl Pts',(0.221083721186264,1.8655148043866,6.77070549825435));
#59320=CARTESIAN_POINT('Ctrl Pts',(0.221748671071617,1.86614322660808,6.77076179543896));
#59321=CARTESIAN_POINT('Ctrl Pts',(0.222137754707119,1.86651278083923,6.77079485687244));
#59322=CARTESIAN_POINT('Ctrl Pts',(0.223575895791958,1.86788558536415,6.77091750722796));
#59323=CARTESIAN_POINT('Ctrl Pts',(0.224619082267808,1.86889493637861,6.77100736093444));
#59324=CARTESIAN_POINT('Ctrl Pts',(0.242252503340233,1.88618859956074,6.77254151569527));
#59325=CARTESIAN_POINT('Ctrl Pts',(0.257036192194062,1.90421038442269,6.77406789104859));
#59326=CARTESIAN_POINT('Ctrl Pts',(0.278439762049603,1.93695210442297,6.77670327256075));
#59327=CARTESIAN_POINT('Ctrl Pts',(0.286134086416015,1.95086713285716,6.77778576052273));
#59328=CARTESIAN_POINT('Ctrl Pts',(0.296045782475372,1.9724091118301,6.77936535156051));
#59329=CARTESIAN_POINT('Ctrl Pts',(0.299059829220571,1.97964312217989,6.77988039487894));
#59330=CARTESIAN_POINT('Ctrl Pts',(0.302583432206568,1.98905254199192,6.78052480271146));
#59331=CARTESIAN_POINT('Ctrl Pts',(0.303338090653373,1.99113276316231,6.78066569849326));
#59332=CARTESIAN_POINT('Ctrl Pts',(0.304367841520667,1.99406514370936,6.78086195440985));
#59333=CARTESIAN_POINT('Ctrl Pts',(0.304660881200354,1.99491087478021,6.78091828314932));
#59334=CARTESIAN_POINT('Ctrl Pts',(0.305161429082977,1.99637517921468,6.78101532523165));
#59335=CARTESIAN_POINT('Ctrl Pts',(0.305370587516357,1.99699317702071,6.78105613195548));
#59336=CARTESIAN_POINT('Ctrl Pts',(0.305673202820218,1.99789633335023,6.78111554596668));
#59337=CARTESIAN_POINT('Ctrl Pts',(0.30576813873378,1.99818098899159,6.78113423988265));
#59338=CARTESIAN_POINT('Ctrl Pts',(0.305932910277509,1.99867734839268,6.78116678035159));
#59339=CARTESIAN_POINT('Ctrl Pts',(0.306002923974494,1.99888899248922,6.78118063749877));
#59340=CARTESIAN_POINT('Ctrl Pts',(0.306137338614457,1.99929673227065,6.78120729915661));
#59341=CARTESIAN_POINT('Ctrl Pts',(0.306201770640241,1.9994928167607,6.78122010552555));
#59342=CARTESIAN_POINT('Ctrl Pts',(0.30635421635015,1.99995825846805,6.78125046755219));
#59343=CARTESIAN_POINT('Ctrl Pts',(0.306442063409475,2.00022767067453,6.78126801330627));
#59344=CARTESIAN_POINT('Ctrl Pts',(0.306749625091868,2.0011751489905,6.78132961900819));
#59345=CARTESIAN_POINT('Ctrl Pts',(0.306967447514603,2.00185383420496,6.78137356801362));
#59346=CARTESIAN_POINT('Ctrl Pts',(0.309853077375612,2.01094838633347,6.78196016409799));
#59347=CARTESIAN_POINT('Ctrl Pts',(0.31217650115249,2.0194705994882,6.78248317402636));
#59348=CARTESIAN_POINT('Ctrl Pts',(0.319665781305849,2.05218308000831,6.78442784987435));
#59349=CARTESIAN_POINT('Ctrl Pts',(0.322392088917836,2.07684418030572,6.78577123025557));
#59350=CARTESIAN_POINT('Ctrl Pts',(0.322188812319144,2.118412714764,6.78813102960269));
#59351=CARTESIAN_POINT('Ctrl Pts',(0.3207872500352,2.13521470559871,6.78910989030885));
#59352=CARTESIAN_POINT('Ctrl Pts',(0.317888527833361,2.15300451201013,6.7902056407977));
#59353=CARTESIAN_POINT('Ctrl Pts',(0.317690453446088,2.15417905638807,6.7902782566166));
#59354=CARTESIAN_POINT('Ctrl Pts',(0.317394174823475,2.15587842569497,6.79038372066029));
#59355=CARTESIAN_POINT('Ctrl Pts',(0.317301168882254,2.15640415667803,6.7904164035814));
#59356=CARTESIAN_POINT('Ctrl Pts',(0.317136586631268,2.15732119405874,6.79047351081591));
#59357=CARTESIAN_POINT('Ctrl Pts',(0.317065591214247,2.15771260463813,6.79049791659506));
#59358=CARTESIAN_POINT('Ctrl Pts',(0.31692702171328,2.15846858997967,6.79054511559125));
#59359=CARTESIAN_POINT('Ctrl Pts',(0.316859542747316,2.15883318174668,6.79056790574401));
#59360=CARTESIAN_POINT('Ctrl Pts',(0.316698035873523,2.15969747264203,6.79062199661888));
#59361=CARTESIAN_POINT('Ctrl Pts',(0.316603454475463,2.16019706616992,6.79065331494687));
#59362=CARTESIAN_POINT('Ctrl Pts',(0.316266717042569,2.16195301763072,6.79076357463993));
#59363=CARTESIAN_POINT('Ctrl Pts',(0.316018264212374,2.16320814275396,6.79084271670036));
#59364=CARTESIAN_POINT('Ctrl Pts',(0.312238252707394,2.18172432446622,6.79201522237486));
#59365=CARTESIAN_POINT('Ctrl Pts',(0.307305162130927,2.19866581049313,6.79315439192311));
#59366=CARTESIAN_POINT('Ctrl Pts',(0.293527889532114,2.23469126497403,6.79572051521411));
#59367=CARTESIAN_POINT('Ctrl Pts',(0.284151298061953,2.25348721669295,6.79715601492943));
#59368=CARTESIAN_POINT('Ctrl Pts',(0.269753047903673,2.27644319869376,6.79896557159278));
#59369=CARTESIAN_POINT('Ctrl Pts',(0.266340814353595,2.28155298971093,6.7993719763893));
#59370=CARTESIAN_POINT('Ctrl Pts',(0.259797692651815,2.29076937367466,6.80010769002199));
#59371=CARTESIAN_POINT('Ctrl Pts',(0.256710150033287,2.29490433867707,6.80043881622971));
#59372=CARTESIAN_POINT('Ctrl Pts',(0.252923175368309,2.29972979619699,6.80082478543587));
#59373=CARTESIAN_POINT('Ctrl Pts',(0.25231843076531,2.30049322602366,6.80088583511165));
#59374=CARTESIAN_POINT('Ctrl Pts',(0.251493508429981,2.30152496440155,6.80096830803059));
#59375=CARTESIAN_POINT('Ctrl Pts',(0.251276352473662,2.30179566583477,6.80098994371064));
#59376=CARTESIAN_POINT('Ctrl Pts',(0.250930674640275,2.3022251563981,6.80102426491124));
#59377=CARTESIAN_POINT('Ctrl Pts',(0.250802439104796,2.30238417402382,6.80103697100736));
#59378=CARTESIAN_POINT('Ctrl Pts',(0.250535444734357,2.30271461515251,6.80106337172469));
#59379=CARTESIAN_POINT('Ctrl Pts',(0.250396661510784,2.3028860176778,6.80107706441354));
#59380=CARTESIAN_POINT('Ctrl Pts',(0.250077028247968,2.30327994931401,6.80110853073044));
#59381=CARTESIAN_POINT('Ctrl Pts',(0.249896056552528,2.30350238025995,6.80112629552463));
#59382=CARTESIAN_POINT('Ctrl Pts',(0.24941228093658,2.30409536678504,6.80117364965696));
#59383=CARTESIAN_POINT('Ctrl Pts',(0.249108946684217,2.30446549174358,6.80120320081684));
#59384=CARTESIAN_POINT('Ctrl Pts',(0.247030885342589,2.30698962948522,6.80140470089151));
#59385=CARTESIAN_POINT('Ctrl Pts',(0.245228996862376,2.30912126956893,6.80157472009918));
#59386=CARTESIAN_POINT('Ctrl Pts',(0.221389415797427,2.33659162209649,6.80376787697726));
#59387=CARTESIAN_POINT('Ctrl Pts',(0.195547219496606,2.35836209614145,6.80554796599594));
#59388=CARTESIAN_POINT('Ctrl Pts',(0.154406560414664,2.38324850156204,6.80829840060562));
#59389=CARTESIAN_POINT('Ctrl Pts',(0.141519497075983,2.38990213221643,6.8091471784033));
#59390=CARTESIAN_POINT('Ctrl Pts',(0.127219863668643,2.39610385604822,6.81009533823911));
#59391=CARTESIAN_POINT('Ctrl Pts',(0.126207770222817,2.39653665197878,6.81016247331863));
#59392=CARTESIAN_POINT('Ctrl Pts',(0.12471716954825,2.39716505590014,6.81026139525233));
#59393=CARTESIAN_POINT('Ctrl Pts',(0.124240369743966,2.39736471436474,6.81029304439665));
#59394=CARTESIAN_POINT('Ctrl Pts',(0.123398239717564,2.39771497477697,6.81034895649544));
#59395=CARTESIAN_POINT('Ctrl Pts',(0.123033108108095,2.39786605392165,6.81037320321135));
#59396=CARTESIAN_POINT('Ctrl Pts',(0.12232021182031,2.39815949190292,6.8104205521335));
#59397=CARTESIAN_POINT('Ctrl Pts',(0.12197247404919,2.39830191485144,6.81044365212389));
#59398=CARTESIAN_POINT('Ctrl Pts',(0.121136179867646,2.3986427290243,6.8104992167175));
#59399=CARTESIAN_POINT('Ctrl Pts',(0.120647385285245,2.39884052953133,6.81053170122564));
#59400=CARTESIAN_POINT('Ctrl Pts',(0.119150204066588,2.39944212193575,6.81063122815866));
#59401=CARTESIAN_POINT('Ctrl Pts',(0.11814026731536,2.39984201291814,6.81069840188693));
#59402=CARTESIAN_POINT('Ctrl Pts',(0.106259712374632,2.40447685354085,6.81148908428356));
#59403=CARTESIAN_POINT('Ctrl Pts',(0.0951701630401514,2.40812313236201,
6.8122322551355));
#59404=CARTESIAN_POINT('Ctrl Pts',(0.062759138451729,2.41686319684023,6.81442167471014));
#59405=CARTESIAN_POINT('Ctrl Pts',(0.041085348085757,2.42039472754361,6.81591081071072));
#59406=CARTESIAN_POINT('Ctrl Pts',(0.00242777394123436,2.4227048382318,
6.81852494522203));
#59407=CARTESIAN_POINT('Ctrl Pts',(-0.014424059179768,2.4223917037847,6.81964869117217));
#59408=CARTESIAN_POINT('Ctrl Pts',(-0.031878476210447,2.42069523865256,
6.82074888976668));
#59409=CARTESIAN_POINT('Ctrl Pts',(-0.0325804383976772,2.42062468463301,
6.82079302614161));
#59410=CARTESIAN_POINT('Ctrl Pts',(-0.0335853418388151,2.42052034778143,
6.82085604684138));
#59411=CARTESIAN_POINT('Ctrl Pts',(-0.0338884693153122,2.42048844000629,
6.82087503563732));
#59412=CARTESIAN_POINT('Ctrl Pts',(-0.0344129678737063,2.42043247783264,
6.8209078543737));
#59413=CARTESIAN_POINT('Ctrl Pts',(-0.0346343597642312,2.42040862399872,
6.82092169568889));
#59414=CARTESIAN_POINT('Ctrl Pts',(-0.0350612630779742,2.42036217972936,
6.82094836302101));
#59415=CARTESIAN_POINT('Ctrl Pts',(-0.0352667770187361,2.42033962104131,
6.82096119082727));
#59416=CARTESIAN_POINT('Ctrl Pts',(-0.0357552482891056,2.42028552715295,
6.82099165680791));
#59417=CARTESIAN_POINT('Ctrl Pts',(-0.0360381863900791,2.42025381466427,
6.82100928491814));
#59418=CARTESIAN_POINT('Ctrl Pts',(-0.036887200113352,2.42015751545781,
6.82106212637427));
#59419=CARTESIAN_POINT('Ctrl Pts',(-0.0374531506814395,2.42009180206938,
6.82109727656668));
#59420=CARTESIAN_POINT('Ctrl Pts',(-0.0429892991701606,2.41943410748912,
6.82144042067905));
#59421=CARTESIAN_POINT('Ctrl Pts',(-0.0479455764284708,2.41872787347188,
6.82174213051543));
#59422=CARTESIAN_POINT('Ctrl Pts',(-0.0662573599042714,2.41568170930456,
6.82284309040585));
#59423=CARTESIAN_POINT('Ctrl Pts',(-0.07947865079888,2.41261508945703,6.82361101719858));
#59424=CARTESIAN_POINT('Ctrl Pts',(-0.108737676633516,2.40385148298188,
6.8253246971275));
#59425=CARTESIAN_POINT('Ctrl Pts',(-0.12459569211984,2.39770035930134,6.82626459498531));
#59426=CARTESIAN_POINT('Ctrl Pts',(-0.153305656229379,2.38386643671697,
6.82808393367285));
#59427=CARTESIAN_POINT('Ctrl Pts',(-0.166250747039522,2.37648395363061,
6.82895410287386));
#59428=CARTESIAN_POINT('Ctrl Pts',(-0.179677563983831,2.36754197372882,
6.82993440911893));
#59429=CARTESIAN_POINT('Ctrl Pts',(-0.180712775149128,2.36684382611399,
6.83001050998267));
#59430=CARTESIAN_POINT('Ctrl Pts',(-0.182193374894341,2.36583274068711,
6.83012011071171));
#59431=CARTESIAN_POINT('Ctrl Pts',(-0.182642077491884,2.36552465685943,
6.83015342645639));
#59432=CARTESIAN_POINT('Ctrl Pts',(-0.183418827037244,2.36498843215475,
6.83021127530816));
#59433=CARTESIAN_POINT('Ctrl Pts',(-0.183747235113236,2.3647608144599,6.83023578845402));
#59434=CARTESIAN_POINT('Ctrl Pts',(-0.18437747314091,2.36432226281163,6.83028293666907));
#59435=CARTESIAN_POINT('Ctrl Pts',(-0.184679366747797,2.36411142102449,
6.8303055681922));
#59436=CARTESIAN_POINT('Ctrl Pts',(-0.185389122664073,2.36361391721632,
6.83035888588452));
#59437=CARTESIAN_POINT('Ctrl Pts',(-0.185796681613986,2.36332682591992,
6.83038958847558));
#59438=CARTESIAN_POINT('Ctrl Pts',(-0.186996818953137,2.36247725594961,
6.83048025427954));
#59439=CARTESIAN_POINT('Ctrl Pts',(-0.187787515677048,2.36191214006249,
6.83054031883728));
#59440=CARTESIAN_POINT('Ctrl Pts',(-0.194721389368632,2.35690891693216,
6.83106998258677));
#59441=CARTESIAN_POINT('Ctrl Pts',(-0.200708342372131,2.35225930449738,
6.8315477745733));
#59442=CARTESIAN_POINT('Ctrl Pts',(-0.210527541120479,2.34406250737537,
6.83236783588203));
#59443=CARTESIAN_POINT('Ctrl Pts',(-0.21444776180887,2.34062523939864,6.83270573019566));
#59444=CARTESIAN_POINT('Ctrl Pts',(-0.237697555721537,2.3192201564564,6.8347740198608));
#59445=CARTESIAN_POINT('Ctrl Pts',(-0.254842425256783,2.29902927550685,
6.83658859195294));
#59446=CARTESIAN_POINT('Ctrl Pts',(-0.273875175313273,2.27006474872148,
6.83890116622805));
#59447=CARTESIAN_POINT('Ctrl Pts',(-0.278151177437159,2.26297722292027,
6.83944610281646));
#59448=CARTESIAN_POINT('Ctrl Pts',(-0.283802239828319,2.25273884881567,
6.84019655784098));
#59449=CARTESIAN_POINT('Ctrl Pts',(-0.285406881337291,2.24971900907254,
6.84041355413997));
#59450=CARTESIAN_POINT('Ctrl Pts',(-0.287201255395476,2.24620837199312,
6.84066034763926));
#59451=CARTESIAN_POINT('Ctrl Pts',(-0.287438146261026,2.24574210518857,
6.84069301554226));
#59452=CARTESIAN_POINT('Ctrl Pts',(-0.287795471898968,2.24503452937019,
6.84074242118496));
#59453=CARTESIAN_POINT('Ctrl Pts',(-0.28791673908383,2.2447936452742,6.8407592110165));
#59454=CARTESIAN_POINT('Ctrl Pts',(-0.288135542048399,2.24435765519145,
6.84078954598172));
#59455=CARTESIAN_POINT('Ctrl Pts',(-0.2882331818201,2.2441626029962,6.84080309764972));
#59456=CARTESIAN_POINT('Ctrl Pts',(-0.288429017856206,2.24377039262779,
6.84083030806667));
#59457=CARTESIAN_POINT('Ctrl Pts',(-0.288527209592251,2.24357323379884,
6.84084396651655));
#59458=CARTESIAN_POINT('Ctrl Pts',(-0.288806761486751,2.24301047757681,
6.84088289604643));
#59459=CARTESIAN_POINT('Ctrl Pts',(-0.288987630252294,2.24264463446878,
6.84090813623155));
#59460=CARTESIAN_POINT('Ctrl Pts',(-0.28975856074101,2.24107778943558,6.84101595104108));
#59461=CARTESIAN_POINT('Ctrl Pts',(-0.290341845169806,2.23987344024012,
6.84109810783992));
#59462=CARTESIAN_POINT('Ctrl Pts',(-0.301583658052285,2.21628832188976,
6.84269377026068));
#59463=CARTESIAN_POINT('Ctrl Pts',(-0.30963420551681,2.19275112314791,6.84405818746292));
#59464=CARTESIAN_POINT('Ctrl Pts',(-0.317976313350995,2.15441227793425,
6.84625322047779));
#59465=CARTESIAN_POINT('Ctrl Pts',(-0.32009434862226,2.14011479458717,6.84706532725283));
#59466=CARTESIAN_POINT('Ctrl Pts',(-0.321930825274427,2.11718079129356,
6.84840088056807));
#59467=CARTESIAN_POINT('Ctrl Pts',(-0.322273821431241,2.10861398800965,
6.8489067771116));
#59468=CARTESIAN_POINT('Ctrl Pts',(-0.322275339951301,2.0975438245451,6.8495741530653));
#59469=CARTESIAN_POINT('Ctrl Pts',(-0.322246583978123,2.0950435789177,6.84972577132713));
#59470=CARTESIAN_POINT('Ctrl Pts',(-0.322171516039962,2.09179975378732,
6.84992371478668));
#59471=CARTESIAN_POINT('Ctrl Pts',(-0.322151715013854,2.09105560038719,
6.84996920843145));
#59472=CARTESIAN_POINT('Ctrl Pts',(-0.322116040958226,2.08986948364505,
6.85004185791066));
#59473=CARTESIAN_POINT('Ctrl Pts',(-0.322101836077988,2.08942746972945,
6.8500689614242));
#59474=CARTESIAN_POINT('Ctrl Pts',(-0.322074663913055,2.08863290037682,
6.85011773786434));
#59475=CARTESIAN_POINT('Ctrl Pts',(-0.322062027425214,2.08828033372048,
6.85013940038503));
#59476=CARTESIAN_POINT('Ctrl Pts',(-0.322031109308002,2.08745553505984,
6.85019012369995));
#59477=CARTESIAN_POINT('Ctrl Pts',(-0.322012367856535,2.08698332198871,
6.85021919886788));
#59478=CARTESIAN_POINT('Ctrl Pts',(-0.321955643363727,2.08562925018755,
6.85030267353166));
#59479=CARTESIAN_POINT('Ctrl Pts',(-0.321915076134098,2.08474750916423,
6.85035715393022));
#59480=CARTESIAN_POINT('Ctrl Pts',(-0.321626381809608,2.07898811737928,
6.85071383130632));
#59481=CARTESIAN_POINT('Ctrl Pts',(-0.321271037165977,2.07411670145508,
6.85101937526794));
#59482=CARTESIAN_POINT('Ctrl Pts',(-0.319875621343921,2.05955618433568,
6.85194486541953));
#59483=CARTESIAN_POINT('Ctrl Pts',(-0.318506783384072,2.04990495970286,
6.85257477945267));
#59484=CARTESIAN_POINT('Ctrl Pts',(-0.313632911979409,2.02403595594415,
6.85430675114566));
#59485=CARTESIAN_POINT('Ctrl Pts',(-0.309309905902645,2.00800305556802,
6.85542847676373));
#59486=CARTESIAN_POINT('Ctrl Pts',(-0.29740141106219,1.97439103594679,6.85784107566176));
#59487=CARTESIAN_POINT('Ctrl Pts',(-0.289444329073496,1.95700567954791,
6.85912741669602));
#59488=CARTESIAN_POINT('Ctrl Pts',(-0.279866330954978,1.94019987637498,
6.86034676044441));
#59489=CARTESIAN_POINT('Ctrl Pts',(-0.279737808378602,1.93997499796166,
6.86036307149682));
#59490=CARTESIAN_POINT('Ctrl Pts',(-0.279140736230509,1.93893320675976,
6.86043861149927));
#59491=CARTESIAN_POINT('Ctrl Pts',(-0.278668872009114,1.93811818405514,
6.86049764012618));
#59492=CARTESIAN_POINT('Ctrl Pts',(-0.278014773839143,1.93699973497293,
6.86057853770992));
#59493=CARTESIAN_POINT('Ctrl Pts',(-0.277835608558162,1.93669453318488,
6.86060060199568));
#59494=CARTESIAN_POINT('Ctrl Pts',(-0.277549635772109,1.9362092214014,6.86063566886617));
#59495=CARTESIAN_POINT('Ctrl Pts',(-0.277443155497015,1.93602892041693,
6.86064869273221));
#59496=CARTESIAN_POINT('Ctrl Pts',(-0.277235163384659,1.935677514048,6.86067406816989));
#59497=CARTESIAN_POINT('Ctrl Pts',(-0.277133669126158,1.93550639938528,
6.86068642078655));
#59498=CARTESIAN_POINT('Ctrl Pts',(-0.276887669849256,1.93509252981834,
6.86071628877096));
#59499=CARTESIAN_POINT('Ctrl Pts',(-0.276743003584368,1.9348498701035,6.86073379354769));
#59500=CARTESIAN_POINT('Ctrl Pts',(-0.27629720933969,1.93410433611787,6.86078755246351));
#59501=CARTESIAN_POINT('Ctrl Pts',(-0.275995026260432,1.93360208932785,
6.8608237379404));
#59502=CARTESIAN_POINT('Ctrl Pts',(-0.272680379048862,1.92812681305507,
6.86121791432844));
#59503=CARTESIAN_POINT('Ctrl Pts',(-0.269535001026556,1.92323497202769,
6.86156736514408));
#59504=CARTESIAN_POINT('Ctrl Pts',(-0.262668591950594,1.91316586886582,
6.8622867595852));
#59505=CARTESIAN_POINT('Ctrl Pts',(-0.258922885183182,1.90800851508295,
6.86265530016712));
#59506=CARTESIAN_POINT('Ctrl Pts',(-0.237973409018472,1.88089312125577,
6.8646126627787));
#59507=CARTESIAN_POINT('Ctrl Pts',(-0.218127423927669,1.86112826977649,
6.86612226118976));
#59508=CARTESIAN_POINT('Ctrl Pts',(-0.194072972230402,1.84270124329628,
6.86787988325165));
#59509=CARTESIAN_POINT('Ctrl Pts',(-0.192145979192528,1.84125902712357,
6.86802015094564));
#59510=CARTESIAN_POINT('Ctrl Pts',(-0.188736364265365,1.83876627061052,
6.86826757304807));
#59511=CARTESIAN_POINT('Ctrl Pts',(-0.187260663703092,1.83770642360667,
6.86837441148749));
#59512=CARTESIAN_POINT('Ctrl Pts',(-0.180429728434084,1.832887481177,6.86886799676653));
#59513=CARTESIAN_POINT('Ctrl Pts',(-0.174970057487257,1.82927974889284,
6.86925984125394));
#59514=CARTESIAN_POINT('Ctrl Pts',(-0.16852416354373,1.82529679071907,6.86972099830477));
#59515=CARTESIAN_POINT('Ctrl Pts',(-0.167641066644662,1.82475698079259,
6.8697841451864));
#59516=CARTESIAN_POINT('Ctrl Pts',(-0.166324057272614,1.82396062296709,
6.86987827748827));
#59517=CARTESIAN_POINT('Ctrl Pts',(-0.165892112478669,1.82370082028145,
6.8699091437479));
#59518=CARTESIAN_POINT('Ctrl Pts',(-0.165121942260404,1.82324004155807,
6.86996416806702));
#59519=CARTESIAN_POINT('Ctrl Pts',(-0.164783954231261,1.82303866905584,
6.8699883116039));
#59520=CARTESIAN_POINT('Ctrl Pts',(-0.164071916458155,1.82261620333812,
6.8700391670955));
#59521=CARTESIAN_POINT('Ctrl Pts',(-0.163697786888806,1.8223952468246,6.87006588396085));
#59522=CARTESIAN_POINT('Ctrl Pts',(-0.162711274003919,1.82181531167767,
6.87013632067883));
#59523=CARTESIAN_POINT('Ctrl Pts',(-0.162098152025379,1.82145759999231,
6.87018008638548));
#59524=CARTESIAN_POINT('Ctrl Pts',(-0.159344794585676,1.81986338759023,
6.87037658114278));
#59525=CARTESIAN_POINT('Ctrl Pts',(-0.157191603775599,1.81864953469204,
6.87053012503778));
#59526=CARTESIAN_POINT('Ctrl Pts',(-0.14128666908987,1.80992275937943,6.87166369552062));
#59527=CARTESIAN_POINT('Ctrl Pts',(-0.127019277660994,1.80339807582073,
6.87267880649944));
#59528=CARTESIAN_POINT('Ctrl Pts',(-0.085328135570271,1.78789331312937,
6.87563456593586));
#59529=CARTESIAN_POINT('Ctrl Pts',(-0.0570974322106372,1.78151724541543,
6.87763399856384));
#59530=CARTESIAN_POINT('Ctrl Pts',(-0.0277340098856623,1.77891988188452,
6.8795391927951));
#59531=CARTESIAN_POINT('Ctrl Pts',(-0.0270716332813282,1.77886335581295,
6.87958207315246));
#59532=CARTESIAN_POINT('Ctrl Pts',(-0.0226198282752288,1.77849731805119,
6.87986959953397));
#59533=CARTESIAN_POINT('Ctrl Pts',(-0.0188251486561185,1.77825281966406,
6.88011142264051));
#59534=CARTESIAN_POINT('Ctrl Pts',(-0.0144424466234604,1.77804824335031,
6.88038628197067));
#59535=CARTESIAN_POINT('Ctrl Pts',(-0.0138579835002017,1.77802255641059,
6.8804228453553));
#59536=CARTESIAN_POINT('Ctrl Pts',(-0.0129913996345142,1.77798683435746,
6.88047691980647));
#59537=CARTESIAN_POINT('Ctrl Pts',(-0.0127093345773721,1.77797557836764,
6.88049449885556));
#59538=CARTESIAN_POINT('Ctrl Pts',(-0.0122081325580716,1.77795623711976,
6.88052569613782));
#59539=CARTESIAN_POINT('Ctrl Pts',(-0.011989002192633,1.77794800491513,
6.88053932264051));
#59540=CARTESIAN_POINT('Ctrl Pts',(-0.0115250607254074,1.77793104991664,
6.88056814441545));
#59541=CARTESIAN_POINT('Ctrl Pts',(-0.011280248717201,1.77792238261196,
6.88058333649427));
#59542=CARTESIAN_POINT('Ctrl Pts',(-0.0106262935710699,1.77789997656651,
6.88062387474249));
#59543=CARTESIAN_POINT('Ctrl Pts',(-0.0102171320334495,1.77788673819862,
6.88064919275271));
#59544=CARTESIAN_POINT('Ctrl Pts',(-0.00829096335637178,1.77782809105331,
6.8807681696053));
#59545=CARTESIAN_POINT('Ctrl Pts',(-0.00677364064662362,1.77779261803498,
6.88086127890078));
#59546=CARTESIAN_POINT('Ctrl Pts',(0.00552489325638143,1.77759201051274,
6.8816114035902));
#59547=CARTESIAN_POINT('Ctrl Pts',(0.0163091749536936,1.77795730168867,
6.88224082061855));
#59548=CARTESIAN_POINT('Ctrl Pts',(0.0589632798324055,1.78155092872221,
6.88468784954465));
#59549=CARTESIAN_POINT('Ctrl Pts',(0.0902907587631205,1.78897876182508,
6.88640991858218));
#59550=CARTESIAN_POINT('Ctrl Pts',(0.121136138778605,1.80135525637921,6.8883696450711));
#59551=CARTESIAN_POINT('Ctrl Pts',(0.122259334126513,1.80181330986426,6.88844135895844));
#59552=CARTESIAN_POINT('Ctrl Pts',(0.128646470044153,1.80446022009727,6.88885123935213));
#59553=CARTESIAN_POINT('Ctrl Pts',(0.133853921971374,1.80678199723371,6.88919349808833));
#59554=CARTESIAN_POINT('Ctrl Pts',(0.139881487167089,1.80966345967125,6.88960023588085));
#59555=CARTESIAN_POINT('Ctrl Pts',(0.140764205308178,1.81009040103376,6.88966007096946));
#59556=CARTESIAN_POINT('Ctrl Pts',(0.142093904676987,1.81074103696969,6.88975061768401));
#59557=CARTESIAN_POINT('Ctrl Pts',(0.142542341989202,1.810961756552,6.88978122553538));
#59558=CARTESIAN_POINT('Ctrl Pts',(0.143342395495558,1.81135785534634,6.88983596087808));
#59559=CARTESIAN_POINT('Ctrl Pts',(0.14369420857446,1.8115328364672,6.88986007441029));
#59560=CARTESIAN_POINT('Ctrl Pts',(0.144436477512356,1.81190371328301,6.88991104429282));
#59561=CARTESIAN_POINT('Ctrl Pts',(0.14482685654768,1.81209976020187,6.88993790590811));
#59562=CARTESIAN_POINT('Ctrl Pts',(0.145847000538548,1.8126146727144,6.89000824625368));
#59563=CARTESIAN_POINT('Ctrl Pts',(0.14647611605023,1.81293481346686,6.8900517697257));
#59564=CARTESIAN_POINT('Ctrl Pts',(0.149285543638173,1.81437609900589,6.89024678613384));
#59565=CARTESIAN_POINT('Ctrl Pts',(0.151454025335213,1.81552001118883,6.89039908039086));
#59566=CARTESIAN_POINT('Ctrl Pts',(0.167273529946703,1.824097219141,6.89152341526636));
#59567=CARTESIAN_POINT('Ctrl Pts',(0.18038189828198,1.8324836042563,6.89252996350282));
#59568=CARTESIAN_POINT('Ctrl Pts',(0.212522953705439,1.85648594887202,6.89519450315251));
#59569=CARTESIAN_POINT('Ctrl Pts',(0.230465225751054,1.87339290239737,6.89688705799964));
#59570=CARTESIAN_POINT('Ctrl Pts',(0.251873065757921,1.89876503393261,6.89908019706598));
#59571=CARTESIAN_POINT('Ctrl Pts',(0.257168373819225,1.90557774958595,6.8996397013343));
#59572=CARTESIAN_POINT('Ctrl Pts',(0.262596811378652,1.91317229024472,6.90022548506959));
#59573=CARTESIAN_POINT('Ctrl Pts',(0.263007268821166,1.91375055691784,6.90026985767464));
#59574=CARTESIAN_POINT('Ctrl Pts',(0.263578714845979,1.91456128599946,6.90033174106603));
#59575=CARTESIAN_POINT('Ctrl Pts',(0.263741307412986,1.91479260723279,6.90034936086878));
#59576=CARTESIAN_POINT('Ctrl Pts',(0.264021968994568,1.9151930248978,6.90037979631037));
#59577=CARTESIAN_POINT('Ctrl Pts',(0.264140180146376,1.91536202072439,6.90039262173551));
#59578=CARTESIAN_POINT('Ctrl Pts',(0.264385899180326,1.91571402199706,6.90041929437713));
#59579=CARTESIAN_POINT('Ctrl Pts',(0.264513379156064,1.91589704613556,6.90043313960832));
#59580=CARTESIAN_POINT('Ctrl Pts',(0.264815812444016,1.91633221488298,6.90046600387927));
#59581=CARTESIAN_POINT('Ctrl Pts',(0.264990596386728,1.91658447819595,6.90048501124917));
#59582=CARTESIAN_POINT('Ctrl Pts',(0.26554081044429,1.91738102288873,6.90054489222762));
#59583=CARTESIAN_POINT('Ctrl Pts',(0.265914929071084,1.91792621460541,6.90058567679077));
#59584=CARTESIAN_POINT('Ctrl Pts',(0.270630306686199,1.92484332589904,6.90110064693492));
#59585=CARTESIAN_POINT('Ctrl Pts',(0.274743640307383,1.93136851370839,6.90155983601539));
#59586=CARTESIAN_POINT('Ctrl Pts',(0.282395221631989,1.94453114631521,6.90244773380957));
#59587=CARTESIAN_POINT('Ctrl Pts',(0.2859430615527,1.95115711960808,6.90287665316356));
#59588=CARTESIAN_POINT('Ctrl Pts',(0.299347135989773,1.97844247609117,6.90459463499572));
#59589=CARTESIAN_POINT('Ctrl Pts',(0.307221120035105,1.99999935510897,6.90584813836431));
#59590=CARTESIAN_POINT('Ctrl Pts',(0.313940419517456,2.0270130230886,6.90745168833202));
#59591=CARTESIAN_POINT('Ctrl Pts',(0.315024538895809,2.03184413135056,6.90773943658765));
#59592=CARTESIAN_POINT('Ctrl Pts',(0.317482117308508,2.0441121309603,6.90847467088267));
#59593=CARTESIAN_POINT('Ctrl Pts',(0.318705837155645,2.05157558416667,6.90892617765654));
#59594=CARTESIAN_POINT('Ctrl Pts',(0.319789255054213,2.06003812682986,6.9094452538242));
#59595=CARTESIAN_POINT('Ctrl Pts',(0.319908236213122,2.06100205997668,6.90950448202995));
#59596=CARTESIAN_POINT('Ctrl Pts',(0.320081671634351,2.06246138690652,6.90959430920316));
#59597=CARTESIAN_POINT('Ctrl Pts',(0.320139337840275,2.06295639931097,6.90962480691013));
#59598=CARTESIAN_POINT('Ctrl Pts',(0.320237610987965,2.06381735639922,6.90967789950418));
#59599=CARTESIAN_POINT('Ctrl Pts',(0.320278739543545,2.06418324157894,6.90970047791583));
#59600=CARTESIAN_POINT('Ctrl Pts',(0.320363198621967,2.06494637990663,6.90974760284944));
#59601=CARTESIAN_POINT('Ctrl Pts',(0.320406417445705,2.06534364458988,6.90977215285043));
#59602=CARTESIAN_POINT('Ctrl Pts',(0.320506776338543,2.06628237264813,6.90983020770833));
#59603=CARTESIAN_POINT('Ctrl Pts',(0.320563283199028,2.06682390119348,6.90986373244416));
#59604=CARTESIAN_POINT('Ctrl Pts',(0.320741504644544,2.0685748456329,6.90997224178341));
#59605=CARTESIAN_POINT('Ctrl Pts',(0.320857748162699,2.06978479674563,6.91004739829891));
#59606=CARTESIAN_POINT('Ctrl Pts',(0.321114770830753,2.07262902584098,6.91022448740044));
#59607=CARTESIAN_POINT('Ctrl Pts',(0.321249922033687,2.0742637666848,6.91032659521263));
#59608=CARTESIAN_POINT('Ctrl Pts',(0.322558293768807,2.09171045168674,6.9114199002776));
#59609=CARTESIAN_POINT('Ctrl Pts',(0.322575423068484,2.10758494703581,6.91244755852085));
#59610=CARTESIAN_POINT('Ctrl Pts',(0.320082331425727,2.14183866310184,6.91473105829981));
#59611=CARTESIAN_POINT('Ctrl Pts',(0.317154786697315,2.16013276498108,6.91599282916249));
#59612=CARTESIAN_POINT('Ctrl Pts',(0.30926222505182,2.19174159439278,6.91818319896648));
#59613=CARTESIAN_POINT('Ctrl Pts',(0.304956284510689,2.20517325489084,6.9191164632231));
#59614=CARTESIAN_POINT('Ctrl Pts',(0.29945626199369,2.21911306402177,6.92005873773542));
#59615=CARTESIAN_POINT('Ctrl Pts',(0.299124680872261,2.21994332080568,6.92011475550323));
#59616=CARTESIAN_POINT('Ctrl Pts',(0.29867282324115,2.22106121368575,6.92019002890422));
#59617=CARTESIAN_POINT('Ctrl Pts',(0.298555582100099,2.22135006057178,6.92020946476912));
#59618=CARTESIAN_POINT('Ctrl Pts',(0.298357111768316,2.22183700308775,6.92024220643058));
#59619=CARTESIAN_POINT('Ctrl Pts',(0.298276104263787,2.22203518791711,6.92025552562627));
#59620=CARTESIAN_POINT('Ctrl Pts',(0.298120056766718,2.22241587444413,6.92028109710688));
#59621=CARTESIAN_POINT('Ctrl Pts',(0.298045047213376,2.22259838658941,6.92029335107687));
#59622=CARTESIAN_POINT('Ctrl Pts',(0.297866654957414,2.22303131668672,6.92032240476938));
#59623=CARTESIAN_POINT('Ctrl Pts',(0.297763124195144,2.22328167297707,6.92033919535156));
#59624=CARTESIAN_POINT('Ctrl Pts',(0.297460611141861,2.22401060062407,6.92038805184601));
#59625=CARTESIAN_POINT('Ctrl Pts',(0.297260788745861,2.22448882572775,6.92042006685903));
#59626=CARTESIAN_POINT('Ctrl Pts',(0.296019576436037,2.22743932915773,6.92061736656948));
#59627=CARTESIAN_POINT('Ctrl Pts',(0.294948465540441,2.22989909949198,6.92078088197342));
#59628=CARTESIAN_POINT('Ctrl Pts',(0.291478915804195,2.2376025524802,6.92129078241875));
#59629=CARTESIAN_POINT('Ctrl Pts',(0.288970291683267,2.24279565801502,6.92163129037745));
#59630=CARTESIAN_POINT('Ctrl Pts',(0.276234500829984,2.26744804906988,6.9232450976797));
#59631=CARTESIAN_POINT('Ctrl Pts',(0.264173269128736,2.28589509884087,6.92444808012059));
#59632=CARTESIAN_POINT('Ctrl Pts',(0.237678598725944,2.31857124291158,6.92681640327721));
#59633=CARTESIAN_POINT('Ctrl Pts',(0.223601777943976,2.33295185625463,6.92797111173281));
#59634=CARTESIAN_POINT('Ctrl Pts',(0.207290181620077,2.34676636359385,6.92926939203645));
#59635=CARTESIAN_POINT('Ctrl Pts',(0.206295471013514,2.34759853828308,6.92934840367674));
#59636=CARTESIAN_POINT('Ctrl Pts',(0.204901541170681,2.34875046856641,6.92945891545481));
#59637=CARTESIAN_POINT('Ctrl Pts',(0.204506533438807,2.34907531985769,6.92949020858004));
#59638=CARTESIAN_POINT('Ctrl Pts',(0.203823218801629,2.34963455120821,6.92954430232737));
#59639=CARTESIAN_POINT('Ctrl Pts',(0.203535275908072,2.34986937615228,6.92956708491375));
#59640=CARTESIAN_POINT('Ctrl Pts',(0.202938582970869,2.3503542790381,6.92961427182778));
#59641=CARTESIAN_POINT('Ctrl Pts',(0.202629775377135,2.35060428491811,6.92963867900566));
#59642=CARTESIAN_POINT('Ctrl Pts',(0.201907179833363,2.35118707834066,6.92969575951856));
#59643=CARTESIAN_POINT('Ctrl Pts',(0.201493031062161,2.35151941480049,6.92972845088862));
#59644=CARTESIAN_POINT('Ctrl Pts',(0.200189704809308,2.35255999279017,6.92983125748689));
#59645=CARTESIAN_POINT('Ctrl Pts',(0.199297607590355,2.3532645482998,6.9299015197753));
#59646=CARTESIAN_POINT('Ctrl Pts',(0.192490649627179,2.35858227387704,6.93043686572223));
#59647=CARTESIAN_POINT('Ctrl Pts',(0.186420506963353,2.3629920568123,6.93090992055428));
#59648=CARTESIAN_POINT('Ctrl Pts',(0.174726979381646,2.37087871208087,6.93181432129725));
#59649=CARTESIAN_POINT('Ctrl Pts',(0.169139604457566,2.37440222082553,6.93224367080748));
#59650=CARTESIAN_POINT('Ctrl Pts',(0.14931448806461,2.38606869595261,6.93375664156678));
#59651=CARTESIAN_POINT('Ctrl Pts',(0.134567556897141,2.39329440062634,6.93486542684595));
#59652=CARTESIAN_POINT('Ctrl Pts',(0.101268433777865,2.40656842744533,6.9372909766152));
#59653=CARTESIAN_POINT('Ctrl Pts',(0.0825832733741295,2.41212127601144,
6.93860343936805));
#59654=CARTESIAN_POINT('Ctrl Pts',(0.062460643711344,2.41616607650144,6.93989636197436));
#59655=CARTESIAN_POINT('Ctrl Pts',(0.0614108320279248,2.41637166391644,
6.93996346946841));
#59656=CARTESIAN_POINT('Ctrl Pts',(0.0599935040764152,2.41664190230448,
6.94005358673988));
#59657=CARTESIAN_POINT('Ctrl Pts',(0.0596268861248823,2.41671114486353,
6.94007685370341));
#59658=CARTESIAN_POINT('Ctrl Pts',(0.0590505768257732,2.41681895533253,
6.94011335920189));
#59659=CARTESIAN_POINT('Ctrl Pts',(0.0588409675050555,2.41685795180989,
6.94012662221829));
#59660=CARTESIAN_POINT('Ctrl Pts',(0.0584370502230526,2.41693268341788,
6.94015215213424));
#59661=CARTESIAN_POINT('Ctrl Pts',(0.0582427495707399,2.41696844760936,
6.94016442059113));
#59662=CARTESIAN_POINT('Ctrl Pts',(0.0577800154651128,2.41705318148768,
6.94019360883034));
#59663=CARTESIAN_POINT('Ctrl Pts',(0.0575115528697855,2.41710198890331,
6.94021051922052));
#59664=CARTESIAN_POINT('Ctrl Pts',(0.0569543651722057,2.41720255666255,
6.94024556790815));
#59665=CARTESIAN_POINT('Ctrl Pts',(0.0566656305711251,2.41725426392566,
6.94026370317271));
#59666=CARTESIAN_POINT('Ctrl Pts',(0.0550166961769833,2.41754723603684,
6.94036712002625));
#59667=CARTESIAN_POINT('Ctrl Pts',(0.0536549994686444,2.41778015225312,
6.94045193243892));
#59668=CARTESIAN_POINT('Ctrl Pts',(0.0428446834331676,2.41955777307926,
6.94112087597888));
#59669=CARTESIAN_POINT('Ctrl Pts',(0.0333319879555434,2.42068965443206,
6.94168312635542));
#59670=CARTESIAN_POINT('Ctrl Pts',(0.00709862688728745,2.42263082072342,
6.94319573480625));
#59671=CARTESIAN_POINT('Ctrl Pts',(-0.00965646364775639,2.42256448958444,
6.94412089556285));
#59672=CARTESIAN_POINT('Ctrl Pts',(-0.0331721590932399,2.42063670125974,
6.94544289408972));
#59673=CARTESIAN_POINT('Ctrl Pts',(-0.0399931148771294,2.4198575197543,
6.9458290004088));
#59674=CARTESIAN_POINT('Ctrl Pts',(-0.0516428523980954,2.41814825121427,
6.94649833002995));
#59675=CARTESIAN_POINT('Ctrl Pts',(-0.0564848021687353,2.41732437422424,
6.94677947390256));
#59676=CARTESIAN_POINT('Ctrl Pts',(-0.0725254988566162,2.41421622027278,
6.947723872382));
#59677=CARTESIAN_POINT('Ctrl Pts',(-0.0836203602850281,2.41144722106272,
6.9483987061421));
#59678=CARTESIAN_POINT('Ctrl Pts',(-0.0956921648825162,2.40774279492059,
6.94916630417527));
#59679=CARTESIAN_POINT('Ctrl Pts',(-0.0968384180018671,2.40738402525708,
6.94923952370293));
#59680=CARTESIAN_POINT('Ctrl Pts',(-0.0984419545824516,2.4068722693139,
6.94934243072406));
#59681=CARTESIAN_POINT('Ctrl Pts',(-0.0989009508320979,2.40672464853088,
6.94937194182115));
#59682=CARTESIAN_POINT('Ctrl Pts',(-0.0997407191295573,2.40645248419772,
6.94942603605397));
#59683=CARTESIAN_POINT('Ctrl Pts',(-0.100121594124359,2.4063282594067,6.94945060865386));
#59684=CARTESIAN_POINT('Ctrl Pts',(-0.100891324790674,2.40607561795556,
6.94950034661922));
#59685=CARTESIAN_POINT('Ctrl Pts',(-0.101280169238756,2.40594716969013,
6.94952551298922));
#59686=CARTESIAN_POINT('Ctrl Pts',(-0.102058141513457,2.40568853387949,
6.94957594516013));
#59687=CARTESIAN_POINT('Ctrl Pts',(-0.102447267617827,2.40555834361007,
6.94960121101185));
#59688=CARTESIAN_POINT('Ctrl Pts',(-0.103374142362199,2.40524626872766,
6.94966149027512));
#59689=CARTESIAN_POINT('Ctrl Pts',(-0.103911659801901,2.40506370618593,
6.94969652608011));
#59690=CARTESIAN_POINT('Ctrl Pts',(-0.107521907810104,2.40382687198106,
6.94993237568279));
#59691=CARTESIAN_POINT('Ctrl Pts',(-0.110578936456974,2.40272764387393,
6.95013467575528));
#59692=CARTESIAN_POINT('Ctrl Pts',(-0.119015080409722,2.39954939487083,
6.95070037825136));
#59693=CARTESIAN_POINT('Ctrl Pts',(-0.124355584241294,2.39737200805112,
6.95106701001202));
#59694=CARTESIAN_POINT('Ctrl Pts',(-0.139427699016517,2.39074991268826,
6.95212669889253));
#59695=CARTESIAN_POINT('Ctrl Pts',(-0.148999692873216,2.38596267197528,
6.9528303803244));
#59696=CARTESIAN_POINT('Ctrl Pts',(-0.165942334182022,2.37640729519951,
6.9541288497474));
#59697=CARTESIAN_POINT('Ctrl Pts',(-0.173390669436343,2.3717968304015,6.9547196486308));
#59698=CARTESIAN_POINT('Ctrl Pts',(-0.198777682056132,2.35461382338246,
6.95679344974949));
#59699=CARTESIAN_POINT('Ctrl Pts',(-0.215617196123676,2.34052069462305,
6.95828286081767));
#59700=CARTESIAN_POINT('Ctrl Pts',(-0.231745221586659,2.32395714283031,
6.95974119456232));
#59701=CARTESIAN_POINT('Ctrl Pts',(-0.232587269943504,2.32308252178152,
6.95981742489979));
#59702=CARTESIAN_POINT('Ctrl Pts',(-0.23369509726322,2.32191874935333,6.95991781068218));
#59703=CARTESIAN_POINT('Ctrl Pts',(-0.23396530485812,2.32163385555001,6.95994230306239));
#59704=CARTESIAN_POINT('Ctrl Pts',(-0.234384129806912,2.32119064733504,
6.95998027720748));
#59705=CARTESIAN_POINT('Ctrl Pts',(-0.234533107797189,2.32103267659218,
6.95999378689288));
#59706=CARTESIAN_POINT('Ctrl Pts',(-0.234816737187704,2.32073131688219,
6.96001951089539));
#59707=CARTESIAN_POINT('Ctrl Pts',(-0.234951416065557,2.3205879561652,6.96003172731854));
#59708=CARTESIAN_POINT('Ctrl Pts',(-0.23526724784478,2.32025114745237,6.96006037960331));
#59709=CARTESIAN_POINT('Ctrl Pts',(-0.2354482931548,2.32005759953758,6.96007680708775));
#59710=CARTESIAN_POINT('Ctrl Pts',(-0.235821767381931,2.31965734544828,
6.96011070180902));
#59711=CARTESIAN_POINT('Ctrl Pts',(-0.236014163853594,2.31945060911844,
6.96012816655049));
#59712=CARTESIAN_POINT('Ctrl Pts',(-0.236510062692875,2.31891634305834,
6.96017319221157));
#59713=CARTESIAN_POINT('Ctrl Pts',(-0.236813157803925,2.31858843361338,
6.96020072230402));
#59714=CARTESIAN_POINT('Ctrl Pts',(-0.240470518039745,2.31461511055141,
6.96053305964955));
#59715=CARTESIAN_POINT('Ctrl Pts',(-0.243741205637736,2.31089321219542,
6.96083168738644));
#59716=CARTESIAN_POINT('Ctrl Pts',(-0.254233219154438,2.29838342891621,
6.96180022949518));
#59717=CARTESIAN_POINT('Ctrl Pts',(-0.261075748884775,2.28928817513233,
6.96244940082143));
#59718=CARTESIAN_POINT('Ctrl Pts',(-0.269950742157918,2.27609168038358,
6.96334567196271));
#59719=CARTESIAN_POINT('Ctrl Pts',(-0.272398480622213,2.27228102566769,
6.96359947493373));
#59720=CARTESIAN_POINT('Ctrl Pts',(-0.277286795834698,2.26430609135024,
6.96412281761958));
#59721=CARTESIAN_POINT('Ctrl Pts',(-0.279715754307783,2.26013605352149,
6.96439223218429));
#59722=CARTESIAN_POINT('Ctrl Pts',(-0.293866292507904,2.23453741633889,
6.9660285358304));
#59723=CARTESIAN_POINT('Ctrl Pts',(-0.303212357072985,2.21189160382883,
6.96741091003816));
#59724=CARTESIAN_POINT('Ctrl Pts',(-0.310307931684961,2.18701870239421,
6.96898029825098));
#59725=CARTESIAN_POINT('Ctrl Pts',(-0.31069528767595,2.18562537674433,6.96906834488947));
#59726=CARTESIAN_POINT('Ctrl Pts',(-0.311213277066018,2.18371235784494,
6.96918942906307));
#59727=CARTESIAN_POINT('Ctrl Pts',(-0.311352015812389,2.18319486115274,
6.96922220362307));
#59728=CARTESIAN_POINT('Ctrl Pts',(-0.31158645398836,2.18231160461384,6.96927817728737));
#59729=CARTESIAN_POINT('Ctrl Pts',(-0.311682801746273,2.181946016723,6.9693013553528));
#59730=CARTESIAN_POINT('Ctrl Pts',(-0.311868319561988,2.18123701596273,
6.96934632542909));
#59731=CARTESIAN_POINT('Ctrl Pts',(-0.311957566309265,2.18089362354218,
6.96936811492308));
#59732=CARTESIAN_POINT('Ctrl Pts',(-0.312168638996795,2.18007594049113,
6.96942002163478));
#59733=CARTESIAN_POINT('Ctrl Pts',(-0.312289951087387,2.17960151923348,
6.96945015541383));
#59734=CARTESIAN_POINT('Ctrl Pts',(-0.31253896927483,2.17861834043678,6.96951264066866));
#59735=CARTESIAN_POINT('Ctrl Pts',(-0.312666515419028,2.17810954422419,
6.96954499721795));
#59736=CARTESIAN_POINT('Ctrl Pts',(-0.312995530133078,2.17678334764678,
6.96962938984752));
#59737=CARTESIAN_POINT('Ctrl Pts',(-0.313195038014143,2.1759654691349,6.96968148904755));
#59738=CARTESIAN_POINT('Ctrl Pts',(-0.319317992010291,2.1504303815822,6.97130979865669));
#59739=CARTESIAN_POINT('Ctrl Pts',(-0.322298355976539,2.12510622756114,
6.97298570556493));
#59740=CARTESIAN_POINT('Ctrl Pts',(-0.322274862187325,2.09970196117587,
6.97470119138623));
#59741=CARTESIAN_POINT('',(-0.3219654526091,2.10024677492677,7.22472265507269));
#59742=CARTESIAN_POINT('Ctrl Pts',(-0.322274862242446,2.09970202078479,
6.97470118736099));
#59743=CARTESIAN_POINT('Ctrl Pts',(-0.322254792744558,2.07799616233327,
6.97616692902254));
#59744=CARTESIAN_POINT('Ctrl Pts',(-0.320041910222358,2.05634574280106,
6.97765048953118));
#59745=CARTESIAN_POINT('Ctrl Pts',(-0.314997195943813,2.03181606877893,
6.97925888435003));
#59746=CARTESIAN_POINT('Ctrl Pts',(-0.31427524269446,2.02856222364379,6.9794706346778));
#59747=CARTESIAN_POINT('Ctrl Pts',(-0.313397127533594,2.02487593948198,
6.97970824887217));
#59748=CARTESIAN_POINT('Ctrl Pts',(-0.313290400305139,2.02443208949767,
6.97973682125599));
#59749=CARTESIAN_POINT('Ctrl Pts',(-0.313091214045297,2.02361140226623,
6.97978958036946));
#59750=CARTESIAN_POINT('Ctrl Pts',(-0.312999017050846,2.0232345031602,6.97981378185102));
#59751=CARTESIAN_POINT('Ctrl Pts',(-0.312848648111069,2.02262457311482,
6.97985290027779));
#59752=CARTESIAN_POINT('Ctrl Pts',(-0.312790896299247,2.02239144052486,
6.97986784145167));
#59753=CARTESIAN_POINT('Ctrl Pts',(-0.312679612762009,2.02194435299197,
6.97989647332939));
#59754=CARTESIAN_POINT('Ctrl Pts',(-0.3126261221968,2.02173038912028,6.97991016631736));
#59755=CARTESIAN_POINT('Ctrl Pts',(-0.312502571952335,2.02123833170854,
6.97994163491793));
#59756=CARTESIAN_POINT('Ctrl Pts',(-0.31243236048083,2.0209602758432,6.97995940169246));
#59757=CARTESIAN_POINT('Ctrl Pts',(-0.312213660337644,2.02009901062124,
6.98001438565315));
#59758=CARTESIAN_POINT('Ctrl Pts',(-0.31206390805354,2.01951611894747,6.98005153002816));
#59759=CARTESIAN_POINT('Ctrl Pts',(-0.31081035419789,2.01469292018172,6.98035834787495));
#59760=CARTESIAN_POINT('Ctrl Pts',(-0.309621749147266,2.01047485702557,
6.98062323055529));
#59761=CARTESIAN_POINT('Ctrl Pts',(-0.302498597866835,1.98703850955839,
6.98208238234991));
#59762=CARTESIAN_POINT('Ctrl Pts',(-0.294860426573917,1.9683822720351,6.98319811786653));
#59763=CARTESIAN_POINT('Ctrl Pts',(-0.283385561392874,1.94645776178699,
6.98458152913997));
#59764=CARTESIAN_POINT('Ctrl Pts',(-0.281151386680398,1.94240402142001,
6.98484045433555));
#59765=CARTESIAN_POINT('Ctrl Pts',(-0.276632149757246,1.93460636838058,
6.98534674806971));
#59766=CARTESIAN_POINT('Ctrl Pts',(-0.274356444052104,1.93085822492165,
6.98559395237056));
#59767=CARTESIAN_POINT('Ctrl Pts',(-0.265021826999951,1.916168168351,6.98658141772468));
#59768=CARTESIAN_POINT('Ctrl Pts',(-0.257379771736471,1.90561298929361,
6.98733341773803));
#59769=CARTESIAN_POINT('Ctrl Pts',(-0.246245651698839,1.89204616962227,
6.98838041746954));
#59770=CARTESIAN_POINT('Ctrl Pts',(-0.243296964569347,1.88860392525328,
6.98865357757056));
#59771=CARTESIAN_POINT('Ctrl Pts',(-0.239863908470939,1.8847632353686,6.98896750425641));
#59772=CARTESIAN_POINT('Ctrl Pts',(-0.239449707636792,1.88430253376502,
6.98900531366845));
#59773=CARTESIAN_POINT('Ctrl Pts',(-0.238744922490738,1.8835231568928,6.98906953814448));
#59774=CARTESIAN_POINT('Ctrl Pts',(-0.238455021080262,1.88320386411302,
6.98909592438253));
#59775=CARTESIAN_POINT('Ctrl Pts',(-0.237879247311214,1.88257226814362,
6.98914826857364));
#59776=CARTESIAN_POINT('Ctrl Pts',(-0.237593398657462,1.88225994444465,
6.98917422549375));
#59777=CARTESIAN_POINT('Ctrl Pts',(-0.237038388916846,1.88165592442344,
6.98922456671188));
#59778=CARTESIAN_POINT('Ctrl Pts',(-0.236769302659316,1.88136416013001,
6.98924894779716));
#59779=CARTESIAN_POINT('Ctrl Pts',(-0.236146874516471,1.88069177168446,
6.98930528483119));
#59780=CARTESIAN_POINT('Ctrl Pts',(-0.23579315087413,1.88031150383642,6.98933725708172));
#59781=CARTESIAN_POINT('Ctrl Pts',(-0.234657732686394,1.87909678255724,
6.98943974608736));
#59782=CARTESIAN_POINT('Ctrl Pts',(-0.233872522470797,1.8782656405398,6.98951041389108));
#59783=CARTESIAN_POINT('Ctrl Pts',(-0.226611118696692,1.87066095286541,
6.99016205137652));
#59784=CARTESIAN_POINT('Ctrl Pts',(-0.219847387035011,1.86416935179256,
6.99075558471187));
#59785=CARTESIAN_POINT('Ctrl Pts',(-0.202537593674635,1.84894851597665,
6.99224502900062));
#59786=CARTESIAN_POINT('Ctrl Pts',(-0.191700482554144,1.84057914690088,
6.99315340432819));
#59787=CARTESIAN_POINT('Ctrl Pts',(-0.17348095558115,1.82827486697669,6.9946330472514));
#59788=CARTESIAN_POINT('Ctrl Pts',(-0.16641926340663,1.82389347177389,6.99519588975997));
#59789=CARTESIAN_POINT('Ctrl Pts',(-0.152166532422991,1.81579604058651,
6.99630466136703));
#59790=CARTESIAN_POINT('Ctrl Pts',(-0.144988726235248,1.81206802614663,
6.9968502549413));
#59791=CARTESIAN_POINT('Ctrl Pts',(-0.130487550700357,1.80521631336783,
6.99791911633876));
#59792=CARTESIAN_POINT('Ctrl Pts',(-0.12317308996342,1.80208586322981,6.99844224554016));
#59793=CARTESIAN_POINT('Ctrl Pts',(-0.113671559665417,1.79842926089034,
6.99909529680369));
#59794=CARTESIAN_POINT('Ctrl Pts',(-0.111585065740821,1.79765101638616,
6.99923710103793));
#59795=CARTESIAN_POINT('Ctrl Pts',(-0.108218436434433,1.79643489125952,
6.99946315122764));
#59796=CARTESIAN_POINT('Ctrl Pts',(-0.106943357078685,1.79598334953672,
6.99954813544767));
#59797=CARTESIAN_POINT('Ctrl Pts',(-0.105389961834506,1.79544423071917,
6.99965087243873));
#59798=CARTESIAN_POINT('Ctrl Pts',(-0.105114346584899,1.79534899507577,
6.99966907041602));
#59799=CARTESIAN_POINT('Ctrl Pts',(-0.104581751369334,1.79516577179543,
6.99970417672085));
#59800=CARTESIAN_POINT('Ctrl Pts',(-0.10432478882804,1.79507773475549,6.99972108795617));
#59801=CARTESIAN_POINT('Ctrl Pts',(-0.103861152295083,1.79491954453971,
6.99975155250005));
#59802=CARTESIAN_POINT('Ctrl Pts',(-0.103654518868025,1.79484927662042,
6.99976511261138));
#59803=CARTESIAN_POINT('Ctrl Pts',(-0.103240246777219,1.79470886828655,
6.99979226405422));
#59804=CARTESIAN_POINT('Ctrl Pts',(-0.10303260887135,1.79463873007968,6.99980585523009));
#59805=CARTESIAN_POINT('Ctrl Pts',(-0.102443256551049,1.79444032175268,
6.99984438292737));
#59806=CARTESIAN_POINT('Ctrl Pts',(-0.102061371327203,1.79431255460784,
6.99986928957191));
#59807=CARTESIAN_POINT('Ctrl Pts',(-0.100451880764203,1.7937774204431,6.9999740194041));
#59808=CARTESIAN_POINT('Ctrl Pts',(-0.099222046459794,1.79337672265726,
7.00005345373485));
#59809=CARTESIAN_POINT('Ctrl Pts',(-0.0772259307896723,1.78635627036069,
7.00146419388377));
#59810=CARTESIAN_POINT('Ctrl Pts',(-0.0558396019943225,1.78185146262231,
7.00267957198056));
#59811=CARTESIAN_POINT('Ctrl Pts',(-0.0175874211049619,1.77777398462785,
7.00482988239314));
#59812=CARTESIAN_POINT('Ctrl Pts',(-0.000904172467797171,1.77729571242723,
7.00576005327469));
#59813=CARTESIAN_POINT('Ctrl Pts',(0.0269410660454354,1.77865732786812,
7.00737321285849));
#59814=CARTESIAN_POINT('Ctrl Pts',(0.0381045312832558,1.77978923199218,
7.00803602404254));
#59815=CARTESIAN_POINT('Ctrl Pts',(0.0503120790039915,1.78167442793353,
7.0087871611806));
#59816=CARTESIAN_POINT('Ctrl Pts',(0.0514377380760737,1.78185438212276,
7.0088566684155));
#59817=CARTESIAN_POINT('Ctrl Pts',(0.0530860746424093,1.78212687118067,
7.00895881689084));
#59818=CARTESIAN_POINT('Ctrl Pts',(0.0536095246281474,1.78221473254704,
7.00899130974107));
#59819=CARTESIAN_POINT('Ctrl Pts',(0.0545243936914246,1.78237061856081,
7.0090481955905));
#59820=CARTESIAN_POINT('Ctrl Pts',(0.0549159095393933,1.78243807479794,
7.00907257048062));
#59821=CARTESIAN_POINT('Ctrl Pts',(0.0556734053631594,1.78257003030272,
7.00911979035278));
#59822=CARTESIAN_POINT('Ctrl Pts',(0.0560394006742645,1.78263443901863,
7.00914263242039));
#59823=CARTESIAN_POINT('Ctrl Pts',(0.0569090578074398,1.78278903459385,
7.00919697321516));
#59824=CARTESIAN_POINT('Ctrl Pts',(0.0574126167115783,1.78287978797948,
7.00922848993396));
#59825=CARTESIAN_POINT('Ctrl Pts',(0.0591931611535906,1.78320506476013,
7.00934011486137));
#59826=CARTESIAN_POINT('Ctrl Pts',(0.0604689303352418,1.78344610299987,
7.00942043036366));
#59827=CARTESIAN_POINT('Ctrl Pts',(0.0818068747996287,1.78761129851937,
7.01076947578114));
#59828=CARTESIAN_POINT('Ctrl Pts',(0.101448431137458,1.79342701559916,7.0121007371681));
#59829=CARTESIAN_POINT('Ctrl Pts',(0.135864813987744,1.8072889776216,7.01458661498581));
#59830=CARTESIAN_POINT('Ctrl Pts',(0.150818733051426,1.81470597713951,7.01572364862022));
#59831=CARTESIAN_POINT('Ctrl Pts',(0.171358997214046,1.82696180547616,7.01732719211138));
#59832=CARTESIAN_POINT('Ctrl Pts',(0.177459528211848,1.83088684558264,7.01780892246554));
#59833=CARTESIAN_POINT('Ctrl Pts',(0.186804858036504,1.8373556779254,7.01855002469984));
#59834=CARTESIAN_POINT('Ctrl Pts',(0.190142007627846,1.83976142603937,7.0188153163938));
#59835=CARTESIAN_POINT('Ctrl Pts',(0.194557739821838,1.84307502810489,7.01916626420745));
#59836=CARTESIAN_POINT('Ctrl Pts',(0.195677609977771,1.84392690803876,7.01925525969968));
#59837=CARTESIAN_POINT('Ctrl Pts',(0.197542998685717,1.84536528339368,7.01940343737787));
#59838=CARTESIAN_POINT('Ctrl Pts',(0.198291559967675,1.84594777597882,7.01946288214594));
#59839=CARTESIAN_POINT('Ctrl Pts',(0.19931025359011,1.84674771735716,7.01954374213382));
#59840=CARTESIAN_POINT('Ctrl Pts',(0.199582613126948,1.84696230243286,7.01956535739938));
#59841=CARTESIAN_POINT('Ctrl Pts',(0.200035895414153,1.84732061904196,7.01960132448628));
#59842=CARTESIAN_POINT('Ctrl Pts',(0.200217010015924,1.84746410568679,7.01961569378468));
#59843=CARTESIAN_POINT('Ctrl Pts',(0.200572208129372,1.84774613095406,7.01964387074479));
#59844=CARTESIAN_POINT('Ctrl Pts',(0.200746302468499,1.8478846550322,7.01965767938979));
#59845=CARTESIAN_POINT('Ctrl Pts',(0.20112886694132,1.84818970295575,7.01968801961105));
#59846=CARTESIAN_POINT('Ctrl Pts',(0.201337274452864,1.84835630599656,7.01970454549394));
#59847=CARTESIAN_POINT('Ctrl Pts',(0.202059612325509,1.84893522187206,7.01976181664903));
#59848=CARTESIAN_POINT('Ctrl Pts',(0.202572489442351,1.84934885540107,7.01980246760025));
#59849=CARTESIAN_POINT('Ctrl Pts',(0.207611232228897,1.85343815031116,7.0202017542648));
#59850=CARTESIAN_POINT('Ctrl Pts',(0.212038176777069,1.85723469882466,7.02055186820207));
#59851=CARTESIAN_POINT('Ctrl Pts',(0.216491383011562,1.86126858577677,7.0209062581015));
#59852=CARTESIAN_POINT('Ctrl Pts',(0.216622678369134,1.86138771558939,7.02091670871348));
#59853=CARTESIAN_POINT('Ctrl Pts',(0.217056353430299,1.86178186020601,7.02095123453494));
#59854=CARTESIAN_POINT('Ctrl Pts',(0.217358309353345,1.86205734293598,7.02097528506401));
#59855=CARTESIAN_POINT('Ctrl Pts',(0.218655209722032,1.86324506978252,7.02107863431232));
#59856=CARTESIAN_POINT('Ctrl Pts',(0.219644952947361,1.86416299598713,7.02115763907955));
#59857=CARTESIAN_POINT('Ctrl Pts',(0.226692960356299,1.87078244676926,7.02172143991755));
#59858=CARTESIAN_POINT('Ctrl Pts',(0.232534557943049,1.87671077091138,7.02219520868321));
#59859=CARTESIAN_POINT('Ctrl Pts',(0.247872276352638,1.89353176996463,7.02347881856043));
#59860=CARTESIAN_POINT('Ctrl Pts',(0.256875600910535,1.90484690750524,7.02427846625861));
#59861=CARTESIAN_POINT('Ctrl Pts',(0.272266173905734,1.92710824065107,7.02580309642709));
#59862=CARTESIAN_POINT('Ctrl Pts',(0.278826239208303,1.93790028804703,7.02652332578263));
#59863=CARTESIAN_POINT('Ctrl Pts',(0.288176330987927,1.95553715483856,7.02769673061448));
#59864=CARTESIAN_POINT('Ctrl Pts',(0.291393227305255,1.96214106630717,7.0281352146176));
#59865=CARTESIAN_POINT('Ctrl Pts',(0.29485569520998,1.96991290647565,7.02865251066988));
#59866=CARTESIAN_POINT('Ctrl Pts',(0.295324026915276,1.9709796451325,7.02872353832026));
#59867=CARTESIAN_POINT('Ctrl Pts',(0.295998891375999,1.97253973972819,7.02882746058706));
#59868=CARTESIAN_POINT('Ctrl Pts',(0.296210000059583,1.97303111600225,7.02886019901778));
#59869=CARTESIAN_POINT('Ctrl Pts',(0.296576059324835,1.97388903685823,7.02891737103253));
#59870=CARTESIAN_POINT('Ctrl Pts',(0.296731556348385,1.97425534820932,7.02894178595786));
#59871=CARTESIAN_POINT('Ctrl Pts',(0.297030531716962,1.97496330075563,7.0289889793721));
#59872=CARTESIAN_POINT('Ctrl Pts',(0.297174100185118,1.97530490343493,7.02901175475345));
#59873=CARTESIAN_POINT('Ctrl Pts',(0.297512923641364,1.97611499888253,7.02906577425903));
#59874=CARTESIAN_POINT('Ctrl Pts',(0.297707661215579,1.97658370575829,7.02909703587927));
#59875=CARTESIAN_POINT('Ctrl Pts',(0.298387361061039,1.97823062064229,7.02920690665641));
#59876=CARTESIAN_POINT('Ctrl Pts',(0.298866437925924,1.97941123105248,7.02928571464882));
#59877=CARTESIAN_POINT('Ctrl Pts',(0.305665512298149,1.99645589853904,7.03042421643172));
#59878=CARTESIAN_POINT('Ctrl Pts',(0.31072080174336,2.0127922077944,7.03152683671944));
#59879=CARTESIAN_POINT('Ctrl Pts',(0.319603290784243,2.05238341187556,7.0342222451962));
#59880=CARTESIAN_POINT('Ctrl Pts',(0.322224013824275,2.07580928575558,7.03583815506516));
#59881=CARTESIAN_POINT('Ctrl Pts',(0.322293176912857,2.10815679139511,7.03798389968668));
#59882=CARTESIAN_POINT('Ctrl Pts',(0.321947877706716,2.11700060934334,7.03856089700817));
#59883=CARTESIAN_POINT('Ctrl Pts',(0.32116725132738,2.12671282266034,7.03917617712368));
#59884=CARTESIAN_POINT('Ctrl Pts',(0.321091751784266,2.12760552842893,7.03923255874372));
#59885=CARTESIAN_POINT('Ctrl Pts',(0.320953571610498,2.12916204789581,7.03933055129066));
#59886=CARTESIAN_POINT('Ctrl Pts',(0.320892552122379,2.12982599836106,7.03937225124895));
#59887=CARTESIAN_POINT('Ctrl Pts',(0.320801231452367,2.13078692297071,7.03943245365061));
#59888=CARTESIAN_POINT('Ctrl Pts',(0.320772577993986,2.13108404632893,7.03945104790475));
#59889=CARTESIAN_POINT('Ctrl Pts',(0.32072193331689,2.13160168068814,7.03948340541087));
#59890=CARTESIAN_POINT('Ctrl Pts',(0.32070012743129,2.13182220921936,7.03949717916308));
#59891=CARTESIAN_POINT('Ctrl Pts',(0.320657370066782,2.13225011769745,7.03952388280717));
#59892=CARTESIAN_POINT('Ctrl Pts',(0.320636444926637,2.13245749921168,7.03953681417184));
#59893=CARTESIAN_POINT('Ctrl Pts',(0.320585815996408,2.13295443720816,7.03956777661595));
#59894=CARTESIAN_POINT('Ctrl Pts',(0.320555921019732,2.13324397464996,7.03958579685738));
#59895=CARTESIAN_POINT('Ctrl Pts',(0.320446709358328,2.13428786108203,7.03965069613542));
#59896=CARTESIAN_POINT('Ctrl Pts',(0.320365121052315,2.13504197763636,7.03969744803567));
#59897=CARTESIAN_POINT('Ctrl Pts',(0.318922930098314,2.14794589568213,7.04049527859276));
#59898=CARTESIAN_POINT('Ctrl Pts',(0.316874517048569,2.1600105221783,7.04120861049668));
#59899=CARTESIAN_POINT('Ctrl Pts',(0.30942305302643,2.19255340371752,7.04311333347171));
#59900=CARTESIAN_POINT('Ctrl Pts',(0.302681830683638,2.21266113052972,7.0442717244115));
#59901=CARTESIAN_POINT('Ctrl Pts',(0.287284903905455,2.24696585816649,7.04640569301412));
#59902=CARTESIAN_POINT('Ctrl Pts',(0.279414150299898,2.26142861548592,7.04736068426978));
#59903=CARTESIAN_POINT('Ctrl Pts',(0.269643080645295,2.27651098181804,7.048450619341));
#59904=CARTESIAN_POINT('Ctrl Pts',(0.268801867576734,2.27778940773735,7.04854377105531));
#59905=CARTESIAN_POINT('Ctrl Pts',(0.267623517663034,2.27955271390534,7.0486733376551));
#59906=CARTESIAN_POINT('Ctrl Pts',(0.267294096329676,2.28004274586078,7.04870946191507));
#59907=CARTESIAN_POINT('Ctrl Pts',(0.266733118802135,2.28087229707631,7.04877081493999));
#59908=CARTESIAN_POINT('Ctrl Pts',(0.266502255628791,2.2812122850633,7.04879601745041));
#59909=CARTESIAN_POINT('Ctrl Pts',(0.266045709841255,2.28188187229255,7.04884576583939));
#59910=CARTESIAN_POINT('Ctrl Pts',(0.265820063438153,2.28221149542505,7.04887031031383));
#59911=CARTESIAN_POINT('Ctrl Pts',(0.265323248928546,2.28293435262041,7.0489242559801));
#59912=CARTESIAN_POINT('Ctrl Pts',(0.265051818583454,2.2833274045317,7.04895366712411));
#59913=CARTESIAN_POINT('Ctrl Pts',(0.264110263514108,2.28468438635085,7.04905547918036));
#59914=CARTESIAN_POINT('Ctrl Pts',(0.263435752274419,2.28564524831094,7.04912804754129));
#59915=CARTESIAN_POINT('Ctrl Pts',(0.256730594076715,2.29508682408247,7.04984587661982));
#59916=CARTESIAN_POINT('Ctrl Pts',(0.250298408644388,2.30327354321823,7.05050668382026));
#59917=CARTESIAN_POINT('Ctrl Pts',(0.225153041468552,2.33227144318951,7.05299752426387));
#59918=CARTESIAN_POINT('Ctrl Pts',(0.204150559004003,2.35093034998928,7.05491988664511));
#59919=CARTESIAN_POINT('Ctrl Pts',(0.171892839572546,2.37282857960462,7.05752651879063));
#59920=CARTESIAN_POINT('Ctrl Pts',(0.162464046834826,2.37854635231268,7.05825146107769));
#59921=CARTESIAN_POINT('Ctrl Pts',(0.151867060814155,2.38425094465483,7.05901267943664));
#59922=CARTESIAN_POINT('Ctrl Pts',(0.150971987795774,2.38472734793461,7.05907657070885));
#59923=CARTESIAN_POINT('Ctrl Pts',(0.14942704564438,2.38554031099556,7.05918613545004));
#59924=CARTESIAN_POINT('Ctrl Pts',(0.148778257268236,2.3858788928244,7.05923193070509));
#59925=CARTESIAN_POINT('Ctrl Pts',(0.147850811300943,2.38635888471757,7.05929708181036));
#59926=CARTESIAN_POINT('Ctrl Pts',(0.147573098735881,2.38650210084832,7.05931655055731));
#59927=CARTESIAN_POINT('Ctrl Pts',(0.147095884659297,2.38674732177676,7.05934993599278));
#59928=CARTESIAN_POINT('Ctrl Pts',(0.14689648462927,2.38684952263256,7.05936386512978));
#59929=CARTESIAN_POINT('Ctrl Pts',(0.146514463445131,2.38704482166296,7.05939051148031));
#59930=CARTESIAN_POINT('Ctrl Pts',(0.146331860317846,2.38713795342769,7.05940323084658));
#59931=CARTESIAN_POINT('Ctrl Pts',(0.145901520745474,2.38735691931166,7.05943316586396));
#59932=CARTESIAN_POINT('Ctrl Pts',(0.145653709699228,2.38748260762058,7.05945037226648));
#59933=CARTESIAN_POINT('Ctrl Pts',(0.144921289292561,2.38785289682239,7.05950113422942));
#59934=CARTESIAN_POINT('Ctrl Pts',(0.144436221058027,2.38809659552977,7.05953463335479));
#59935=CARTESIAN_POINT('Ctrl Pts',(0.140181081151138,2.39022093361568,7.05982747000392));
#59936=CARTESIAN_POINT('Ctrl Pts',(0.136374866212024,2.39202880991834,7.06008236690488));
#59937=CARTESIAN_POINT('Ctrl Pts',(0.132254320782541,2.39388784332185,7.06035197954533));
#59938=CARTESIAN_POINT('Ctrl Pts',(0.131974384628198,2.39401365890281,7.06037026508446));
#59939=CARTESIAN_POINT('Ctrl Pts',(0.131051192966086,2.39442699756022,7.06043046742698));
#59940=CARTESIAN_POINT('Ctrl Pts',(0.130407170009668,2.39471281291533,7.06047230362381));
#59941=CARTESIAN_POINT('Ctrl Pts',(0.103852017062125,2.40639381636734,7.06219092124355));
#59942=CARTESIAN_POINT('Ctrl Pts',(0.0765503682063327,2.41432923185706,
7.0637158310133));
#59943=CARTESIAN_POINT('Ctrl Pts',(0.0333218479986648,2.42091810897705,
7.06619663437679));
#59944=CARTESIAN_POINT('Ctrl Pts',(0.0179384048535991,2.42214422122447,
7.0670899545166));
#59945=CARTESIAN_POINT('Ctrl Pts',(7.96595485979168E-5,2.42228428702588,
7.06816724825204));
#59946=CARTESIAN_POINT('Ctrl Pts',(-0.00236828513133685,2.42227559436703,
7.06831575554552));
#59947=CARTESIAN_POINT('Ctrl Pts',(-0.00552313522269598,2.42222844532618,
7.06850830501083));
#59948=CARTESIAN_POINT('Ctrl Pts',(-0.00623038693984165,2.42221554628234,
7.06855154548899));
#59949=CARTESIAN_POINT('Ctrl Pts',(-0.00737143835275037,2.42219097727389,
7.06862143075003));
#59950=CARTESIAN_POINT('Ctrl Pts',(-0.00780526965702664,2.4221807593615,
7.06864802999268));
#59951=CARTESIAN_POINT('Ctrl Pts',(-0.00863250842986229,2.42215960378743,
7.06869880513676));
#59952=CARTESIAN_POINT('Ctrl Pts',(-0.00902591937755676,2.42214882165154,
7.06872297611904));
#59953=CARTESIAN_POINT('Ctrl Pts',(-0.00992419464094185,2.42212255604658,
7.06877822047647));
#59954=CARTESIAN_POINT('Ctrl Pts',(-0.0104290433625144,2.42210660627061,
7.06880930841204));
#59955=CARTESIAN_POINT('Ctrl Pts',(-0.0119735212883351,2.42205417645872,
7.06890453741189));
#59956=CARTESIAN_POINT('Ctrl Pts',(-0.0130130054638803,2.42201384975603,
7.06896879886838));
#59957=CARTESIAN_POINT('Ctrl Pts',(-0.0207030291127939,2.42167821982743,
7.06944547540725));
#59958=CARTESIAN_POINT('Ctrl Pts',(-0.0273427632544859,2.42118196582502,
7.06986415895268));
#59959=CARTESIAN_POINT('Ctrl Pts',(-0.0358116689572604,2.42028449808203,
7.0704078687766));
#59960=CARTESIAN_POINT('Ctrl Pts',(-0.0376595818808863,2.42007247775069,
7.07052709518816));
#59961=CARTESIAN_POINT('Ctrl Pts',(-0.0418092754205066,2.41955992918412,
7.07079615898283));
#59962=CARTESIAN_POINT('Ctrl Pts',(-0.0441098366241475,2.41925050625653,
7.07094624719358));
#59963=CARTESIAN_POINT('Ctrl Pts',(-0.0684693614032441,2.41570585212978,
7.07254517118954));
#59964=CARTESIAN_POINT('Ctrl Pts',(-0.0901369512278037,2.41021497589176,
7.07405822799484));
#59965=CARTESIAN_POINT('Ctrl Pts',(-0.115653584872897,2.40084772983796,
7.07589449045489));
#59966=CARTESIAN_POINT('Ctrl Pts',(-0.120207120565101,2.39905744980875,
7.07622412330533));
#59967=CARTESIAN_POINT('Ctrl Pts',(-0.135336391650622,2.39270777545903,
7.07732271935609));
#59968=CARTESIAN_POINT('Ctrl Pts',(-0.145709373346801,2.38768493202435,
7.07808178952665));
#59969=CARTESIAN_POINT('Ctrl Pts',(-0.156700950913653,2.38161510128957,
7.07887623940425));
#59970=CARTESIAN_POINT('Ctrl Pts',(-0.157607285925889,2.38110886998203,
7.0789416697534));
#59971=CARTESIAN_POINT('Ctrl Pts',(-0.159165080916036,2.38022886484133,
7.07905397518339));
#59972=CARTESIAN_POINT('Ctrl Pts',(-0.159817703220184,2.37985718042873,
7.07910097711435));
#59973=CARTESIAN_POINT('Ctrl Pts',(-0.160740188345622,2.37932752324656,
7.07916734095207));
#59974=CARTESIAN_POINT('Ctrl Pts',(-0.161011123383687,2.37917143754537,
7.0791868230639));
#59975=CARTESIAN_POINT('Ctrl Pts',(-0.161475854312515,2.3789028044352,7.07922022435599));
#59976=CARTESIAN_POINT('Ctrl Pts',(-0.16166976038697,2.37879044894924,7.07923415601498));
#59977=CARTESIAN_POINT('Ctrl Pts',(-0.162040762312015,2.37857496113782,
7.07926080210328));
#59978=CARTESIAN_POINT('Ctrl Pts',(-0.162217876736977,2.37847186229695,
7.07927351869513));
#59979=CARTESIAN_POINT('Ctrl Pts',(-0.16263474548547,2.37822866907277,7.07930343994072));
#59980=CARTESIAN_POINT('Ctrl Pts',(-0.162874417783053,2.37808843335584,
7.07932063536708));
#59981=CARTESIAN_POINT('Ctrl Pts',(-0.163700383119109,2.37760371502831,
7.07937987046904));
#59982=CARTESIAN_POINT('Ctrl Pts',(-0.16428577215988,2.37725768360229,7.07942181014637));
#59983=CARTESIAN_POINT('Ctrl Pts',(-0.17105001857142,2.37323030077992,7.07990599145593));
#59984=CARTESIAN_POINT('Ctrl Pts',(-0.177105628573264,2.36934461405321,
7.08033522524814));
#59985=CARTESIAN_POINT('Ctrl Pts',(-0.187664495926979,2.36205908285699,
7.08108545653552));
#59986=CARTESIAN_POINT('Ctrl Pts',(-0.192217844814387,2.35873776629691,
7.08140961719347));
#59987=CARTESIAN_POINT('Ctrl Pts',(-0.202302524056698,2.35096853369105,
7.0821345884973));
#59988=CARTESIAN_POINT('Ctrl Pts',(-0.207778731450337,2.34645389117074,
7.08253331290991));
#59989=CARTESIAN_POINT('Ctrl Pts',(-0.223264097021067,2.33280428871435,
7.08368919425291));
#59990=CARTESIAN_POINT('Ctrl Pts',(-0.232851590242998,2.32321474087947,
7.0844419604639));
#59991=CARTESIAN_POINT('Ctrl Pts',(-0.251933419974083,2.30155735618141,
7.08608001480512));
#59992=CARTESIAN_POINT('Ctrl Pts',(-0.261226325242482,2.28935821004901,
7.08696804258917));
#59993=CARTESIAN_POINT('Ctrl Pts',(-0.270952073854046,2.27450529312675,
7.08803903124635));
#59994=CARTESIAN_POINT('Ctrl Pts',(-0.272264872822716,2.27244988308826,
7.08818699249668));
#59995=CARTESIAN_POINT('Ctrl Pts',(-0.273927660473173,2.26978018578954,
7.08837893193387));
#59996=CARTESIAN_POINT('Ctrl Pts',(-0.274299156291246,2.26917933533512,
7.08842211471879));
#59997=CARTESIAN_POINT('Ctrl Pts',(-0.274895554537778,2.26820760342883,
7.08849192920926));
#59998=CARTESIAN_POINT('Ctrl Pts',(-0.275121690404882,2.26783747859686,
7.08851851554316));
#59999=CARTESIAN_POINT('Ctrl Pts',(-0.275551613073455,2.26713060487741,
7.08856928093525));
#60000=CARTESIAN_POINT('Ctrl Pts',(-0.275755531635995,2.26679393671245,
7.08859345510692));
#60001=CARTESIAN_POINT('Ctrl Pts',(-0.276219929132113,2.26602404016256,
7.08864872761308));
#60002=CARTESIAN_POINT('Ctrl Pts',(-0.27648000607169,2.26559057159031,7.08867984056168));
#60003=CARTESIAN_POINT('Ctrl Pts',(-0.277273213120687,2.26426146022828,
7.08877522056662));
#60004=CARTESIAN_POINT('Ctrl Pts',(-0.277803014988361,2.26336384806036,
7.0888396085735));
#60005=CARTESIAN_POINT('Ctrl Pts',(-0.281706971019057,2.25667569500715,
7.08931919253454));
#60006=CARTESIAN_POINT('Ctrl Pts',(-0.284903902327578,2.25078410558769,
7.08974074312677));
#60007=CARTESIAN_POINT('Ctrl Pts',(-0.288795207152222,2.24304665213507,
7.09029379543921));
#60008=CARTESIAN_POINT('Ctrl Pts',(-0.289659727893182,2.24128785558589,
7.09041946800069));
#60009=CARTESIAN_POINT('Ctrl Pts',(-0.291530681329827,2.23739219843099,
7.09069773826261));
#60010=CARTESIAN_POINT('Ctrl Pts',(-0.292529765694621,2.23525195040702,
7.09085056001177));
#60011=CARTESIAN_POINT('Ctrl Pts',(-0.305097009313708,2.20753951564825,
7.09282849154357));
#60012=CARTESIAN_POINT('Ctrl Pts',(-0.313298970645674,2.18057466656254,
7.09475910487376));
#60013=CARTESIAN_POINT('Ctrl Pts',(-0.319636665225482,2.14248482875779,
7.09733682916207));
#60014=CARTESIAN_POINT('Ctrl Pts',(-0.320856640142542,2.13199412749797,
7.09802995583749));
#60015=CARTESIAN_POINT('Ctrl Pts',(-0.321659466671179,2.11996525965469,
7.09879224077578));
#60016=CARTESIAN_POINT('Ctrl Pts',(-0.321748881939039,2.11846838571895,
7.0988865248788));
#60017=CARTESIAN_POINT('Ctrl Pts',(-0.321849314519228,2.11656383228518,
7.09900571040348));
#60018=CARTESIAN_POINT('Ctrl Pts',(-0.321870008559195,2.11615671349427,
7.09903114244822));
#60019=CARTESIAN_POINT('Ctrl Pts',(-0.32190188266075,2.1155052694972,7.09907176367977));
#60020=CARTESIAN_POINT('Ctrl Pts',(-0.321913557060609,2.11526097061979,
7.09908698058751));
#60021=CARTESIAN_POINT('Ctrl Pts',(-0.321935175041236,2.11479752745301,
7.0991158159427));
#60022=CARTESIAN_POINT('Ctrl Pts',(-0.321945172890431,2.11457838812704,
7.09912943730214));
#60023=CARTESIAN_POINT('Ctrl Pts',(-0.321967555510945,2.11407653726298,
7.09916060098398));
#60024=CARTESIAN_POINT('Ctrl Pts',(-0.321979791658115,2.11379381993052,
7.09917813482476));
#60025=CARTESIAN_POINT('Ctrl Pts',(-0.32201632914032,2.11292307091952,7.09923207043524));
#60026=CARTESIAN_POINT('Ctrl Pts',(-0.322039392263881,2.112334984322,7.0992684028843));
#60027=CARTESIAN_POINT('Ctrl Pts',(-0.322202278613281,2.10786915782674,
7.09954360923591));
#60028=CARTESIAN_POINT('Ctrl Pts',(-0.322273676964038,2.103989033816,7.09977873866915));
#60029=CARTESIAN_POINT('Ctrl Pts',(-0.322277943000648,2.0913013741075,7.10053731914127));
#60030=CARTESIAN_POINT('Ctrl Pts',(-0.321919891811834,2.08249722386882,
7.10104757242948));
#60031=CARTESIAN_POINT('Ctrl Pts',(-0.319211921990328,2.04940199492332,
7.10294069795412));
#60032=CARTESIAN_POINT('Ctrl Pts',(-0.314467639224258,2.02539044210436,
7.1042693866788));
#60033=CARTESIAN_POINT('Ctrl Pts',(-0.30567200480236,1.99779105241879,7.10593111732195));
#60034=CARTESIAN_POINT('Ctrl Pts',(-0.304192581746576,1.99346871691982,
7.10619522486907));
#60035=CARTESIAN_POINT('Ctrl Pts',(-0.299517386227723,1.98070199020298,
7.1069889409143));
#60036=CARTESIAN_POINT('Ctrl Pts',(-0.296058353421467,1.97235945827574,
7.10752575666223));
#60037=CARTESIAN_POINT('Ctrl Pts',(-0.291776683206179,1.96314670199933,
7.10814361298504));
#60038=CARTESIAN_POINT('Ctrl Pts',(-0.291294000854892,1.96212228950569,
7.10821266981727));
#60039=CARTESIAN_POINT('Ctrl Pts',(-0.290582974552082,1.96063365493668,
7.10831354542218));
#60040=CARTESIAN_POINT('Ctrl Pts',(-0.290358892421207,1.96016739713914,
7.10834521623515));
#60041=CARTESIAN_POINT('Ctrl Pts',(-0.28996104752605,1.95934466305481,7.10840123504849));
#60042=CARTESIAN_POINT('Ctrl Pts',(-0.289787747158715,1.95898796332222,
7.10842556691501));
#60043=CARTESIAN_POINT('Ctrl Pts',(-0.289427701710891,1.95825035777583,
7.10847597480966));
#60044=CARTESIAN_POINT('Ctrl Pts',(-0.289240862124544,1.95786949918107,
7.10850205409969));
#60045=CARTESIAN_POINT('Ctrl Pts',(-0.288759771102451,1.9568937082195,7.10856900405214));
#60046=CARTESIAN_POINT('Ctrl Pts',(-0.288464433838895,1.95629931609841,
7.10860991262841));
#60047=CARTESIAN_POINT('Ctrl Pts',(-0.287244703520973,1.95386341461201,
7.10877808621948));
#60048=CARTESIAN_POINT('Ctrl Pts',(-0.286304512078766,1.95202991067064,
7.10890590462081));
#60049=CARTESIAN_POINT('Ctrl Pts',(-0.279946029491782,1.93991749142864,
7.10975866922158));
#60050=CARTESIAN_POINT('Ctrl Pts',(-0.273993429947364,1.92993020715675,
7.11050260852844));
#60051=CARTESIAN_POINT('Ctrl Pts',(-0.248903020062674,1.89258139615628,
7.11344902178578));
#60052=CARTESIAN_POINT('Ctrl Pts',(-0.226103662915226,1.86793995548581,
7.11578066242824));
#60053=CARTESIAN_POINT('Ctrl Pts',(-0.199486445672673,1.8468860819622,7.11797424850297));
#60054=CARTESIAN_POINT('Ctrl Pts',(-0.199040537904893,1.8465352849186,7.1180108583174));
#60055=CARTESIAN_POINT('Ctrl Pts',(-0.195517071114537,1.8437783944682,7.11829903657008));
#60056=CARTESIAN_POINT('Ctrl Pts',(-0.192396748829027,1.84142712694815,
7.11854761752251));
#60057=CARTESIAN_POINT('Ctrl Pts',(-0.188756945138123,1.83878679392749,
7.11882933053229));
#60058=CARTESIAN_POINT('Ctrl Pts',(-0.188278660338053,1.83844184310379,
7.11886618752649));
#60059=CARTESIAN_POINT('Ctrl Pts',(-0.187569272479577,1.83793316910757,
7.11892061199511));
#60060=CARTESIAN_POINT('Ctrl Pts',(-0.187338899510602,1.83776843713208,
7.11893824872901));
#60061=CARTESIAN_POINT('Ctrl Pts',(-0.186929677403547,1.83747663063074,
7.11896951064209));
#60062=CARTESIAN_POINT('Ctrl Pts',(-0.18675091567227,1.83734943507416,7.11898314421709));
#60063=CARTESIAN_POINT('Ctrl Pts',(-0.186372702278239,1.83708090364854,
7.11901194131849));
#60064=CARTESIAN_POINT('Ctrl Pts',(-0.18617322020817,1.83693961252398,7.11902710173152));
#60065=CARTESIAN_POINT('Ctrl Pts',(-0.185641118671591,1.83656363881565,
7.11906746653094));
#60066=CARTESIAN_POINT('Ctrl Pts',(-0.185308213614012,1.8363293582759,7.11909264318052));
#60067=CARTESIAN_POINT('Ctrl Pts',(-0.183751792665983,1.83523843720898,
7.11920999506939));
#60068=CARTESIAN_POINT('Ctrl Pts',(-0.182522749359586,1.83438966020019,
7.11930163885746));
#60069=CARTESIAN_POINT('Ctrl Pts',(-0.172622625957208,1.82765380720749,
7.1200320548807));
#60070=CARTESIAN_POINT('Ctrl Pts',(-0.16367399107364,1.82218370598194,7.12064473475317));
#60071=CARTESIAN_POINT('Ctrl Pts',(-0.130445673127193,1.80403604933509,
7.12281205583066));
#60072=CARTESIAN_POINT('Ctrl Pts',(-0.104843479137785,1.79402826287495,
7.12429384654248));
#60073=CARTESIAN_POINT('Ctrl Pts',(-0.0670853146933372,1.78457331872525,
7.12654263421604));
#60074=CARTESIAN_POINT('Ctrl Pts',(-0.0557460321925753,1.78237323090294,
7.12722404940653));
#60075=CARTESIAN_POINT('Ctrl Pts',(-0.0431215920958387,1.78062067494908,
7.12799881170899));
#60076=CARTESIAN_POINT('Ctrl Pts',(-0.0419282327445183,1.78046182041535,
7.12807220085131));
#60077=CARTESIAN_POINT('Ctrl Pts',(-0.0402552827254262,1.78024865793598,
7.12817530636383));
#60078=CARTESIAN_POINT('Ctrl Pts',(-0.0397764072498257,1.78018873384238,
7.1282048454214));
#60079=CARTESIAN_POINT('Ctrl Pts',(-0.0388996485715129,1.78008102031784,
7.12825897495029));
#60080=CARTESIAN_POINT('Ctrl Pts',(-0.0385018067514579,1.78003289685589,
7.1282835548352));
#60081=CARTESIAN_POINT('Ctrl Pts',(-0.037697380447532,1.77993711443681,
7.12833329121868));
#60082=CARTESIAN_POINT('Ctrl Pts',(-0.0372907929166976,1.77988948788141,
7.12835844869064));
#60083=CARTESIAN_POINT('Ctrl Pts',(-0.0362931625080061,1.77977455466068,
7.1284202234262));
#60084=CARTESIAN_POINT('Ctrl Pts',(-0.0357020236072169,1.77970810970246,
7.12845686778367));
#60085=CARTESIAN_POINT('Ctrl Pts',(-0.0335647189203274,1.77947386368942,
7.12858950544548));
#60086=CARTESIAN_POINT('Ctrl Pts',(-0.032017546546237,1.7793156209114,7.12868579922816));
#60087=CARTESIAN_POINT('Ctrl Pts',(-0.0231794226756824,1.7784762656267,
7.12923751714671));
#60088=CARTESIAN_POINT('Ctrl Pts',(-0.0158685849866832,1.7780326549048,
7.12970035524123));
#60089=CARTESIAN_POINT('Ctrl Pts',(-0.00289208019701325,1.77768828797407,
7.13053411471465));
#60090=CARTESIAN_POINT('Ctrl Pts',(0.00276796796728354,1.77768720740032,
7.13090188141825));
#60091=CARTESIAN_POINT('Ctrl Pts',(0.0352027912077775,1.77853540294144,
7.13303191850251));
#60092=CARTESIAN_POINT('Ctrl Pts',(0.061784958986285,1.78257114794478,7.13487763144612));
#60093=CARTESIAN_POINT('Ctrl Pts',(0.0972662818958669,1.79258794082323,
7.13732734817175));
#60094=CARTESIAN_POINT('Ctrl Pts',(0.106840108412954,1.79578273889988,7.13798535614099));
#60095=CARTESIAN_POINT('Ctrl Pts',(0.116932834428128,1.79968612255806,7.13866458056378));
#60096=CARTESIAN_POINT('Ctrl Pts',(0.117615486753771,1.79995282029013,7.13871044896925));
#60097=CARTESIAN_POINT('Ctrl Pts',(0.118564030454495,1.80032713073458,7.138774075309));
#60098=CARTESIAN_POINT('Ctrl Pts',(0.118830690286628,1.8004327705857,7.13879195042558));
#60099=CARTESIAN_POINT('Ctrl Pts',(0.119289838085621,1.80061537593076,7.13882270775962));
#60100=CARTESIAN_POINT('Ctrl Pts',(0.119482392858993,1.80069217117353,7.13883560025157));
#60101=CARTESIAN_POINT('Ctrl Pts',(0.119881274915942,1.80085170071506,7.1388622940213));
#60102=CARTESIAN_POINT('Ctrl Pts',(0.120087590361259,1.80093446256378,7.13887609350972));
#60103=CARTESIAN_POINT('Ctrl Pts',(0.120574576572685,1.80113039851237,7.13890864851831));
#60104=CARTESIAN_POINT('Ctrl Pts',(0.12085517478159,1.80124375497848,7.13892739296166));
#60105=CARTESIAN_POINT('Ctrl Pts',(0.121778037864629,1.80161808746332,7.13898899854824));
#60106=CARTESIAN_POINT('Ctrl Pts',(0.122419625975329,1.80188074293622,7.13903175864886));
#60107=CARTESIAN_POINT('Ctrl Pts',(0.123927931981081,1.80250390852192,7.13913213174345));
#60108=CARTESIAN_POINT('Ctrl Pts',(0.124793937513339,1.8028661413107,7.13918964366859));
#60109=CARTESIAN_POINT('Ctrl Pts',(0.134494618900455,1.80697363391175,7.13983267776966));
#60110=CARTESIAN_POINT('Ctrl Pts',(0.143160325168732,1.81110830088701,7.14039601304263));
#60111=CARTESIAN_POINT('Ctrl Pts',(0.177722036964782,1.82953662072146,7.14264763419519));
#60112=CARTESIAN_POINT('Ctrl Pts',(0.201776009326334,1.84697392182734,7.14423964867464));
#60113=CARTESIAN_POINT('Ctrl Pts',(0.230604817933909,1.87463296325583,7.14655866757371));
#60114=CARTESIAN_POINT('Ctrl Pts',(0.237741562551963,1.88217484460242,7.14717337216882));
#60115=CARTESIAN_POINT('Ctrl Pts',(0.245265900505138,1.89093735371872,7.14787560113998));
#60116=CARTESIAN_POINT('Ctrl Pts',(0.246025331195607,1.89183158651262,7.14794712972961));
#60117=CARTESIAN_POINT('Ctrl Pts',(0.247117402617992,1.89313182844161,7.14805094794052));
#60118=CARTESIAN_POINT('Ctrl Pts',(0.247453966939947,1.89353454206306,7.14808307704597));
#60119=CARTESIAN_POINT('Ctrl Pts',(0.248043919009222,1.89424395965151,7.14813963125053));
#60120=CARTESIAN_POINT('Ctrl Pts',(0.248297726024389,1.89455031480625,7.14816403921836));
#60121=CARTESIAN_POINT('Ctrl Pts',(0.248813660907834,1.89517542119086,7.14821381385264));
#60122=CARTESIAN_POINT('Ctrl Pts',(0.249075745001279,1.89549420744576,7.14823918222942));
#60123=CARTESIAN_POINT('Ctrl Pts',(0.249728483834574,1.89629128305521,7.14830257444544));
#60124=CARTESIAN_POINT('Ctrl Pts',(0.250118376256505,1.89677019202898,7.14834062899051));
#60125=CARTESIAN_POINT('Ctrl Pts',(0.250960873299347,1.897811136724,7.14842327229059));
#60126=CARTESIAN_POINT('Ctrl Pts',(0.251412970754599,1.89837357692311,7.14846788120274));
#60127=CARTESIAN_POINT('Ctrl Pts',(0.25269068172186,1.89997411596522,7.14859470146078));
#60128=CARTESIAN_POINT('Ctrl Pts',(0.253511773554806,1.901015790834,7.14867709293906));
#60129=CARTESIAN_POINT('Ctrl Pts',(0.273077032596814,1.92615484604641,7.15066210033693));
#60130=CARTESIAN_POINT('Ctrl Pts',(0.288305116808705,1.95278424782804,7.15271337312039));
#60131=CARTESIAN_POINT('Ctrl Pts',(0.300805321201804,1.98429018158299,7.15500565593547));
#60132=CARTESIAN_POINT('Ctrl Pts',(0.302002508421689,1.9874518385644,7.1552340245765));
#60133=CARTESIAN_POINT('Ctrl Pts',(0.308290016881722,2.0048797202458,7.15648216933656));
#60134=CARTESIAN_POINT('Ctrl Pts',(0.312420146394423,2.01947436860702,7.15748931116751));
#60135=CARTESIAN_POINT('Ctrl Pts',(0.315694341713643,2.03519961990106,7.15849948684836));
#60136=CARTESIAN_POINT('Ctrl Pts',(0.315876379523323,2.03609288335539,7.15855661456581));
#60137=CARTESIAN_POINT('Ctrl Pts',(0.31611607956451,2.0372951465529,7.15863315070452));
#60138=CARTESIAN_POINT('Ctrl Pts',(0.316177081344159,2.03760346452093,7.15865274703949));
#60139=CARTESIAN_POINT('Ctrl Pts',(0.316279018192595,2.038122666324,7.15868569382008));
#60140=CARTESIAN_POINT('Ctrl Pts',(0.316320193447893,2.03833350188774,7.15869905800062));
#60141=CARTESIAN_POINT('Ctrl Pts',(0.316398753785029,2.03873791468038,7.15872466396509));
#60142=CARTESIAN_POINT('Ctrl Pts',(0.316436171767975,2.03893148363099,7.15873690753517));
#60143=CARTESIAN_POINT('Ctrl Pts',(0.316524305927,2.03938967104083,7.15876585918351));
#60144=CARTESIAN_POINT('Ctrl Pts',(0.316574867840449,2.03965431852916,7.15878255831355));
#60145=CARTESIAN_POINT('Ctrl Pts',(0.316722372208424,2.0404316625897,7.15883154093794));
#60146=CARTESIAN_POINT('Ctrl Pts',(0.316818402084771,2.04094453464202,7.15886377236693));
#60147=CARTESIAN_POINT('Ctrl Pts',(0.317528596811942,2.0447891026014,7.15910475479407));
#60148=CARTESIAN_POINT('Ctrl Pts',(0.318091466890424,2.04813022175631,7.15931064142299));
#60149=CARTESIAN_POINT('Ctrl Pts',(0.319823245807952,2.05950171179576,7.1600012918486));
#60150=CARTESIAN_POINT('Ctrl Pts',(0.320741611420546,2.06756761233605,7.16047420936283));
#60151=CARTESIAN_POINT('Ctrl Pts',(0.323881355451705,2.1090211348548,7.16285667348626));
#60152=CARTESIAN_POINT('Ctrl Pts',(0.321198429221979,2.1425710082323,7.16464967167782));
#60153=CARTESIAN_POINT('Ctrl Pts',(0.313318833953293,2.17544936214753,7.16665056897304));
#60154=CARTESIAN_POINT('Ctrl Pts',(0.313236765231017,2.17578935851811,7.1666712845979));
#60155=CARTESIAN_POINT('Ctrl Pts',(0.311800040832471,2.18169926013288,7.16703179500768));
#60156=CARTESIAN_POINT('Ctrl Pts',(0.310297640138955,2.18723189099882,7.16737590616462));
#60157=CARTESIAN_POINT('Ctrl Pts',(0.308365982052197,2.19366195326035,7.16778465049679));
#60158=CARTESIAN_POINT('Ctrl Pts',(0.30807909327924,2.19460133522471,7.16784458681572));
#60159=CARTESIAN_POINT('Ctrl Pts',(0.307639639309348,2.19601707204352,7.1679352570114));
#60160=CARTESIAN_POINT('Ctrl Pts',(0.307490250286527,2.19649441316712,7.16796588668877));
#60161=CARTESIAN_POINT('Ctrl Pts',(0.307221508568814,2.19734615925498,7.16802064635261));
#60162=CARTESIAN_POINT('Ctrl Pts',(0.307102580912326,2.19772069813407,7.16804476233239));
#60163=CARTESIAN_POINT('Ctrl Pts',(0.306852745720532,2.19850254364545,7.16809518079205));
#60164=CARTESIAN_POINT('Ctrl Pts',(0.30672171163757,2.19890980875607,7.16812148739707));
#60165=CARTESIAN_POINT('Ctrl Pts',(0.306389328207243,2.19993587263861,7.16818787464146));
#60166=CARTESIAN_POINT('Ctrl Pts',(0.306186915577639,2.2005543226244,7.16822799026202));
#60167=CARTESIAN_POINT('Ctrl Pts',(0.305733974676915,2.20192418623585,7.16831707287149));
#60168=CARTESIAN_POINT('Ctrl Pts',(0.305482547092245,2.20267529603392,7.16836606940177));
#60169=CARTESIAN_POINT('Ctrl Pts',(0.30474431457889,2.20485396154392,7.16850863330048));
#60170=CARTESIAN_POINT('Ctrl Pts',(0.304250258802843,2.20627902151181,7.16860244015751));
#60171=CARTESIAN_POINT('Ctrl Pts',(0.302540715828281,2.21110041995744,7.16892173382152));
#60172=CARTESIAN_POINT('Ctrl Pts',(0.301278250510866,2.21447970178233,7.16914876989356));
#60173=CARTESIAN_POINT('Ctrl Pts',(0.295638752613398,2.22883529978783,7.17012750251643));
#60174=CARTESIAN_POINT('Ctrl Pts',(0.290716989389823,2.23958647770634,7.17089697834695));
#60175=CARTESIAN_POINT('Ctrl Pts',(0.270049185383439,2.27887408868154,7.17384286216314));
#60176=CARTESIAN_POINT('Ctrl Pts',(0.250599239559919,2.30523748408877,7.1761193685785));
#60177=CARTESIAN_POINT('Ctrl Pts',(0.226488499113328,2.32927339904247,7.17827201546946));
#60178=CARTESIAN_POINT('Ctrl Pts',(0.225441494859509,2.33030298376181,7.17836435233834));
#60179=CARTESIAN_POINT('Ctrl Pts',(0.22408377294486,2.3316199847557,7.17848258713693));
#60180=CARTESIAN_POINT('Ctrl Pts',(0.223779497287755,2.33191397377896,7.17850898810828));
#60181=CARTESIAN_POINT('Ctrl Pts',(0.223295927562847,2.33237935768715,7.17855079198686));
#60182=CARTESIAN_POINT('Ctrl Pts',(0.223117014412688,2.33255114496775,7.17856622549574));
#60183=CARTESIAN_POINT('Ctrl Pts',(0.222795758114769,2.33285889404903,7.17859387799154));
#60184=CARTESIAN_POINT('Ctrl Pts',(0.222653489772382,2.33299493098383,7.17860610286065));
#60185=CARTESIAN_POINT('Ctrl Pts',(0.222318309545093,2.33331484284125,7.17863485494019));
#60186=CARTESIAN_POINT('Ctrl Pts',(0.222125294429452,2.33349860861445,7.17865137358169));
#60187=CARTESIAN_POINT('Ctrl Pts',(0.221563812790055,2.33403185764265,7.17869931577494));
#60188=CARTESIAN_POINT('Ctrl Pts',(0.221194745726188,2.33438071166631,7.17873069057425));
#60189=CARTESIAN_POINT('Ctrl Pts',(0.218603498120495,2.33681847016637,7.1789500236647));
#60190=CARTESIAN_POINT('Ctrl Pts',(0.216352492677694,2.33887669989179,7.17913566870703));
#60191=CARTESIAN_POINT('Ctrl Pts',(0.209329151504021,2.3451178252093,7.17970129097684));
#60192=CARTESIAN_POINT('Ctrl Pts',(0.204462004820493,2.34919217784713,7.18007439744852));
#60193=CARTESIAN_POINT('Ctrl Pts',(0.188122383355537,2.36206899489701,7.1812785256904));
#60194=CARTESIAN_POINT('Ctrl Pts',(0.176177346588848,2.37024393572151,7.18208447508553));
#60195=CARTESIAN_POINT('Ctrl Pts',(0.147385652487123,2.38722535685445,7.18395283498972));
#60196=CARTESIAN_POINT('Ctrl Pts',(0.130231043386789,2.39539926367027,7.18501474082521));
#60197=CARTESIAN_POINT('Ctrl Pts',(0.11085954001258,2.40261237200339,7.18622681780977));
#60198=CARTESIAN_POINT('Ctrl Pts',(0.10925630645183,2.40319489549231,7.18632720113826));
#60199=CARTESIAN_POINT('Ctrl Pts',(0.101584536312963,2.40591362813335,7.18680802332566));
#60200=CARTESIAN_POINT('Ctrl Pts',(0.0954578942667162,2.40788041106997,
7.18719344223938));
#60201=CARTESIAN_POINT('Ctrl Pts',(0.0882872019016843,2.40994774773028,
7.18764765319786));
#60202=CARTESIAN_POINT('Ctrl Pts',(0.0872962442046343,2.41022830633561,
7.1877104901779));
#60203=CARTESIAN_POINT('Ctrl Pts',(0.0858192992364137,2.41063882010222,
7.18780424925866));
#60204=CARTESIAN_POINT('Ctrl Pts',(0.0853343182806539,2.41077239709307,
7.18783505358634));
#60205=CARTESIAN_POINT('Ctrl Pts',(0.084469598281967,2.41100838779882,7.18789000844686));
#60206=CARTESIAN_POINT('Ctrl Pts',(0.0840899799342798,2.41111124310705,
7.1879141445922));
#60207=CARTESIAN_POINT('Ctrl Pts',(0.0833560756061799,2.4113086486802,7.18796082702655));
#60208=CARTESIAN_POINT('Ctrl Pts',(0.0830018145008967,2.41140328975678,
7.1879833703278));
#60209=CARTESIAN_POINT('Ctrl Pts',(0.082035653744319,2.41165963439264,7.18804487754866));
#60210=CARTESIAN_POINT('Ctrl Pts',(0.0814234403976755,2.41182013972752,
7.18808388021184));
#60211=CARTESIAN_POINT('Ctrl Pts',(0.0790414342392191,2.41243714225304,
7.18823574482878));
#60212=CARTESIAN_POINT('Ctrl Pts',(0.0772682701159036,2.41288037713807,
7.18834903447287));
#60213=CARTESIAN_POINT('Ctrl Pts',(0.0728376085493974,2.41394794190226,
7.18863275465341));
#60214=CARTESIAN_POINT('Ctrl Pts',(0.0701758074652522,2.41455362460552,
7.18880377672876));
#60215=CARTESIAN_POINT('Ctrl Pts',(0.0596396439274277,2.41681069938714,
7.18948312548077));
#60216=CARTESIAN_POINT('Ctrl Pts',(0.0517128472239275,2.41820067527034,
7.18999958319172));
#60217=CARTESIAN_POINT('Ctrl Pts',(0.032605481168604,2.42081837204902,7.19125731425797));
#60218=CARTESIAN_POINT('Ctrl Pts',(0.021396757741781,2.42176029519217,7.19200570697803));
#60219=CARTESIAN_POINT('Ctrl Pts',(-0.0164326227418953,2.42295379152613,
7.19455264444582));
#60220=CARTESIAN_POINT('Ctrl Pts',(-0.0430306160610507,2.42049607370513,
7.19638649478743));
#60221=CARTESIAN_POINT('Ctrl Pts',(-0.0703810063063582,2.41449899351517,
7.19815564912526));
#60222=CARTESIAN_POINT('Ctrl Pts',(-0.0717351724495111,2.41419288370309,
7.19824290998145));
#60223=CARTESIAN_POINT('Ctrl Pts',(-0.0734905773858463,2.41378413291825,
7.19835555540831));
#60224=CARTESIAN_POINT('Ctrl Pts',(-0.0738936292391306,2.41368946204519,
7.19838138719749));
#60225=CARTESIAN_POINT('Ctrl Pts',(-0.0745119826531165,2.41354296213611,
7.19842096697865));
#60226=CARTESIAN_POINT('Ctrl Pts',(-0.0747274131820014,2.41349168790226,
7.19843474686019));
#60227=CARTESIAN_POINT('Ctrl Pts',(-0.0751548315140514,2.41338949321313,
7.19846206737511));
#60228=CARTESIAN_POINT('Ctrl Pts',(-0.0753668191636071,2.41333858001526,
7.19847560825721));
#60229=CARTESIAN_POINT('Ctrl Pts',(-0.0758389769710143,2.41322467471814,
7.19850574701212));
#60230=CARTESIAN_POINT('Ctrl Pts',(-0.0760991197051235,2.41316157373096,
7.19852233845807));
#60231=CARTESIAN_POINT('Ctrl Pts',(-0.0768580096499789,2.41297649369226,
7.19857069914261));
#60232=CARTESIAN_POINT('Ctrl Pts',(-0.0773565472843937,2.41285364605851,
7.19860241830899));
#60233=CARTESIAN_POINT('Ctrl Pts',(-0.0809409877734502,2.41196129091386,
7.19883012729805));
#60234=CARTESIAN_POINT('Ctrl Pts',(-0.0840157813233215,2.41114729770155,
7.19902359793514));
#60235=CARTESIAN_POINT('Ctrl Pts',(-0.0914916249952602,2.40904930179883,
7.19949055579906));
#60236=CARTESIAN_POINT('Ctrl Pts',(-0.0958783945567755,2.40771663296007,
7.19976163194437));
#60237=CARTESIAN_POINT('Ctrl Pts',(-0.114111452681419,2.40174975711589,
7.20088171396187));
#60238=CARTESIAN_POINT('Ctrl Pts',(-0.127663939002439,2.39627069405924,
7.20169867588525));
#60239=CARTESIAN_POINT('Ctrl Pts',(-0.154204702977334,2.38337994355875,
7.20334821530274));
#60240=CARTESIAN_POINT('Ctrl Pts',(-0.167142213809476,2.37594697780071,
7.20417905263917));
#60241=CARTESIAN_POINT('Ctrl Pts',(-0.183300197286749,2.36510931582671,
7.2052954717734));
#60242=CARTESIAN_POINT('Ctrl Pts',(-0.187027678167634,2.36249296534632,
7.20555881678487));
#60243=CARTESIAN_POINT('Ctrl Pts',(-0.197927452028649,2.3544922710342,7.20634836907675));
#60244=CARTESIAN_POINT('Ctrl Pts',(-0.204931320866296,2.34888696867695,
7.2068816840926));
#60245=CARTESIAN_POINT('Ctrl Pts',(-0.212459121869228,2.34232897561804,
7.2074888831766));
#60246=CARTESIAN_POINT('Ctrl Pts',(-0.213223131211375,2.34165700314452,
7.20755091396228));
#60247=CARTESIAN_POINT('Ctrl Pts',(-0.214365411281454,2.34064269432955,
7.20764427345308));
#60248=CARTESIAN_POINT('Ctrl Pts',(-0.214746077159248,2.34030305497026,
7.20767548924522));
#60249=CARTESIAN_POINT('Ctrl Pts',(-0.215402343392353,2.33971471355354,
7.20772948536364));
#60250=CARTESIAN_POINT('Ctrl Pts',(-0.215678324238804,2.33946643582065,
7.20775224780742));
#60251=CARTESIAN_POINT('Ctrl Pts',(-0.216232205412781,2.33896641933254,
7.20779804278728));
#60252=CARTESIAN_POINT('Ctrl Pts',(-0.216510096595333,2.33871467130599,
7.20782107569694));
#60253=CARTESIAN_POINT('Ctrl Pts',(-0.217073276123506,2.33820268162525,
7.2078678704868));
#60254=CARTESIAN_POINT('Ctrl Pts',(-0.217358537272114,2.3379424111278,7.20789163356988));
#60255=CARTESIAN_POINT('Ctrl Pts',(-0.218260045614617,2.33711690653498,
7.20796692462412));
#60256=CARTESIAN_POINT('Ctrl Pts',(-0.218874557278458,2.3365497897515,7.2080185327248));
#60257=CARTESIAN_POINT('Ctrl Pts',(-0.222667778699551,2.33302168910037,
7.20833888492995));
#60258=CARTESIAN_POINT('Ctrl Pts',(-0.225788427638567,2.32999919615949,
7.20861026591442));
#60259=CARTESIAN_POINT('Ctrl Pts',(-0.234845730527272,2.32086476756189,
7.20942202879155));
#60260=CARTESIAN_POINT('Ctrl Pts',(-0.240601795031474,2.31457986302706,
7.20996998163263));
#60261=CARTESIAN_POINT('Ctrl Pts',(-0.24966590761539,2.303859226455,7.21088781990901));
#60262=CARTESIAN_POINT('Ctrl Pts',(-0.253121022527009,2.29955298261628,
7.21125231329694));
#60263=CARTESIAN_POINT('Ctrl Pts',(-0.27552916716822,2.27010602979294,7.21371474962178));
#60264=CARTESIAN_POINT('Ctrl Pts',(-0.290819687747357,2.24239475184208,
7.21590979668551));
#60265=CARTESIAN_POINT('Ctrl Pts',(-0.302391678940644,2.21145780564612,
7.21799977192156));
#60266=CARTESIAN_POINT('Ctrl Pts',(-0.302923353477104,2.21000460025734,
7.21809711887514));
#60267=CARTESIAN_POINT('Ctrl Pts',(-0.303588233500547,2.20814592955057,
7.21822052514394));
#60268=CARTESIAN_POINT('Ctrl Pts',(-0.303731117227819,2.207743983734,7.21824714682433));
#60269=CARTESIAN_POINT('Ctrl Pts',(-0.303956903541944,2.20710480644401,
7.21828937549967));
#60270=CARTESIAN_POINT('Ctrl Pts',(-0.304040326829884,2.20686776144576,
7.21830501342331));
#60271=CARTESIAN_POINT('Ctrl Pts',(-0.304195705405711,2.20642460287695,
7.21833420545718));
#60272=CARTESIAN_POINT('Ctrl Pts',(-0.304267727977743,2.20621851531857,
7.21834776349157));
#60273=CARTESIAN_POINT('Ctrl Pts',(-0.304429143692553,2.20575512418161,
7.21837820976048));
#60274=CARTESIAN_POINT('Ctrl Pts',(-0.304518419857189,2.20549778096738,
7.21839509093392));
#60275=CARTESIAN_POINT('Ctrl Pts',(-0.304782404824621,2.20473370343698,
7.21844513330403));
#60276=CARTESIAN_POINT('Ctrl Pts',(-0.30495617691483,2.2042266429354,7.21847823895089));
#60277=CARTESIAN_POINT('Ctrl Pts',(-0.306346400221008,2.2001367808294,7.21874444627241));
#60278=CARTESIAN_POINT('Ctrl Pts',(-0.30750099835517,2.196533055817,7.21897396368596));
#60279=CARTESIAN_POINT('Ctrl Pts',(-0.311460670305453,2.18338132334846,
7.21979619343975));
#60280=CARTESIAN_POINT('Ctrl Pts',(-0.313886840694076,2.17372435827734,
7.22037084623118));
#60281=CARTESIAN_POINT('Ctrl Pts',(-0.320111158949036,2.14299066923983,
7.22215240170525));
#60282=CARTESIAN_POINT('Ctrl Pts',(-0.322259181944044,2.12164123795382,
7.22332463650292));
#60283=CARTESIAN_POINT('Ctrl Pts',(-0.322274912962847,2.10023685394134,
7.22454439956175));
#60284=CARTESIAN_POINT('',(-0.321882949708748,2.09979413277033,7.34972265507269));
#60285=CARTESIAN_POINT('Ctrl Pts',(-0.3219654526091,2.10024677492677,7.22472265507269));
#60286=CARTESIAN_POINT('Ctrl Pts',(-0.321458228780833,2.02894014117497,
7.22911504031661));
#60287=CARTESIAN_POINT('Ctrl Pts',(-0.262891613614646,1.84935084621839,
7.24013087340147));
#60288=CARTESIAN_POINT('Ctrl Pts',(0.034383760505689,1.72048342076356,7.25777015432727));
#60289=CARTESIAN_POINT('Ctrl Pts',(0.337716885669452,1.92347129968311,7.27764049785004));
#60290=CARTESIAN_POINT('Ctrl Pts',(0.331240744233873,2.28840022893095,7.29751084137284));
#60291=CARTESIAN_POINT('Ctrl Pts',(0.0208963143190576,2.48049759650978,
7.31738118489562));
#60292=CARTESIAN_POINT('Ctrl Pts',(-0.267716732443814,2.34302254774173,
7.33478512279558));
#60293=CARTESIAN_POINT('Ctrl Pts',(-0.32148895242199,2.1673236380514,7.3455656128546));
#60294=CARTESIAN_POINT('Ctrl Pts',(-0.321882949708748,2.09979413277033,
7.34972265507269));
#60295=CARTESIAN_POINT('',(-0.322274866683432,2.10029313678766,7.59976792125168));
#60296=CARTESIAN_POINT('Ctrl Pts',(-0.32227492433765,2.09977916485371,7.34949702710362));
#60297=CARTESIAN_POINT('Ctrl Pts',(-0.322261526895343,2.08022765877105,
7.35077232927699));
#60298=CARTESIAN_POINT('Ctrl Pts',(-0.320468946951427,2.0607191748254,7.35209519898572));
#60299=CARTESIAN_POINT('Ctrl Pts',(-0.313453942902018,2.02271891291142,
7.35470899680524));
#60300=CARTESIAN_POINT('Ctrl Pts',(-0.308325470672367,2.0042851036715,7.35599397997341));
#60301=CARTESIAN_POINT('Ctrl Pts',(-0.301330739653725,1.98571299797414,
7.35723962346725));
#60302=CARTESIAN_POINT('Ctrl Pts',(-0.301065055575812,1.98501493214401,
7.35728636570966));
#60303=CARTESIAN_POINT('Ctrl Pts',(-0.300684958015297,1.98402660228161,
7.35735242747226));
#60304=CARTESIAN_POINT('Ctrl Pts',(-0.300572548783337,1.98373557777692,
7.35737186572807));
#60305=CARTESIAN_POINT('Ctrl Pts',(-0.300378713467072,1.98323590327112,
7.35740521500175));
#60306=CARTESIAN_POINT('Ctrl Pts',(-0.300297492295101,1.98302717447438,
7.35741913839949));
#60307=CARTESIAN_POINT('Ctrl Pts',(-0.300141482836316,1.98262748206851,
7.35744578541107));
#60308=CARTESIAN_POINT('Ctrl Pts',(-0.300066729973869,1.98243650546134,
7.35745851115518));
#60309=CARTESIAN_POINT('Ctrl Pts',(-0.299890118738951,1.9819865696529,7.35748847778705));
#60310=CARTESIAN_POINT('Ctrl Pts',(-0.299788106970629,1.98172767026954,
7.35750570937793));
#60311=CARTESIAN_POINT('Ctrl Pts',(-0.299485520503827,1.98096263175371,
7.3575565946343));
#60312=CARTESIAN_POINT('Ctrl Pts',(-0.299283997157887,1.98045686516639,
7.3575901914773));
#60313=CARTESIAN_POINT('Ctrl Pts',(-0.297495480792886,1.97600106535583,
7.35788581698478));
#60314=CARTESIAN_POINT('Ctrl Pts',(-0.295831558408913,1.97208209588234,
7.35814331137904));
#60315=CARTESIAN_POINT('Ctrl Pts',(-0.29397869153214,1.96794781665378,7.35841343419876));
#60316=CARTESIAN_POINT('Ctrl Pts',(-0.293866688269368,1.96769875386821,
7.35842970137416));
#60317=CARTESIAN_POINT('Ctrl Pts',(-0.293703563278234,1.96733724033889,
7.35845330491927));
#60318=CARTESIAN_POINT('Ctrl Pts',(-0.293652693554999,1.96722467679861,
7.35846065314043));
#60319=CARTESIAN_POINT('Ctrl Pts',(-0.293200061794657,1.96622463448198,
7.35852592653383));
#60320=CARTESIAN_POINT('Ctrl Pts',(-0.292794337953979,1.96533894267379,
7.35858366605395));
#60321=CARTESIAN_POINT('Ctrl Pts',(-0.292167466632221,1.96398671538254,
7.35867173229371));
#60322=CARTESIAN_POINT('Ctrl Pts',(-0.291949207105771,1.96351885614851,
7.35870218639288));
#60323=CARTESIAN_POINT('Ctrl Pts',(-0.290771418524515,1.96100991222749,
7.35886542374839));
#60324=CARTESIAN_POINT('Ctrl Pts',(-0.289791587259936,1.95897837493863,
7.35899732995153));
#60325=CARTESIAN_POINT('Ctrl Pts',(-0.276973670951746,1.93310015156548,
7.36067617644098));
#60326=CARTESIAN_POINT('Ctrl Pts',(-0.262245586195704,1.91079782598986,
7.36211581844594));
#60327=CARTESIAN_POINT('Ctrl Pts',(-0.24084272486558,1.88576713348248,7.36399246416441));
#60328=CARTESIAN_POINT('Ctrl Pts',(-0.236605073266455,1.88109597406637,
7.36435522998365));
#60329=CARTESIAN_POINT('Ctrl Pts',(-0.227816800433414,1.87196216183603,
7.36509426499083));
#60330=CARTESIAN_POINT('Ctrl Pts',(-0.223265442835,1.86750422730543,7.36547046707366));
#60331=CARTESIAN_POINT('Ctrl Pts',(-0.216897506407837,1.86162650673583,
7.36599019398776));
#60332=CARTESIAN_POINT('Ctrl Pts',(-0.215193244512747,1.86008685388274,
7.36612866865216));
#60333=CARTESIAN_POINT('Ctrl Pts',(-0.212279073396333,1.85751018737441,
7.36636449914988));
#60334=CARTESIAN_POINT('Ctrl Pts',(-0.211077649320833,1.85646367818252,
7.3664614568349));
#60335=CARTESIAN_POINT('Ctrl Pts',(-0.209413159194657,1.85503538126217,
7.36659543929197));
#60336=CARTESIAN_POINT('Ctrl Pts',(-0.208956699348618,1.85464590187465,
7.36663214642671));
#60337=CARTESIAN_POINT('Ctrl Pts',(-0.208219933323152,1.85402079542729,
7.36669133923831));
#60338=CARTESIAN_POINT('Ctrl Pts',(-0.207940307135927,1.85378436608983,
7.36671379194235));
#60339=CARTESIAN_POINT('Ctrl Pts',(-0.207356961395593,1.85329283855796,
7.3667606055309));
#60340=CARTESIAN_POINT('Ctrl Pts',(-0.207053172801086,1.8530378235908,7.36678496976293));
#60341=CARTESIAN_POINT('Ctrl Pts',(-0.206351776221203,1.85245124095413,
7.36684118892952));
#60342=CARTESIAN_POINT('Ctrl Pts',(-0.205953839282455,1.85212006992372,
7.3668730599499));
#60343=CARTESIAN_POINT('Ctrl Pts',(-0.204681255525725,1.85106618029524,
7.36697490402675));
#60344=CARTESIAN_POINT('Ctrl Pts',(-0.203803596628387,1.85034712718464,
7.36704502546367));
#60345=CARTESIAN_POINT('Ctrl Pts',(-0.195856494145233,1.8439060166101,7.36767895228184));
#60346=CARTESIAN_POINT('Ctrl Pts',(-0.188552215527339,1.83848149261084,
7.36825457976716));
#60347=CARTESIAN_POINT('Ctrl Pts',(-0.167723009508977,1.82433928251443,
7.36987952474492));
#60348=CARTESIAN_POINT('Ctrl Pts',(-0.153761059997696,1.81631485004823,
7.37095176845409));
#60349=CARTESIAN_POINT('Ctrl Pts',(-0.127699142116004,1.80382699188026,
7.37290251104633));
#60350=CARTESIAN_POINT('Ctrl Pts',(-0.115817745704351,1.79898209588476,
7.37377406913718));
#60351=CARTESIAN_POINT('Ctrl Pts',(-0.0952859930722547,1.79200595013497,
7.37522549140947));
#60352=CARTESIAN_POINT('Ctrl Pts',(-0.0867779253147608,1.78950141303003,
7.37581163260688));
#60353=CARTESIAN_POINT('Ctrl Pts',(-0.0744120500520206,1.78640937235369,
7.37663215051821));
#60354=CARTESIAN_POINT('Ctrl Pts',(-0.0706304143673872,1.78553603885967,
7.37687892080602));
#60355=CARTESIAN_POINT('Ctrl Pts',(-0.066306250351506,1.78461936089861,
7.37715567121209));
#60356=CARTESIAN_POINT('Ctrl Pts',(-0.0657784934869911,1.78450886516372,
7.37718935655519));
#60357=CARTESIAN_POINT('Ctrl Pts',(-0.0649830671551264,1.78434441053295,
7.37723998608531));
#60358=CARTESIAN_POINT('Ctrl Pts',(-0.0647156057062469,1.78428946714106,
7.37725698632624));
#60359=CARTESIAN_POINT('Ctrl Pts',(-0.0642341231477217,1.7841911959269,
7.3772875466632));
#60360=CARTESIAN_POINT('Ctrl Pts',(-0.0640201282999115,1.78414774580501,
7.37730111375834));
#60361=CARTESIAN_POINT('Ctrl Pts',(-0.0635602291084476,1.78405485315791,
7.37733023775003));
#60362=CARTESIAN_POINT('Ctrl Pts',(-0.0633143119057035,1.78400548035397,
7.37734579057241));
#60363=CARTESIAN_POINT('Ctrl Pts',(-0.0626519814308786,1.78387330846248,
7.37738762491545));
#60364=CARTESIAN_POINT('Ctrl Pts',(-0.0622354599460625,1.78379104470323,
7.37741387575172));
#60365=CARTESIAN_POINT('Ctrl Pts',(-0.0603190239079019,1.78341647839241,
7.37753439723656));
#60366=CARTESIAN_POINT('Ctrl Pts',(-0.0588171728557488,1.78313401698438,
7.37762811434973));
#60367=CARTESIAN_POINT('Ctrl Pts',(-0.0288296998344187,1.77771466201601,
7.37948581521866));
#60368=CARTESIAN_POINT('Ctrl Pts',(0.000222891550511969,1.77642687310158,
7.3810505465331));
#60369=CARTESIAN_POINT('Ctrl Pts',(0.0425923321829934,1.78026312012273,
7.3834449487952));
#60370=CARTESIAN_POINT('Ctrl Pts',(0.0560316428543165,1.78234266440841,
7.38421986580922));
#60371=CARTESIAN_POINT('Ctrl Pts',(0.0739291284730726,1.78628334695308,
7.38529947857499));
#60372=CARTESIAN_POINT('Ctrl Pts',(0.0785361515495423,1.78740485622242,
7.38558165384037));
#60373=CARTESIAN_POINT('Ctrl Pts',(0.0849010629692599,1.78910388170572,
7.38597822965838));
#60374=CARTESIAN_POINT('Ctrl Pts',(0.0866813775760356,1.78959554541157,
7.38608989283481));
#60375=CARTESIAN_POINT('Ctrl Pts',(0.0897453161601677,1.79047011792881,
7.38628338747504));
#60376=CARTESIAN_POINT('Ctrl Pts',(0.0910309725165503,1.79084578019089,
7.38636498328308));
#60377=CARTESIAN_POINT('Ctrl Pts',(0.0928494995379397,1.79138947169846,
7.38648098400849));
#60378=CARTESIAN_POINT('Ctrl Pts',(0.0933843446142382,1.79155089249964,
7.38651517287877));
#60379=CARTESIAN_POINT('Ctrl Pts',(0.0942704159147848,1.79182083223603,
7.38657193363579));
#60380=CARTESIAN_POINT('Ctrl Pts',(0.0946218825030613,1.79192856330026,
7.38659447968531));
#60381=CARTESIAN_POINT('Ctrl Pts',(0.0953548527065584,1.79215460498317,
7.38664156467746));
#60382=CARTESIAN_POINT('Ctrl Pts',(0.0957363220272728,1.79227302391541,
7.38666610713915));
#60383=CARTESIAN_POINT('Ctrl Pts',(0.0965733761510479,1.79253457643338,
7.38672004300031));
#60384=CARTESIAN_POINT('Ctrl Pts',(0.097028864352117,1.79267801388635,7.3867494463382));
#60385=CARTESIAN_POINT('Ctrl Pts',(0.0986022926192273,1.79317734769137,
7.38685120380645));
#60386=CARTESIAN_POINT('Ctrl Pts',(0.0997185968205904,1.79353833278979,
7.38692372514454));
#60387=CARTESIAN_POINT('Ctrl Pts',(0.12516221009088,1.80191990226256,7.38858426778419));
#60388=CARTESIAN_POINT('Ctrl Pts',(0.148443742406816,1.8128045452929,7.39027366115344));
#60389=CARTESIAN_POINT('Ctrl Pts',(0.183464851425994,1.83458278099478,7.39305887087783));
#60390=CARTESIAN_POINT('Ctrl Pts',(0.196124457419223,1.84379524243491,7.39412327804836));
#60391=CARTESIAN_POINT('Ctrl Pts',(0.214491405840648,1.85932300563061,7.39571576287857));
#60392=CARTESIAN_POINT('Ctrl Pts',(0.22070265019479,1.8650056453983,7.39626363823343));
#60393=CARTESIAN_POINT('Ctrl Pts',(0.227618231980305,1.87184908418765,7.39687779162366));
#60394=CARTESIAN_POINT('Ctrl Pts',(0.228545970845989,1.8727784357365,7.39696027073779));
#60395=CARTESIAN_POINT('Ctrl Pts',(0.229740926924612,1.87399019228399,7.39706659086489));
#60396=CARTESIAN_POINT('Ctrl Pts',(0.230013332592185,1.87426742919633,7.39709083365577));
#60397=CARTESIAN_POINT('Ctrl Pts',(0.230453363141809,1.87471688745468,7.39713000252832));
#60398=CARTESIAN_POINT('Ctrl Pts',(0.230621297046185,1.87488880363003,7.39714495295291));
#60399=CARTESIAN_POINT('Ctrl Pts',(0.230942943047865,1.87521881461686,7.39717359116464));
#60400=CARTESIAN_POINT('Ctrl Pts',(0.231096684701733,1.87537687882599,7.39718728125961));
#60401=CARTESIAN_POINT('Ctrl Pts',(0.231449791351423,1.87574065956226,7.39721872772094));
#60402=CARTESIAN_POINT('Ctrl Pts',(0.231649044939236,1.87594648480675,7.39723647529021));
#60403=CARTESIAN_POINT('Ctrl Pts',(0.232264966565486,1.87658442028152,7.39729134510506));
#60404=CARTESIAN_POINT('Ctrl Pts',(0.232680704992113,1.87701743231214,7.39732839497164));
#60405=CARTESIAN_POINT('Ctrl Pts',(0.236093581268659,1.88059204900149,7.39763268164981));
#60406=CARTESIAN_POINT('Ctrl Pts',(0.239028335869683,1.88379295285257,7.39789521493852));
#60407=CARTESIAN_POINT('Ctrl Pts',(0.24260398846304,1.88785471245867,7.39821766138594));
#60408=CARTESIAN_POINT('Ctrl Pts',(0.243306313639451,1.88866056675538,7.39828112420555));
#60409=CARTESIAN_POINT('Ctrl Pts',(0.245074101451898,1.89070943493942,7.39844123404827));
#60410=CARTESIAN_POINT('Ctrl Pts',(0.246134136028889,1.8919571123703,7.3985375876602));
#60411=CARTESIAN_POINT('Ctrl Pts',(0.264412197142547,1.91380593389285,7.40020614956665));
#60412=CARTESIAN_POINT('Ctrl Pts',(0.279000303184931,1.93647274494139,7.40165739095483));
#60413=CARTESIAN_POINT('Ctrl Pts',(0.297124752025477,1.97428097870768,7.40403862586409));
#60414=CARTESIAN_POINT('Ctrl Pts',(0.302678281025226,1.98831221643822,7.40491322212158));
#60415=CARTESIAN_POINT('Ctrl Pts',(0.307710577184216,2.00419856029788,7.40591861884607));
#60416=CARTESIAN_POINT('Ctrl Pts',(0.308180528578827,2.0057212811669,7.40601512261245));
#60417=CARTESIAN_POINT('Ctrl Pts',(0.308876459743618,2.00803702886921,7.40616211532462));
#60418=CARTESIAN_POINT('Ctrl Pts',(0.309110725779828,2.00882755552749,7.40621233470371));
#60419=CARTESIAN_POINT('Ctrl Pts',(0.309536888972073,2.01028615972665,7.40630507303871));
#60420=CARTESIAN_POINT('Ctrl Pts',(0.309729663776775,2.01095397742793,7.40634756318936));
#60421=CARTESIAN_POINT('Ctrl Pts',(0.310037633506612,2.01203395780428,7.40641632791855));
#60422=CARTESIAN_POINT('Ctrl Pts',(0.310154171274403,2.0124457379207,7.40644255871901));
#60423=CARTESIAN_POINT('Ctrl Pts',(0.310376138366452,2.01323605149106,7.4064929256906));
#60424=CARTESIAN_POINT('Ctrl Pts',(0.31048169633051,2.01361454827525,7.40651705762646));
#60425=CARTESIAN_POINT('Ctrl Pts',(0.310719982902284,2.01447504579175,7.40657194422518));
#60426=CARTESIAN_POINT('Ctrl Pts',(0.310852282445289,2.01495716337526,7.40660271276375));
#60427=CARTESIAN_POINT('Ctrl Pts',(0.311240896900857,2.01638635062781,7.406693973734));
#60428=CARTESIAN_POINT('Ctrl Pts',(0.311494007582491,2.01733427874208,7.40675456991313));
#60429=CARTESIAN_POINT('Ctrl Pts',(0.313191139698531,2.02380870742002,7.40716891497506));
#60430=CARTESIAN_POINT('Ctrl Pts',(0.314492261299111,2.02937129556919,7.40752725518391));
#60431=CARTESIAN_POINT('Ctrl Pts',(0.322073452769963,2.06616645044225,7.40991501907185));
#60432=CARTESIAN_POINT('Ctrl Pts',(0.323839053401613,2.09814453984804,7.41209741555548));
#60433=CARTESIAN_POINT('Ctrl Pts',(0.319774007427222,2.14184258940461,7.41504018461208));
#60434=CARTESIAN_POINT('Ctrl Pts',(0.317987028940872,2.15376369778721,7.41583561941497));
#60435=CARTESIAN_POINT('Ctrl Pts',(0.315208850233183,2.16713532403285,7.41670001334998));
#60436=CARTESIAN_POINT('Ctrl Pts',(0.314869302333308,2.16871021542138,7.4168013714739));
#60437=CARTESIAN_POINT('Ctrl Pts',(0.314426803136517,2.17069042209416,7.41692819173013));
#60438=CARTESIAN_POINT('Ctrl Pts',(0.314334861747314,2.17109813641367,7.41695426999124));
#60439=CARTESIAN_POINT('Ctrl Pts',(0.314187348941903,2.1717464029843,7.41699568009487));
#60440=CARTESIAN_POINT('Ctrl Pts',(0.314132294206982,2.17198707046107,7.41701104156667));
#60441=CARTESIAN_POINT('Ctrl Pts',(0.314027899205345,2.17244102477784,7.41703999400814));
#60442=CARTESIAN_POINT('Ctrl Pts',(0.313978618571107,2.17265432286305,7.41705358824294));
#60443=CARTESIAN_POINT('Ctrl Pts',(0.313866032424949,2.17313936811134,7.41708448032186));
#60444=CARTESIAN_POINT('Ctrl Pts',(0.313802591432197,2.17341108288094,7.41710177021502));
#60445=CARTESIAN_POINT('Ctrl Pts',(0.313608795213759,2.17423626137171,7.41715423264765));
#60446=CARTESIAN_POINT('Ctrl Pts',(0.313477327155475,2.17478946656445,7.4171893412582));
#60447=CARTESIAN_POINT('Ctrl Pts',(0.312535906159033,2.17870478227281,7.41743739826131));
#60448=CARTESIAN_POINT('Ctrl Pts',(0.311673307312672,2.18205417262405,7.41764738195327));
#60449=CARTESIAN_POINT('Ctrl Pts',(0.303264346761115,2.21265690653161,7.41955097657269));
#60450=CARTESIAN_POINT('Ctrl Pts',(0.292214438948206,2.23882383662416,7.42107755472311));
#60451=CARTESIAN_POINT('Ctrl Pts',(0.26923611032039,2.27794655281542,7.42363947516003));
#60452=CARTESIAN_POINT('Ctrl Pts',(0.259427175492304,2.29196479429241,7.42462390033303));
#60453=CARTESIAN_POINT('Ctrl Pts',(0.247466119363986,2.30645730495474,7.42575643688147));
#60454=CARTESIAN_POINT('Ctrl Pts',(0.246367322318854,2.30776727683412,7.42585989821044));
#60455=CARTESIAN_POINT('Ctrl Pts',(0.244695015922741,2.3097290594753,7.42601652744217));
#60456=CARTESIAN_POINT('Ctrl Pts',(0.244129199863142,2.31038741159343,7.42606938097697));
#60457=CARTESIAN_POINT('Ctrl Pts',(0.24321003398437,2.31144820121549,7.42615501812706));
#60458=CARTESIAN_POINT('Ctrl Pts',(0.242858326274361,2.31185206107502,7.42618773385038));
#60459=CARTESIAN_POINT('Ctrl Pts',(0.242182203720644,2.31262454457155,7.42625052759352));
#60460=CARTESIAN_POINT('Ctrl Pts',(0.241857949567405,2.31299330735982,7.42628059888398));
#60461=CARTESIAN_POINT('Ctrl Pts',(0.241277497750128,2.31365040013009,7.4263343535673));
#60462=CARTESIAN_POINT('Ctrl Pts',(0.24102162234473,2.31393901457315,7.42635802345106));
#60463=CARTESIAN_POINT('Ctrl Pts',(0.240512675459503,2.31451100885014,7.42640505207505));
#60464=CARTESIAN_POINT('Ctrl Pts',(0.240259619718885,2.31479440194104,7.42642841013404));
#60465=CARTESIAN_POINT('Ctrl Pts',(0.23964396653593,2.31548141291726,7.42648517660794));
#60466=CARTESIAN_POINT('Ctrl Pts',(0.239280850744737,2.3158845628363,7.42651860685005));
#60467=CARTESIAN_POINT('Ctrl Pts',(0.237916682786574,2.31739146268785,7.42664401033311));
#60468=CARTESIAN_POINT('Ctrl Pts',(0.236909009562826,2.31848916921896,7.42673626390827));
#60469=CARTESIAN_POINT('Ctrl Pts',(0.218762569928013,2.33798381975717,7.42839103011352));
#60470=CARTESIAN_POINT('Ctrl Pts',(0.199540319895566,2.35431575926016,7.4300506923714));
#60471=CARTESIAN_POINT('Ctrl Pts',(0.165499797724477,2.37698283545666,7.43281276530607));
#60472=CARTESIAN_POINT('Ctrl Pts',(0.151755063936069,2.38474568469427,7.43388594890604));
#60473=CARTESIAN_POINT('Ctrl Pts',(0.131738306342143,2.3941882692157,7.43535050661704));
#60474=CARTESIAN_POINT('Ctrl Pts',(0.125899863970404,2.39673381125721,7.43576648652181));
#60475=CARTESIAN_POINT('Ctrl Pts',(0.117206728503596,2.40022116530097,7.43636578380568));
#60476=CARTESIAN_POINT('Ctrl Pts',(0.114408445075333,2.40129864683227,7.43655570224769));
#60477=CARTESIAN_POINT('Ctrl Pts',(0.111121139626074,2.40251202212807,7.43677499326239));
#60478=CARTESIAN_POINT('Ctrl Pts',(0.110646452993243,2.40268596540325,7.43680656648272));
#60479=CARTESIAN_POINT('Ctrl Pts',(0.109921364433264,2.40294973185579,7.43685465185827));
#60480=CARTESIAN_POINT('Ctrl Pts',(0.109671260088295,2.40304036216689,7.43687121199087));
#60481=CARTESIAN_POINT('Ctrl Pts',(0.109235939529656,2.40319749977158,7.43689999038019));
#60482=CARTESIAN_POINT('Ctrl Pts',(0.109050775118479,2.4032641469073,7.43691221701533));
#60483=CARTESIAN_POINT('Ctrl Pts',(0.108631762250848,2.40341453088364,7.43693985255746));
#60484=CARTESIAN_POINT('Ctrl Pts',(0.10839787845273,2.40349816682973,7.43695525534996));
#60485=CARTESIAN_POINT('Ctrl Pts',(0.107763847112237,2.40372406759573,7.43699694944475));
#60486=CARTESIAN_POINT('Ctrl Pts',(0.107363512904892,2.40386581262615,7.43702320970577));
#60487=CARTESIAN_POINT('Ctrl Pts',(0.105564184375826,2.40449889521849,7.43714094762509));
#60488=CARTESIAN_POINT('Ctrl Pts',(0.104162060550437,2.40498137574661,7.43723190667217));
#60489=CARTESIAN_POINT('Ctrl Pts',(0.072038281751541,2.41578800860379,7.43929895379844));
#60490=CARTESIAN_POINT('Ctrl Pts',(0.0399310982912344,2.42143106456642,
7.44102682020046));
#60491=CARTESIAN_POINT('Ctrl Pts',(-0.00785175016274551,2.42254589197846,
7.44373876415127));
#60492=CARTESIAN_POINT('Ctrl Pts',(-0.0232245135824139,2.4218043386661,
7.44462980949059));
#60493=CARTESIAN_POINT('Ctrl Pts',(-0.0409110140993787,2.41967708374758,
7.44570439295655));
#60494=CARTESIAN_POINT('Ctrl Pts',(-0.0433341118570751,2.41935764150812,
7.44585266583824));
#60495=CARTESIAN_POINT('Ctrl Pts',(-0.0464530958618366,2.41891030919293,
7.44604495344453));
#60496=CARTESIAN_POINT('Ctrl Pts',(-0.0471525635412023,2.41880763975104,
7.4460881691795));
#60497=CARTESIAN_POINT('Ctrl Pts',(-0.0482807359620205,2.41863825005176,
7.44615802408864));
#60498=CARTESIAN_POINT('Ctrl Pts',(-0.0487096563519322,2.41857296375595,
7.4461846177949));
#60499=CARTESIAN_POINT('Ctrl Pts',(-0.0495274213639583,2.41844680099558,
7.44623538875211));
#60500=CARTESIAN_POINT('Ctrl Pts',(-0.049916289143771,2.41838607791047,
7.44625956109785));
#60501=CARTESIAN_POINT('Ctrl Pts',(-0.0508041250859461,2.41824577263861,
7.44631481750648));
#60502=CARTESIAN_POINT('Ctrl Pts',(-0.05130301836948,2.41816572918785,7.44634591615278));
#60503=CARTESIAN_POINT('Ctrl Pts',(-0.0528293236139818,2.41791716243199,
7.44644120979776));
#60504=CARTESIAN_POINT('Ctrl Pts',(-0.0538561013263279,2.41774483459452,
7.44650552542752));
#60505=CARTESIAN_POINT('Ctrl Pts',(-0.0614607330363169,2.41643060226578,
7.44698344451386));
#60506=CARTESIAN_POINT('Ctrl Pts',(-0.0680020980278876,2.41508959309327,
7.44740335318742));
#60507=CARTESIAN_POINT('Ctrl Pts',(-0.0763225056268109,2.41311271514275,
7.44794939112691));
#60508=CARTESIAN_POINT('Ctrl Pts',(-0.0781444245685719,2.41266299097908,
7.44806969422149));
#60509=CARTESIAN_POINT('Ctrl Pts',(-0.0817246995185879,2.41174598472427,
7.44830756008916));
#60510=CARTESIAN_POINT('Ctrl Pts',(-0.083483234745857,2.41127967298985,
7.44842509022123));
#60511=CARTESIAN_POINT('Ctrl Pts',(-0.112843499242343,2.40322750602925,
7.45039899757463));
#60512=CARTESIAN_POINT('Ctrl Pts',(-0.139315655900175,2.39201244060027,
7.45236792164115));
#60513=CARTESIAN_POINT('Ctrl Pts',(-0.173115774615028,2.37203930138863,
7.45498959912348));
#60514=CARTESIAN_POINT('Ctrl Pts',(-0.182005952877563,2.36617350799146,
7.45568883829962));
#60515=CARTESIAN_POINT('Ctrl Pts',(-0.191805300488816,2.35898681879531,
7.45645727735599));
#60516=CARTESIAN_POINT('Ctrl Pts',(-0.193014002410747,2.35808727339693,
7.45655201516556));
#60517=CARTESIAN_POINT('Ctrl Pts',(-0.194542227019738,2.356933190266,7.45667169193729));
#60518=CARTESIAN_POINT('Ctrl Pts',(-0.194867609153495,2.35668649606329,
7.45669716682055));
#60519=CARTESIAN_POINT('Ctrl Pts',(-0.195387258846602,2.35629095691814,
7.45673784035899));
#60520=CARTESIAN_POINT('Ctrl Pts',(-0.195581825884623,2.35614250897147,
7.45675306685999));
#60521=CARTESIAN_POINT('Ctrl Pts',(-0.195950449892836,2.35586059665337,
7.4567819097855));
#60522=CARTESIAN_POINT('Ctrl Pts',(-0.196124538258917,2.35572717733169,
7.45679552914569));
#60523=CARTESIAN_POINT('Ctrl Pts',(-0.196522703474639,2.35542138235988,
7.45682667386535));
#60524=CARTESIAN_POINT('Ctrl Pts',(-0.19674668946289,2.35524888978107,7.45684419078004));
#60525=CARTESIAN_POINT('Ctrl Pts',(-0.197435160396986,2.35471725068142,
7.45689802344901));
#60526=CARTESIAN_POINT('Ctrl Pts',(-0.197898894374068,2.35435712683947,
7.45693427026667));
#60527=CARTESIAN_POINT('Ctrl Pts',(-0.201395177642832,2.35162665380411,
7.4572074714067));
#60528=CARTESIAN_POINT('Ctrl Pts',(-0.204386188379017,2.34920328985304,
7.45744074210153));
#60529=CARTESIAN_POINT('Ctrl Pts',(-0.228711538102684,2.32876184085922,
7.45934090498066));
#60530=CARTESIAN_POINT('Ctrl Pts',(-0.247667265827999,2.30809212563943,
7.46084937356339));
#60531=CARTESIAN_POINT('Ctrl Pts',(-0.271443359884391,2.27424160842031,
7.46318549050736));
#60532=CARTESIAN_POINT('Ctrl Pts',(-0.278468973331682,2.26277779984589,
7.4639561390373));
#60533=CARTESIAN_POINT('Ctrl Pts',(-0.287482427280929,2.24576991684566,
7.46509724704549));
#60534=CARTESIAN_POINT('Ctrl Pts',(-0.290066573691369,2.24055742919544,
7.46544656587996));
#60535=CARTESIAN_POINT('Ctrl Pts',(-0.292896224973288,2.23443895201392,
7.46585718806442));
#60536=CARTESIAN_POINT('Ctrl Pts',(-0.293280698861437,2.23359813647496,
7.46591362865117));
#60537=CARTESIAN_POINT('Ctrl Pts',(-0.293859878024684,2.2323169661157,7.46599965084002));
#60538=CARTESIAN_POINT('Ctrl Pts',(-0.294057225576128,2.23187780524878,
7.46602914158545));
#60539=CARTESIAN_POINT('Ctrl Pts',(-0.294413147627628,2.23108099476309,
7.46608265725775));
#60540=CARTESIAN_POINT('Ctrl Pts',(-0.294572056674591,2.23072349486014,
7.46610667065653));
#60541=CARTESIAN_POINT('Ctrl Pts',(-0.294911848864742,2.22995529392316,
7.46615827754153));
#60542=CARTESIAN_POINT('Ctrl Pts',(-0.295092525739823,2.22954450304324,
7.46618587802615));
#60543=CARTESIAN_POINT('Ctrl Pts',(-0.295574530191809,2.22844236639545,
7.46625994057599));
#60544=CARTESIAN_POINT('Ctrl Pts',(-0.295874288674136,2.2277503411717,7.46630645610841));
#60545=CARTESIAN_POINT('Ctrl Pts',(-0.297223172016263,2.22460608236259,
7.4665178625672));
#60546=CARTESIAN_POINT('Ctrl Pts',(-0.298244233745826,2.222141991528,7.46668370469839));
#60547=CARTESIAN_POINT('Ctrl Pts',(-0.299475739143415,2.21906250099698,
7.46689122679276));
#60548=CARTESIAN_POINT('Ctrl Pts',(-0.299715084313064,2.21845870885847,
7.46693192773647));
#60549=CARTESIAN_POINT('Ctrl Pts',(-0.311966751852016,2.18727679492721,
7.46903452546429));
#60550=CARTESIAN_POINT('Ctrl Pts',(-0.319232292372442,2.15504722634259,
7.47127041119508));
#60551=CARTESIAN_POINT('Ctrl Pts',(-0.322020786084112,2.11482461997514,
7.47398440293776));
#60552=CARTESIAN_POINT('Ctrl Pts',(-0.322278183387271,2.10734437814288,
7.47448450862746));
#60553=CARTESIAN_POINT('Ctrl Pts',(-0.32227471063135,2.0992569169113,7.47501614503034));
#60554=CARTESIAN_POINT('Ctrl Pts',(-0.322272749041375,2.09865221691015,
7.47505584039782));
#60555=CARTESIAN_POINT('Ctrl Pts',(-0.322259178914493,2.09641237956066,
7.47520266167197));
#60556=CARTESIAN_POINT('Ctrl Pts',(-0.322236827622263,2.09477730615424,
7.4753094217966));
#60557=CARTESIAN_POINT('Ctrl Pts',(-0.322179229564705,2.09207106305374,
7.47548535647127));
#60558=CARTESIAN_POINT('Ctrl Pts',(-0.322151082943541,2.09099978769373,
7.47555480197062));
#60559=CARTESIAN_POINT('Ctrl Pts',(-0.32198193068935,2.08558969215906,7.47590444358153));
#60560=CARTESIAN_POINT('Ctrl Pts',(-0.321758603911821,2.08125363840353,
7.47618120513538));
#60561=CARTESIAN_POINT('Ctrl Pts',(-0.3214047372209,2.07632446825163,7.47649088283619));
#60562=CARTESIAN_POINT('Ctrl Pts',(-0.321360083558188,2.07572588578635,
7.47652840594408));
#60563=CARTESIAN_POINT('Ctrl Pts',(-0.32129164870998,2.07484181733002,7.4765836988531));
#60564=CARTESIAN_POINT('Ctrl Pts',(-0.321269159140845,2.07455623706101,
7.47660154061435));
#60565=CARTESIAN_POINT('Ctrl Pts',(-0.321228684833388,2.07405089047564,
7.4766330774373));
#60566=CARTESIAN_POINT('Ctrl Pts',(-0.321210855306483,2.07383111237841,
7.47664678126998));
#60567=CARTESIAN_POINT('Ctrl Pts',(-0.321173121353051,2.07337182876216,
7.47667539435594));
#60568=CARTESIAN_POINT('Ctrl Pts',(-0.321153174622573,2.07313232771745,
7.4766903011586));
#60569=CARTESIAN_POINT('Ctrl Pts',(-0.321100267017823,2.07250554199368,
7.47672927694563));
#60570=CARTESIAN_POINT('Ctrl Pts',(-0.321066873260514,2.07211829276273,
7.47675332148254));
#60571=CARTESIAN_POINT('Ctrl Pts',(-0.320917583532146,2.07042289957278,
7.47685843545395));
#60572=CARTESIAN_POINT('Ctrl Pts',(-0.320794390675278,2.06911538668003,
7.4769390993658));
#60573=CARTESIAN_POINT('Ctrl Pts',(-0.319822549819421,2.05943472772793,
7.4775335894894));
#60574=CARTESIAN_POINT('Ctrl Pts',(-0.318654112941115,2.0510961313201,7.47803051485388));
#60575=CARTESIAN_POINT('Ctrl Pts',(-0.314329149005187,2.027110162878,7.4794403800165));
#60576=CARTESIAN_POINT('Ctrl Pts',(-0.310335574272976,2.01163915384284,
7.48032616214036));
#60577=CARTESIAN_POINT('Ctrl Pts',(-0.297284708618472,1.97314335527495,
7.48259947086348));
#60578=CARTESIAN_POINT('Ctrl Pts',(-0.286697875668781,1.95075226935366,
7.4839945729806));
#60579=CARTESIAN_POINT('Ctrl Pts',(-0.272832694084156,1.92846005943784,
7.48558619437701));
#60580=CARTESIAN_POINT('Ctrl Pts',(-0.271995563643761,1.92713576601158,
7.48568153045452));
#60581=CARTESIAN_POINT('Ctrl Pts',(-0.270849335729347,1.92535143859102,
7.48581107009117));
#60582=CARTESIAN_POINT('Ctrl Pts',(-0.270548649270705,1.92488600558778,
7.48584496064615));
#60583=CARTESIAN_POINT('Ctrl Pts',(-0.270038034241506,1.92410007824352,
7.48590235975522));
#60584=CARTESIAN_POINT('Ctrl Pts',(-0.269828731039281,1.92377917740904,
7.48592584491846));
#60585=CARTESIAN_POINT('Ctrl Pts',(-0.269425268453555,1.92316299812767,
7.48597103399035));
#60586=CARTESIAN_POINT('Ctrl Pts',(-0.269231194518096,1.92286766413426,
7.48599273467583));
#60587=CARTESIAN_POINT('Ctrl Pts',(-0.268773272006708,1.92217330707748,
7.48604385334323));
#60588=CARTESIAN_POINT('Ctrl Pts',(-0.268509020519237,1.92177455188203,
7.48607328643624));
#60589=CARTESIAN_POINT('Ctrl Pts',(-0.267739590108587,1.9206190775345,7.48615879861507));
#60590=CARTESIAN_POINT('Ctrl Pts',(-0.267232096282438,1.91986391215137,
7.48621496489547));
#60591=CARTESIAN_POINT('Ctrl Pts',(-0.263653355716719,1.91458705017719,
7.48660941580433));
#60592=CARTESIAN_POINT('Ctrl Pts',(-0.26047086313411,1.91014221773362,7.48695191335197));
#60593=CARTESIAN_POINT('Ctrl Pts',(-0.250142239746943,1.89646549082929,
7.48803936477488));
#60594=CARTESIAN_POINT('Ctrl Pts',(-0.24260730075123,1.88754039879937,7.48879918587341));
#60595=CARTESIAN_POINT('Ctrl Pts',(-0.213860096148085,1.85701727220393,
7.49158026631161));
#60596=CARTESIAN_POINT('Ctrl Pts',(-0.190117817070804,1.83802321876545,
7.49368525504334));
#60597=CARTESIAN_POINT('Ctrl Pts',(-0.160910778273966,1.82074666665782,
7.49586774973772));
#60598=CARTESIAN_POINT('Ctrl Pts',(-0.157713210773484,1.81892839212649,
7.49610154944893));
#60599=CARTESIAN_POINT('Ctrl Pts',(-0.153976653499718,1.81688747575884,
7.49636825370207));
#60600=CARTESIAN_POINT('Ctrl Pts',(-0.153467502293264,1.81661115590509,
7.49640445726968));
#60601=CARTESIAN_POINT('Ctrl Pts',(-0.152710134902788,1.81620276715513,
7.49645810241774));
#60602=CARTESIAN_POINT('Ctrl Pts',(-0.152462490044769,1.81606964973214,
7.49647561043107));
#60603=CARTESIAN_POINT('Ctrl Pts',(-0.152021502629277,1.81583334750356,
7.49650672838327));
#60604=CARTESIAN_POINT('Ctrl Pts',(-0.151828229115562,1.81573003588593,
7.49652034643599));
#60605=CARTESIAN_POINT('Ctrl Pts',(-0.151418121047094,1.81551135599188,
7.49654919982685));
#60606=CARTESIAN_POINT('Ctrl Pts',(-0.151201260561406,1.81539603875452,
7.49656443187123));
#60607=CARTESIAN_POINT('Ctrl Pts',(-0.150620038808862,1.81508782142063,
7.49660518909658));
#60608=CARTESIAN_POINT('Ctrl Pts',(-0.15025543733087,1.81489537157278,7.4966306855814));
#60609=CARTESIAN_POINT('Ctrl Pts',(-0.148519522585434,1.81398334784071,
7.49675174698456));
#60610=CARTESIAN_POINT('Ctrl Pts',(-0.147143373848165,1.81327294920144,
7.49684673866733));
#60611=CARTESIAN_POINT('Ctrl Pts',(-0.135788546076031,1.80751461458152,
7.49762294409451));
#60612=CARTESIAN_POINT('Ctrl Pts',(-0.125557267455462,1.80297868711241,
7.49827449733968));
#60613=CARTESIAN_POINT('Ctrl Pts',(-0.0824529427827286,1.7864954440634,
7.50090808862388));
#60614=CARTESIAN_POINT('Ctrl Pts',(-0.0479838896690525,1.77940478345643,
7.50278448911669));
#60615=CARTESIAN_POINT('Ctrl Pts',(-0.00928726900057291,1.77783686879122,
7.50510314487613));
#60616=CARTESIAN_POINT('Ctrl Pts',(-0.00552501174200246,1.77775039348909,
7.50533038893702));
#60617=CARTESIAN_POINT('Ctrl Pts',(-0.000983001639697015,1.77772555712258,
7.50560719164472));
#60618=CARTESIAN_POINT('Ctrl Pts',(-0.000203775976239631,1.77772412240012,
7.50565476701871));
#60619=CARTESIAN_POINT('Ctrl Pts',(0.00107203310947944,1.77772640043957,
7.50573280663182));
#60620=CARTESIAN_POINT('Ctrl Pts',(0.00156861940101777,1.7777284349226,
7.50576321827106));
#60621=CARTESIAN_POINT('Ctrl Pts',(0.00245775825731967,1.77773413280312,
7.5058177357273));
#60622=CARTESIAN_POINT('Ctrl Pts',(0.00285031338416871,1.77773736572904,
7.50584182801245));
#60623=CARTESIAN_POINT('Ctrl Pts',(0.00368154973764707,1.77774573038595,
7.50589289218606));
#60624=CARTESIAN_POINT('Ctrl Pts',(0.0041202280146117,1.77775104063623,
7.50591986961889));
#60625=CARTESIAN_POINT('Ctrl Pts',(0.00528744962038929,1.77776755376991,
7.50599172746481));
#60626=CARTESIAN_POINT('Ctrl Pts',(0.00601596499620415,1.77778033163982,
7.5060366571325));
#60627=CARTESIAN_POINT('Ctrl Pts',(0.00940372142326487,1.77785124461056,
7.50624596699108));
#60628=CARTESIAN_POINT('Ctrl Pts',(0.0120621591330603,1.77793982827692,
7.50641129822334));
#60629=CARTESIAN_POINT('Ctrl Pts',(0.0325425236953344,1.77887619666149,
7.50769367321661));
#60630=CARTESIAN_POINT('Ctrl Pts',(0.0502644214661067,1.78116961752135,
7.50885664924497));
#60631=CARTESIAN_POINT('Ctrl Pts',(0.084688649647664,1.78856648065074,7.511210923269));
#60632=CARTESIAN_POINT('Ctrl Pts',(0.10135050723683,1.79358353913651,7.51239655913679));
#60633=CARTESIAN_POINT('Ctrl Pts',(0.126732013946108,1.80352417784261,7.51422485677772));
#60634=CARTESIAN_POINT('Ctrl Pts',(0.13576764884014,1.80755154919271,7.5148799230681));
#60635=CARTESIAN_POINT('Ctrl Pts',(0.147830730121591,1.81360816494451,7.51574766435115));
#60636=CARTESIAN_POINT('Ctrl Pts',(0.151029679621281,1.81528216329809,7.51597707884198));
#60637=CARTESIAN_POINT('Ctrl Pts',(0.154705915595677,1.81728532533884,7.51623932295906));
#60638=CARTESIAN_POINT('Ctrl Pts',(0.155211110196343,1.8175623628606,7.51627532994188));
#60639=CARTESIAN_POINT('Ctrl Pts',(0.155961175529324,1.81797630232479,7.51632874037461));
#60640=CARTESIAN_POINT('Ctrl Pts',(0.156206611343792,1.81811216965465,7.5163462094178));
#60641=CARTESIAN_POINT('Ctrl Pts',(0.15664340465935,1.81835471351617,7.51637728397507));
#60642=CARTESIAN_POINT('Ctrl Pts',(0.156834830674453,1.81846126463625,7.5163908975176));
#60643=CARTESIAN_POINT('Ctrl Pts',(0.157240953385629,1.81868786249397,7.516419768848));
#60644=CARTESIAN_POINT('Ctrl Pts',(0.157455620722199,1.81880795951202,7.51643502328626));
#60645=CARTESIAN_POINT('Ctrl Pts',(0.158023893143474,1.81912673795696,7.5164753890674));
#60646=CARTESIAN_POINT('Ctrl Pts',(0.15837726244995,1.81932584216203,7.51650047319099));
#60647=CARTESIAN_POINT('Ctrl Pts',(0.160025257669488,1.82025850025271,7.51661738415348));
#60648=CARTESIAN_POINT('Ctrl Pts',(0.161315196117022,1.82100036294766,7.51670868363776));
#60649=CARTESIAN_POINT('Ctrl Pts',(0.171640689189943,1.82703426015247,7.51743818624322));
#60650=CARTESIAN_POINT('Ctrl Pts',(0.180419584255306,1.83275546090998,7.51805034015976));
#60651=CARTESIAN_POINT('Ctrl Pts',(0.209374302340331,1.85370369233939,7.52009621756664));
#60652=CARTESIAN_POINT('Ctrl Pts',(0.228031324597575,1.87086839377805,7.52146865531097));
#60653=CARTESIAN_POINT('Ctrl Pts',(0.247034115806452,1.8929962827731,7.52314091686641));
#60654=CARTESIAN_POINT('Ctrl Pts',(0.249521611401101,1.8960015752848,7.52336605420259));
#60655=CARTESIAN_POINT('Ctrl Pts',(0.258081153194738,1.90673371152912,7.52416471678739));
#60656=CARTESIAN_POINT('Ctrl Pts',(0.263853298654219,1.91469175103825,7.52474768380718));
#60657=CARTESIAN_POINT('Ctrl Pts',(0.269824951733037,1.92377072868257,7.52540846569277));
#60658=CARTESIAN_POINT('Ctrl Pts',(0.270393137505785,1.92464375746289,7.52547196104456));
#60659=CARTESIAN_POINT('Ctrl Pts',(0.271236568907388,1.92595355270691,7.52556716143676));
#60660=CARTESIAN_POINT('Ctrl Pts',(0.271515017542906,1.92638825681486,7.52559874722855));
#60661=CARTESIAN_POINT('Ctrl Pts',(0.27199275710952,1.9271380472721,7.52565321096264));
#60662=CARTESIAN_POINT('Ctrl Pts',(0.272192548569439,1.92745281479456,7.52567607028625));
#60663=CARTESIAN_POINT('Ctrl Pts',(0.272603746965568,1.92810314122026,7.52572328900514));
#60664=CARTESIAN_POINT('Ctrl Pts',(0.2728150815016,1.92843874498858,7.52574765102988));
#60665=CARTESIAN_POINT('Ctrl Pts',(0.273305525353882,1.92922077808542,7.52580440798869));
#60666=CARTESIAN_POINT('Ctrl Pts',(0.27358416064105,1.92966750202092,7.52583682034686));
#60667=CARTESIAN_POINT('Ctrl Pts',(0.274450590248883,1.93106422186664,7.52593813314234));
#60668=CARTESIAN_POINT('Ctrl Pts',(0.275034535720964,1.93201658494995,7.52600717489425));
#60669=CARTESIAN_POINT('Ctrl Pts',(0.284427550475583,1.94751602871191,7.52713023977432));
#60670=CARTESIAN_POINT('Ctrl Pts',(0.292075055211723,1.96273242974542,7.52822689351689));
#60671=CARTESIAN_POINT('Ctrl Pts',(0.307202067195499,1.9998880943741,7.53088937974676));
#60672=CARTESIAN_POINT('Ctrl Pts',(0.313589000834757,2.02217110125456,7.53247717853517));
#60673=CARTESIAN_POINT('Ctrl Pts',(0.319302345149324,2.05512338869548,7.53470131759485));
#60674=CARTESIAN_POINT('Ctrl Pts',(0.320576932530829,2.06538240071531,7.53537590430649));
#60675=CARTESIAN_POINT('Ctrl Pts',(0.321412060614349,2.07642023987314,7.53607073093546));
#60676=CARTESIAN_POINT('Ctrl Pts',(0.321465096523879,2.07715466048096,7.53611681545331));
#60677=CARTESIAN_POINT('Ctrl Pts',(0.321535333763853,2.07817599104091,7.53618069317203));
#60678=CARTESIAN_POINT('Ctrl Pts',(0.32155466854812,2.07846274478563,7.53619860475853));
#60679=CARTESIAN_POINT('Ctrl Pts',(0.321587299286734,2.07895653068464,7.53622940815392));
#60680=CARTESIAN_POINT('Ctrl Pts',(0.321600778931337,2.07916354985433,7.53624231030758));
#60681=CARTESIAN_POINT('Ctrl Pts',(0.321628281901789,2.07959232308535,7.53626900761201));
#60682=CARTESIAN_POINT('Ctrl Pts',(0.32164227576583,2.07981407825817,7.53628280100086));
#60683=CARTESIAN_POINT('Ctrl Pts',(0.321669634198054,2.08025486858505,7.53631019091756));
#60684=CARTESIAN_POINT('Ctrl Pts',(0.321683004426913,2.08047390353233,7.53632378778158));
#60685=CARTESIAN_POINT('Ctrl Pts',(0.321727579013203,2.08121661020578,7.53636984671027));
#60686=CARTESIAN_POINT('Ctrl Pts',(0.32175772865227,2.08174034798887,7.53640224960014));
#60687=CARTESIAN_POINT('Ctrl Pts',(0.321979725704294,2.08576810659435,7.5366508674772));
#60688=CARTESIAN_POINT('Ctrl Pts',(0.322115616753237,2.08927514783993,7.53686400586497));
#60689=CARTESIAN_POINT('Ctrl Pts',(0.322389338252756,2.10149660401304,7.53759730453807));
#60690=CARTESIAN_POINT('Ctrl Pts',(0.322230998615781,2.11021441198464,7.53810369316131));
#60691=CARTESIAN_POINT('Ctrl Pts',(0.320589753881509,2.13812872716889,7.53970135358148));
#60692=CARTESIAN_POINT('Ctrl Pts',(0.317741294467233,2.15720243738382,7.54075888617756));
#60693=CARTESIAN_POINT('Ctrl Pts',(0.308724619168357,2.19440629439183,7.54291889424128));
#60694=CARTESIAN_POINT('Ctrl Pts',(0.302612471913952,2.21246763174207,7.54401698247043));
#60695=CARTESIAN_POINT('Ctrl Pts',(0.294423087930708,2.23106444239101,7.54525121573497));
#60696=CARTESIAN_POINT('Ctrl Pts',(0.293895628593212,2.23224296648183,7.54532988031166));
#60697=CARTESIAN_POINT('Ctrl Pts',(0.293149782878248,2.23388293764343,7.54543998389657));
#60698=CARTESIAN_POINT('Ctrl Pts',(0.292937355710624,2.23434709456529,7.54547121790912));
#60699=CARTESIAN_POINT('Ctrl Pts',(0.292568507967334,2.23514799901131,7.54552523702457));
#60700=CARTESIAN_POINT('Ctrl Pts',(0.292412606084908,2.23548498548457,7.5455480042089));
#60701=CARTESIAN_POINT('Ctrl Pts',(0.292088607567802,2.23618215353597,7.54559518525006));
#60702=CARTESIAN_POINT('Ctrl Pts',(0.291920426326473,2.23654229492635,7.54561960200237));
#60703=CARTESIAN_POINT('Ctrl Pts',(0.291525610134593,2.2373836861714,7.54567675000832));
#60704=CARTESIAN_POINT('Ctrl Pts',(0.291298449564691,2.23786468679899,7.54570949942449));
#60705=CARTESIAN_POINT('Ctrl Pts',(0.290576536256193,2.23938355048045,7.54581316566862));
#60706=CARTESIAN_POINT('Ctrl Pts',(0.290077423923666,2.24041932075781,7.54588423373395));
#60707=CARTESIAN_POINT('Ctrl Pts',(0.27806365433372,2.26501318432381,7.54758073827031));
#60708=CARTESIAN_POINT('Ctrl Pts',(0.26372477522185,2.28707592514208,7.54931284549977));
#60709=CARTESIAN_POINT('Ctrl Pts',(0.237958722599989,2.31778274584016,7.552021529374));
#60710=CARTESIAN_POINT('Ctrl Pts',(0.228363106651417,2.32782447021078,7.55296467383625));
#60711=CARTESIAN_POINT('Ctrl Pts',(0.210555839783719,2.34420044536229,7.55457347628032));
#60712=CARTESIAN_POINT('Ctrl Pts',(0.202629784659497,2.35081634590742,7.55524714752603));
#60713=CARTESIAN_POINT('Ctrl Pts',(0.193811942350944,2.35748523942902,7.55594111347248));
#60714=CARTESIAN_POINT('Ctrl Pts',(0.193223285908746,2.35792727527178,7.555987186263));
#60715=CARTESIAN_POINT('Ctrl Pts',(0.192402727725433,2.35853906585154,7.55605105034629));
#60716=CARTESIAN_POINT('Ctrl Pts',(0.192172111484596,2.3587105289251,7.55606895995923));
#60717=CARTESIAN_POINT('Ctrl Pts',(0.191774622924526,2.35900523674641,7.55609976086153));
#60718=CARTESIAN_POINT('Ctrl Pts',(0.1916078609171,2.35912862886071,7.55611266249185));
#60719=CARTESIAN_POINT('Ctrl Pts',(0.19126223084712,2.35938385464388,7.55613935960183));
#60720=CARTESIAN_POINT('Ctrl Pts',(0.191083345884996,2.35951566412101,7.55615315331808));
#60721=CARTESIAN_POINT('Ctrl Pts',(0.190727518720663,2.35977728420069,7.55618054416707));
#60722=CARTESIAN_POINT('Ctrl Pts',(0.190550579750975,2.35990709944379,7.55619414163548));
#60723=CARTESIAN_POINT('Ctrl Pts',(0.189950141585274,2.3603466816438,7.55624020713036));
#60724=CARTESIAN_POINT('Ctrl Pts',(0.18952601564226,2.36065559716829,7.55627261595687));
#60725=CARTESIAN_POINT('Ctrl Pts',(0.186257526027512,2.36302403238353,7.55652138921393));
#60726=CARTESIAN_POINT('Ctrl Pts',(0.183380286502167,2.36503807386133,7.55673467272383));
#60727=CARTESIAN_POINT('Ctrl Pts',(0.17644450716106,2.36972601979594,7.5572368347689));
#60728=CARTESIAN_POINT('Ctrl Pts',(0.172357203899732,2.37235599708269,7.55752325645542));
#60729=CARTESIAN_POINT('Ctrl Pts',(0.153136519010056,2.38411748056163,7.55883428460118));
#60730=CARTESIAN_POINT('Ctrl Pts',(0.137326822676004,2.39208727429661,7.55981306731855));
#60731=CARTESIAN_POINT('Ctrl Pts',(0.0984474439200499,2.40782826487582,
7.56215992032219));
#60732=CARTESIAN_POINT('Ctrl Pts',(0.0749997813105582,2.41436431793709,
7.56353438164212));
#60733=CARTESIAN_POINT('Ctrl Pts',(0.0496295329358651,2.41843387559515,
7.56509357448261));
#60734=CARTESIAN_POINT('Ctrl Pts',(0.0482150226277544,2.41865111824052,
7.56518070924072));
#60735=CARTESIAN_POINT('Ctrl Pts',(0.046271449059068,2.41893637778122,7.56530072715308));
#60736=CARTESIAN_POINT('Ctrl Pts',(0.045743579333687,2.41901251545133,7.56533335327366));
#60737=CARTESIAN_POINT('Ctrl Pts',(0.0448418510773135,2.41914029274495,
7.56538913785444));
#60738=CARTESIAN_POINT('Ctrl Pts',(0.0444680851611076,2.41919258678972,
7.5654122755827));
#60739=CARTESIAN_POINT('Ctrl Pts',(0.0437425393052485,2.41929279967722,
7.56545721954621));
#60740=CARTESIAN_POINT('Ctrl Pts',(0.0433907701738959,2.41934079403162,
7.56547902336126));
#60741=CARTESIAN_POINT('Ctrl Pts',(0.0425519838049881,2.4194538240735,7.5655310465413));
#60742=CARTESIAN_POINT('Ctrl Pts',(0.0420648968123182,2.41951832731916,
7.56556128268018));
#60743=CARTESIAN_POINT('Ctrl Pts',(0.0410552397786087,2.41964968396805,
7.56562401227821));
#60744=CARTESIAN_POINT('Ctrl Pts',(0.0405326498266147,2.4197163703455,7.5656565109245));
#60745=CARTESIAN_POINT('Ctrl Pts',(0.0375243938921511,2.42009275209141,
7.56584376423246));
#60746=CARTESIAN_POINT('Ctrl Pts',(0.0350354039826819,2.42037473367361,
7.56599939083861));
#60747=CARTESIAN_POINT('Ctrl Pts',(0.0214036742884474,2.42175834263087,
7.56685573187668));
#60748=CARTESIAN_POINT('Ctrl Pts',(0.0102137971727213,2.4223075825396,7.56757368229564));
#60749=CARTESIAN_POINT('Ctrl Pts',(-0.0191384516478878,2.4222182378215,
7.56949671374057));
#60750=CARTESIAN_POINT('Ctrl Pts',(-0.03725727032625,2.42062852560138,7.57072531935603));
#60751=CARTESIAN_POINT('Ctrl Pts',(-0.0736300222395724,2.41431169295863,
7.57322266100388));
#60752=CARTESIAN_POINT('Ctrl Pts',(-0.0918029673777799,2.4094925133396,
7.57448625858238));
#60753=CARTESIAN_POINT('Ctrl Pts',(-0.11001898473321,2.40291477039152,7.57570678831306));
#60754=CARTESIAN_POINT('Ctrl Pts',(-0.110582361969647,2.40270955775722,
7.57574448743863));
#60755=CARTESIAN_POINT('Ctrl Pts',(-0.111792221333861,2.40226503283002,
7.57582533651021));
#60756=CARTESIAN_POINT('Ctrl Pts',(-0.112438516919302,2.40202521543123,
7.57586845747046));
#60757=CARTESIAN_POINT('Ctrl Pts',(-0.113338564281399,2.40168795028591,
7.57592840908233));
#60758=CARTESIAN_POINT('Ctrl Pts',(-0.113592963878698,2.40159225464138,
7.57594534335488));
#60759=CARTESIAN_POINT('Ctrl Pts',(-0.114056599141817,2.4014171824842,7.57597618482715));
#60760=CARTESIAN_POINT('Ctrl Pts',(-0.114265873544572,2.4013379097433,7.57599009826335));
#60761=CARTESIAN_POINT('Ctrl Pts',(-0.114689445478729,2.4011769568133,7.57601824324527));
#60762=CARTESIAN_POINT('Ctrl Pts',(-0.114903738595512,2.40109526578328,
7.57603247411396));
#60763=CARTESIAN_POINT('Ctrl Pts',(-0.115333917545817,2.40093075043041,
7.57606102546662));
#60764=CARTESIAN_POINT('Ctrl Pts',(-0.115549801810046,2.40084792236865,
7.57607534571319));
#60765=CARTESIAN_POINT('Ctrl Pts',(-0.116067207556463,2.40064877082858,
7.57610964758216));
#60766=CARTESIAN_POINT('Ctrl Pts',(-0.116368644315582,2.40053222571464,
7.57612961595105));
#60767=CARTESIAN_POINT('Ctrl Pts',(-0.118475865847565,2.39971386060581,
7.57626910057416));
#60768=CARTESIAN_POINT('Ctrl Pts',(-0.120275516164659,2.39899620344473,
7.57638768050341));
#60769=CARTESIAN_POINT('Ctrl Pts',(-0.125403971786671,2.3968973008883,7.57672433096375));
#60770=CARTESIAN_POINT('Ctrl Pts',(-0.128716329096655,2.39547634832763,
7.57694022925628));
#60771=CARTESIAN_POINT('Ctrl Pts',(-0.141106012973778,2.38991345309271,
7.57774447849008));
#60772=CARTESIAN_POINT('Ctrl Pts',(-0.150013793721498,2.38540604470241,
7.57831602093122));
#60773=CARTESIAN_POINT('Ctrl Pts',(-0.166038142563203,2.37633968588535,
7.57935671772759));
#60774=CARTESIAN_POINT('Ctrl Pts',(-0.173211914282338,2.37190057928035,
7.57982760159066));
#60775=CARTESIAN_POINT('Ctrl Pts',(-0.202006409449512,2.35248008775026,
7.58176890483647));
#60776=CARTESIAN_POINT('Ctrl Pts',(-0.221923980034108,2.3351643447647,7.58324605302351));
#60777=CARTESIAN_POINT('Ctrl Pts',(-0.240572010170563,2.3144499349627,7.58493572957001));
#60778=CARTESIAN_POINT('Ctrl Pts',(-0.241619355069264,2.31326920499904,
7.5850317675072));
#60779=CARTESIAN_POINT('Ctrl Pts',(-0.243064385402854,2.3116158349032,7.58516589031185));
#60780=CARTESIAN_POINT('Ctrl Pts',(-0.243469460672147,2.31114965958932,
7.58520366761837));
#60781=CARTESIAN_POINT('Ctrl Pts',(-0.244116861893139,2.31040026686489,
7.58526433445649));
#60782=CARTESIAN_POINT('Ctrl Pts',(-0.244360042202338,2.31011778680147,
7.5852871886055));
#60783=CARTESIAN_POINT('Ctrl Pts',(-0.244860990891138,2.30953383520275,
7.58533440505151));
#60784=CARTESIAN_POINT('Ctrl Pts',(-0.245118693769062,2.30923230849398,
7.58535876999264));
#60785=CARTESIAN_POINT('Ctrl Pts',(-0.245717358807478,2.30852921310653,
7.58541554812993));
#60786=CARTESIAN_POINT('Ctrl Pts',(-0.246057893582275,2.30812728350399,
7.58544797879015));
#60787=CARTESIAN_POINT('Ctrl Pts',(-0.246768631135511,2.30728422505712,
7.58551594756151));
#60788=CARTESIAN_POINT('Ctrl Pts',(-0.247138639737531,2.30684293561013,
7.58555149346543));
#60789=CARTESIAN_POINT('Ctrl Pts',(-0.248125469814401,2.30565956822895,
7.58564673093253));
#60790=CARTESIAN_POINT('Ctrl Pts',(-0.248740140926261,2.30491571202373,
7.5857065097549));
#60791=CARTESIAN_POINT('Ctrl Pts',(-0.253227412591613,2.29943541331254,
7.5861463076778));
#60792=CARTESIAN_POINT('Ctrl Pts',(-0.256967553582593,2.29459258647957,
7.58653161471535));
#60793=CARTESIAN_POINT('Ctrl Pts',(-0.268390840917365,2.27889740462174,
7.58777106381338));
#60794=CARTESIAN_POINT('Ctrl Pts',(-0.275540736382772,2.26767574343762,
7.58864434037639));
#60795=CARTESIAN_POINT('Ctrl Pts',(-0.284324466800438,2.25180343556272,
7.58985733119353));
#60796=CARTESIAN_POINT('Ctrl Pts',(-0.286576119062603,2.24750868295947,
7.59018335983897));
#60797=CARTESIAN_POINT('Ctrl Pts',(-0.290933053726064,2.23872176636475,
7.59084500210653));
#60798=CARTESIAN_POINT('Ctrl Pts',(-0.293033262153102,2.23422844981656,
7.59118058048565));
#60799=CARTESIAN_POINT('Ctrl Pts',(-0.30314404845961,2.21122737811287,7.59288088150922));
#60800=CARTESIAN_POINT('Ctrl Pts',(-0.309509492590652,2.1920430044328,7.59424532760991));
#60801=CARTESIAN_POINT('Ctrl Pts',(-0.314310947131777,2.17121276232323,
7.59559366311978));
#60802=CARTESIAN_POINT('Ctrl Pts',(-0.314575144575699,2.17003647284579,
7.59566935628951));
#60803=CARTESIAN_POINT('Ctrl Pts',(-0.314916399814976,2.16847620070052,
7.5957691407845));
#60804=CARTESIAN_POINT('Ctrl Pts',(-0.314999363060229,2.1680935401512,7.59579356406139));
#60805=CARTESIAN_POINT('Ctrl Pts',(-0.315127203680706,2.16749865315473,
7.5958314553584));
#60806=CARTESIAN_POINT('Ctrl Pts',(-0.315172564164754,2.16728653264813,
7.59584495110018));
#60807=CARTESIAN_POINT('Ctrl Pts',(-0.315258657106847,2.16688193664784,
7.59587066339529));
#60808=CARTESIAN_POINT('Ctrl Pts',(-0.315299427203429,2.16668947095373,
7.59588288202449));
#60809=CARTESIAN_POINT('Ctrl Pts',(-0.315394787604303,2.16623725557477,
7.59591156113053));
#60810=CARTESIAN_POINT('Ctrl Pts',(-0.315449233195827,2.16597747609163,
7.5959280131785));
#60811=CARTESIAN_POINT('Ctrl Pts',(-0.315561059876289,2.16544060807013,
7.59596196664057));
#60812=CARTESIAN_POINT('Ctrl Pts',(-0.315618397114836,2.16516351048668,
7.59597946553258));
#60813=CARTESIAN_POINT('Ctrl Pts',(-0.315765540141842,2.16444765208037,
7.59602460679799));
#60814=CARTESIAN_POINT('Ctrl Pts',(-0.315854796796701,2.16400877710048,
7.59605221812197));
#60815=CARTESIAN_POINT('Ctrl Pts',(-0.316609741036623,2.16025668453382,
7.59628774401639));
#60816=CARTESIAN_POINT('Ctrl Pts',(-0.317224222368816,2.15693321588249,
7.59649281634104));
#60817=CARTESIAN_POINT('Ctrl Pts',(-0.320756986632099,2.13598819890224,
7.5977664681049));
#60818=CARTESIAN_POINT('Ctrl Pts',(-0.322258617410972,2.11815760258075,
7.5987687044119));
#60819=CARTESIAN_POINT('Ctrl Pts',(-0.322274866683432,2.10029313678766,
7.59976792125168));
#60820=CARTESIAN_POINT('',(-0.322274884703664,2.09971229684994,7.84976773360871));
#60821=CARTESIAN_POINT('Ctrl Pts',(-0.322274866567678,2.10029326402016,
7.59976791413516));
#60822=CARTESIAN_POINT('Ctrl Pts',(-0.322282627172534,2.09176494918208,
7.60024493013726));
#60823=CARTESIAN_POINT('Ctrl Pts',(-0.321951858909869,2.08323959832138,
7.60072047059375));
#60824=CARTESIAN_POINT('Ctrl Pts',(-0.320114986704937,2.05987875615432,
7.60203851720321));
#60825=CARTESIAN_POINT('Ctrl Pts',(-0.317917443161926,2.04512058209853,
7.60288873575766));
#60826=CARTESIAN_POINT('Ctrl Pts',(-0.313824600351961,2.02656930827139,
7.60401283891559));
#60827=CARTESIAN_POINT('Ctrl Pts',(-0.312866208813105,2.02258760168286,
7.60425735170267));
#60828=CARTESIAN_POINT('Ctrl Pts',(-0.311413820421765,2.01702196652574,
7.60460418843131));
#60829=CARTESIAN_POINT('Ctrl Pts',(-0.31098304858881,2.01542184134173,7.60470449569615));
#60830=CARTESIAN_POINT('Ctrl Pts',(-0.310313100591616,2.01300761512598,
7.60485676073409));
#60831=CARTESIAN_POINT('Ctrl Pts',(-0.310083013916828,2.01219100340156,
7.6049084248884));
#60832=CARTESIAN_POINT('Ctrl Pts',(-0.309651932135624,2.01068385485919,
7.60500407797423));
#60833=CARTESIAN_POINT('Ctrl Pts',(-0.309451844431036,2.00999306236091,
7.60504803722253));
#60834=CARTESIAN_POINT('Ctrl Pts',(-0.309126576618208,2.0088839977207,7.60511880426135));
#60835=CARTESIAN_POINT('Ctrl Pts',(-0.309002855106537,2.00846529742173,
7.60514556439013));
#60836=CARTESIAN_POINT('Ctrl Pts',(-0.308766157524181,2.00767021053095,
7.60519646399146));
#60837=CARTESIAN_POINT('Ctrl Pts',(-0.308653343006841,2.00729377634606,
7.60522059814218));
#60838=CARTESIAN_POINT('Ctrl Pts',(-0.308395354779793,2.00643862430486,
7.60527550576607));
#60839=CARTESIAN_POINT('Ctrl Pts',(-0.308249754647873,2.00596003707599,
7.60530629315531));
#60840=CARTESIAN_POINT('Ctrl Pts',(-0.30781487220525,2.00454244138303,7.60539766059838));
#60841=CARTESIAN_POINT('Ctrl Pts',(-0.307522411175606,2.0036044210643,7.60545834476044));
#60842=CARTESIAN_POINT('Ctrl Pts',(-0.305492471747742,1.99719699118218,
7.60587443567609));
#60843=CARTESIAN_POINT('Ctrl Pts',(-0.303613556244517,1.99177379918732,
7.6062344776727));
#60844=CARTESIAN_POINT('Ctrl Pts',(-0.301468200117906,1.98607800371821,
7.60662137106605));
#60845=CARTESIAN_POINT('Ctrl Pts',(-0.301344912325454,1.98575228346607,
7.60664352658161));
#60846=CARTESIAN_POINT('Ctrl Pts',(-0.293042496448928,1.96392464795292,
7.60813029886089));
#60847=CARTESIAN_POINT('Ctrl Pts',(-0.282586417274222,1.94336353475165,
7.60967188986564));
#60848=CARTESIAN_POINT('Ctrl Pts',(-0.265874628036835,1.91770924492085,
7.61174374413981));
#60849=CARTESIAN_POINT('Ctrl Pts',(-0.261490345514521,1.91147403405841,
7.61225964928539));
#60850=CARTESIAN_POINT('Ctrl Pts',(-0.250889714718192,1.89748026786927,
7.6134390402329));
#60851=CARTESIAN_POINT('Ctrl Pts',(-0.244526749046959,1.88984150594009,
7.61409919278889));
#60852=CARTESIAN_POINT('Ctrl Pts',(-0.23560385684265,1.88008459196654,7.61495262560708));
#60853=CARTESIAN_POINT('Ctrl Pts',(-0.233350190940766,1.87769468204636,
7.61516252906186));
#60854=CARTESIAN_POINT('Ctrl Pts',(-0.230152089300836,1.87440547723299,
7.61545210991204));
#60855=CARTESIAN_POINT('Ctrl Pts',(-0.229238223255117,1.87347691056317,
7.61553393976824));
#60856=CARTESIAN_POINT('Ctrl Pts',(-0.228115317688583,1.87234969682733,
7.61563334319043));
#60857=CARTESIAN_POINT('Ctrl Pts',(-0.227911627488441,1.87214577301291,
7.615651328959));
#60858=CARTESIAN_POINT('Ctrl Pts',(-0.227517165797678,1.87175191707393,
7.61568607123645));
#60859=CARTESIAN_POINT('Ctrl Pts',(-0.227326429468672,1.87156195028338,
7.61570283048679));
#60860=CARTESIAN_POINT('Ctrl Pts',(-0.226995609761852,1.87123328993824,
7.61573182893887));
#60861=CARTESIAN_POINT('Ctrl Pts',(-0.226855637421857,1.87109448618632,
7.61574407694198));
#60862=CARTESIAN_POINT('Ctrl Pts',(-0.226562780386366,1.87080460657884,
7.61576965793466));
#60863=CARTESIAN_POINT('Ctrl Pts',(-0.226409872381463,1.87065355570506,
7.61578298894362));
#60864=CARTESIAN_POINT('Ctrl Pts',(-0.225984988272528,1.87023467101025,
7.61581996146411));
#60865=CARTESIAN_POINT('Ctrl Pts',(-0.225712686126458,1.86996716613611,
7.61584357690281));
#60866=CARTESIAN_POINT('Ctrl Pts',(-0.224631552848655,1.86890884768716,
7.61593702607609));
#60867=CARTESIAN_POINT('Ctrl Pts',(-0.223819023335212,1.86812179900863,
7.6160065674809));
#60868=CARTESIAN_POINT('Ctrl Pts',(-0.209391213088773,1.85429294046512,
7.61722961883035));
#60869=CARTESIAN_POINT('Ctrl Pts',(-0.194659164794283,1.84246422384312,
7.61829535380736));
#60870=CARTESIAN_POINT('Ctrl Pts',(-0.167965688585287,1.82463849064139,
7.62009370560276));
#60871=CARTESIAN_POINT('Ctrl Pts',(-0.156513830330996,1.81797190364002,
7.62082906162481));
#60872=CARTESIAN_POINT('Ctrl Pts',(-0.133489201985662,1.8064036992444,7.62228830139366));
#60873=CARTESIAN_POINT('Ctrl Pts',(-0.121976232835162,1.80143692946991,
7.62300942403435));
#60874=CARTESIAN_POINT('Ctrl Pts',(-0.106731420851478,1.79588943422921,
7.62397206999624));
#60875=CARTESIAN_POINT('Ctrl Pts',(-0.103237326017269,1.79468559604599,
7.6241931708423));
#60876=CARTESIAN_POINT('Ctrl Pts',(-0.0975213145023391,1.79282556823799,
7.62455601876995));
#60877=CARTESIAN_POINT('Ctrl Pts',(-0.0953116096362679,1.79213276409057,
7.62469656347766));
#60878=CARTESIAN_POINT('Ctrl Pts',(-0.0926018226668458,1.79131513953503,
7.62486930877767));
#60879=CARTESIAN_POINT('Ctrl Pts',(-0.0921086180276386,1.79116761322408,
7.62490076574525));
#60880=CARTESIAN_POINT('Ctrl Pts',(-0.0911523278631431,1.79088406430516,
7.62496179022892));
#60881=CARTESIAN_POINT('Ctrl Pts',(-0.0906892858261045,1.79074789894379,
7.62499135299994));
#60882=CARTESIAN_POINT('Ctrl Pts',(-0.0898862006454022,1.79051369691227,
7.62504265115158));
#60883=CARTESIAN_POINT('Ctrl Pts',(-0.0895462977544971,1.79041517895375,
7.62506437079241));
#60884=CARTESIAN_POINT('Ctrl Pts',(-0.0888400215349069,1.79021173127658,
7.62510951818272));
#60885=CARTESIAN_POINT('Ctrl Pts',(-0.0884736231336985,1.79010689121468,
7.62513294881542));
#60886=CARTESIAN_POINT('Ctrl Pts',(-0.0875810556523122,1.78985320681173,
7.62519005021932));
#60887=CARTESIAN_POINT('Ctrl Pts',(-0.0870546934337768,1.78970505163731,
7.62522374336172));
#60888=CARTESIAN_POINT('Ctrl Pts',(-0.0850656938766144,1.78915066722938,
7.62535113714026));
#60889=CARTESIAN_POINT('Ctrl Pts',(-0.0836005876066289,1.78875343924163,
7.62544512964909));
#60890=CARTESIAN_POINT('Ctrl Pts',(-0.0569263426189914,1.78172329113667,
7.62715934229412));
#60891=CARTESIAN_POINT('Ctrl Pts',(-0.0310126781057647,1.77816415002519,
7.62888461008634));
#60892=CARTESIAN_POINT('Ctrl Pts',(0.0107898038386987,1.77752076425262,
7.6317106256321));
#60893=CARTESIAN_POINT('Ctrl Pts',(0.0265363553429475,1.77843330420052,
7.63278180849565));
#60894=CARTESIAN_POINT('Ctrl Pts',(0.0473904299778287,1.78118465379786,
7.63416827861842));
#60895=CARTESIAN_POINT('Ctrl Pts',(0.052609849427483,1.782004263736,7.63451243056053));
#60896=CARTESIAN_POINT('Ctrl Pts',(0.060879218885872,1.78351200927402,7.63505074558761));
#60897=CARTESIAN_POINT('Ctrl Pts',(0.063943219805935,1.78411680324568,7.63524867083693));
#60898=CARTESIAN_POINT('Ctrl Pts',(0.0674968135246448,1.78487206445999,
7.6354760530861));
#60899=CARTESIAN_POINT('Ctrl Pts',(0.0679952969282747,1.78497924640143,
7.63550789945115));
#60900=CARTESIAN_POINT('Ctrl Pts',(0.0687565049252962,1.78514480934257,
7.63555645192006));
#60901=CARTESIAN_POINT('Ctrl Pts',(0.0690194113359994,1.78520233655002,
7.63557320668361));
#60902=CARTESIAN_POINT('Ctrl Pts',(0.0694747555877969,1.78530256941549,
7.63560220014495));
#60903=CARTESIAN_POINT('Ctrl Pts',(0.0696672259412174,1.78534512221979,
7.63561444763467));
#60904=CARTESIAN_POINT('Ctrl Pts',(0.070069517538475,1.78543445110896,7.6356400303097));
#60905=CARTESIAN_POINT('Ctrl Pts',(0.0702793303757291,1.78548126039962,
7.63565336350943));
#60906=CARTESIAN_POINT('Ctrl Pts',(0.0707963099453595,1.78559714179906,
7.63568619399884));
#60907=CARTESIAN_POINT('Ctrl Pts',(0.0711034233863667,1.78566645433312,
7.635705677421));
#60908=CARTESIAN_POINT('Ctrl Pts',(0.0723030486474282,1.78593904623824,
7.63578170720328));
#60909=CARTESIAN_POINT('Ctrl Pts',(0.0731948055165846,1.78614568026774,
7.63583806258971));
#60910=CARTESIAN_POINT('Ctrl Pts',(0.0899864871920014,1.79011203591269,
7.63689637351517));
#60911=CARTESIAN_POINT('Ctrl Pts',(0.105581208741519,1.79507232211674,7.63783145380563));
#60912=CARTESIAN_POINT('Ctrl Pts',(0.137222385028771,1.80785717085118,7.63975289566128));
#60913=CARTESIAN_POINT('Ctrl Pts',(0.153130457127615,1.81587242733715,7.64073415353935));
#60914=CARTESIAN_POINT('Ctrl Pts',(0.174727180110384,1.82909696602539,7.64217534513245));
#60915=CARTESIAN_POINT('Ctrl Pts',(0.181017677694464,1.83325924299381,7.64260927791923));
#60916=CARTESIAN_POINT('Ctrl Pts',(0.194073658011579,1.84257274184813,7.64354752861949));
#60917=CARTESIAN_POINT('Ctrl Pts',(0.200792768955453,1.84777862434406,7.64405344031565));
#60918=CARTESIAN_POINT('Ctrl Pts',(0.208166112695658,1.85397290633075,7.64463905229903));
#60919=CARTESIAN_POINT('Ctrl Pts',(0.209030422120792,1.85470682057848,7.6447081899481));
#60920=CARTESIAN_POINT('Ctrl Pts',(0.210293358067197,1.85579074432932,7.64480994713881));
#60921=CARTESIAN_POINT('Ctrl Pts',(0.210695028700754,1.85613720686034,7.64484242025708));
#60922=CARTESIAN_POINT('Ctrl Pts',(0.211395994881534,1.85674485253725,7.64489928316279));
#60923=CARTESIAN_POINT('Ctrl Pts',(0.211695667121723,1.85700560101377,7.6449236548852));
#60924=CARTESIAN_POINT('Ctrl Pts',(0.212274821677775,1.85751141496069,7.64497087708462));
#60925=CARTESIAN_POINT('Ctrl Pts',(0.212554363750437,1.857756411351,7.64499372466289));
#60926=CARTESIAN_POINT('Ctrl Pts',(0.213217953092829,1.85834002760045,7.645048091906));
#60927=CARTESIAN_POINT('Ctrl Pts',(0.213601617603051,1.85867907936986,7.64507962960342));
#60928=CARTESIAN_POINT('Ctrl Pts',(0.214956805069971,1.8598824486145,7.64519139950662));
#60929=CARTESIAN_POINT('Ctrl Pts',(0.215923893206026,1.86075172144294,7.6452718397134));
#60930=CARTESIAN_POINT('Ctrl Pts',(0.232673910789583,1.87599185414803,7.64667705901706));
#60931=CARTESIAN_POINT('Ctrl Pts',(0.246992743009958,1.89188690915617,7.64807035270954));
#60932=CARTESIAN_POINT('Ctrl Pts',(0.269513355504437,1.92251242015414,7.65062206910837));
#60933=CARTESIAN_POINT('Ctrl Pts',(0.278335080892861,1.93669396118157,7.6517600312076));
#60934=CARTESIAN_POINT('Ctrl Pts',(0.29012781088824,1.95940658105974,7.65347159965461));
#60935=CARTESIAN_POINT('Ctrl Pts',(0.293906238454361,1.96748658240961,7.65406030247668));
#60936=CARTESIAN_POINT('Ctrl Pts',(0.298715390051944,1.97899207300769,7.65486129222814));
#60937=CARTESIAN_POINT('Ctrl Pts',(0.300031544497606,1.98229325613311,7.65508694159062));
#60938=CARTESIAN_POINT('Ctrl Pts',(0.301479659184068,1.98610764898124,7.65534236059185));
#60939=CARTESIAN_POINT('Ctrl Pts',(0.301665222182729,1.98660006059487,7.65537523261527));
#60940=CARTESIAN_POINT('Ctrl Pts',(0.301926520519513,1.98729862439793,7.65542172179269));
#60941=CARTESIAN_POINT('Ctrl Pts',(0.302003251182413,1.98750439950132,7.65543539825272));
#60942=CARTESIAN_POINT('Ctrl Pts',(0.302157223648336,1.9879186133441,7.65546289216664));
#60943=CARTESIAN_POINT('Ctrl Pts',(0.302234460370589,1.98812705419416,7.65547670931627));
#60944=CARTESIAN_POINT('Ctrl Pts',(0.30238331287976,1.9885300457749,7.65550338722137));
#60945=CARTESIAN_POINT('Ctrl Pts',(0.302454956426713,1.98872458521033,7.6555162496574));
#60946=CARTESIAN_POINT('Ctrl Pts',(0.302625284311501,1.98918846988976,7.65554688265321));
#60947=CARTESIAN_POINT('Ctrl Pts',(0.302723797054619,1.98945787857878,7.65556464288974));
#60948=CARTESIAN_POINT('Ctrl Pts',(0.303072787575791,1.9904162490999,7.65562771481072));
#60949=CARTESIAN_POINT('Ctrl Pts',(0.303321276580222,1.99110594034042,7.65567290849936));
#60950=CARTESIAN_POINT('Ctrl Pts',(0.306958275080049,2.00130962170744,7.65633872033921));
#60951=CARTESIAN_POINT('Ctrl Pts',(0.309900483222269,2.01097803085273,7.65693361398019));
#60952=CARTESIAN_POINT('Ctrl Pts',(0.31706126377891,2.03921108816337,7.65861076261609));
#60953=CARTESIAN_POINT('Ctrl Pts',(0.320096628769684,2.05803134278968,7.65965768632261));
#60954=CARTESIAN_POINT('Ctrl Pts',(0.32289076322274,2.09710043748009,7.66185883407635));
#60955=CARTESIAN_POINT('Ctrl Pts',(0.322440930026884,2.11727788974356,7.6630120298648));
#60956=CARTESIAN_POINT('Ctrl Pts',(0.319881450294143,2.13925543779138,7.66435018529346));
#60957=CARTESIAN_POINT('Ctrl Pts',(0.319633091555802,2.14122885089238,7.66447103743562));
#60958=CARTESIAN_POINT('Ctrl Pts',(0.31927785080493,2.14385506622871,7.66463283617608));
#60959=CARTESIAN_POINT('Ctrl Pts',(0.319187199544413,2.14451004926154,7.66467326951541));
#60960=CARTESIAN_POINT('Ctrl Pts',(0.319035159339379,2.14558423219985,7.66473971449814));
#60961=CARTESIAN_POINT('Ctrl Pts',(0.318974958047902,2.14600360046319,7.66476568852064));
#60962=CARTESIAN_POINT('Ctrl Pts',(0.318856773448181,2.14681550058235,7.66481603970489));
#60963=CARTESIAN_POINT('Ctrl Pts',(0.318798891776286,2.14720804665027,7.66484041360587));
#60964=CARTESIAN_POINT('Ctrl Pts',(0.318663679155768,2.14811345151512,7.66489670055097));
#60965=CARTESIAN_POINT('Ctrl Pts',(0.318585834954727,2.1486262315111,7.6649286298051));
#60966=CARTESIAN_POINT('Ctrl Pts',(0.318332984257065,2.15026515276589,7.66503084457905));
#60967=CARTESIAN_POINT('Ctrl Pts',(0.318153243375403,2.15139054509174,7.66510128000994));
#60968=CARTESIAN_POINT('Ctrl Pts',(0.316459783595278,2.16164410621306,7.66574532391633));
#60969=CARTESIAN_POINT('Ctrl Pts',(0.314559713562472,2.17070324404687,7.66633117520644));
#60970=CARTESIAN_POINT('Ctrl Pts',(0.310352786517696,2.18719315707374,7.6674302968538));
#60971=CARTESIAN_POINT('Ctrl Pts',(0.308161508710353,2.19464654772916,7.66793972644221));
#60972=CARTESIAN_POINT('Ctrl Pts',(0.298538275863968,2.22348455142405,7.66995762257628));
#60973=CARTESIAN_POINT('Ctrl Pts',(0.289131803603431,2.24413963968149,7.67151123890643));
#60974=CARTESIAN_POINT('Ctrl Pts',(0.272619389909045,2.27215573413383,7.67367717072749));
#60975=CARTESIAN_POINT('Ctrl Pts',(0.26720929408885,2.28043880847528,7.67432480367485));
#60976=CARTESIAN_POINT('Ctrl Pts',(0.260867972785904,2.28923527152023,7.67501013469854));
#60977=CARTESIAN_POINT('Ctrl Pts',(0.260306192193256,2.29000729873281,7.67507026059871));
#60978=CARTESIAN_POINT('Ctrl Pts',(0.259325266363233,2.29134282065335,7.67517421604834));
#60979=CARTESIAN_POINT('Ctrl Pts',(0.258907698395762,2.29190745822746,7.67521814934222));
#60980=CARTESIAN_POINT('Ctrl Pts',(0.258308662744803,2.29271196338546,7.67528071589409));
#60981=CARTESIAN_POINT('Ctrl Pts',(0.258128703517364,2.29295294375339,7.6752994530861));
#60982=CARTESIAN_POINT('Ctrl Pts',(0.257814694324563,2.2933722026742,7.67533204482165));
#60983=CARTESIAN_POINT('Ctrl Pts',(0.257680796320666,2.29355059438157,7.6753459100532));
#60984=CARTESIAN_POINT('Ctrl Pts',(0.257422744005917,2.29389365389967,7.67537256916636));
#60985=CARTESIAN_POINT('Ctrl Pts',(0.257298617096428,2.29405834121462,7.67538536494083));
#60986=CARTESIAN_POINT('Ctrl Pts',(0.257003954595633,2.29444850956187,7.67541567542274));
#60987=CARTESIAN_POINT('Ctrl Pts',(0.256833279880444,2.29467388601427,7.675433180306));
#60988=CARTESIAN_POINT('Ctrl Pts',(0.256233593242599,2.29546361262195,7.67549450638565));
#60989=CARTESIAN_POINT('Ctrl Pts',(0.255803011989643,2.29602677685642,7.67553821796193));
#60990=CARTESIAN_POINT('Ctrl Pts',(0.250117198696013,2.3034127085152,7.6761112905374));
#60991=CARTESIAN_POINT('Ctrl Pts',(0.244591840034279,2.31002429735919,7.67662196977456));
#60992=CARTESIAN_POINT('Ctrl Pts',(0.218866253677617,2.33841275828205,7.6788445624055));
#60993=CARTESIAN_POINT('Ctrl Pts',(0.195978364654515,2.3575574639317,7.68043916532117));
#60994=CARTESIAN_POINT('Ctrl Pts',(0.161446403587191,2.37913732276244,7.68278696891977));
#60995=CARTESIAN_POINT('Ctrl Pts',(0.151809872449005,2.38449307467799,7.68343513773508));
#60996=CARTESIAN_POINT('Ctrl Pts',(0.140136153002332,2.39021884200434,7.68422152465313));
#60997=CARTESIAN_POINT('Ctrl Pts',(0.138345570024417,2.39107665762414,7.68434216549759));
#60998=CARTESIAN_POINT('Ctrl Pts',(0.135949624369565,2.39219738276677,7.68450365968567));
#60999=CARTESIAN_POINT('Ctrl Pts',(0.135351189781173,2.39247506949584,7.68454400152066));
#61000=CARTESIAN_POINT('Ctrl Pts',(0.134367356869488,2.3929279232953,7.68461033453553));
#61001=CARTESIAN_POINT('Ctrl Pts',(0.133982456554868,2.39310417289934,7.684636288343));
#61002=CARTESIAN_POINT('Ctrl Pts',(0.133235995958048,2.39344420689029,7.68468662775838));
#61003=CARTESIAN_POINT('Ctrl Pts',(0.132874477993955,2.39360808277702,7.6847110101623));
#61004=CARTESIAN_POINT('Ctrl Pts',(0.132039126491449,2.39398488831605,7.6847673563651));
#61005=CARTESIAN_POINT('Ctrl Pts',(0.131565079966595,2.3941973405916,7.68479933648259));
#61006=CARTESIAN_POINT('Ctrl Pts',(0.130292630787299,2.39476392052288,7.68488519210596));
#61007=CARTESIAN_POINT('Ctrl Pts',(0.129493302917554,2.39511594832361,7.68493913936043));
#61008=CARTESIAN_POINT('Ctrl Pts',(0.123833053926022,2.39758132535605,7.68532126866551));
#61009=CARTESIAN_POINT('Ctrl Pts',(0.118922321009848,2.39957761367977,7.68565341456002));
#61010=CARTESIAN_POINT('Ctrl Pts',(0.112486785114604,2.4020105885899,7.68608982877782));
#61011=CARTESIAN_POINT('Ctrl Pts',(0.111004680896542,2.40255847885103,7.68619041031641));
#61012=CARTESIAN_POINT('Ctrl Pts',(0.104348801382813,2.40496347310704,7.6866424533139));
#61013=CARTESIAN_POINT('Ctrl Pts',(0.099132284114397,2.40669883751386,7.68699770113815));
#61014=CARTESIAN_POINT('Ctrl Pts',(0.0658731152984475,2.41682591571437,
7.68926820793129));
#61015=CARTESIAN_POINT('Ctrl Pts',(0.0368463247491426,2.42149631890393,
7.69129150223799));
#61016=CARTESIAN_POINT('Ctrl Pts',(-0.000754476213337938,2.42238220977441,
7.69378110817522));
#61017=CARTESIAN_POINT('Ctrl Pts',(-0.00910512026353613,2.42225453034135,
7.69432447945846));
#61018=CARTESIAN_POINT('Ctrl Pts',(-0.01874709040981,2.4217319228053,7.69493398291066));
#61019=CARTESIAN_POINT('Ctrl Pts',(-0.0200516356364027,2.42165325367172,
7.69501606672404));
#61020=CARTESIAN_POINT('Ctrl Pts',(-0.0217428297209001,2.42154093909962,
7.69512195306316));
#61021=CARTESIAN_POINT('Ctrl Pts',(-0.0221299227381875,2.42151452950793,
7.69514615335335));
#61022=CARTESIAN_POINT('Ctrl Pts',(-0.0227565565787065,2.4214706400921,
7.69518527032531));
#61023=CARTESIAN_POINT('Ctrl Pts',(-0.022996125731761,2.42145359153504,
7.69520021123239));
#61024=CARTESIAN_POINT('Ctrl Pts',(-0.0234556528949428,2.4214203736771,
7.695228842928));
#61025=CARTESIAN_POINT('Ctrl Pts',(-0.0236756126656092,2.42140424644455,
7.69524253599996));
#61026=CARTESIAN_POINT('Ctrl Pts',(-0.0241815579501206,2.4213666288356,
7.69527400524159));
#61027=CARTESIAN_POINT('Ctrl Pts',(-0.024467532290785,2.42134498243971,
7.695291772572));
#61028=CARTESIAN_POINT('Ctrl Pts',(-0.025353559332595,2.42127672634035,
7.69534675983841));
#61029=CARTESIAN_POINT('Ctrl Pts',(-0.0259535150184322,2.42122881709272,
7.69538390695073));
#61030=CARTESIAN_POINT('Ctrl Pts',(-0.0309211943292435,2.4208181165863,
7.69569079793071));
#61031=CARTESIAN_POINT('Ctrl Pts',(-0.0352814940747872,2.42036792129348,
7.69595574847398));
#61032=CARTESIAN_POINT('Ctrl Pts',(-0.0398140977481186,2.41980626494128,
7.69622781639151));
#61033=CARTESIAN_POINT('Ctrl Pts',(-0.0399966664845369,2.41978348322828,
7.69623876933111));
#61034=CARTESIAN_POINT('Ctrl Pts',(-0.0685396888196573,2.41619693611508,
7.69795029059364));
#61035=CARTESIAN_POINT('Ctrl Pts',(-0.0963035101548373,2.40887582910447,
7.69948957840477));
#61036=CARTESIAN_POINT('Ctrl Pts',(-0.13730168874294,2.39198876011352,7.70200256126843));
#61037=CARTESIAN_POINT('Ctrl Pts',(-0.151402187655715,2.38493239541957,
7.70291419626693));
#61038=CARTESIAN_POINT('Ctrl Pts',(-0.167059228957503,2.3756057605764,7.70401332021529));
#61039=CARTESIAN_POINT('Ctrl Pts',(-0.169174272798061,2.3743125701388,7.70416369835424));
#61040=CARTESIAN_POINT('Ctrl Pts',(-0.171876080648981,2.37261748563579,
7.70435833660206));
#61041=CARTESIAN_POINT('Ctrl Pts',(-0.172476764307002,2.37223784882908,
7.70440177327053));
#61042=CARTESIAN_POINT('Ctrl Pts',(-0.173442855206537,2.371622790916,7.70447189920152));
#61043=CARTESIAN_POINT('Ctrl Pts',(-0.173809052608442,2.37138861029088,
7.70449854234858));
#61044=CARTESIAN_POINT('Ctrl Pts',(-0.174505763414764,2.3709410801583,7.70454935092744));
#61045=CARTESIAN_POINT('Ctrl Pts',(-0.174836362388252,2.37072786477749,
7.70457351132938));
#61046=CARTESIAN_POINT('Ctrl Pts',(-0.175589406401248,2.37024024449193,
7.70462866124025));
#61047=CARTESIAN_POINT('Ctrl Pts',(-0.176011599351105,2.36996545385044,
7.70465966512925));
#61048=CARTESIAN_POINT('Ctrl Pts',(-0.177297957180039,2.36912390826298,
7.70475438769765));
#61049=CARTESIAN_POINT('Ctrl Pts',(-0.178160035407185,2.36855398966096,
7.70481822490645));
#61050=CARTESIAN_POINT('Ctrl Pts',(-0.184431644300477,2.36436435014612,
7.70528527566721));
#61051=CARTESIAN_POINT('Ctrl Pts',(-0.18973281568978,2.36058585866802,7.70569447673474));
#61052=CARTESIAN_POINT('Ctrl Pts',(-0.196355075678692,2.35555650413883,
7.7062250027743));
#61053=CARTESIAN_POINT('Ctrl Pts',(-0.197785238188114,2.35445125643444,
7.70634076801978));
#61054=CARTESIAN_POINT('Ctrl Pts',(-0.204139354505823,2.34945477802752,
7.70686047278658));
#61055=CARTESIAN_POINT('Ctrl Pts',(-0.208958066600866,2.34543243628884,
7.70726920031167));
#61056=CARTESIAN_POINT('Ctrl Pts',(-0.231300447782583,2.32564737507268,
7.70923411880967));
#61057=CARTESIAN_POINT('Ctrl Pts',(-0.247176887376128,2.30813467009008,
7.71084974170074));
#61058=CARTESIAN_POINT('Ctrl Pts',(-0.266191809007985,2.28188300157065,
7.71301940431304));
#61059=CARTESIAN_POINT('Ctrl Pts',(-0.271086553062576,2.27450390153318,
7.71360463705952));
#61060=CARTESIAN_POINT('Ctrl Pts',(-0.277691097829145,2.26359715716246,
7.71442550875905));
#61061=CARTESIAN_POINT('Ctrl Pts',(-0.279649990149578,2.26022565977059,
7.71467344857037));
#61062=CARTESIAN_POINT('Ctrl Pts',(-0.281809978508257,2.25634769904972,
7.71495137026948));
#61063=CARTESIAN_POINT('Ctrl Pts',(-0.282071451878627,2.25587547283041,
7.71498509223173));
#61064=CARTESIAN_POINT('Ctrl Pts',(-0.282463461444175,2.25516327913916,
7.71503576575282));
#61065=CARTESIAN_POINT('Ctrl Pts',(-0.282594879330144,2.2549238019865,7.71505277351064));
#61066=CARTESIAN_POINT('Ctrl Pts',(-0.282830805813152,2.25449258426823,
7.71508334196713));
#61067=CARTESIAN_POINT('Ctrl Pts',(-0.282935423783227,2.25430090498878,
7.71509690968145));
#61068=CARTESIAN_POINT('Ctrl Pts',(-0.283159748678892,2.25388890545698,
7.71512602903156));
#61069=CARTESIAN_POINT('Ctrl Pts',(-0.28327939296606,2.25366855246422,7.71514157660566));
#61070=CARTESIAN_POINT('Ctrl Pts',(-0.283600758804313,2.25307503119626,
7.71518338319139));
#61071=CARTESIAN_POINT('Ctrl Pts',(-0.283802001821224,2.25270160227473,
7.715209611588));
#61072=CARTESIAN_POINT('Ctrl Pts',(-0.284723167831009,2.25098416461056,
7.71532989823764));
#61073=CARTESIAN_POINT('Ctrl Pts',(-0.28543430007864,2.24963542634218,7.71542340556752));
#61074=CARTESIAN_POINT('Ctrl Pts',(-0.300856923577085,2.21987473000819,
7.71746687796392));
#61075=CARTESIAN_POINT('Ctrl Pts',(-0.311268623925318,2.18942870693895,
7.71917530570832));
#61076=CARTESIAN_POINT('Ctrl Pts',(-0.320075159774721,2.14124543488957,
7.72195175980088));
#61077=CARTESIAN_POINT('Ctrl Pts',(-0.321802671577201,2.12433537806756,
7.72293636262128));
#61078=CARTESIAN_POINT('Ctrl Pts',(-0.322224436732959,2.10589581504815,
7.72405550158802));
#61079=CARTESIAN_POINT('Ctrl Pts',(-0.322248031643791,2.1044220189982,7.72414524873119));
#61080=CARTESIAN_POINT('Ctrl Pts',(-0.322266841072826,2.10236595246547,
7.72427088711324));
#61081=CARTESIAN_POINT('Ctrl Pts',(-0.322270589364442,2.10178376282133,
7.72430651099395));
#61082=CARTESIAN_POINT('Ctrl Pts',(-0.322274276684768,2.10079478700175,
7.72436710941423));
#61083=CARTESIAN_POINT('Ctrl Pts',(-0.322275023155283,2.10038800376921,
7.72439205861316));
#61084=CARTESIAN_POINT('Ctrl Pts',(-0.322274975684238,2.09957330169344,
7.72444207515811));
#61085=CARTESIAN_POINT('Ctrl Pts',(-0.322274177427816,2.09916538361351,
7.72446714259294));
#61086=CARTESIAN_POINT('Ctrl Pts',(-0.322270338419107,2.09816966763754,
7.72452839141201));
#61087=CARTESIAN_POINT('Ctrl Pts',(-0.322266463987034,2.09758187607652,
7.72456459884681));
#61088=CARTESIAN_POINT('Ctrl Pts',(-0.322246901720612,2.09548461458602,
7.7246939723881));
#61089=CARTESIAN_POINT('Ctrl Pts',(-0.322222216542256,2.09397526630236,
7.72478741982268));
#61090=CARTESIAN_POINT('Ctrl Pts',(-0.321749558177897,2.07376186946427,
7.72604356066092));
#61091=CARTESIAN_POINT('Ctrl Pts',(-0.31968436819104,2.05513463260738,7.72725805362947));
#61092=CARTESIAN_POINT('Ctrl Pts',(-0.310084166221126,2.00713544075561,
7.73052644916394));
#61093=CARTESIAN_POINT('Ctrl Pts',(-0.300006792080827,1.97845991596012,
7.73262950984543));
#61094=CARTESIAN_POINT('Ctrl Pts',(-0.285390834993922,1.95028198303144,
7.73463711044471));
#61095=CARTESIAN_POINT('Ctrl Pts',(-0.284692807219456,1.94895888299198,
7.73473119228828));
#61096=CARTESIAN_POINT('Ctrl Pts',(-0.28378412276943,1.94726516812631,7.73485134174637));
#61097=CARTESIAN_POINT('Ctrl Pts',(-0.283581923420975,1.9468900724403,7.73487793232737));
#61098=CARTESIAN_POINT('Ctrl Pts',(-0.283260531620537,1.9462966860919,7.73491996750274));
#61099=CARTESIAN_POINT('Ctrl Pts',(-0.283141830321619,1.94607813214683,
7.73493544327615));
#61100=CARTESIAN_POINT('Ctrl Pts',(-0.282928771256614,1.94568692624474,
7.73496313260724));
#61101=CARTESIAN_POINT('Ctrl Pts',(-0.282834509062742,1.94551422453788,
7.7349753521463));
#61102=CARTESIAN_POINT('Ctrl Pts',(-0.282612635268746,1.94510860402726,
7.73500404214789));
#61103=CARTESIAN_POINT('Ctrl Pts',(-0.282484894055848,1.94487575691916,
7.73502050416059));
#61104=CARTESIAN_POINT('Ctrl Pts',(-0.282114144152394,1.94420192937727,
7.73506812192688));
#61105=CARTESIAN_POINT('Ctrl Pts',(-0.28187038827982,1.9437613576617,7.73509922993938));
#61106=CARTESIAN_POINT('Ctrl Pts',(-0.280189839225027,1.94074061647781,
7.73531235229594));
#61107=CARTESIAN_POINT('Ctrl Pts',(-0.27871861205453,1.93817962418204,7.73549220017288));
#61108=CARTESIAN_POINT('Ctrl Pts',(-0.273994511379368,1.93021192009098,
7.7360502531131));
#61109=CARTESIAN_POINT('Ctrl Pts',(-0.270617787235335,1.92488001687209,
7.7364215247782));
#61110=CARTESIAN_POINT('Ctrl Pts',(-0.258383994817622,1.90676254116668,
7.73768775441519));
#61111=CARTESIAN_POINT('Ctrl Pts',(-0.248759537234503,1.89452065582141,
7.73855244538971));
#61112=CARTESIAN_POINT('Ctrl Pts',(-0.227423412915464,1.87108914866398,
7.74032418162177));
#61113=CARTESIAN_POINT('Ctrl Pts',(-0.215678380409823,1.85999090158165,
7.74122950041062));
#61114=CARTESIAN_POINT('Ctrl Pts',(-0.19553047000612,1.84363032168451,7.74273954613139));
#61115=CARTESIAN_POINT('Ctrl Pts',(-0.187630317063021,1.83779318982994,
7.74332203418941));
#61116=CARTESIAN_POINT('Ctrl Pts',(-0.178611654321421,1.83174613306845,
7.74398229859104));
#61117=CARTESIAN_POINT('Ctrl Pts',(-0.177743876704504,1.83117036168348,
7.74404578045392));
#61118=CARTESIAN_POINT('Ctrl Pts',(-0.176441835193752,1.83031551608606,
7.74414096390663));
#61119=CARTESIAN_POINT('Ctrl Pts',(-0.176009660903805,1.83003325883712,
7.74417254630693));
#61120=CARTESIAN_POINT('Ctrl Pts',(-0.175264190211969,1.82954893559221,
7.74422700574909));
#61121=CARTESIAN_POINT('Ctrl Pts',(-0.174951216939581,1.82934637209262,
7.74424986417901));
#61122=CARTESIAN_POINT('Ctrl Pts',(-0.174304563642449,1.82892943350893,
7.74429708250409));
#61123=CARTESIAN_POINT('Ctrl Pts',(-0.173970838069511,1.82871513049273,
7.74432144503122));
#61124=CARTESIAN_POINT('Ctrl Pts',(-0.173193129765183,1.82821774766822,
7.74437820564126));
#61125=CARTESIAN_POINT('Ctrl Pts',(-0.172748848121884,1.82793513944702,
7.74441062115514));
#61126=CARTESIAN_POINT('Ctrl Pts',(-0.171330767636939,1.82703797030089,
7.74451405575814));
#61127=CARTESIAN_POINT('Ctrl Pts',(-0.17035437494087,1.82642754436919,7.74458522750354));
#61128=CARTESIAN_POINT('Ctrl Pts',(-0.149232484045475,1.81337937984627,
7.74612395229316));
#61129=CARTESIAN_POINT('Ctrl Pts',(-0.12778487432275,1.80319652752802,7.74767705029028));
#61130=CARTESIAN_POINT('Ctrl Pts',(-0.0841474590898502,1.78809112455826,
7.7507879369035));
#61131=CARTESIAN_POINT('Ctrl Pts',(-0.0621607463559797,1.78297621808199,
7.75233154489361));
#61132=CARTESIAN_POINT('Ctrl Pts',(-0.0393030596261878,1.78013015745656,
7.75382047173914));
#61133=CARTESIAN_POINT('Ctrl Pts',(-0.0387862756358132,1.78006708282181,
7.75385407231093));
#61134=CARTESIAN_POINT('Ctrl Pts',(-0.0343386619931378,1.77953517648902,
7.75414270215606));
#61135=CARTESIAN_POINT('Ctrl Pts',(-0.0303994324227468,1.7791375296862,
7.75439466285182));
#61136=CARTESIAN_POINT('Ctrl Pts',(-0.0258636736898057,1.77876395523703,
7.75467979869705));
#61137=CARTESIAN_POINT('Ctrl Pts',(-0.0252735476693131,1.77871698788587,
7.75471679961649));
#61138=CARTESIAN_POINT('Ctrl Pts',(-0.0244004638428416,1.77864992072209,
7.75477139556526));
#61139=CARTESIAN_POINT('Ctrl Pts',(-0.0241176077816137,1.77862856834492,
7.75478906048402));
#61140=CARTESIAN_POINT('Ctrl Pts',(-0.0236158733734507,1.77859135931309,
7.75482035404235));
#61141=CARTESIAN_POINT('Ctrl Pts',(-0.023397007028472,1.77857535277048,
7.75483399113954));
#61142=CARTESIAN_POINT('Ctrl Pts',(-0.0229345523295774,1.77854200652439,
7.7548627765025));
#61143=CARTESIAN_POINT('Ctrl Pts',(-0.0226909612358904,1.77852472017422,
7.75487792169359));
#61144=CARTESIAN_POINT('Ctrl Pts',(-0.0220423638416082,1.77847943357468,
7.75491820312795));
#61145=CARTESIAN_POINT('Ctrl Pts',(-0.0216373222189689,1.77845192158921,
7.75494331183649));
#61146=CARTESIAN_POINT('Ctrl Pts',(-0.0197533042653283,1.77832752784366,
7.7550598907854));
#61147=CARTESIAN_POINT('Ctrl Pts',(-0.0182736920653518,1.77824008212772,
7.75515083806837));
#61148=CARTESIAN_POINT('Ctrl Pts',(-0.00646758888353097,1.77762403844278,
7.75587205036314));
#61149=CARTESIAN_POINT('Ctrl Pts',(0.0038794469008034,1.77758243324402,
7.75647691100931));
#61150=CARTESIAN_POINT('Ctrl Pts',(0.0435014725895693,1.77933137914622,
7.75874871504159));
#61151=CARTESIAN_POINT('Ctrl Pts',(0.0724776566637045,1.78461470851599,
7.76033005174923));
#61152=CARTESIAN_POINT('Ctrl Pts',(0.109685900557101,1.79680554651173,7.76260798048083));
#61153=CARTESIAN_POINT('Ctrl Pts',(0.118884766532973,1.80029304965327,7.76319133893898));
#61154=CARTESIAN_POINT('Ctrl Pts',(0.128865459385863,1.80460881123032,7.76385254375402));
#61155=CARTESIAN_POINT('Ctrl Pts',(0.129819694152113,1.80502693683003,7.76391605012076));
#61156=CARTESIAN_POINT('Ctrl Pts',(0.13124374586941,1.80565917485821,7.76401126434545));
#61157=CARTESIAN_POINT('Ctrl Pts',(0.13171510941765,1.80586980413228,7.76404285290647));
#61158=CARTESIAN_POINT('Ctrl Pts',(0.132525991113844,1.80623448754287,7.76409732014512));
#61159=CARTESIAN_POINT('Ctrl Pts',(0.132865752816791,1.8063880003194,7.76412018019851));
#61160=CARTESIAN_POINT('Ctrl Pts',(0.133566378863496,1.80670602571804,7.76416739923939));
#61161=CARTESIAN_POINT('Ctrl Pts',(0.133927207328215,1.80687061551613,7.76419176085427));
#61162=CARTESIAN_POINT('Ctrl Pts',(0.134766306408868,1.80725523840757,7.76424851483342));
#61163=CARTESIAN_POINT('Ctrl Pts',(0.135244342480983,1.80747577774731,7.76428092461616));
#61164=CARTESIAN_POINT('Ctrl Pts',(0.136732234250004,1.8081666353005,7.76438204177389));
#61165=CARTESIAN_POINT('Ctrl Pts',(0.137740185050097,1.80864101522819,7.76445088945287));
#61166=CARTESIAN_POINT('Ctrl Pts',(0.143828822133454,1.81154521506301,7.76486890237278));
#61167=CARTESIAN_POINT('Ctrl Pts',(0.14884728945677,1.81410251664506,7.76522248547441));
#61168=CARTESIAN_POINT('Ctrl Pts',(0.166135537625027,1.82349081874894,7.76647356544263));
#61169=CARTESIAN_POINT('Ctrl Pts',(0.178022466737198,1.83099022604891,7.76739422079178));
#61170=CARTESIAN_POINT('Ctrl Pts',(0.211479762072975,1.85528914297911,7.77015802566485));
#61171=CARTESIAN_POINT('Ctrl Pts',(0.231447870817435,1.87408188193071,7.77204784094079));
#61172=CARTESIAN_POINT('Ctrl Pts',(0.251178104135047,1.89804788902278,7.77404508414141));
#61173=CARTESIAN_POINT('Ctrl Pts',(0.253499323255273,1.90096937117097,7.77428230650393));
#61174=CARTESIAN_POINT('Ctrl Pts',(0.256123343070602,1.90439236414173,7.77455249206801));
#61175=CARTESIAN_POINT('Ctrl Pts',(0.256476034371073,1.9048550336863,7.77458885072494));
#61176=CARTESIAN_POINT('Ctrl Pts',(0.256997610600598,1.9055431073641,7.77464268096086));
#61177=CARTESIAN_POINT('Ctrl Pts',(0.257167453526111,1.9057677786865,7.77466021963864));
#61178=CARTESIAN_POINT('Ctrl Pts',(0.25746896459633,1.90616771180441,7.77469137180001));
#61179=CARTESIAN_POINT('Ctrl Pts',(0.257600748396059,1.90634288522152,7.77470499346462));
#61180=CARTESIAN_POINT('Ctrl Pts',(0.257879642140193,1.90671439271894,7.77473383303792));
#61181=CARTESIAN_POINT('Ctrl Pts',(0.258026706241336,1.90691075980373,7.77474904769641));
#61182=CARTESIAN_POINT('Ctrl Pts',(0.258414618013022,1.90742995288603,7.77478919908587));
#61183=CARTESIAN_POINT('Ctrl Pts',(0.258655085941057,1.90775306408344,7.77481410910981));
#61184=CARTESIAN_POINT('Ctrl Pts',(0.259758560345059,1.90924159539474,7.77492851451173));
#61185=CARTESIAN_POINT('Ctrl Pts',(0.260614317756808,1.91041240503098,7.77501751045227));
#61186=CARTESIAN_POINT('Ctrl Pts',(0.267325429512785,1.91972556388609,7.77571797421593));
#61187=CARTESIAN_POINT('Ctrl Pts',(0.272806346021825,1.92813232211608,7.77630552164729));
#61188=CARTESIAN_POINT('Ctrl Pts',(0.289315307935573,1.95623963039215,7.77817544973955));
#61189=CARTESIAN_POINT('Ctrl Pts',(0.298669039715419,1.97684442666317,7.77940730875144));
#61190=CARTESIAN_POINT('Ctrl Pts',(0.311068185546339,2.01411116006017,7.78163674768107));
#61191=CARTESIAN_POINT('Ctrl Pts',(0.315101211316615,2.03034789996888,7.78260776830101));
#61192=CARTESIAN_POINT('Ctrl Pts',(0.318067016899126,2.04807542151478,7.78369965197339));
#61193=CARTESIAN_POINT('Ctrl Pts',(0.318269200547256,2.0493294464078,7.78377704731128));
#61194=CARTESIAN_POINT('Ctrl Pts',(0.318541685889781,2.05108551429919,7.78388565704629));
#61195=CARTESIAN_POINT('Ctrl Pts',(0.318618226389089,2.05158658895598,7.78391667373389));
#61196=CARTESIAN_POINT('Ctrl Pts',(0.318748647138123,2.05245409849474,7.7839704187687));
#61197=CARTESIAN_POINT('Ctrl Pts',(0.318803078585654,2.05282045056614,7.78399312962639));
#61198=CARTESIAN_POINT('Ctrl Pts',(0.318914699932508,2.05358073411826,7.78404029074662));
#61199=CARTESIAN_POINT('Ctrl Pts',(0.318971791732013,2.05397467919619,7.78406474407294));
#61200=CARTESIAN_POINT('Ctrl Pts',(0.319103971868309,2.05489880825572,7.78412214670083));
#61201=CARTESIAN_POINT('Ctrl Pts',(0.319178468800585,2.05542907441529,7.78415511464611));
#61202=CARTESIAN_POINT('Ctrl Pts',(0.319411080886695,2.05711529111568,7.7842600484781));
#61203=CARTESIAN_POINT('Ctrl Pts',(0.319564239165475,2.05827190588451,7.78433217077017));
#61204=CARTESIAN_POINT('Ctrl Pts',(0.319907435102527,2.06097640924704,7.78450116414507));
#61205=CARTESIAN_POINT('Ctrl Pts',(0.320092523125963,2.06252488598625,7.78459818993511));
#61206=CARTESIAN_POINT('Ctrl Pts',(0.32188521623478,2.07850632743434,7.785602416623));
#61207=CARTESIAN_POINT('Ctrl Pts',(0.322526540231538,2.09302887188142,7.78654007058299));
#61208=CARTESIAN_POINT('Ctrl Pts',(0.321674641207534,2.12941387095035,7.78894944602776));
#61209=CARTESIAN_POINT('Ctrl Pts',(0.318936951345095,2.1511747464266,7.79044779904293));
#61210=CARTESIAN_POINT('Ctrl Pts',(0.312848697030029,2.17754900199409,7.79225948446135));
#61211=CARTESIAN_POINT('Ctrl Pts',(0.311558161917351,2.18258130013824,7.7926046746758));
#61212=CARTESIAN_POINT('Ctrl Pts',(0.309412804020751,2.19017860799573,7.79312308482443));
#61213=CARTESIAN_POINT('Ctrl Pts',(0.308646468176721,2.19276757615912,7.7932992553002));
#61214=CARTESIAN_POINT('Ctrl Pts',(0.307788388571434,2.19553807424186,7.79348703670735));
#61215=CARTESIAN_POINT('Ctrl Pts',(0.307728932355303,2.19572941011571,7.7935000014288));
#61216=CARTESIAN_POINT('Ctrl Pts',(0.307591503259304,2.19617021921587,7.79352986120156));
#61217=CARTESIAN_POINT('Ctrl Pts',(0.307513405134188,2.1964196536242,7.79354675088289));
#61218=CARTESIAN_POINT('Ctrl Pts',(0.306153450925803,2.20074469634268,7.79383948928161));
#61219=CARTESIAN_POINT('Ctrl Pts',(0.304790898013345,2.20479476246311,7.79411179324649));
#61220=CARTESIAN_POINT('Ctrl Pts',(0.303164109932842,2.20932975390627,7.79441369604927));
#61221=CARTESIAN_POINT('Ctrl Pts',(0.302978790013457,2.20984227534452,7.79444777184432));
#61222=CARTESIAN_POINT('Ctrl Pts',(0.302696833853365,2.21061591167039,7.79449913950461));
#61223=CARTESIAN_POINT('Ctrl Pts',(0.302601159055137,2.21087737226075,7.79451648799274));
#61224=CARTESIAN_POINT('Ctrl Pts',(0.302434407635974,2.21133124798399,7.7945465825807));
#61225=CARTESIAN_POINT('Ctrl Pts',(0.302363486115709,2.21152371929007,7.79455933795447));
#61226=CARTESIAN_POINT('Ctrl Pts',(0.3022147513561,2.21192618030643,7.79458599569032));
#61227=CARTESIAN_POINT('Ctrl Pts',(0.302136903039917,2.21213615651077,7.79459989585083));
#61228=CARTESIAN_POINT('Ctrl Pts',(0.301981259876219,2.21255462598113,7.79462758236381));
#61229=CARTESIAN_POINT('Ctrl Pts',(0.301903467707945,2.21276312044642,7.79464136889677));
#61230=CARTESIAN_POINT('Ctrl Pts',(0.301631485066761,2.21348977504726,7.79468939189644));
#61231=CARTESIAN_POINT('Ctrl Pts',(0.301436174642718,2.21400751927559,7.79472356151797));
#61232=CARTESIAN_POINT('Ctrl Pts',(0.299666496691615,2.21866238118381,7.79503036792827));
#61233=CARTESIAN_POINT('Ctrl Pts',(0.298008286421634,2.22276740592593,7.79529808048655));
#61234=CARTESIAN_POINT('Ctrl Pts',(0.292937673050119,2.23461132767112,7.79606574579406));
#61235=CARTESIAN_POINT('Ctrl Pts',(0.289304453078017,2.2422520476952,7.79655501470293));
#61236=CARTESIAN_POINT('Ctrl Pts',(0.277746558924407,2.2642788663434,7.79797239992448));
#61237=CARTESIAN_POINT('Ctrl Pts',(0.269018651123098,2.27821251223945,7.79887907141783));
#61238=CARTESIAN_POINT('Ctrl Pts',(0.246707911063124,2.30843092604645,7.80098954235841));
#61239=CARTESIAN_POINT('Ctrl Pts',(0.232507740680082,2.32416108773845,7.80220099347435));
#61240=CARTESIAN_POINT('Ctrl Pts',(0.215909414530784,2.33926134355247,7.80356386064021));
#61241=CARTESIAN_POINT('Ctrl Pts',(0.214942481842434,2.34013037130609,7.80364306359823));
#61242=CARTESIAN_POINT('Ctrl Pts',(0.213587487072899,2.34133342723037,7.80375380032486));
#61243=CARTESIAN_POINT('Ctrl Pts',(0.213203838107999,2.34167242528703,7.80378512596495));
#61244=CARTESIAN_POINT('Ctrl Pts',(0.212540261190554,2.34225596206613,7.80383926077788));
#61245=CARTESIAN_POINT('Ctrl Pts',(0.212260714144713,2.34250093404446,7.80386205185047));
#61246=CARTESIAN_POINT('Ctrl Pts',(0.211681533731948,2.34300671122778,7.80390924207554));
#61247=CARTESIAN_POINT('Ctrl Pts',(0.211381840817271,2.34326744705232,7.80393364405347));
#61248=CARTESIAN_POINT('Ctrl Pts',(0.210680797992579,2.34387508771395,7.80399068775535));
#61249=CARTESIAN_POINT('Ctrl Pts',(0.210279072955018,2.34422155621912,7.8040233474448));
#61250=CARTESIAN_POINT('Ctrl Pts',(0.209015848393551,2.34530559908987,7.80412595773305));
#61251=CARTESIAN_POINT('Ctrl Pts',(0.208151316940547,2.34603961272067,7.80419605459133));
#61252=CARTESIAN_POINT('Ctrl Pts',(0.200781098066636,2.35223050530183,7.80479258925983));
#61253=CARTESIAN_POINT('Ctrl Pts',(0.194066507643606,2.35743241013519,7.80532930185445));
#61254=CARTESIAN_POINT('Ctrl Pts',(0.181019659289397,2.36673929792265,7.80636118000203));
#61255=CARTESIAN_POINT('Ctrl Pts',(0.174733230890601,2.37089897509574,7.8068538961858));
#61256=CARTESIAN_POINT('Ctrl Pts',(0.153149799494756,2.38411656192535,7.80852888650995));
#61257=CARTESIAN_POINT('Ctrl Pts',(0.137251281498932,2.39212854808915,7.80973767408629));
#61258=CARTESIAN_POINT('Ctrl Pts',(0.10560827789721,2.40491913236995,7.8120411096631));
#61259=CARTESIAN_POINT('Ctrl Pts',(0.0899947172923275,2.40988688402467,
7.81313327882749));
#61260=CARTESIAN_POINT('Ctrl Pts',(0.0731782221931669,2.41385818805318,
7.81422001269156));
#61261=CARTESIAN_POINT('Ctrl Pts',(0.0722859806585192,2.41406488415594,
7.81427740821395));
#61262=CARTESIAN_POINT('Ctrl Pts',(0.0710857753133844,2.41433753727323,
7.81435424870901));
#61263=CARTESIAN_POINT('Ctrl Pts',(0.0707785895888558,2.41440684796736,
7.81437388347206));
#61264=CARTESIAN_POINT('Ctrl Pts',(0.0702615142085858,2.41452272011223,
7.81440687939338));
#61265=CARTESIAN_POINT('Ctrl Pts',(0.0700516795127248,2.41456952179725,
7.81442025436745));
#61266=CARTESIAN_POINT('Ctrl Pts',(0.069649367517086,2.41465883124986,7.81444586875617));
#61267=CARTESIAN_POINT('Ctrl Pts',(0.0694568994500815,2.41470137209441,
7.81445810998107));
#61268=CARTESIAN_POINT('Ctrl Pts',(0.0690015932658903,2.4148015694989,7.81448703785629));
#61269=CARTESIAN_POINT('Ctrl Pts',(0.068738722207993,2.41485907340059,7.81450371560332));
#61270=CARTESIAN_POINT('Ctrl Pts',(0.0679777301039346,2.41502454446437,
7.81455192849065));
#61271=CARTESIAN_POINT('Ctrl Pts',(0.0674794216712453,2.41513165988902,
7.81458341476739));
#61272=CARTESIAN_POINT('Ctrl Pts',(0.0639306184851298,2.41588570028342,
7.81480706505685));
#61273=CARTESIAN_POINT('Ctrl Pts',(0.0608709965770389,2.41648953086046,
7.81499680913416));
#61274=CARTESIAN_POINT('Ctrl Pts',(0.0524138916075015,2.41803139301057,
7.81551402478171));
#61275=CARTESIAN_POINT('Ctrl Pts',(0.0470003206310586,2.41887640251969,
7.81583701016565));
#61276=CARTESIAN_POINT('Ctrl Pts',(0.0260955798092798,2.42159544026768,
7.81706218971309));
#61277=CARTESIAN_POINT('Ctrl Pts',(0.0104967851393392,2.42248177316093,
7.81793086150959));
#61278=CARTESIAN_POINT('Ctrl Pts',(-0.0311254436506786,2.42182227345409,
7.82025774231299));
#61279=CARTESIAN_POINT('Ctrl Pts',(-0.0569949724175114,2.41826039531,7.82172144340392));
#61280=CARTESIAN_POINT('Ctrl Pts',(-0.0836205209930331,2.41124120296321,
7.82339137909399));
#61281=CARTESIAN_POINT('Ctrl Pts',(-0.0850849650266446,2.41084405504504,
7.82348373086133));
#61282=CARTESIAN_POINT('Ctrl Pts',(-0.087073165000146,2.41028976531911,
7.82360981513051));
#61283=CARTESIAN_POINT('Ctrl Pts',(-0.087599422318235,2.41014160592967,
7.82364325563485));
#61284=CARTESIAN_POINT('Ctrl Pts',(-0.0884918496502678,2.40988790455496,
7.82370007914616));
#61285=CARTESIAN_POINT('Ctrl Pts',(-0.0888582153931184,2.40978305053556,
7.82372343972041));
#61286=CARTESIAN_POINT('Ctrl Pts',(-0.0895644599052865,2.409579567143,7.82376853595656));
#61287=CARTESIAN_POINT('Ctrl Pts',(-0.0899043640735989,2.4094810271883,
7.82379026867599));
#61288=CARTESIAN_POINT('Ctrl Pts',(-0.0907075025220222,2.4092467584632,
7.82384168759514));
#61289=CARTESIAN_POINT('Ctrl Pts',(-0.0911705945694027,2.40911054869678,
7.82387138946149));
#61290=CARTESIAN_POINT('Ctrl Pts',(-0.0921270068576774,2.40882690189701,
7.82393284344144));
#61291=CARTESIAN_POINT('Ctrl Pts',(-0.0926202829979628,2.40867932211327,
7.82396460015662));
#61292=CARTESIAN_POINT('Ctrl Pts',(-0.0953313940116427,2.40786112042951,
7.82413947939449));
#61293=CARTESIAN_POINT('Ctrl Pts',(-0.0975422548252596,2.4071677916532,
7.8242833441271));
#61294=CARTESIAN_POINT('Ctrl Pts',(-0.10326193876419,2.40530611479243,7.82465887785764));
#61295=CARTESIAN_POINT('Ctrl Pts',(-0.106758390033697,2.40410112800867,
7.8248917377807));
#61296=CARTESIAN_POINT('Ctrl Pts',(-0.122024532935296,2.39854421102713,
7.82592332641025));
#61297=CARTESIAN_POINT('Ctrl Pts',(-0.133553760828635,2.39356764433169,
7.82674224145896));
#61298=CARTESIAN_POINT('Ctrl Pts',(-0.156552798271399,2.38200451497779,
7.82845473999739));
#61299=CARTESIAN_POINT('Ctrl Pts',(-0.167967363648404,2.37535841787191,
7.8293484479648));
#61300=CARTESIAN_POINT('Ctrl Pts',(-0.194637220954538,2.35755324445342,
7.83151783137158));
#61301=CARTESIAN_POINT('Ctrl Pts',(-0.209384019391688,2.34571494708776,
7.8327892954898));
#61302=CARTESIAN_POINT('Ctrl Pts',(-0.223828972014007,2.33186860541699,
7.83405051977083));
#61303=CARTESIAN_POINT('Ctrl Pts',(-0.224642633234347,2.33108038929128,
7.8341216133455));
#61304=CARTESIAN_POINT('Ctrl Pts',(-0.225725065035867,2.33002068716734,
7.83421623790147));
#61305=CARTESIAN_POINT('Ctrl Pts',(-0.225997520919612,2.32975300227019,
7.83424005961378));
#61306=CARTESIAN_POINT('Ctrl Pts',(-0.226422585834484,2.3293338929733,7.83427722979112));
#61307=CARTESIAN_POINT('Ctrl Pts',(-0.226575519197391,2.32918280027819,
7.83429060427191));
#61308=CARTESIAN_POINT('Ctrl Pts',(-0.226868386514299,2.328892878177,7.8343162182744));
#61309=CARTESIAN_POINT('Ctrl Pts',(-0.227008343269147,2.32875407442538,
7.83432845960528));
#61310=CARTESIAN_POINT('Ctrl Pts',(-0.227339068855871,2.32842547102381,
7.83435738856153));
#61311=CARTESIAN_POINT('Ctrl Pts',(-0.227529727135925,2.3282355610141,7.83437406728155));
#61312=CARTESIAN_POINT('Ctrl Pts',(-0.227924005593286,2.32784184492002,
7.83440856255477));
#61313=CARTESIAN_POINT('Ctrl Pts',(-0.228127590914905,2.32763800404839,
7.83442637633619));
#61314=CARTESIAN_POINT('Ctrl Pts',(-0.229248898328521,2.32651227412544,
7.83452450502748));
#61315=CARTESIAN_POINT('Ctrl Pts',(-0.230161323089784,2.3255850908257,7.83460440538622));
#61316=CARTESIAN_POINT('Ctrl Pts',(-0.233356934308235,2.32229821771889,
7.83488453724095));
#61317=CARTESIAN_POINT('Ctrl Pts',(-0.235609732292113,2.31990910018318,
7.83508255678206));
#61318=CARTESIAN_POINT('Ctrl Pts',(-0.244540977625731,2.31014258110534,
7.83587185224763));
#61319=CARTESIAN_POINT('Ctrl Pts',(-0.250913126686691,2.30249155800404,
7.83644489805314));
#61320=CARTESIAN_POINT('Ctrl Pts',(-0.261526996009817,2.28847547709734,
7.83744196561603));
#61321=CARTESIAN_POINT('Ctrl Pts',(-0.265915241467133,2.28223189876138,
7.83786920841151));
#61322=CARTESIAN_POINT('Ctrl Pts',(-0.282611472057146,2.25658742244511,
7.83958028896554));
#61323=CARTESIAN_POINT('Ctrl Pts',(-0.293049622222281,2.23605386273079,
7.84085943326052));
#61324=CARTESIAN_POINT('Ctrl Pts',(-0.301339757035058,2.21426131099904,
7.84223922115728));
#61325=CARTESIAN_POINT('Ctrl Pts',(-0.301462776026184,2.21393634639763,
7.84225979950111));
#61326=CARTESIAN_POINT('Ctrl Pts',(-0.303612089474638,2.20823091098701,
7.84262115785176));
#61327=CARTESIAN_POINT('Ctrl Pts',(-0.305494466068497,2.20279764505322,
7.84296627853491));
#61328=CARTESIAN_POINT('Ctrl Pts',(-0.307527308421526,2.19637996020461,
7.84337611627586));
#61329=CARTESIAN_POINT('Ctrl Pts',(-0.30781988841825,2.19544138732548,7.84343610752144));
#61330=CARTESIAN_POINT('Ctrl Pts',(-0.308254890759444,2.19402312649331,
7.84352684471022));
#61331=CARTESIAN_POINT('Ctrl Pts',(-0.308400499835402,2.19354441559765,
7.84355748622322));
#61332=CARTESIAN_POINT('Ctrl Pts',(-0.308658479176102,2.19268912179596,
7.84361225908258));
#61333=CARTESIAN_POINT('Ctrl Pts',(-0.308771276825858,2.19231266799182,
7.84363637639647));
#61334=CARTESIAN_POINT('Ctrl Pts',(-0.309007915036776,2.19151761922301,
7.84368733076293));
#61335=CARTESIAN_POINT('Ctrl Pts',(-0.309131594148688,2.19109897738026,
7.84371417303347));
#61336=CARTESIAN_POINT('Ctrl Pts',(-0.309456698058431,2.18999024640339,
7.84378529366064));
#61337=CARTESIAN_POINT('Ctrl Pts',(-0.309656664210244,2.18929973526148,
7.8438296194956));
#61338=CARTESIAN_POINT('Ctrl Pts',(-0.310087463381698,2.18779327837854,
7.84392639587658));
#61339=CARTESIAN_POINT('Ctrl Pts',(-0.310317389244331,2.18697708080565,
7.84397887564971));
#61340=CARTESIAN_POINT('Ctrl Pts',(-0.310986797476033,2.18456435111375,
7.84413415057298));
#61341=CARTESIAN_POINT('Ctrl Pts',(-0.311417194025377,2.18296534688794,
7.84423723966543));
#61342=CARTESIAN_POINT('Ctrl Pts',(-0.312868146516092,2.1774043738214,7.84459642798809));
#61343=CARTESIAN_POINT('Ctrl Pts',(-0.313825532676101,2.17342647180308,
7.84485454297649));
#61344=CARTESIAN_POINT('Ctrl Pts',(-0.317894230765282,2.15498460924081,
7.84605701148127));
#61345=CARTESIAN_POINT('Ctrl Pts',(-0.320082583443454,2.14033719035447,
7.84702967888952));
#61346=CARTESIAN_POINT('Ctrl Pts',(-0.321943102381381,2.11698286673872,
7.84859929369352));
#61347=CARTESIAN_POINT('Ctrl Pts',(-0.322282578411479,2.1083490653952,7.84918328118932));
#61348=CARTESIAN_POINT('Ctrl Pts',(-0.322274871694426,2.0997124250686,7.84976774768668));
#61349=CARTESIAN_POINT('',(-0.321883070004627,2.10020594158585,8.09972265507268));
#61350=CARTESIAN_POINT('Ctrl Pts',(-0.322274871581366,2.09971229839457,
7.84976775625908));
#61351=CARTESIAN_POINT('Ctrl Pts',(-0.322258932177978,2.08185744780233,
7.85097604578122));
#61352=CARTESIAN_POINT('Ctrl Pts',(-0.320759214031128,2.06403261792786,
7.85218492979292));
#61353=CARTESIAN_POINT('Ctrl Pts',(-0.317227215097624,2.04308309014836,
7.85354975638942));
#61354=CARTESIAN_POINT('Ctrl Pts',(-0.316611681255006,2.0397531232916,7.85376492348035));
#61355=CARTESIAN_POINT('Ctrl Pts',(-0.315854814762916,2.03599129032254,
7.85400550858418));
#61356=CARTESIAN_POINT('Ctrl Pts',(-0.315764952135085,2.0355494458331,7.85403372735028));
#61357=CARTESIAN_POINT('Ctrl Pts',(-0.315616929148595,2.03482937433395,
7.85407964998335));
#61358=CARTESIAN_POINT('Ctrl Pts',(-0.315559327852224,2.03455103498279,
7.85409738517302));
#61359=CARTESIAN_POINT('Ctrl Pts',(-0.315447040121666,2.03401203566707,
7.8541316977061));
#61360=CARTESIAN_POINT('Ctrl Pts',(-0.315392398681621,2.03375136670536,
7.85414827759786));
#61361=CARTESIAN_POINT('Ctrl Pts',(-0.315296814488741,2.03329817740091,
7.8541770776898));
#61362=CARTESIAN_POINT('Ctrl Pts',(-0.315256018611684,2.03310562733237,
7.85418930631074));
#61363=CARTESIAN_POINT('Ctrl Pts',(-0.315169995147034,2.032701436713,7.85421495933809));
#61364=CARTESIAN_POINT('Ctrl Pts',(-0.315124730916052,2.03248980501274,
7.85422838156139));
#61365=CARTESIAN_POINT('Ctrl Pts',(-0.314997493993823,2.0318978283478,7.854265899938));
#61366=CARTESIAN_POINT('Ctrl Pts',(-0.314915045304004,2.03151758436582,
7.85428996870754));
#61367=CARTESIAN_POINT('Ctrl Pts',(-0.314578371219292,2.02997834709904,
7.8543872800327));
#61368=CARTESIAN_POINT('Ctrl Pts',(-0.314318430502202,2.02882059382544,
7.85446019883639));
#61369=CARTESIAN_POINT('Ctrl Pts',(-0.309515824382371,2.00796964281188,
7.85576892476597));
#61370=CARTESIAN_POINT('Ctrl Pts',(-0.303136182553172,1.98874194307644,
7.85690426773417));
#61371=CARTESIAN_POINT('Ctrl Pts',(-0.292999455965349,1.96569781215525,
7.85831268057875));
#61372=CARTESIAN_POINT('Ctrl Pts',(-0.290898593475207,1.96120602613415,
7.8585894997276));
#61373=CARTESIAN_POINT('Ctrl Pts',(-0.286540373701567,1.95242191886493,
7.85913816899843));
#61374=CARTESIAN_POINT('Ctrl Pts',(-0.284288125615973,1.94812855309445,
7.85940991992784));
#61375=CARTESIAN_POINT('Ctrl Pts',(-0.275495460623045,1.93224894047294,
7.86043294951374));
#61376=CARTESIAN_POINT('Ctrl Pts',(-0.268337097808095,1.92102145748324,
7.86119341598281));
#61377=CARTESIAN_POINT('Ctrl Pts',(-0.256910170231663,1.90533196326534,
7.86233884940617));
#61378=CARTESIAN_POINT('Ctrl Pts',(-0.2531749733236,1.9004983571356,7.86270409391885));
#61379=CARTESIAN_POINT('Ctrl Pts',(-0.248698624034314,1.89503394112871,
7.86313288381852));
#61380=CARTESIAN_POINT('Ctrl Pts',(-0.248089079704336,1.89429657419839,
7.86319108844901));
#61381=CARTESIAN_POINT('Ctrl Pts',(-0.247109567352257,1.8931223427714,7.86328433414638));
#61382=CARTESIAN_POINT('Ctrl Pts',(-0.246741699692676,1.89268372721,7.86331928979842));
#61383=CARTESIAN_POINT('Ctrl Pts',(-0.246034663581908,1.8918452622313,7.86338635328193));
#61384=CARTESIAN_POINT('Ctrl Pts',(-0.245695683866944,1.89144525547607,
7.86341845333226));
#61385=CARTESIAN_POINT('Ctrl Pts',(-0.24509880589746,1.89074439554351,7.86347488391181));
#61386=CARTESIAN_POINT('Ctrl Pts',(-0.244841325437408,1.89044318669011,
7.86349919720603));
#61387=CARTESIAN_POINT('Ctrl Pts',(-0.244340103315882,1.88985902586917,
7.86354646937504));
#61388=CARTESIAN_POINT('Ctrl Pts',(-0.24409642394058,1.8895760210559,7.86356942565344));
#61389=CARTESIAN_POINT('Ctrl Pts',(-0.24344602015584,1.88882330395995,7.8636306293497));
#61390=CARTESIAN_POINT('Ctrl Pts',(-0.243038429856108,1.88835434499014,
7.86366891265978));
#61391=CARTESIAN_POINT('Ctrl Pts',(-0.24157557931191,1.8866810389704,7.86380606034529));
#61392=CARTESIAN_POINT('Ctrl Pts',(-0.240512715969049,1.88548339699866,
7.86390524162596));
#61393=CARTESIAN_POINT('Ctrl Pts',(-0.221774834238887,1.86468373663772,
7.86564587480005));
#61394=CARTESIAN_POINT('Ctrl Pts',(-0.20177052469913,1.84732256586555,7.86739519596161));
#61395=CARTESIAN_POINT('Ctrl Pts',(-0.172347192043686,1.82752975350544,
7.86979298453034));
#61396=CARTESIAN_POINT('Ctrl Pts',(-0.164603854095112,1.82278318159002,
7.87040856968137));
#61397=CARTESIAN_POINT('Ctrl Pts',(-0.147342991688531,1.8131809930222,7.87173644584256));
#61398=CARTESIAN_POINT('Ctrl Pts',(-0.137762692351258,1.80845826870893,
7.87244597945534));
#61399=CARTESIAN_POINT('Ctrl Pts',(-0.125567137491608,1.8031820508526,7.87330155634401));
#61400=CARTESIAN_POINT('Ctrl Pts',(-0.123156768891748,1.80217385571919,
7.87346840191766));
#61401=CARTESIAN_POINT('Ctrl Pts',(-0.119319230421289,1.80062327029458,
7.87373018491216));
#61402=CARTESIAN_POINT('Ctrl Pts',(-0.117900062024642,1.80006153859348,
7.87382616988519));
#61403=CARTESIAN_POINT('Ctrl Pts',(-0.116195186491908,1.79940068935003,
7.87394044609689));
#61404=CARTESIAN_POINT('Ctrl Pts',(-0.115913294594358,1.79929187728765,
7.87395930736223));
#61405=CARTESIAN_POINT('Ctrl Pts',(-0.115423052440332,1.79910343248774,
7.87399205021005));
#61406=CARTESIAN_POINT('Ctrl Pts',(-0.115214772386363,1.7990236195314,7.87400594255496));
#61407=CARTESIAN_POINT('Ctrl Pts',(-0.114796930297791,1.79886399965439,
7.87403377542652));
#61408=CARTESIAN_POINT('Ctrl Pts',(-0.114587367160357,1.79878419497256,
7.8740477158247));
#61409=CARTESIAN_POINT('Ctrl Pts',(-0.114186269614117,1.79863193037106,
7.8740743611343));
#61410=CARTESIAN_POINT('Ctrl Pts',(-0.113994749690766,1.7985594343759,7.87408706824206));
#61411=CARTESIAN_POINT('Ctrl Pts',(-0.113543937295348,1.79838927953756,
7.87411694232161));
#61412=CARTESIAN_POINT('Ctrl Pts',(-0.1132845872233,1.79829177224778,7.87413410013843));
#61413=CARTESIAN_POINT('Ctrl Pts',(-0.112519621679996,1.79800529521695,
7.87418462460534));
#61414=CARTESIAN_POINT('Ctrl Pts',(-0.112013653656151,1.79781725994929,
7.87421793556288));
#61415=CARTESIAN_POINT('Ctrl Pts',(-0.107632552538369,1.79620160638566,
7.87450546291387));
#61416=CARTESIAN_POINT('Ctrl Pts',(-0.103730563266756,1.79484724402656,
7.87475541420429));
#61417=CARTESIAN_POINT('Ctrl Pts',(-0.099557752997718,1.79348817936978,
7.87501731675413));
#61418=CARTESIAN_POINT('Ctrl Pts',(-0.0993120098759176,1.79340846870266,
7.87503272084469));
#61419=CARTESIAN_POINT('Ctrl Pts',(-0.0846749539895292,1.78868015293434,
7.87594906517088));
#61420=CARTESIAN_POINT('Ctrl Pts',(-0.0699727079321773,1.78504950584,7.87680324809009));
#61421=CARTESIAN_POINT('Ctrl Pts',(-0.0371963059840335,1.7793652691963,
7.87866722719831));
#61422=CARTESIAN_POINT('Ctrl Pts',(-0.0190952416640365,1.77778029876138,
7.87967193504103));
#61423=CARTESIAN_POINT('Ctrl Pts',(0.0102113351150218,1.7776932464846,7.88135666728746));
#61424=CARTESIAN_POINT('Ctrl Pts',(0.0213730601444318,1.77824066885499,
7.88201142037582));
#61425=CARTESIAN_POINT('Ctrl Pts',(0.0349971557098768,1.77962091173683,
7.8828370401502));
#61426=CARTESIAN_POINT('Ctrl Pts',(0.0375080976576649,1.77990516537533,
7.88299029258626));
#61427=CARTESIAN_POINT('Ctrl Pts',(0.0405394914810656,1.78028449483028,
7.88317670621085));
#61428=CARTESIAN_POINT('Ctrl Pts',(0.0410634350588698,1.78035136647965,
7.8832089762678));
#61429=CARTESIAN_POINT('Ctrl Pts',(0.0420754214693971,1.78048305691186,
7.88327140378583));
#61430=CARTESIAN_POINT('Ctrl Pts',(0.0425634851191913,1.78054770662511,
7.88330155583706));
#61431=CARTESIAN_POINT('Ctrl Pts',(0.0434033807515645,1.78066091954123,
7.88335352071114));
#61432=CARTESIAN_POINT('Ctrl Pts',(0.0437552851259638,1.78070894658507,
7.88337531654926));
#61433=CARTESIAN_POINT('Ctrl Pts',(0.0444805795560989,1.7808091545632,7.88342028730183));
#61434=CARTESIAN_POINT('Ctrl Pts',(0.0448539587654445,1.78086140918169,
7.88344346451782));
#61435=CARTESIAN_POINT('Ctrl Pts',(0.0457538841185101,1.78098896471327,
7.88349939076852));
#61436=CARTESIAN_POINT('Ctrl Pts',(0.0462803358973223,1.78106491404918,
7.88353216028183));
#61437=CARTESIAN_POINT('Ctrl Pts',(0.0482137010783108,1.78134872153592,
7.8836527006894));
#61438=CARTESIAN_POINT('Ctrl Pts',(0.0496194062492849,1.78156458636344,
7.88374072482089));
#61439=CARTESIAN_POINT('Ctrl Pts',(0.0749922357072826,1.7856330082916,7.88533659576262));
#61440=CARTESIAN_POINT('Ctrl Pts',(0.0984446508668024,1.79217111215096,
7.88693453538845));
#61441=CARTESIAN_POINT('Ctrl Pts',(0.137371964881999,1.80793063132598,7.88976775531084));
#61442=CARTESIAN_POINT('Ctrl Pts',(0.153230639388537,1.81592961670599,7.8909774892196));
#61443=CARTESIAN_POINT('Ctrl Pts',(0.172469956947232,1.82771591963494,7.89246428407692));
#61444=CARTESIAN_POINT('Ctrl Pts',(0.176531704672809,1.83033155766143,7.89277920322749));
#61445=CARTESIAN_POINT('Ctrl Pts',(0.183427389747883,1.83499476568953,7.89331368558763));
#61446=CARTESIAN_POINT('Ctrl Pts',(0.18628958747963,1.83699890952607,7.89353548195043));
#61447=CARTESIAN_POINT('Ctrl Pts',(0.189543088370175,1.83935681882906,7.89378701588884));
#61448=CARTESIAN_POINT('Ctrl Pts',(0.189966661559608,1.83966537351916,7.89381975147414));
#61449=CARTESIAN_POINT('Ctrl Pts',(0.190566489631344,1.84010456567569,7.89386609007485));
#61450=CARTESIAN_POINT('Ctrl Pts',(0.19074336372377,1.84023434994392,7.89387975183531));
#61451=CARTESIAN_POINT('Ctrl Pts',(0.191099087100104,1.84049592702523,7.89390722301798));
#61452=CARTESIAN_POINT('Ctrl Pts',(0.191277933162101,1.84062772455903,7.89392103212303));
#61453=CARTESIAN_POINT('Ctrl Pts',(0.191623565235151,1.84088298409545,7.89394771410498));
#61454=CARTESIAN_POINT('Ctrl Pts',(0.191790367860852,1.84100642193073,7.89396058862522));
#61455=CARTESIAN_POINT('Ctrl Pts',(0.19218806724616,1.84130132364875,7.89399127965306));
#61456=CARTESIAN_POINT('Ctrl Pts',(0.192418854411754,1.84147293602784,7.89400908574712));
#61457=CARTESIAN_POINT('Ctrl Pts',(0.193240617378158,1.84208570553367,7.89407247450046));
#61458=CARTESIAN_POINT('Ctrl Pts',(0.193830314057742,1.8425285863009,7.89411793760893));
#61459=CARTESIAN_POINT('Ctrl Pts',(0.202724822756754,1.84925651870783,7.89480338037994));
#61460=CARTESIAN_POINT('Ctrl Pts',(0.210722707799278,1.85593927249584,7.89541599658786));
#61461=CARTESIAN_POINT('Ctrl Pts',(0.228586565704996,1.87239981988116,7.89681263473243));
#61462=CARTESIAN_POINT('Ctrl Pts',(0.238172226417083,1.88245071754785,7.89758496006825));
#61463=CARTESIAN_POINT('Ctrl Pts',(0.263848382977891,1.91311157436162,7.89982070972837));
#61464=CARTESIAN_POINT('Ctrl Pts',(0.278117328138475,1.93509479545138,7.90129274457144));
#61465=CARTESIAN_POINT('Ctrl Pts',(0.29008272192339,1.95959160908565,7.90295046925214));
#61466=CARTESIAN_POINT('Ctrl Pts',(0.290582590157954,1.96062905596628,7.90302068287719));
#61467=CARTESIAN_POINT('Ctrl Pts',(0.291305358697669,1.96214991130708,7.90312363373724));
#61468=CARTESIAN_POINT('Ctrl Pts',(0.291532642641951,1.96263123634737,7.90315621892845));
#61469=CARTESIAN_POINT('Ctrl Pts',(0.291927584997375,1.96347301081714,7.90321321224776));
#61470=CARTESIAN_POINT('Ctrl Pts',(0.292095771331766,1.96383321247255,7.90323760206043));
#61471=CARTESIAN_POINT('Ctrl Pts',(0.292419717669013,1.96453036450791,7.90328481144513));
#61472=CARTESIAN_POINT('Ctrl Pts',(0.292575562896564,1.96486727481489,7.90330762802961));
#61473=CARTESIAN_POINT('Ctrl Pts',(0.292944182258829,1.9656677927261,7.90336184632108));
#61474=CARTESIAN_POINT('Ctrl Pts',(0.293156437975896,1.96613163667662,7.90339326583043));
#61475=CARTESIAN_POINT('Ctrl Pts',(0.29390119940669,1.96776943490269,7.90350422058128));
#61476=CARTESIAN_POINT('Ctrl Pts',(0.294427756465662,1.96894606643142,7.90358395986331));
#61477=CARTESIAN_POINT('Ctrl Pts',(0.302496790197261,1.98727102548914,7.90482633082116));
#61478=CARTESIAN_POINT('Ctrl Pts',(0.308535654506631,2.00503865699358,7.90604102274337));
#61479=CARTESIAN_POINT('Ctrl Pts',(0.317501653290525,2.04159242584183,7.90855253286967));
#61480=CARTESIAN_POINT('Ctrl Pts',(0.320381002975282,2.0603173631063,7.90984497495856));
#61481=CARTESIAN_POINT('Ctrl Pts',(0.322157595687597,2.08776815255019,7.91168669990593));
#61482=CARTESIAN_POINT('Ctrl Pts',(0.322369319103746,2.09636962812861,7.91225580190674));
#61483=CARTESIAN_POINT('Ctrl Pts',(0.322171496127166,2.10919606604382,7.91308342685875));
#61484=CARTESIAN_POINT('Ctrl Pts',(0.322023176726636,2.11342082261824,7.91335260906187));
#61485=CARTESIAN_POINT('Ctrl Pts',(0.321761789542182,2.11818863581479,7.91365161772659));
#61486=CARTESIAN_POINT('Ctrl Pts',(0.321730409049222,2.11873551669189,7.91368584372121));
#61487=CARTESIAN_POINT('Ctrl Pts',(0.321681055505062,2.11955890924342,7.91373726514261));
#61488=CARTESIAN_POINT('Ctrl Pts',(0.321664120151505,2.11983547857213,7.91375451842785));
#61489=CARTESIAN_POINT('Ctrl Pts',(0.321634463203355,2.12030977503769,7.91378407416897));
#61490=CARTESIAN_POINT('Ctrl Pts',(0.321621915959067,2.12050751222978,7.91379638647316));
#61491=CARTESIAN_POINT('Ctrl Pts',(0.321595603366356,2.12091621900285,7.9138218149182));
#61492=CARTESIAN_POINT('Ctrl Pts',(0.321581812813738,2.12112718604032,7.91383492958663));
#61493=CARTESIAN_POINT('Ctrl Pts',(0.321543705029712,2.12170147399554,7.9138706002601));
#61494=CARTESIAN_POINT('Ctrl Pts',(0.321518979522512,2.12206476892519,7.91389313321644));
#61495=CARTESIAN_POINT('Ctrl Pts',(0.321423564658934,2.12343248962119,7.91397784539681));
#61496=CARTESIAN_POINT('Ctrl Pts',(0.321348782927495,2.12443663770256,7.91403979708322));
#61497=CARTESIAN_POINT('Ctrl Pts',(0.319855870133592,2.14328957994406,7.91519867320213));
#61498=CARTESIAN_POINT('Ctrl Pts',(0.316957151100179,2.16099288480806,7.91621576110948));
#61499=CARTESIAN_POINT('Ctrl Pts',(0.305065577006273,2.20842838594641,7.91896009332865));
#61500=CARTESIAN_POINT('Ctrl Pts',(0.29323380259033,2.23724233499828,7.92066539462707));
#61501=CARTESIAN_POINT('Ctrl Pts',(0.276447241611424,2.26565672543972,7.92266108121648));
#61502=CARTESIAN_POINT('Ctrl Pts',(0.275407105148127,2.26738026833172,7.92278338833579));
#61503=CARTESIAN_POINT('Ctrl Pts',(0.27400307467952,2.26965827469059,7.92294675948895));
#61504=CARTESIAN_POINT('Ctrl Pts',(0.273653503179996,2.27022154767181,7.92298729650321));
#61505=CARTESIAN_POINT('Ctrl Pts',(0.273077483030194,2.27114334255704,7.92305386836502));
#61506=CARTESIAN_POINT('Ctrl Pts',(0.27285205913344,2.27150250512346,7.9230798653094));
#61507=CARTESIAN_POINT('Ctrl Pts',(0.272414409501804,2.27219675503421,7.9231302300102));
#61508=CARTESIAN_POINT('Ctrl Pts',(0.272202272617804,2.27253189771168,7.92315459444175));
#61509=CARTESIAN_POINT('Ctrl Pts',(0.271711807710557,2.27330359842089,7.9232108150113));
#61510=CARTESIAN_POINT('Ctrl Pts',(0.271433045861665,2.27373987822097,7.92324268723768));
#61511=CARTESIAN_POINT('Ctrl Pts',(0.270539973869678,2.27513019651722,7.9233445389832));
#61512=CARTESIAN_POINT('Ctrl Pts',(0.269921680961147,2.2760816551714,7.92341466691436));
#61513=CARTESIAN_POINT('Ctrl Pts',(0.264300602926611,2.28463245881778,7.9240488014076));
#61514=CARTESIAN_POINT('Ctrl Pts',(0.258983579072112,2.29201935412604,7.92462463863247));
#61515=CARTESIAN_POINT('Ctrl Pts',(0.249886318203063,2.30359181178599,7.92557471837433));
#61516=CARTESIAN_POINT('Ctrl Pts',(0.246296043712791,2.30792078077566,7.92594177541064));
#61517=CARTESIAN_POINT('Ctrl Pts',(0.225474136926969,2.33173034383116,7.92802627813301));
#61518=CARTESIAN_POINT('Ctrl Pts',(0.206049340942353,2.34916058980704,7.92981807853498));
#61519=CARTESIAN_POINT('Ctrl Pts',(0.177424243971776,2.36918691121252,7.93213627465463));
#61520=CARTESIAN_POINT('Ctrl Pts',(0.169895068998796,2.37400119232201,7.93271909344267));
#61521=CARTESIAN_POINT('Ctrl Pts',(0.161003271363964,2.37917908293114,7.93336889858684));
#61522=CARTESIAN_POINT('Ctrl Pts',(0.15982735262647,2.37985394626998,7.93345408126176));
#61523=CARTESIAN_POINT('Ctrl Pts',(0.15830568088081,2.38071451860004,7.93356330836455));
#61524=CARTESIAN_POINT('Ctrl Pts',(0.157963821577807,2.38090703200243,7.93358778254492));
#61525=CARTESIAN_POINT('Ctrl Pts',(0.157409703889777,2.38121774440651,7.93362734667651));
#61526=CARTESIAN_POINT('Ctrl Pts',(0.157197663226957,2.38133632777278,7.93364246137268));
#61527=CARTESIAN_POINT('Ctrl Pts',(0.156793569883267,2.38156171678587,7.93367121798969));
#61528=CARTESIAN_POINT('Ctrl Pts',(0.156601543653029,2.38166856488058,7.93368486256854));
#61529=CARTESIAN_POINT('Ctrl Pts',(0.156163475179066,2.38191173044604,7.93371594307616));
#61530=CARTESIAN_POINT('Ctrl Pts',(0.155917363996643,2.38204792207862,7.9337333708238));
#61531=CARTESIAN_POINT('Ctrl Pts',(0.155149764107383,2.38247138048533,7.93378762288085));
#61532=CARTESIAN_POINT('Ctrl Pts',(0.154627653655933,2.38275752657373,7.93382437552342));
#61533=CARTESIAN_POINT('Ctrl Pts',(0.150559087996966,2.38497269175915,7.93410963925556));
#61534=CARTESIAN_POINT('Ctrl Pts',(0.14697726624696,2.38683647064676,7.93435409292421));
#61535=CARTESIAN_POINT('Ctrl Pts',(0.142956236081539,2.38883367984733,7.93462221551448));
#61536=CARTESIAN_POINT('Ctrl Pts',(0.142550876936337,2.38903395568328,7.93464917444293));
#61537=CARTESIAN_POINT('Ctrl Pts',(0.141334512184778,2.38963174382366,7.93472986333274));
#61538=CARTESIAN_POINT('Ctrl Pts',(0.140522249355728,2.39002670365849,7.93478347040678));
#61539=CARTESIAN_POINT('Ctrl Pts',(0.138267128069659,2.39111155017826,7.93493157003802));
#61540=CARTESIAN_POINT('Ctrl Pts',(0.136820762216312,2.39179412700156,7.93502572992031));
#61541=CARTESIAN_POINT('Ctrl Pts',(0.132740678451923,2.39368261469346,7.93528919456026));
#61542=CARTESIAN_POINT('Ctrl Pts',(0.130095652471343,2.39486384650226,7.93545748973609));
#61543=CARTESIAN_POINT('Ctrl Pts',(0.107461645344667,2.40460801559988,7.93687934773295));
#61544=CARTESIAN_POINT('Ctrl Pts',(0.0866683002105105,2.41116357892471,
7.93806878319673));
#61545=CARTESIAN_POINT('Ctrl Pts',(0.0549097768024357,2.41774242499981,
7.9398999275065));
#61546=CARTESIAN_POINT('Ctrl Pts',(0.0443468393510754,2.41938795235659,
7.94051059119462));
#61547=CARTESIAN_POINT('Ctrl Pts',(0.0260817354073458,2.42130973074655,
7.94158585419155));
#61548=CARTESIAN_POINT('Ctrl Pts',(0.0184154012885111,2.4218401133452,7.94204287624618));
#61549=CARTESIAN_POINT('Ctrl Pts',(0.00913806175046046,2.42214939654715,
7.9426056456217));
#61550=CARTESIAN_POINT('Ctrl Pts',(0.00753789751668553,2.42219080965365,
7.94270305724656));
#61551=CARTESIAN_POINT('Ctrl Pts',(0.00533588394085926,2.42223138588347,
7.94283760223657));
#61552=CARTESIAN_POINT('Ctrl Pts',(0.00473422794086623,2.42224078696507,
7.94287441478547));
#61553=CARTESIAN_POINT('Ctrl Pts',(0.00372178955027446,2.42225377059293,
7.94293644798275));
#61554=CARTESIAN_POINT('Ctrl Pts',(0.00331101857959443,2.42225825285368,
7.94296164039817));
#61555=CARTESIAN_POINT('Ctrl Pts',(0.00250066928757386,2.42226554570591,
7.94301138663945));
#61556=CARTESIAN_POINT('Ctrl Pts',(0.00210109200908594,2.42226839855328,
7.94303593909606));
#61557=CARTESIAN_POINT('Ctrl Pts',(0.00122335238087326,2.42227303281044,
7.94308992360258));
#61558=CARTESIAN_POINT('Ctrl Pts',(0.000745189921370165,2.42227449318234,
7.94311936565926));
#61559=CARTESIAN_POINT('Ctrl Pts',(-0.000909951061609263,2.42227586458622,
7.94322139406877));
#61560=CARTESIAN_POINT('Ctrl Pts',(-0.002086913932684,2.42227039211981,
7.94329414882692));
#61561=CARTESIAN_POINT('Ctrl Pts',(-0.0137774730839854,2.42215199107151,
7.9440188673165));
#61562=CARTESIAN_POINT('Ctrl Pts',(-0.0242785074332012,2.42153108221361,
7.9446867072892));
#61563=CARTESIAN_POINT('Ctrl Pts',(-0.0404548765975516,2.41977764674232,
7.94574310583009));
#61564=CARTESIAN_POINT('Ctrl Pts',(-0.0461622976310948,2.41900372557221,
7.94612114172282));
#61565=CARTESIAN_POINT('Ctrl Pts',(-0.0724682015490074,2.41471593984277,
7.94788663715116));
#61566=CARTESIAN_POINT('Ctrl Pts',(-0.0927143413632195,2.40935692994802,
7.94931567080794));
#61567=CARTESIAN_POINT('Ctrl Pts',(-0.124781816505537,2.39743584391792,
7.95161010768108));
#61568=CARTESIAN_POINT('Ctrl Pts',(-0.136968519178387,2.39202448964841,
7.95248872204807));
#61569=CARTESIAN_POINT('Ctrl Pts',(-0.149380189184174,2.38556467289061,
7.95336617278646));
#61570=CARTESIAN_POINT('Ctrl Pts',(-0.149972758908458,2.38525391308138,
7.95340802074615));
#61571=CARTESIAN_POINT('Ctrl Pts',(-0.150828075396917,2.38480195971763,
7.95346835555974));
#61572=CARTESIAN_POINT('Ctrl Pts',(-0.15109159572406,2.38466224598675,7.95348693507904));
#61573=CARTESIAN_POINT('Ctrl Pts',(-0.151550532338594,2.38441810924009,
7.95351927545306));
#61574=CARTESIAN_POINT('Ctrl Pts',(-0.151746035254182,2.38431385035144,
7.95353304677546));
#61575=CARTESIAN_POINT('Ctrl Pts',(-0.152125306120398,2.38411108801945,
7.95355975215387));
#61576=CARTESIAN_POINT('Ctrl Pts',(-0.152309085463493,2.38401260814218,
7.95357268767051));
#61577=CARTESIAN_POINT('Ctrl Pts',(-0.1527494200689,2.38377610041267,7.95360366984434));
#61578=CARTESIAN_POINT('Ctrl Pts',(-0.153005884541916,2.38363790260454,
7.9536217056325));
#61579=CARTESIAN_POINT('Ctrl Pts',(-0.153786694861446,2.38321578990748,
7.95367658896102));
#61580=CARTESIAN_POINT('Ctrl Pts',(-0.154310444212702,2.38293076536419,
7.9537133663687));
#61581=CARTESIAN_POINT('Ctrl Pts',(-0.160050479431413,2.37978635651616,
7.95411605489116));
#61582=CARTESIAN_POINT('Ctrl Pts',(-0.165187836793753,2.37678430380563,
7.95447307178854));
#61583=CARTESIAN_POINT('Ctrl Pts',(-0.170360685129585,2.37356613999067,
7.95483211706501));
#61584=CARTESIAN_POINT('Ctrl Pts',(-0.170481797560588,2.37349068117173,
7.95484052317632));
#61585=CARTESIAN_POINT('Ctrl Pts',(-0.182947339921855,2.36571255607436,
7.95570570353242));
#61586=CARTESIAN_POINT('Ctrl Pts',(-0.194757159022596,2.35718206897935,
7.95652368609568));
#61587=CARTESIAN_POINT('Ctrl Pts',(-0.215347442424132,2.34007478333718,
7.95802167416347));
#61588=CARTESIAN_POINT('Ctrl Pts',(-0.224292416405225,2.33173978105501,
7.95870150368423));
#61589=CARTESIAN_POINT('Ctrl Pts',(-0.243749195134019,2.31142544222842,
7.9602949519516));
#61590=CARTESIAN_POINT('Ctrl Pts',(-0.253888320057476,2.29913565459063,
7.96121557017588));
#61591=CARTESIAN_POINT('Ctrl Pts',(-0.264518388113055,2.2841125160232,7.96232540748322));
#61592=CARTESIAN_POINT('Ctrl Pts',(-0.265935288851899,2.28205992917191,
7.96247669224427));
#61593=CARTESIAN_POINT('Ctrl Pts',(-0.267725928230209,2.279400418427,7.96267234201996));
#61594=CARTESIAN_POINT('Ctrl Pts',(-0.268121701952594,2.27880837706252,
7.96271587294973));
#61595=CARTESIAN_POINT('Ctrl Pts',(-0.268756070509483,2.2778525778087,7.96278611451706));
#61596=CARTESIAN_POINT('Ctrl Pts',(-0.268995898340527,2.27748963784382,
7.96281277876174));
#61597=CARTESIAN_POINT('Ctrl Pts',(-0.269451159659886,2.27679763255968,
7.96286360355131));
#61598=CARTESIAN_POINT('Ctrl Pts',(-0.269666727203407,2.27646865602137,
7.96288775901338));
#61599=CARTESIAN_POINT('Ctrl Pts',(-0.270156660806904,2.2757179767614,7.96294286423652));
#61600=CARTESIAN_POINT('Ctrl Pts',(-0.27043064220822,2.27529602529929,7.96297382829223));
#61601=CARTESIAN_POINT('Ctrl Pts',(-0.271262646656974,2.27400808453257,
7.96306831135616));
#61602=CARTESIAN_POINT('Ctrl Pts',(-0.271817502237051,2.27314006582006,
7.96313194801796));
#61603=CARTESIAN_POINT('Ctrl Pts',(-0.275810554755725,2.26682681232695,
7.96359451411695));
#61604=CARTESIAN_POINT('Ctrl Pts',(-0.279088802291413,2.26128260356565,
7.96399930246104));
#61605=CARTESIAN_POINT('Ctrl Pts',(-0.283036697898372,2.2541246726383,7.96452065743821));
#61606=CARTESIAN_POINT('Ctrl Pts',(-0.283862494322685,2.25259839844246,
7.96463175155426));
#61607=CARTESIAN_POINT('Ctrl Pts',(-0.286775971722933,2.24710808762827,
7.96503112148844));
#61608=CARTESIAN_POINT('Ctrl Pts',(-0.28879319864089,2.24310741718386,7.96532166545972));
#61609=CARTESIAN_POINT('Ctrl Pts',(-0.30174725267772,2.21602617207257,7.96728485773741));
#61610=CARTESIAN_POINT('Ctrl Pts',(-0.309989515824185,2.19175892271045,
7.96903713270421));
#61611=CARTESIAN_POINT('Ctrl Pts',(-0.31763907958223,2.15564304431348,7.97150799990326));
#61612=CARTESIAN_POINT('Ctrl Pts',(-0.319406302270793,2.14438926152066,
7.97225792046781));
#61613=CARTESIAN_POINT('Ctrl Pts',(-0.32068021565817,2.1320380932898,7.97304347750477));
#61614=CARTESIAN_POINT('Ctrl Pts',(-0.320781142646429,2.13101126771642,
7.97310850305196));
#61615=CARTESIAN_POINT('Ctrl Pts',(-0.320946673354063,2.1292398198769,7.97322017580404));
#61616=CARTESIAN_POINT('Ctrl Pts',(-0.321013620552848,2.12849543208073,
7.97326694799747));
#61617=CARTESIAN_POINT('Ctrl Pts',(-0.321104849460066,2.12743990996202,
7.97333304460863));
#61618=CARTESIAN_POINT('Ctrl Pts',(-0.321131269090855,2.12712897011615,
7.97335248793103));
#61619=CARTESIAN_POINT('Ctrl Pts',(-0.321175876291508,2.12659477926577,
7.97338584321219));
#61620=CARTESIAN_POINT('Ctrl Pts',(-0.321194282787789,2.1263715471935,7.9733997675622));
#61621=CARTESIAN_POINT('Ctrl Pts',(-0.321229095117471,2.12594390347759,
7.97342641445788));
#61622=CARTESIAN_POINT('Ctrl Pts',(-0.321245538554226,2.12573949566795,
7.97343913913755));
#61623=CARTESIAN_POINT('Ctrl Pts',(-0.321283829968317,2.12525774381251,
7.97346910049723));
#61624=CARTESIAN_POINT('Ctrl Pts',(-0.321305513989276,2.12498038636707,
7.97348632788842));
#61625=CARTESIAN_POINT('Ctrl Pts',(-0.321368550280487,2.12416043525954,
7.97353719258001));
#61626=CARTESIAN_POINT('Ctrl Pts',(-0.321408887730428,2.12361776110019,
7.9735707731226));
#61627=CARTESIAN_POINT('Ctrl Pts',(-0.321752120898366,2.11883632461891,
7.97386593130243));
#61628=CARTESIAN_POINT('Ctrl Pts',(-0.321972541793684,2.1145918126738,7.97412299043251));
#61629=CARTESIAN_POINT('Ctrl Pts',(-0.322138624691726,2.10942001207882,
7.97443152541405));
#61630=CARTESIAN_POINT('Ctrl Pts',(-0.32216431984864,2.10849595194501,7.9744864703627));
#61631=CARTESIAN_POINT('Ctrl Pts',(-0.322189581817633,2.10742103305464,
7.97455018702444));
#61632=CARTESIAN_POINT('Ctrl Pts',(-0.32219301886017,2.10727027931688,7.97455911853231));
#61633=CARTESIAN_POINT('Ctrl Pts',(-0.322203769155405,2.10678377117518,
7.97458792755029));
#61634=CARTESIAN_POINT('Ctrl Pts',(-0.322210663417825,2.10644800673407,
7.97460778787639));
#61635=CARTESIAN_POINT('Ctrl Pts',(-0.322243049164172,2.10474073498525,
7.97470866180329));
#61636=CARTESIAN_POINT('Ctrl Pts',(-0.322260309064804,2.10336906707049,
7.97478934413744));
#61637=CARTESIAN_POINT('Ctrl Pts',(-0.322272586116957,2.10138814841775,
7.97490539229644));
#61638=CARTESIAN_POINT('Ctrl Pts',(-0.322274634324835,2.10077897251971,
7.97494101537436));
#61639=CARTESIAN_POINT('Ctrl Pts',(-0.322278855065594,2.09276771086691,
7.97540869041609));
#61640=CARTESIAN_POINT('Ctrl Pts',(-0.32202773443698,2.08536728885032,7.97583171717467));
#61641=CARTESIAN_POINT('Ctrl Pts',(-0.319167646610688,2.04360284295726,
7.97819942833365));
#61642=CARTESIAN_POINT('Ctrl Pts',(-0.311315845336575,2.00982780241766,
7.98006769064258));
#61643=CARTESIAN_POINT('Ctrl Pts',(-0.298120433186201,1.97758461131722,
7.98217448017197));
#61644=CARTESIAN_POINT('Ctrl Pts',(-0.29797586204607,1.97723312455924,7.98219748383168));
#61645=CARTESIAN_POINT('Ctrl Pts',(-0.29718658971003,1.97532382365179,7.98232264548775));
#61646=CARTESIAN_POINT('Ctrl Pts',(-0.296530302786638,1.97377085354978,
7.98242518812886));
#61647=CARTESIAN_POINT('Ctrl Pts',(-0.295610154105342,1.97164028873369,
7.9825669159028));
#61648=CARTESIAN_POINT('Ctrl Pts',(-0.295356717537208,1.97105819885271,
7.98260574538362));
#61649=CARTESIAN_POINT('Ctrl Pts',(-0.294950410957761,1.97013248232345,
7.98266767100056));
#61650=CARTESIAN_POINT('Ctrl Pts',(-0.294798655657859,1.96978836575791,
7.98269072896484));
#61651=CARTESIAN_POINT('Ctrl Pts',(-0.294502278353795,1.96911948174347,
7.98273562339036));
#61652=CARTESIAN_POINT('Ctrl Pts',(-0.294357720570051,1.9687946862588,7.98275745762591));
#61653=CARTESIAN_POINT('Ctrl Pts',(-0.294010706762027,1.96801846831673,
7.98280972140552));
#61654=CARTESIAN_POINT('Ctrl Pts',(-0.293807748541964,1.96756727259281,
7.98284016816148));
#61655=CARTESIAN_POINT('Ctrl Pts',(-0.293196067167288,1.96621577287938,
7.98293157021642));
#61656=CARTESIAN_POINT('Ctrl Pts',(-0.292784241760667,1.96531688684037,
7.98299263219577));
#61657=CARTESIAN_POINT('Ctrl Pts',(-0.289106971866324,1.95738712978435,
7.98353372389257));
#61658=CARTESIAN_POINT('Ctrl Pts',(-0.285593214855551,1.95047484898909,
7.98402232911353));
#61659=CARTESIAN_POINT('Ctrl Pts',(-0.278630521139103,1.93792028600481,
7.9849428633235));
#61660=CARTESIAN_POINT('Ctrl Pts',(-0.275250490306978,1.93224434677021,
7.98537225044948));
#61661=CARTESIAN_POINT('Ctrl Pts',(-0.262805660311028,1.91273606082892,
7.98689421936328));
#61662=CARTESIAN_POINT('Ctrl Pts',(-0.252853611858638,1.89950170830973,
7.98801248217074));
#61663=CARTESIAN_POINT('Ctrl Pts',(-0.229217042412051,1.87264324352422,
7.99043323637256));
#61664=CARTESIAN_POINT('Ctrl Pts',(-0.215232663582003,1.85936202528794,
7.99173128890212));
#61665=CARTESIAN_POINT('Ctrl Pts',(-0.200099249302323,1.84737088557421,
7.99294818405348));
#61666=CARTESIAN_POINT('Ctrl Pts',(-0.200053524706638,1.84733467535221,
7.99295185920715));
#61667=CARTESIAN_POINT('Ctrl Pts',(-0.199163638787225,1.84663034989125,
7.99302335312529));
#61668=CARTESIAN_POINT('Ctrl Pts',(-0.198316130541619,1.84596644501931,
7.99309089226384));
#61669=CARTESIAN_POINT('Ctrl Pts',(-0.197169705419999,1.84507761419416,
7.99318149583913));
#61670=CARTESIAN_POINT('Ctrl Pts',(-0.196873713084509,1.84484895332363,
7.99320482100931));
#61671=CARTESIAN_POINT('Ctrl Pts',(-0.196408224745283,1.84449064515518,
7.99324139622688));
#61672=CARTESIAN_POINT('Ctrl Pts',(-0.196238998095383,1.8443606509397,7.99325467091501));
#61673=CARTESIAN_POINT('Ctrl Pts',(-0.195912887889294,1.8441106586911,7.99328020932289));
#61674=CARTESIAN_POINT('Ctrl Pts',(-0.195756024315178,1.843990637708,7.9932924746267));
#61675=CARTESIAN_POINT('Ctrl Pts',(-0.195382519217882,1.84370540185631,
7.99332163423241));
#61676=CARTESIAN_POINT('Ctrl Pts',(-0.195165778664042,1.84354031760658,
7.99333851919561));
#61677=CARTESIAN_POINT('Ctrl Pts',(-0.194521775168591,1.8430510902317,7.99338858374208));
#61678=CARTESIAN_POINT('Ctrl Pts',(-0.194093909494702,1.84272773652661,
7.99342170770138));
#61679=CARTESIAN_POINT('Ctrl Pts',(-0.190633811872276,1.84012635921396,
7.99368848219602));
#61680=CARTESIAN_POINT('Ctrl Pts',(-0.187562231108778,1.83790083567827,
7.9939185313181));
#61681=CARTESIAN_POINT('Ctrl Pts',(-0.176256844167683,1.83001004291888,
7.99474381544702));
#61682=CARTESIAN_POINT('Ctrl Pts',(-0.167799374888341,1.82467390653016,
7.99532083149949));
#61683=CARTESIAN_POINT('Ctrl Pts',(-0.131743415463936,1.80420458645057,
7.99767598523277));
#61684=CARTESIAN_POINT('Ctrl Pts',(-0.102254432046472,1.79276176038056,
7.99937736302653));
#61685=CARTESIAN_POINT('Ctrl Pts',(-0.0712554161033839,1.7857008621921,
8.0012616863351));
#61686=CARTESIAN_POINT('Ctrl Pts',(-0.070936776215713,1.78562879246045,
8.00128106287805));
#61687=CARTESIAN_POINT('Ctrl Pts',(-0.0652971462924663,1.78436223601831,
8.00162414610145));
#61688=CARTESIAN_POINT('Ctrl Pts',(-0.0599470543503156,1.78330257246682,
8.00195178608463));
#61689=CARTESIAN_POINT('Ctrl Pts',(-0.0537042533029964,1.78222994854732,
8.00233746201053));
#61690=CARTESIAN_POINT('Ctrl Pts',(-0.052835018429724,1.78208426709833,
8.0023912375245));
#61691=CARTESIAN_POINT('Ctrl Pts',(-0.051450222259879,1.78185801512595,
8.00247703128507));
#61692=CARTESIAN_POINT('Ctrl Pts',(-0.0509350397262251,1.78177512725556,
8.00250897597185));
#61693=CARTESIAN_POINT('Ctrl Pts',(-0.0500272355011672,1.78163133132422,
8.00256531420451));
#61694=CARTESIAN_POINT('Ctrl Pts',(-0.0496346972491237,1.78156989728824,
8.00258969102141));
#61695=CARTESIAN_POINT('Ctrl Pts',(-0.0488245968536997,1.78144464719917,
8.00264003193276));
#61696=CARTESIAN_POINT('Ctrl Pts',(-0.0484070210244022,1.78138092591806,
8.00266599897939));
#61697=CARTESIAN_POINT('Ctrl Pts',(-0.0473410933620343,1.78122041120201,
8.00273233102465));
#61698=CARTESIAN_POINT('Ctrl Pts',(-0.0466925715596229,1.78112477502017,
8.0027727325874));
#61699=CARTESIAN_POINT('Ctrl Pts',(-0.0440700350332399,1.78074620687141,
8.00293629400941));
#61700=CARTESIAN_POINT('Ctrl Pts',(-0.0420937385077417,1.7804796261488,
8.00305996976343));
#61701=CARTESIAN_POINT('Ctrl Pts',(-0.0291818473656847,1.77885982292568,
8.00387084785819));
#61702=CARTESIAN_POINT('Ctrl Pts',(-0.0181866238236534,1.77805001437369,
8.00457509382631));
#61703=CARTESIAN_POINT('Ctrl Pts',(0.0236713919595222,1.77711819757734,
8.00731002993426));
#61704=CARTESIAN_POINT('Ctrl Pts',(0.0544482356536206,1.78086375105238,
8.00945064021308));
#61705=CARTESIAN_POINT('Ctrl Pts',(0.0848024713733795,1.78908187636469,
8.01151772230319));
#61706=CARTESIAN_POINT('Ctrl Pts',(0.0853836944600332,1.78924098808699,
8.01155727803791));
#61707=CARTESIAN_POINT('Ctrl Pts',(0.0874214974412825,1.78980499205283,
8.01169586829089));
#61708=CARTESIAN_POINT('Ctrl Pts',(0.0888756922704561,1.79021850822738,
8.01179459794157));
#61709=CARTESIAN_POINT('Ctrl Pts',(0.0912164185633628,1.79090195856612,
8.01195318682969));
#61710=CARTESIAN_POINT('Ctrl Pts',(0.0921047757328037,1.79116550620301,
8.01201329776371));
#61711=CARTESIAN_POINT('Ctrl Pts',(0.0931326345568202,1.79147526909201,
8.01208274931372));
#61712=CARTESIAN_POINT('Ctrl Pts',(0.0932732468130623,1.79151774989402,
8.01209224821875));
#61713=CARTESIAN_POINT('Ctrl Pts',(0.0939233130916909,1.79171462852633,
8.01213615264867));
#61714=CARTESIAN_POINT('Ctrl Pts',(0.0944324162780242,1.7918701933109,8.01217050803259));
#61715=CARTESIAN_POINT('Ctrl Pts',(0.0987115379628434,1.79318935017212,
8.01245901828756));
#61716=CARTESIAN_POINT('Ctrl Pts',(0.102460494093283,1.79442088876476,8.0127101250091));
#61717=CARTESIAN_POINT('Ctrl Pts',(0.106744475737754,1.79591589602634,8.01299439628836));
#61718=CARTESIAN_POINT('Ctrl Pts',(0.107302328235808,1.79611229745454,8.01303136101743));
#61719=CARTESIAN_POINT('Ctrl Pts',(0.108126836695061,1.79640513309702,8.01308591385298));
#61720=CARTESIAN_POINT('Ctrl Pts',(0.108393907101428,1.79650038397341,8.01310357169027));
#61721=CARTESIAN_POINT('Ctrl Pts',(0.108867439755196,1.79666997455176,8.01313485729367));
#61722=CARTESIAN_POINT('Ctrl Pts',(0.109073951774108,1.79674417264828,8.01314849350185));
#61723=CARTESIAN_POINT('Ctrl Pts',(0.109510182437678,1.79690141004515,8.01317728179479));
#61724=CARTESIAN_POINT('Ctrl Pts',(0.109739881873043,1.79698449937735,8.01319243079518));
#61725=CARTESIAN_POINT('Ctrl Pts',(0.110351352779289,1.79720647364527,8.01323273309103));
#61726=CARTESIAN_POINT('Ctrl Pts',(0.110732958053222,1.79734582000635,8.01325785880126));
#61727=CARTESIAN_POINT('Ctrl Pts',(0.112508245611008,1.79799788822094,8.01337463068625));
#61728=CARTESIAN_POINT('Ctrl Pts',(0.113898665957808,1.79851952809187,8.01346575179029));
#61729=CARTESIAN_POINT('Ctrl Pts',(0.124973839897785,1.80276212593847,8.01418925166488));
#61730=CARTESIAN_POINT('Ctrl Pts',(0.134478457384338,1.8069395855513,8.01479605597399));
#61731=CARTESIAN_POINT('Ctrl Pts',(0.167085939366902,1.82319248850407,8.01688267436618));
#61732=CARTESIAN_POINT('Ctrl Pts',(0.18891050529078,1.83760135536174,8.01829597067789));
#61733=CARTESIAN_POINT('Ctrl Pts',(0.218614898526131,1.86285880727917,8.02053678631184));
#61734=CARTESIAN_POINT('Ctrl Pts',(0.227952779632836,1.87182049459948,8.02129706269674));
#61735=CARTESIAN_POINT('Ctrl Pts',(0.23754737208645,1.88220678292567,8.02215638969351));
#61736=CARTESIAN_POINT('Ctrl Pts',(0.238363311768323,1.88310009006638,8.02223012804065));
#61737=CARTESIAN_POINT('Ctrl Pts',(0.239506906854062,1.88436636715142,8.0223344226344));
#61738=CARTESIAN_POINT('Ctrl Pts',(0.239838767164566,1.88473553984249,8.02236480146124));
#61739=CARTESIAN_POINT('Ctrl Pts',(0.240414954124197,1.8853794961803,8.0224177450542));
#61740=CARTESIAN_POINT('Ctrl Pts',(0.240659666557461,1.88565393468273,8.02244029357517));
#61741=CARTESIAN_POINT('Ctrl Pts',(0.241164201206696,1.88622171009245,8.02248691326849));
#61742=CARTESIAN_POINT('Ctrl Pts',(0.241423959064496,1.88651510318767,8.02251098708016));
#61743=CARTESIAN_POINT('Ctrl Pts',(0.242034173186306,1.88720687004315,8.02256771031642));
#61744=CARTESIAN_POINT('Ctrl Pts',(0.242384181224886,1.88760563606022,8.02260037834183));
#61745=CARTESIAN_POINT('Ctrl Pts',(0.243121531211282,1.88844989910624,8.022669480765));
#61746=CARTESIAN_POINT('Ctrl Pts',(0.243508636633396,1.88889559927798,8.02270592482671));
#61747=CARTESIAN_POINT('Ctrl Pts',(0.24454814620666,1.8900991192603,8.02280423857034));
#61748=CARTESIAN_POINT('Ctrl Pts',(0.245198247520846,1.89085891143797,8.02286620306268));
#61749=CARTESIAN_POINT('Ctrl Pts',(0.256941257899232,1.90471332015096,8.02399429765951));
#61750=CARTESIAN_POINT('Ctrl Pts',(0.26697240246131,1.91866809131453,8.02510386989432));
#61751=CARTESIAN_POINT('Ctrl Pts',(0.292275155676151,1.96055068692588,8.02835748734154));
#61752=CARTESIAN_POINT('Ctrl Pts',(0.304592873076093,1.99002722309371,8.03057428696961));
#61753=CARTESIAN_POINT('Ctrl Pts',(0.312780121345811,2.02233289139819,8.03268311463891));
#61754=CARTESIAN_POINT('Ctrl Pts',(0.313150509496931,2.02384001904503,8.03278075101568));
#61755=CARTESIAN_POINT('Ctrl Pts',(0.313608926693887,2.02576524329903,8.03290447308806));
#61756=CARTESIAN_POINT('Ctrl Pts',(0.313707023389319,2.02618088671783,8.0329311246088));
#61757=CARTESIAN_POINT('Ctrl Pts',(0.313861556033892,2.02684152493356,8.03297338999459));
#61758=CARTESIAN_POINT('Ctrl Pts',(0.313918531566079,2.02708639104738,8.03298903487884));
#61759=CARTESIAN_POINT('Ctrl Pts',(0.314024444384473,2.02754400225804,8.03301823317692));
#61760=CARTESIAN_POINT('Ctrl Pts',(0.314073451676662,2.02775672881094,8.03303179053127));
#61761=CARTESIAN_POINT('Ctrl Pts',(0.314183089369426,2.02823485462372,8.03306222665873));
#61762=CARTESIAN_POINT('Ctrl Pts',(0.314243599508734,2.02850028038028,8.03307909839138));
#61763=CARTESIAN_POINT('Ctrl Pts',(0.314422085626569,2.0292878072633,8.03312908553812));
#61764=CARTESIAN_POINT('Ctrl Pts',(0.314539098022451,2.02981012924671,8.03316214558673));
#61765=CARTESIAN_POINT('Ctrl Pts',(0.315467961716257,2.03400537746912,8.03342694803447));
#61766=CARTESIAN_POINT('Ctrl Pts',(0.316216794712723,2.03769216089017,8.03365514847465));
#61767=CARTESIAN_POINT('Ctrl Pts',(0.318691461989134,2.05107286658834,8.03446989314532));
#61768=CARTESIAN_POINT('Ctrl Pts',(0.320037544871541,2.060832196817,8.03503876440866));
#61769=CARTESIAN_POINT('Ctrl Pts',(0.323858630121932,2.10259862205488,8.03742265182372));
#61770=CARTESIAN_POINT('Ctrl Pts',(0.321992567900392,2.13481397971778,8.03915598276016));
#61771=CARTESIAN_POINT('Ctrl Pts',(0.314298964755468,2.17145571713681,8.04137948920178));
#61772=CARTESIAN_POINT('Ctrl Pts',(0.313070388406846,2.17665954300122,8.04170079662869));
#61773=CARTESIAN_POINT('Ctrl Pts',(0.311490622949169,2.18267729123685,8.04207963299852));
#61774=CARTESIAN_POINT('Ctrl Pts',(0.311264791433999,2.18352348329259,8.04213307174817));
#61775=CARTESIAN_POINT('Ctrl Pts',(0.310899336081152,2.18487077847462,8.04221842849841));
#61776=CARTESIAN_POINT('Ctrl Pts',(0.310761942299494,2.18537248636313,8.04225027411254));
#61777=CARTESIAN_POINT('Ctrl Pts',(0.310517538020945,2.18625654671252,8.04230649661029));
#61778=CARTESIAN_POINT('Ctrl Pts',(0.310411034223105,2.18663903912014,8.04233085698053));
#61779=CARTESIAN_POINT('Ctrl Pts',(0.310191897641845,2.18742044429211,8.04238069645845));
#61780=CARTESIAN_POINT('Ctrl Pts',(0.310079201565583,2.18781933839864,8.04240617758718));
#61781=CARTESIAN_POINT('Ctrl Pts',(0.30979157556242,2.1888299506696,8.04247083418969));
#61782=CARTESIAN_POINT('Ctrl Pts',(0.309615603721355,2.18944136821627,8.04251004356273));
#61783=CARTESIAN_POINT('Ctrl Pts',(0.309231061084397,2.19076273472439,8.04259498245305));
#61784=CARTESIAN_POINT('Ctrl Pts',(0.309021853783321,2.19147249326278,8.04264073260259));
#61785=CARTESIAN_POINT('Ctrl Pts',(0.308417408890938,2.19349739750329,8.04277161897104));
#61786=CARTESIAN_POINT('Ctrl Pts',(0.308016210753199,2.19481073391865,8.04285694980391));
#61787=CARTESIAN_POINT('Ctrl Pts',(0.306658432921034,2.19915587718971,8.04314074315344));
#61788=CARTESIAN_POINT('Ctrl Pts',(0.305665410158883,2.20217601641843,8.0433403937669));
#61789=CARTESIAN_POINT('Ctrl Pts',(0.301466364047907,2.2143374141486,8.04415429729472));
#61790=CARTESIAN_POINT('Ctrl Pts',(0.297893890697003,2.22334590420502,8.04478036189242));
#61791=CARTESIAN_POINT('Ctrl Pts',(0.287139829580337,2.24725927601229,8.04650493511214));
#61792=CARTESIAN_POINT('Ctrl Pts',(0.27920815999822,2.26179399088306,8.04762314863608));
#61793=CARTESIAN_POINT('Ctrl Pts',(0.259706423815186,2.29179213334084,8.05004403844249));
#61794=CARTESIAN_POINT('Ctrl Pts',(0.24778955565927,2.3069593492444,8.05134227725306));
#61795=CARTESIAN_POINT('Ctrl Pts',(0.234465770358515,2.32110407120128,8.05256695714794));
#61796=CARTESIAN_POINT('Ctrl Pts',(0.234342724542055,2.32123448019273,8.05257824934252));
#61797=CARTESIAN_POINT('Ctrl Pts',(0.233544093234559,2.32207948848807,8.05265142592055));
#61798=CARTESIAN_POINT('Ctrl Pts',(0.232865338646995,2.32279110576569,8.0527130825534));
#61799=CARTESIAN_POINT('Ctrl Pts',(0.231933435417272,2.3237592165674,8.05279699169251));
#61800=CARTESIAN_POINT('Ctrl Pts',(0.23168310718535,2.32401839949272,8.05281945874867));
#61801=CARTESIAN_POINT('Ctrl Pts',(0.231285739549084,2.32442844446465,8.05285500690835));
#61802=CARTESIAN_POINT('Ctrl Pts',(0.231138986952012,2.32457958214185,8.05286811034594));
#61803=CARTESIAN_POINT('Ctrl Pts',(0.230853725020348,2.32487279212537,8.05289353264205));
#61804=CARTESIAN_POINT('Ctrl Pts',(0.23071523372932,2.32501487932895,8.05290585268387));
#61805=CARTESIAN_POINT('Ctrl Pts',(0.230381672973994,2.32535646925533,8.05293547276838));
#61806=CARTESIAN_POINT('Ctrl Pts',(0.230186475649989,2.32555584653644,8.05295276261958));
#61807=CARTESIAN_POINT('Ctrl Pts',(0.229592710226044,2.32616075332619,8.0530052248007));
#61808=CARTESIAN_POINT('Ctrl Pts',(0.229193324893439,2.32656548450716,8.05304033320261));
#61809=CARTESIAN_POINT('Ctrl Pts',(0.225301149129364,2.33048893406631,8.05338076666994));
#61810=CARTESIAN_POINT('Ctrl Pts',(0.221728436540492,2.33392790250292,8.053679899582));
#61811=CARTESIAN_POINT('Ctrl Pts',(0.211340187973619,2.34347532539091,8.05451749462918));
#61812=CARTESIAN_POINT('Ctrl Pts',(0.204341613830049,2.34937810610984,8.05504414396834));
#61813=CARTESIAN_POINT('Ctrl Pts',(0.17297161656457,2.37362770444534,8.05729360379517));
#61814=CARTESIAN_POINT('Ctrl Pts',(0.146318762130083,2.38875967756152,8.05894600705478));
#61815=CARTESIAN_POINT('Ctrl Pts',(0.11653239710867,2.40047237841021,8.06083799351339));
#61816=CARTESIAN_POINT('Ctrl Pts',(0.115125136911787,2.40101437259044,8.0609274338485));
#61817=CARTESIAN_POINT('Ctrl Pts',(0.109117322363898,2.40327993877601,8.06130957430957));
#61818=CARTESIAN_POINT('Ctrl Pts',(0.104481671834036,2.40490799850585,8.06160520877488));
#61819=CARTESIAN_POINT('Ctrl Pts',(0.099000307656386,2.40669339951746,8.06195629870211));
#61820=CARTESIAN_POINT('Ctrl Pts',(0.0981887732054333,2.40695417739159,
8.06200831703418));
#61821=CARTESIAN_POINT('Ctrl Pts',(0.0968869307338629,2.40736681950774,
8.06209182828128));
#61822=CARTESIAN_POINT('Ctrl Pts',(0.0963972741225356,2.40752073851736,
8.06212325366222));
#61823=CARTESIAN_POINT('Ctrl Pts',(0.0955292675201147,2.40779131148993,
8.06217898766003));
#61824=CARTESIAN_POINT('Ctrl Pts',(0.0951510654583473,2.4079084395101,8.06220328067417));
#61825=CARTESIAN_POINT('Ctrl Pts',(0.094373727649485,2.4081476096914,8.06225323015188));
#61826=CARTESIAN_POINT('Ctrl Pts',(0.0939745688870358,2.40826957395901,
8.06227888911364));
#61827=CARTESIAN_POINT('Ctrl Pts',(0.0929773829730055,2.40857215062055,
8.06234301676043));
#61828=CARTESIAN_POINT('Ctrl Pts',(0.0923790673796352,2.40875179964559,
8.06238151687857));
#61829=CARTESIAN_POINT('Ctrl Pts',(0.0910694708266693,2.40914086899944,
8.06246583854892));
#61830=CARTESIAN_POINT('Ctrl Pts',(0.0903579832691287,2.40934957612252,
8.062511683191));
#61831=CARTESIAN_POINT('Ctrl Pts',(0.0883229911429242,2.4099388994536,8.0626429071377));
#61832=CARTESIAN_POINT('Ctrl Pts',(0.0869977707612186,2.41031348656928,
8.06272848228498));
#61833=CARTESIAN_POINT('Ctrl Pts',(0.0825937519070526,2.41152789925992,
8.06301328618101));
#61834=CARTESIAN_POINT('Ctrl Pts',(0.0795049592836114,2.41233046624247,
8.06321371261066));
#61835=CARTESIAN_POINT('Ctrl Pts',(0.066965101686883,2.41539065667375,8.06403034295932));
#61836=CARTESIAN_POINT('Ctrl Pts',(0.0574268727891681,2.41726599951836,
8.0646584268736));
#61837=CARTESIAN_POINT('Ctrl Pts',(0.0314433697613744,2.42116459415678,
8.06638685156063));
#61838=CARTESIAN_POINT('Ctrl Pts',(0.0149036741358159,2.42235567102332,
8.06750687707209));
#61839=CARTESIAN_POINT('Ctrl Pts',(-0.0208089795883369,2.42217251997626,
8.06992318325287));
#61840=CARTESIAN_POINT('Ctrl Pts',(-0.0399208290263174,2.42036644504946,
8.07121497634501));
#61841=CARTESIAN_POINT('Ctrl Pts',(-0.059876679886445,2.41666582780565,
8.07249429183234));
#61842=CARTESIAN_POINT('Ctrl Pts',(-0.0609913324165863,2.41645303088322,
8.07256550815842));
#61843=CARTESIAN_POINT('Ctrl Pts',(-0.06247992346075,2.41616068840008,8.0726602720277));
#61844=CARTESIAN_POINT('Ctrl Pts',(-0.0628548606445195,2.41608636196811,
8.07268411136308));
#61845=CARTESIAN_POINT('Ctrl Pts',(-0.0634405261655854,2.41596917809562,
8.07272130266208));
#61846=CARTESIAN_POINT('Ctrl Pts',(-0.063651343789003,2.41592677680295,
8.0727346806908));
#61847=CARTESIAN_POINT('Ctrl Pts',(-0.0640553143773882,2.41584510630179,
8.07276029747395));
#61848=CARTESIAN_POINT('Ctrl Pts',(-0.0642484723543551,2.4158058711854,
8.07277253804542));
#61849=CARTESIAN_POINT('Ctrl Pts',(-0.0647051517315274,2.41571267209139,
8.07280145924154));
#61850=CARTESIAN_POINT('Ctrl Pts',(-0.0649686413212397,2.41565855544532,
8.07281813097552));
#61851=CARTESIAN_POINT('Ctrl Pts',(-0.0657409614018235,2.41549892497306,
8.07286695503118));
#61852=CARTESIAN_POINT('Ctrl Pts',(-0.0662496078596602,2.41539250963293,
8.0728990557993));
#61853=CARTESIAN_POINT('Ctrl Pts',(-0.0700190274722311,2.41459437772303,
8.07313655498883));
#61854=CARTESIAN_POINT('Ctrl Pts',(-0.0732693029911311,2.41385330659291,
8.0733391818633));
#61855=CARTESIAN_POINT('Ctrl Pts',(-0.0840935240639338,2.41120802882875,
8.07400850584284));
#61856=CARTESIAN_POINT('Ctrl Pts',(-0.0916101244380889,2.40907889321617,
8.07446430428317));
#61857=CARTESIAN_POINT('Ctrl Pts',(-0.112143208152841,2.40244769105528,
8.07570282561714));
#61858=CARTESIAN_POINT('Ctrl Pts',(-0.12495999630363,2.39738147408969,8.07646887047718));
#61859=CARTESIAN_POINT('Ctrl Pts',(-0.152490164970555,2.38440415157265,
8.07817055229565));
#61860=CARTESIAN_POINT('Ctrl Pts',(-0.166991450120111,2.37613903100072,
8.07910612718435));
#61861=CARTESIAN_POINT('Ctrl Pts',(-0.188398332358233,2.36163288361778,
8.0806146686472));
#61862=CARTESIAN_POINT('Ctrl Pts',(-0.195784282584122,2.3561526646729,8.08116107127087));
#61863=CARTESIAN_POINT('Ctrl Pts',(-0.20380932385925,2.34964821181058,8.08178929736777));
#61864=CARTESIAN_POINT('Ctrl Pts',(-0.204689412312811,2.34892712706179,
8.08185867785068));
#61865=CARTESIAN_POINT('Ctrl Pts',(-0.205964830487254,2.34787079874053,
8.08195993927896));
#61866=CARTESIAN_POINT('Ctrl Pts',(-0.206363205824805,2.34753923233027,
8.08199167064877));
#61867=CARTESIAN_POINT('Ctrl Pts',(-0.20706509940704,2.34695217680815,8.08204775994896));
#61868=CARTESIAN_POINT('Ctrl Pts',(-0.207368949718518,2.34669708493036,
8.08207210161414));
#61869=CARTESIAN_POINT('Ctrl Pts',(-0.207952346974062,2.34620546522189,
8.08211895500641));
#61870=CARTESIAN_POINT('Ctrl Pts',(-0.208231963494635,2.34596902059925,
8.08214146329741));
#61871=CARTESIAN_POINT('Ctrl Pts',(-0.208968140815141,2.34534435170966,
8.08220086086279));
#61872=CARTESIAN_POINT('Ctrl Pts',(-0.209424021156393,2.34495533092078,
8.08223778289992));
#61873=CARTESIAN_POINT('Ctrl Pts',(-0.211084180373076,2.34353062917742,
8.08237275439994));
#61874=CARTESIAN_POINT('Ctrl Pts',(-0.21228186790583,2.34248733361709,8.08247111871724));
#61875=CARTESIAN_POINT('Ctrl Pts',(-0.215185716620661,2.33991981389111,
8.08271206880286));
#61876=CARTESIAN_POINT('Ctrl Pts',(-0.216883433752606,2.33838621072542,
8.08285504530595));
#61877=CARTESIAN_POINT('Ctrl Pts',(-0.223221122955843,2.33253742747787,
8.08339689057492));
#61878=CARTESIAN_POINT('Ctrl Pts',(-0.227749570916298,2.3281040307674,8.08380074562501));
#61879=CARTESIAN_POINT('Ctrl Pts',(-0.236537295890935,2.31897807334195,
8.08461905831328));
#61880=CARTESIAN_POINT('Ctrl Pts',(-0.240794744729038,2.31428759168804,
8.0850333334376));
#61881=CARTESIAN_POINT('Ctrl Pts',(-0.261778803401388,2.2897537385695,8.08716705776583));
#61882=CARTESIAN_POINT('Ctrl Pts',(-0.276201077863411,2.26806967271759,
8.08895650022701));
#61883=CARTESIAN_POINT('Ctrl Pts',(-0.291873112809776,2.23693306167294,
8.0912621531797));
#61884=CARTESIAN_POINT('Ctrl Pts',(-0.295547939101266,2.22881004235692,
8.09184088793663));
#61885=CARTESIAN_POINT('Ctrl Pts',(-0.299148800702242,2.21988194518528,
8.09244501478758));
#61886=CARTESIAN_POINT('Ctrl Pts',(-0.299413751203288,2.21921867033464,
8.09248970855261));
#61887=CARTESIAN_POINT('Ctrl Pts',(-0.299780831841562,2.21829078123557,
8.0925519661125));
#61888=CARTESIAN_POINT('Ctrl Pts',(-0.299884818498321,2.21802691091733,
8.09256964065442));
#61889=CARTESIAN_POINT('Ctrl Pts',(-0.300063901101739,2.21757071704998,
8.09260014502208));
#61890=CARTESIAN_POINT('Ctrl Pts',(-0.300139160585324,2.21737845856768,
8.09261298473829));
#61891=CARTESIAN_POINT('Ctrl Pts',(-0.300295278239088,2.21697850728355,
8.09263966135788));
#61892=CARTESIAN_POINT('Ctrl Pts',(-0.300376105613391,2.21677080318206,
8.09265349631855));
#61893=CARTESIAN_POINT('Ctrl Pts',(-0.30056737738462,2.2162777746808,8.09268629212091));
#61894=CARTESIAN_POINT('Ctrl Pts',(-0.300677631433077,2.21599237556941,
8.0927052414243));
#61895=CARTESIAN_POINT('Ctrl Pts',(-0.301043123260012,2.21504225554338,
8.09276820977808));
#61896=CARTESIAN_POINT('Ctrl Pts',(-0.301296566809617,2.21437683976274,
8.09281212149621));
#61897=CARTESIAN_POINT('Ctrl Pts',(-0.30552105533322,2.20317396645069,8.09354834292224));
#61898=CARTESIAN_POINT('Ctrl Pts',(-0.308939832790488,2.19243497996905,
8.09420852233683));
#61899=CARTESIAN_POINT('Ctrl Pts',(-0.318734983840597,2.15497962738738,
8.0964267746084));
#61900=CARTESIAN_POINT('Ctrl Pts',(-0.322258489260165,2.12764421150429,
8.09791182346188));
#61901=CARTESIAN_POINT('Ctrl Pts',(-0.322274942115673,2.10019315625606,
8.09949688950528));
#61902=CARTESIAN_POINT('',(-0.321965306320612,2.09975328274957,8.22472265507268));
#61903=CARTESIAN_POINT('Ctrl Pts',(-0.321883070004627,2.10020594158585,
8.09972265507268));
#61904=CARTESIAN_POINT('Ctrl Pts',(-0.321488885205279,2.0326703045558,8.10388007865086));
#61905=CARTESIAN_POINT('Ctrl Pts',(-0.267709080667653,1.85696506890364,
8.11466095006996));
#61906=CARTESIAN_POINT('Ctrl Pts',(0.0209181958432102,1.71950360581931,
8.13206526932999));
#61907=CARTESIAN_POINT('Ctrl Pts',(0.331251578158445,1.9116188202888,8.15193561285278));
#61908=CARTESIAN_POINT('Ctrl Pts',(0.337706733343549,2.27654812136149,8.17180595637557));
#61909=CARTESIAN_POINT('Ctrl Pts',(0.0343619353062186,2.47951855594141,
8.19167629989838));
#61910=CARTESIAN_POINT('Ctrl Pts',(-0.262899600533858,2.35063682153811,
8.20931519946406));
#61911=CARTESIAN_POINT('Ctrl Pts',(-0.321458260237508,2.17105380698424,
8.22033065118884));
#61912=CARTESIAN_POINT('Ctrl Pts',(-0.321965306320612,2.09975328274957,
8.22472265507268));
#61913=CARTESIAN_POINT('',(-0.322274858416085,2.100295336748,8.47470128209576));
#61914=CARTESIAN_POINT('Ctrl Pts',(-0.322274896144014,2.09974127163842,
8.22454451420393));
#61915=CARTESIAN_POINT('Ctrl Pts',(-0.322255995347832,2.07619823179053,
8.22610054604818));
#61916=CARTESIAN_POINT('Ctrl Pts',(-0.319657178017348,2.05272766680074,
8.22771693421608));
#61917=CARTESIAN_POINT('Ctrl Pts',(-0.31282525226628,2.02213862653997,8.22980782044883));
#61918=CARTESIAN_POINT('Ctrl Pts',(-0.310848803978768,2.01458880939707,
8.2303218442946));
#61919=CARTESIAN_POINT('Ctrl Pts',(-0.307505365589767,2.00348028881086,
8.23106819917312));
#61920=CARTESIAN_POINT('Ctrl Pts',(-0.306346311450068,1.9998623690893,8.23130966313781));
#61921=CARTESIAN_POINT('Ctrl Pts',(-0.30495080866007,1.99575764893316,8.23158109427415));
#61922=CARTESIAN_POINT('Ctrl Pts',(-0.304776849216764,1.99525012816356,
8.23161461050934));
#61923=CARTESIAN_POINT('Ctrl Pts',(-0.304512624828613,1.99448549296031,
8.2316650368354));
#61924=CARTESIAN_POINT('Ctrl Pts',(-0.304423300925214,1.99422805792199,
8.23168200231245));
#61925=CARTESIAN_POINT('Ctrl Pts',(-0.304262480994648,1.99376645973344,
8.23171240078252));
#61926=CARTESIAN_POINT('Ctrl Pts',(-0.304191106073464,1.99356225572985,
8.23172584093098));
#61927=CARTESIAN_POINT('Ctrl Pts',(-0.304036637645502,1.99312174525002,
8.23175481750411));
#61928=CARTESIAN_POINT('Ctrl Pts',(-0.303953474467364,1.99288546443444,
8.23177034966491));
#61929=CARTESIAN_POINT('Ctrl Pts',(-0.303729090229062,1.99225031595683,
8.23181207474879));
#61930=CARTESIAN_POINT('Ctrl Pts',(-0.303587358358929,1.9918516273249,8.23183823726004));
#61931=CARTESIAN_POINT('Ctrl Pts',(-0.302934708263323,1.99002713011228,
8.23195783675143));
#61932=CARTESIAN_POINT('Ctrl Pts',(-0.302414517224714,1.98860462503037,
8.2320507304143));
#61933=CARTESIAN_POINT('Ctrl Pts',(-0.290661122720945,1.95715321580582,
8.2340978292654));
#61934=CARTESIAN_POINT('Ctrl Pts',(-0.275017226733627,1.92895780443477,
8.23580937968716));
#61935=CARTESIAN_POINT('Ctrl Pts',(-0.251173373899254,1.89795383644452,
8.23802673896079));
#61936=CARTESIAN_POINT('Ctrl Pts',(-0.246701086865196,1.89251679079154,
8.23842950892459));
#61937=CARTESIAN_POINT('Ctrl Pts',(-0.235223364088875,1.87945928945521,
8.2394389324722));
#61938=CARTESIAN_POINT('Ctrl Pts',(-0.228022512535002,1.87202207205858,
8.24005196337986));
#61939=CARTESIAN_POINT('Ctrl Pts',(-0.219650645401829,1.86416943955152,
8.24074999282841));
#61940=CARTESIAN_POINT('Ctrl Pts',(-0.218820219059982,1.86339870890864,
8.24081907704328));
#61941=CARTESIAN_POINT('Ctrl Pts',(-0.217680088669632,1.86235167400246,
8.24091372229927));
#61942=CARTESIAN_POINT('Ctrl Pts',(-0.21737388246518,1.86207155892554,8.24093912138518));
#61943=CARTESIAN_POINT('Ctrl Pts',(-0.216796467180539,1.86154538892985,
8.24098697967823));
#61944=CARTESIAN_POINT('Ctrl Pts',(-0.216525377875889,1.86129920306684,
8.24100943329567));
#61945=CARTESIAN_POINT('Ctrl Pts',(-0.215959565466856,1.86078712562081,
8.24105626664384));
#61946=CARTESIAN_POINT('Ctrl Pts',(-0.215664769695718,1.86052131557226,
8.24108064975591));
#61947=CARTESIAN_POINT('Ctrl Pts',(-0.214982988143061,1.8599088498866,8.24113700087975));
#61948=CARTESIAN_POINT('Ctrl Pts',(-0.214595654431348,1.85956258475887,
8.2411689852191));
#61949=CARTESIAN_POINT('Ctrl Pts',(-0.21335242771577,1.85845657329933,8.24127155140891));
#61950=CARTESIAN_POINT('Ctrl Pts',(-0.212493331604829,1.85770045529584,
8.24134228462895));
#61951=CARTESIAN_POINT('Ctrl Pts',(-0.204537251833345,1.85077291088792,
8.24199607719296));
#61952=CARTESIAN_POINT('Ctrl Pts',(-0.197177991955495,1.84491091934045,
8.2425917920397));
#61953=CARTESIAN_POINT('Ctrl Pts',(-0.186368396457859,1.83704809381521,
8.24345565035917));
#61954=CARTESIAN_POINT('Ctrl Pts',(-0.183120607179277,1.83477608442076,
8.24371382080624));
#61955=CARTESIAN_POINT('Ctrl Pts',(-0.168256252022952,1.82478083104544,
8.2448889410407));
#61956=CARTESIAN_POINT('Ctrl Pts',(-0.156188414067491,1.81775741242609,
8.24582637186048));
#61957=CARTESIAN_POINT('Ctrl Pts',(-0.132347121462362,1.80588026165995,
8.24762772974648));
#61958=CARTESIAN_POINT('Ctrl Pts',(-0.120665092825832,1.8008977847092,8.24848893588757));
#61959=CARTESIAN_POINT('Ctrl Pts',(-0.0997302592355138,1.79339564059978,
8.24996822128051));
#61960=CARTESIAN_POINT('Ctrl Pts',(-0.0906013623910445,1.79057506674255,
8.25059286368307));
#61961=CARTESIAN_POINT('Ctrl Pts',(-0.0804540240822051,1.78792756949624,
8.25125546823024));
#61962=CARTESIAN_POINT('Ctrl Pts',(-0.0795472261459676,1.78769519578758,
8.25131440545272));
#61963=CARTESIAN_POINT('Ctrl Pts',(-0.0779686028522084,1.78729798357846,
8.25141651440416));
#61964=CARTESIAN_POINT('Ctrl Pts',(-0.0772972408954239,1.78713135236047,
8.25145978484391));
#61965=CARTESIAN_POINT('Ctrl Pts',(-0.0763316572703518,1.78689499342699,
8.25152179092407));
#61966=CARTESIAN_POINT('Ctrl Pts',(-0.0760378717655394,1.78682351764239,
8.25154062648893));
#61967=CARTESIAN_POINT('Ctrl Pts',(-0.0755279623172703,1.78670022035226,
8.25157326554582));
#61968=CARTESIAN_POINT('Ctrl Pts',(-0.0753118849150722,1.78664820885966,
8.25158708007219));
#61969=CARTESIAN_POINT('Ctrl Pts',(-0.0748940856722545,1.78654809848911,
8.25161375927465));
#61970=CARTESIAN_POINT('Ctrl Pts',(-0.0746923717178264,1.78649997091347,
8.25162662561923));
#61971=CARTESIAN_POINT('Ctrl Pts',(-0.0742112904962405,1.78638567888054,
8.25165727739857));
#61972=CARTESIAN_POINT('Ctrl Pts',(-0.0739318804191332,1.78631969282802,
8.25167505248091));
#61973=CARTESIAN_POINT('Ctrl Pts',(-0.0729373210322925,1.78608621834283,
8.25173822675518));
#61974=CARTESIAN_POINT('Ctrl Pts',(-0.0722216807667435,1.7859207998511,
8.25178350745024));
#61975=CARTESIAN_POINT('Ctrl Pts',(-0.0615599619685552,1.78349473705332,
8.25245556306786));
#61976=CARTESIAN_POINT('Ctrl Pts',(-0.0515114270030518,1.78170480426918,
8.2530560977969));
#61977=CARTESIAN_POINT('Ctrl Pts',(-0.0241580255962727,1.77816211978753,
8.25464352260644));
#61978=CARTESIAN_POINT('Ctrl Pts',(-0.00676900199513222,1.77732759733156,
8.25560345244038));
#61979=CARTESIAN_POINT('Ctrl Pts',(0.0220277845513836,1.77827556342132,
8.25721874264397));
#61980=CARTESIAN_POINT('Ctrl Pts',(0.0334236257123433,1.77925918005283,
8.25786436917472));
#61981=CARTESIAN_POINT('Ctrl Pts',(0.051242427986826,1.78175721916992,8.25890481099587));
#61982=CARTESIAN_POINT('Ctrl Pts',(0.0577125837788584,1.78286674166639,
8.25928904260863));
#61983=CARTESIAN_POINT('Ctrl Pts',(0.067506178420532,1.78485580832934,8.25988319018327));
#61984=CARTESIAN_POINT('Ctrl Pts',(0.070857068035082,1.78559227071052,8.26008873558658));
#61985=CARTESIAN_POINT('Ctrl Pts',(0.0756095789940844,1.78671661579665,
8.26038375458923));
#61986=CARTESIAN_POINT('Ctrl Pts',(0.0770213913476366,1.78706072087082,
8.26047183681467));
#61987=CARTESIAN_POINT('Ctrl Pts',(0.0794998507213796,1.78768259069385,
8.26062726653322));
#61988=CARTESIAN_POINT('Ctrl Pts',(0.0805674971549476,1.78795630309947,
8.26069448315496));
#61989=CARTESIAN_POINT('Ctrl Pts',(0.0821331235687456,1.78836625318486,
8.26079344395835));
#61990=CARTESIAN_POINT('Ctrl Pts',(0.0826322216510079,1.78849822138338,
8.26082504988412));
#61991=CARTESIAN_POINT('Ctrl Pts',(0.0834915754548075,1.78872765664655,
8.26087957140916));
#61992=CARTESIAN_POINT('Ctrl Pts',(0.083851984000042,1.78882455160146,8.26090246841936));
#61993=CARTESIAN_POINT('Ctrl Pts',(0.0845679481265212,1.78901837097817,
8.2609480160272));
#61994=CARTESIAN_POINT('Ctrl Pts',(0.0849235074327807,1.78911527968882,
8.26097066608611));
#61995=CARTESIAN_POINT('Ctrl Pts',(0.0857607867220597,1.78934502613618,
8.26102407494874));
#61996=CARTESIAN_POINT('Ctrl Pts',(0.0862423644823651,1.78947837452197,
8.26105485031326));
#61997=CARTESIAN_POINT('Ctrl Pts',(0.087664063633908,1.789875603934,8.2611458716149));
#61998=CARTESIAN_POINT('Ctrl Pts',(0.0886032917876881,1.79014263646177,
8.26120622002157));
#61999=CARTESIAN_POINT('Ctrl Pts',(0.0969406660654781,1.79255404727747,
8.26174387036586));
#62000=CARTESIAN_POINT('Ctrl Pts',(0.10426037610646,1.794958586243,8.26222963917548));
#62001=CARTESIAN_POINT('Ctrl Pts',(0.114717113164343,1.79881398516656,8.26294457310198));
#62002=CARTESIAN_POINT('Ctrl Pts',(0.117928374047243,1.80005679070078,8.26316704928007));
#62003=CARTESIAN_POINT('Ctrl Pts',(0.145521566749939,1.81124737832489,8.26510394805226));
#62004=CARTESIAN_POINT('Ctrl Pts',(0.168617334283851,1.82409702523694,8.26690873278305));
#62005=CARTESIAN_POINT('Ctrl Pts',(0.200420973227003,1.84728962164024,8.26954757731479));
#62006=CARTESIAN_POINT('Ctrl Pts',(0.210479180620339,1.85560338473454,8.270407131995));
#62007=CARTESIAN_POINT('Ctrl Pts',(0.220560879729639,1.8650220261108,8.27127321558611));
#62008=CARTESIAN_POINT('Ctrl Pts',(0.221112802813991,1.86554130781846,8.27132064328367));
#62009=CARTESIAN_POINT('Ctrl Pts',(0.221890695934833,1.86627838532623,8.27138750200485));
#62010=CARTESIAN_POINT('Ctrl Pts',(0.222118181917902,1.86649456671921,8.27140705566144));
#62011=CARTESIAN_POINT('Ctrl Pts',(0.22250773376119,1.86686584471434,8.27144054190119));
#62012=CARTESIAN_POINT('Ctrl Pts',(0.222669953814464,1.86702077857953,8.27145448712507));
#62013=CARTESIAN_POINT('Ctrl Pts',(0.222979894059801,1.86731741713022,8.27148113208948));
#62014=CARTESIAN_POINT('Ctrl Pts',(0.223127640820691,1.86745909300031,8.27149383404484));
#62015=CARTESIAN_POINT('Ctrl Pts',(0.223474816027414,1.86779263833444,8.27152368244175));
#62016=CARTESIAN_POINT('Ctrl Pts',(0.223674132903451,1.86798462447203,8.2715408197679));
#62017=CARTESIAN_POINT('Ctrl Pts',(0.224260551239826,1.86855093271814,8.27159124420043));
#62018=CARTESIAN_POINT('Ctrl Pts',(0.224646964538702,1.86892597090661,8.27162447592548));
#62019=CARTESIAN_POINT('Ctrl Pts',(0.227963786366516,1.87216133679109,8.27190978795215));
#62020=CARTESIAN_POINT('Ctrl Pts',(0.230840536355453,1.87507646869592,8.2721576753221));
#62021=CARTESIAN_POINT('Ctrl Pts',(0.254331126491047,1.89980606264411,8.27419371474141));
#62022=CARTESIAN_POINT('Ctrl Pts',(0.271862949925925,1.92434975671978,8.27580295489753));
#62023=CARTESIAN_POINT('Ctrl Pts',(0.291060358721008,1.9611579636798,8.27816189879016));
#62024=CARTESIAN_POINT('Ctrl Pts',(0.295825432924316,1.97162352570644,8.27882566702504));
#62025=CARTESIAN_POINT('Ctrl Pts',(0.301326912092194,1.9856494244943,8.27972045744278));
#62026=CARTESIAN_POINT('Ctrl Pts',(0.302577093982221,1.98899971732683,8.27993453052497));
#62027=CARTESIAN_POINT('Ctrl Pts',(0.304271690262339,1.99378248898462,8.28024092505828));
#62028=CARTESIAN_POINT('Ctrl Pts',(0.304762280734173,1.99519841000071,8.2803317286314));
#62029=CARTESIAN_POINT('Ctrl Pts',(0.30549586282019,1.99736435851528,8.28047079957808));
#62030=CARTESIAN_POINT('Ctrl Pts',(0.305746011003941,1.99811195437565,8.28051883145515));
#62031=CARTESIAN_POINT('Ctrl Pts',(0.306196819816607,1.99947585735974,8.28060651859447));
#62032=CARTESIAN_POINT('Ctrl Pts',(0.306398369558215,2.00009186798982,8.28064614440556));
#62033=CARTESIAN_POINT('Ctrl Pts',(0.306729676281944,2.00111489590947,8.28071198968264));
#62034=CARTESIAN_POINT('Ctrl Pts',(0.306860485345735,2.00152157264853,8.28073817446935));
#62035=CARTESIAN_POINT('Ctrl Pts',(0.307110109638165,2.00230296467212,8.28078850542785));
#62036=CARTESIAN_POINT('Ctrl Pts',(0.307229048700757,2.00267763984534,8.28081264747702));
#62037=CARTESIAN_POINT('Ctrl Pts',(0.307498109728462,2.00353062941936,8.28086762929784));
#62038=CARTESIAN_POINT('Ctrl Pts',(0.307647801462758,2.00400907752602,8.28089848312788));
#62039=CARTESIAN_POINT('Ctrl Pts',(0.308089057640011,2.00543106500771,8.28099022630835));
#62040=CARTESIAN_POINT('Ctrl Pts',(0.308377400126561,2.00637559100586,8.28105122104512));
#62041=CARTESIAN_POINT('Ctrl Pts',(0.310339149882183,2.01290910078152,8.28147354218179));
#62042=CARTESIAN_POINT('Ctrl Pts',(0.311864770852018,2.01854099071496,8.28183966233875));
#62043=CARTESIAN_POINT('Ctrl Pts',(0.321019348210053,2.05637689265291,8.28431529201753));
#62044=CARTESIAN_POINT('Ctrl Pts',(0.323799612953773,2.08954634954697,8.2865913944019));
#62045=CARTESIAN_POINT('Ctrl Pts',(0.320730677539727,2.1333077457305,8.28952219706427));
#62046=CARTESIAN_POINT('Ctrl Pts',(0.319435873417244,2.1440266764052,8.29023140140384));
#62047=CARTESIAN_POINT('Ctrl Pts',(0.317348062861834,2.15615770208835,8.29100985918171));
#62048=CARTESIAN_POINT('Ctrl Pts',(0.317079986355857,2.15765208560087,8.29110532855341));
#62049=CARTESIAN_POINT('Ctrl Pts',(0.316726215694184,2.15954701958721,8.29122579694933));
#62050=CARTESIAN_POINT('Ctrl Pts',(0.316650310758013,2.15994934487509,8.29125134049104));
#62051=CARTESIAN_POINT('Ctrl Pts',(0.316527763073654,2.16059216815155,8.29129209786023));
#62052=CARTESIAN_POINT('Ctrl Pts',(0.316481612760247,2.16083275781478,8.29130733973422));
#62053=CARTESIAN_POINT('Ctrl Pts',(0.316393632298905,2.16128860539198,8.29133619485268));
#62054=CARTESIAN_POINT('Ctrl Pts',(0.316351857127204,2.16150387144435,8.29134981107063));
#62055=CARTESIAN_POINT('Ctrl Pts',(0.316255804313102,2.16199614132562,8.29138092569395));
#62056=CARTESIAN_POINT('Ctrl Pts',(0.3162013825176,2.16227311616107,8.29139841571307));
#62057=CARTESIAN_POINT('Ctrl Pts',(0.31603306901943,2.1631238231516,8.29145208503395));
#62058=CARTESIAN_POINT('Ctrl Pts',(0.315917978380196,2.16369732107371,8.29148819600614));
#62059=CARTESIAN_POINT('Ctrl Pts',(0.315043511355309,2.16799412617874,8.2917582473801));
#62060=CARTESIAN_POINT('Ctrl Pts',(0.314219857622185,2.17170424948038,8.29198859868031));
#62061=CARTESIAN_POINT('Ctrl Pts',(0.306117238230526,2.20537572071285,8.29406048866452));
#62062=CARTESIAN_POINT('Ctrl Pts',(0.29463850933332,2.23416612043077,8.29570948487915));
#62063=CARTESIAN_POINT('Ctrl Pts',(0.272021860239076,2.27341973789832,8.29828754604229));
#62064=CARTESIAN_POINT('Ctrl Pts',(0.263968165960037,2.28544817587149,8.2991283592283));
#62065=CARTESIAN_POINT('Ctrl Pts',(0.254184382675395,2.29812595845684,8.30009484875323));
#62066=CARTESIAN_POINT('Ctrl Pts',(0.25322503670252,2.29935063698686,8.30018908140717));
#62067=CARTESIAN_POINT('Ctrl Pts',(0.251752675637069,2.30120244103574,8.30033292084229));
#62068=CARTESIAN_POINT('Ctrl Pts',(0.251246091442515,2.30183466869024,8.30038227191472));
#62069=CARTESIAN_POINT('Ctrl Pts',(0.25030747279461,2.30299707491932,8.30047346054869));
#62070=CARTESIAN_POINT('Ctrl Pts',(0.249876123208658,2.30352780252703,8.30051527048573));
#62071=CARTESIAN_POINT('Ctrl Pts',(0.249173402209867,2.30438682117714,8.30058322974469));
#62072=CARTESIAN_POINT('Ctrl Pts',(0.248903062038938,2.3047159562531,8.30060933728236));
#62073=CARTESIAN_POINT('Ctrl Pts',(0.248381790471071,2.30534803756207,8.30065960802339));
#62074=CARTESIAN_POINT('Ctrl Pts',(0.248130955176592,2.3056510623585,8.30068376729336));
#62075=CARTESIAN_POINT('Ctrl Pts',(0.247557736704661,2.30634097080579,8.30073890699828));
#62076=CARTESIAN_POINT('Ctrl Pts',(0.247235000817604,2.30672755888255,8.30076990179382));
#62077=CARTESIAN_POINT('Ctrl Pts',(0.246247686062536,2.30790459158825,8.30086456965716));
#62078=CARTESIAN_POINT('Ctrl Pts',(0.245580217643585,2.30869259391986,8.30092836105402));
#62079=CARTESIAN_POINT('Ctrl Pts',(0.240688526905232,2.31441167948182,8.30139438356912));
#62080=CARTESIAN_POINT('Ctrl Pts',(0.236320188553444,2.31921700179485,8.30180257258702));
#62081=CARTESIAN_POINT('Ctrl Pts',(0.230559261812351,2.32518180105656,8.3023315934675));
#62082=CARTESIAN_POINT('Ctrl Pts',(0.229297765532181,2.32646622541267,8.3024468902202));
#62083=CARTESIAN_POINT('Ctrl Pts',(0.223608901927806,2.33216222321378,8.30296442255023));
#62084=CARTESIAN_POINT('Ctrl Pts',(0.219064741631382,2.33645479486463,8.30337140916914));
#62085=CARTESIAN_POINT('Ctrl Pts',(0.196763273493759,2.35632663462441,8.30533777969493));
#62086=CARTESIAN_POINT('Ctrl Pts',(0.177454028160258,2.37005372547209,8.30695707265761));
#62087=CARTESIAN_POINT('Ctrl Pts',(0.149082864337998,2.38585650783233,8.30913077668616));
#62088=CARTESIAN_POINT('Ctrl Pts',(0.141169058535459,2.38984645238553,8.30971651174549));
#62089=CARTESIAN_POINT('Ctrl Pts',(0.129558740692125,2.39511155589719,8.31053718738767));
#62090=CARTESIAN_POINT('Ctrl Pts',(0.125988193025744,2.39665346163708,8.31078448009236));
#62091=CARTESIAN_POINT('Ctrl Pts',(0.121891378278172,2.39833531225558,8.31106175375366));
#62092=CARTESIAN_POINT('Ctrl Pts',(0.121391820428101,2.39853892975686,8.31109545548291));
#62093=CARTESIAN_POINT('Ctrl Pts',(0.120638593145714,2.39884373851871,8.31114610469839));
#62094=CARTESIAN_POINT('Ctrl Pts',(0.120385305673937,2.39894586196691,8.31116310830342));
#62095=CARTESIAN_POINT('Ctrl Pts',(0.119931112370513,2.39912831816193,8.31119354815077));
#62096=CARTESIAN_POINT('Ctrl Pts',(0.119730255867269,2.39920877037899,8.31120699163204));
#62097=CARTESIAN_POINT('Ctrl Pts',(0.119297092820497,2.39938176597631,8.31123594506605));
#62098=CARTESIAN_POINT('Ctrl Pts',(0.119064760226522,2.39947424100869,8.31125145081788));
#62099=CARTESIAN_POINT('Ctrl Pts',(0.118440710375996,2.39972178973153,8.31129303631262));
#62100=CARTESIAN_POINT('Ctrl Pts',(0.118048794587964,2.39987636655022,8.31131908599037));
#62101=CARTESIAN_POINT('Ctrl Pts',(0.116262508225279,2.40057685720457,8.31143751674716));
#62102=CARTESIAN_POINT('Ctrl Pts',(0.114864617323409,2.40111382863789,8.31152936731556));
#62103=CARTESIAN_POINT('Ctrl Pts',(0.0833370490654287,2.41297299891607,
8.31358341059271));
#62104=CARTESIAN_POINT('Ctrl Pts',(0.0516778241459738,2.41973018248313,
8.3153008581447));
#62105=CARTESIAN_POINT('Ctrl Pts',(0.00400927344428922,2.42262534987356,
8.31800903592352));
#62106=CARTESIAN_POINT('Ctrl Pts',(-0.0115648770916579,2.42244278508247,
8.31891017150142));
#62107=CARTESIAN_POINT('Ctrl Pts',(-0.0295162987467325,2.42092993248103,
8.3199967787625));
#62108=CARTESIAN_POINT('Ctrl Pts',(-0.0319663677915664,2.4206951578455,
8.32014608800993));
#62109=CARTESIAN_POINT('Ctrl Pts',(-0.035118162808726,2.42035666468081,
8.32033953309254));
#62110=CARTESIAN_POINT('Ctrl Pts',(-0.0358226134232033,2.42027865729606,
8.32038285794817));
#62111=CARTESIAN_POINT('Ctrl Pts',(-0.0369582616171983,2.42014910761688,
8.32045284671485));
#62112=CARTESIAN_POINT('Ctrl Pts',(-0.0373896250489441,2.42009901615817,
8.3204794648386));
#62113=CARTESIAN_POINT('Ctrl Pts',(-0.038211652044458,2.42000187515843,
8.32053025431114));
#62114=CARTESIAN_POINT('Ctrl Pts',(-0.0386023335506537,2.41995498167576,
8.3205544206931));
#62115=CARTESIAN_POINT('Ctrl Pts',(-0.0394937355143449,2.41984633031453,
8.32060962419098));
#62116=CARTESIAN_POINT('Ctrl Pts',(-0.0399943978858773,2.41978411200947,
8.32064067578934));
#62117=CARTESIAN_POINT('Ctrl Pts',(-0.041524001538584,2.41959037679496,
8.32073568565396));
#62118=CARTESIAN_POINT('Ctrl Pts',(-0.0425524481596547,2.41945506845101,
8.32079976350455));
#62119=CARTESIAN_POINT('Ctrl Pts',(-0.0501122391539524,2.41842330508963,
8.32127225138458));
#62120=CARTESIAN_POINT('Ctrl Pts',(-0.0566149458339473,2.41733164874971,
8.32168680680054));
#62121=CARTESIAN_POINT('Ctrl Pts',(-0.064876279194895,2.41568275534116,
8.32222447841607));
#62122=CARTESIAN_POINT('Ctrl Pts',(-0.0666701970753574,2.41530876649616,
8.32234189744928));
#62123=CARTESIAN_POINT('Ctrl Pts',(-0.072661012976683,2.41400641449459,
8.32273625455804));
#62124=CARTESIAN_POINT('Ctrl Pts',(-0.0768423816233633,2.41300941986759,
8.32301519030779));
#62125=CARTESIAN_POINT('Ctrl Pts',(-0.105648435930526,2.40552900275532,
8.32496203457186));
#62126=CARTESIAN_POINT('Ctrl Pts',(-0.129447740793255,2.39623060791731,
8.32670900758343));
#62127=CARTESIAN_POINT('Ctrl Pts',(-0.161937044286073,2.37886747709717,
8.3291745575876));
#62128=CARTESIAN_POINT('Ctrl Pts',(-0.171683579581393,2.37297524388826,
8.32992430557303));
#62129=CARTESIAN_POINT('Ctrl Pts',(-0.181952223863904,2.3659993009728,8.33070969475765));
#62130=CARTESIAN_POINT('Ctrl Pts',(-0.182802791802399,2.36541548421857,
8.33077471261378));
#62131=CARTESIAN_POINT('Ctrl Pts',(-0.184264653831585,2.3644017236102,8.3308863733415));
#62132=CARTESIAN_POINT('Ctrl Pts',(-0.184877276955737,2.36397372329758,
8.3309331411664));
#62133=CARTESIAN_POINT('Ctrl Pts',(-0.185743592255013,2.36336398944111,
8.33099923269483));
#62134=CARTESIAN_POINT('Ctrl Pts',(-0.185998511843769,2.36318401659677,
8.33101867527838));
#62135=CARTESIAN_POINT('Ctrl Pts',(-0.186435962630036,2.36287422397991,
8.33105202968345));
#62136=CARTESIAN_POINT('Ctrl Pts',(-0.18661862027742,2.36274458388653,8.33106595389455));
#62137=CARTESIAN_POINT('Ctrl Pts',(-0.186968250658633,2.3624958874427,8.33109260080698));
#62138=CARTESIAN_POINT('Ctrl Pts',(-0.187135244663637,2.36237686232584,
8.33110532564177));
#62139=CARTESIAN_POINT('Ctrl Pts',(-0.187528526363154,2.36209598399671,
8.33113528776981));
#62140=CARTESIAN_POINT('Ctrl Pts',(-0.187754718737168,2.36193399668699,
8.33115251577308));
#62141=CARTESIAN_POINT('Ctrl Pts',(-0.188422738581413,2.36145428542849,
8.33120338346171));
#62142=CARTESIAN_POINT('Ctrl Pts',(-0.188863974165728,2.36113573301246,
8.33123696637981));
#62143=CARTESIAN_POINT('Ctrl Pts',(-0.192744428215652,2.35831923835979,
8.33153219260575));
#62144=CARTESIAN_POINT('Ctrl Pts',(-0.196134920719671,2.35575445378477,
8.33178931511299));
#62145=CARTESIAN_POINT('Ctrl Pts',(-0.200199106889556,2.35255166962367,
8.33209784960425));
#62146=CARTESIAN_POINT('Ctrl Pts',(-0.200921890638701,2.35197702698514,
8.33215273267425));
#62147=CARTESIAN_POINT('Ctrl Pts',(-0.201730786758905,2.35132822800901,
8.33221418134362));
#62148=CARTESIAN_POINT('Ctrl Pts',(-0.201819333610174,2.35125712945452,
8.33222090826365));
#62149=CARTESIAN_POINT('Ctrl Pts',(-0.217084600729435,2.33898663128751,
8.33338067948435));
#62150=CARTESIAN_POINT('Ctrl Pts',(-0.231126217796276,2.32543551820192,
8.3344605382151));
#62151=CARTESIAN_POINT('Ctrl Pts',(-0.260778874754767,2.29111589421998,
8.33699638420464));
#62152=CARTESIAN_POINT('Ctrl Pts',(-0.275275200653457,2.26957061701527,
8.33845637976977));
#62153=CARTESIAN_POINT('Ctrl Pts',(-0.287564354508336,2.24549657303681,
8.34009997474716));
#62154=CARTESIAN_POINT('Ctrl Pts',(-0.288084159677424,2.24446462417411,
8.34017042873191));
#62155=CARTESIAN_POINT('Ctrl Pts',(-0.288833072790938,2.2429577200604,8.3402733177258));
#62156=CARTESIAN_POINT('Ctrl Pts',(-0.289066586456472,2.24248495447557,
8.34030559860681));
#62157=CARTESIAN_POINT('Ctrl Pts',(-0.289473756932274,2.24165548723899,
8.34036223838518));
#62158=CARTESIAN_POINT('Ctrl Pts',(-0.289647917755419,2.24129903310028,
8.34038657964588));
#62159=CARTESIAN_POINT('Ctrl Pts',(-0.289984367652972,2.24060718675741,
8.34043382615094));
#62160=CARTESIAN_POINT('Ctrl Pts',(-0.290146734237677,2.24027183274031,
8.34045672865102));
#62161=CARTESIAN_POINT('Ctrl Pts',(-0.290532301513119,2.23947194346743,
8.34051135869919));
#62162=CARTESIAN_POINT('Ctrl Pts',(-0.290754969650857,2.23900715397236,
8.34054310468744));
#62163=CARTESIAN_POINT('Ctrl Pts',(-0.291422828228239,2.23760446455367,
8.34063891898839));
#62164=CARTESIAN_POINT('Ctrl Pts',(-0.29186459914382,2.23666495236097,8.34070310556189));
#62165=CARTESIAN_POINT('Ctrl Pts',(-0.296386475694923,2.22692637069945,
8.3413685785848));
#62166=CARTESIAN_POINT('Ctrl Pts',(-0.300071533507521,2.21795036559158,
8.34198337493987));
#62167=CARTESIAN_POINT('Ctrl Pts',(-0.304702522471836,2.20504135540363,
8.34287080321147));
#62168=CARTESIAN_POINT('Ctrl Pts',(-0.305988146833679,2.2012351988422,8.34313281083461));
#62169=CARTESIAN_POINT('Ctrl Pts',(-0.314529584705017,2.17429696507946,
8.3449890988564));
#62170=CARTESIAN_POINT('Ctrl Pts',(-0.319225504080827,2.15043574997385,
8.34665142814623));
#62171=CARTESIAN_POINT('Ctrl Pts',(-0.321918916382813,2.11751334094391,
8.34886255247666));
#62172=CARTESIAN_POINT('Ctrl Pts',(-0.322276976597949,2.10872244622439,
8.34944413543821));
#62173=CARTESIAN_POINT('Ctrl Pts',(-0.322274112328226,2.09603013592404,
8.35026164780834));
#62174=CARTESIAN_POINT('Ctrl Pts',(-0.322202543125355,2.09213311512152,
8.35050962374752));
#62175=CARTESIAN_POINT('Ctrl Pts',(-0.322038789492845,2.08764925349233,
8.35079072369609));
#62176=CARTESIAN_POINT('Ctrl Pts',(-0.32201566754641,2.08706041944243,8.35082755472705));
#62177=CARTESIAN_POINT('Ctrl Pts',(-0.321979045376265,2.08618876815533,
8.350881948255));
#62178=CARTESIAN_POINT('Ctrl Pts',(-0.32196678749655,2.08590590417565,8.35089957989809));
#62179=CARTESIAN_POINT('Ctrl Pts',(-0.32194436986702,2.08540388867636,8.35093083609994));
#62180=CARTESIAN_POINT('Ctrl Pts',(-0.321934359105089,2.08518473140471,
8.35094446904338));
#62181=CARTESIAN_POINT('Ctrl Pts',(-0.321912718568679,2.08472135390612,
8.35097326828698));
#62182=CARTESIAN_POINT('Ctrl Pts',(-0.321901034695205,2.08447713731783,
8.35098843146677));
#62183=CARTESIAN_POINT('Ctrl Pts',(-0.321869147169632,2.08382614457258,
8.35102881141952));
#62184=CARTESIAN_POINT('Ctrl Pts',(-0.321848450236824,2.08341939133873,
8.35105400041887));
#62185=CARTESIAN_POINT('Ctrl Pts',(-0.32174814382633,2.08151907384536,8.35117149336452));
#62186=CARTESIAN_POINT('Ctrl Pts',(-0.321658906930937,2.08002600483372,
8.35126326430161));
#62187=CARTESIAN_POINT('Ctrl Pts',(-0.320859447470214,2.06805039015372,
8.35199537142328));
#62188=CARTESIAN_POINT('Ctrl Pts',(-0.31964730836709,2.05760648607181,8.3526094877765));
#62189=CARTESIAN_POINT('Ctrl Pts',(-0.313399767065271,2.0199598011947,8.35479375427832));
#62190=CARTESIAN_POINT('Ctrl Pts',(-0.305380696477646,1.99337634306458,
8.35628978082287));
#62191=CARTESIAN_POINT('Ctrl Pts',(-0.29251938846195,1.96469343297168,8.35810796097955));
#62192=CARTESIAN_POINT('Ctrl Pts',(-0.290912543196602,1.96127238765257,
8.3583281322873));
#62193=CARTESIAN_POINT('Ctrl Pts',(-0.285875503296402,1.95102085177581,
8.35899908790642));
#62194=CARTESIAN_POINT('Ctrl Pts',(-0.282262344403604,1.94428376946158,
8.35945536209082));
#62195=CARTESIAN_POINT('Ctrl Pts',(-0.2779226613954,1.93684020385766,8.35997957399958));
#62196=CARTESIAN_POINT('Ctrl Pts',(-0.27742815590886,1.93600078332297,8.36003898418915));
#62197=CARTESIAN_POINT('Ctrl Pts',(-0.276674560084789,1.93473472064,8.36012904111841));
#62198=CARTESIAN_POINT('Ctrl Pts',(-0.276418269242805,1.93430641175822,
8.36015958585972));
#62199=CARTESIAN_POINT('Ctrl Pts',(-0.275971095500023,1.93356302759901,
8.36021273745393));
#62200=CARTESIAN_POINT('Ctrl Pts',(-0.275780664954729,1.93324768016969,
8.36023532774009));
#62201=CARTESIAN_POINT('Ctrl Pts',(-0.275382614641563,1.93259106730347,
8.36028245525117));
#62202=CARTESIAN_POINT('Ctrl Pts',(-0.27517490032497,1.93224986014218,8.36030699591665));
#62203=CARTESIAN_POINT('Ctrl Pts',(-0.274683013387382,1.93144522164978,
8.36036498894045));
#62204=CARTESIAN_POINT('Ctrl Pts',(-0.274398302162044,1.93098212250452,
8.3603984610604));
#62205=CARTESIAN_POINT('Ctrl Pts',(-0.273457757713399,1.92946091331325,
8.36050872638518));
#62206=CARTESIAN_POINT('Ctrl Pts',(-0.272796971398159,1.92840589267734,
8.36058570214581));
#62207=CARTESIAN_POINT('Ctrl Pts',(-0.271234714189636,1.92594340282012,
8.36076656173354));
#62208=CARTESIAN_POINT('Ctrl Pts',(-0.270328380099697,1.9245390757275,8.36087062514322));
#62209=CARTESIAN_POINT('Ctrl Pts',(-0.264722303532908,1.91599923762277,
8.36150916704484));
#62210=CARTESIAN_POINT('Ctrl Pts',(-0.259751634075699,1.90904648453232,
8.3620537711795));
#62211=CARTESIAN_POINT('Ctrl Pts',(-0.245685032853088,1.89093772043069,
8.3635413631272));
#62212=CARTESIAN_POINT('Ctrl Pts',(-0.236109014993976,1.88018046450449,
8.36450105773741));
#62213=CARTESIAN_POINT('Ctrl Pts',(-0.210723619630669,1.8552425705878,8.36690194105967));
#62214=CARTESIAN_POINT('Ctrl Pts',(-0.194169971108228,1.8419132634194,8.36835205146717));
#62215=CARTESIAN_POINT('Ctrl Pts',(-0.176315920496391,1.8302336395527,8.36973294610763));
#62216=CARTESIAN_POINT('Ctrl Pts',(-0.176205410938968,1.83016144418298,
8.36974148657233));
#62217=CARTESIAN_POINT('Ctrl Pts',(-0.175903749687777,1.82996463465255,
8.36976478131237));
#62218=CARTESIAN_POINT('Ctrl Pts',(-0.175712509591243,1.8298401553408,8.36977952899657));
#62219=CARTESIAN_POINT('Ctrl Pts',(-0.171899896619578,1.82736426382098,
8.37007313877608));
#62220=CARTESIAN_POINT('Ctrl Pts',(-0.168231536846383,1.82508551576612,
8.3703483885368));
#62221=CARTESIAN_POINT('Ctrl Pts',(-0.164048256972519,1.8226020119296,8.37065324280955));
#62222=CARTESIAN_POINT('Ctrl Pts',(-0.163577527748032,1.82232416952954,
8.37068741999957));
#62223=CARTESIAN_POINT('Ctrl Pts',(-0.162865609188858,1.82190640655792,
8.37073891457079));
#62224=CARTESIAN_POINT('Ctrl Pts',(-0.162624944383984,1.82176560091257,
8.37075628896612));
#62225=CARTESIAN_POINT('Ctrl Pts',(-0.162206825123207,1.82152169990013,
8.37078641604224));
#62226=CARTESIAN_POINT('Ctrl Pts',(-0.162029454883633,1.82141846167825,
8.3707991780456));
#62227=CARTESIAN_POINT('Ctrl Pts',(-0.161658411584607,1.82120297042727,
8.37082583684298));
#62228=CARTESIAN_POINT('Ctrl Pts',(-0.161464720298202,1.82109074982354,
8.37083973145648));
#62229=CARTESIAN_POINT('Ctrl Pts',(-0.161001374931853,1.82082294181753,
8.37087291831654));
#62230=CARTESIAN_POINT('Ctrl Pts',(-0.160731611086281,1.82066754262183,
8.37089219827109));
#62231=CARTESIAN_POINT('Ctrl Pts',(-0.159817226633964,1.82014256877044,
8.3709574093419));
#62232=CARTESIAN_POINT('Ctrl Pts',(-0.159171547042178,1.81977482914385,
8.37100322233764));
#62233=CARTESIAN_POINT('Ctrl Pts',(-0.157632852281189,1.81890551672235,
8.37111185406888));
#62234=CARTESIAN_POINT('Ctrl Pts',(-0.156738700406101,1.81840595797006,
8.37117454781781));
#62235=CARTESIAN_POINT('Ctrl Pts',(-0.146015241581794,1.81248171037654,
8.37192144240463));
#62236=CARTESIAN_POINT('Ctrl Pts',(-0.13591015483748,1.80756931447792,8.37257542789105));
#62237=CARTESIAN_POINT('Ctrl Pts',(-0.114987700837369,1.79871776199675,
8.37387164294198));
#62238=CARTESIAN_POINT('Ctrl Pts',(-0.104175069907032,1.79481033373575,
8.37451241336183));
#62239=CARTESIAN_POINT('Ctrl Pts',(-0.0681977911061162,1.78394448654688,
8.37661313558764));
#62240=CARTESIAN_POINT('Ctrl Pts',(-0.0423996271884223,1.77946289505241,
8.37808015783452));
#62241=CARTESIAN_POINT('Ctrl Pts',(-0.0148020113481421,1.77806139810893,
8.37975573076812));
#62242=CARTESIAN_POINT('Ctrl Pts',(-0.0132583878551417,1.77799413367224,
8.37984976039698));
#62243=CARTESIAN_POINT('Ctrl Pts',(-0.0111638324911713,1.77791794841732,
8.37997778829323));
#62244=CARTESIAN_POINT('Ctrl Pts',(-0.0106132562710758,1.77789933577686,
8.38001148284188));
#62245=CARTESIAN_POINT('Ctrl Pts',(-0.00968059233818868,1.77787020029484,
8.38006863115311));
#62246=CARTESIAN_POINT('Ctrl Pts',(-0.00929852734156827,1.77785894531533,
8.38009206194372));
#62247=CARTESIAN_POINT('Ctrl Pts',(-0.00856297469243163,1.77783858684496,
8.38013720988414));
#62248=CARTESIAN_POINT('Ctrl Pts',(-0.00820949009489424,1.77782938536787,
8.3801589239324));
#62249=CARTESIAN_POINT('Ctrl Pts',(-0.00737591060267823,1.77780905943351,
8.38021017063445));
#62250=CARTESIAN_POINT('Ctrl Pts',(-0.0068958055477118,1.77779842628839,
8.38023971863681));
#62251=CARTESIAN_POINT('Ctrl Pts',(-0.00549721487744029,1.77777057836495,
8.38032588936334));
#62252=CARTESIAN_POINT('Ctrl Pts',(-0.00457868290780011,1.77775621778919,
8.38038260136456));
#62253=CARTESIAN_POINT('Ctrl Pts',(0.0020123287590675,1.77768135817776,
8.38079041227238));
#62254=CARTESIAN_POINT('Ctrl Pts',(0.00768516421377774,1.77776671808107,
8.38114605540946));
#62255=CARTESIAN_POINT('Ctrl Pts',(0.0261250649637962,1.7785313776521,8.38231823212648));
#62256=CARTESIAN_POINT('Ctrl Pts',(0.0388533011378991,1.77982044408159,
8.38315311713507));
#62257=CARTESIAN_POINT('Ctrl Pts',(0.0796599171670877,1.78642236011341,
8.38590523017834));
#62258=CARTESIAN_POINT('Ctrl Pts',(0.107116888338767,1.79470906028241,8.38788587532245));
#62259=CARTESIAN_POINT('Ctrl Pts',(0.136780512800453,1.8081637392716,8.3899855218027));
#62260=CARTESIAN_POINT('Ctrl Pts',(0.140407643486822,1.80989138397474,8.39024125840119));
#62261=CARTESIAN_POINT('Ctrl Pts',(0.14453358337266,1.81195213532323,8.39053021461082));
#62262=CARTESIAN_POINT('Ctrl Pts',(0.145064712788122,1.81221925327693,8.39056737415495));
#62263=CARTESIAN_POINT('Ctrl Pts',(0.145845894700233,1.81261484093938,8.39062196936374));
#62264=CARTESIAN_POINT('Ctrl Pts',(0.146096519265338,1.81274216858507,8.39063947606104));
#62265=CARTESIAN_POINT('Ctrl Pts',(0.14654274463031,1.81296960456806,8.39067062954465));
#62266=CARTESIAN_POINT('Ctrl Pts',(0.146738409723914,1.81306958505861,8.39068428438318));
#62267=CARTESIAN_POINT('Ctrl Pts',(0.147150279987368,1.81328057304923,8.39071301547411));
#62268=CARTESIAN_POINT('Ctrl Pts',(0.147366461313003,1.81339162473445,8.39072808883609));
#62269=CARTESIAN_POINT('Ctrl Pts',(0.147938790227462,1.81368644708487,8.39076797695414));
#62270=CARTESIAN_POINT('Ctrl Pts',(0.148294722433425,1.81387063845286,8.39079276512074));
#62271=CARTESIAN_POINT('Ctrl Pts',(0.149891275716121,1.81470061818552,8.39090387564516));
#62272=CARTESIAN_POINT('Ctrl Pts',(0.151128052745254,1.81535382728715,8.39098973571893));
#62273=CARTESIAN_POINT('Ctrl Pts',(0.160656583402995,1.82046597308272,8.39164988801422));
#62274=CARTESIAN_POINT('Ctrl Pts',(0.168754472454573,1.82527873234048,8.3922030728907));
#62275=CARTESIAN_POINT('Ctrl Pts',(0.200645091961242,1.8461752214554,8.39439686892825));
#62276=CARTESIAN_POINT('Ctrl Pts',(0.222449475160951,1.86504917268763,8.39594460023162));
#62277=CARTESIAN_POINT('Ctrl Pts',(0.249012395592701,1.89510043033793,8.39826316738812));
#62278=CARTESIAN_POINT('Ctrl Pts',(0.25609982618789,1.90403101956672,8.39893606448791));
#62279=CARTESIAN_POINT('Ctrl Pts',(0.26339430895806,1.91429578825574,8.39970155486363));
#62280=CARTESIAN_POINT('Ctrl Pts',(0.26408409927393,1.91527803405993,8.39977472404634));
#62281=CARTESIAN_POINT('Ctrl Pts',(0.265043186872483,1.9166601051141,8.39987757214404));
#62282=CARTESIAN_POINT('Ctrl Pts',(0.265317104500601,1.91705672458457,8.39990707493418));
#62283=CARTESIAN_POINT('Ctrl Pts',(0.265817034317198,1.91778408312762,8.39996115868353));
#62284=CARTESIAN_POINT('Ctrl Pts',(0.266043321968399,1.91811463245067,8.39998572912189));
#62285=CARTESIAN_POINT('Ctrl Pts',(0.266499715445926,1.91878398242116,8.4000354675717));
#62286=CARTESIAN_POINT('Ctrl Pts',(0.266729792870285,1.91912280145688,8.40006063659699));
#62287=CARTESIAN_POINT('Ctrl Pts',(0.267286287777501,1.91994568359164,8.4001217448425));
#62288=CARTESIAN_POINT('Ctrl Pts',(0.267612036032181,1.92043019559317,8.40015770924133));
#62289=CARTESIAN_POINT('Ctrl Pts',(0.268763226097576,1.92215254424173,8.40028550107465));
#62290=CARTESIAN_POINT('Ctrl Pts',(0.26958140090896,1.92339519432673,8.40037760104398));
#62291=CARTESIAN_POINT('Ctrl Pts',(0.280262733450074,1.93986526874697,8.4015970931591));
#62292=CARTESIAN_POINT('Ctrl Pts',(0.288829797175336,1.95589074399111,8.40277306604974));
#62293=CARTESIAN_POINT('Ctrl Pts',(0.304123502124761,1.99141015214696,8.40535141409662));
#62294=CARTESIAN_POINT('Ctrl Pts',(0.310422819527596,2.01100293492122,8.40675790509365));
#62295=CARTESIAN_POINT('Ctrl Pts',(0.315502735721852,2.0342008423504,8.40834194451299));
#62296=CARTESIAN_POINT('Ctrl Pts',(0.316143264527338,2.03735063632381,8.40855524728323));
#62297=CARTESIAN_POINT('Ctrl Pts',(0.316942815293981,2.04160757229913,8.4088407193618));
#62298=CARTESIAN_POINT('Ctrl Pts',(0.31714333796636,2.04270665816837,8.40891417353523));
#62299=CARTESIAN_POINT('Ctrl Pts',(0.317738036289297,2.04606507845205,8.40913781640207));
#62300=CARTESIAN_POINT('Ctrl Pts',(0.318113821739515,2.04832764351941,8.40928737142928));
#62301=CARTESIAN_POINT('Ctrl Pts',(0.318547934559806,2.05112588990915,8.40947081292755));
#62302=CARTESIAN_POINT('Ctrl Pts',(0.318629105927412,2.05165790537173,8.40950562189478));
#62303=CARTESIAN_POINT('Ctrl Pts',(0.319345581933388,2.05643405909756,8.40981749600457));
#62304=CARTESIAN_POINT('Ctrl Pts',(0.319897426308408,2.06069054819696,8.41009103224958));
#62305=CARTESIAN_POINT('Ctrl Pts',(0.320423449612298,2.06549947362142,8.41039417013517));
#62306=CARTESIAN_POINT('Ctrl Pts',(0.320481406564421,2.06604206368645,8.41042828865567));
#62307=CARTESIAN_POINT('Ctrl Pts',(0.320566871198163,2.06686189011352,8.4104797097972));
#62308=CARTESIAN_POINT('Ctrl Pts',(0.320595397591823,2.06713901582408,8.41049706920583));
#62309=CARTESIAN_POINT('Ctrl Pts',(0.320644308151127,2.06762029388172,8.41052717748673));
#62310=CARTESIAN_POINT('Ctrl Pts',(0.320664856717466,2.06782442875524,8.41053993565342));
#62311=CARTESIAN_POINT('Ctrl Pts',(0.320707422895147,2.06825138336867,8.41056659382704));
#62312=CARTESIAN_POINT('Ctrl Pts',(0.320729403220996,2.06847420630827,8.41058049164128));
#62313=CARTESIAN_POINT('Ctrl Pts',(0.320781417591502,2.06900718069372,8.41061369906985));
#62314=CARTESIAN_POINT('Ctrl Pts',(0.320811234171217,2.06931735421999,8.41063299635232));
#62315=CARTESIAN_POINT('Ctrl Pts',(0.320908662582816,2.07034654392444,8.41069693426005));
#62316=CARTESIAN_POINT('Ctrl Pts',(0.320974308035185,2.07106575069344,8.41074146474658));
#62317=CARTESIAN_POINT('Ctrl Pts',(0.321125059428692,2.07278104982611,8.41084732506675));
#62318=CARTESIAN_POINT('Ctrl Pts',(0.321207949788138,2.07377733624378,8.41090853460866));
#62319=CARTESIAN_POINT('Ctrl Pts',(0.322126593262677,2.08547746936625,8.41162428623593));
#62320=CARTESIAN_POINT('Ctrl Pts',(0.322431683697765,2.09621749507579,8.41225115407617));
#62321=CARTESIAN_POINT('Ctrl Pts',(0.321724317202829,2.12899278310915,8.41412562405545));
#62322=CARTESIAN_POINT('Ctrl Pts',(0.318988739280889,2.15092524378861,8.41533045696976));
#62323=CARTESIAN_POINT('Ctrl Pts',(0.313972921640174,2.17267914297819,8.41659862160365));
#62324=CARTESIAN_POINT('Ctrl Pts',(0.313909932427393,2.17295072083493,8.41661446456874));
#62325=CARTESIAN_POINT('Ctrl Pts',(0.312661413783001,2.17830214749635,8.41692687132574));
#62326=CARTESIAN_POINT('Ctrl Pts',(0.311353112126086,2.18335239884336,8.41722565788024));
#62327=CARTESIAN_POINT('Ctrl Pts',(0.308971055259537,2.19170666106868,8.41772843339678));
#62328=CARTESIAN_POINT('Ctrl Pts',(0.307965406128891,2.19502911209026,8.41793066015776));
#62329=CARTESIAN_POINT('Ctrl Pts',(0.306336575709194,2.2001127588084,8.41824403041404));
#62330=CARTESIAN_POINT('Ctrl Pts',(0.305751406570611,2.20188591304335,8.41835407804502));
#62331=CARTESIAN_POINT('Ctrl Pts',(0.305035311241287,2.20399405564536,8.41848585311103));
#62332=CARTESIAN_POINT('Ctrl Pts',(0.3049191839852,2.2043340593957,8.41850713512105));
#62333=CARTESIAN_POINT('Ctrl Pts',(0.302948696563384,2.21007197169169,8.41886678806722));
#62334=CARTESIAN_POINT('Ctrl Pts',(0.300951926554263,2.21541959711119,8.41920943974378));
#62335=CARTESIAN_POINT('Ctrl Pts',(0.298446908288367,2.22162064269975,8.41961660319025));
#62336=CARTESIAN_POINT('Ctrl Pts',(0.298075354254859,2.2225284495538,8.41967645979995));
#62337=CARTESIAN_POINT('Ctrl Pts',(0.297508201564514,2.22389630954061,8.41976703276733));
#62338=CARTESIAN_POINT('Ctrl Pts',(0.29731566507344,2.22435763271075,8.4197976452602));
#62339=CARTESIAN_POINT('Ctrl Pts',(0.29696987114851,2.22518077190033,8.41985238577364));
#62340=CARTESIAN_POINT('Ctrl Pts',(0.29681702353858,2.22554275988305,8.41987649982497));
#62341=CARTESIAN_POINT('Ctrl Pts',(0.29649286871903,2.22630655255101,8.41992746755679));
#62342=CARTESIAN_POINT('Ctrl Pts',(0.296321406006372,2.22670829001284,8.41995432649574));
#62343=CARTESIAN_POINT('Ctrl Pts',(0.295870789081046,2.22775816924708,8.42002465259536));
#62344=CARTESIAN_POINT('Ctrl Pts',(0.295590322883945,2.22840574226066,8.42006816446474));
#62345=CARTESIAN_POINT('Ctrl Pts',(0.294328378687823,2.23129342141016,8.42026279880509));
#62346=CARTESIAN_POINT('Ctrl Pts',(0.293323567647281,2.23352318577301,8.42041471837392));
#62347=CARTESIAN_POINT('Ctrl Pts',(0.290622543758115,2.23933933762203,8.42081537344335));
#62348=CARTESIAN_POINT('Ctrl Pts',(0.288885357859103,2.24290612901568,8.42106550621722));
#62349=CARTESIAN_POINT('Ctrl Pts',(0.280277445407858,2.25978121043864,8.42227065807382));
#62350=CARTESIAN_POINT('Ctrl Pts',(0.272551238605597,2.27263023996599,8.4232549979425));
#62351=CARTESIAN_POINT('Ctrl Pts',(0.255821728664446,2.29651380919368,8.42520855876348));
#62352=CARTESIAN_POINT('Ctrl Pts',(0.246924422897168,2.30758310271861,8.426173585409));
#62353=CARTESIAN_POINT('Ctrl Pts',(0.226962375438949,2.32931195581173,8.4281619160929));
#62354=CARTESIAN_POINT('Ctrl Pts',(0.215804750006076,2.33984230020496,8.42918118325994));
#62355=CARTESIAN_POINT('Ctrl Pts',(0.20323530841813,2.35011479461538,8.43020205794527));
#62356=CARTESIAN_POINT('Ctrl Pts',(0.202529379716162,2.35068675966678,8.43025899241625));
#62357=CARTESIAN_POINT('Ctrl Pts',(0.201576344870802,2.35145228437,8.43033530885438));
#62358=CARTESIAN_POINT('Ctrl Pts',(0.201331369852359,2.35164847236129,8.43035487738665));
#62359=CARTESIAN_POINT('Ctrl Pts',(0.200918333549415,2.35197826287601,8.43038778861869));
#62360=CARTESIAN_POINT('Ctrl Pts',(0.200750425323612,2.35211205534701,8.43040114499502));
#62361=CARTESIAN_POINT('Ctrl Pts',(0.200428047906117,2.35236840554695,8.43042674490399));
#62362=CARTESIAN_POINT('Ctrl Pts',(0.200273601065332,2.35249098839829,8.43043899020527));
#62363=CARTESIAN_POINT('Ctrl Pts',(0.199907648648315,2.35278089399213,8.43046795921089));
#62364=CARTESIAN_POINT('Ctrl Pts',(0.199696045731322,2.35294809284932,8.43048467393425));
#62365=CARTESIAN_POINT('Ctrl Pts',(0.199081713413944,2.35343225853603,8.43053309748792));
#62366=CARTESIAN_POINT('Ctrl Pts',(0.198678435137737,2.35374853241406,8.43056475679251));
#62367=CARTESIAN_POINT('Ctrl Pts',(0.195754801823926,2.35603017009604,8.43079336338358));
#62368=CARTESIAN_POINT('Ctrl Pts',(0.19320597567093,2.3579589953376,8.43098776625499));
#62369=CARTESIAN_POINT('Ctrl Pts',(0.185764100317055,2.36341844225202,8.4315427451628));
#62370=CARTESIAN_POINT('Ctrl Pts',(0.180799859106272,2.36685013975899,8.43189755566925));
#62371=CARTESIAN_POINT('Ctrl Pts',(0.158872968525616,2.38111483178102,8.43341278685427));
#62372=CARTESIAN_POINT('Ctrl Pts',(0.141012145262795,2.39048555531205,8.43451860139516));
#62373=CARTESIAN_POINT('Ctrl Pts',(0.102815970011274,2.40616645734095,8.43683842911468));
#62374=CARTESIAN_POINT('Ctrl Pts',(0.0824983582121419,2.4122544511575,8.43805086071517));
#62375=CARTESIAN_POINT('Ctrl Pts',(0.0604564839611807,2.41655628160546,
8.43941484745044));
#62376=CARTESIAN_POINT('Ctrl Pts',(0.0591789813705468,2.41679759147346,
8.43949405216134));
#62377=CARTESIAN_POINT('Ctrl Pts',(0.0573964288908414,2.41712314278283,
8.43960479094875));
#62378=CARTESIAN_POINT('Ctrl Pts',(0.0568925735448265,2.41721392278485,
8.4396361168865));
#62379=CARTESIAN_POINT('Ctrl Pts',(0.0560225421013413,2.4173685374466,8.43969025207543));
#62380=CARTESIAN_POINT('Ctrl Pts',(0.0556564668790967,2.41743294012617,
8.43971304322576));
#62381=CARTESIAN_POINT('Ctrl Pts',(0.0548989325062827,2.41756486051501,
8.43976023348141));
#62382=CARTESIAN_POINT('Ctrl Pts',(0.054507458442941,2.41763228802522,8.43978463541195));
#62383=CARTESIAN_POINT('Ctrl Pts',(0.0535929039131717,2.41778807041089,
8.43984167877783));
#62384=CARTESIAN_POINT('Ctrl Pts',(0.0530697291148096,2.41787585767345,
8.43987433817805));
#62385=CARTESIAN_POINT('Ctrl Pts',(0.0514231181477317,2.41814797600156,
8.43997721641948));
#62386=CARTESIAN_POINT('Ctrl Pts',(0.0502989299011547,2.41832764459189,
8.44004758296037));
#62387=CARTESIAN_POINT('Ctrl Pts',(0.0380842663052069,2.42021348188773,
8.44081357653443));
#62388=CARTESIAN_POINT('Ctrl Pts',(0.0269141238935459,2.42134508728867,
8.44152734950925));
#62389=CARTESIAN_POINT('Ctrl Pts',(-0.00094347221127675,2.42270457418021,
8.44334280122242));
#62390=CARTESIAN_POINT('Ctrl Pts',(-0.0176319661942657,2.42222373875657,
8.44446273442364));
#62391=CARTESIAN_POINT('Ctrl Pts',(-0.0559735906195382,2.41813100078004,
8.44707124596398));
#62392=CARTESIAN_POINT('Ctrl Pts',(-0.0774496561311467,2.41359550571066,
8.44855999820637));
#62393=CARTESIAN_POINT('Ctrl Pts',(-0.0994548686942221,2.40654750168359,
8.45001752161645));
#62394=CARTESIAN_POINT('Ctrl Pts',(-0.100605911993593,2.40617167125275,
8.4500935469848));
#62395=CARTESIAN_POINT('Ctrl Pts',(-0.102126997406757,2.40566551305355,
8.45019370336743));
#62396=CARTESIAN_POINT('Ctrl Pts',(-0.102498939531805,2.40554099048795,
8.45021816941118));
#62397=CARTESIAN_POINT('Ctrl Pts',(-0.10307635409797,2.40534650474978,8.45025611198134));
#62398=CARTESIAN_POINT('Ctrl Pts',(-0.10328198314249,2.40527701304859,8.45026961635238));
#62399=CARTESIAN_POINT('Ctrl Pts',(-0.103673838847605,2.40514414538069,
8.45029533588346));
#62400=CARTESIAN_POINT('Ctrl Pts',(-0.103860076437212,2.40508080707297,
8.45030755313817));
#62401=CARTESIAN_POINT('Ctrl Pts',(-0.104297232579509,2.4049316861513,8.45033621560172));
#62402=CARTESIAN_POINT('Ctrl Pts',(-0.104548102947228,2.40484576446814,
8.45035265241376));
#62403=CARTESIAN_POINT('Ctrl Pts',(-0.105066129068437,2.40466762877337,
8.45038656944156));
#62404=CARTESIAN_POINT('Ctrl Pts',(-0.105333270276923,2.40457537273067,
8.45040404715185));
#62405=CARTESIAN_POINT('Ctrl Pts',(-0.106751976128618,2.4040833391314,8.45049679868113));
#62406=CARTESIAN_POINT('Ctrl Pts',(-0.107901407388321,2.40367737475766,
8.45057171000643));
#62407=CARTESIAN_POINT('Ctrl Pts',(-0.110877350222705,2.40260727993817,
8.45076511465639));
#62408=CARTESIAN_POINT('Ctrl Pts',(-0.112700235596778,2.4019331216899,8.45088304779185));
#62409=CARTESIAN_POINT('Ctrl Pts',(-0.120394342735421,2.39900821643135,
8.45137899815008));
#62410=CARTESIAN_POINT('Ctrl Pts',(-0.126205489376465,2.39660225307005,
8.45174905479962));
#62411=CARTESIAN_POINT('Ctrl Pts',(-0.140468669379752,2.39020174849718,
8.45265472868859));
#62412=CARTESIAN_POINT('Ctrl Pts',(-0.148824478333991,2.38600663467383,
8.45318302032387));
#62413=CARTESIAN_POINT('Ctrl Pts',(-0.164822153083709,2.37708361813717,
8.45421110403603));
#62414=CARTESIAN_POINT('Ctrl Pts',(-0.172471870442244,2.37238782826001,
8.45471074376862));
#62415=CARTESIAN_POINT('Ctrl Pts',(-0.188411024728193,2.36166258570287,
8.45578723807841));
#62416=CARTESIAN_POINT('Ctrl Pts',(-0.196628731048234,2.35554480848539,
8.45636447709347));
#62417=CARTESIAN_POINT('Ctrl Pts',(-0.205412272779601,2.34833091844971,
8.4570178570847));
#62418=CARTESIAN_POINT('Ctrl Pts',(-0.206279805775255,2.34761076018854,
8.45708280005337));
#62419=CARTESIAN_POINT('Ctrl Pts',(-0.216161363688582,2.33931988799238,
8.45782736116971));
#62420=CARTESIAN_POINT('Ctrl Pts',(-0.224756929824862,2.33126611890626,
8.45852176521525));
#62421=CARTESIAN_POINT('Ctrl Pts',(-0.233644531959335,2.32197430752714,
8.45930333329821));
#62422=CARTESIAN_POINT('Ctrl Pts',(-0.234392939503212,2.32118388364044,
8.45936966939292));
#62423=CARTESIAN_POINT('Ctrl Pts',(-0.235498305847194,2.32000455043293,
8.45946843090707));
#62424=CARTESIAN_POINT('Ctrl Pts',(-0.235858342044654,2.31961852551825,
8.45950072430516));
#62425=CARTESIAN_POINT('Ctrl Pts',(-0.236473155571586,2.31895607696545,
8.45955608558057));
#62426=CARTESIAN_POINT('Ctrl Pts',(-0.23672840143305,2.31868008802608,8.45957913340888));
#62427=CARTESIAN_POINT('Ctrl Pts',(-0.237224135961085,2.31814218156596,
8.45962402174879));
#62428=CARTESIAN_POINT('Ctrl Pts',(-0.237464675306515,2.31788031127402,
8.45964586005976));
#62429=CARTESIAN_POINT('Ctrl Pts',(-0.238039159366992,2.31725280077638,
8.45969815544192));
#62430=CARTESIAN_POINT('Ctrl Pts',(-0.238372694939274,2.31688678876394,
8.45972862978243));
#62431=CARTESIAN_POINT('Ctrl Pts',(-0.239062910492958,2.316125851389,8.45979192793603));
#62432=CARTESIAN_POINT('Ctrl Pts',(-0.239419458298895,2.3157308086352,8.45982475720346));
#62433=CARTESIAN_POINT('Ctrl Pts',(-0.24034965668487,2.31469503433844,8.45991075044783));
#62434=CARTESIAN_POINT('Ctrl Pts',(-0.240921721004999,2.31405288963972,
8.45996398086783));
#62435=CARTESIAN_POINT('Ctrl Pts',(-0.245480400421749,2.30889432685496,
8.46039095428239));
#62436=CARTESIAN_POINT('Ctrl Pts',(-0.24934200503406,2.30426948722472,8.46076985029906));
#62437=CARTESIAN_POINT('Ctrl Pts',(-0.260117069755862,2.29060370305715,
8.46187939957853));
#62438=CARTESIAN_POINT('Ctrl Pts',(-0.266683675229906,2.2813020461917,8.46262281460333));
#62439=CARTESIAN_POINT('Ctrl Pts',(-0.27495287018226,2.26816446217166,8.46365480892187));
#62440=CARTESIAN_POINT('Ctrl Pts',(-0.277093580512788,2.26461322326421,
8.46393202486914));
#62441=CARTESIAN_POINT('Ctrl Pts',(-0.281392767825059,2.2571596761643,8.46450973788012));
#62442=CARTESIAN_POINT('Ctrl Pts',(-0.283539984604242,2.25325185008603,
8.4648103564494));
#62443=CARTESIAN_POINT('Ctrl Pts',(-0.294565571132059,2.2321604211386,8.46641851296347));
#62444=CARTESIAN_POINT('Ctrl Pts',(-0.301965070820477,2.21424727773257,
8.46773701697062));
#62445=CARTESIAN_POINT('Ctrl Pts',(-0.30921991471604,2.19093900410105,8.46932095262835));
#62446=CARTESIAN_POINT('Ctrl Pts',(-0.310611787633625,2.18606499090623,
8.4696450500948));
#62447=CARTESIAN_POINT('Ctrl Pts',(-0.312048071163627,2.18054551429612,
8.47000255969751));
#62448=CARTESIAN_POINT('Ctrl Pts',(-0.312206120470207,2.17993070090641,
8.47004225081337));
#62449=CARTESIAN_POINT('Ctrl Pts',(-0.312433418700957,2.1790355482132,8.47009984438616));
#62450=CARTESIAN_POINT('Ctrl Pts',(-0.312504107824726,2.17875558136897,
8.47011782947241));
#62451=CARTESIAN_POINT('Ctrl Pts',(-0.31262820011313,2.17826131161598,8.47014953186297));
#62452=CARTESIAN_POINT('Ctrl Pts',(-0.312681759335453,2.17804704851501,
8.47016325824607));
#62453=CARTESIAN_POINT('Ctrl Pts',(-0.312792884789983,2.17760054187807,
8.47019182851542));
#62454=CARTESIAN_POINT('Ctrl Pts',(-0.312850412525768,2.17736828974691,
8.47020667012873));
#62455=CARTESIAN_POINT('Ctrl Pts',(-0.312999579040515,2.17676318493524,
8.47024528835668));
#62456=CARTESIAN_POINT('Ctrl Pts',(-0.31309081060403,2.17639023078829,8.47026904134436));
#62457=CARTESIAN_POINT('Ctrl Pts',(-0.313287658567591,2.17557924081101,
8.47032058713231));
#62458=CARTESIAN_POINT('Ctrl Pts',(-0.31339302345367,2.1751411439136,8.47034836557216));
#62459=CARTESIAN_POINT('Ctrl Pts',(-0.314267400564064,2.17147173764769,
8.47058048559791));
#62460=CARTESIAN_POINT('Ctrl Pts',(-0.314987369257546,2.16822878878098,
8.47078208482908));
#62461=CARTESIAN_POINT('Ctrl Pts',(-0.320037310506056,2.14369556163156,
8.47228454619064));
#62462=CARTESIAN_POINT('Ctrl Pts',(-0.322254947008397,2.12202539477509,
8.47348612124905));
#62463=CARTESIAN_POINT('Ctrl Pts',(-0.322274864620942,2.10029539558797,
8.47470126795611));
#62464=CARTESIAN_POINT('',(-0.322274924948143,2.09973710004718,8.72483341161327));
#62465=CARTESIAN_POINT('Ctrl Pts',(-0.322274864675418,2.1002953361489,8.47470127127996));
#62466=CARTESIAN_POINT('Ctrl Pts',(-0.322298157958911,2.07487738506705,
8.47612264914654));
#62467=CARTESIAN_POINT('Ctrl Pts',(-0.319314602306005,2.04954914401777,
8.47755844204353));
#62468=CARTESIAN_POINT('Ctrl Pts',(-0.313190622656218,2.02401632946606,
8.47915428160579));
#62469=CARTESIAN_POINT('Ctrl Pts',(-0.312991074432553,2.0231984921232,8.47920554819074));
#62470=CARTESIAN_POINT('Ctrl Pts',(-0.312661995217988,2.02187236403647,
8.47928892536041));
#62471=CARTESIAN_POINT('Ctrl Pts',(-0.312534422737548,2.02136358760759,
8.47932097287557));
#62472=CARTESIAN_POINT('Ctrl Pts',(-0.31228535331439,2.02038044514755,8.4793830163082));
#62473=CARTESIAN_POINT('Ctrl Pts',(-0.312164016106489,2.01990603984275,
8.47941300700011));
#62474=CARTESIAN_POINT('Ctrl Pts',(-0.311952899388195,2.01908838111012,
8.47946478816371));
#62475=CARTESIAN_POINT('Ctrl Pts',(-0.311863633140215,2.01874499504009,
8.47948656199237));
#62476=CARTESIAN_POINT('Ctrl Pts',(-0.311678073725247,2.01803600226395,
8.47953157613093));
#62477=CARTESIAN_POINT('Ctrl Pts',(-0.311581703915576,2.01767041631876,
8.47955481889614));
#62478=CARTESIAN_POINT('Ctrl Pts',(-0.311347209606714,2.01678715385805,
8.47961105070911));
#62479=CARTESIAN_POINT('Ctrl Pts',(-0.311208437370691,2.01626965187767,
8.47964406072336));
#62480=CARTESIAN_POINT('Ctrl Pts',(-0.31069030235538,2.01435653375134,8.47976633138556));
#62481=CARTESIAN_POINT('Ctrl Pts',(-0.310302841181847,2.01296314611725,
8.47985585471153));
#62482=CARTESIAN_POINT('Ctrl Pts',(-0.303201636624754,1.98807604272175,
8.48146337717821));
#62483=CARTESIAN_POINT('Ctrl Pts',(-0.293848405738632,1.9654234671219,8.4830727320084));
#62484=CARTESIAN_POINT('Ctrl Pts',(-0.279702605687232,1.93984149803431,
8.48504532844743));
#62485=CARTESIAN_POINT('Ctrl Pts',(-0.277282085069137,1.93568646421829,
8.4853706935095));
#62486=CARTESIAN_POINT('Ctrl Pts',(-0.272413496451516,1.92774324614534,
8.48600116994133));
#62487=CARTESIAN_POINT('Ctrl Pts',(-0.269977041663995,1.9239491555125,8.48630621317142));
#62488=CARTESIAN_POINT('Ctrl Pts',(-0.261177484899353,1.91085882160613,
8.48737014607697));
#62489=CARTESIAN_POINT('Ctrl Pts',(-0.254406851938782,1.90184536906323,
8.48812372579876));
#62490=CARTESIAN_POINT('Ctrl Pts',(-0.243957012551486,1.88935493790551,
8.48918063605117));
#62491=CARTESIAN_POINT('Ctrl Pts',(-0.240646724324148,1.88558095431011,
8.4895017439435));
#62492=CARTESIAN_POINT('Ctrl Pts',(-0.236926435956432,1.88153428805485,
8.48984655820794));
#62493=CARTESIAN_POINT('Ctrl Pts',(-0.236602682444027,1.88118369800704,
8.48987643599668));
#62494=CARTESIAN_POINT('Ctrl Pts',(-0.236077369300966,1.88061736966058,
8.48992470420759));
#62495=CARTESIAN_POINT('Ctrl Pts',(-0.235876291324364,1.88040118856554,
8.48994313049929));
#62496=CARTESIAN_POINT('Ctrl Pts',(-0.235487866938806,1.87998473835891,
8.4899786285144));
#62497=CARTESIAN_POINT('Ctrl Pts',(-0.235300561534521,1.8797844315829,8.48999570332742));
#62498=CARTESIAN_POINT('Ctrl Pts',(-0.234964947855461,1.87942643910998,
8.49002622074851));
#62499=CARTESIAN_POINT('Ctrl Pts',(-0.234816736649928,1.8792686640405,8.4900396707516));
#62500=CARTESIAN_POINT('Ctrl Pts',(-0.234519462130586,1.87895284506744,
8.49006659423363));
#62501=CARTESIAN_POINT('Ctrl Pts',(-0.234370398611091,1.87879480323161,
8.49008006757644));
#62502=CARTESIAN_POINT('Ctrl Pts',(-0.233951096534526,1.87835114559316,
8.49011789147779));
#62503=CARTESIAN_POINT('Ctrl Pts',(-0.233680493737948,1.8780658722056,8.49014221390746));
#62504=CARTESIAN_POINT('Ctrl Pts',(-0.232569402664169,1.87689882900213,
8.49024172596749));
#62505=CARTESIAN_POINT('Ctrl Pts',(-0.231724426237672,1.8760213180857,8.49031657319546));
#62506=CARTESIAN_POINT('Ctrl Pts',(-0.215266184678152,1.8591222105287,8.49175893641388));
#62507=CARTESIAN_POINT('Ctrl Pts',(-0.198028736053994,1.84476167561535,
8.49300375565353));
#62508=CARTESIAN_POINT('Ctrl Pts',(-0.169385222980104,1.82556177567674,
8.49493115286423));
#62509=CARTESIAN_POINT('Ctrl Pts',(-0.158959197454201,1.81939413697203,
8.49560739826756));
#62510=CARTESIAN_POINT('Ctrl Pts',(-0.13957510084302,1.80935492859208,8.49685255649649));
#62511=CARTESIAN_POINT('Ctrl Pts',(-0.130741439654788,1.80527569032136,
8.49741570603977));
#62512=CARTESIAN_POINT('Ctrl Pts',(-0.118131539108899,1.8001312268028,8.49822269578325));
#62513=CARTESIAN_POINT('Ctrl Pts',(-0.114499464785686,1.79872568596785,
8.49845545503784));
#62514=CARTESIAN_POINT('Ctrl Pts',(-0.108578731967018,1.79655700870703,
8.49883586517626));
#62515=CARTESIAN_POINT('Ctrl Pts',(-0.106305351733928,1.79575312375438,
8.49898216099628));
#62516=CARTESIAN_POINT('Ctrl Pts',(-0.103530056554027,1.79480666045679,
8.49916110157431));
#62517=CARTESIAN_POINT('Ctrl Pts',(-0.103036496911362,1.79463967610239,
8.49919293762443));
#62518=CARTESIAN_POINT('Ctrl Pts',(-0.102080694484082,1.79431888386117,
8.49925461613643));
#62519=CARTESIAN_POINT('Ctrl Pts',(-0.101618503365226,1.79416492562182,
8.49928445354622));
#62520=CARTESIAN_POINT('Ctrl Pts',(-0.100819417167313,1.79390075728381,
8.4993360609682));
#62521=CARTESIAN_POINT('Ctrl Pts',(-0.100482685134412,1.79379005362996,
8.4993578146614));
#62522=CARTESIAN_POINT('Ctrl Pts',(-0.0997854205558294,1.79356209568316,
8.4994028733816));
#62523=CARTESIAN_POINT('Ctrl Pts',(-0.0994248625074841,1.79344492163551,
8.49942618101374));
#62524=CARTESIAN_POINT('Ctrl Pts',(-0.0985506143273258,1.79316251333776,
8.49948271405068));
#62525=CARTESIAN_POINT('Ctrl Pts',(-0.0980367156482074,1.79299793293082,
8.49951596090577));
#62526=CARTESIAN_POINT('Ctrl Pts',(-0.0961205360674598,1.79238956208202,
8.49963998907533));
#62527=CARTESIAN_POINT('Ctrl Pts',(-0.0947156521184655,1.79195408767742,
8.49973104289575));
#62528=CARTESIAN_POINT('Ctrl Pts',(-0.0714744453803711,1.7849239879905,
8.50123947653329));
#62529=CARTESIAN_POINT('Ctrl Pts',(-0.0490062202099829,1.78065772378202,
8.50273565493494));
#62530=CARTESIAN_POINT('Ctrl Pts',(-0.00961311279734053,1.77743462748962,
8.50539683366068));
#62531=CARTESIAN_POINT('Ctrl Pts',(0.00713495622397891,1.77737028299389,
8.50653783079707));
#62532=CARTESIAN_POINT('Ctrl Pts',(0.0333573205564837,1.77931312919962,
8.5082868217346));
#62533=CARTESIAN_POINT('Ctrl Pts',(0.0428669914389807,1.78044524774001,
8.50891283919201));
#62534=CARTESIAN_POINT('Ctrl Pts',(0.05367535124866,1.78222328854958,8.50960474027681));
#62535=CARTESIAN_POINT('Ctrl Pts',(0.0550362127610522,1.78245614929647,
8.50969149523809));
#62536=CARTESIAN_POINT('Ctrl Pts',(0.056684313212086,1.78274907364949,8.50979608877205));
#62537=CARTESIAN_POINT('Ctrl Pts',(0.0569729930320736,1.7828007886183,8.50981439166232));
#62538=CARTESIAN_POINT('Ctrl Pts',(0.0575300862652771,1.78290137302047,
8.50984967795719));
#62539=CARTESIAN_POINT('Ctrl Pts',(0.0577985088457912,1.78295018934792,
8.50986666435275));
#62540=CARTESIAN_POINT('Ctrl Pts',(0.0582611970181856,1.78303494265621,
8.50989591721373));
#62541=CARTESIAN_POINT('Ctrl Pts',(0.0584554913431511,1.78307071737125,
8.5099081929619));
#62542=CARTESIAN_POINT('Ctrl Pts',(0.0588594157771167,1.78314547460537,
8.50993369613674));
#62543=CARTESIAN_POINT('Ctrl Pts',(0.0590690394808009,1.78318448638976,
8.5099469218247));
#62544=CARTESIAN_POINT('Ctrl Pts',(0.0596454393599121,1.78329234860351,
8.50998326222909));
#62545=CARTESIAN_POINT('Ctrl Pts',(0.0600121363832061,1.78336162838408,
8.51000635235882));
#62546=CARTESIAN_POINT('Ctrl Pts',(0.0614301271179904,1.78363208002385,
8.51009553052319));
#62547=CARTESIAN_POINT('Ctrl Pts',(0.0624805516175137,1.78383785480682,
8.51016135890689));
#62548=CARTESIAN_POINT('Ctrl Pts',(0.0825881666887994,1.78788099820235,
8.51141733271637));
#62549=CARTESIAN_POINT('Ctrl Pts',(0.101263874154127,1.79343034922647,8.51251377699693));
#62550=CARTESIAN_POINT('Ctrl Pts',(0.134568304867893,1.80670539640465,8.51452126888673));
#62551=CARTESIAN_POINT('Ctrl Pts',(0.149322454176347,1.81393508954759,8.51543178774858));
#62552=CARTESIAN_POINT('Ctrl Pts',(0.169153404684813,1.82560626402644,8.51674939128876));
#62553=CARTESIAN_POINT('Ctrl Pts',(0.174740820852452,1.82913022542743,8.51713173276097));
#62554=CARTESIAN_POINT('Ctrl Pts',(0.186446155509846,1.83702569549574,8.51796125900637));
#62555=CARTESIAN_POINT('Ctrl Pts',(0.192527173766854,1.84144453720802,8.51840986863519));
#62556=CARTESIAN_POINT('Ctrl Pts',(0.199336608998842,1.84676618660709,8.51893544069666));
#62557=CARTESIAN_POINT('Ctrl Pts',(0.20022169960771,1.8474654105113,8.51900422011868));
#62558=CARTESIAN_POINT('Ctrl Pts',(0.201516702376564,1.84849955376657,8.51910554779072));
#62559=CARTESIAN_POINT('Ctrl Pts',(0.201929495922301,1.84883086482685,8.51913795138844));
#62560=CARTESIAN_POINT('Ctrl Pts',(0.202650505000997,1.84941247817276,8.51919473351801));
#62561=CARTESIAN_POINT('Ctrl Pts',(0.202959078489603,1.84966233657509,8.5192190941399));
#62562=CARTESIAN_POINT('Ctrl Pts',(0.203555881700145,1.85014740935363,8.51926632478465));
#62563=CARTESIAN_POINT('Ctrl Pts',(0.20384416757373,1.85038255395146,8.51928919196431));
#62564=CARTESIAN_POINT('Ctrl Pts',(0.204529179163417,1.85094327175224,8.51934365316465));
#62565=CARTESIAN_POINT('Ctrl Pts',(0.204925534695703,1.85126929373405,8.51937526536341));
#62566=CARTESIAN_POINT('Ctrl Pts',(0.206328890910064,1.85242925474074,8.51948755111807));
#62567=CARTESIAN_POINT('Ctrl Pts',(0.207331583152448,1.85326836506218,8.51956843520224));
#62568=CARTESIAN_POINT('Ctrl Pts',(0.223690240677228,1.86712835939027,8.52089895254329));
#62569=CARTESIAN_POINT('Ctrl Pts',(0.237794986637941,1.88155139091264,8.52220913604721));
#62570=CARTESIAN_POINT('Ctrl Pts',(0.264299569133966,1.91428374563332,8.52502915288392));
#62571=CARTESIAN_POINT('Ctrl Pts',(0.276352588634905,1.93274562434885,8.52653916103517));
#62572=CARTESIAN_POINT('Ctrl Pts',(0.28905054417156,1.95736899163948,8.52836514342316));
#62573=CARTESIAN_POINT('Ctrl Pts',(0.291533972804677,1.96251628114577,8.5287370145117));
#62574=CARTESIAN_POINT('Ctrl Pts',(0.294972671495013,1.97015626948368,8.52927196157799));
#62575=CARTESIAN_POINT('Ctrl Pts',(0.296035859308263,1.9725988916549,8.52944049942771));
#62576=CARTESIAN_POINT('Ctrl Pts',(0.29726927942361,1.97553145436602,8.52963963837981));
#62577=CARTESIAN_POINT('Ctrl Pts',(0.297468732389164,1.97600888499204,8.52967195814453));
#62578=CARTESIAN_POINT('Ctrl Pts',(0.297770795324136,1.97673685720115,8.52972108283385));
#62579=CARTESIAN_POINT('Ctrl Pts',(0.297874239639976,1.97698704832085,8.52973793818996));
#62580=CARTESIAN_POINT('Ctrl Pts',(0.298052526644022,1.97741979803185,8.52976704387263));
#62581=CARTESIAN_POINT('Ctrl Pts',(0.298127516838931,1.9776022947206,8.52977930320437));
#62582=CARTESIAN_POINT('Ctrl Pts',(0.298283566009757,1.97798305138086,8.52980484954653));
#62583=CARTESIAN_POINT('Ctrl Pts',(0.29836459468634,1.97818132269577,8.52981813468054));
#62584=CARTESIAN_POINT('Ctrl Pts',(0.298563186448095,1.97866864916119,8.52985074501205));
#62585=CARTESIAN_POINT('Ctrl Pts',(0.298680527785691,1.97895779528616,8.52987005670967));
#62586=CARTESIAN_POINT('Ctrl Pts',(0.299133228380408,1.98007798202666,8.52994473091039));
#62587=CARTESIAN_POINT('Ctrl Pts',(0.299465544823922,1.980910259786,8.52999991093429));
#62588=CARTESIAN_POINT('Ctrl Pts',(0.304984677020462,1.9949019711,8.53092268331537));
#62589=CARTESIAN_POINT('Ctrl Pts',(0.309303830367882,2.00838940012572,8.53174015932404));
#62590=CARTESIAN_POINT('Ctrl Pts',(0.317211088658042,2.04014006726122,8.53359337687551));
#62591=CARTESIAN_POINT('Ctrl Pts',(0.320133031877508,2.05851564408632,8.53461538679904));
#62592=CARTESIAN_POINT('Ctrl Pts',(0.322576716223429,2.09273022512197,8.53655956497202));
#62593=CARTESIAN_POINT('Ctrl Pts',(0.322547057551053,2.10847856355302,8.5374701523147));
#62594=CARTESIAN_POINT('Ctrl Pts',(0.321245661597191,2.1257888931757,8.53851710436484));
#62595=CARTESIAN_POINT('Ctrl Pts',(0.321110869980468,2.12741625678343,8.53861596496862));
#62596=CARTESIAN_POINT('Ctrl Pts',(0.320854578506306,2.13024866638306,8.53878882063849));
#62597=CARTESIAN_POINT('Ctrl Pts',(0.320738641458448,2.13145419175834,8.53886264075579));
#62598=CARTESIAN_POINT('Ctrl Pts',(0.32056081909363,2.1331998863911,8.538969909188));
#62599=CARTESIAN_POINT('Ctrl Pts',(0.320504356582679,2.1337406075844,8.53900318675328));
#62600=CARTESIAN_POINT('Ctrl Pts',(0.320404034035923,2.13467838192459,8.53906099067864));
#62601=CARTESIAN_POINT('Ctrl Pts',(0.320360803362932,2.135075502359,8.5390854971641));
#62602=CARTESIAN_POINT('Ctrl Pts',(0.320276287716734,2.13583867816492,8.53913264767996));
#62603=CARTESIAN_POINT('Ctrl Pts',(0.320235113216692,2.13620474537355,8.53915528819268));
#62604=CARTESIAN_POINT('Ctrl Pts',(0.32013667552013,2.13706661177312,8.53920865013098));
#62605=CARTESIAN_POINT('Ctrl Pts',(0.320078888166211,2.13756234906433,8.53923938804583));
#62606=CARTESIAN_POINT('Ctrl Pts',(0.319904916426641,2.13902523475362,8.53933022633979));
#62607=CARTESIAN_POINT('Ctrl Pts',(0.319785499182839,2.13999198645359,8.53939042860866));
#62608=CARTESIAN_POINT('Ctrl Pts',(0.318690869276193,2.14853512276183,8.53992397292191));
#62609=CARTESIAN_POINT('Ctrl Pts',(0.317451025307856,2.15607458234423,8.54040564037596));
#62610=CARTESIAN_POINT('Ctrl Pts',(0.314982444566395,2.16834496291487,8.5412083176936));
#62611=CARTESIAN_POINT('Ctrl Pts',(0.31391185045856,2.1731048604808,8.54152437327844));
#62612=CARTESIAN_POINT('Ctrl Pts',(0.307207189187937,2.20004236586333,8.54333934688574));
#62613=CARTESIAN_POINT('Ctrl Pts',(0.299332052898711,2.2215929180072,8.5449002552512));
#62614=CARTESIAN_POINT('Ctrl Pts',(0.28593047106801,2.2488669652428,8.54694651120588));
#62615=CARTESIAN_POINT('Ctrl Pts',(0.282382692096742,2.25549158846926,8.54744890952973));
#62616=CARTESIAN_POINT('Ctrl Pts',(0.274731595035463,2.26865099140515,8.5484502763893));
#62617=CARTESIAN_POINT('Ctrl Pts',(0.270618447379577,2.27517501308584,8.54894850228024));
#62618=CARTESIAN_POINT('Ctrl Pts',(0.265902495166367,2.28209194276354,8.54947354487824));
#62619=CARTESIAN_POINT('Ctrl Pts',(0.265528449677218,2.28263694857682,8.54951489216924));
#62620=CARTESIAN_POINT('Ctrl Pts',(0.264978520714319,2.28343296627837,8.54957524520067));
#62621=CARTESIAN_POINT('Ctrl Pts',(0.264803954837154,2.28368487978628,8.54959433944103));
#62622=CARTESIAN_POINT('Ctrl Pts',(0.264501770184818,2.2841196320595,8.5496272821941));
#62623=CARTESIAN_POINT('Ctrl Pts',(0.264374320748109,2.28430258780272,8.54964114231642));
#62624=CARTESIAN_POINT('Ctrl Pts',(0.264128565109189,2.28465459456044,8.54966780301087));
#62625=CARTESIAN_POINT('Ctrl Pts',(0.264010286678735,2.28482366387271,8.54968060545407));
#62626=CARTESIAN_POINT('Ctrl Pts',(0.263729325535709,2.28522445475037,8.54971094839437));
#62627=CARTESIAN_POINT('Ctrl Pts',(0.263566499350684,2.28545607621898,8.54972847901731));
#62628=CARTESIAN_POINT('Ctrl Pts',(0.262993510643645,2.28626887820114,8.54978998110197));
#62629=CARTESIAN_POINT('Ctrl Pts',(0.262581725491865,2.28684892048763,8.54983384211226));
#62630=CARTESIAN_POINT('Ctrl Pts',(0.25708056593167,2.29454377489242,8.55041538694619));
#62631=CARTESIAN_POINT('Ctrl Pts',(0.251704939767702,2.30145062169001,8.55093379330792));
#62632=CARTESIAN_POINT('Ctrl Pts',(0.230145342531506,2.32693859594889,8.55286913108312));
#62633=CARTESIAN_POINT('Ctrl Pts',(0.212131559118262,2.34386141348969,8.55420770103896));
#62634=CARTESIAN_POINT('Ctrl Pts',(0.180029914514718,2.36774381106247,8.55647793074426));
#62635=CARTESIAN_POINT('Ctrl Pts',(0.167056283744873,2.37602468103237,8.55736900477858));
#62636=CARTESIAN_POINT('Ctrl Pts',(0.152125351440082,2.38411555887143,8.55839341339151));
#62637=CARTESIAN_POINT('Ctrl Pts',(0.150702568394904,2.38487279455553,8.55849100464118));
#62638=CARTESIAN_POINT('Ctrl Pts',(0.148210306780509,2.3861753336353,8.55866193856896));
#62639=CARTESIAN_POINT('Ctrl Pts',(0.147143342073657,2.38672539727,8.55873511254563));
#62640=CARTESIAN_POINT('Ctrl Pts',(0.145591531290294,2.38751447581604,8.55884154025076));
#62641=CARTESIAN_POINT('Ctrl Pts',(0.14510910903397,2.38775825662693,8.55887462648465));
#62642=CARTESIAN_POINT('Ctrl Pts',(0.144269583262879,2.38817984334013,8.55893220560762));
#62643=CARTESIAN_POINT('Ctrl Pts',(0.143912757636174,2.38835820250103,8.55895667905511));
#62644=CARTESIAN_POINT('Ctrl Pts',(0.14322512742581,2.38870031996441,8.5590038425264));
#62645=CARTESIAN_POINT('Ctrl Pts',(0.142894370653338,2.38886417345791,8.559026529176));
#62646=CARTESIAN_POINT('Ctrl Pts',(0.14211311447227,2.3892495295305,8.5590801173357));
#62647=CARTESIAN_POINT('Ctrl Pts',(0.141662378548815,2.38947054796294,8.55911103568034));
#62648=CARTESIAN_POINT('Ctrl Pts',(0.140094794417585,2.39023467491219,8.55921857042302));
#62649=CARTESIAN_POINT('Ctrl Pts',(0.138975335402668,2.39077237493402,8.55929537467757));
#62650=CARTESIAN_POINT('Ctrl Pts',(0.124578655756466,2.39758527676272,8.56028330680299));
#62651=CARTESIAN_POINT('Ctrl Pts',(0.110892653860461,2.40295139470231,8.56122587143526));
#62652=CARTESIAN_POINT('Ctrl Pts',(0.0873168228179365,2.41038315704674,
8.56285578520356));
#62653=CARTESIAN_POINT('Ctrl Pts',(0.0776082624895371,2.41295186130109,
8.56352835861894));
#62654=CARTESIAN_POINT('Ctrl Pts',(0.0502986055330913,2.41882843156283,
8.56541342118114));
#62655=CARTESIAN_POINT('Ctrl Pts',(0.0325172825177378,2.42112955149173,
8.56663444467349));
#62656=CARTESIAN_POINT('Ctrl Pts',(0.00985150512526624,2.42216000060252,
8.56812708619422));
#62657=CARTESIAN_POINT('Ctrl Pts',(0.00506208514787253,2.42227084650992,
8.568438765919));
#62658=CARTESIAN_POINT('Ctrl Pts',(-0.00291035897192122,2.42227756838619,
8.56894953175527));
#62659=CARTESIAN_POINT('Ctrl Pts',(-0.00609245613933498,2.42223312234828,
8.56915126012565));
#62660=CARTESIAN_POINT('Ctrl Pts',(-0.00978682072199205,2.42212677234905,
8.56938257943543));
#62661=CARTESIAN_POINT('Ctrl Pts',(-0.0103000924292323,2.42211076888002,
8.56941465277231));
#62662=CARTESIAN_POINT('Ctrl Pts',(-0.0110808771168979,2.42208455636771,
8.56946334176545));
#62663=CARTESIAN_POINT('Ctrl Pts',(-0.0113484162099816,2.42207524080413,
8.56948000725967));
#62664=CARTESIAN_POINT('Ctrl Pts',(-0.011833819865078,2.4220577337432,8.56951021090698));
#62665=CARTESIAN_POINT('Ctrl Pts',(-0.0120516869455893,2.42204965455501,
8.56952375531863));
#62666=CARTESIAN_POINT('Ctrl Pts',(-0.0124908255963676,2.42203292368306,
8.56955103138261));
#62667=CARTESIAN_POINT('Ctrl Pts',(-0.0127120954584672,2.42202426506354,
8.5695647625837));
#62668=CARTESIAN_POINT('Ctrl Pts',(-0.0133469961452603,2.42199876504766,
8.56960412691129));
#62669=CARTESIAN_POINT('Ctrl Pts',(-0.0137606056074492,2.42198135464058,
8.56962972802481));
#62670=CARTESIAN_POINT('Ctrl Pts',(-0.0155607395557798,2.4219021051102,
8.56974096791646));
#62671=CARTESIAN_POINT('Ctrl Pts',(-0.0169469165689319,2.42183210540889,
8.5698261553968));
#62672=CARTESIAN_POINT('Ctrl Pts',(-0.0524099184088968,2.41981151914836,
8.57199443971786));
#62673=CARTESIAN_POINT('Ctrl Pts',(-0.0859689423470034,2.41246843317864,
8.57380206380365));
#62674=CARTESIAN_POINT('Ctrl Pts',(-0.132068625013949,2.39437308028247,
8.57662533821058));
#62675=CARTESIAN_POINT('Ctrl Pts',(-0.145960146760766,2.38773802158973,
8.57752310117291));
#62676=CARTESIAN_POINT('Ctrl Pts',(-0.160380612686434,2.37953660299457,
8.57853144882258));
#62677=CARTESIAN_POINT('Ctrl Pts',(-0.161433863959101,2.37892967006633,
8.57860554856585));
#62678=CARTESIAN_POINT('Ctrl Pts',(-0.162948572271037,2.37804537084887,
8.57871277616127));
#62679=CARTESIAN_POINT('Ctrl Pts',(-0.163412816373294,2.377772779255,8.57874573081852));
#62680=CARTESIAN_POINT('Ctrl Pts',(-0.164219549077923,2.3772963652254,8.57880315568855));
#62681=CARTESIAN_POINT('Ctrl Pts',(-0.1645623476377,2.37709306776647,8.57882760675657));
#62682=CARTESIAN_POINT('Ctrl Pts',(-0.16522235657758,2.37669999123729,8.57887478055871));
#62683=CARTESIAN_POINT('Ctrl Pts',(-0.165539619479028,2.37651030115483,
8.57889750001862));
#62684=CARTESIAN_POINT('Ctrl Pts',(-0.16628874485693,2.3760606510241,8.5789512482236));
#62685=CARTESIAN_POINT('Ctrl Pts',(-0.166720324219239,2.37580022334575,
8.57898229404809));
#62686=CARTESIAN_POINT('Ctrl Pts',(-0.16822326760528,2.37488848627861,8.57909069266373));
#62687=CARTESIAN_POINT('Ctrl Pts',(-0.169291429875897,2.37423194444059,
8.57916823733298));
#62688=CARTESIAN_POINT('Ctrl Pts',(-0.183502144444412,2.36538271508641,
8.58020671063603));
#62689=CARTESIAN_POINT('Ctrl Pts',(-0.196039317029163,2.35626057063135,
8.58120271100038));
#62690=CARTESIAN_POINT('Ctrl Pts',(-0.214319834075695,2.34083065204934,
8.5827841754068));
#62691=CARTESIAN_POINT('Ctrl Pts',(-0.220552173325257,2.33513638651739,
8.583349340232));
#62692=CARTESIAN_POINT('Ctrl Pts',(-0.237526636305793,2.31835823567996,
8.58495827450552));
#62693=CARTESIAN_POINT('Ctrl Pts',(-0.24770669807064,2.30673806021719,8.58600952560816));
#62694=CARTESIAN_POINT('Ctrl Pts',(-0.261760270500657,2.28816107837605,
8.58756139889997));
#62695=CARTESIAN_POINT('Ctrl Pts',(-0.266274420518883,2.28171676650787,
8.58807855988608));
#62696=CARTESIAN_POINT('Ctrl Pts',(-0.272364802746784,2.27230717533677,
8.5887974610413));
#62697=CARTESIAN_POINT('Ctrl Pts',(-0.274137369081325,2.26947286949933,
8.58900951590757));
#62698=CARTESIAN_POINT('Ctrl Pts',(-0.276134441350277,2.26616623105738,
8.58925131015467));
#62699=CARTESIAN_POINT('Ctrl Pts',(-0.27640220731496,2.26572044485839,8.58928379160596));
#62700=CARTESIAN_POINT('Ctrl Pts',(-0.276806881088675,2.26504302046026,
8.58933297262597));
#62701=CARTESIAN_POINT('Ctrl Pts',(-0.276944578130796,2.26481185838983,
8.5893497235749));
#62702=CARTESIAN_POINT('Ctrl Pts',(-0.277182647517975,2.26441105313428,
8.58937871279436));
#62703=CARTESIAN_POINT('Ctrl Pts',(-0.277283153530108,2.26424149063785,
8.58939095984863));
#62704=CARTESIAN_POINT('Ctrl Pts',(-0.277492962631956,2.26388678268848,
8.58941654395893));
#62705=CARTESIAN_POINT('Ctrl Pts',(-0.277602235675585,2.26370162063583,
8.58942987902521));
#62706=CARTESIAN_POINT('Ctrl Pts',(-0.277905164528154,2.26318713524465,
8.58946687585156));
#62707=CARTESIAN_POINT('Ctrl Pts',(-0.278098420969849,2.26285757531793,
8.58949051148097));
#62708=CARTESIAN_POINT('Ctrl Pts',(-0.278862705856799,2.26154891399755,
8.58958412001901));
#62709=CARTESIAN_POINT('Ctrl Pts',(-0.27942916214763,2.26056713163912,8.58965379935056));
#62710=CARTESIAN_POINT('Ctrl Pts',(-0.289476872674266,2.24293822336309,
8.5908955656493));
#62711=CARTESIAN_POINT('Ctrl Pts',(-0.297461900549118,2.22547848241258,
8.59197703886323));
#62712=CARTESIAN_POINT('Ctrl Pts',(-0.309366087925198,2.19180315291237,
8.59397741497382));
#62713=CARTESIAN_POINT('Ctrl Pts',(-0.313672408857621,2.1757943992234,8.59489570014111));
#62714=CARTESIAN_POINT('Ctrl Pts',(-0.318525031848314,2.14997442214091,
8.59639978979804));
#62715=CARTESIAN_POINT('Ctrl Pts',(-0.319887082928467,2.14034684959598,
8.59696521339813));
#62716=CARTESIAN_POINT('Ctrl Pts',(-0.321275281259053,2.12582755222279,
8.59783389740767));
#62717=CARTESIAN_POINT('Ctrl Pts',(-0.321628702471114,2.12097242586813,
8.59812699352486));
#62718=CARTESIAN_POINT('Ctrl Pts',(-0.32191611057508,2.11523059574938,8.5984773035488));
#62719=CARTESIAN_POINT('Ctrl Pts',(-0.321956581193793,2.1143496723443,8.59853115066144));
#62720=CARTESIAN_POINT('Ctrl Pts',(-0.322013178468303,2.11299660299506,
8.59861401810306));
#62721=CARTESIAN_POINT('Ctrl Pts',(-0.322031883638001,2.1125245644011,8.59864295755724));
#62722=CARTESIAN_POINT('Ctrl Pts',(-0.322062743976273,2.1116999580824,8.59869356485156));
#62723=CARTESIAN_POINT('Ctrl Pts',(-0.322075358291699,2.11134740747459,
8.59871521826279));
#62724=CARTESIAN_POINT('Ctrl Pts',(-0.322102485784134,2.110552723335,8.59876406553171));
#62725=CARTESIAN_POINT('Ctrl Pts',(-0.322116667512639,2.11011057988189,
8.59879126973305));
#62726=CARTESIAN_POINT('Ctrl Pts',(-0.322152289030624,2.10892375009722,
8.59886436546013));
#62727=CARTESIAN_POINT('Ctrl Pts',(-0.322172056930501,2.10817901960742,
8.59891030928292));
#62728=CARTESIAN_POINT('Ctrl Pts',(-0.322247036446666,2.10492951209401,
8.59911111672114));
#62729=CARTESIAN_POINT('Ctrl Pts',(-0.322275619572637,2.10242426216178,
8.59926681202063));
#62730=CARTESIAN_POINT('Ctrl Pts',(-0.322272832832555,2.09133812609189,
8.5999598458512));
#62731=CARTESIAN_POINT('Ctrl Pts',(-0.321927971084576,2.08276149861095,
8.60050688914823));
#62732=CARTESIAN_POINT('Ctrl Pts',(-0.320084275941854,2.0597968364723,8.60200185316021));
#62733=CARTESIAN_POINT('Ctrl Pts',(-0.317958670844613,2.04547987579012,
8.60296663528113));
#62734=CARTESIAN_POINT('Ctrl Pts',(-0.309606539234907,2.00716788135307,
8.6056126165525));
#62735=CARTESIAN_POINT('Ctrl Pts',(-0.301563889964951,1.98366667577301,
8.60731034970665));
#62736=CARTESIAN_POINT('Ctrl Pts',(-0.290333431154184,1.96010909948202,
8.60895852370223));
#62737=CARTESIAN_POINT('Ctrl Pts',(-0.289750221951268,1.9589050875445,8.60904258535201));
#62738=CARTESIAN_POINT('Ctrl Pts',(-0.288979344626559,1.9573385808161,8.6091516921087));
#62739=CARTESIAN_POINT('Ctrl Pts',(-0.288798472480428,1.9569727842622,8.60917715088927));
#62740=CARTESIAN_POINT('Ctrl Pts',(-0.288518907869344,1.95641008414183,
8.60921628361089));
#62741=CARTESIAN_POINT('Ctrl Pts',(-0.288420708355805,1.95621293825068,
8.60922998831388));
#62742=CARTESIAN_POINT('Ctrl Pts',(-0.288224852827786,1.95582074553898,
8.60925724018274));
#62743=CARTESIAN_POINT('Ctrl Pts',(-0.288127201545608,1.95562569849688,
8.60927078743857));
#62744=CARTESIAN_POINT('Ctrl Pts',(-0.287908367010099,1.95518970834806,
8.60930105693745));
#62745=CARTESIAN_POINT('Ctrl Pts',(-0.287787079593905,1.95494881874721,
8.60931777248146));
#62746=CARTESIAN_POINT('Ctrl Pts',(-0.287429679258594,1.95424119685872,
8.60936685022283));
#62747=CARTESIAN_POINT('Ctrl Pts',(-0.287192730872771,1.95377488398083,
8.60939916004662));
#62748=CARTESIAN_POINT('Ctrl Pts',(-0.285397468414168,1.95026301606031,
8.60964226594377));
#62749=CARTESIAN_POINT('Ctrl Pts',(-0.283791809350712,1.94724172505508,
8.60985014027847));
#62750=CARTESIAN_POINT('Ctrl Pts',(-0.278135424112408,1.93699552183511,
8.61055269420806));
#62751=CARTESIAN_POINT('Ctrl Pts',(-0.27385421177145,1.92990100805802,8.611034998999));
#62752=CARTESIAN_POINT('Ctrl Pts',(-0.25471416661972,1.90078307138899,8.61303023353306));
#62753=CARTESIAN_POINT('Ctrl Pts',(-0.237436334732314,1.88047597171762,
8.61446972800151));
#62754=CARTESIAN_POINT('Ctrl Pts',(-0.214697841373923,1.85961604274329,
8.61624665156091));
#62755=CARTESIAN_POINT('Ctrl Pts',(-0.211476390761636,1.85677717202346,
8.61649580996712));
#62756=CARTESIAN_POINT('Ctrl Pts',(-0.206808855092645,1.85282679924358,
8.61685398235208));
#62757=CARTESIAN_POINT('Ctrl Pts',(-0.205408501234214,1.85166184111768,
8.61696108820524));
#62758=CARTESIAN_POINT('Ctrl Pts',(-0.198919788094088,1.84635629507863,
8.61745593192391));
#62759=CARTESIAN_POINT('Ctrl Pts',(-0.193715907030422,1.84236003959812,
8.61784879210187));
#62760=CARTESIAN_POINT('Ctrl Pts',(-0.187553576607034,1.83792004188325,
8.61831104705655));
#62761=CARTESIAN_POINT('Ctrl Pts',(-0.186710269714065,1.83731858899306,
8.61837424250285));
#62762=CARTESIAN_POINT('Ctrl Pts',(-0.185452170570876,1.83643042229541,
8.6184684332785));
#62763=CARTESIAN_POINT('Ctrl Pts',(-0.185039575543705,1.83614059550802,
8.61849930922907));
#62764=CARTESIAN_POINT('Ctrl Pts',(-0.184303817899745,1.8356263380448,8.61855434442802));
#62765=CARTESIAN_POINT('Ctrl Pts',(-0.183980920540885,1.83540152815487,
8.61857848913262));
#62766=CARTESIAN_POINT('Ctrl Pts',(-0.183300636776477,1.83492974345595,
8.61862934054027));
#62767=CARTESIAN_POINT('Ctrl Pts',(-0.182943161302258,1.8346828990118,8.61865605214097));
#62768=CARTESIAN_POINT('Ctrl Pts',(-0.182000570671358,1.83403483077372,
8.61872646014563));
#62769=CARTESIAN_POINT('Ctrl Pts',(-0.181414630216673,1.83363481665813,
8.61877020233591));
#62770=CARTESIAN_POINT('Ctrl Pts',(-0.178784421993921,1.83185191124407,
8.61896644638034));
#62771=CARTESIAN_POINT('Ctrl Pts',(-0.176725673175903,1.83049062549386,
8.61911976052625));
#62772=CARTESIAN_POINT('Ctrl Pts',(-0.161515276034905,1.82068242857172,
8.62025060656303));
#62773=CARTESIAN_POINT('Ctrl Pts',(-0.14778219989945,1.81317987803289,8.62126304009206));
#62774=CARTESIAN_POINT('Ctrl Pts',(-0.117525313290562,1.79940153180281,
8.62347199148681));
#62775=CARTESIAN_POINT('Ctrl Pts',(-0.100918428102868,1.79342693035838,
8.6246722434427));
#62776=CARTESIAN_POINT('Ctrl Pts',(-0.069244537682779,1.78488570633752,
8.62688240334311));
#62777=CARTESIAN_POINT('Ctrl Pts',(-0.0543179440716717,1.78197247164592,
8.62789235741758));
#62778=CARTESIAN_POINT('Ctrl Pts',(-0.0383355576014893,1.78001188994944,
8.62890502288658));
#62779=CARTESIAN_POINT('Ctrl Pts',(-0.0374308540527212,1.77990480046906,
8.62896211252217));
#62780=CARTESIAN_POINT('Ctrl Pts',(-0.0362135146670193,1.77976593606299,
8.62903860537103));
#62781=CARTESIAN_POINT('Ctrl Pts',(-0.0359012800986873,1.7797307813113,
8.6290581962319));
#62782=CARTESIAN_POINT('Ctrl Pts',(-0.0353755134088078,1.77967236333363,
8.62909113601298));
#62783=CARTESIAN_POINT('Ctrl Pts',(-0.0351620094043913,1.77964885694529,
8.62910449865661));
#62784=CARTESIAN_POINT('Ctrl Pts',(-0.0347524850985844,1.77960418342912,
8.62913010342618));
#62785=CARTESIAN_POINT('Ctrl Pts',(-0.0345564703069038,1.77958298288507,
8.62914234733483));
#62786=CARTESIAN_POINT('Ctrl Pts',(-0.0340924879393328,1.77953323025312,
8.62917130239016));
#62787=CARTESIAN_POINT('Ctrl Pts',(-0.033824504243271,1.77950483442045,
8.6291880045822));
#62788=CARTESIAN_POINT('Ctrl Pts',(-0.0330373039361792,1.77942242019123,
8.6292370049441));
#62789=CARTESIAN_POINT('Ctrl Pts',(-0.032517988192475,1.77936932682542,
8.62926925099118));
#62790=CARTESIAN_POINT('Ctrl Pts',(-0.0286213198927139,1.77898050704224,
8.62951062744522));
#62791=CARTESIAN_POINT('Ctrl Pts',(-0.0252388215946294,1.77869687376856,
8.62971688288239));
#62792=CARTESIAN_POINT('Ctrl Pts',(-0.0137246983724219,1.77791434134935,
8.63040978726543));
#62793=CARTESIAN_POINT('Ctrl Pts',(-0.00557838692804692,1.77767029018376,
8.63088448994781));
#62794=CARTESIAN_POINT('Ctrl Pts',(0.0304526758666886,1.77795752248239,
8.63294912131454));
#62795=CARTESIAN_POINT('Ctrl Pts',(0.058189563717908,1.78179749128044,8.63445652636926));
#62796=CARTESIAN_POINT('Ctrl Pts',(0.0888553993195147,1.79019174012449,
8.63629530784051));
#62797=CARTESIAN_POINT('Ctrl Pts',(0.0926045416386487,1.79129166338582,
8.63652293621822));
#62798=CARTESIAN_POINT('Ctrl Pts',(0.103536562859958,1.79471596206472,8.6371961567505));
#62799=CARTESIAN_POINT('Ctrl Pts',(0.110658458306603,1.79722474455812,8.63764694817855));
#62800=CARTESIAN_POINT('Ctrl Pts',(0.118589066858118,1.80033560220971,8.63816525394164));
#62801=CARTESIAN_POINT('Ctrl Pts',(0.11949121150046,1.80069418912565,8.63822445485515));
#62802=CARTESIAN_POINT('Ctrl Pts',(0.120853888431524,1.80124297242638,8.63831424756699));
#62803=CARTESIAN_POINT('Ctrl Pts',(0.121315628032383,1.80143017187875,8.63834473821528));
#62804=CARTESIAN_POINT('Ctrl Pts',(0.12211779530301,1.80175755627689,8.63839782195723));
#62805=CARTESIAN_POINT('Ctrl Pts',(0.122458421218158,1.80189725556692,8.63842039858915));
#62806=CARTESIAN_POINT('Ctrl Pts',(0.123168289842822,1.80218981261848,8.6384675231486));
#62807=CARTESIAN_POINT('Ctrl Pts',(0.123537488934966,1.80234277405643,8.63849207456093));
#62808=CARTESIAN_POINT('Ctrl Pts',(0.124409139833329,1.80270580540699,8.63855013874764));
#62809=CARTESIAN_POINT('Ctrl Pts',(0.124911344365616,1.80291646249625,8.63858367141864));
#62810=CARTESIAN_POINT('Ctrl Pts',(0.126564815856991,1.80361496929238,8.6386943368392));
#62811=CARTESIAN_POINT('Ctrl Pts',(0.127713766876184,1.8041082415475,8.63877165398284));
#62812=CARTESIAN_POINT('Ctrl Pts',(0.15405447441484,1.81559894048176,8.64055398776295));
#62813=CARTESIAN_POINT('Ctrl Pts',(0.17773372852645,1.82976529809131,8.64237719618967));
#62814=CARTESIAN_POINT('Ctrl Pts',(0.214126927098644,1.85841000209708,8.64550986373934));
#62815=CARTESIAN_POINT('Ctrl Pts',(0.227881152534135,1.87133789495012,8.64679049860684));
#62816=CARTESIAN_POINT('Ctrl Pts',(0.240840237491832,1.88585626532937,8.6480463317393));
#62817=CARTESIAN_POINT('Ctrl Pts',(0.241251271381388,1.8863194366283,8.6480862179897));
#62818=CARTESIAN_POINT('Ctrl Pts',(0.244046633668339,1.88948772282619,8.64835782922808));
#62819=CARTESIAN_POINT('Ctrl Pts',(0.246386873265539,1.89223164430725,8.64858697783846));
#62820=CARTESIAN_POINT('Ctrl Pts',(0.249047026945283,1.89545884099768,8.64884895068513));
#62821=CARTESIAN_POINT('Ctrl Pts',(0.249412182966242,1.8959042617875,8.64888494497765));
#62822=CARTESIAN_POINT('Ctrl Pts',(0.249953391924104,1.89656805519794,8.64893834025456));
#62823=CARTESIAN_POINT('Ctrl Pts',(0.250130354511707,1.8967856795066,8.64895580677819));
#62824=CARTESIAN_POINT('Ctrl Pts',(0.25044502724324,1.89717369019531,8.64898687853296));
#62825=CARTESIAN_POINT('Ctrl Pts',(0.250582847683207,1.89734398585804,8.64900049178701));
#62826=CARTESIAN_POINT('Ctrl Pts',(0.250871941356647,1.8977019457203,8.64902905632544));
#62827=CARTESIAN_POINT('Ctrl Pts',(0.251023177262946,1.89788963855572,8.64904400489544));
#62828=CARTESIAN_POINT('Ctrl Pts',(0.251425015297271,1.89838949047335,8.64908373851545));
#62829=CARTESIAN_POINT('Ctrl Pts',(0.251675247648462,1.89870194836009,8.64910849682829));
#62830=CARTESIAN_POINT('Ctrl Pts',(0.252224391398879,1.89939027284592,8.64916286584248));
#62831=CARTESIAN_POINT('Ctrl Pts',(0.252523046814001,1.89976634378787,8.6491924584077));
#62832=CARTESIAN_POINT('Ctrl Pts',(0.253408836917653,1.9008868765289,8.64928030299234));
#62833=CARTESIAN_POINT('Ctrl Pts',(0.253993534290668,1.90163327104521,8.64933838677612));
#62834=CARTESIAN_POINT('Ctrl Pts',(0.2605633465122,1.91009662769758,8.64999229315507));
#62835=CARTESIAN_POINT('Ctrl Pts',(0.266198664745275,1.91808007293643,8.65056514777496));
#62836=CARTESIAN_POINT('Ctrl Pts',(0.282950778912228,1.9442619425724,8.65235047111826));
#62837=CARTESIAN_POINT('Ctrl Pts',(0.292629374975802,1.9633119269917,8.65351706044498));
#62838=CARTESIAN_POINT('Ctrl Pts',(0.306963177572893,2.00016529081372,8.65575257943072));
#62839=CARTESIAN_POINT('Ctrl Pts',(0.312116087044209,2.01767890847305,8.65680681817659));
#62840=CARTESIAN_POINT('Ctrl Pts',(0.316018236103701,2.03679160313739,8.65799171126637));
#62841=CARTESIAN_POINT('Ctrl Pts',(0.316267760267555,2.03805219354455,8.65807000482565));
#62842=CARTESIAN_POINT('Ctrl Pts',(0.316605661235126,2.03981453327043,8.65817967187188));
#62843=CARTESIAN_POINT('Ctrl Pts',(0.31670040000447,2.04031506250406,8.6582108425084));
#62844=CARTESIAN_POINT('Ctrl Pts',(0.316862089280427,2.04118053327133,8.65826478164746));
#62845=CARTESIAN_POINT('Ctrl Pts',(0.316929597235285,2.04154537072383,8.65828753235682));
#62846=CARTESIAN_POINT('Ctrl Pts',(0.317068149534322,2.04230145325715,8.65833470731456));
#62847=CARTESIAN_POINT('Ctrl Pts',(0.31713910007669,2.0426927147241,8.65835913450717));
#62848=CARTESIAN_POINT('Ctrl Pts',(0.31730345047005,2.04360868868258,8.65841635570135));
#62849=CARTESIAN_POINT('Ctrl Pts',(0.317396272992565,2.04413350237142,8.6584491680037));
#62850=CARTESIAN_POINT('Ctrl Pts',(0.317691461446308,2.04582696569904,8.6585551349574));
#62851=CARTESIAN_POINT('Ctrl Pts',(0.317888676225886,2.0469964926789,8.65862845302382));
#62852=CARTESIAN_POINT('Ctrl Pts',(0.320697573345813,2.06423365017761,8.65971112310684));
#62853=CARTESIAN_POINT('Ctrl Pts',(0.322094251481028,2.0804728499953,8.66075938610701));
#62854=CARTESIAN_POINT('Ctrl Pts',(0.322511813901921,2.12182534544475,8.66349881246203));
#62855=CARTESIAN_POINT('Ctrl Pts',(0.319836704247099,2.14684613788721,8.66522659305696));
#62856=CARTESIAN_POINT('Ctrl Pts',(0.312287975047061,2.18011950945565,8.6674845439894));
#62857=CARTESIAN_POINT('Ctrl Pts',(0.30991731349674,2.18884936263284,8.66807203137488));
#62858=CARTESIAN_POINT('Ctrl Pts',(0.306965664652279,2.19815176891556,8.66868449319783));
#62859=CARTESIAN_POINT('Ctrl Pts',(0.30674668291707,2.19883401013424,8.66872933095073));
#62860=CARTESIAN_POINT('Ctrl Pts',(0.306437725610052,2.19978565332511,8.66879175617843));
#62861=CARTESIAN_POINT('Ctrl Pts',(0.306349668556235,2.20005566882286,8.66880945518048));
#62862=CARTESIAN_POINT('Ctrl Pts',(0.306196949718405,2.20052186964667,8.66883999036363));
#62863=CARTESIAN_POINT('Ctrl Pts',(0.306132456239882,2.20071810925153,8.66885283648184));
#62864=CARTESIAN_POINT('Ctrl Pts',(0.30599800742989,2.2011258854847,8.66887951497889));
#62865=CARTESIAN_POINT('Ctrl Pts',(0.305928021496317,2.20133741130375,8.66889334543396));
#62866=CARTESIAN_POINT('Ctrl Pts',(0.305763475409961,2.2018330121822,8.66892573036467));
#62867=CARTESIAN_POINT('Ctrl Pts',(0.305668738334773,2.20211702929209,8.66894427433671));
#62868=CARTESIAN_POINT('Ctrl Pts',(0.305367427793272,2.2030161672356,8.66900293410981));
#62869=CARTESIAN_POINT('Ctrl Pts',(0.305159390649157,2.20363080133284,8.66904296384211));
#62870=CARTESIAN_POINT('Ctrl Pts',(0.304661907110309,2.20508610021847,8.66913758977227));
#62871=CARTESIAN_POINT('Ctrl Pts',(0.304370833728097,2.20592620885011,8.66919209259535));
#62872=CARTESIAN_POINT('Ctrl Pts',(0.303349863577725,2.20883402020328,8.66938034964859));
#62873=CARTESIAN_POINT('Ctrl Pts',(0.302602325483185,2.21089552237283,8.6695131300002));
#62874=CARTESIAN_POINT('Ctrl Pts',(0.29915461053368,2.2201088320558,8.67010414988252));
#62875=CARTESIAN_POINT('Ctrl Pts',(0.296221335244625,2.2271713457132,8.6705506811821));
#62876=CARTESIAN_POINT('Ctrl Pts',(0.286376291092042,2.24868129121374,8.67190966754929));
#62877=CARTESIAN_POINT('Ctrl Pts',(0.278637263801769,2.26272318402109,8.67279629043257));
#62878=CARTESIAN_POINT('Ctrl Pts',(0.261703453147865,2.28867074440385,8.67453133740211));
#62879=CARTESIAN_POINT('Ctrl Pts',(0.252657347459537,2.30062292434542,8.67537647152513));
#62880=CARTESIAN_POINT('Ctrl Pts',(0.241070603887207,2.31389990449348,8.67640600982071));
#62881=CARTESIAN_POINT('Ctrl Pts',(0.239302748722093,2.31587588819111,8.67656176004499));
#62882=CARTESIAN_POINT('Ctrl Pts',(0.233214445075489,2.32251427090134,8.67709407076778));
#62883=CARTESIAN_POINT('Ctrl Pts',(0.228780742600018,2.32707034475708,8.67747494837282));
#62884=CARTESIAN_POINT('Ctrl Pts',(0.22347829058257,2.33220612063115,8.67792424948242));
#62885=CARTESIAN_POINT('Ctrl Pts',(0.222737727214367,2.33291658089851,8.67798686443318));
#62886=CARTESIAN_POINT('Ctrl Pts',(0.221629654358644,2.33396949427333,8.67808035602638));
#62887=CARTESIAN_POINT('Ctrl Pts',(0.221264712195126,2.334314649722,8.67811111588517));
#62888=CARTESIAN_POINT('Ctrl Pts',(0.220612650659917,2.33492847553018,8.67816602094904));
#62889=CARTESIAN_POINT('Ctrl Pts',(0.220325843080183,2.33519747684651,8.67819015186363));
#62890=CARTESIAN_POINT('Ctrl Pts',(0.219720387990236,2.33576326334799,8.67824105315812));
#62891=CARTESIAN_POINT('Ctrl Pts',(0.219401630071303,2.33605992875151,8.67826782859273));
#62892=CARTESIAN_POINT('Ctrl Pts',(0.218558577354822,2.33684136839186,8.67833858472978));
#62893=CARTESIAN_POINT('Ctrl Pts',(0.218033273119016,2.337325045701,8.67838261204206));
#62894=CARTESIAN_POINT('Ctrl Pts',(0.21565209318303,2.33950295411902,8.67858191720156));
#62895=CARTESIAN_POINT('Ctrl Pts',(0.213778088120343,2.34117715229746,8.6787380387998));
#62896=CARTESIAN_POINT('Ctrl Pts',(0.205483993376011,2.34841430456749,8.67942599987128));
#62897=CARTESIAN_POINT('Ctrl Pts',(0.198865464501719,2.35374365721168,8.67996732857903));
#62898=CARTESIAN_POINT('Ctrl Pts',(0.180749550684643,2.36718645791379,8.68143036422119));
#62899=CARTESIAN_POINT('Ctrl Pts',(0.168919020419637,2.37481865881849,8.68236773658319));
#62900=CARTESIAN_POINT('Ctrl Pts',(0.143747347497387,2.38881677584888,8.68430995647952));
#62901=CARTESIAN_POINT('Ctrl Pts',(0.130389340437173,2.39508822395324,8.68531364011999));
#62902=CARTESIAN_POINT('Ctrl Pts',(0.113602003427085,2.40160643804579,8.68651514136518));
#62903=CARTESIAN_POINT('Ctrl Pts',(0.110537226817099,2.40274309450574,8.68673210350815));
#62904=CARTESIAN_POINT('Ctrl Pts',(0.106243873291195,2.40426151084052,8.68703227399758));
#62905=CARTESIAN_POINT('Ctrl Pts',(0.105029566409871,2.40468281516359,8.68711675661527));
#62906=CARTESIAN_POINT('Ctrl Pts',(0.102283052369747,2.40561734855506,8.68730685540025));
#62907=CARTESIAN_POINT('Ctrl Pts',(0.100749428044346,2.40612634560497,8.68741231727358));
#62908=CARTESIAN_POINT('Ctrl Pts',(0.0987757888328263,2.40676494157526,
8.68754710284833));
#62909=CARTESIAN_POINT('Ctrl Pts',(0.0983392610149304,2.40690515731545,
8.68757685613368));
#62910=CARTESIAN_POINT('Ctrl Pts',(0.0932633386534025,2.40852363686374,
8.68792213532385));
#62911=CARTESIAN_POINT('Ctrl Pts',(0.0885909960822404,2.4098976067008,8.68823327129162));
#62912=CARTESIAN_POINT('Ctrl Pts',(0.0833431179823502,2.41131241537206,
8.68857395002852));
#62913=CARTESIAN_POINT('Ctrl Pts',(0.082796836798722,2.41145814984909,8.68860930772208));
#62914=CARTESIAN_POINT('Ctrl Pts',(0.0819759555784916,2.41167482857076,
8.68866227748653));
#62915=CARTESIAN_POINT('Ctrl Pts',(0.0817016443932521,2.41174684819992,
8.68867995122046));
#62916=CARTESIAN_POINT('Ctrl Pts',(0.0812274762474998,2.41187067087675,
8.6887104545704));
#62917=CARTESIAN_POINT('Ctrl Pts',(0.0810276645329549,2.41192264398651,
8.6887232940753));
#62918=CARTESIAN_POINT('Ctrl Pts',(0.0806120469780002,2.41203032413868,
8.68874997063392));
#62919=CARTESIAN_POINT('Ctrl Pts',(0.0803962335592368,2.41208599925314,
8.6887638057443));
#62920=CARTESIAN_POINT('Ctrl Pts',(0.0799666240730491,2.41219635385069,
8.68879131320454));
#62921=CARTESIAN_POINT('Ctrl Pts',(0.0797528289626704,2.41225103778283,
8.68880498582793));
#62922=CARTESIAN_POINT('Ctrl Pts',(0.0790194524669056,2.41243781648468,
8.68885183081006));
#62923=CARTESIAN_POINT('Ctrl Pts',(0.0784995940727626,2.41256883526366,
8.68888494097346));
#62924=CARTESIAN_POINT('Ctrl Pts',(0.0742492066112446,2.41362877840991,
8.68915488393508));
#62925=CARTESIAN_POINT('Ctrl Pts',(0.0705024576010375,2.4144922288318,8.68938801496147));
#62926=CARTESIAN_POINT('Ctrl Pts',(0.062545550252067,2.41617656444665,8.68987467350211));
#62927=CARTESIAN_POINT('Ctrl Pts',(0.0583326376750847,2.41698087099498,
8.69012740128338));
#62928=CARTESIAN_POINT('Ctrl Pts',(0.0408897968480715,2.41995140192052,
8.69115808501131));
#62929=CARTESIAN_POINT('Ctrl Pts',(0.0275463330329515,2.42137536593075,
8.69190989759375));
#62930=CARTESIAN_POINT('Ctrl Pts',(-0.00920744555482762,2.42299090349877,
8.69396745206395));
#62931=CARTESIAN_POINT('Ctrl Pts',(-0.0326067896022078,2.42147249786692,
8.69526791844942));
#62932=CARTESIAN_POINT('Ctrl Pts',(-0.0560014621145417,2.41737225806352,
8.69667375113669));
#62933=CARTESIAN_POINT('Ctrl Pts',(-0.0563676828391008,2.41730741919634,
8.69669578307073));
#62934=CARTESIAN_POINT('Ctrl Pts',(-0.0623288190750037,2.41624136266905,
8.69705481836407));
#62935=CARTESIAN_POINT('Ctrl Pts',(-0.0678961103403432,2.41509299138242,
8.69739606797671));
#62936=CARTESIAN_POINT('Ctrl Pts',(-0.0743837459729702,2.4135748613147,
8.69780171258002));
#62937=CARTESIAN_POINT('Ctrl Pts',(-0.0753365840236626,2.41334730633582,
8.69786149228186));
#62938=CARTESIAN_POINT('Ctrl Pts',(-0.0767737800217712,2.41299714366867,
8.69795197142869));
#62939=CARTESIAN_POINT('Ctrl Pts',(-0.0772589206176465,2.41287774677042,
8.6979825673312));
#62940=CARTESIAN_POINT('Ctrl Pts',(-0.078125080418771,2.41266244067464,
8.6980372893661));
#62941=CARTESIAN_POINT('Ctrl Pts',(-0.0785062063791439,2.41256696171676,
8.69806140156535));
#62942=CARTESIAN_POINT('Ctrl Pts',(-0.0793108163144453,2.41236382788214,
8.69811237700117));
#62943=CARTESIAN_POINT('Ctrl Pts',(-0.0797342575422867,2.41225600830862,
8.69813924551946));
#62944=CARTESIAN_POINT('Ctrl Pts',(-0.0808556030816881,2.41196805380572,
8.69821050929332));
#62945=CARTESIAN_POINT('Ctrl Pts',(-0.0815531216571581,2.41178643889611,
8.69825495237002));
#62946=CARTESIAN_POINT('Ctrl Pts',(-0.0847442344969672,2.41094411860663,
8.69845880627202));
#62947=CARTESIAN_POINT('Ctrl Pts',(-0.0872303931161674,2.410255842928,8.69861910877855));
#62948=CARTESIAN_POINT('Ctrl Pts',(-0.105917800988257,2.40483999626897,
8.69983555471317));
#62949=CARTESIAN_POINT('Ctrl Pts',(-0.121730933814442,2.39887693620633,
8.70093260999324));
#62950=CARTESIAN_POINT('Ctrl Pts',(-0.144336276134454,2.38826005966262,
8.70259814290849));
#62951=CARTESIAN_POINT('Ctrl Pts',(-0.151537239450821,2.38454047016076,
8.70314400401242));
#62952=CARTESIAN_POINT('Ctrl Pts',(-0.16617655690857,2.37626521959363,8.7042809203921));
#62953=CARTESIAN_POINT('Ctrl Pts',(-0.173585945467618,2.37167083299168,
8.70487183322863));
#62954=CARTESIAN_POINT('Ctrl Pts',(-0.192890183645024,2.35858820235948,
8.70644131211505));
#62955=CARTESIAN_POINT('Ctrl Pts',(-0.204411054725253,2.3495810804317,8.70741063552269));
#62956=CARTESIAN_POINT('Ctrl Pts',(-0.215959441337407,2.33921438773561,
8.70838660137789));
#62957=CARTESIAN_POINT('Ctrl Pts',(-0.216634003733595,2.33860367154802,
8.7084436235559));
#62958=CARTESIAN_POINT('Ctrl Pts',(-0.217537896780091,2.33777833735934,
8.70852003971562));
#62959=CARTESIAN_POINT('Ctrl Pts',(-0.217769505071698,2.33756623690193,
8.70853962087396));
#62960=CARTESIAN_POINT('Ctrl Pts',(-0.218158966280046,2.33720853098944,
8.7085725482492));
#62961=CARTESIAN_POINT('Ctrl Pts',(-0.218316983725192,2.33706310628248,
8.70858590816913));
#62962=CARTESIAN_POINT('Ctrl Pts',(-0.218619803192187,2.33678385956987,
8.70861151082394));
#62963=CARTESIAN_POINT('Ctrl Pts',(-0.218764626703939,2.33665006360433,
8.70862375533543));
#62964=CARTESIAN_POINT('Ctrl Pts',(-0.219063376292857,2.33637355362213,
8.70864901414304));
#62965=CARTESIAN_POINT('Ctrl Pts',(-0.219217285218453,2.33623082260119,
8.70866202701847));
#62966=CARTESIAN_POINT('Ctrl Pts',(-0.219564391655619,2.33590829403369,
8.7086913751546));
#62967=CARTESIAN_POINT('Ctrl Pts',(-0.219757508271615,2.33572840905674,
8.70870770372155));
#62968=CARTESIAN_POINT('Ctrl Pts',(-0.220657564641559,2.33488795393915,
8.70878380917562));
#62969=CARTESIAN_POINT('Ctrl Pts',(-0.221361758148437,2.33422443046147,
8.70884336210164));
#62970=CARTESIAN_POINT('Ctrl Pts',(-0.229923416863778,2.32608414215394,
8.70956768142848));
#62971=CARTESIAN_POINT('Ctrl Pts',(-0.23740253568767,2.31821757233283,8.71020326249131));
#62972=CARTESIAN_POINT('Ctrl Pts',(-0.249055292319071,2.3046512362283,8.71122819593721));
#62973=CARTESIAN_POINT('Ctrl Pts',(-0.253463360288602,2.29916575733967,
8.71162526417457));
#62974=CARTESIAN_POINT('Ctrl Pts',(-0.272792659146722,2.27342982719718,
8.71343174032465));
#62975=CARTESIAN_POINT('Ctrl Pts',(-0.285489588884242,2.25162237894765,
8.71481676172906));
#62976=CARTESIAN_POINT('Ctrl Pts',(-0.295800567586154,2.22792062984747,
8.71633809485773));
#62977=CARTESIAN_POINT('Ctrl Pts',(-0.296077069642911,2.22727934689565,
8.71637926105461));
#62978=CARTESIAN_POINT('Ctrl Pts',(-0.298928977146458,2.22060542173213,
8.71680775082826));
#62979=CARTESIAN_POINT('Ctrl Pts',(-0.301321567627375,2.21449674539301,
8.71720056617074));
#62980=CARTESIAN_POINT('Ctrl Pts',(-0.303874135358511,2.20734411176951,
8.71766277266108));
#62981=CARTESIAN_POINT('Ctrl Pts',(-0.304217563481681,2.20636692390714,
8.71772596596596));
#62982=CARTESIAN_POINT('Ctrl Pts',(-0.304721155312714,2.20491161689075,
8.71782015416331));
#62983=CARTESIAN_POINT('Ctrl Pts',(-0.304884919655724,2.20443474333623,
8.71785102968665));
#62984=CARTESIAN_POINT('Ctrl Pts',(-0.305174479942624,2.20358507237578,
8.71790606440589));
#62985=CARTESIAN_POINT('Ctrl Pts',(-0.305300713845271,2.20321242440102,
8.71793020905894));
#62986=CARTESIAN_POINT('Ctrl Pts',(-0.305564891805026,2.20242783433434,
8.71798106064633));
#62987=CARTESIAN_POINT('Ctrl Pts',(-0.30570268586448,2.20201584289972,8.71800777247888));
#62988=CARTESIAN_POINT('Ctrl Pts',(-0.306063324250148,2.20093027563092,
8.71807818174809));
#62989=CARTESIAN_POINT('Ctrl Pts',(-0.30628477712196,2.20025624309972,8.71812192497404));
#62990=CARTESIAN_POINT('Ctrl Pts',(-0.30726667673414,2.19723403322372,8.71831818005326));
#62991=CARTESIAN_POINT('Ctrl Pts',(-0.308002341522887,2.1948779474879,8.71847150431057));
#62992=CARTESIAN_POINT('Ctrl Pts',(-0.313198332671817,2.17753933768661,
8.71960247013815));
#62993=CARTESIAN_POINT('Ctrl Pts',(-0.316589686574244,2.16226062690177,
8.72061502137044));
#62994=CARTESIAN_POINT('Ctrl Pts',(-0.321146229598096,2.13121460337009,
8.72269988635691));
#62995=CARTESIAN_POINT('Ctrl Pts',(-0.322287724825793,2.11548544269752,
8.72376975591092));
#62996=CARTESIAN_POINT('Ctrl Pts',(-0.322274893015885,2.09973740411269,
8.72483344686166));
#62997=CARTESIAN_POINT('',(-0.322274962187229,2.10015611604601,8.97472265507268));
#62998=CARTESIAN_POINT('Ctrl Pts',(-0.322274892771064,2.09973710382478,
8.72483346714441));
#62999=CARTESIAN_POINT('Ctrl Pts',(-0.322260696355795,2.08233423288161,
8.72600893253744));
#63000=CARTESIAN_POINT('Ctrl Pts',(-0.320836875012741,2.06495801800556,
8.72717327402486));
#63001=CARTESIAN_POINT('Ctrl Pts',(-0.317940286355703,2.0473182359678,8.72829440674435));
#63002=CARTESIAN_POINT('Ctrl Pts',(-0.31786357071133,2.04685732063037,8.72832365698864));
#63003=CARTESIAN_POINT('Ctrl Pts',(-0.317737437134452,2.04610954261467,
8.72837103834983));
#63004=CARTESIAN_POINT('Ctrl Pts',(-0.317688632838165,2.04582257923291,
8.72838920358338));
#63005=CARTESIAN_POINT('Ctrl Pts',(-0.317602439820313,2.04531989596424,
8.72842099292514));
#63006=CARTESIAN_POINT('Ctrl Pts',(-0.317565220040452,2.04510414789333,
8.72843462657574));
#63007=CARTESIAN_POINT('Ctrl Pts',(-0.317489830078936,2.04466978519519,
8.72846205443247));
#63008=CARTESIAN_POINT('Ctrl Pts',(-0.317451653830905,2.04445117143337,
8.72847584829638));
#63009=CARTESIAN_POINT('Ctrl Pts',(-0.31737727683206,2.04402783731317,8.72850253883455));
#63010=CARTESIAN_POINT('Ctrl Pts',(-0.317341103900015,2.04382311310411,
8.72851543708006));
#63011=CARTESIAN_POINT('Ctrl Pts',(-0.317254163107915,2.04333382695032,
8.72854624169374));
#63012=CARTESIAN_POINT('Ctrl Pts',(-0.317203210348791,2.04304929742896,
8.72856413747114));
#63013=CARTESIAN_POINT('Ctrl Pts',(-0.317047606122362,2.04218706225256,
8.72861831599577));
#63014=CARTESIAN_POINT('Ctrl Pts',(-0.316941758010437,2.04160956961178,
8.72865453106242));
#63015=CARTESIAN_POINT('Ctrl Pts',(-0.315808840250748,2.03552237897722,
8.72903553860515));
#63016=CARTESIAN_POINT('Ctrl Pts',(-0.314639712590034,2.03003967012019,
8.72937244093462));
#63017=CARTESIAN_POINT('Ctrl Pts',(-0.312846623179465,2.02258940917239,
8.72982508042066));
#63018=CARTESIAN_POINT('Ctrl Pts',(-0.31234600957366,2.02059357791735,8.72994582436981));
#63019=CARTESIAN_POINT('Ctrl Pts',(-0.310762677926306,2.01452797041486,
8.73031159170614));
#63020=CARTESIAN_POINT('Ctrl Pts',(-0.30961924938343,2.01047440226361,8.73055439134698));
#63021=CARTESIAN_POINT('Ctrl Pts',(-0.306882044035726,2.00145149075179,
8.73109346529664));
#63022=CARTESIAN_POINT('Ctrl Pts',(-0.30524636004538,1.99649608629821,8.73138858059926));
#63023=CARTESIAN_POINT('Ctrl Pts',(-0.302406289795634,1.98854593456659,
8.73186352575278));
#63024=CARTESIAN_POINT('Ctrl Pts',(-0.301276016993766,1.98552583380336,
8.7320442979145));
#63025=CARTESIAN_POINT('Ctrl Pts',(-0.299068084915275,1.97988555720773,
8.73238334644627));
#63026=CARTESIAN_POINT('Ctrl Pts',(-0.298000834323777,1.9772616539135,8.73254167031454));
#63027=CARTESIAN_POINT('Ctrl Pts',(-0.294703160179138,1.96945077698144,
8.73301556488068));
#63028=CARTESIAN_POINT('Ctrl Pts',(-0.292370899332094,1.96430803774405,
8.73333105765857));
#63029=CARTESIAN_POINT('Ctrl Pts',(-0.283108752483761,1.94523347323296,
8.73452173821856));
#63030=CARTESIAN_POINT('Ctrl Pts',(-0.275308865188227,1.93174959309689,
8.73540663830876));
#63031=CARTESIAN_POINT('Ctrl Pts',(-0.263174894708821,1.91389098056518,
8.73668245830491));
#63032=CARTESIAN_POINT('Ctrl Pts',(-0.259644110619399,1.9089960186471,8.73704377447665));
#63033=CARTESIAN_POINT('Ctrl Pts',(-0.255217113772652,1.90320830901687,
8.73748656098228));
#63034=CARTESIAN_POINT('Ctrl Pts',(-0.254450274820983,1.90221779054555,
8.73756290645172));
#63035=CARTESIAN_POINT('Ctrl Pts',(-0.253341546524175,1.90080277747021,
8.73767279686496));
#63036=CARTESIAN_POINT('Ctrl Pts',(-0.253004318061632,1.90037463163403,
8.73770615633022));
#63037=CARTESIAN_POINT('Ctrl Pts',(-0.252417889532214,1.89963397385541,
8.73776405665592));
#63038=CARTESIAN_POINT('Ctrl Pts',(-0.252169190378016,1.89932106535403,
8.73778857745584));
#63039=CARTESIAN_POINT('Ctrl Pts',(-0.25169036002893,1.8987209057868,8.73783572314968));
#63040=CARTESIAN_POINT('Ctrl Pts',(-0.251460317444367,1.89843358452408,
8.73785834446517));
#63041=CARTESIAN_POINT('Ctrl Pts',(-0.250917944696875,1.89775853903116,
8.7379116118476));
#63042=CARTESIAN_POINT('Ctrl Pts',(-0.250605207932157,1.89737114406246,
8.73794227425981));
#63043=CARTESIAN_POINT('Ctrl Pts',(-0.249680926940995,1.8962316265383,8.73803274401803));
#63044=CARTESIAN_POINT('Ctrl Pts',(-0.249066889553967,1.89548154167325,
8.7380926520914));
#63045=CARTESIAN_POINT('Ctrl Pts',(-0.243666075723224,1.88894450677984,
8.73861790660274));
#63046=CARTESIAN_POINT('Ctrl Pts',(-0.238682108603656,1.88332417427561,
8.73909129644687));
#63047=CARTESIAN_POINT('Ctrl Pts',(-0.217588256326666,1.86114863221881,
8.7410529224041));
#63048=CARTESIAN_POINT('Ctrl Pts',(-0.199919201675758,1.84617601021165,
8.74260890005521));
#63049=CARTESIAN_POINT('Ctrl Pts',(-0.173816208021734,1.82848500097667,
8.74474255100959));
#63050=CARTESIAN_POINT('Ctrl Pts',(-0.166643019397468,1.82402431086632,
8.74531309350797));
#63051=CARTESIAN_POINT('Ctrl Pts',(-0.152020182018295,1.81570926057497,
8.74643595576111));
#63052=CARTESIAN_POINT('Ctrl Pts',(-0.144578284204794,1.81185333076884,
8.74698796541639));
#63053=CARTESIAN_POINT('Ctrl Pts',(-0.134927128523312,1.80732089286679,
8.74767229865384));
#63054=CARTESIAN_POINT('Ctrl Pts',(-0.132849930750197,1.80637219761226,
8.74781777440189));
#63055=CARTESIAN_POINT('Ctrl Pts',(-0.129502643317078,1.80488622223059,
8.74804910533886));
#63056=CARTESIAN_POINT('Ctrl Pts',(-0.128238923441014,1.80433489361735,
8.74813574081585));
#63057=CARTESIAN_POINT('Ctrl Pts',(-0.126702132708159,1.80367613798968,
8.74824021564959));
#63058=CARTESIAN_POINT('Ctrl Pts',(-0.126432428871207,1.80356096316298,
8.74825851799625));
#63059=CARTESIAN_POINT('Ctrl Pts',(-0.125960373451495,1.80336013715884,
8.74829049430182));
#63060=CARTESIAN_POINT('Ctrl Pts',(-0.125758091333839,1.80327432471857,
8.74830417804093));
#63061=CARTESIAN_POINT('Ctrl Pts',(-0.125350936754697,1.80310209209146,
8.74833168322957));
#63062=CARTESIAN_POINT('Ctrl Pts',(-0.125146061997697,1.80301567678846,
8.74834550438119));
#63063=CARTESIAN_POINT('Ctrl Pts',(-0.124750087023205,1.80284913873433,
8.74837218036557));
#63064=CARTESIAN_POINT('Ctrl Pts',(-0.124558999434806,1.80276898845571,
8.74838503689722));
#63065=CARTESIAN_POINT('Ctrl Pts',(-0.124103536938228,1.80257846443069,
8.74841564149292));
#63066=CARTESIAN_POINT('Ctrl Pts',(-0.123839091354566,1.80246825857577,
8.74843337927783));
#63067=CARTESIAN_POINT('Ctrl Pts',(-0.122899429292558,1.80207813075246,
8.74849629679433));
#63068=CARTESIAN_POINT('Ctrl Pts',(-0.12222340129491,1.80180015074258,8.74854135928366));
#63069=CARTESIAN_POINT('Ctrl Pts',(-0.112330754647716,1.79777162673305,
8.74919790441448));
#63070=CARTESIAN_POINT('Ctrl Pts',(-0.102945133706881,1.79444716865806,
8.74978441829878));
#63071=CARTESIAN_POINT('Ctrl Pts',(-0.0857908400194216,1.78925147505316,
8.75081721926188));
#63072=CARTESIAN_POINT('Ctrl Pts',(-0.0780785500121411,1.78722457757065,
8.75126781189534));
#63073=CARTESIAN_POINT('Ctrl Pts',(-0.0443138837009667,1.77967766057423,
8.75321054427306));
#63074=CARTESIAN_POINT('Ctrl Pts',(-0.0177120305236979,1.77711255364482,
8.75467479387227));
#63075=CARTESIAN_POINT('Ctrl Pts',(0.0148563386640629,1.77801250497585,
8.75660263305416));
#63076=CARTESIAN_POINT('Ctrl Pts',(0.0208047252700085,1.77834208521132,
8.75695973339654));
#63077=CARTESIAN_POINT('Ctrl Pts',(0.0278372007182144,1.77892761338925,
8.7573890124909));
#63078=CARTESIAN_POINT('Ctrl Pts',(0.0289336293793941,1.77902456132658,
8.75745614506992));
#63079=CARTESIAN_POINT('Ctrl Pts',(0.0305441895539643,1.77917528881871,
8.75755506400842));
#63080=CARTESIAN_POINT('Ctrl Pts',(0.0310587307676597,1.77922469225601,
8.75758671267006));
#63081=CARTESIAN_POINT('Ctrl Pts',(0.0319664006810245,1.77931404614726,
8.75764262421642));
#63082=CARTESIAN_POINT('Ctrl Pts',(0.032359579890751,1.77935348223007,8.75766687086365));
#63083=CARTESIAN_POINT('Ctrl Pts',(0.0331265157681409,1.77943183129544,
8.7577142198783));
#63084=CARTESIAN_POINT('Ctrl Pts',(0.0335002790241556,1.77947067507485,
8.75773732003031));
#63085=CARTESIAN_POINT('Ctrl Pts',(0.0345037177054995,1.77957673289986,
8.75779940380947));
#63086=CARTESIAN_POINT('Ctrl Pts',(0.0351332619766329,1.77964514904817,
8.75783842525451));
#63087=CARTESIAN_POINT('Ctrl Pts',(0.0374279163017484,1.77990136743283,
8.75798091755415));
#63088=CARTESIAN_POINT('Ctrl Pts',(0.0390917341974001,1.78010029753503,
8.75808473858858));
#63089=CARTESIAN_POINT('Ctrl Pts',(0.0673841753349688,1.78370702663367,
8.75985892414296));
#63090=CARTESIAN_POINT('Ctrl Pts',(0.0934800062884635,1.79041521019778,
8.76164116536206));
#63091=CARTESIAN_POINT('Ctrl Pts',(0.133196876933989,1.80610944923135,8.76452972936043));
#63092=CARTESIAN_POINT('Ctrl Pts',(0.147507000707802,1.81302473610557,8.76560757647378));
#63093=CARTESIAN_POINT('Ctrl Pts',(0.165513696467116,1.82343058250576,8.76697145076985));
#63094=CARTESIAN_POINT('Ctrl Pts',(0.169720679573648,1.82599211119791,8.76729056943461));
#63095=CARTESIAN_POINT('Ctrl Pts',(0.175217492881881,1.82951418450674,8.76770653218142));
#63096=CARTESIAN_POINT('Ctrl Pts',(0.176561005927488,1.83038924794715,8.76780811898252));
#63097=CARTESIAN_POINT('Ctrl Pts',(0.178773970572868,1.83185424342745,8.76797523877158));
#63098=CARTESIAN_POINT('Ctrl Pts',(0.17964715101956,1.83243845469619,8.76804112564475));
#63099=CARTESIAN_POINT('Ctrl Pts',(0.180813073435839,1.83322680901411,8.76812901168384));
#63100=CARTESIAN_POINT('Ctrl Pts',(0.181108343146563,1.83342717505389,8.76815126103359));
#63101=CARTESIAN_POINT('Ctrl Pts',(0.181572373698216,1.83374318677741,8.76818621392171));
#63102=CARTESIAN_POINT('Ctrl Pts',(0.181741357112701,1.83385850268467,8.76819893979343));
#63103=CARTESIAN_POINT('Ctrl Pts',(0.182091513180357,1.83409794156049,8.76822530363758));
#63104=CARTESIAN_POINT('Ctrl Pts',(0.182272667340052,1.8342220878333,8.76823893974835));
#63105=CARTESIAN_POINT('Ctrl Pts',(0.182684697413777,1.83450507445787,8.76826994742903));
#63106=CARTESIAN_POINT('Ctrl Pts',(0.182915492797769,1.83466403060693,8.76828731095464));
#63107=CARTESIAN_POINT('Ctrl Pts',(0.183631540248659,1.83515857360068,8.76834116653154));
#63108=CARTESIAN_POINT('Ctrl Pts',(0.184116081808442,1.83549519447874,8.7683775884164));
#63109=CARTESIAN_POINT('Ctrl Pts',(0.187807285508566,1.83807460628332,8.76865490516783));
#63110=CARTESIAN_POINT('Ctrl Pts',(0.190973955757526,1.8403744235781,8.76889199097375));
#63111=CARTESIAN_POINT('Ctrl Pts',(0.194546229958606,1.84306955195291,8.76915947535224));
#63112=CARTESIAN_POINT('Ctrl Pts',(0.194993458407329,1.84340880390833,8.76919296344005));
#63113=CARTESIAN_POINT('Ctrl Pts',(0.196045023192711,1.84421082143432,8.76927171100662));
#63114=CARTESIAN_POINT('Ctrl Pts',(0.196648613313292,1.84467456473654,8.7693169172034));
#63115=CARTESIAN_POINT('Ctrl Pts',(0.202992241002735,1.849584265379,8.7697921529898));
#63116=CARTESIAN_POINT('Ctrl Pts',(0.208582489825422,1.85422113909048,8.77021206647014));
#63117=CARTESIAN_POINT('Ctrl Pts',(0.229272364076566,1.87259735362667,8.7717908520609));
#63118=CARTESIAN_POINT('Ctrl Pts',(0.24321124562788,1.88757088328228,8.7729099371792));
#63119=CARTESIAN_POINT('Ctrl Pts',(0.260543291125407,1.91014954018143,8.77452207103142));
#63120=CARTESIAN_POINT('Ctrl Pts',(0.265204698588115,1.9167175401006,8.77498284455656));
#63121=CARTESIAN_POINT('Ctrl Pts',(0.274922117527831,1.93155756178613,8.77601551048747));
#63122=CARTESIAN_POINT('Ctrl Pts',(0.279860544777585,1.9398966809335,8.77659048054858));
#63123=CARTESIAN_POINT('Ctrl Pts',(0.284955152850656,1.94945747186269,8.7772492787722));
#63124=CARTESIAN_POINT('Ctrl Pts',(0.285489271375744,1.95047285266493,8.77731923677799));
#63125=CARTESIAN_POINT('Ctrl Pts',(0.286260229435344,1.95195766452471,8.77742153400054));
#63126=CARTESIAN_POINT('Ctrl Pts',(0.286501364179161,1.95242486534765,8.77745372159955));
#63127=CARTESIAN_POINT('Ctrl Pts',(0.286922335528286,1.95324542187343,8.77751025337633));
#63128=CARTESIAN_POINT('Ctrl Pts',(0.287102665797678,1.95359852420242,8.7775345801248));
#63129=CARTESIAN_POINT('Ctrl Pts',(0.287451395209751,1.95428448890782,8.77758183952082));
#63130=CARTESIAN_POINT('Ctrl Pts',(0.287619869010104,1.95461731282687,8.77760476950006));
#63131=CARTESIAN_POINT('Ctrl Pts',(0.288020478083653,1.95541214722366,8.77765953052191));
#63132=CARTESIAN_POINT('Ctrl Pts',(0.288252079560253,1.95587442423281,8.77769138020848));
#63133=CARTESIAN_POINT('Ctrl Pts',(0.289075665002224,1.95752822836355,8.77780532656314));
#63134=CARTESIAN_POINT('Ctrl Pts',(0.289661375319058,1.95872284907736,8.77788764201278));
#63135=CARTESIAN_POINT('Ctrl Pts',(0.299662889516564,1.97944570635287,8.77931577445174));
#63136=CARTESIAN_POINT('Ctrl Pts',(0.307090040568869,1.99986732285151,8.78073238544349));
#63137=CARTESIAN_POINT('Ctrl Pts',(0.31688438347207,2.03853895590807,8.78341212989071));
#63138=CARTESIAN_POINT('Ctrl Pts',(0.319851863138486,2.05654935492758,8.78465750305385));
#63139=CARTESIAN_POINT('Ctrl Pts',(0.322017719441619,2.08406849100827,8.78649255061327));
#63140=CARTESIAN_POINT('Ctrl Pts',(0.322345127745983,2.09345172232237,8.7871059573917));
#63141=CARTESIAN_POINT('Ctrl Pts',(0.322254357045707,2.10376349600042,8.78775742936807));
#63142=CARTESIAN_POINT('Ctrl Pts',(0.322242201653298,2.10469020888693,8.78781577493486));
#63143=CARTESIAN_POINT('Ctrl Pts',(0.322214187898982,2.1062972893788,8.78791659123541));
#63144=CARTESIAN_POINT('Ctrl Pts',(0.322200171904551,2.10697767737924,8.78795916024547));
#63145=CARTESIAN_POINT('Ctrl Pts',(0.322176874657326,2.10795782592793,8.78802031554977));
#63146=CARTESIAN_POINT('Ctrl Pts',(0.32216933012098,2.1082576200331,8.78803899816941));
#63147=CARTESIAN_POINT('Ctrl Pts',(0.322155448658234,2.10878021668604,8.78807152533318));
#63148=CARTESIAN_POINT('Ctrl Pts',(0.322149299038407,2.10900302368569,8.78808538044692));
#63149=CARTESIAN_POINT('Ctrl Pts',(0.322137008366368,2.10943218342938,8.7881120427815));
#63150=CARTESIAN_POINT('Ctrl Pts',(0.322130900200218,2.10963853621049,8.78812485185188));
#63151=CARTESIAN_POINT('Ctrl Pts',(0.322115932129284,2.1101282914895,8.78815522700341));
#63152=CARTESIAN_POINT('Ctrl Pts',(0.322106896469763,2.11041168901096,8.78817278316068));
#63153=CARTESIAN_POINT('Ctrl Pts',(0.322073799759564,2.11140844374886,8.78823446016852));
#63154=CARTESIAN_POINT('Ctrl Pts',(0.322047742638686,2.11212173933942,8.78827846973815));
#63155=CARTESIAN_POINT('Ctrl Pts',(0.321665481461743,2.12171238658769,8.78886855655391));
#63156=CARTESIAN_POINT('Ctrl Pts',(0.320944658955875,2.13057235535916,8.78939474612698));
#63157=CARTESIAN_POINT('Ctrl Pts',(0.316347648893621,2.16789946524014,8.79157348813092));
#63158=CARTESIAN_POINT('Ctrl Pts',(0.309041647680371,2.19581066888568,8.79311950746693));
#63159=CARTESIAN_POINT('Ctrl Pts',(0.29371756233942,2.2331402184187,8.79544024328249));
#63160=CARTESIAN_POINT('Ctrl Pts',(0.288724551688154,2.24364683117515,8.79612270671749));
#63161=CARTESIAN_POINT('Ctrl Pts',(0.282191295736733,2.25567111679856,8.79695002621638));
#63162=CARTESIAN_POINT('Ctrl Pts',(0.281189927467982,2.25747269090075,8.79707523921317));
#63163=CARTESIAN_POINT('Ctrl Pts',(0.279843320442655,2.25984158490248,8.79724159771543));
#63164=CARTESIAN_POINT('Ctrl Pts',(0.279513496203458,2.26041764768951,8.7972821877295));
#63165=CARTESIAN_POINT('Ctrl Pts',(0.278969967835434,2.2613601953682,8.79734882446085));
#63166=CARTESIAN_POINT('Ctrl Pts',(0.27875731451587,2.26172728651821,8.79737483313035));
#63167=CARTESIAN_POINT('Ctrl Pts',(0.278344478827622,2.2624367076563,8.79742520481471));
#63168=CARTESIAN_POINT('Ctrl Pts',(0.278144388115525,2.26277909032073,8.79744956447199));
#63169=CARTESIAN_POINT('Ctrl Pts',(0.27768184869669,2.26356721583485,8.79750575141895));
#63170=CARTESIAN_POINT('Ctrl Pts',(0.277418958272868,2.26401269700056,8.79753759473544));
#63171=CARTESIAN_POINT('Ctrl Pts',(0.276577230343338,2.26543123397116,8.79763926274733));
#63172=CARTESIAN_POINT('Ctrl Pts',(0.275994341886924,2.2664018651085,8.79770923509907));
#63173=CARTESIAN_POINT('Ctrl Pts',(0.270721457989278,2.27507839611782,8.79833841171719));
#63174=CARTESIAN_POINT('Ctrl Pts',(0.265715376629005,2.28258659570454,8.79890924320437));
#63175=CARTESIAN_POINT('Ctrl Pts',(0.257776643450155,2.2934740931857,8.79977863669193));
#63176=CARTESIAN_POINT('Ctrl Pts',(0.255077637659044,2.2970188279369,8.80006866589417));
#63177=CARTESIAN_POINT('Ctrl Pts',(0.238002577770641,2.31850513974181,8.80186971172069));
#63178=CARTESIAN_POINT('Ctrl Pts',(0.221814876426225,2.33492060095534,8.80344146712607));
#63179=CARTESIAN_POINT('Ctrl Pts',(0.193370247451214,2.35818297835718,8.80591021540188));
#63180=CARTESIAN_POINT('Ctrl Pts',(0.182170533410412,2.36620386777425,8.80682068596833));
#63181=CARTESIAN_POINT('Ctrl Pts',(0.169971149655269,2.37380898286792,8.80772458044402));
#63182=CARTESIAN_POINT('Ctrl Pts',(0.169450426986674,2.37413154437732,8.80776300186166));
#63183=CARTESIAN_POINT('Ctrl Pts',(0.16851369083295,2.37470811638072,8.80783182614452));
#63184=CARTESIAN_POINT('Ctrl Pts',(0.168098016439848,2.37496267033908,8.80786226375829));
#63185=CARTESIAN_POINT('Ctrl Pts',(0.167458972517395,2.37535202234476,8.80790889768027));
#63186=CARTESIAN_POINT('Ctrl Pts',(0.167236016443831,2.37548749244037,8.8079251380064));
#63187=CARTESIAN_POINT('Ctrl Pts',(0.166844569762744,2.37572468859786,8.80795359878342));
#63188=CARTESIAN_POINT('Ctrl Pts',(0.1666761509022,2.37582653078125,8.80796582689884));
#63189=CARTESIAN_POINT('Ctrl Pts',(0.16629511898072,2.37605646277275,8.80799345327738));
#63190=CARTESIAN_POINT('Ctrl Pts',(0.166082451614913,2.37618446100748,8.8080088454511));
#63191=CARTESIAN_POINT('Ctrl Pts',(0.165506183125178,2.3765303937591,8.80805048120272));
#63192=CARTESIAN_POINT('Ctrl Pts',(0.165142297933698,2.37674785773928,8.80807669388768));
#63193=CARTESIAN_POINT('Ctrl Pts',(0.16350972488175,2.3777191446436,8.80819395194698));
#63194=CARTESIAN_POINT('Ctrl Pts',(0.162236271300806,2.37846498146501,8.80828448385238));
#63195=CARTESIAN_POINT('Ctrl Pts',(0.137305765971917,2.39283721444691,8.81003962155796));
#63196=CARTESIAN_POINT('Ctrl Pts',(0.112012697052257,2.4034142518641,8.81152574565271));
#63197=CARTESIAN_POINT('Ctrl Pts',(0.0644520308146028,2.41653157999843,
8.81429426335219));
#63198=CARTESIAN_POINT('Ctrl Pts',(0.0426783635898178,2.4201946969691,8.81555308599202));
#63199=CARTESIAN_POINT('Ctrl Pts',(0.019450692515286,2.4216899459763,8.81696744759775));
#63200=CARTESIAN_POINT('Ctrl Pts',(0.0181977863153876,2.42176325347233,
8.81704393754693));
#63201=CARTESIAN_POINT('Ctrl Pts',(0.0163998204168731,2.42185791742771,
8.81715399902614));
#63202=CARTESIAN_POINT('Ctrl Pts',(0.0158550740017596,2.42188521206049,
8.81718738427328));
#63203=CARTESIAN_POINT('Ctrl Pts',(0.0149109352396885,2.42193011580013,
8.81724531496638));
#63204=CARTESIAN_POINT('Ctrl Pts',(0.0145115733687877,2.42194836493581,
8.81726984029324));
#63205=CARTESIAN_POINT('Ctrl Pts',(0.0137445614716117,2.42198198405806,
8.81731698455669));
#63206=CARTESIAN_POINT('Ctrl Pts',(0.0133769168115668,2.42199746757216,
8.81733959989577));
#63207=CARTESIAN_POINT('Ctrl Pts',(0.0125121573914139,2.42203240371802,
8.81739283778809));
#63208=CARTESIAN_POINT('Ctrl Pts',(0.0120150235689858,2.42205133493157,
8.81742347664173));
#63209=CARTESIAN_POINT('Ctrl Pts',(0.0105505746195737,2.42210370662052,
8.81751383152523));
#63210=CARTESIAN_POINT('Ctrl Pts',(0.00958315677007563,2.42213394033701,
8.81757364792153));
#63211=CARTESIAN_POINT('Ctrl Pts',(0.00114818908164743,2.42235951944911,
8.81809632557724));
#63212=CARTESIAN_POINT('Ctrl Pts',(-0.00632337799140969,2.42229951596798,
8.81856714358265));
#63213=CARTESIAN_POINT('Ctrl Pts',(-0.0452221131712706,2.42063405834695,
8.82106213584235));
#63214=CARTESIAN_POINT('Ctrl Pts',(-0.0762890915469068,2.41469109347257,
8.82322720676722));
#63215=CARTESIAN_POINT('Ctrl Pts',(-0.117051324841573,2.40049506249168,
8.8261097325587));
#63216=CARTESIAN_POINT('Ctrl Pts',(-0.127893051336785,2.39604346267437,
8.82687787116214));
#63217=CARTESIAN_POINT('Ctrl Pts',(-0.139095793645375,2.39071294568465,
8.82765609697782));
#63218=CARTESIAN_POINT('Ctrl Pts',(-0.139721080584836,2.39041294093043,
8.82769948064076));
#63219=CARTESIAN_POINT('Ctrl Pts',(-0.140617868455738,2.38997910667554,
8.82776161950276));
#63220=CARTESIAN_POINT('Ctrl Pts',(-0.140890151361558,2.38984691215967,
8.82778047521528));
#63221=CARTESIAN_POINT('Ctrl Pts',(-0.14136209187765,2.38961696087007,8.82781313785937));
#63222=CARTESIAN_POINT('Ctrl Pts',(-0.14156183498671,2.38951938090572,8.82782695586999));
#63223=CARTESIAN_POINT('Ctrl Pts',(-0.141947637480392,2.38933041113613,
8.82785363335594));
#63224=CARTESIAN_POINT('Ctrl Pts',(-0.142133709195218,2.3892390487218,8.82786649451581));
#63225=CARTESIAN_POINT('Ctrl Pts',(-0.142576989772869,2.38902086404293,
8.82789712137573));
#63226=CARTESIAN_POINT('Ctrl Pts',(-0.142834118289561,2.38889387760688,
8.82791487676211));
#63227=CARTESIAN_POINT('Ctrl Pts',(-0.143747520811072,2.38844126371283,
8.82797791528867));
#63228=CARTESIAN_POINT('Ctrl Pts',(-0.14440285995952,2.38811373867302,8.82802308059625));
#63229=CARTESIAN_POINT('Ctrl Pts',(-0.154046628178938,2.38325281170862,
8.82868687305661));
#63230=CARTESIAN_POINT('Ctrl Pts',(-0.162819991638525,2.37830238230672,
8.82927994136813));
#63231=CARTESIAN_POINT('Ctrl Pts',(-0.182365272159847,2.36603250847289,
8.83060895750549));
#63232=CARTESIAN_POINT('Ctrl Pts',(-0.192954204416631,2.35845521681986,
8.83133509974725));
#63233=CARTESIAN_POINT('Ctrl Pts',(-0.212911693850643,2.34226194539666,
8.8327716051899));
#63234=CARTESIAN_POINT('Ctrl Pts',(-0.222285561657763,2.33369071317039,
8.83348073371653));
#63235=CARTESIAN_POINT('Ctrl Pts',(-0.241380749795235,2.314039489622,8.83504697116557));
#63236=CARTESIAN_POINT('Ctrl Pts',(-0.25089653278207,2.30280140706446,8.83590816030668));
#63237=CARTESIAN_POINT('Ctrl Pts',(-0.260264370181138,2.29006538244534,
8.83686991007667));
#63238=CARTESIAN_POINT('Ctrl Pts',(-0.260913280849371,2.2891736023311,8.83693717484378));
#63239=CARTESIAN_POINT('Ctrl Pts',(-0.261859826732141,2.28785865536907,
8.8370362521097));
#63240=CARTESIAN_POINT('Ctrl Pts',(-0.262161045711064,2.28743806806519,
8.83706792627387));
#63241=CARTESIAN_POINT('Ctrl Pts',(-0.2626905925084,2.28669489662663,8.83712386701633));
#63242=CARTESIAN_POINT('Ctrl Pts',(-0.262919342634793,2.28637261355971,
8.83714811730096));
#63243=CARTESIAN_POINT('Ctrl Pts',(-0.263364356188542,2.28574318996892,
8.83719546145926));
#63244=CARTESIAN_POINT('Ctrl Pts',(-0.263580676674741,2.28543609037149,
8.8372185530955));
#63245=CARTESIAN_POINT('Ctrl Pts',(-0.264159823708576,2.28461084281381,
8.83728058500736));
#63246=CARTESIAN_POINT('Ctrl Pts',(-0.264521661105536,2.28409200564671,
8.83731956298646));
#63247=CARTESIAN_POINT('Ctrl Pts',(-0.265833916905219,2.28219851050813,
8.83746173654556));
#63248=CARTESIAN_POINT('Ctrl Pts',(-0.266775153432269,2.28081754879097,
8.83756528027127));
#63249=CARTESIAN_POINT('Ctrl Pts',(-0.267929849436996,2.27909476163688,
8.83769428828531));
#63250=CARTESIAN_POINT('Ctrl Pts',(-0.268153478127074,2.27875975506551,
8.837719366966));
#63251=CARTESIAN_POINT('Ctrl Pts',(-0.287540395923266,2.24959897488626,
8.83990169283422));
#63252=CARTESIAN_POINT('Ctrl Pts',(-0.301931254759561,2.2178795043545,8.84225666039802));
#63253=CARTESIAN_POINT('Ctrl Pts',(-0.31485105909334,2.17032470634958,8.84557219905085));
#63254=CARTESIAN_POINT('Ctrl Pts',(-0.317728279144217,2.15590717156857,
8.84654588727399));
#63255=CARTESIAN_POINT('Ctrl Pts',(-0.319708477482743,2.14059836451964,
8.84751480552321));
#63256=CARTESIAN_POINT('Ctrl Pts',(-0.319802064784626,2.13985444971627,
8.84756172789254));
#63257=CARTESIAN_POINT('Ctrl Pts',(-0.319930975701138,2.13880005213162,
8.8476279992011));
#63258=CARTESIAN_POINT('Ctrl Pts',(-0.319968444333143,2.1384898414066,8.84764746789428));
#63259=CARTESIAN_POINT('Ctrl Pts',(-0.320032006584502,2.13795708881445,
8.84768085326594));
#63260=CARTESIAN_POINT('Ctrl Pts',(-0.320058319333889,2.13773457374957,
8.8476947823928));
#63261=CARTESIAN_POINT('Ctrl Pts',(-0.320108259446001,2.13730844243144,
8.84772142874444));
#63262=CARTESIAN_POINT('Ctrl Pts',(-0.320131924574502,2.13710483137036,
8.8477341481219));
#63263=CARTESIAN_POINT('Ctrl Pts',(-0.320187211364249,2.13662516227013,
8.84776408319475));
#63264=CARTESIAN_POINT('Ctrl Pts',(-0.320218670357147,2.13634908511332,
8.84778128964151));
#63265=CARTESIAN_POINT('Ctrl Pts',(-0.320310533907743,2.13553353585035,
8.84783205182091));
#63266=CARTESIAN_POINT('Ctrl Pts',(-0.320369932914362,2.1349939480032,8.84786555111782));
#63267=CARTESIAN_POINT('Ctrl Pts',(-0.320878396509613,2.13026517998466,
8.84815839263795));
#63268=CARTESIAN_POINT('Ctrl Pts',(-0.32124666110887,2.12606747643924,8.84841329407567));
#63269=CARTESIAN_POINT('Ctrl Pts',(-0.321544051180808,2.12169395446229,
8.84867474294954));
#63270=CARTESIAN_POINT('Ctrl Pts',(-0.321555447073908,2.12152438076493,
8.84868487360629));
#63271=CARTESIAN_POINT('Ctrl Pts',(-0.321633513349248,2.12034883625798,
8.84875505866966));
#63272=CARTESIAN_POINT('Ctrl Pts',(-0.321695597827328,2.11934255496585,
8.84881491357782));
#63273=CARTESIAN_POINT('Ctrl Pts',(-0.321847816361753,2.11667148176497,
8.84897323585806));
#63274=CARTESIAN_POINT('Ctrl Pts',(-0.321929756761703,2.1150062356838,8.84907136647059));
#63275=CARTESIAN_POINT('Ctrl Pts',(-0.32204088584863,2.11232390002778,8.84922861551369));
#63276=CARTESIAN_POINT('Ctrl Pts',(-0.32207818617969,2.11130719671791,8.84928802972966));
#63277=CARTESIAN_POINT('Ctrl Pts',(-0.32221786023398,2.10693507943468,8.84954277943375));
#63278=CARTESIAN_POINT('Ctrl Pts',(-0.322272620580041,2.10357827202705,
8.84973647614376));
#63279=CARTESIAN_POINT('Ctrl Pts',(-0.322290768041176,2.07713063214126,
8.8512517776118));
#63280=CARTESIAN_POINT('Ctrl Pts',(-0.319825063208097,2.05410476171697,
8.85251106920004));
#63281=CARTESIAN_POINT('Ctrl Pts',(-0.313582461707878,2.02538880381381,
8.8541831089166));
#63282=CARTESIAN_POINT('Ctrl Pts',(-0.312065577726141,2.01927912088184,
8.85454453917948));
#63283=CARTESIAN_POINT('Ctrl Pts',(-0.307731685966037,2.00377920850272,
8.85548100968785));
#63284=CARTESIAN_POINT('Ctrl Pts',(-0.304663580332873,1.99446657045809,
8.85606248285969));
#63285=CARTESIAN_POINT('Ctrl Pts',(-0.300805753399857,1.98433601285977,
8.85672165078864));
#63286=CARTESIAN_POINT('Ctrl Pts',(-0.300430593039771,1.98336502271776,
8.85678510402785));
#63287=CARTESIAN_POINT('Ctrl Pts',(-0.299862416655417,1.98191539886184,
8.85688025153368));
#63288=CARTESIAN_POINT('Ctrl Pts',(-0.299672941906687,1.98143537697742,
8.8569118267362));
#63289=CARTESIAN_POINT('Ctrl Pts',(-0.29934461740526,1.98060940314597,8.85696627706987));
#63290=CARTESIAN_POINT('Ctrl Pts',(-0.299206318471468,1.98026323216522,
8.85698913360348));
#63291=CARTESIAN_POINT('Ctrl Pts',(-0.298919632775466,1.97954923794643,
8.85703635109468));
#63292=CARTESIAN_POINT('Ctrl Pts',(-0.298771167029535,1.97918144725447,
8.85706071468962));
#63293=CARTESIAN_POINT('Ctrl Pts',(-0.298423982093608,1.97832592755294,
8.85711748305613));
#63294=CARTESIAN_POINT('Ctrl Pts',(-0.29822474596679,1.97783841077389,8.85714990527332));
#63295=CARTESIAN_POINT('Ctrl Pts',(-0.29758586554852,1.97628599289326,8.85725338233978));
#63296=CARTESIAN_POINT('Ctrl Pts',(-0.297141709289092,1.9752229689639,8.8573245900226));
#63297=CARTESIAN_POINT('Ctrl Pts',(-0.287349671482454,1.95213593403689,
8.85887885290199));
#63298=CARTESIAN_POINT('Ctrl Pts',(-0.275585829744622,1.93122318310951,
8.86044940394228));
#63299=CARTESIAN_POINT('Ctrl Pts',(-0.246663942788651,1.89101663788483,
8.86378722553699));
#63300=CARTESIAN_POINT('Ctrl Pts',(-0.229281848669844,1.87208076536259,
8.86554801978358));
#63301=CARTESIAN_POINT('Ctrl Pts',(-0.208754706573058,1.85447058540916,
8.86725753455761));
#63302=CARTESIAN_POINT('Ctrl Pts',(-0.207663052093727,1.85354660091356,
8.86734744811972));
#63303=CARTESIAN_POINT('Ctrl Pts',(-0.206243786767565,1.85236144998933,
8.86746301827893));
#63304=CARTESIAN_POINT('Ctrl Pts',(-0.205921789298037,1.85209363112531,
8.8674891508703));
#63305=CARTESIAN_POINT('Ctrl Pts',(-0.205427995137265,1.85168454758796,
8.8675290910772));
#63306=CARTESIAN_POINT('Ctrl Pts',(-0.205256574328739,1.8515428330914,8.86754293150418));
#63307=CARTESIAN_POINT('Ctrl Pts',(-0.204918493577907,1.85126392860915,
8.86757017884476));
#63308=CARTESIAN_POINT('Ctrl Pts',(-0.20475184347794,1.85112672941004,8.86758358637682));
#63309=CARTESIAN_POINT('Ctrl Pts',(-0.204380148803442,1.8508213477693,8.86761343815956));
#63310=CARTESIAN_POINT('Ctrl Pts',(-0.204175034968636,1.85065325137634,
8.86762987608733));
#63311=CARTESIAN_POINT('Ctrl Pts',(-0.203581311731131,1.85016790277527,
8.86767735615302));
#63312=CARTESIAN_POINT('Ctrl Pts',(-0.203192166538295,1.84985130271099,
8.867708350976));
#63313=CARTESIAN_POINT('Ctrl Pts',(-0.200538069222985,1.84770226672015,
8.86791890794821));
#63314=CARTESIAN_POINT('Ctrl Pts',(-0.198249005885499,1.84589963297107,
8.86809636279078));
#63315=CARTESIAN_POINT('Ctrl Pts',(-0.19098816397572,1.84033958947094,8.86864749567428));
#63316=CARTESIAN_POINT('Ctrl Pts',(-0.185931422846102,1.83669499787208,
8.86901439166271));
#63317=CARTESIAN_POINT('Ctrl Pts',(-0.168350578715503,1.82478303779293,
8.87024519320756));
#63318=CARTESIAN_POINT('Ctrl Pts',(-0.155355905336822,1.81724410504196,
8.87108090119991));
#63319=CARTESIAN_POINT('Ctrl Pts',(-0.118521572621929,1.79918319523656,
8.8733740149801));
#63320=CARTESIAN_POINT('Ctrl Pts',(-0.0938636196441517,1.79060143293861,
8.87483698948597));
#63321=CARTESIAN_POINT('Ctrl Pts',(-0.0669083229615542,1.78474308615827,
8.87650932755639));
#63322=CARTESIAN_POINT('Ctrl Pts',(-0.0653702207950793,1.78442056546173,
8.87660495715832));
#63323=CARTESIAN_POINT('Ctrl Pts',(-0.0632859993804361,1.78399942128491,
8.87673483624149));
#63324=CARTESIAN_POINT('Ctrl Pts',(-0.0627418764662671,1.78389093591408,
8.87676877061321));
#63325=CARTESIAN_POINT('Ctrl Pts',(-0.061821358498288,1.78370987654059,
8.87682622581015));
#63326=CARTESIAN_POINT('Ctrl Pts',(-0.0614451078126426,1.78363656771305,
8.87684972315053));
#63327=CARTESIAN_POINT('Ctrl Pts',(-0.0607217814529869,1.78349697357264,
8.87689492155951));
#63328=CARTESIAN_POINT('Ctrl Pts',(-0.0603747255848012,1.78343058740698,
8.87691661937788));
#63329=CARTESIAN_POINT('Ctrl Pts',(-0.0595579664270996,1.78327574657764,
8.87696770998058));
#63330=CARTESIAN_POINT('Ctrl Pts',(-0.0590881750887718,1.78318776596906,
8.87699711782385));
#63331=CARTESIAN_POINT('Ctrl Pts',(-0.0577254124541961,1.7829356899484,
8.87708248559026));
#63332=CARTESIAN_POINT('Ctrl Pts',(-0.0568319466828875,1.78277432361056,
8.87713853225449));
#63333=CARTESIAN_POINT('Ctrl Pts',(-0.050598047280674,1.78167561812943,
8.87753013364932));
#63334=CARTESIAN_POINT('Ctrl Pts',(-0.0452356590802402,1.78086945640211,
8.87786983233231));
#63335=CARTESIAN_POINT('Ctrl Pts',(-0.0286035072074248,1.77879664658106,
8.87893308587018));
#63336=CARTESIAN_POINT('Ctrl Pts',(-0.0172862883562451,1.77798929953014,
8.87967049463249));
#63337=CARTESIAN_POINT('Ctrl Pts',(0.0248631475781336,1.7772108452284,8.88246349016681));
#63338=CARTESIAN_POINT('Ctrl Pts',(0.0555967588339537,1.78106448826708,
8.88460965130779));
#63339=CARTESIAN_POINT('Ctrl Pts',(0.0887021012420303,1.79015252929423,
8.8868151246211));
#63340=CARTESIAN_POINT('Ctrl Pts',(0.0920746595262546,1.79113793136097,
8.88703828513017));
#63341=CARTESIAN_POINT('Ctrl Pts',(0.0959763346076498,1.79234752515739,
8.88729414340403));
#63342=CARTESIAN_POINT('Ctrl Pts',(0.096521627993712,1.79251816732877,8.88732984892155));
#63343=CARTESIAN_POINT('Ctrl Pts',(0.0973330608546645,1.79277446549635,
8.88738289918576));
#63344=CARTESIAN_POINT('Ctrl Pts',(0.0975995436049225,1.79285901791535,
8.88740030824783));
#63345=CARTESIAN_POINT('Ctrl Pts',(0.0980745526824929,1.79301041435947,
8.88743131619295));
#63346=CARTESIAN_POINT('Ctrl Pts',(0.09828312074374,1.7930771240954,8.88744492297298));
#63347=CARTESIAN_POINT('Ctrl Pts',(0.0987263746579838,1.79321939540149,
8.8874738227648));
#63348=CARTESIAN_POINT('Ctrl Pts',(0.0989610411599483,1.79329501349921,
8.88748911233976));
#63349=CARTESIAN_POINT('Ctrl Pts',(0.0995918534760068,1.79349908356311,
8.88753018495524));
#63350=CARTESIAN_POINT('Ctrl Pts',(0.0999878391649064,1.7936280347695,8.88755593851882));
#63351=CARTESIAN_POINT('Ctrl Pts',(0.101898567340829,1.79425435504504,8.8876800690918));
#63352=CARTESIAN_POINT('Ctrl Pts',(0.103409888985203,1.79476220328917,8.88777783701345));
#63353=CARTESIAN_POINT('Ctrl Pts',(0.116078997629744,1.79912429186519,8.88859439840179));
#63354=CARTESIAN_POINT('Ctrl Pts',(0.12702238586571,1.80357816318646,8.88928018287624));
#63355=CARTESIAN_POINT('Ctrl Pts',(0.166147476990419,1.82206775399998,8.8917434812219));
#63356=CARTESIAN_POINT('Ctrl Pts',(0.192473461255659,1.83960536062014,8.89344198000537));
#63357=CARTESIAN_POINT('Ctrl Pts',(0.216998486171563,1.86172440113803,8.8953941844975));
#63358=CARTESIAN_POINT('Ctrl Pts',(0.218148091113861,1.86277644670589,8.89548661571909));
#63359=CARTESIAN_POINT('Ctrl Pts',(0.222861208161219,1.86715282441087,8.89586947834959));
#63360=CARTESIAN_POINT('Ctrl Pts',(0.226356575607455,1.87054930365324,8.89616277370531));
#63361=CARTESIAN_POINT('Ctrl Pts',(0.230369594465517,1.87462975266717,8.89651133297455));
#63362=CARTESIAN_POINT('Ctrl Pts',(0.230963330217309,1.87523826279754,8.89656321631688));
#63363=CARTESIAN_POINT('Ctrl Pts',(0.231911188212521,1.87621742876866,8.89664655198655));
#63364=CARTESIAN_POINT('Ctrl Pts',(0.232266848745611,1.87658659535731,8.89667793723287));
#63365=CARTESIAN_POINT('Ctrl Pts',(0.232895569621621,1.87724231561999,8.89673362479218));
#63366=CARTESIAN_POINT('Ctrl Pts',(0.233168986314741,1.87752852740528,8.89675791158907));
#63367=CARTESIAN_POINT('Ctrl Pts',(0.233729849183261,1.87811780670513,8.8968078749422));
#63368=CARTESIAN_POINT('Ctrl Pts',(0.234017234707306,1.87842093068635,8.89683355404813));
#63369=CARTESIAN_POINT('Ctrl Pts',(0.23471540153008,1.87916020539984,8.89689612885302));
#63370=CARTESIAN_POINT('Ctrl Pts',(0.235125556269604,1.87959694336141,8.89693305138742));
#63371=CARTESIAN_POINT('Ctrl Pts',(0.236029585552976,1.88056496054974,8.89701479239995));
#63372=CARTESIAN_POINT('Ctrl Pts',(0.236522888009921,1.8810967674325,8.89705963510838));
#63373=CARTESIAN_POINT('Ctrl Pts',(0.237919617337709,1.88261275084432,8.89718728670297));
#63374=CARTESIAN_POINT('Ctrl Pts',(0.238818717719707,1.88360087710475,8.89727027863465));
#63375=CARTESIAN_POINT('Ctrl Pts',(0.247174704874004,1.89289974765042,8.8980493630745));
#63376=CARTESIAN_POINT('Ctrl Pts',(0.254200282124472,1.9015862480755,8.89876329669453));
#63377=CARTESIAN_POINT('Ctrl Pts',(0.279222252804439,1.93603921425327,8.90154646187504));
#63378=CARTESIAN_POINT('Ctrl Pts',(0.293864757746272,1.96401740517007,8.90372971502152));
#63379=CARTESIAN_POINT('Ctrl Pts',(0.304591832199293,1.99470894525708,8.90585942279916));
#63380=CARTESIAN_POINT('Ctrl Pts',(0.304950154036124,1.99575128747471,8.90593142749199));
#63381=CARTESIAN_POINT('Ctrl Pts',(0.307139853746894,2.00222893045918,8.90637681035773));
#63382=CARTESIAN_POINT('Ctrl Pts',(0.308831351091482,2.00771089703728,8.90674463577063));
#63383=CARTESIAN_POINT('Ctrl Pts',(0.310552385674948,2.01386741670208,8.90714545396255));
#63384=CARTESIAN_POINT('Ctrl Pts',(0.310727108467706,2.0144998816654,8.90718648731425));
#63385=CARTESIAN_POINT('Ctrl Pts',(0.310976975400687,2.01541523742082,8.90724566300259));
#63386=CARTESIAN_POINT('Ctrl Pts',(0.311053666235849,2.01569769865062,8.90726389445221));
#63387=CARTESIAN_POINT('Ctrl Pts',(0.311187718825959,2.01619410320164,8.90729588339691));
#63388=CARTESIAN_POINT('Ctrl Pts',(0.311245244918827,2.01640800156178,8.90730965050072));
#63389=CARTESIAN_POINT('Ctrl Pts',(0.311364014517086,2.01685144301477,8.9073381566845));
#63390=CARTESIAN_POINT('Ctrl Pts',(0.311425224624566,2.01708099413683,8.90735289378404));
#63391=CARTESIAN_POINT('Ctrl Pts',(0.311582741691439,2.01767435190335,8.9073909376204));
#63392=CARTESIAN_POINT('Ctrl Pts',(0.311678665675963,2.01803826124121,8.90741422202649));
#63393=CARTESIAN_POINT('Ctrl Pts',(0.312078701058168,2.01956674394809,8.90751182208519));
#63394=CARTESIAN_POINT('Ctrl Pts',(0.312376929627991,2.02073286761323,8.90758580056656));
#63395=CARTESIAN_POINT('Ctrl Pts',(0.314432149371889,2.02896088461722,8.90810455857716));
#63396=CARTESIAN_POINT('Ctrl Pts',(0.315956190123305,2.03607944859552,8.90853667440967));
#63397=CARTESIAN_POINT('Ctrl Pts',(0.318670169255978,2.05124927929915,8.90943408763561));
#63398=CARTESIAN_POINT('Ctrl Pts',(0.319798908404867,2.05930624162602,8.90989702052615));
#63399=CARTESIAN_POINT('Ctrl Pts',(0.321941336036895,2.08037555605419,8.91109105610421));
#63400=CARTESIAN_POINT('Ctrl Pts',(0.322471822641228,2.09342168576267,8.91181450003036));
#63401=CARTESIAN_POINT('Ctrl Pts',(0.321786860081639,2.12756400069777,8.91373333809356));
#63402=CARTESIAN_POINT('Ctrl Pts',(0.319292234244214,2.14856774392116,8.914942662245));
#63403=CARTESIAN_POINT('Ctrl Pts',(0.314484286871246,2.17044500721736,8.91630310348402));
#63404=CARTESIAN_POINT('Ctrl Pts',(0.31419756013777,2.17171303129051,8.91638230479323));
#63405=CARTESIAN_POINT('Ctrl Pts',(0.313787238746545,2.17347793225166,8.91649303958141));
#63406=CARTESIAN_POINT('Ctrl Pts',(0.313670117674537,2.17397631378644,8.91652436494148));
#63407=CARTESIAN_POINT('Ctrl Pts',(0.313465915068896,2.17483604661298,8.91657849940072));
#63408=CARTESIAN_POINT('Ctrl Pts',(0.313379394776107,2.17519753127945,8.9166012904002));
#63409=CARTESIAN_POINT('Ctrl Pts',(0.313201102241993,2.17593679158553,8.91664796031189));
#63410=CARTESIAN_POINT('Ctrl Pts',(0.313109271429653,2.17631455237787,8.91667184108002));
#63411=CARTESIAN_POINT('Ctrl Pts',(0.312894393844351,2.17719156899034,8.9167273591163));
#63412=CARTESIAN_POINT('Ctrl Pts',(0.312770835552658,2.1776906972888,8.9167590128429));
#63413=CARTESIAN_POINT('Ctrl Pts',(0.312508225395731,2.17874076168891,8.91682572730963));
#63414=CARTESIAN_POINT('Ctrl Pts',(0.312368910060966,2.17929162952068,8.91686079648195));
#63415=CARTESIAN_POINT('Ctrl Pts',(0.311993661246145,2.1807590659377,8.91695440539228));
#63416=CARTESIAN_POINT('Ctrl Pts',(0.311755147069329,2.18167496332411,8.91701302851905));
#63417=CARTESIAN_POINT('Ctrl Pts',(0.311019757524381,2.18444870950738,8.91719117105373));
#63418=CARTESIAN_POINT('Ctrl Pts',(0.310510290512103,2.18630314789058,8.91731109734575));
#63419=CARTESIAN_POINT('Ctrl Pts',(0.301707762110398,2.21725670480012,8.91932696347975));
#63420=CARTESIAN_POINT('Ctrl Pts',(0.289375299231291,2.24504416850141,8.92136748264914));
#63421=CARTESIAN_POINT('Ctrl Pts',(0.265490327263784,2.28329375984226,8.9244152083093));
#63422=CARTESIAN_POINT('Ctrl Pts',(0.256762393972877,2.29533273655835,8.92541211550288));
#63423=CARTESIAN_POINT('Ctrl Pts',(0.245089131575015,2.30929328050275,8.92657983209037));
#63424=CARTESIAN_POINT('Ctrl Pts',(0.242904001756527,2.31182541816605,8.92679210179912));
#63425=CARTESIAN_POINT('Ctrl Pts',(0.240305419965702,2.31474356238312,8.92703682078126));
#63426=CARTESIAN_POINT('Ctrl Pts',(0.239929988045259,2.3151629459221,8.92707199295912));
#63427=CARTESIAN_POINT('Ctrl Pts',(0.239367579638569,2.31578789274175,8.92712440534689));
#63428=CARTESIAN_POINT('Ctrl Pts',(0.239181435446284,2.3159941984758,8.92714170764004));
#63429=CARTESIAN_POINT('Ctrl Pts',(0.238848242056302,2.31636252162515,8.92717259757277));
#63430=CARTESIAN_POINT('Ctrl Pts',(0.238701294854324,2.31652462985372,8.92718619287522));
#63431=CARTESIAN_POINT('Ctrl Pts',(0.238387705128317,2.3168698664483,8.9272151459766));
#63432=CARTESIAN_POINT('Ctrl Pts',(0.238221017112637,2.31705295191832,8.92723050017975));
#63433=CARTESIAN_POINT('Ctrl Pts',(0.237770234739882,2.31754693392924,8.92727192740529));
#63434=CARTESIAN_POINT('Ctrl Pts',(0.237485740450284,2.31785746734467,8.9272979700624));
#63435=CARTESIAN_POINT('Ctrl Pts',(0.236085516971168,2.3193798480159,8.92742564934313));
#63436=CARTESIAN_POINT('Ctrl Pts',(0.234961090739875,2.32058371460265,8.92752663397393));
#63437=CARTESIAN_POINT('Ctrl Pts',(0.228475385859191,2.32742176645885,8.92810070933279));
#63438=CARTESIAN_POINT('Ctrl Pts',(0.22292031983579,2.33286952202615,8.92855994614469));
#63439=CARTESIAN_POINT('Ctrl Pts',(0.204768037342205,2.34942558660646,8.92998287038919));
#63440=CARTESIAN_POINT('Ctrl Pts',(0.191496963064975,2.3597538479926,8.93091339431608));
#63441=CARTESIAN_POINT('Ctrl Pts',(0.169365888073198,2.37435540297082,8.93239684847875));
#63442=CARTESIAN_POINT('Ctrl Pts',(0.161013196783965,2.37933927476415,8.93294276876294));
#63443=CARTESIAN_POINT('Ctrl Pts',(0.13939703375399,2.3909451502094,8.93434359747116));
#63444=CARTESIAN_POINT('Ctrl Pts',(0.125879873193419,2.39704340017954,8.93520957022873));
#63445=CARTESIAN_POINT('Ctrl Pts',(0.110826028632106,2.40262239585278,8.93618502588585));
#63446=CARTESIAN_POINT('Ctrl Pts',(0.109657102572407,2.40304792175766,8.93626083108995));
#63447=CARTESIAN_POINT('Ctrl Pts',(0.108012704879563,2.40363577454573,8.93636756664988));
#63448=CARTESIAN_POINT('Ctrl Pts',(0.107539262275934,2.40380377723791,8.93639830825601));
#63449=CARTESIAN_POINT('Ctrl Pts',(0.10671719027324,2.40409332982125,8.93645170708666));
#63450=CARTESIAN_POINT('Ctrl Pts',(0.106368740282479,2.40421538920717,8.936474347361));
#63451=CARTESIAN_POINT('Ctrl Pts',(0.105650958820011,2.40446543861813,8.93652099780195));
#63452=CARTESIAN_POINT('Ctrl Pts',(0.10528160281724,2.40459335599886,8.93654501033346));
#63453=CARTESIAN_POINT('Ctrl Pts',(0.104416144219568,2.40489132405972,8.93660129259252));
#63454=CARTESIAN_POINT('Ctrl Pts',(0.103919858534033,2.40506083599448,8.93663358008765));
#63455=CARTESIAN_POINT('Ctrl Pts',(0.102872132782956,2.40541584506591,8.93670177202064));
#63456=CARTESIAN_POINT('Ctrl Pts',(0.102320600264549,2.40560106163925,8.93673768561277));
#63457=CARTESIAN_POINT('Ctrl Pts',(0.100839409636644,2.40609401833207,8.93683418114682));
#63458=CARTESIAN_POINT('Ctrl Pts',(0.099908850880177,2.4063990144833,8.93689485339801));
#63459=CARTESIAN_POINT('Ctrl Pts',(0.097060093387592,2.40731835414597,8.93708074836289));
#63460=CARTESIAN_POINT('Ctrl Pts',(0.0951375411472141,2.40791895117248,
8.9372064206804));
#63461=CARTESIAN_POINT('Ctrl Pts',(0.0881062408479981,2.4100433628044,8.93766688828996));
#63462=CARTESIAN_POINT('Ctrl Pts',(0.0829657499102364,2.41145830446664,
8.9380051759722));
#63463=CARTESIAN_POINT('Ctrl Pts',(0.0715603971888622,2.41429529248572,
8.93875964645394));
#63464=CARTESIAN_POINT('Ctrl Pts',(0.065283432379469,2.41565881293745,8.93917743793338));
#63465=CARTESIAN_POINT('Ctrl Pts',(0.0426728059678572,2.4198671829655,8.94069058204958));
#63466=CARTESIAN_POINT('Ctrl Pts',(0.0261668043160319,2.42163830251601,
8.94181195692942));
#63467=CARTESIAN_POINT('Ctrl Pts',(-0.00948715886695256,2.42270077233948,
8.94422528357856));
#63468=CARTESIAN_POINT('Ctrl Pts',(-0.028588996447638,2.42157215106553,
8.94551271211166));
#63469=CARTESIAN_POINT('Ctrl Pts',(-0.0486076322654278,2.418590289491,8.94678852344306));
#63470=CARTESIAN_POINT('Ctrl Pts',(-0.049733987095753,2.41841640204645,
8.94686005046168));
#63471=CARTESIAN_POINT('Ctrl Pts',(-0.0512375521396569,2.41817610770617,
8.94695516647691));
#63472=CARTESIAN_POINT('Ctrl Pts',(-0.0516155829978412,2.41811500099764,
8.94697904996131));
#63473=CARTESIAN_POINT('Ctrl Pts',(-0.0522058678254474,2.41801850463794,
8.9470162941752));
#63474=CARTESIAN_POINT('Ctrl Pts',(-0.0524181952141211,2.41798357620908,
8.94702968109365));
#63475=CARTESIAN_POINT('Ctrl Pts',(-0.05282491475024,2.41791625130544,8.94705530487045));
#63476=CARTESIAN_POINT('Ctrl Pts',(-0.0530193107610832,2.4178838894143,
8.94706754356569));
#63477=CARTESIAN_POINT('Ctrl Pts',(-0.0534786960207722,2.41780698057106,
8.94709644544344));
#63478=CARTESIAN_POINT('Ctrl Pts',(-0.0537436589901876,2.41776228056109,
8.94711309977187));
#63479=CARTESIAN_POINT('Ctrl Pts',(-0.0545195420548629,2.41763038865867,
8.94716182320525));
#63480=CARTESIAN_POINT('Ctrl Pts',(-0.0550303111361263,2.41754229502612,
8.94719384108015));
#63481=CARTESIAN_POINT('Ctrl Pts',(-0.0587908349926369,2.41688436208507,
8.94742916590621));
#63482=CARTESIAN_POINT('Ctrl Pts',(-0.0620320308223173,2.41626585402224,
8.94762975844531));
#63483=CARTESIAN_POINT('Ctrl Pts',(-0.0726883433434493,2.41406220580999,
8.94828357590692));
#63484=CARTESIAN_POINT('Ctrl Pts',(-0.080057468392593,2.41226508582347,
8.94872659776379));
#63485=CARTESIAN_POINT('Ctrl Pts',(-0.101767029822699,2.40615154332826,
8.9500226933532));
#63486=CARTESIAN_POINT('Ctrl Pts',(-0.115877658273491,2.40109418864508,
8.95085379849453));
#63487=CARTESIAN_POINT('Ctrl Pts',(-0.136913215012995,2.39185610721325,
8.95213904616455));
#63488=CARTESIAN_POINT('Ctrl Pts',(-0.14411772392343,2.38836659281184,8.95258795138594));
#63489=CARTESIAN_POINT('Ctrl Pts',(-0.166061897899345,2.37670996447366,
8.95399851793362));
#63490=CARTESIAN_POINT('Ctrl Pts',(-0.180294431458085,2.36765416603103,
8.95497789715423));
#63491=CARTESIAN_POINT('Ctrl Pts',(-0.194606628745201,2.35688631136057,
8.95606675364755));
#63492=CARTESIAN_POINT('Ctrl Pts',(-0.195457105451215,2.35623980331256,
8.95613186500964));
#63493=CARTESIAN_POINT('Ctrl Pts',(-0.196719028445348,2.35527058756554,
8.95622909274544));
#63494=CARTESIAN_POINT('Ctrl Pts',(-0.197132935212526,2.35495108330413,
8.95626108268312));
#63495=CARTESIAN_POINT('Ctrl Pts',(-0.197842023553578,2.35440096237444,
8.95631605856195));
#63496=CARTESIAN_POINT('Ctrl Pts',(-0.198137584889666,2.35417083505584,
8.95633902507114));
#63497=CARTESIAN_POINT('Ctrl Pts',(-0.198729996299828,2.35370791573786,
8.95638516213873));
#63498=CARTESIAN_POINT('Ctrl Pts',(-0.199026840188522,2.35347511676706,
8.95640833295378));
#63499=CARTESIAN_POINT('Ctrl Pts',(-0.199716152667372,2.35293256802114,
8.95646226160738));
#63500=CARTESIAN_POINT('Ctrl Pts',(-0.200108309752366,2.35262242569809,
8.95649303509207));
#63501=CARTESIAN_POINT('Ctrl Pts',(-0.201300525589124,2.35167502897891,
8.9565868756943));
#63502=CARTESIAN_POINT('Ctrl Pts',(-0.202098267919176,2.35103488179819,
8.95665005872169));
#63503=CARTESIAN_POINT('Ctrl Pts',(-0.203921648938973,2.34955738776692,
8.95679538395917));
#63504=CARTESIAN_POINT('Ctrl Pts',(-0.204945196540839,2.34871750044116,
8.95687762835488));
#63505=CARTESIAN_POINT('Ctrl Pts',(-0.208291380710295,2.34593705839446,
8.95714872155706));
#63506=CARTESIAN_POINT('Ctrl Pts',(-0.210591803545795,2.34397013596802,
8.95733864147238));
#63507=CARTESIAN_POINT('Ctrl Pts',(-0.21955526616318,2.33608490035683,8.95809300443898));
#63508=CARTESIAN_POINT('Ctrl Pts',(-0.225998811123837,2.3299241358665,8.95866737650572));
#63509=CARTESIAN_POINT('Ctrl Pts',(-0.256154937521758,2.29859773330147,
8.96151719372327));
#63510=CARTESIAN_POINT('Ctrl Pts',(-0.275963802860107,2.26999977396766,
8.96393974722564));
#63511=CARTESIAN_POINT('Ctrl Pts',(-0.292192277528338,2.23599464477283,
8.96635357884874));
#63512=CARTESIAN_POINT('Ctrl Pts',(-0.29349260337437,2.2331651755648,8.96655100239203));
#63513=CARTESIAN_POINT('Ctrl Pts',(-0.29497158628689,2.22982000772364,8.96678003229308));
#63514=CARTESIAN_POINT('Ctrl Pts',(-0.295190142031184,2.22932227642538,
8.966813997086));
#63515=CARTESIAN_POINT('Ctrl Pts',(-0.295518428274151,2.22856948031794,
8.96686519438217));
#63516=CARTESIAN_POINT('Ctrl Pts',(-0.295629088832514,2.22831482594112,
8.96688248347486));
#63517=CARTESIAN_POINT('Ctrl Pts',(-0.295826354172688,2.22785926507287,
8.96691335886861));
#63518=CARTESIAN_POINT('Ctrl Pts',(-0.295913083379698,2.22765841364295,
8.96692695280361));
#63519=CARTESIAN_POINT('Ctrl Pts',(-0.29609758450565,2.22722993926506,8.9669559127394));
#63520=CARTESIAN_POINT('Ctrl Pts',(-0.296195298223147,2.22700229252641,
8.96697127512441));
#63521=CARTESIAN_POINT('Ctrl Pts',(-0.296458652282342,2.22638679115667,
8.9670127472706));
#63522=CARTESIAN_POINT('Ctrl Pts',(-0.296623794655047,2.22599872198236,
8.96703882655314));
#63523=CARTESIAN_POINT('Ctrl Pts',(-0.297432870103816,2.22408706366514,
8.96716696299609));
#63524=CARTESIAN_POINT('Ctrl Pts',(-0.298065843703337,2.22255882130027,
8.96726836252298));
#63525=CARTESIAN_POINT('Ctrl Pts',(-0.30161367615232,2.21380290202484,8.96784378978326));
#63526=CARTESIAN_POINT('Ctrl Pts',(-0.304277623218085,2.20647562985073,
8.96830391459757));
#63527=CARTESIAN_POINT('Ctrl Pts',(-0.316996295114574,2.16710005743181,
8.97070014466733));
#63528=CARTESIAN_POINT('Ctrl Pts',(-0.322260308621024,2.13372621392319,
8.972489958609));
#63529=CARTESIAN_POINT('Ctrl Pts',(-0.322274969295649,2.10014067867101,
8.97445939472581));
#63530=CARTESIAN_POINT('',(-0.322274881362357,2.09972347173989,9.09972265507268));
#63531=CARTESIAN_POINT('Ctrl Pts',(-0.322274962187229,2.10015611604601,
8.97472265507268));
#63532=CARTESIAN_POINT('Ctrl Pts',(-0.322283729205766,2.0820581008871,8.9758346106162));
#63533=CARTESIAN_POINT('Ctrl Pts',(-0.320763654444053,2.06396370109893,
8.97694656615972));
#63534=CARTESIAN_POINT('Ctrl Pts',(-0.317742702268281,2.04614138156014,
8.97805852170324));
#63535=CARTESIAN_POINT('Ctrl Pts',(-0.314719940415267,2.02830838570335,
8.97917114335484));
#63536=CARTESIAN_POINT('Ctrl Pts',(-0.310194678618889,2.01074851592955,
8.98028376500643));
#63537=CARTESIAN_POINT('Ctrl Pts',(-0.304245854863578,1.99371907309714,
8.98139638665803));
#63538=CARTESIAN_POINT('Ctrl Pts',(-0.298280377608901,1.97664195700577,
8.98251212305041));
#63539=CARTESIAN_POINT('Ctrl Pts',(-0.290883676387714,1.96009891314594,
8.98362785944279));
#63540=CARTESIAN_POINT('Ctrl Pts',(-0.282182837315571,1.94432719585768,
8.98474359583517));
#63541=CARTESIAN_POINT('Ctrl Pts',(-0.277643074226491,1.93609812054632,
8.98532574416009));
#63542=CARTESIAN_POINT('Ctrl Pts',(-0.272749034639811,1.92807859711184,
8.98590789248501));
#63543=CARTESIAN_POINT('Ctrl Pts',(-0.26752335448613,1.92029905278634,8.98649004080994));
#63544=CARTESIAN_POINT('Ctrl Pts',(-0.257673757412418,1.90563581761505,
8.98758730016547));
#63545=CARTESIAN_POINT('Ctrl Pts',(-0.246584156538608,1.89173885726974,
8.98868455952099));
#63546=CARTESIAN_POINT('Ctrl Pts',(-0.234398341562797,1.87882451967361,
8.98978181887652));
#63547=CARTESIAN_POINT('Ctrl Pts',(-0.222235837736759,1.86593488687223,
8.9908769792032));
#63548=CARTESIAN_POINT('Ctrl Pts',(-0.208981760378368,1.85402474602817,
8.99197213952988));
#63549=CARTESIAN_POINT('Ctrl Pts',(-0.194820638675809,1.84327817706523,
8.99306729985656));
#63550=CARTESIAN_POINT('Ctrl Pts',(-0.180496633437845,1.83240799931036,
8.99417505689624));
#63551=CARTESIAN_POINT('Ctrl Pts',(-0.16524513381604,1.822728927404,8.99528281393592));
#63552=CARTESIAN_POINT('Ctrl Pts',(-0.149292342938792,1.81439017530056,
8.9963905709756));
#63553=CARTESIAN_POINT('Ctrl Pts',(-0.133528595180004,1.80615023874066,
8.99748520091753));
#63554=CARTESIAN_POINT('Ctrl Pts',(-0.117080824816662,1.79921931751597,
8.99857983085945));
#63555=CARTESIAN_POINT('Ctrl Pts',(-0.100191661963566,1.79369491271287,
8.99967446080138));
#63556=CARTESIAN_POINT('Ctrl Pts',(-0.0829986900103658,1.78807113267924,
9.00078878138994));
#63557=CARTESIAN_POINT('Ctrl Pts',(-0.0653490595285042,1.78390527915881,
9.00190310197849));
#63558=CARTESIAN_POINT('Ctrl Pts',(-0.0475129112710903,1.78124664882147,
9.00301742256705));
#63559=CARTESIAN_POINT('Ctrl Pts',(-0.0296767630136734,1.77858801848412,
9.0041317431556));
#63560=CARTESIAN_POINT('Ctrl Pts',(-0.0116549354123172,1.77743660794139,
9.00524606374416));
#63561=CARTESIAN_POINT('Ctrl Pts',(0.00628054822842578,1.77778620399035,
9.00636038433272));
#63562=CARTESIAN_POINT('Ctrl Pts',(0.0239414237635632,1.77813044741483,
9.00745764368825));
#63563=CARTESIAN_POINT('Ctrl Pts',(0.0416292381677865,1.77993210664495,
9.00855490304378));
#63564=CARTESIAN_POINT('Ctrl Pts',(0.0590842462719857,1.78318739376806,
9.00965216239931));
#63565=CARTESIAN_POINT('Ctrl Pts',(0.0765058633958602,1.78643645361087,
9.01074732272599));
#63566=CARTESIAN_POINT('Ctrl Pts',(0.0936947946213764,1.79113354471842,
9.01184248305267));
#63567=CARTESIAN_POINT('Ctrl Pts',(0.110396373268946,1.79722315743429,9.01293764337936));
#63568=CARTESIAN_POINT('Ctrl Pts',(0.127290056202733,1.8033828138705,9.01404540041904));
#63569=CARTESIAN_POINT('Ctrl Pts',(0.143684305481806,1.81096709130857,9.01515315745872));
#63570=CARTESIAN_POINT('Ctrl Pts',(0.15933121150109,1.81986656631777,9.0162609144984));
#63571=CARTESIAN_POINT('Ctrl Pts',(0.174792699186319,1.82866058112748,9.01735554444033));
#63572=CARTESIAN_POINT('Ctrl Pts',(0.189523817135947,1.83873832804346,9.01845017438226));
#63573=CARTESIAN_POINT('Ctrl Pts',(0.203311244625655,1.84994857842082,9.01954480432419));
#63574=CARTESIAN_POINT('Ctrl Pts',(0.217346685943797,1.86136048332118,9.02065912491275));
#63575=CARTESIAN_POINT('Ctrl Pts',(0.230403474059228,1.87394555685329,9.0217734455013));
#63576=CARTESIAN_POINT('Ctrl Pts',(0.242293927378484,1.88750334501336,9.02288776608986));
#63577=CARTESIAN_POINT('Ctrl Pts',(0.254184380697738,1.90106113317343,9.02400208667842));
#63578=CARTESIAN_POINT('Ctrl Pts',(0.264908048211737,1.91559092915891,9.02511640726697));
#63579=CARTESIAN_POINT('Ctrl Pts',(0.274322902962821,1.93086064758593,9.02623072785553));
#63580=CARTESIAN_POINT('Ctrl Pts',(0.283593607966985,1.94589657312872,9.02732798721106));
#63581=CARTESIAN_POINT('Ctrl Pts',(0.291653474164235,1.96174407486439,9.02842524656658));
#63582=CARTESIAN_POINT('Ctrl Pts',(0.298365081745992,1.97818270393861,9.02952250592211));
#63583=CARTESIAN_POINT('Ctrl Pts',(0.30506385019554,1.99458988633938,9.03061766624879));
#63584=CARTESIAN_POINT('Ctrl Pts',(0.31041913095044,2.01158526775857,9.03171282657547));
#63585=CARTESIAN_POINT('Ctrl Pts',(0.314339741848481,2.02892467151233,9.03280798690215));
#63586=CARTESIAN_POINT('Ctrl Pts',(0.318305448253605,2.0464635159209,9.03391574394183));
#63587=CARTESIAN_POINT('Ctrl Pts',(0.320802955351907,2.06435360066012,9.03502350098151));
#63588=CARTESIAN_POINT('Ctrl Pts',(0.321790070374446,2.08232724601514,9.03613125802119));
#63589=CARTESIAN_POINT('Ctrl Pts',(0.322765487926393,2.10008790080355,9.03722588796312));
#63590=CARTESIAN_POINT('Ctrl Pts',(0.322266158204137,2.11792935502614,9.03832051790505));
#63591=CARTESIAN_POINT('Ctrl Pts',(0.320303762597408,2.13559038200052,9.03941514784697));
#63592=CARTESIAN_POINT('Ctrl Pts',(0.3183060666239,2.15356910267936,9.04052946843553));
#63593=CARTESIAN_POINT('Ctrl Pts',(0.314792186798191,2.17136001160134,9.04164378902408));
#63594=CARTESIAN_POINT('Ctrl Pts',(0.309829072997926,2.18869679334816,9.04275810961264));
#63595=CARTESIAN_POINT('Ctrl Pts',(0.304865959197661,2.20603357509497,9.0438724302012));
#63596=CARTESIAN_POINT('Ctrl Pts',(0.298453961575723,2.22291546784511,9.04498675078975));
#63597=CARTESIAN_POINT('Ctrl Pts',(0.290711339919773,2.23909742077785,9.04610107137831));
#63598=CARTESIAN_POINT('Ctrl Pts',(0.283087264644172,2.25503161370986,9.04719833073383));
#63599=CARTESIAN_POINT('Ctrl Pts',(0.274125352650181,2.27038703255115,9.04829559008936));
#63600=CARTESIAN_POINT('Ctrl Pts',(0.263936573456107,2.28492879931814,9.04939284944489));
#63601=CARTESIAN_POINT('Ctrl Pts',(0.253767285133859,2.29944274806035,9.05048800977157));
#63602=CARTESIAN_POINT('Ctrl Pts',(0.242376174381177,2.31314547105133,9.05158317009825));
#63603=CARTESIAN_POINT('Ctrl Pts',(0.229919190773728,2.32582812344558,9.05267833042493));
#63604=CARTESIAN_POINT('Ctrl Pts',(0.217318924905658,2.33865665377971,9.05378608746461));
#63605=CARTESIAN_POINT('Ctrl Pts',(0.203628567065381,2.35044082858695,9.05489384450429));
#63606=CARTESIAN_POINT('Ctrl Pts',(0.189050347441566,2.36100027156542,9.05600160154397));
#63607=CARTESIAN_POINT('Ctrl Pts',(0.174644882047434,2.37143458345898,9.0570962314859));
#63608=CARTESIAN_POINT('Ctrl Pts',(0.159373171695866,2.38067263963363,9.05819086142782));
#63609=CARTESIAN_POINT('Ctrl Pts',(0.143461183805843,2.38858285528774,9.05928549136975));
#63610=CARTESIAN_POINT('Ctrl Pts',(0.127262964634619,2.39663536310403,9.06039981195831));
#63611=CARTESIAN_POINT('Ctrl Pts',(0.110401923236308,2.40331137049352,9.06151413254687));
#63612=CARTESIAN_POINT('Ctrl Pts',(0.0931382235613252,2.40852300876408,
9.06262845313543));
#63613=CARTESIAN_POINT('Ctrl Pts',(0.0758745238863453,2.41373464703464,
9.06374277372398));
#63614=CARTESIAN_POINT('Ctrl Pts',(0.0582089960319397,2.41748179821334,
9.06485709431254));
#63615=CARTESIAN_POINT('Ctrl Pts',(0.0404116992755282,2.41973124680998,
9.0659714149011));
#63616=CARTESIAN_POINT('Ctrl Pts',(0.0228868948613931,2.42194625436058,
9.06706867425663));
#63617=CARTESIAN_POINT('Ctrl Pts',(0.00512453887649297,2.42272308397212,
9.06816593361216));
#63618=CARTESIAN_POINT('Ctrl Pts',(-0.0126178092598918,2.42202789710595,
9.06926319296769));
#63619=CARTESIAN_POINT('Ctrl Pts',(-0.0303262167418809,2.42133404011433,
9.07035835329437));
#63620=CARTESIAN_POINT('Ctrl Pts',(-0.0480139256462691,2.41917372179016,
9.07145351362105));
#63621=CARTESIAN_POINT('Ctrl Pts',(-0.0654209171645705,2.41556501584039,
9.07254867394773));
#63622=CARTESIAN_POINT('Ctrl Pts',(-0.0830281267431725,2.41191480196521,
9.07365643098741));
#63623=CARTESIAN_POINT('Ctrl Pts',(-0.100347309977487,2.40678269072537,
9.07476418802709));
#63624=CARTESIAN_POINT('Ctrl Pts',(-0.117117332388186,2.4002410799329,9.07587194506677));
#63625=CARTESIAN_POINT('Ctrl Pts',(-0.133688627356306,2.39377698827257,
9.0769665750087));
#63626=CARTESIAN_POINT('Ctrl Pts',(-0.149723003145249,2.38593698750682,
9.07806120495063));
#63627=CARTESIAN_POINT('Ctrl Pts',(-0.164987500651015,2.37683984585665,
9.07915583489255));
#63628=CARTESIAN_POINT('Ctrl Pts',(-0.180526582118754,2.36757906113889,
9.08027015548111));
#63629=CARTESIAN_POINT('Ctrl Pts',(-0.195267075030213,2.35701583907237,
9.08138447606966));
#63630=CARTESIAN_POINT('Ctrl Pts',(-0.20899426636859,2.34532136525394,9.08249879665822));
#63631=CARTESIAN_POINT('Ctrl Pts',(-0.222721457706969,2.3336268914355,9.08361311724678));
#63632=CARTESIAN_POINT('Ctrl Pts',(-0.235434798931871,2.32080179996489,
9.08472743783533));
#63633=CARTESIAN_POINT('Ctrl Pts',(-0.246960173897901,2.30705518137279,
9.08584175842389));
#63634=CARTESIAN_POINT('Ctrl Pts',(-0.258246551289241,2.29359362148927,
9.08693297174532));
#63635=CARTESIAN_POINT('Ctrl Pts',(-0.268466945430599,2.27916115582596,
9.08802418506674));
#63636=CARTESIAN_POINT('Ctrl Pts',(-0.277453675406663,2.26395314461252,
9.08911539838817));
#63637=CARTESIAN_POINT('Ctrl Pts',(-0.286422256699789,2.24877584594684,
9.09020440800651));
#63638=CARTESIAN_POINT('Ctrl Pts',(-0.294161666304057,2.23282674204478,
9.09129341762485));
#63639=CARTESIAN_POINT('Ctrl Pts',(-0.300546385562578,2.21633161973544,
9.09238242724319));
#63640=CARTESIAN_POINT('Ctrl Pts',(-0.306923858795906,2.19985521775928,
9.09347020094327));
#63641=CARTESIAN_POINT('Ctrl Pts',(-0.311949384609126,2.18283474338672,
9.09455797464335));
#63642=CARTESIAN_POINT('Ctrl Pts',(-0.315545106443843,2.16551687892707,
9.09564574834343));
#63643=CARTESIAN_POINT('Ctrl Pts',(-0.319141554491157,2.14819551685222,
9.09673374173652));
#63644=CARTESIAN_POINT('Ctrl Pts',(-0.32130745995202,2.13057740961706,9.09782173512961));
#63645=CARTESIAN_POINT('Ctrl Pts',(-0.322015914725242,2.11291999569138,
9.0989097285227));
#63646=CARTESIAN_POINT('Ctrl Pts',(-0.32219236239434,2.10852224209124,9.09918070403936));
#63647=CARTESIAN_POINT('Ctrl Pts',(-0.322278655583543,2.10412206985998,
9.09945167955602));
#63648=CARTESIAN_POINT('Ctrl Pts',(-0.322274881362357,2.09972347173989,
9.09972265507268));
#63649=CARTESIAN_POINT('',(-0.322274875432262,2.10028335511254,9.34963671698665));
#63650=CARTESIAN_POINT('Ctrl Pts',(-0.322274874243154,2.09971529566301,
9.09960026516195));
#63651=CARTESIAN_POINT('Ctrl Pts',(-0.322258472261694,2.08114885383066,
9.10084055535965));
#63652=CARTESIAN_POINT('Ctrl Pts',(-0.320637716279971,2.06261890227565,
9.10210934893191));
#63653=CARTESIAN_POINT('Ctrl Pts',(-0.315899320326289,2.0355998352095,9.10394542848056));
#63654=CARTESIAN_POINT('Ctrl Pts',(-0.314008279355452,2.02693435888201,
9.10453159358843));
#63655=CARTESIAN_POINT('Ctrl Pts',(-0.310779179419296,2.01460367167756,
9.10535210223544));
#63656=CARTESIAN_POINT('Ctrl Pts',(-0.309728444291832,2.0108679328407,9.10559884178897));
#63657=CARTESIAN_POINT('Ctrl Pts',(-0.308455099497607,2.00663556387459,
9.10587556140901));
#63658=CARTESIAN_POINT('Ctrl Pts',(-0.308298464016908,2.00611963232959,
9.10590924578666));
#63659=CARTESIAN_POINT('Ctrl Pts',(-0.308060557794192,2.00534302504051,
9.10595987415689));
#63660=CARTESIAN_POINT('Ctrl Pts',(-0.307980250360868,2.00508205877742,
9.10597687419959));
#63661=CARTESIAN_POINT('Ctrl Pts',(-0.307835121556776,2.004612572932,9.10600743432248));
#63662=CARTESIAN_POINT('Ctrl Pts',(-0.307770420056702,2.00440401762833,
9.10602100140136));
#63663=CARTESIAN_POINT('Ctrl Pts',(-0.307630941685702,2.00395603998124,
9.10605012551575));
#63664=CARTESIAN_POINT('Ctrl Pts',(-0.307556097483437,2.00371663985764,
9.10606567847678));
#63665=CARTESIAN_POINT('Ctrl Pts',(-0.307353812000797,2.00307224269368,
9.10610751355303));
#63666=CARTESIAN_POINT('Ctrl Pts',(-0.307225849199085,2.00266740794239,
9.10613376498207));
#63667=CARTESIAN_POINT('Ctrl Pts',(-0.306633619003731,2.00080657897697,
9.1062542926759));
#63668=CARTESIAN_POINT('Ctrl Pts',(-0.30615978903774,1.99935361471708,9.10634801533614));
#63669=CARTESIAN_POINT('Ctrl Pts',(-0.296460502603906,1.97031391943269,
9.10821445833314));
#63670=CARTESIAN_POINT('Ctrl Pts',(-0.283550760047593,1.94409326228964,
9.10978601547487));
#63671=CARTESIAN_POINT('Ctrl Pts',(-0.263185535209028,1.91385855220464,
9.11183830144321));
#63672=CARTESIAN_POINT('Ctrl Pts',(-0.2588694193366,1.90790137640211,9.11225533826638));
#63673=CARTESIAN_POINT('Ctrl Pts',(-0.247369166838068,1.89312073824048,
9.11333196654901));
#63674=CARTESIAN_POINT('Ctrl Pts',(-0.239915280582552,1.88452111563952,
9.11399901409463));
#63675=CARTESIAN_POINT('Ctrl Pts',(-0.230394595692527,1.87464469926597,
9.11482694699622));
#63676=CARTESIAN_POINT('Ctrl Pts',(-0.228747764730766,1.87297325934145,
9.11496933821882));
#63677=CARTESIAN_POINT('Ctrl Pts',(-0.226716233923845,1.8709559172089,9.11514406507556));
#63678=CARTESIAN_POINT('Ctrl Pts',(-0.226348732561406,1.87059273366087,
9.11517563646829));
#63679=CARTESIAN_POINT('Ctrl Pts',(-0.22570160793421,1.86995628096857,9.11523116672119));
#63680=CARTESIAN_POINT('Ctrl Pts',(-0.225422357098112,1.86968263329028,
9.11525510893262));
#63681=CARTESIAN_POINT('Ctrl Pts',(-0.224857883156401,1.86913149552027,
9.11530346448591));
#63682=CARTESIAN_POINT('Ctrl Pts',(-0.224572642723948,1.86885402422718,
9.11532787858507));
#63683=CARTESIAN_POINT('Ctrl Pts',(-0.224020788283589,1.86831918645996,
9.11537507249279));
#63684=CARTESIAN_POINT('Ctrl Pts',(-0.223754242699118,1.86806174998906,
9.11539784919771));
#63685=CARTESIAN_POINT('Ctrl Pts',(-0.223121509272482,1.86745274583675,
9.11545187510309));
#63686=CARTESIAN_POINT('Ctrl Pts',(-0.222754934429039,1.86710158329928,
9.11548314180942));
#63687=CARTESIAN_POINT('Ctrl Pts',(-0.221465036704191,1.86587174938988,
9.11559304743202));
#63688=CARTESIAN_POINT('Ctrl Pts',(-0.220537341401229,1.86499769961032,
9.11567188535008));
#63689=CARTESIAN_POINT('Ctrl Pts',(-0.207067371122049,1.85245665654059,
9.11681371582356));
#63690=CARTESIAN_POINT('Ctrl Pts',(-0.1936217585474,1.84180424973892,9.11791991247994));
#63691=CARTESIAN_POINT('Ctrl Pts',(-0.169364568862311,1.82555034123905,
9.11985990927497));
#63692=CARTESIAN_POINT('Ctrl Pts',(-0.158964284120615,1.81939832252074,
9.1206757329195));
#63693=CARTESIAN_POINT('Ctrl Pts',(-0.137489862973049,1.80827341274372,
9.122312408251));
#63694=CARTESIAN_POINT('Ctrl Pts',(-0.126429791880727,1.80331262613866,
9.12313196302028));
#63695=CARTESIAN_POINT('Ctrl Pts',(-0.109233677734899,1.79673634301453,
9.12434965175588));
#63696=CARTESIAN_POINT('Ctrl Pts',(-0.10328594037938,1.79465942357064,9.12476089698939));
#63697=CARTESIAN_POINT('Ctrl Pts',(-0.0944714051371783,1.79186851352077,
9.12535225067944));
#63698=CARTESIAN_POINT('Ctrl Pts',(-0.0916498562243471,1.79101753332767,
9.12553886560109));
#63699=CARTESIAN_POINT('Ctrl Pts',(-0.0883331904049763,1.79006665826838,
9.12575478217274));
#63700=CARTESIAN_POINT('Ctrl Pts',(-0.0878491407277201,1.78992910919337,
9.12578620857896));
#63701=CARTESIAN_POINT('Ctrl Pts',(-0.087109187900887,1.78972071369493,
9.12583411661762));
#63702=CARTESIAN_POINT('Ctrl Pts',(-0.086853518855257,1.7896490496383,9.12585064568728));
#63703=CARTESIAN_POINT('Ctrl Pts',(-0.0863898251143923,1.78951969411308,
9.12588057946306));
#63704=CARTESIAN_POINT('Ctrl Pts',(-0.0861818318575394,1.78946189592036,
9.12589399036292));
#63705=CARTESIAN_POINT('Ctrl Pts',(-0.0857596294837019,1.78934502909263,
9.12592118024344));
#63706=CARTESIAN_POINT('Ctrl Pts',(-0.0855454182802888,1.78928597326381,
9.12593495843733));
#63707=CARTESIAN_POINT('Ctrl Pts',(-0.0849282911958205,1.78911652423032,
9.12597460383864));
#63708=CARTESIAN_POINT('Ctrl Pts',(-0.0845252196139656,1.78900669234538,
9.12600043830105));
#63709=CARTESIAN_POINT('Ctrl Pts',(-0.0827503053433083,1.78852675634932,
9.12611394201476));
#63710=CARTESIAN_POINT('Ctrl Pts',(-0.0813762102549527,1.78816493602542,
9.12620113708507));
#63711=CARTESIAN_POINT('Ctrl Pts',(-0.0558778029100651,1.78163083717593,
9.1278074235099));
#63712=CARTESIAN_POINT('Ctrl Pts',(-0.0311162946684242,1.77826491360616,
9.12917691824217));
#63713=CARTESIAN_POINT('Ctrl Pts',(0.00506599152502737,1.77756748815989,
9.13120182978354));
#63714=CARTESIAN_POINT('Ctrl Pts',(0.0163459817285308,1.77794227393381,
9.13183571511754));
#63715=CARTESIAN_POINT('Ctrl Pts',(0.034974104765286,1.77954247645762,9.13290912731224));
#63716=CARTESIAN_POINT('Ctrl Pts',(0.0423410168123546,1.78043241763628,
9.13334051791606));
#63717=CARTESIAN_POINT('Ctrl Pts',(0.0558401505882859,1.7825381184018,9.13414878559052));
#63718=CARTESIAN_POINT('Ctrl Pts',(0.0619803548452364,1.78367959880508,
9.13452329825408));
#63719=CARTESIAN_POINT('Ctrl Pts',(0.069003608049313,1.78519757883599,9.13496091425843));
#63720=CARTESIAN_POINT('Ctrl Pts',(0.0699231029898691,1.78540053729659,
9.13501839052465));
#63721=CARTESIAN_POINT('Ctrl Pts',(0.0712244772589702,1.78569377443052,
9.13510000107385));
#63722=CARTESIAN_POINT('Ctrl Pts',(0.0716071076670508,1.78578072668603,
9.13512402856535));
#63723=CARTESIAN_POINT('Ctrl Pts',(0.0723782086693916,1.78595743998373,
9.13517251591159));
#63724=CARTESIAN_POINT('Ctrl Pts',(0.0727666733458124,1.78604722355164,
9.13519697645204));
#63725=CARTESIAN_POINT('Ctrl Pts',(0.073514746327156,1.78622158428419,9.13524414572068));
#63726=CARTESIAN_POINT('Ctrl Pts',(0.0738743780000734,1.78630605939864,
9.13526685113204));
#63727=CARTESIAN_POINT('Ctrl Pts',(0.0747235196489008,1.78650705839744,
9.13532053089127));
#63728=CARTESIAN_POINT('Ctrl Pts',(0.0752129024647078,1.78662411049731,
9.13535152221376));
#63729=CARTESIAN_POINT('Ctrl Pts',(0.0769157755237287,1.78703562763256,
9.13545955097957));
#63730=CARTESIAN_POINT('Ctrl Pts',(0.078127815138552,1.78733599611269,9.13553677857381));
#63731=CARTESIAN_POINT('Ctrl Pts',(0.0939937055300143,1.79136590626235,
9.13655219682045));
#63732=CARTESIAN_POINT('Ctrl Pts',(0.108366944324479,1.79611465005757,9.13752377269832));
#63733=CARTESIAN_POINT('Ctrl Pts',(0.144066310137117,1.81076483023157,9.14007182548812));
#63734=CARTESIAN_POINT('Ctrl Pts',(0.164741442780121,1.82202124665936,9.1416824549965));
#63735=CARTESIAN_POINT('Ctrl Pts',(0.192777070003411,1.84151931887298,9.14396311271342));
#63736=CARTESIAN_POINT('Ctrl Pts',(0.201238381091352,1.84805074723259,9.14466494535187));
#63737=CARTESIAN_POINT('Ctrl Pts',(0.210508180778111,1.85597180381185,9.14543599351815));
#63738=CARTESIAN_POINT('Ctrl Pts',(0.211649021090287,1.85696060649992,9.14553092269137));
#63739=CARTESIAN_POINT('Ctrl Pts',(0.213089782537022,1.85822719928189,9.14565080659364));
#63740=CARTESIAN_POINT('Ctrl Pts',(0.213396156618565,1.85849757157831,9.14567629948603));
#63741=CARTESIAN_POINT('Ctrl Pts',(0.213885252529585,1.85893085162249,9.14571699501363));
#63742=CARTESIAN_POINT('Ctrl Pts',(0.214068303124133,1.85909338500652,9.14573222554726));
#63743=CARTESIAN_POINT('Ctrl Pts',(0.214415005376566,1.8594019343462,9.14576107166391));
#63744=CARTESIAN_POINT('Ctrl Pts',(0.214578691806236,1.85954790757827,9.14577469019254));
#63745=CARTESIAN_POINT('Ctrl Pts',(0.214952945883327,1.85988234854823,9.14580582698294));
#63746=CARTESIAN_POINT('Ctrl Pts',(0.215163414415457,1.86007092593606,9.14582333681536));
#63747=CARTESIAN_POINT('Ctrl Pts',(0.215809973437433,1.86065177035025,9.14587712644387));
#63748=CARTESIAN_POINT('Ctrl Pts',(0.216245244357999,1.86104495406694,9.14591333746357));
#63749=CARTESIAN_POINT('Ctrl Pts',(0.219519015664243,1.8640184489747,9.14618570482448));
#63750=CARTESIAN_POINT('Ctrl Pts',(0.222312466094142,1.86664820283091,9.14641820268445));
#63751=CARTESIAN_POINT('Ctrl Pts',(0.234991758822656,1.87901890144542,9.14747767387963));
#63752=CARTESIAN_POINT('Ctrl Pts',(0.24428982087052,1.88934307640058,9.14826699627979));
#63753=CARTESIAN_POINT('Ctrl Pts',(0.271639667051752,1.92396693480952,9.15074664319979));
#63754=CARTESIAN_POINT('Ctrl Pts',(0.286949783059319,1.95021540284296,9.15240546797203));
#63755=CARTESIAN_POINT('Ctrl Pts',(0.299200252366479,1.98022885415913,9.15435153972689));
#63756=CARTESIAN_POINT('Ctrl Pts',(0.300002762336829,1.98225340502009,9.15448293652728));
#63757=CARTESIAN_POINT('Ctrl Pts',(0.301333525877102,1.98571256229793,9.15470772923827));
#63758=CARTESIAN_POINT('Ctrl Pts',(0.301872209853844,1.98714309490997,9.15480077490439));
#63759=CARTESIAN_POINT('Ctrl Pts',(0.302604440203599,1.98913036621863,9.15493016514653));
#63760=CARTESIAN_POINT('Ctrl Pts',(0.302806672871608,1.98968390061783,9.15496621968648));
#63761=CARTESIAN_POINT('Ctrl Pts',(0.303147268688875,1.99062414435107,9.15502748782927));
#63762=CARTESIAN_POINT('Ctrl Pts',(0.303286413463739,1.99101057061216,9.15505267534497));
#63763=CARTESIAN_POINT('Ctrl Pts',(0.303559496240895,1.99177353563899,9.1551024205723));
#63764=CARTESIAN_POINT('Ctrl Pts',(0.303693473300852,1.99215005972052,9.15512697693167));
#63765=CARTESIAN_POINT('Ctrl Pts',(0.30398629062281,1.99297785456089,9.1551809804028));
#63766=CARTESIAN_POINT('Ctrl Pts',(0.304144826895351,1.99342923116603,9.155210437548));
#63767=CARTESIAN_POINT('Ctrl Pts',(0.304690396410581,1.99499368260546,9.15531257166522));
#63768=CARTESIAN_POINT('Ctrl Pts',(0.305072325606169,1.99610851600007,9.15538541751101));
#63769=CARTESIAN_POINT('Ctrl Pts',(0.308818057608964,2.0072409058005,9.15611352218554));
#63770=CARTESIAN_POINT('Ctrl Pts',(0.311692990637474,2.01741501427231,9.15678482066411));
#63771=CARTESIAN_POINT('Ctrl Pts',(0.320231424730917,2.05451065713549,9.15925675265897));
#63772=CARTESIAN_POINT('Ctrl Pts',(0.322943658201463,2.08198781363458,9.16114487968192));
#63773=CARTESIAN_POINT('Ctrl Pts',(0.321774090001628,2.12177647121397,9.16380844989872));
#63774=CARTESIAN_POINT('Ctrl Pts',(0.320707237087258,2.13405474278516,9.16461825995984));
#63775=CARTESIAN_POINT('Ctrl Pts',(0.318831436977289,2.14699216036942,9.16543887969094));
#63776=CARTESIAN_POINT('Ctrl Pts',(0.318720207620647,2.14774073337185,9.16548624343311));
#63777=CARTESIAN_POINT('Ctrl Pts',(0.318559150032686,2.14879899518658,9.16555302784647));
#63778=CARTESIAN_POINT('Ctrl Pts',(0.318511506067473,2.14910900635726,9.16557257078445));
#63779=CARTESIAN_POINT('Ctrl Pts',(0.318429016241406,2.14964058365201,9.16560604429084));
#63780=CARTESIAN_POINT('Ctrl Pts',(0.318394391586701,2.14986218343634,9.16561998747565));
#63781=CARTESIAN_POINT('Ctrl Pts',(0.318327718604069,2.15028599316591,9.16564663257866));
#63782=CARTESIAN_POINT('Ctrl Pts',(0.318295708968677,2.1504882084556,9.1656593367039));
#63783=CARTESIAN_POINT('Ctrl Pts',(0.318219956239749,2.15096382774621,9.16568919592193));
#63784=CARTESIAN_POINT('Ctrl Pts',(0.318176053374253,2.15123720667924,9.16570634188262));
#63785=CARTESIAN_POINT('Ctrl Pts',(0.318045643331123,2.15204262610709,9.16575680845929));
#63786=CARTESIAN_POINT('Ctrl Pts',(0.317958153056366,2.15257450987804,9.16579007356293));
#63787=CARTESIAN_POINT('Ctrl Pts',(0.317192129240031,2.15715957875916,9.16607631710921));
#63788=CARTESIAN_POINT('Ctrl Pts',(0.3164374213785,2.16119988968931,9.16632507234972));
#63789=CARTESIAN_POINT('Ctrl Pts',(0.313685665327031,2.17451489372656,9.16713660437448));
#63790=CARTESIAN_POINT('Ctrl Pts',(0.311356320299432,2.1837164148254,9.1676841486425));
#63791=CARTESIAN_POINT('Ctrl Pts',(0.3029051775992,2.21182156622319,9.16935176870362));
#63792=CARTESIAN_POINT('Ctrl Pts',(0.29544033066617,2.23027148417016,9.17044205494023));
#63793=CARTESIAN_POINT('Ctrl Pts',(0.278694809583666,2.2626859020224,9.17251158505862));
#63794=CARTESIAN_POINT('Ctrl Pts',(0.269935118322576,2.27684008111278,9.17347644893916));
#63795=CARTESIAN_POINT('Ctrl Pts',(0.25950999006673,2.29109375160174,9.17454748352658));
#63796=CARTESIAN_POINT('Ctrl Pts',(0.258892082961262,2.29193005545316,9.17461070311868));
#63797=CARTESIAN_POINT('Ctrl Pts',(0.257768441672667,2.29343554393617,9.17472520379362));
#63798=CARTESIAN_POINT('Ctrl Pts',(0.257264119796638,2.29410577483576,9.17477642965546));
#63799=CARTESIAN_POINT('Ctrl Pts',(0.25647837765781,2.29514156461832,9.17485598881477));
#63800=CARTESIAN_POINT('Ctrl Pts',(0.256198776730041,2.29550850428091,9.17488425053767));
#63801=CARTESIAN_POINT('Ctrl Pts',(0.255704063766449,2.29615486674713,9.17493417014095));
#63802=CARTESIAN_POINT('Ctrl Pts',(0.255489278707218,2.29643453983288,9.17495581508745));
#63803=CARTESIAN_POINT('Ctrl Pts',(0.255037786703901,2.29702043747325,9.17500125543092));
#63804=CARTESIAN_POINT('Ctrl Pts',(0.254800986398235,2.29732658907866,9.17502505450536));
#63805=CARTESIAN_POINT('Ctrl Pts',(0.254140555110172,2.29817726874747,9.17509133671047));
#63806=CARTESIAN_POINT('Ctrl Pts',(0.253715728087504,2.29872086178636,9.17513386732795));
#63807=CARTESIAN_POINT('Ctrl Pts',(0.252013409770457,2.30088472863147,9.17530387418962));
#63808=CARTESIAN_POINT('Ctrl Pts',(0.250722138563106,2.30249405378318,9.17543190033613));
#63809=CARTESIAN_POINT('Ctrl Pts',(0.225741065353069,2.3330229474704,9.17789154864242));
#63810=CARTESIAN_POINT('Ctrl Pts',(0.197215876685887,2.35761022942843,9.18045858130194));
#63811=CARTESIAN_POINT('Ctrl Pts',(0.155819778857383,2.38230998972758,9.18367961993618));
#63812=CARTESIAN_POINT('Ctrl Pts',(0.146233287374389,2.38739278366106,9.18439249788832));
#63813=CARTESIAN_POINT('Ctrl Pts',(0.135028488436193,2.39262740921821,9.18517464453166));
#63814=CARTESIAN_POINT('Ctrl Pts',(0.133644607389639,2.39326202012556,9.18527038102681));
#63815=CARTESIAN_POINT('Ctrl Pts',(0.131882530920689,2.3940549976001,9.18539113833416));
#63816=CARTESIAN_POINT('Ctrl Pts',(0.131508489727078,2.39422246805738,9.18541670681925));
#63817=CARTESIAN_POINT('Ctrl Pts',(0.130910268484528,2.39448894255419,9.1854574946429));
#63818=CARTESIAN_POINT('Ctrl Pts',(0.130686294764353,2.39458840446138,9.1854727421011));
#63819=CARTESIAN_POINT('Ctrl Pts',(0.130261711679657,2.39477637315822,9.18550160166721));
#63820=CARTESIAN_POINT('Ctrl Pts',(0.130061127108632,2.3948649299553,9.18551521676232));
#63821=CARTESIAN_POINT('Ctrl Pts',(0.129602255386049,2.39506695953797,9.18554632054076));
#63822=CARTESIAN_POINT('Ctrl Pts',(0.129343909918394,2.39518029775141,9.18556380085897));
#63823=CARTESIAN_POINT('Ctrl Pts',(0.12855019057871,2.39552726665042,9.18561741132981));
#63824=CARTESIAN_POINT('Ctrl Pts',(0.128014326303372,2.39575978277213,9.18565347337094));
#63825=CARTESIAN_POINT('Ctrl Pts',(0.124003881406022,2.39748700784234,9.18592239976159));
#63826=CARTESIAN_POINT('Ctrl Pts',(0.120503679033797,2.39892197780236,9.18615170846144));
#63827=CARTESIAN_POINT('Ctrl Pts',(0.115912166306965,2.40071058474788,9.18644653887563));
#63828=CARTESIAN_POINT('Ctrl Pts',(0.114843269962672,2.40112042357502,9.18651475786318));
#63829=CARTESIAN_POINT('Ctrl Pts',(0.111695483025373,2.40230815645427,9.18671449541018));
#63830=CARTESIAN_POINT('Ctrl Pts',(0.109610678126212,2.40307029234126,9.18684530227731));
#63831=CARTESIAN_POINT('Ctrl Pts',(0.106453792041393,2.40418750869589,9.18704138283768));
#63832=CARTESIAN_POINT('Ctrl Pts',(0.105387484032473,2.40455857983375,9.18710727305348));
#63833=CARTESIAN_POINT('Ctrl Pts',(0.0755785433885693,2.41475667998751,
9.18894033688237));
#63834=CARTESIAN_POINT('Ctrl Pts',(0.0455907947716183,2.42047729148712,
9.19056806203115));
#63835=CARTESIAN_POINT('Ctrl Pts',(0.00435261472609193,2.42242999542373,
9.19294955545122));
#63836=CARTESIAN_POINT('Ctrl Pts',(-0.00655612161160735,2.42239265856827,
9.19359116068032));
#63837=CARTESIAN_POINT('Ctrl Pts',(-0.019419547863179,2.42169548033113,
9.19437034970359));
#63838=CARTESIAN_POINT('Ctrl Pts',(-0.0213968101145816,2.42157001904668,
9.19449074248126));
#63839=CARTESIAN_POINT('Ctrl Pts',(-0.0240249457020883,2.4213789122036,
9.19465163356744));
#63840=CARTESIAN_POINT('Ctrl Pts',(-0.0246769854787377,2.42132950316289,
9.19469162167063));
#63841=CARTESIAN_POINT('Ctrl Pts',(-0.0257496132859311,2.42124493952232,
9.19475752200417));
#63842=CARTESIAN_POINT('Ctrl Pts',(-0.0261702928103834,2.42121094241107,
9.19478339781715));
#63843=CARTESIAN_POINT('Ctrl Pts',(-0.0269870214463744,2.42114332358624,
9.19483369320375));
#63844=CARTESIAN_POINT('Ctrl Pts',(-0.0273830777037293,2.42110979534076,
9.19485810979491));
#63845=CARTESIAN_POINT('Ctrl Pts',(-0.0282998566475121,2.42103047672796,
9.19491469119259));
#63846=CARTESIAN_POINT('Ctrl Pts',(-0.0288205309150977,2.42098415204973,
9.19494687274844));
#63847=CARTESIAN_POINT('Ctrl Pts',(-0.0302219295388583,2.42085603152695,
9.19503361677299));
#63848=CARTESIAN_POINT('Ctrl Pts',(-0.0311024289517391,2.42077187669837,
9.19508825333711));
#63849=CARTESIAN_POINT('Ctrl Pts',(-0.0374699062007123,2.42013683352641,
9.19548435933184));
#63850=CARTESIAN_POINT('Ctrl Pts',(-0.0429420022529031,2.41944884476655,
9.19583012526517));
#63851=CARTESIAN_POINT('Ctrl Pts',(-0.079632879734054,2.4138760775783,9.198186634193));
#63852=CARTESIAN_POINT('Ctrl Pts',(-0.110000398399723,2.40456307509838,
9.20034825134858));
#63853=CARTESIAN_POINT('Ctrl Pts',(-0.146611337647609,2.38713520403494,
9.20307014969199));
#63854=CARTESIAN_POINT('Ctrl Pts',(-0.154540518051768,2.38294657077944,
9.20366555098833));
#63855=CARTESIAN_POINT('Ctrl Pts',(-0.166278561583133,2.37610501471716,
9.20454577493825));
#63856=CARTESIAN_POINT('Ctrl Pts',(-0.170221572836756,2.37369172581329,
9.20484122222881));
#63857=CARTESIAN_POINT('Ctrl Pts',(-0.174750431413928,2.37078411838863,
9.20517907187464));
#63858=CARTESIAN_POINT('Ctrl Pts',(-0.175387877025763,2.37037167875161,
9.20522658963348));
#63859=CARTESIAN_POINT('Ctrl Pts',(-0.176286943228662,2.36978544791447,
9.20529355297633));
#63860=CARTESIAN_POINT('Ctrl Pts',(-0.176549770130788,2.36961352512085,
9.20531312170985));
#63861=CARTESIAN_POINT('Ctrl Pts',(-0.176999929400635,2.36931812222151,
9.20534662586448));
#63862=CARTESIAN_POINT('Ctrl Pts',(-0.177187384547364,2.36919483041682,
9.20536057396056));
#63863=CARTESIAN_POINT('Ctrl Pts',(-0.177545574537902,2.36895870773709,
9.20538721874755));
#63864=CARTESIAN_POINT('Ctrl Pts',(-0.177716330449988,2.3688459101373,9.20539991766426));
#63865=CARTESIAN_POINT('Ctrl Pts',(-0.178117578729359,2.36858030502818,
9.20542975089488));
#63866=CARTESIAN_POINT('Ctrl Pts',(-0.178347982535267,2.36842736303955,
9.20544687611678));
#63867=CARTESIAN_POINT('Ctrl Pts',(-0.17902580915851,2.36797616390847,9.20549724149264));
#63868=CARTESIAN_POINT('Ctrl Pts',(-0.179472685500309,2.36767708145655,
9.2055304264486));
#63869=CARTESIAN_POINT('Ctrl Pts',(-0.183299289330032,2.36510214667537,
9.20581443808981));
#63870=CARTESIAN_POINT('Ctrl Pts',(-0.1866365124877,2.36276337949726,9.20606111391321));
#63871=CARTESIAN_POINT('Ctrl Pts',(-0.200885109389166,2.35236931701582,
9.20711408268274));
#63872=CARTESIAN_POINT('Ctrl Pts',(-0.211327327125846,2.34369230024236,
9.20788545526469));
#63873=CARTESIAN_POINT('Ctrl Pts',(-0.233930133501104,2.32236144585911,
9.20963225194391));
#63874=CARTESIAN_POINT('Ctrl Pts',(-0.245666306574055,2.30932266259556,
9.21059983675026));
#63875=CARTESIAN_POINT('Ctrl Pts',(-0.260673406462534,2.28963897554837,
9.21201086642339));
#63876=CARTESIAN_POINT('Ctrl Pts',(-0.264866489011503,2.28373703940968,
9.21242806451234));
#63877=CARTESIAN_POINT('Ctrl Pts',(-0.273055988707078,2.27134640569059,
9.21329791751021));
#63878=CARTESIAN_POINT('Ctrl Pts',(-0.277028051356033,2.2648472274589,9.21375101322573));
#63879=CARTESIAN_POINT('Ctrl Pts',(-0.281547667589517,2.25682672479033,
9.21430919151071));
#63880=CARTESIAN_POINT('Ctrl Pts',(-0.282319022907817,2.25543384411447,
9.21440608928429));
#63881=CARTESIAN_POINT('Ctrl Pts',(-0.283367011184956,2.2535078927868,9.21454003921946));
#63882=CARTESIAN_POINT('Ctrl Pts',(-0.283652531725253,2.25297966339973,
9.21457677430012));
#63883=CARTESIAN_POINT('Ctrl Pts',(-0.284130772403353,2.25208894875669,
9.21463871371018));
#63884=CARTESIAN_POINT('Ctrl Pts',(-0.284324279963388,2.25172688615163,
9.21466388999783));
#63885=CARTESIAN_POINT('Ctrl Pts',(-0.284704868607723,2.25101150039954,
9.21471363297264));
#63886=CARTESIAN_POINT('Ctrl Pts',(-0.284891985112615,2.25065819685023,
9.21473819834659));
#63887=CARTESIAN_POINT('Ctrl Pts',(-0.285301828758954,2.24988085783625,
9.21479224555848));
#63888=CARTESIAN_POINT('Ctrl Pts',(-0.285524268684286,2.24945667274259,
9.21482173749133));
#63889=CARTESIAN_POINT('Ctrl Pts',(-0.286271431098901,2.24802410457041,
9.21492133603052));
#63890=CARTESIAN_POINT('Ctrl Pts',(-0.286791759242231,2.24701345031991,
9.21499159737818));
#63891=CARTESIAN_POINT('Ctrl Pts',(-0.291672960867762,2.23740796174153,
9.21565937862092));
#63892=CARTESIAN_POINT('Ctrl Pts',(-0.295651150585205,2.22862515004463,
9.21627020420648));
#63893=CARTESIAN_POINT('Ctrl Pts',(-0.307746451678849,2.1983834054305,9.21837722942361));
#63894=CARTESIAN_POINT('Ctrl Pts',(-0.313964835083191,2.17624290408021,
9.21993178354173));
#63895=CARTESIAN_POINT('Ctrl Pts',(-0.320771365033645,2.13591432430947,
9.22269576647163));
#63896=CARTESIAN_POINT('Ctrl Pts',(-0.322275132160368,2.11797292193138,
9.22390021191208));
#63897=CARTESIAN_POINT('Ctrl Pts',(-0.322274995589501,2.09939897745547,
9.22506493325287));
#63898=CARTESIAN_POINT('Ctrl Pts',(-0.322273323115425,2.09880032001375,
9.22510238362959));
#63899=CARTESIAN_POINT('Ctrl Pts',(-0.322268353573463,2.09790975499496,
9.22515795787839));
#63900=CARTESIAN_POINT('Ctrl Pts',(-0.322266328030864,2.09761784587171,
9.22517615208023));
#63901=CARTESIAN_POINT('Ctrl Pts',(-0.32226217452405,2.09711728694944,9.22520731303542));
#63902=CARTESIAN_POINT('Ctrl Pts',(-0.322260240543767,2.09690863642755,
9.22522029068208));
#63903=CARTESIAN_POINT('Ctrl Pts',(-0.322255836046731,2.09647852146802,
9.22524701940766));
#63904=CARTESIAN_POINT('Ctrl Pts',(-0.322253339880275,2.09625705818156,
9.22526076893302));
#63905=CARTESIAN_POINT('Ctrl Pts',(-0.322246953047899,2.09573789786962,
9.22529297097684));
#63906=CARTESIAN_POINT('Ctrl Pts',(-0.322242878138978,2.09544020245614,
9.22531141309229));
#63907=CARTESIAN_POINT('Ctrl Pts',(-0.32222835038992,2.09447645366835,9.22537104343758));
#63908=CARTESIAN_POINT('Ctrl Pts',(-0.322216244926181,2.09381042138694,
9.2254121393879));
#63909=CARTESIAN_POINT('Ctrl Pts',(-0.321797515193333,2.07413073331827,
9.22662319427765));
#63910=CARTESIAN_POINT('Ctrl Pts',(-0.31971061374058,2.05518676054616,9.22770078146485));
#63911=CARTESIAN_POINT('Ctrl Pts',(-0.313474902300085,2.0241419544787,9.22947603343592));
#63912=CARTESIAN_POINT('Ctrl Pts',(-0.310258700092123,2.01190634070192,
9.23017811048497));
#63913=CARTESIAN_POINT('Ctrl Pts',(-0.300543368385666,1.98217746120095,
9.23194451258543));
#63914=CARTESIAN_POINT('Ctrl Pts',(-0.293229940625628,1.96500180125661,
9.2330210443297));
#63915=CARTESIAN_POINT('Ctrl Pts',(-0.283869100244403,1.94741831888985,
9.23423099464817));
#63916=CARTESIAN_POINT('Ctrl Pts',(-0.283256865453793,1.94628473211179,
9.23430948825398));
#63917=CARTESIAN_POINT('Ctrl Pts',(-0.282392824214243,1.94470760309457,
9.23441939069695));
#63918=CARTESIAN_POINT('Ctrl Pts',(-0.282146731438201,1.94426093091856,
9.23445059552838));
#63919=CARTESIAN_POINT('Ctrl Pts',(-0.281719695425607,1.94349017089206,
9.23450457781423));
#63920=CARTESIAN_POINT('Ctrl Pts',(-0.281539250083858,1.94316580711323,
9.23452733740783));
#63921=CARTESIAN_POINT('Ctrl Pts',(-0.281164377597431,1.94249467804651,
9.23457451562032));
#63922=CARTESIAN_POINT('Ctrl Pts',(-0.280969868441365,1.94214795947072,
9.23459893715711));
#63923=CARTESIAN_POINT('Ctrl Pts',(-0.280513368757434,1.94133775170132,
9.23465611875502));
#63924=CARTESIAN_POINT('Ctrl Pts',(-0.280250870814821,1.94087455109586,
9.23468889704213));
#63925=CARTESIAN_POINT('Ctrl Pts',(-0.279401386990875,1.93938418447322,
9.23479464539101));
#63926=CARTESIAN_POINT('Ctrl Pts',(-0.278809897653228,1.93835960851158,
9.23486777792404));
#63927=CARTESIAN_POINT('Ctrl Pts',(-0.269436192681703,1.92232703934681,
9.23601906333756));
#63928=CARTESIAN_POINT('Ctrl Pts',(-0.25946065184863,1.908053307656,9.23714183366535));
#63929=CARTESIAN_POINT('Ctrl Pts',(-0.230326005810092,1.87281209831388,
9.24018053548816));
#63930=CARTESIAN_POINT('Ctrl Pts',(-0.209466684786698,1.85344772086862,
9.24214545802994));
#63931=CARTESIAN_POINT('Ctrl Pts',(-0.185590656364188,1.83652677909995,
9.24404169192221));
#63932=CARTESIAN_POINT('Ctrl Pts',(-0.184834272856886,1.83599560329842,
9.24410142186924));
#63933=CARTESIAN_POINT('Ctrl Pts',(-0.18081665974169,1.83319993516573,9.24441683493926));
#63934=CARTESIAN_POINT('Ctrl Pts',(-0.177515896862501,1.83099247415949,
9.24466954884462));
#63935=CARTESIAN_POINT('Ctrl Pts',(-0.173676495061207,1.828526241167,9.24495544707642));
#63936=CARTESIAN_POINT('Ctrl Pts',(-0.173177101425418,1.82820739850611,
9.24499247981865));
#63937=CARTESIAN_POINT('Ctrl Pts',(-0.172437237377411,1.82773789226243,
9.24504711367425));
#63938=CARTESIAN_POINT('Ctrl Pts',(-0.172197446318721,1.82758616843696,
9.24506478481674));
#63939=CARTESIAN_POINT('Ctrl Pts',(-0.171771842888959,1.82731766140926,
9.24509608536871));
#63940=CARTESIAN_POINT('Ctrl Pts',(-0.171586111620487,1.82720075130444,
9.24510972324946));
#63941=CARTESIAN_POINT('Ctrl Pts',(-0.171193504358359,1.8269541809532,9.24513850604796));
#63942=CARTESIAN_POINT('Ctrl Pts',(-0.17098660097096,1.82682456639958,9.24515364789954));
#63943=CARTESIAN_POINT('Ctrl Pts',(-0.170435471189059,1.82648018279805,
9.24519391104559));
#63944=CARTESIAN_POINT('Ctrl Pts',(-0.170090984759505,1.82626582758185,
9.24521900484957));
#63945=CARTESIAN_POINT('Ctrl Pts',(-0.168488331055755,1.82527277662101,
9.24533541492642));
#63946=CARTESIAN_POINT('Ctrl Pts',(-0.167225189226694,1.82450208484835,
9.24542621008789));
#63947=CARTESIAN_POINT('Ctrl Pts',(-0.15711931551246,1.81843121450526,9.24614542535052));
#63948=CARTESIAN_POINT('Ctrl Pts',(-0.148031211999004,1.81354883950229,
9.24674858908856));
#63949=CARTESIAN_POINT('Ctrl Pts',(-0.116389496695447,1.79845908535726,
9.24875690034716));
#63950=CARTESIAN_POINT('Ctrl Pts',(-0.0929026318538538,1.79041536118521,
9.25010214219421));
#63951=CARTESIAN_POINT('Ctrl Pts',(-0.0683257705576937,1.78505090526437,
9.25154099103011));
#63952=CARTESIAN_POINT('Ctrl Pts',(-0.0679256660838118,1.78496437172494,
9.25156442123641));
#63953=CARTESIAN_POINT('Ctrl Pts',(-0.061523656446614,1.78359252501878,
9.25193943147789));
#63954=CARTESIAN_POINT('Ctrl Pts',(-0.0554866577776933,1.78247822843998,
9.25229460043902));
#63955=CARTESIAN_POINT('Ctrl Pts',(-0.0477416910453507,1.78127629969844,
9.25275431304524));
#63956=CARTESIAN_POINT('Ctrl Pts',(-0.0460596181757361,1.78102887650557,
9.25285439507981));
#63957=CARTESIAN_POINT('Ctrl Pts',(-0.0380615186182831,1.77991698628041,
9.25333155553501));
#63958=CARTESIAN_POINT('Ctrl Pts',(-0.0317230610866462,1.77922678774512,
9.25371352670742));
#63959=CARTESIAN_POINT('Ctrl Pts',(-0.0243446696689885,1.77864417276754,
9.25416401019866));
#63960=CARTESIAN_POINT('Ctrl Pts',(-0.0233203476112143,1.77856821565604,
9.25422667886042));
#63961=CARTESIAN_POINT('Ctrl Pts',(-0.0217944049762667,1.77846239406403,
9.25432023516853));
#63962=CARTESIAN_POINT('Ctrl Pts',(-0.021293042442949,1.77842880343801,
9.25435100579226));
#63963=CARTESIAN_POINT('Ctrl Pts',(-0.0203991847801133,1.7783710157292,
9.25440592290483));
#63964=CARTESIAN_POINT('Ctrl Pts',(-0.0200067192086265,1.77834636416311,
9.25443005507973));
#63965=CARTESIAN_POINT('Ctrl Pts',(-0.0191796630295581,1.77829593461542,
9.25448095165898));
#63966=CARTESIAN_POINT('Ctrl Pts',(-0.0187450636472245,1.77827031883149,
9.25450772110336));
#63967=CARTESIAN_POINT('Ctrl Pts',(-0.0175979326795973,1.77820503784865,
9.25457844457243));
#63968=CARTESIAN_POINT('Ctrl Pts',(-0.0168853218916665,1.7781668587729,
9.25462244512944));
#63969=CARTESIAN_POINT('Ctrl Pts',(-0.0136670870658746,1.77800515567262,
9.25482146104727));
#63970=CARTESIAN_POINT('Ctrl Pts',(-0.0111602539462873,1.77790852665464,
9.25497731715918));
#63971=CARTESIAN_POINT('Ctrl Pts',(-0.00016948184314906,1.77761333437575,
9.25566445474171));
#63972=CARTESIAN_POINT('Ctrl Pts',(0.00831861923177028,1.7777206648977,
9.25620520749217));
#63973=CARTESIAN_POINT('Ctrl Pts',(0.0310260047299391,1.778905432777,9.25767980904175));
#63974=CARTESIAN_POINT('Ctrl Pts',(0.0451936281512032,1.7805914925298,9.25863004311568));
#63975=CARTESIAN_POINT('Ctrl Pts',(0.0837792052296277,1.78780236500515,
9.26127765193915));
#63976=CARTESIAN_POINT('Ctrl Pts',(0.107740338692095,1.79524019021462,9.26299382321312));
#63977=CARTESIAN_POINT('Ctrl Pts',(0.131907595360206,1.80595306161003,9.264664710065));
#63978=CARTESIAN_POINT('Ctrl Pts',(0.133209530231184,1.80654057022214,9.26475450708809));
#63979=CARTESIAN_POINT('Ctrl Pts',(0.134887948594719,1.8073114416635,9.2648699489321));
#63980=CARTESIAN_POINT('Ctrl Pts',(0.135268014536934,1.80748689754962,9.26489606846483));
#63981=CARTESIAN_POINT('Ctrl Pts',(0.135849454124314,1.80775669231238,9.26493599302665));
#63982=CARTESIAN_POINT('Ctrl Pts',(0.136051071946451,1.80785049906427,9.26494983082696));
#63983=CARTESIAN_POINT('Ctrl Pts',(0.136448215969172,1.80803577859409,9.26497707569316));
#63984=CARTESIAN_POINT('Ctrl Pts',(0.13664374621373,1.80812723860632,9.26499048337205));
#63985=CARTESIAN_POINT('Ctrl Pts',(0.13707934540302,1.80833152544253,9.26502033930313));
#63986=CARTESIAN_POINT('Ctrl Pts',(0.137319366378446,1.80844445193851,9.26503678122364));
#63987=CARTESIAN_POINT('Ctrl Pts',(0.138013191676665,1.80877193384008,9.26508428410554));
#63988=CARTESIAN_POINT('Ctrl Pts',(0.138466637084566,1.80898725454274,9.26511529768147));
#63989=CARTESIAN_POINT('Ctrl Pts',(0.141503895057553,1.81043821699306,9.26532283186054));
#63990=CARTESIAN_POINT('Ctrl Pts',(0.144071744119346,1.81170724531417,9.26549731831639));
#63991=CARTESIAN_POINT('Ctrl Pts',(0.152078489829783,1.81579787629006,9.26603936614333));
#63992=CARTESIAN_POINT('Ctrl Pts',(0.157454315306971,1.81874057722857,9.26640035519251));
#63993=CARTESIAN_POINT('Ctrl Pts',(0.169999682119959,1.82608037282053,9.2672434206219));
#63994=CARTESIAN_POINT('Ctrl Pts',(0.177087536894045,1.83060832828774,9.26772029051195));
#63995=CARTESIAN_POINT('Ctrl Pts',(0.210408630096527,1.85377900994109,9.27000322078026));
#63996=CARTESIAN_POINT('Ctrl Pts',(0.233923402722349,1.87599943669894,9.27176448193724));
#63997=CARTESIAN_POINT('Ctrl Pts',(0.255014094907295,1.90293873792034,9.27383266479325));
#63998=CARTESIAN_POINT('Ctrl Pts',(0.256255225133291,1.90455540705853,9.27395645884159));
#63999=CARTESIAN_POINT('Ctrl Pts',(0.257893769093772,1.90673217869587,9.27412276002631));
#64000=CARTESIAN_POINT('Ctrl Pts',(0.258304866384437,1.90728196016027,9.2741647300531));
#64001=CARTESIAN_POINT('Ctrl Pts',(0.258944579696721,1.90814320563806,9.27423042857951));
#64002=CARTESIAN_POINT('Ctrl Pts',(0.259174399218538,1.90845377663665,9.27425411010876));
#64003=CARTESIAN_POINT('Ctrl Pts',(0.259612977163245,1.90904869169004,9.27429945494492));
#64004=CARTESIAN_POINT('Ctrl Pts',(0.259821828450057,1.9093329668869,9.27432111459966));
#64005=CARTESIAN_POINT('Ctrl Pts',(0.26030346127108,1.90999079593874,9.27437121813774));
#64006=CARTESIAN_POINT('Ctrl Pts',(0.260575905662381,1.9103645946496,9.27439967503089));
#64007=CARTESIAN_POINT('Ctrl Pts',(0.261342808765185,1.91142157292852,9.2744801044996));
#64008=CARTESIAN_POINT('Ctrl Pts',(0.261835389186077,1.91210610494704,9.27453214946206));
#64009=CARTESIAN_POINT('Ctrl Pts',(0.262933666079342,1.91364507039714,9.27464906316954));
#64010=CARTESIAN_POINT('Ctrl Pts',(0.263537893544775,1.91450053593183,9.27471398770104));
#64011=CARTESIAN_POINT('Ctrl Pts',(0.268324825427074,1.92134847207295,9.27523321509284));
#64012=CARTESIAN_POINT('Ctrl Pts',(0.272306476642403,1.92747826475906,9.27569509443316));
#64013=CARTESIAN_POINT('Ctrl Pts',(0.279091136079439,1.93874409255423,9.27653971044202));
#64014=CARTESIAN_POINT('Ctrl Pts',(0.281969262502211,1.94383131420171,9.2769196055743));
#64015=CARTESIAN_POINT('Ctrl Pts',(0.294778660739563,1.9679821666332,9.27871532824959));
#64016=CARTESIAN_POINT('Ctrl Pts',(0.302924371818978,1.98792935304771,9.28018121119283));
#64017=CARTESIAN_POINT('Ctrl Pts',(0.313265455631432,2.02286806746097,9.28263504820887));
#64018=CARTESIAN_POINT('Ctrl Pts',(0.316505846438503,2.03748000787696,9.28362822331295));
#64019=CARTESIAN_POINT('Ctrl Pts',(0.31885555975502,2.05316900972577,9.28462593138143));
#64020=CARTESIAN_POINT('Ctrl Pts',(0.318986988108309,2.05407276295913,9.28468316228142));
#64021=CARTESIAN_POINT('Ctrl Pts',(0.319158515719454,2.05528852051733,9.28475981570073));
#64022=CARTESIAN_POINT('Ctrl Pts',(0.319202000828369,2.05560003127266,9.28477942685575));
#64023=CARTESIAN_POINT('Ctrl Pts',(0.319274426982014,2.05612447065233,9.28481239258689));
#64024=CARTESIAN_POINT('Ctrl Pts',(0.319303611114518,2.05633736459992,9.2848257609291));
#64025=CARTESIAN_POINT('Ctrl Pts',(0.319359160928617,2.0567456265861,9.284851370135));
#64026=CARTESIAN_POINT('Ctrl Pts',(0.319385560086513,2.05694098820292,9.28486361279413));
#64027=CARTESIAN_POINT('Ctrl Pts',(0.319447597797777,2.05740328172236,9.28489255524443));
#64028=CARTESIAN_POINT('Ctrl Pts',(0.3194830809984,2.05767023383205,9.28490924610476));
#64029=CARTESIAN_POINT('Ctrl Pts',(0.31958624767971,2.05845391109278,9.28495818083918));
#64030=CARTESIAN_POINT('Ctrl Pts',(0.319653012868413,2.05897075941926,9.28499037280276));
#64031=CARTESIAN_POINT('Ctrl Pts',(0.320134106178299,2.06276750054387,9.28522627128089));
#64032=CARTESIAN_POINT('Ctrl Pts',(0.320499216787296,2.06605358546599,9.28542725350824));
#64033=CARTESIAN_POINT('Ctrl Pts',(0.321542105045374,2.07696767212112,9.28608594554629));
#64034=CARTESIAN_POINT('Ctrl Pts',(0.321998636700488,2.08461463118804,9.28653321635976));
#64035=CARTESIAN_POINT('Ctrl Pts',(0.32281194090703,2.11851775518767,9.28848131290178));
#64036=CARTESIAN_POINT('Ctrl Pts',(0.320232143351835,2.14474342978141,9.289903849634));
#64037=CARTESIAN_POINT('Ctrl Pts',(0.313498370728776,2.17483952120189,9.29167315690037));
#64038=CARTESIAN_POINT('Ctrl Pts',(0.312402362596835,2.17929025021266,9.29193816881204));
#64039=CARTESIAN_POINT('Ctrl Pts',(0.308875290159987,2.1924020465289,9.29273095220771));
#64040=CARTESIAN_POINT('Ctrl Pts',(0.306176306637433,2.20098578759863,9.29326585016435));
#64041=CARTESIAN_POINT('Ctrl Pts',(0.302737869754027,2.21050899426926,9.29388163263373));
#64042=CARTESIAN_POINT('Ctrl Pts',(0.302348062437887,2.21157107459621,9.29395062413024));
#64043=CARTESIAN_POINT('Ctrl Pts',(0.301771951168544,2.21311557149981,9.29405142182942));
#64044=CARTESIAN_POINT('Ctrl Pts',(0.30159006267522,2.21359963520379,9.29408308039754));
#64045=CARTESIAN_POINT('Ctrl Pts',(0.301266638796291,2.21445411838799,9.29413908496814));
#64046=CARTESIAN_POINT('Ctrl Pts',(0.301125582968606,2.21482471923403,9.2941634148633));
#64047=CARTESIAN_POINT('Ctrl Pts',(0.300832179275959,2.21559133,9.294213825944));
#64048=CARTESIAN_POINT('Ctrl Pts',(0.300679732678443,2.21598730108409,9.29423991040554));
#64049=CARTESIAN_POINT('Ctrl Pts',(0.300291471339335,2.21698987753377,9.29430607214552));
#64050=CARTESIAN_POINT('Ctrl Pts',(0.300054601022688,2.21759606966093,9.29434618485862));
#64051=CARTESIAN_POINT('Ctrl Pts',(0.299094119402971,2.22003231259936,9.29450783752528));
#64052=CARTESIAN_POINT('Ctrl Pts',(0.29835560073337,2.22185640551228,9.29462987915179));
#64053=CARTESIAN_POINT('Ctrl Pts',(0.296449994918476,2.22644193688992,9.29493927411264));
#64054=CARTESIAN_POINT('Ctrl Pts',(0.295261015388246,2.22919401962474,9.29512736259417));
#64055=CARTESIAN_POINT('Ctrl Pts',(0.290314085929752,2.24021937595996,9.29589079442097));
#64056=CARTESIAN_POINT('Ctrl Pts',(0.286245693683029,2.24834796629056,9.29647654477005));
#64057=CARTESIAN_POINT('Ctrl Pts',(0.273670845445757,2.2710238720236,9.29817669186159));
#64058=CARTESIAN_POINT('Ctrl Pts',(0.264360406265617,2.2850901847439,9.2993142090678));
#64059=CARTESIAN_POINT('Ctrl Pts',(0.244245175457211,2.31084676501312,9.30152571400347));
#64060=CARTESIAN_POINT('Ctrl Pts',(0.233587958237221,2.3225956243493,9.30259608444995));
#64061=CARTESIAN_POINT('Ctrl Pts',(0.221974953148232,2.33364145628118,9.30363371413978));
#64062=CARTESIAN_POINT('Ctrl Pts',(0.221840661888979,2.333768968538,9.3036456968559));
#64063=CARTESIAN_POINT('Ctrl Pts',(0.221528606161668,2.33406476068633,9.30367350341307));
#64064=CARTESIAN_POINT('Ctrl Pts',(0.221350759492087,2.33423295416334,9.30368932237285));
#64065=CARTESIAN_POINT('Ctrl Pts',(0.218048943265193,2.33734843510757,9.30398247804967));
#64066=CARTESIAN_POINT('Ctrl Pts',(0.214866364296733,2.34023336833978,9.30425623660791));
#64067=CARTESIAN_POINT('Ctrl Pts',(0.2112152517576,2.34341238863278,9.30455959725218));
#64068=CARTESIAN_POINT('Ctrl Pts',(0.210802711185122,2.34376974890723,9.30459372343867));
#64069=CARTESIAN_POINT('Ctrl Pts',(0.210178204231378,2.34430795263381,9.30464515417546));
#64070=CARTESIAN_POINT('Ctrl Pts',(0.209966910505311,2.34448956981505,9.3046625155429));
#64071=CARTESIAN_POINT('Ctrl Pts',(0.209599612816335,2.34480445263217,9.30469262628015));
#64072=CARTESIAN_POINT('Ctrl Pts',(0.20944371707812,2.34493784333649,9.30470538494806));
#64073=CARTESIAN_POINT('Ctrl Pts',(0.209117432923521,2.34521648599239,9.30473204320171));
#64074=CARTESIAN_POINT('Ctrl Pts',(0.20894702061857,2.34536170917635,9.30474594059635));
#64075=CARTESIAN_POINT('Ctrl Pts',(0.208539108955493,2.34570859312132,9.30477914533061));
#64076=CARTESIAN_POINT('Ctrl Pts',(0.208301467405451,2.34591008799214,9.30479844034362));
#64077=CARTESIAN_POINT('Ctrl Pts',(0.207494996909642,2.34659188172576,9.30486375485412));
#64078=CARTESIAN_POINT('Ctrl Pts',(0.206924790565097,2.34707055864894,9.30490965572031));
#64079=CARTESIAN_POINT('Ctrl Pts',(0.205564284719224,2.3482046627318,9.30501852679852));
#64080=CARTESIAN_POINT('Ctrl Pts',(0.204772496335225,2.34885830217888,9.30508137128727));
#64081=CARTESIAN_POINT('Ctrl Pts',(0.201911848269049,2.35119693548841,9.30530662675852));
#64082=CARTESIAN_POINT('Ctrl Pts',(0.199825143401271,2.35286005607218,9.30546758454704));
#64083=CARTESIAN_POINT('Ctrl Pts',(0.188523108315542,2.36164056856456,9.30632301050846));
#64084=CARTESIAN_POINT('Ctrl Pts',(0.178946949472971,2.36828117997872,9.30699046576959));
#64085=CARTESIAN_POINT('Ctrl Pts',(0.153545734144269,2.38392903426079,9.30867549964184));
#64086=CARTESIAN_POINT('Ctrl Pts',(0.137280313603271,2.39214057659763,9.30967751877737));
#64087=CARTESIAN_POINT('Ctrl Pts',(0.104939158971385,2.40516731135652,9.3116568457012));
#64088=CARTESIAN_POINT('Ctrl Pts',(0.0890112943534987,2.41018733778611,
9.31262622861209));
#64089=CARTESIAN_POINT('Ctrl Pts',(0.071531320563508,2.41423885390322,9.3137162631697));
#64090=CARTESIAN_POINT('Ctrl Pts',(0.0702929871033947,2.41451817597141,
9.31379361161546));
#64091=CARTESIAN_POINT('Ctrl Pts',(0.0685580627147062,2.4148987527181,9.31390216612746));
#64092=CARTESIAN_POINT('Ctrl Pts',(0.0680628229743746,2.41500616589321,
9.31393317475301));
#64093=CARTESIAN_POINT('Ctrl Pts',(0.0672052247278319,2.41519005464356,
9.31398690962972));
#64094=CARTESIAN_POINT('Ctrl Pts',(0.0668429829217559,2.4152670747306,9.31400961840719));
#64095=CARTESIAN_POINT('Ctrl Pts',(0.0660910884008059,2.41542558889517,
9.31405677884015));
#64096=CARTESIAN_POINT('Ctrl Pts',(0.0657014159944474,2.41550698570709,
9.31408123356577));
#64097=CARTESIAN_POINT('Ctrl Pts',(0.0649284619885563,2.41566695032384,
9.31412976937126));
#64098=CARTESIAN_POINT('Ctrl Pts',(0.0645451861255913,2.41574554256365,
9.31415384962059));
#64099=CARTESIAN_POINT('Ctrl Pts',(0.0633313427595625,2.41599214344634,
9.31423015514773));
#64100=CARTESIAN_POINT('Ctrl Pts',(0.0625002603399509,2.41615757326218,
9.31428246272126));
#64101=CARTESIAN_POINT('Ctrl Pts',(0.0569298591988327,2.41724355838911,
9.31463349473452));
#64102=CARTESIAN_POINT('Ctrl Pts',(0.052171237743816,2.41806075218673,9.31493549621284));
#64103=CARTESIAN_POINT('Ctrl Pts',(0.0378364111312539,2.42019211830719,
9.3158522360954));
#64104=CARTESIAN_POINT('Ctrl Pts',(0.0282183395614718,2.42118262937666,
9.31647681062151));
#64105=CARTESIAN_POINT('Ctrl Pts',(0.00680963320186511,2.4224183556767,
9.31788709111213));
#64106=CARTESIAN_POINT('Ctrl Pts',(-0.00497935150054212,2.42245176032486,
9.31867721899912));
#64107=CARTESIAN_POINT('Ctrl Pts',(-0.0361772342734136,2.42082876753904,
9.32078753453597));
#64108=CARTESIAN_POINT('Ctrl Pts',(-0.05548104489608,2.41805947824297,9.32211492148567));
#64109=CARTESIAN_POINT('Ctrl Pts',(-0.0745369065890626,2.41353698369352,
9.32338709907955));
#64110=CARTESIAN_POINT('Ctrl Pts',(-0.0746559061223345,2.41350867016502,
9.32339504190501));
#64111=CARTESIAN_POINT('Ctrl Pts',(-0.0755791648016716,2.41328844398702,
9.32345665353613));
#64112=CARTESIAN_POINT('Ctrl Pts',(-0.0763827067508067,2.41309350268692,
9.32351020056131));
#64113=CARTESIAN_POINT('Ctrl Pts',(-0.0809182204460799,2.41197467574403,
9.32381198128239));
#64114=CARTESIAN_POINT('Ctrl Pts',(-0.0846343706815731,2.41098711092148,
9.32405748337377));
#64115=CARTESIAN_POINT('Ctrl Pts',(-0.0892476148320064,2.4096723187868,
9.32435929202675));
#64116=CARTESIAN_POINT('Ctrl Pts',(-0.0901619332109386,2.40940734902357,
9.32441896255034));
#64117=CARTESIAN_POINT('Ctrl Pts',(-0.0914160792180088,2.40903786573837,
9.32450059703569));
#64118=CARTESIAN_POINT('Ctrl Pts',(-0.0917569162566877,2.40893683872547,
9.32452276094028));
#64119=CARTESIAN_POINT('Ctrl Pts',(-0.0922985492737435,2.40877531864463,
9.32455794679089));
#64120=CARTESIAN_POINT('Ctrl Pts',(-0.0924994533216363,2.40871519356512,
9.32457099027684));
#64121=CARTESIAN_POINT('Ctrl Pts',(-0.0928907080424122,2.40859768552311,
9.32459637678469));
#64122=CARTESIAN_POINT('Ctrl Pts',(-0.093081063727561,2.40854032269113,
9.32460872089945));
#64123=CARTESIAN_POINT('Ctrl Pts',(-0.0935409338230394,2.4084012785868,
9.32463852545799));
#64124=CARTESIAN_POINT('Ctrl Pts',(-0.0938103951527391,2.40831941991576,
9.3246559754266));
#64125=CARTESIAN_POINT('Ctrl Pts',(-0.0946360549059517,2.40806741314544,
9.32470940201458));
#64126=CARTESIAN_POINT('Ctrl Pts',(-0.0951919041861844,2.40789611124561,
9.32474531120143));
#64127=CARTESIAN_POINT('Ctrl Pts',(-0.0994105648733737,2.40658348613522,
9.3250174229573));
#64128=CARTESIAN_POINT('Ctrl Pts',(-0.103053390348468,2.40537828390361,
9.32524996335253));
#64129=CARTESIAN_POINT('Ctrl Pts',(-0.116655505600875,2.40060698203345,
9.32611212822289));
#64130=CARTESIAN_POINT('Ctrl Pts',(-0.126459525647403,2.39661607235071,
9.32672117577617));
#64131=CARTESIAN_POINT('Ctrl Pts',(-0.143342881597667,2.38875371715189,
9.32777668239566));
#64132=CARTESIAN_POINT('Ctrl Pts',(-0.150505935692425,2.38508570667653,
9.32822673572628));
#64133=CARTESIAN_POINT('Ctrl Pts',(-0.165369889900727,2.37675774494261,
9.32917918994205));
#64134=CARTESIAN_POINT('Ctrl Pts',(-0.17302788853198,2.37203565120332,9.3296811195897));
#64135=CARTESIAN_POINT('Ctrl Pts',(-0.196184954583837,2.35638264124531,
9.33125854023691));
#64136=CARTESIAN_POINT('Ctrl Pts',(-0.21092179052807,2.34440219363547,9.33235257380039));
#64137=CARTESIAN_POINT('Ctrl Pts',(-0.225445235354195,2.33029825732799,
9.33358223559826));
#64138=CARTESIAN_POINT('Ctrl Pts',(-0.226365735707659,2.32939353760302,
9.33366086982803));
#64139=CARTESIAN_POINT('Ctrl Pts',(-0.227642606261134,2.32812338749328,
9.33377093771352));
#64140=CARTESIAN_POINT('Ctrl Pts',(-0.228003589057303,2.32776259455633,
9.33380216654944));
#64141=CARTESIAN_POINT('Ctrl Pts',(-0.228625691729252,2.32713785804182,
9.33385617913084));
#64142=CARTESIAN_POINT('Ctrl Pts',(-0.228887216089035,2.32687431715301,
9.33387894496799));
#64143=CARTESIAN_POINT('Ctrl Pts',(-0.229427781996047,2.32632769709366,
9.33392612550393));
#64144=CARTESIAN_POINT('Ctrl Pts',(-0.229706756302274,2.32604455253384,
9.33395054310217));
#64145=CARTESIAN_POINT('Ctrl Pts',(-0.230258513828674,2.32548247082932,
9.33399897328838));
#64146=CARTESIAN_POINT('Ctrl Pts',(-0.230531315783888,2.32520355299751,
9.33402298498937));
#64147=CARTESIAN_POINT('Ctrl Pts',(-0.23116260062137,2.32455576651155,9.33407870519483));
#64148=CARTESIAN_POINT('Ctrl Pts',(-0.231520707502572,2.32418653436863,
9.3341104300423));
#64149=CARTESIAN_POINT('Ctrl Pts',(-0.233483254752722,2.32215329958119,
9.33428493742793));
#64150=CARTESIAN_POINT('Ctrl Pts',(-0.23507060760306,2.32047296378069,9.33442845856515));
#64151=CARTESIAN_POINT('Ctrl Pts',(-0.245360785143318,2.30934254884466,
9.33537479751482));
#64152=CARTESIAN_POINT('Ctrl Pts',(-0.253508896483958,2.29939755197797,
9.33620084103928));
#64153=CARTESIAN_POINT('Ctrl Pts',(-0.265659212282505,2.28261536638295,
9.33756489605877));
#64154=CARTESIAN_POINT('Ctrl Pts',(-0.270041747005516,2.27606996439986,
9.33809007366851));
#64155=CARTESIAN_POINT('Ctrl Pts',(-0.287328519772448,2.24808590209848,
9.34030086907598));
#64156=CARTESIAN_POINT('Ctrl Pts',(-0.29795412321071,2.22534175292491,9.3420235074827));
#64157=CARTESIAN_POINT('Ctrl Pts',(-0.306915483240647,2.19836493000829,
9.34384834081225));
#64158=CARTESIAN_POINT('Ctrl Pts',(-0.307937833344241,2.1951160679989,9.34406456008923));
#64159=CARTESIAN_POINT('Ctrl Pts',(-0.309069832391499,2.19130900610683,
9.34431331829989));
#64160=CARTESIAN_POINT('Ctrl Pts',(-0.30922969742782,2.19076612876508,9.3443486819231));
#64161=CARTESIAN_POINT('Ctrl Pts',(-0.309466095826875,2.18995548182837,
9.34440132338054));
#64162=CARTESIAN_POINT('Ctrl Pts',(-0.309543712374288,2.18968803324999,
9.34441866409503));
#64163=CARTESIAN_POINT('Ctrl Pts',(-0.309681708947806,2.18921021616435,
9.34444959641043));
#64164=CARTESIAN_POINT('Ctrl Pts',(-0.309742221283587,2.1889998869678,9.3444631957585));
#64165=CARTESIAN_POINT('Ctrl Pts',(-0.30987062967239,2.18855184699738,9.34449212927638));
#64166=CARTESIAN_POINT('Ctrl Pts',(-0.309938466280587,2.18831412039325,
9.34450745990819));
#64167=CARTESIAN_POINT('Ctrl Pts',(-0.310120658846409,2.18767284930989,
9.34454875775674));
#64168=CARTESIAN_POINT('Ctrl Pts',(-0.310234501148351,2.1872691575037,9.34457469493356));
#64169=CARTESIAN_POINT('Ctrl Pts',(-0.310483049340056,2.18638115763045,
9.34463161812143));
#64170=CARTESIAN_POINT('Ctrl Pts',(-0.31061741116021,2.18589675321653,9.34466258437064));
#64171=CARTESIAN_POINT('Ctrl Pts',(-0.311018160631981,2.18443872498491,
9.34475553976064));
#64172=CARTESIAN_POINT('Ctrl Pts',(-0.311281110982906,2.18346415114804,
9.34481733646845));
#64173=CARTESIAN_POINT('Ctrl Pts',(-0.318641213874295,2.15566673697281,
9.34657079076452));
#64174=CARTESIAN_POINT('Ctrl Pts',(-0.322250473770379,2.12803666604931,
9.34807817638457));
#64175=CARTESIAN_POINT('Ctrl Pts',(-0.322274875432262,2.10028335511254,
9.34963671698665));
#64176=CARTESIAN_POINT('',(-0.322274971935003,2.09977570497444,9.59989500205939));
#64177=CARTESIAN_POINT('Ctrl Pts',(-0.322274875630863,2.10028312914261,
9.34963672967643));
#64178=CARTESIAN_POINT('Ctrl Pts',(-0.322293905266275,2.07862243632518,
9.3508531277297));
#64179=CARTESIAN_POINT('Ctrl Pts',(-0.320129274946486,2.05701771372018,
9.35209326684815));
#64180=CARTESIAN_POINT('Ctrl Pts',(-0.315652217724324,2.03499602690769,
9.35345949425794));
#64181=CARTESIAN_POINT('Ctrl Pts',(-0.315486918798168,2.034198456551,9.35350910970234));
#64182=CARTESIAN_POINT('Ctrl Pts',(-0.315212577168667,2.032899552619,9.35359013421058));
#64183=CARTESIAN_POINT('Ctrl Pts',(-0.315105357043244,2.03239783434005,
9.35362148504255));
#64184=CARTESIAN_POINT('Ctrl Pts',(-0.314914592177069,2.0315154973075,9.35367671559367));
#64185=CARTESIAN_POINT('Ctrl Pts',(-0.31483155408659,2.0311347691182,9.35370057906101));
#64186=CARTESIAN_POINT('Ctrl Pts',(-0.314662472793085,2.03036623204061,
9.35374881383568));
#64187=CARTESIAN_POINT('Ctrl Pts',(-0.314576402694029,2.02997842982138,
9.35377318596776));
#64188=CARTESIAN_POINT('Ctrl Pts',(-0.314408409264114,2.0292280707614,9.35382040786416));
#64189=CARTESIAN_POINT('Ctrl Pts',(-0.314326575223432,2.02886549437401,
9.35384325472771));
#64190=CARTESIAN_POINT('Ctrl Pts',(-0.314130533897973,2.02800385142772,
9.35389761854134));
#64191=CARTESIAN_POINT('Ctrl Pts',(-0.314015764540868,2.02750491498554,
9.35392915351871));
#64192=CARTESIAN_POINT('Ctrl Pts',(-0.313605343649847,2.02573995497256,
9.35404090461757));
#64193=CARTESIAN_POINT('Ctrl Pts',(-0.313303223653341,2.02447546211863,
9.35412132864826));
#64194=CARTESIAN_POINT('Ctrl Pts',(-0.307952360392867,2.00266471442149,
9.35551487286207));
#64195=CARTESIAN_POINT('Ctrl Pts',(-0.300901130828245,1.98266710950557,
9.35689523677099));
#64196=CARTESIAN_POINT('Ctrl Pts',(-0.289453561004378,1.9581818922806,9.35870888205722));
#64197=CARTESIAN_POINT('Ctrl Pts',(-0.28681837249172,1.95292533082108,9.35910565754199));
#64198=CARTESIAN_POINT('Ctrl Pts',(-0.281420778202499,1.94285586478276,
9.35987829670385));
#64199=CARTESIAN_POINT('Ctrl Pts',(-0.278674879403395,1.93803628365411,
9.36025394585873));
#64200=CARTESIAN_POINT('Ctrl Pts',(-0.267994925262872,1.92036731081013,
9.36164885612311));
#64201=CARTESIAN_POINT('Ctrl Pts',(-0.259284420180758,1.90800815028088,
9.36266124421665));
#64202=CARTESIAN_POINT('Ctrl Pts',(-0.247935542658628,1.89409400626534,
9.36380890890688));
#64203=CARTESIAN_POINT('Ctrl Pts',(-0.246103352304488,1.89190758561332,
9.36398946988456));
#64204=CARTESIAN_POINT('Ctrl Pts',(-0.243915170828827,1.88936568066,9.36419935710503));
#64205=CARTESIAN_POINT('Ctrl Pts',(-0.243587153879473,1.88898643285974,
9.36423067107927));
#64206=CARTESIAN_POINT('Ctrl Pts',(-0.243084334672872,1.88840781639797,
9.36427844326892));
#64207=CARTESIAN_POINT('Ctrl Pts',(-0.242910171154434,1.88820789751323,
9.36429494850975));
#64208=CARTESIAN_POINT('Ctrl Pts',(-0.242593768694897,1.8878456090236,9.36432485743772));
#64209=CARTESIAN_POINT('Ctrl Pts',(-0.242451613928936,1.88768316806204,
9.36433826726574));
#64210=CARTESIAN_POINT('Ctrl Pts',(-0.242162633106145,1.88735361692522,
9.36436547120151));
#64211=CARTESIAN_POINT('Ctrl Pts',(-0.24201579787261,1.88718651666657,9.36437926449163));
#64212=CARTESIAN_POINT('Ctrl Pts',(-0.24159189763467,1.88670511921467,9.36441900023277));
#64213=CARTESIAN_POINT('Ctrl Pts',(-0.241314391261022,1.88639120863836,
9.36444490970192));
#64214=CARTESIAN_POINT('Ctrl Pts',(-0.240085975021403,1.8850070936514,9.36455914951093));
#64215=CARTESIAN_POINT('Ctrl Pts',(-0.239128533454196,1.88394266999483,
9.36464699809856));
#64216=CARTESIAN_POINT('Ctrl Pts',(-0.221286845089395,1.86437128628977,
9.36626294318893));
#64217=CARTESIAN_POINT('Ctrl Pts',(-0.202305480853914,1.84788555396402,
9.36763976992079));
#64218=CARTESIAN_POINT('Ctrl Pts',(-0.174643391834059,1.829016924532,9.36951361341396));
#64219=CARTESIAN_POINT('Ctrl Pts',(-0.16750083080066,1.82454472941497,9.36998666544951));
#64220=CARTESIAN_POINT('Ctrl Pts',(-0.150794226285885,1.81497445123109,
9.37108238757193));
#64221=CARTESIAN_POINT('Ctrl Pts',(-0.141132380713601,1.81006883346267,
9.37170862185046));
#64222=CARTESIAN_POINT('Ctrl Pts',(-0.12789411421198,1.8041660731153,9.37256890132675));
#64223=CARTESIAN_POINT('Ctrl Pts',(-0.124520554091748,1.80273034677676,
9.37278828283996));
#64224=CARTESIAN_POINT('Ctrl Pts',(-0.118990523464957,1.80048751599635,
9.37314853488349));
#64225=CARTESIAN_POINT('Ctrl Pts',(-0.11684855208458,1.79964539590766,9.37328822471829));
#64226=CARTESIAN_POINT('Ctrl Pts',(-0.114217583312692,1.79864342826637,
9.37346004808157));
#64227=CARTESIAN_POINT('Ctrl Pts',(-0.113736945508574,1.79846169913854,
9.37349144742457));
#64228=CARTESIAN_POINT('Ctrl Pts',(-0.112890786752646,1.79814407747496,
9.37354674381974));
#64229=CARTESIAN_POINT('Ctrl Pts',(-0.112525449031058,1.7980076970926,9.37357062453296));
#64230=CARTESIAN_POINT('Ctrl Pts',(-0.111787317701912,1.79773367844616,
9.37361888568023));
#64231=CARTESIAN_POINT('Ctrl Pts',(-0.1114145153072,1.79759606596267,9.37364326692416));
#64232=CARTESIAN_POINT('Ctrl Pts',(-0.110692761408097,1.79733116089089,
9.37369048223614));
#64233=CARTESIAN_POINT('Ctrl Pts',(-0.110343842296186,1.79720378129619,
9.37371331335844));
#64234=CARTESIAN_POINT('Ctrl Pts',(-0.10951438989669,1.79690259791433,9.37376760157657));
#64235=CARTESIAN_POINT('Ctrl Pts',(-0.109033663008653,1.79672933364461,
9.37379907658278));
#64236=CARTESIAN_POINT('Ctrl Pts',(-0.107333800319685,1.79612123089425,
9.373910413615));
#64237=CARTESIAN_POINT('Ctrl Pts',(-0.106112471378754,1.7956925989336,9.37399048153383));
#64238=CARTESIAN_POINT('Ctrl Pts',(-0.0863832012927313,1.78890171922341,
9.37528517247159));
#64239=CARTESIAN_POINT('Ctrl Pts',(-0.06733963026167,1.78423217539372,9.3765568498142));
#64240=CARTESIAN_POINT('Ctrl Pts',(-0.0299072985257442,1.77859487964436,
9.37908804780099));
#64241=CARTESIAN_POINT('Ctrl Pts',(-0.0116230347082161,1.7774157926223,
9.38033772504611));
#64242=CARTESIAN_POINT('Ctrl Pts',(0.0155271427417528,1.77797716614114,
9.38215476398131));
#64243=CARTESIAN_POINT('Ctrl Pts',(0.0243815822328268,1.77852626540802,
9.3827407513187));
#64244=CARTESIAN_POINT('Ctrl Pts',(0.0369409743264621,1.77982713385704,
9.38355290669376));
#64245=CARTESIAN_POINT('Ctrl Pts',(0.040672336647712,1.78027970992947,9.3837917723761));
#64246=CARTESIAN_POINT('Ctrl Pts',(0.0449276023634252,1.78087153810816,
9.38406075141584));
#64247=CARTESIAN_POINT('Ctrl Pts',(0.0454598999144294,1.78094692893927,
9.38409433692993));
#64248=CARTESIAN_POINT('Ctrl Pts',(0.0462619371237329,1.78106257169552,
9.38414484651368));
#64249=CARTESIAN_POINT('Ctrl Pts',(0.0465318150575613,1.78110183414029,
9.38416182624261));
#64250=CARTESIAN_POINT('Ctrl Pts',(0.0470176651122379,1.78117314657818,
9.38419236444613));
#64251=CARTESIAN_POINT('Ctrl Pts',(0.0472336540090899,1.78120507340084,
9.38420592987459));
#64252=CARTESIAN_POINT('Ctrl Pts',(0.0476658017074738,1.78126940098881,
9.38423305013833));
#64253=CARTESIAN_POINT('Ctrl Pts',(0.0478819590347595,1.78130180201619,
9.38424660489682));
#64254=CARTESIAN_POINT('Ctrl Pts',(0.0484933628282909,1.78139408481404,
9.38428491510517));
#64255=CARTESIAN_POINT('Ctrl Pts',(0.0488885328371591,1.78145448238752,
9.38430964122306));
#64256=CARTESIAN_POINT('Ctrl Pts',(0.0505383924314835,1.78170978849045,
9.38441273191768));
#64257=CARTESIAN_POINT('Ctrl Pts',(0.051792058816934,1.78191137929603,9.3844907225774));
#64258=CARTESIAN_POINT('Ctrl Pts',(0.0746908074174633,1.78573249007612,
9.38590949672349));
#64259=CARTESIAN_POINT('Ctrl Pts',(0.0959154033819419,1.7915468504694,9.38713257838033));
#64260=CARTESIAN_POINT('Ctrl Pts',(0.130295122235821,1.80486137051123,9.38919335073471));
#64261=CARTESIAN_POINT('Ctrl Pts',(0.143812240678983,1.81120658492307,9.3900260020898));
#64262=CARTESIAN_POINT('Ctrl Pts',(0.163894937197353,1.82239447007665,9.39134817235584));
#64263=CARTESIAN_POINT('Ctrl Pts',(0.170798485187874,1.82658777726573,9.39181924967101));
#64264=CARTESIAN_POINT('Ctrl Pts',(0.181845376726697,1.83387956672711,9.39260641226734));
#64265=CARTESIAN_POINT('Ctrl Pts',(0.186084659846815,1.8368264436245,9.39291698534842));
#64266=CARTESIAN_POINT('Ctrl Pts',(0.190972236384032,1.84040111974668,9.39328590247239));
#64267=CARTESIAN_POINT('Ctrl Pts',(0.191691107200913,1.84093148957632,9.39334044458028));
#64268=CARTESIAN_POINT('Ctrl Pts',(0.192719321851519,1.84169671034368,9.39341886565087));
#64269=CARTESIAN_POINT('Ctrl Pts',(0.193030465322343,1.84192914554809,9.39344265027479));
#64270=CARTESIAN_POINT('Ctrl Pts',(0.193658455124436,1.84240004727871,9.39349076508444));
#64271=CARTESIAN_POINT('Ctrl Pts',(0.19397528293384,1.84263853728334,9.39351509616395));
#64272=CARTESIAN_POINT('Ctrl Pts',(0.194589183397091,1.84310242432811,9.39356235161898));
#64273=CARTESIAN_POINT('Ctrl Pts',(0.194886306763208,1.84332775351507,9.39358527330334));
#64274=CARTESIAN_POINT('Ctrl Pts',(0.195594072083972,1.84386643833788,9.39363999482435));
#64275=CARTESIAN_POINT('Ctrl Pts',(0.196004352103471,1.84418026582054,9.39367181324343));
#64276=CARTESIAN_POINT('Ctrl Pts',(0.197240675919896,1.8451306629686,9.39376798911634));
#64277=CARTESIAN_POINT('Ctrl Pts',(0.198064380009028,1.84577025247464,9.39383246606994));
#64278=CARTESIAN_POINT('Ctrl Pts',(0.206653357776954,1.8525064969228,9.39450901333605));
#64279=CARTESIAN_POINT('Ctrl Pts',(0.214136917744299,1.85895230666839,9.39513508877155));
#64280=CARTESIAN_POINT('Ctrl Pts',(0.226309182941974,1.87045135245252,9.3962193882094));
#64281=CARTESIAN_POINT('Ctrl Pts',(0.231153482423853,1.87533027437389,9.39667052080783));
#64282=CARTESIAN_POINT('Ctrl Pts',(0.251870509400426,1.89757513541451,9.39868675085785));
#64283=CARTESIAN_POINT('Ctrl Pts',(0.265968746776228,1.91649225684921,9.40030348969872));
#64284=CARTESIAN_POINT('Ctrl Pts',(0.28154240915932,1.94300550062641,9.40234695746611));
#64285=CARTESIAN_POINT('Ctrl Pts',(0.284992248894844,1.94935858864712,9.40282102421913));
#64286=CARTESIAN_POINT('Ctrl Pts',(0.289678059808428,1.95872602710037,9.40349242003798));
#64287=CARTESIAN_POINT('Ctrl Pts',(0.291086465160418,1.96165121774778,9.40369829552711));
#64288=CARTESIAN_POINT('Ctrl Pts',(0.292670774985091,1.96507310134358,9.40393434035085));
#64289=CARTESIAN_POINT('Ctrl Pts',(0.292889896592284,1.96554941801986,9.40396709036049));
#64290=CARTESIAN_POINT('Ctrl Pts',(0.293220081670156,1.96627179726101,9.4040165948859));
#64291=CARTESIAN_POINT('Ctrl Pts',(0.293331998618923,1.96651746522499,9.40403340180831));
#64292=CARTESIAN_POINT('Ctrl Pts',(0.293525139910082,1.96694284401612,9.40406245337255));
#64293=CARTESIAN_POINT('Ctrl Pts',(0.293606507841787,1.96712248846603,9.40407470691692));
#64294=CARTESIAN_POINT('Ctrl Pts',(0.293776057526267,1.96749773705492,9.40410027039347));
#64295=CARTESIAN_POINT('Ctrl Pts',(0.293864208569767,1.96769335397047,9.40411357839707));
#64296=CARTESIAN_POINT('Ctrl Pts',(0.294080627217723,1.96817489418025,9.40414629355887));
#64297=CARTESIAN_POINT('Ctrl Pts',(0.294208673588825,1.96846091753322,9.40416568704251));
#64298=CARTESIAN_POINT('Ctrl Pts',(0.294704994718336,1.96957392424243,9.4042410051272));
#64299=CARTESIAN_POINT('Ctrl Pts',(0.295070206078204,1.97040228134483,9.40429674323942));
#64300=CARTESIAN_POINT('Ctrl Pts',(0.301844110849039,1.98594364649578,9.40533674853517));
#64301=CARTESIAN_POINT('Ctrl Pts',(0.307149481955308,2.00111587611416,9.40625645772988));
#64302=CARTESIAN_POINT('Ctrl Pts',(0.315761891685831,2.0332715556909,9.4081320705102));
#64303=CARTESIAN_POINT('Ctrl Pts',(0.318878263655718,2.05025149494832,9.40908340975898));
#64304=CARTESIAN_POINT('Ctrl Pts',(0.322160179407236,2.08252846682303,9.41092520354666));
#64305=CARTESIAN_POINT('Ctrl Pts',(0.322625578948256,2.09774571043346,9.41180714661301));
#64306=CARTESIAN_POINT('Ctrl Pts',(0.321950901364855,2.11453816428942,9.4128210172081));
#64307=CARTESIAN_POINT('Ctrl Pts',(0.321874671138459,2.11613806208383,9.41291800755346));
#64308=CARTESIAN_POINT('Ctrl Pts',(0.321720838577729,2.1189288608512,9.41308791065645));
#64309=CARTESIAN_POINT('Ctrl Pts',(0.321648541136978,2.12012003163019,9.41316065695271));
#64310=CARTESIAN_POINT('Ctrl Pts',(0.321534375178657,2.12184274369171,9.41326620421207));
#64311=CARTESIAN_POINT('Ctrl Pts',(0.321497800229628,2.12237463554175,9.4132988389927));
#64312=CARTESIAN_POINT('Ctrl Pts',(0.321431507998527,2.12330495479299,9.41335600245721));
#64313=CARTESIAN_POINT('Ctrl Pts',(0.321402369269883,2.12370342332857,9.41338051292542));
#64314=CARTESIAN_POINT('Ctrl Pts',(0.321344946620158,2.12446909365008,9.41342766205336));
#64315=CARTESIAN_POINT('Ctrl Pts',(0.321316774063191,2.12483630339331,9.41345029717843));
#64316=CARTESIAN_POINT('Ctrl Pts',(0.321248967248624,2.1257006891357,9.41350363260593));
#64317=CARTESIAN_POINT('Ctrl Pts',(0.321208808255606,2.12619782194969,9.41353434935725));
#64318=CARTESIAN_POINT('Ctrl Pts',(0.321086918148299,2.12766428944318,9.41362508429229));
#64319=CARTESIAN_POINT('Ctrl Pts',(0.321001952555254,2.12863334313052,9.41368520403908));
#64320=CARTESIAN_POINT('Ctrl Pts',(0.320214261455708,2.13717263423444,9.41421642369828));
#64321=CARTESIAN_POINT('Ctrl Pts',(0.319248297052032,2.14471562345521,9.41469576945104));
#64322=CARTESIAN_POINT('Ctrl Pts',(0.317395269729055,2.15600111193666,9.41542908976962));
#64323=CARTESIAN_POINT('Ctrl Pts',(0.316706449256916,2.15977378095019,9.41567696340226));
#64324=CARTESIAN_POINT('Ctrl Pts',(0.310558210433744,2.19034898985035,9.41770786880935));
#64325=CARTESIAN_POINT('Ctrl Pts',(0.301773983632801,2.21636767891518,9.41958800651799));
#64326=CARTESIAN_POINT('Ctrl Pts',(0.288278933120266,2.24411362657803,9.42164917565765));
#64327=CARTESIAN_POINT('Ctrl Pts',(0.286693197301422,2.24724297138602,9.42188230031728));
#64328=CARTESIAN_POINT('Ctrl Pts',(0.281510629397849,2.25706914932774,9.4226151341318));
#64329=CARTESIAN_POINT('Ctrl Pts',(0.277727524980031,2.26366549782313,9.42310834655076));
#64330=CARTESIAN_POINT('Ctrl Pts',(0.273066095713724,2.27116539070468,9.423665364877));
#64331=CARTESIAN_POINT('Ctrl Pts',(0.272411892341,2.27220465914063,9.42374246436211));
#64332=CARTESIAN_POINT('Ctrl Pts',(0.271545457693763,2.27356378454799,9.42384315163782));
#64333=CARTESIAN_POINT('Ctrl Pts',(0.27133858407659,2.27388701991723,9.42386708714367));
#64334=CARTESIAN_POINT('Ctrl Pts',(0.271001814037888,2.27441115114478,9.42390588079707));
#64335=CARTESIAN_POINT('Ctrl Pts',(0.27087227120859,2.27461227203914,9.42392076244257));
#64336=CARTESIAN_POINT('Ctrl Pts',(0.27062269629981,2.27499880187041,9.42394935449233));
#64337=CARTESIAN_POINT('Ctrl Pts',(0.270502697916237,2.27518423110806,9.42396306702688));
#64338=CARTESIAN_POINT('Ctrl Pts',(0.270225331889106,2.27561187049936,9.42399468238821));
#64339=CARTESIAN_POINT('Ctrl Pts',(0.270067828685458,2.27585399331703,9.42401257610559));
#64340=CARTESIAN_POINT('Ctrl Pts',(0.269562871587066,2.27662796344427,9.42406975576439));
#64341=CARTESIAN_POINT('Ctrl Pts',(0.269214167780233,2.27715899946471,9.42410895845359));
#64342=CARTESIAN_POINT('Ctrl Pts',(0.266061789665223,2.2819289099315,9.42446085589621));
#64343=CARTESIAN_POINT('Ctrl Pts',(0.263159592701876,2.28610223000424,9.42476708997274));
#64344=CARTESIAN_POINT('Ctrl Pts',(0.260036684061468,2.29037369043887,9.42508074119694));
#64345=CARTESIAN_POINT('Ctrl Pts',(0.259913504681772,2.29054183045582,9.42509308798623));
#64346=CARTESIAN_POINT('Ctrl Pts',(0.25932147906525,2.29134830390119,9.42515231092131));
#64347=CARTESIAN_POINT('Ctrl Pts',(0.258850440098123,2.29198503221156,9.42519907565717));
#64348=CARTESIAN_POINT('Ctrl Pts',(0.256999955442098,2.29446723923914,9.42538143701996));
#64349=CARTESIAN_POINT('Ctrl Pts',(0.255603054913416,2.296299676604,9.42551618059549));
#64350=CARTESIAN_POINT('Ctrl Pts',(0.240165254001852,2.31610656686588,9.42697581477699));
#64351=CARTESIAN_POINT('Ctrl Pts',(0.224272862623354,2.33255804960562,9.4282212133178));
#64352=CARTESIAN_POINT('Ctrl Pts',(0.19938621607212,2.35337544520435,9.43005147965133));
#64353=CARTESIAN_POINT('Ctrl Pts',(0.191724027836489,2.35922163952094,9.43060068106986));
#64354=CARTESIAN_POINT('Ctrl Pts',(0.176489233658036,2.36980029911379,9.43168014871905));
#64355=CARTESIAN_POINT('Ctrl Pts',(0.168959322308485,2.37457854332827,9.43220827828904));
#64356=CARTESIAN_POINT('Ctrl Pts',(0.160226663581501,2.37962468730197,9.43281917128163));
#64357=CARTESIAN_POINT('Ctrl Pts',(0.159208622307278,2.38020557453047,9.43289036182301));
#64358=CARTESIAN_POINT('Ctrl Pts',(0.157380071232551,2.38123575084875,9.43301819428699));
#64359=CARTESIAN_POINT('Ctrl Pts',(0.156570745881377,2.38168712409802,9.4330747609426));
#64360=CARTESIAN_POINT('Ctrl Pts',(0.155339561859942,2.38236682920168,9.43316079802449));
#64361=CARTESIAN_POINT('Ctrl Pts',(0.154919116873706,2.38259772280643,9.43319017677444));
#64362=CARTESIAN_POINT('Ctrl Pts',(0.154186809634179,2.38299775480658,9.43324134312015));
#64363=CARTESIAN_POINT('Ctrl Pts',(0.15387517986218,2.38316731893261,9.4332631154851));
#64364=CARTESIAN_POINT('Ctrl Pts',(0.153230812612084,2.38351655452129,9.43330813269705));
#64365=CARTESIAN_POINT('Ctrl Pts',(0.152898037736114,2.38369615555367,9.43333138000991));
#64366=CARTESIAN_POINT('Ctrl Pts',(0.152092765056396,2.38412893868529,9.43338763297719));
#64367=CARTESIAN_POINT('Ctrl Pts',(0.151619951357845,2.38438152775036,9.43342065963198));
#64368=CARTESIAN_POINT('Ctrl Pts',(0.149867663437279,2.38531203218161,9.43354305305116));
#64369=CARTESIAN_POINT('Ctrl Pts',(0.148584269826922,2.38598249404803,9.43363268317355));
#64370=CARTESIAN_POINT('Ctrl Pts',(0.125575466630344,2.39780590928345,9.43523950744023));
#64371=CARTESIAN_POINT('Ctrl Pts',(0.102661022236782,2.40646010635937,9.43684794922477));
#64372=CARTESIAN_POINT('Ctrl Pts',(0.0629198669896975,2.4165077838812,9.43961400874966));
#64373=CARTESIAN_POINT('Ctrl Pts',(0.046555244213754,2.41932542191676,9.44074413869801));
#64374=CARTESIAN_POINT('Ctrl Pts',(0.0237242275602795,2.42146330071826,
9.44226132629087));
#64375=CARTESIAN_POINT('Ctrl Pts',(0.0173857367668061,2.42186835842644,
9.44267607759508));
#64376=CARTESIAN_POINT('Ctrl Pts',(0.00806040830968497,2.42218796979088,
9.44327301086615));
#64377=CARTESIAN_POINT('Ctrl Pts',(0.00508041032992029,2.42224873785607,
9.44346177771094));
#64378=CARTESIAN_POINT('Ctrl Pts',(0.00159514308373494,2.42227144754737,
9.44367989290862));
#64379=CARTESIAN_POINT('Ctrl Pts',(0.00109040439749176,2.42227355059362,
9.44371141530839));
#64380=CARTESIAN_POINT('Ctrl Pts',(0.000319813198342206,2.42227495096366,
9.44375943930489));
#64381=CARTESIAN_POINT('Ctrl Pts',(5.39659598036372E-5,2.42227510513226,
9.44377598869163));
#64382=CARTESIAN_POINT('Ctrl Pts',(-0.000427771212261796,2.42227478841018,
9.4438059437003));
#64383=CARTESIAN_POINT('Ctrl Pts',(-0.000643659632893115,2.42227442954117,
9.44381935556109));
#64384=CARTESIAN_POINT('Ctrl Pts',(-0.00108154367626381,2.42227326164294,
9.44384653363649));
#64385=CARTESIAN_POINT('Ctrl Pts',(-0.00130353786061986,2.4222724401752,
9.44386029909049));
#64386=CARTESIAN_POINT('Ctrl Pts',(-0.00194226324689817,2.42226941664924,
9.44389986827118));
#64387=CARTESIAN_POINT('Ctrl Pts',(-0.00235899321992314,2.42226663564444,
9.44392563945212));
#64388=CARTESIAN_POINT('Ctrl Pts',(-0.00418754460761447,2.42225088594671,
9.44403852534218));
#64389=CARTESIAN_POINT('Ctrl Pts',(-0.00559930503995359,2.42222944771996,
9.44412517217553));
#64390=CARTESIAN_POINT('Ctrl Pts',(-0.0318110010635777,2.42165909221178,
9.44572522627955));
#64391=CARTESIAN_POINT('Ctrl Pts',(-0.0564704156518841,2.41825781489996,
9.44709007386456));
#64392=CARTESIAN_POINT('Ctrl Pts',(-0.0944218169442216,2.40846791367448,
9.44928292744702));
#64393=CARTESIAN_POINT('Ctrl Pts',(-0.108088359660273,2.40394867462966,
9.45009194976089));
#64394=CARTESIAN_POINT('Ctrl Pts',(-0.129318534041725,2.39531481854868,
9.45142260314094));
#64395=CARTESIAN_POINT('Ctrl Pts',(-0.13709873535756,2.39178424076615,9.45192681945133));
#64396=CARTESIAN_POINT('Ctrl Pts',(-0.146221588326327,2.3871989084949,9.45254241476187));
#64397=CARTESIAN_POINT('Ctrl Pts',(-0.14770821413167,2.38643716457588,9.45264351988173));
#64398=CARTESIAN_POINT('Ctrl Pts',(-0.150291767365153,2.3850878961813,9.45282064402546));
#64399=CARTESIAN_POINT('Ctrl Pts',(-0.151391347496616,2.38450550736685,
9.45289648189224));
#64400=CARTESIAN_POINT('Ctrl Pts',(-0.15296634063232,2.38365960175618,9.45300577106128));
#64401=CARTESIAN_POINT('Ctrl Pts',(-0.153444512120132,2.38340122217347,
9.45303903969748));
#64402=CARTESIAN_POINT('Ctrl Pts',(-0.154272963672417,2.38295085767419,
9.45309683311902));
#64403=CARTESIAN_POINT('Ctrl Pts',(-0.154623545695276,2.38275942830104,
9.45312133805));
#64404=CARTESIAN_POINT('Ctrl Pts',(-0.155296788107194,2.38239018919724,
9.45316848911739));
#64405=CARTESIAN_POINT('Ctrl Pts',(-0.155619501475434,2.38221247688586,
9.45319113174278));
#64406=CARTESIAN_POINT('Ctrl Pts',(-0.156378801743565,2.38179264578832,
9.45324450407131));
#64407=CARTESIAN_POINT('Ctrl Pts',(-0.156815131240463,2.38155006564499,
9.45327525027954));
#64408=CARTESIAN_POINT('Ctrl Pts',(-0.158320985185207,2.3807082902142,9.45338162526641));
#64409=CARTESIAN_POINT('Ctrl Pts',(-0.159387642975346,2.38010401236891,
9.45345743657322));
#64410=CARTESIAN_POINT('Ctrl Pts',(-0.175185760898387,2.37103468030694,
9.45458722068634));
#64411=CARTESIAN_POINT('Ctrl Pts',(-0.189226195622882,2.36142518482748,
9.45568369345702));
#64412=CARTESIAN_POINT('Ctrl Pts',(-0.20889186676361,2.34554851778675,9.4573619250163));
#64413=CARTESIAN_POINT('Ctrl Pts',(-0.215137967766779,2.34009483680573,
9.45791877329522));
#64414=CARTESIAN_POINT('Ctrl Pts',(-0.232883932008744,2.32335122024046,
9.45956617884787));
#64415=CARTESIAN_POINT('Ctrl Pts',(-0.243756072219131,2.31143249917826,
9.46066334876295));
#64416=CARTESIAN_POINT('Ctrl Pts',(-0.257575779302565,2.29379257220772,
9.46214546943847));
#64417=CARTESIAN_POINT('Ctrl Pts',(-0.261314064662466,2.28872152455604,
9.46255672074514));
#64418=CARTESIAN_POINT('Ctrl Pts',(-0.266579874975248,2.2811215887171,9.46314808354513));
#64419=CARTESIAN_POINT('Ctrl Pts',(-0.268224961715004,2.2786763304488,9.46333470165444));
#64420=CARTESIAN_POINT('Ctrl Pts',(-0.270111483347827,2.27578741539139,
9.46355062148433));
#64421=CARTESIAN_POINT('Ctrl Pts',(-0.270385636642753,2.275365436594,9.46358204803376));
#64422=CARTESIAN_POINT('Ctrl Pts',(-0.270802937888664,2.27471981844616,
9.46362995624542));
#64423=CARTESIAN_POINT('Ctrl Pts',(-0.270946798110636,2.27449664386975,
9.46364648534541));
#64424=CARTESIAN_POINT('Ctrl Pts',(-0.271207119354334,2.27409170180817,
9.46367641915284));
#64425=CARTESIAN_POINT('Ctrl Pts',(-0.271323673087633,2.27390999583102,
9.4636898300541));
#64426=CARTESIAN_POINT('Ctrl Pts',(-0.271559827030519,2.27354101919044,
9.46371701991688));
#64427=CARTESIAN_POINT('Ctrl Pts',(-0.271679415618944,2.27335374275792,
9.46373079809167));
#64428=CARTESIAN_POINT('Ctrl Pts',(-0.272023285189683,2.27281401119528,
9.46377044337863));
#64429=CARTESIAN_POINT('Ctrl Pts',(-0.272247075716551,2.27246124178854,
9.46379627774612));
#64430=CARTESIAN_POINT('Ctrl Pts',(-0.273228985673921,2.27090674619155,
9.46390978053083));
#64431=CARTESIAN_POINT('Ctrl Pts',(-0.273979853806524,2.26970042542414,
9.46399697477659));
#64432=CARTESIAN_POINT('Ctrl Pts',(-0.28774136849943,2.24726217992771,9.46560325088784));
#64433=CARTESIAN_POINT('Ctrl Pts',(-0.298258316118295,2.22459397480774,
9.46697273787475));
#64434=CARTESIAN_POINT('Ctrl Pts',(-0.310544594283947,2.18733976350732,
9.46916768716732));
#64435=CARTESIAN_POINT('Ctrl Pts',(-0.314117621720231,2.17345921458919,
9.46997349802716));
#64436=CARTESIAN_POINT('Ctrl Pts',(-0.318324573656111,2.15102071091626,
9.47129921116356));
#64437=CARTESIAN_POINT('Ctrl Pts',(-0.319561066207244,2.14259522697368,
9.47180184729937));
#64438=CARTESIAN_POINT('Ctrl Pts',(-0.320729624449961,2.13162346569902,
9.47246714147152));
#64439=CARTESIAN_POINT('Ctrl Pts',(-0.320967260234324,2.12911276150998,
9.47262009726594));
#64440=CARTESIAN_POINT('Ctrl Pts',(-0.321234412885735,2.12588703924306,
9.47281761024139));
#64441=CARTESIAN_POINT('Ctrl Pts',(-0.321291053455397,2.12517430792223,
9.47286131353706));
#64442=CARTESIAN_POINT('Ctrl Pts',(-0.321378388716614,2.12402699912974,
9.47293176656261));
#64443=CARTESIAN_POINT('Ctrl Pts',(-0.321410574994004,2.12359253484346,
9.47295846939065));
#64444=CARTESIAN_POINT('Ctrl Pts',(-0.321470132793487,2.12276585014836,
9.47300932406289));
#64445=CARTESIAN_POINT('Ctrl Pts',(-0.321497667725141,2.1223736420003,9.47303347072777));
#64446=CARTESIAN_POINT('Ctrl Pts',(-0.321558720451101,2.12148061612756,
9.47308849536898));
#64447=CARTESIAN_POINT('Ctrl Pts',(-0.321591786024402,2.12097976940913,
9.47311938748575));
#64448=CARTESIAN_POINT('Ctrl Pts',(-0.321686619014133,2.11949040181011,
9.47321134751648));
#64449=CARTESIAN_POINT('Ctrl Pts',(-0.321744999173261,2.11850167796141,
9.473272521558));
#64450=CARTESIAN_POINT('Ctrl Pts',(-0.322118764873831,2.11163367380052,
9.47369834966237));
#64451=CARTESIAN_POINT('Ctrl Pts',(-0.322277523335093,2.10574731414913,
9.47406788771386));
#64452=CARTESIAN_POINT('Ctrl Pts',(-0.322268664214049,2.08532379795546,
9.47536706946818));
#64453=CARTESIAN_POINT('Ctrl Pts',(-0.321278877098094,2.07080633380078,
9.47632145016023));
#64454=CARTESIAN_POINT('Ctrl Pts',(-0.315359557933376,2.02744830219341,
9.47925015796388));
#64455=CARTESIAN_POINT('Ctrl Pts',(-0.307485361907278,1.99916226809078,
9.48127769601501));
#64456=CARTESIAN_POINT('Ctrl Pts',(-0.295302783577381,1.97092731096894,
9.48322301636947));
#64457=CARTESIAN_POINT('Ctrl Pts',(-0.294689784603897,1.9695338200556,9.48331877406412));
#64458=CARTESIAN_POINT('Ctrl Pts',(-0.293893466352226,1.96775785167776,
9.48344044466888));
#64459=CARTESIAN_POINT('Ctrl Pts',(-0.293719248059145,1.9673713504484,9.48346690112843));
#64460=CARTESIAN_POINT('Ctrl Pts',(-0.293440801682592,1.9667568599397,9.48350892651822));
#64461=CARTESIAN_POINT('Ctrl Pts',(-0.293337070153306,1.96652864824182,
9.48352452587794));
#64462=CARTESIAN_POINT('Ctrl Pts',(-0.293142475352939,1.9661018578994,9.48355368339751));
#64463=CARTESIAN_POINT('Ctrl Pts',(-0.293051677210064,1.96590325209454,
9.4835672453907));
#64464=CARTESIAN_POINT('Ctrl Pts',(-0.292846811189296,1.96545634364368,
9.48359774873974));
#64465=CARTESIAN_POINT('Ctrl Pts',(-0.292732629608321,1.96520809425863,
9.48361468291889));
#64466=CARTESIAN_POINT('Ctrl Pts',(-0.292391785114081,1.96446951849386,
9.48366503589277));
#64467=CARTESIAN_POINT('Ctrl Pts',(-0.292164203564573,1.96397961334793,
9.48369839809519));
#64468=CARTESIAN_POINT('Ctrl Pts',(-0.29027864874859,1.95994722522602,9.48397271058692));
#64469=CARTESIAN_POINT('Ctrl Pts',(-0.288557454015435,1.95643443055387,
9.48420982746064));
#64470=CARTESIAN_POINT('Ctrl Pts',(-0.282738861666761,1.94508689881804,
9.48497251934108));
#64471=CARTESIAN_POINT('Ctrl Pts',(-0.278382745406185,1.93738879035215,
9.48548478703197));
#64472=CARTESIAN_POINT('Ctrl Pts',(-0.263121990917532,1.91283508650598,
9.48713306172484));
#64473=CARTESIAN_POINT('Ctrl Pts',(-0.250959803603303,1.89681752392562,
9.48823403895985));
#64474=CARTESIAN_POINT('Ctrl Pts',(-0.225428417107186,1.86901123125861,
9.49037117181415));
#64475=CARTESIAN_POINT('Ctrl Pts',(-0.212420745365698,1.85699573719498,
9.4913956400729));
#64476=CARTESIAN_POINT('Ctrl Pts',(-0.19748630371246,1.84531985922216,9.49254715982183));
#64477=CARTESIAN_POINT('Ctrl Pts',(-0.196473156370865,1.84453745281758,
9.49262515296697));
#64478=CARTESIAN_POINT('Ctrl Pts',(-0.19505102248142,1.84345266927825,9.49273446645517));
#64479=CARTESIAN_POINT('Ctrl Pts',(-0.194645931477413,1.84314518570579,
9.49276558567021));
#64480=CARTESIAN_POINT('Ctrl Pts',(-0.193944224686769,1.84261516976142,
9.4928194599483));
#64481=CARTESIAN_POINT('Ctrl Pts',(-0.193647948686448,1.84239218743609,
9.49284219731972));
#64482=CARTESIAN_POINT('Ctrl Pts',(-0.193033051858006,1.84193106590439,
9.49288936750593));
#64483=CARTESIAN_POINT('Ctrl Pts',(-0.192714373775032,1.84169300436662,
9.49291380330471));
#64484=CARTESIAN_POINT('Ctrl Pts',(-0.191967022234189,1.84113686447298,
9.49297108452006));
#64485=CARTESIAN_POINT('Ctrl Pts',(-0.191537998598352,1.84081926065425,
9.49300394835082));
#64486=CARTESIAN_POINT('Ctrl Pts',(-0.19014953536488,1.839796719296,9.49311024700899));
#64487=CARTESIAN_POINT('Ctrl Pts',(-0.189186986384869,1.83909603833931,
9.49318384668908));
#64488=CARTESIAN_POINT('Ctrl Pts',(-0.17486368694438,1.82879042979709,9.49427776876171));
#64489=CARTESIAN_POINT('Ctrl Pts',(-0.160792622469784,1.82021880171326,
9.49533787817407));
#64490=CARTESIAN_POINT('Ctrl Pts',(-0.118976140481853,1.7989450772965,9.49844746597816));
#64491=CARTESIAN_POINT('Ctrl Pts',(-0.0900024818253041,1.7890517788638,
9.50056766839039));
#64492=CARTESIAN_POINT('Ctrl Pts',(-0.0564190115584183,1.7826801346126,
9.50276673719013));
#64493=CARTESIAN_POINT('Ctrl Pts',(-0.0527538985608195,1.78205026974294,
9.50300315008199));
#64494=CARTESIAN_POINT('Ctrl Pts',(-0.0485041130863901,1.78139544194962,
9.50327251264313));
#64495=CARTESIAN_POINT('Ctrl Pts',(-0.0479294667994533,1.78130848831257,
9.50330883484219));
#64496=CARTESIAN_POINT('Ctrl Pts',(-0.0470761105143446,1.78118172150566,
9.5033626215749));
#64497=CARTESIAN_POINT('Ctrl Pts',(-0.0467975825365779,1.78114071888459,
9.5033801530505));
#64498=CARTESIAN_POINT('Ctrl Pts',(-0.0463021001400073,1.78106844120686,
9.50341129717223));
#64499=CARTESIAN_POINT('Ctrl Pts',(-0.046085167632363,1.78103702252929,
9.50342491798359));
#64500=CARTESIAN_POINT('Ctrl Pts',(-0.045625302319848,1.78097089845441,
9.50345376077885));
#64501=CARTESIAN_POINT('Ctrl Pts',(-0.0453823625692465,1.78093624929591,
9.50346897950236));
#64502=CARTESIAN_POINT('Ctrl Pts',(-0.044732131235611,1.78084426805622,
9.50350966373129));
#64503=CARTESIAN_POINT('Ctrl Pts',(-0.0443247673666703,1.78078743790415,
9.50353510072));
#64504=CARTESIAN_POINT('Ctrl Pts',(-0.0423933919717215,1.78052176575215,
9.50365546307971));
#64505=CARTESIAN_POINT('Ctrl Pts',(-0.0408679738915177,1.78032305248546,
9.50374982321856));
#64506=CARTESIAN_POINT('Ctrl Pts',(-0.0283770495561705,1.77878675495633,
9.50451717478705));
#64507=CARTESIAN_POINT('Ctrl Pts',(-0.0173495505827463,1.77800270991574,
9.5051612146624));
#64508=CARTESIAN_POINT('Ctrl Pts',(0.021258894589797,1.77724753925847,9.50736621207636));
#64509=CARTESIAN_POINT('Ctrl Pts',(0.0487751108935489,1.78024668439134,
9.50885917040709));
#64510=CARTESIAN_POINT('Ctrl Pts',(0.0776070937649643,1.78720184596617,
9.51057801592824));
#64511=CARTESIAN_POINT('Ctrl Pts',(0.0796345344332012,1.78771185285784,
9.51069966392777));
#64512=CARTESIAN_POINT('Ctrl Pts',(0.0839626336116177,1.78884548339104,
9.51096115963452));
#64513=CARTESIAN_POINT('Ctrl Pts',(0.0862616128379872,1.78947497556769,
9.51110115994581));
#64514=CARTESIAN_POINT('Ctrl Pts',(0.0948214199487309,1.79192116081028,
9.5116268549502));
#64515=CARTESIAN_POINT('Ctrl Pts',(0.101033316806052,1.79390208659309,9.51201729693627));
#64516=CARTESIAN_POINT('Ctrl Pts',(0.108155619489423,1.79641375761126,9.51247693793854));
#64517=CARTESIAN_POINT('Ctrl Pts',(0.109129006680805,1.79676229710562,9.51254001757606));
#64518=CARTESIAN_POINT('Ctrl Pts',(0.110574214667697,1.79728764060791,9.51263406890725));
#64519=CARTESIAN_POINT('Ctrl Pts',(0.111047331850594,1.79746087928598,9.51266492174205));
#64520=CARTESIAN_POINT('Ctrl Pts',(0.11188913772098,1.79777135931316,9.51271993099435));
#64521=CARTESIAN_POINT('Ctrl Pts',(0.112257985831564,1.79790816792534,9.51274407291855));
#64522=CARTESIAN_POINT('Ctrl Pts',(0.113033800919043,1.79819754080995,9.51279493409158));
#64523=CARTESIAN_POINT('Ctrl Pts',(0.113440711338705,1.79835025355325,9.51282165826909));
#64524=CARTESIAN_POINT('Ctrl Pts',(0.114511880722566,1.79875473542803,9.51289213486699));
#64525=CARTESIAN_POINT('Ctrl Pts',(0.115175615597057,1.79900787749082,9.51293593323548));
#64526=CARTESIAN_POINT('Ctrl Pts',(0.118149825392962,1.80015349061443,9.51313277673));
#64527=CARTESIAN_POINT('Ctrl Pts',(0.120450752921286,1.80107036613783,9.51328664025806));
#64528=CARTESIAN_POINT('Ctrl Pts',(0.137280980310969,1.80800275127666,9.51442401013526));
#64529=CARTESIAN_POINT('Ctrl Pts',(0.151361044867126,1.81504708540176,9.51544285665507));
#64530=CARTESIAN_POINT('Ctrl Pts',(0.189802305431232,1.83793456828385,9.51841627303041));
#64531=CARTESIAN_POINT('Ctrl Pts',(0.212614617876141,1.85607759062619,9.520430528713));
#64532=CARTESIAN_POINT('Ctrl Pts',(0.235580777745899,1.88004470970184,9.52257251920456));
#64533=CARTESIAN_POINT('Ctrl Pts',(0.238412745553526,1.88311754461179,9.52283870463431));
#64534=CARTESIAN_POINT('Ctrl Pts',(0.241543513364925,1.88665005258505,9.52313446883139));
#64535=CARTESIAN_POINT('Ctrl Pts',(0.24190169365826,1.88705625267219,9.52316832883036));
#64536=CARTESIAN_POINT('Ctrl Pts',(0.24244188082922,1.88767198237343,9.52321942628094));
#64537=CARTESIAN_POINT('Ctrl Pts',(0.24262464152749,1.88788084486705,9.52323671952709));
#64538=CARTESIAN_POINT('Ctrl Pts',(0.242941862053745,1.88824431703072,9.52326674488746));
#64539=CARTESIAN_POINT('Ctrl Pts',(0.243076444274206,1.88839881888922,9.52327948617231));
#64540=CARTESIAN_POINT('Ctrl Pts',(0.243354850055728,1.88871904787771,9.52330584944662));
#64541=CARTESIAN_POINT('Ctrl Pts',(0.243498651628819,1.88888479346428,9.52331946974435));
#64542=CARTESIAN_POINT('Ctrl Pts',(0.243840898407636,1.88928008172286,9.52335189392682));
#64543=CARTESIAN_POINT('Ctrl Pts',(0.244039189601296,1.88950975881168,9.52337068627775));
#64544=CARTESIAN_POINT('Ctrl Pts',(0.244692432966752,1.89026856261424,9.52343261761529));
#64545=CARTESIAN_POINT('Ctrl Pts',(0.245145994975034,1.89079889161819,9.52347565408988));
#64546=CARTESIAN_POINT('Ctrl Pts',(0.246217765048562,1.89206033450812,9.52357744716268));
#64547=CARTESIAN_POINT('Ctrl Pts',(0.246834448624139,1.8927927430431,9.52363609541454));
#64548=CARTESIAN_POINT('Ctrl Pts',(0.25381349692726,1.90115683009499,9.52430085457905));
#64549=CARTESIAN_POINT('Ctrl Pts',(0.259823622435528,1.90907691296325,9.52488320410247));
#64550=CARTESIAN_POINT('Ctrl Pts',(0.277194578880663,1.93431136866626,9.52664138994009));
#64551=CARTESIAN_POINT('Ctrl Pts',(0.287261287564148,1.95245137868623,9.52777563166682));
#64552=CARTESIAN_POINT('Ctrl Pts',(0.302959451080443,1.98853437346439,9.52999794610384));
#64553=CARTESIAN_POINT('Ctrl Pts',(0.30890014571705,2.00624734981947,9.53107527606678));
#64554=CARTESIAN_POINT('Ctrl Pts',(0.313578157120183,2.02562544018355,9.53228612463053));
#64555=CARTESIAN_POINT('Ctrl Pts',(0.313872999191476,2.02687971503066,9.53236462497757));
#64556=CARTESIAN_POINT('Ctrl Pts',(0.31427403345198,2.02863286735863,9.5324745353521));
#64557=CARTESIAN_POINT('Ctrl Pts',(0.314386577545431,2.02913029153313,9.53250574133487));
#64558=CARTESIAN_POINT('Ctrl Pts',(0.314578991486629,2.02999020413533,9.53255972507368));
#64559=CARTESIAN_POINT('Ctrl Pts',(0.314659416923627,2.03035256830887,9.53258248496662));
#64560=CARTESIAN_POINT('Ctrl Pts',(0.31482468396915,2.03110332348554,9.53262966328984));
#64561=CARTESIAN_POINT('Ctrl Pts',(0.314909433264316,2.03149173400273,9.53265408463713));
#64562=CARTESIAN_POINT('Ctrl Pts',(0.315105995962537,2.03240066290525,9.5327112649062));
#64563=CARTESIAN_POINT('Ctrl Pts',(0.315217238401547,2.03292130236603,9.53274404205147));
#64564=CARTESIAN_POINT('Ctrl Pts',(0.315571499736244,2.03459966691907,9.53284978306714));
#64565=CARTESIAN_POINT('Ctrl Pts',(0.315809432362121,2.03575844503607,9.53292290937718));
#64566=CARTESIAN_POINT('Ctrl Pts',(0.319297336476145,2.0532329903578,9.53402754526642));
#64567=CARTESIAN_POINT('Ctrl Pts',(0.321285037015188,2.06977238603252,9.53509975900824));
#64568=CARTESIAN_POINT('Ctrl Pts',(0.323231592584745,2.11582119407242,9.53815608150583));
#64569=CARTESIAN_POINT('Ctrl Pts',(0.320434628341889,2.14528229190852,9.54020227371234));
#64570=CARTESIAN_POINT('Ctrl Pts',(0.313603712207176,2.17425621027312,9.54212712541004));
#64571=CARTESIAN_POINT('Ctrl Pts',(0.313531637237962,2.17455994585998,9.54214729202866));
#64572=CARTESIAN_POINT('Ctrl Pts',(0.312481985730568,2.1789549113422,9.54243892265675));
#64573=CARTESIAN_POINT('Ctrl Pts',(0.311424783449572,2.18302697085351,9.54270694077793));
#64574=CARTESIAN_POINT('Ctrl Pts',(0.310141489237368,2.18759980985889,9.54300454459229));
#64575=CARTESIAN_POINT('Ctrl Pts',(0.309993562065426,2.18812185609623,9.54303846970813));
#64576=CARTESIAN_POINT('Ctrl Pts',(0.309767905786681,2.18891061433645,9.54308964871059));
#64577=CARTESIAN_POINT('Ctrl Pts',(0.309691150034815,2.18917760026315,9.54310695864112));
#64578=CARTESIAN_POINT('Ctrl Pts',(0.309557162688518,2.18964140038983,9.54313700490263));
#64579=CARTESIAN_POINT('Ctrl Pts',(0.30950008853647,2.18983825928897,9.54314975043534));
#64580=CARTESIAN_POINT('Ctrl Pts',(0.309384964243553,2.19023393165153,9.54317535270668));
#64581=CARTESIAN_POINT('Ctrl Pts',(0.309326910301223,2.1904327434342,9.54318820915659));
#64582=CARTESIAN_POINT('Ctrl Pts',(0.309185640020984,2.19091481060904,9.54321936406198));
#64583=CARTESIAN_POINT('Ctrl Pts',(0.309102225757637,2.19119800884122,9.54323765088659));
#64584=CARTESIAN_POINT('Ctrl Pts',(0.308831880195581,2.19211122222652,9.54329657012141));
#64585=CARTESIAN_POINT('Ctrl Pts',(0.308643409458439,2.19274078553139,9.543337112967));
#64586=CARTESIAN_POINT('Ctrl Pts',(0.30819623401549,2.19421805816325,9.54343207856947));
#64587=CARTESIAN_POINT('Ctrl Pts',(0.307935953978102,2.19506529038031,9.54348641191282));
#64588=CARTESIAN_POINT('Ctrl Pts',(0.305088165925829,2.20420064554312,9.54407096359412));
#64589=CARTESIAN_POINT('Ctrl Pts',(0.302169958604867,2.21238286966036,9.54458296135033));
#64590=CARTESIAN_POINT('Ctrl Pts',(0.293043169543791,2.23503536741487,9.54599360109135));
#64591=CARTESIAN_POINT('Ctrl Pts',(0.286100108734918,2.24918323761678,9.54686730760931));
#64592=CARTESIAN_POINT('Ctrl Pts',(0.265710002651048,2.28402747769003,9.54912528271612));
#64593=CARTESIAN_POINT('Ctrl Pts',(0.250875320436816,2.30378724829836,9.55051749627373));
#64594=CARTESIAN_POINT('Ctrl Pts',(0.232869482148884,2.32279000620268,9.5521047987591));
#64595=CARTESIAN_POINT('Ctrl Pts',(0.231794285951151,2.32390844434582,9.55219921212121));
#64596=CARTESIAN_POINT('Ctrl Pts',(0.230325763386399,2.32541411418644,9.55232768420004));
#64597=CARTESIAN_POINT('Ctrl Pts',(0.22993944413791,2.32580817562161,9.5523614364851));
#64598=CARTESIAN_POINT('Ctrl Pts',(0.229283647535119,2.32647368699355,9.55241865865483));
#64599=CARTESIAN_POINT('Ctrl Pts',(0.229014694614836,2.32674565392945,9.5524421054444));
#64600=CARTESIAN_POINT('Ctrl Pts',(0.228496217131304,2.3272680782101,9.55248726539111));
#64601=CARTESIAN_POINT('Ctrl Pts',(0.228246763204345,2.32751860517724,9.55250897541078));
#64602=CARTESIAN_POINT('Ctrl Pts',(0.227657888815688,2.3281080694983,9.55256018396993));
#64603=CARTESIAN_POINT('Ctrl Pts',(0.227318123576451,2.3284466598574,9.55258969778726));
#64604=CARTESIAN_POINT('Ctrl Pts',(0.226327313114705,2.32942964514087,9.55267567236767));
#64605=CARTESIAN_POINT('Ctrl Pts',(0.225674278834751,2.33007202041072,9.55273222178505));
#64606=CARTESIAN_POINT('Ctrl Pts',(0.221002260832091,2.33462875092592,9.55313598936922));
#64607=CARTESIAN_POINT('Ctrl Pts',(0.216884621938633,2.33844014852408,9.55348765011136));
#64608=CARTESIAN_POINT('Ctrl Pts',(0.203288451437431,2.35038147011633,9.55463661105784));
#64609=CARTESIAN_POINT('Ctrl Pts',(0.193437262798419,2.35806789331508,9.55545130936903));
#64610=CARTESIAN_POINT('Ctrl Pts',(0.163876903271003,2.3784872461229,9.55784086479478));
#64611=CARTESIAN_POINT('Ctrl Pts',(0.143192879968853,2.38966618912064,9.55945293553449));
#64612=CARTESIAN_POINT('Ctrl Pts',(0.112896738166894,2.40199565880107,9.56161953866308));
#64613=CARTESIAN_POINT('Ctrl Pts',(0.104165728386744,2.40511733828523,9.56222222941829));
#64614=CARTESIAN_POINT('Ctrl Pts',(0.0946232931880807,2.40807162624372,
9.56284914231799));
#64615=CARTESIAN_POINT('Ctrl Pts',(0.0939344592572533,2.40828235742213,
9.5628942206823));
#64616=CARTESIAN_POINT('Ctrl Pts',(0.0929724265354901,2.40857314297219,
9.562956926307));
#64617=CARTESIAN_POINT('Ctrl Pts',(0.0926998260241585,2.40865514561766,
9.5629746664034));
#64618=CARTESIAN_POINT('Ctrl Pts',(0.0922290641011621,2.40879607850494,
9.56300525337992));
#64619=CARTESIAN_POINT('Ctrl Pts',(0.0920309545939117,2.4088551792703,9.56301811027563));
#64620=CARTESIAN_POINT('Ctrl Pts',(0.09163316271629,2.40897343330362,9.56304389596315));
#64621=CARTESIAN_POINT('Ctrl Pts',(0.0914334802172228,2.40903258354481,
9.56305682451607));
#64622=CARTESIAN_POINT('Ctrl Pts',(0.090955823126286,2.40917357233683,9.56308771443844));
#64623=CARTESIAN_POINT('Ctrl Pts',(0.0906777943401781,2.40925522987861,
9.5631056651384));
#64624=CARTESIAN_POINT('Ctrl Pts',(0.0898160525804968,2.40950706292818,
9.56316121304228));
#64625=CARTESIAN_POINT('Ctrl Pts',(0.0892319635807685,2.40967596289235,
9.56319873596414));
#64626=CARTESIAN_POINT('Ctrl Pts',(0.0878627563749514,2.41006769860641,
9.56328640551743));
#64627=CARTESIAN_POINT('Ctrl Pts',(0.0870772586301308,2.41028920822259,
9.56333647701758));
#64628=CARTESIAN_POINT('Ctrl Pts',(0.0844105515308456,2.41103029315772,
9.56350573554873));
#64629=CARTESIAN_POINT('Ctrl Pts',(0.082525425212537,2.41153577496495,9.56362415592365));
#64630=CARTESIAN_POINT('Ctrl Pts',(0.0745270477796974,2.41360277975589,
9.56412185688444));
#64631=CARTESIAN_POINT('Ctrl Pts',(0.0683728530071468,2.41500182254504,
9.56449312844384));
#64632=CARTESIAN_POINT('Ctrl Pts',(0.0513576742428597,2.41834767507816,
9.5654975470323));
#64633=CARTESIAN_POINT('Ctrl Pts',(0.0404314161564145,2.41991902349606,
9.56611828907221));
#64634=CARTESIAN_POINT('Ctrl Pts',(0.0064523773799224,2.42303665247454,
9.56802880003962));
#64635=CARTESIAN_POINT('Ctrl Pts',(-0.0166987589237333,2.42266912572022,
9.56930764977649));
#64636=CARTESIAN_POINT('Ctrl Pts',(-0.0470715056288379,2.41890744302973,
9.57110646206526));
#64637=CARTESIAN_POINT('Ctrl Pts',(-0.0544965823404676,2.41772282350899,
9.57155539303144));
#64638=CARTESIAN_POINT('Ctrl Pts',(-0.0628246298547019,2.41609362804777,
9.57207169532607));
#64639=CARTESIAN_POINT('Ctrl Pts',(-0.0637753695140291,2.41590317823654,
9.57213082522459));
#64640=CARTESIAN_POINT('Ctrl Pts',(-0.065213024945841,2.41560843612037,
9.57222052826154));
#64641=CARTESIAN_POINT('Ctrl Pts',(-0.0657005881219724,2.41550729989806,
9.57225100053699));
#64642=CARTESIAN_POINT('Ctrl Pts',(-0.0665481510461026,2.41532943837156,
9.57230406124097));
#64643=CARTESIAN_POINT('Ctrl Pts',(-0.0669082583258361,2.41525322532427,
9.57232663324337));
#64644=CARTESIAN_POINT('Ctrl Pts',(-0.0676591206794027,2.41509296845079,
9.57237375684451));
#64645=CARTESIAN_POINT('Ctrl Pts',(-0.0680498513707639,2.41500881432813,
9.57239831194312));
#64646=CARTESIAN_POINT('Ctrl Pts',(-0.0689729264245647,2.41480820827544,
9.57245640047189));
#64647=CARTESIAN_POINT('Ctrl Pts',(-0.0695051327119088,2.41469113285577,
9.57248995384491));
#64648=CARTESIAN_POINT('Ctrl Pts',(-0.0712593552349693,2.41430056958,9.57260075627762));
#64649=CARTESIAN_POINT('Ctrl Pts',(-0.0724800629376421,2.41402131162136,
9.57267819036309));
#64650=CARTESIAN_POINT('Ctrl Pts',(-0.0753382245780173,2.41334990431894,
9.57286028181588));
#64651=CARTESIAN_POINT('Ctrl Pts',(-0.0769742823434019,2.41295202556255,
9.57296512208139));
#64652=CARTESIAN_POINT('Ctrl Pts',(-0.0869298037493087,2.41044811723346,
9.57360686137637));
#64653=CARTESIAN_POINT('Ctrl Pts',(-0.0951648491774735,2.40802346242178,
9.57415397222917));
#64654=CARTESIAN_POINT('Ctrl Pts',(-0.117424419152896,2.40049167901227,
9.57567884256153));
#64655=CARTESIAN_POINT('Ctrl Pts',(-0.131205561355818,2.39473506651518,
9.57667521699707));
#64656=CARTESIAN_POINT('Ctrl Pts',(-0.156583756946295,2.38200064237059,
9.57859224294938));
#64657=CARTESIAN_POINT('Ctrl Pts',(-0.168239395761824,2.37520601761502,
9.57950883040451));
#64658=CARTESIAN_POINT('Ctrl Pts',(-0.182751116727739,2.36547907146556,
9.58067536921705));
#64659=CARTESIAN_POINT('Ctrl Pts',(-0.186025275815827,2.36319518780022,
9.58094029400329));
#64660=CARTESIAN_POINT('Ctrl Pts',(-0.191152488926826,2.35947522047748,
9.58135698907413));
#64661=CARTESIAN_POINT('Ctrl Pts',(-0.193033706137368,2.35807877267938,
9.58151028002283));
#64662=CARTESIAN_POINT('Ctrl Pts',(-0.195765127100436,2.35600463242039,
9.58173325549735));
#64663=CARTESIAN_POINT('Ctrl Pts',(-0.196627361062241,2.35534298062153,
9.58180370273195));
#64664=CARTESIAN_POINT('Ctrl Pts',(-0.197761355400776,2.35446363813542,
9.58189641586467));
#64665=CARTESIAN_POINT('Ctrl Pts',(-0.198036123619149,2.35424985853898,
9.58191888522254));
#64666=CARTESIAN_POINT('Ctrl Pts',(-0.20149937179276,2.35154630617547,9.58220215049142));
#64667=CARTESIAN_POINT('Ctrl Pts',(-0.204641230168573,2.3489970113427,9.58245972929217));
#64668=CARTESIAN_POINT('Ctrl Pts',(-0.208189879611555,2.34600509048688,
9.58275054800604));
#64669=CARTESIAN_POINT('Ctrl Pts',(-0.208644271420657,2.34561982520748,
9.5827877841282));
#64670=CARTESIAN_POINT('Ctrl Pts',(-0.209311686610368,2.34505075521187,
9.58284247031465));
#64671=CARTESIAN_POINT('Ctrl Pts',(-0.20952553844152,2.34486793077867,9.58285999175023));
#64672=CARTESIAN_POINT('Ctrl Pts',(-0.209906002985302,2.34454180385035,
9.58289116197631));
#64673=CARTESIAN_POINT('Ctrl Pts',(-0.210072708605164,2.34439861092093,
9.58290481885064));
#64674=CARTESIAN_POINT('Ctrl Pts',(-0.210394272972469,2.34412182891296,
9.58293116044853));
#64675=CARTESIAN_POINT('Ctrl Pts',(-0.210549150361129,2.3439882635173,9.58294384684597));
#64676=CARTESIAN_POINT('Ctrl Pts',(-0.210884727460055,2.34369830623031,
9.58297133356393));
#64677=CARTESIAN_POINT('Ctrl Pts',(-0.211065380750687,2.34354186043651,
9.58298612987173));
#64678=CARTESIAN_POINT('Ctrl Pts',(-0.211785288656747,2.34291701736114,
9.58304509117304));
#64679=CARTESIAN_POINT('Ctrl Pts',(-0.212323164792294,2.34244702417345,
9.58308913857432));
#64680=CARTESIAN_POINT('Ctrl Pts',(-0.21956193357634,2.33607926295029,9.58368193039609));
#64681=CARTESIAN_POINT('Ctrl Pts',(-0.226017253251032,2.32990671173682,
9.58421058059388));
#64682=CARTESIAN_POINT('Ctrl Pts',(-0.236605132436258,2.31890497407467,
9.58509501434325));
#64683=CARTESIAN_POINT('Ctrl Pts',(-0.240866136554129,2.31420757980559,
9.58545628349211));
#64684=CARTESIAN_POINT('Ctrl Pts',(-0.264506056783994,2.2865485642281,9.5875119236336));
#64685=CARTESIAN_POINT('Ctrl Pts',(-0.28073531957503,2.26109458618406,9.58914715594871));
#64686=CARTESIAN_POINT('Ctrl Pts',(-0.295462859792642,2.22881175616512,
9.59125345225957));
#64687=CARTESIAN_POINT('Ctrl Pts',(-0.297594985291289,2.2238062574249,9.59158030365337));
#64688=CARTESIAN_POINT('Ctrl Pts',(-0.299923823053417,2.21793070666265,
9.59196512777944));
#64689=CARTESIAN_POINT('Ctrl Pts',(-0.300244966647922,2.21711067922002,
9.59201886148015));
#64690=CARTESIAN_POINT('Ctrl Pts',(-0.300750958895294,2.21580288607428,
9.59210460099196));
#64691=CARTESIAN_POINT('Ctrl Pts',(-0.300937993041113,2.21531596610577,
9.59213653338941));
#64692=CARTESIAN_POINT('Ctrl Pts',(-0.301265398003013,2.21445738694076,
9.59219285725472));
#64693=CARTESIAN_POINT('Ctrl Pts',(-0.301406265576937,2.21408591730771,
9.59221723202037));
#64694=CARTESIAN_POINT('Ctrl Pts',(-0.301695520267472,2.21331887386166,
9.59226757576633));
#64695=CARTESIAN_POINT('Ctrl Pts',(-0.301843817046464,2.21292326700398,
9.59229354771251));
#64696=CARTESIAN_POINT('Ctrl Pts',(-0.30222035125099,2.21191275670874,9.59235990677157));
#64697=CARTESIAN_POINT('Ctrl Pts',(-0.302447489390301,2.2112974481997,9.59240033050724));
#64698=CARTESIAN_POINT('Ctrl Pts',(-0.303358609094866,2.20880587357108,
9.59256409123947));
#64699=CARTESIAN_POINT('Ctrl Pts',(-0.304027010673634,2.20692399322836,
9.59268794572183));
#64700=CARTESIAN_POINT('Ctrl Pts',(-0.308277547784344,2.19459446912556,
9.59350061582068));
#64701=CARTESIAN_POINT('Ctrl Pts',(-0.311337696316926,2.18397589875874,
9.59420655617429));
#64702=CARTESIAN_POINT('Ctrl Pts',(-0.319464805452436,2.14914129510034,
9.59654338974039));
#64703=CARTESIAN_POINT('Ctrl Pts',(-0.322292093734264,2.1244962849695,9.59823599948666));
#64704=CARTESIAN_POINT('Ctrl Pts',(-0.322274922248267,2.09977613648567,
9.59989505973818));
#64705=CARTESIAN_POINT('',(-0.322274904352262,2.10008161445013,9.84943339449977));
#64706=CARTESIAN_POINT('Ctrl Pts',(-0.322274921952289,2.09977571079884,
9.59989508830759));
#64707=CARTESIAN_POINT('Ctrl Pts',(-0.322265671419364,2.08648387703572,
9.60078715195519));
#64708=CARTESIAN_POINT('Ctrl Pts',(-0.321434112451775,2.0732031904389,9.60166524079288));
#64709=CARTESIAN_POINT('Ctrl Pts',(-0.319708691269864,2.05940567424189,
9.60253948376591));
#64710=CARTESIAN_POINT('Ctrl Pts',(-0.319631403647282,2.05880154889031,
9.60257768487487));
#64711=CARTESIAN_POINT('Ctrl Pts',(-0.319507081484653,2.05785118517041,
9.60263765375844));
#64712=CARTESIAN_POINT('Ctrl Pts',(-0.319461196144858,2.05750480179114,
9.60265948449201));
#64713=CARTESIAN_POINT('Ctrl Pts',(-0.319382597378943,2.05691879056035,
9.60269637224838));
#64714=CARTESIAN_POINT('Ctrl Pts',(-0.319350177510797,2.0566791246622,9.60271144566598));
#64715=CARTESIAN_POINT('Ctrl Pts',(-0.319289796358272,2.05623650450128,
9.60273925950681));
#64716=CARTESIAN_POINT('Ctrl Pts',(-0.319261911308225,2.05603354022491,
9.60275200424059));
#64717=CARTESIAN_POINT('Ctrl Pts',(-0.319203803245083,2.05561356484504,
9.60277835619602));
#64718=CARTESIAN_POINT('Ctrl Pts',(-0.319173552697779,2.05539655965656,
9.60279196164848));
#64719=CARTESIAN_POINT('Ctrl Pts',(-0.319104038714989,2.05490158641993,
9.60282297015809));
#64720=CARTESIAN_POINT('Ctrl Pts',(-0.319064633440148,2.05462363918519,
9.60284036503596));
#64721=CARTESIAN_POINT('Ctrl Pts',(-0.318943106250876,2.05377442604973,
9.60289345872754));
#64722=CARTESIAN_POINT('Ctrl Pts',(-0.318859812351775,2.05320332499879,
9.60292909132913));
#64723=CARTESIAN_POINT('Ctrl Pts',(-0.318241105588632,2.04903954156366,
9.60318836732557));
#64724=CARTESIAN_POINT('Ctrl Pts',(-0.317646494603501,2.04545573560968,
9.60340873532879));
#64725=CARTESIAN_POINT('Ctrl Pts',(-0.316854094961741,2.04113373003469,
9.6036719407541));
#64726=CARTESIAN_POINT('Ctrl Pts',(-0.316714147963807,2.04038537314566,
9.6037174218293));
#64727=CARTESIAN_POINT('Ctrl Pts',(-0.316373113190074,2.03859681355242,
9.60382591321105));
#64728=CARTESIAN_POINT('Ctrl Pts',(-0.3161695442495,2.0375570868723,9.60388881331254));
#64729=CARTESIAN_POINT('Ctrl Pts',(-0.314510419600608,2.02929928953474,
9.60438717973276));
#64730=CARTESIAN_POINT('Ctrl Pts',(-0.312812907351446,2.02213156428149,
9.60481246343778));
#64731=CARTESIAN_POINT('Ctrl Pts',(-0.310407601730414,2.01333173463978,
9.60533234307907));
#64732=CARTESIAN_POINT('Ctrl Pts',(-0.309930110064764,2.01163940681742,
9.60543221748913));
#64733=CARTESIAN_POINT('Ctrl Pts',(-0.304111048579226,1.9916431331841,9.60661192046668));
#64734=CARTESIAN_POINT('Ctrl Pts',(-0.297169078320852,1.97384412868202,
9.60766043382897));
#64735=CARTESIAN_POINT('Ctrl Pts',(-0.281881698283323,1.94303241663747,
9.60961232575473));
#64736=CARTESIAN_POINT('Ctrl Pts',(-0.274099228679788,1.92980706379206,
9.61050088783487));
#64737=CARTESIAN_POINT('Ctrl Pts',(-0.264022154742173,1.91517730134154,
9.61157251296456));
#64738=CARTESIAN_POINT('Ctrl Pts',(-0.262615427799732,1.91318387459762,
9.61172052944944));
#64739=CARTESIAN_POINT('Ctrl Pts',(-0.260772342886741,1.91063405802477,
9.61191253060131));
#64740=CARTESIAN_POINT('Ctrl Pts',(-0.260356574365398,1.91006282889596,
9.61195571923108));
#64741=CARTESIAN_POINT('Ctrl Pts',(-0.259682522801638,1.90914311349617,
9.61202554089117));
#64742=CARTESIAN_POINT('Ctrl Pts',(-0.25942540712087,1.90879377125256,9.61205212853279));
#64743=CARTESIAN_POINT('Ctrl Pts',(-0.258933635397163,1.90812842052553,
9.61210289491117));
#64744=CARTESIAN_POINT('Ctrl Pts',(-0.258699103999483,1.90781232053615,
9.61212706875809));
#64745=CARTESIAN_POINT('Ctrl Pts',(-0.258162067194254,1.90709126981355,
9.61218233840468));
#64746=CARTESIAN_POINT('Ctrl Pts',(-0.257859187540174,1.9066866002662,9.61221344881301));
#64747=CARTESIAN_POINT('Ctrl Pts',(-0.256928958667069,1.90544982190382,
9.61230881347616));
#64748=CARTESIAN_POINT('Ctrl Pts',(-0.256298529013032,1.90462004815259,
9.61237318862474));
#64749=CARTESIAN_POINT('Ctrl Pts',(-0.251586643897813,1.89848029776362,
9.61285247640672));
#64750=CARTESIAN_POINT('Ctrl Pts',(-0.247344839087903,1.89329598574655,
9.61327373487159));
#64751=CARTESIAN_POINT('Ctrl Pts',(-0.241631033473346,1.8867404923346,9.61382902560213));
#64752=CARTESIAN_POINT('Ctrl Pts',(-0.240303223799621,1.8852454091279,9.61395725866386));
#64753=CARTESIAN_POINT('Ctrl Pts',(-0.222006648773894,1.86502604300508,
9.6157133478048));
#64754=CARTESIAN_POINT('Ctrl Pts',(-0.202908828305303,1.84835076034038,
9.6174303130816));
#64755=CARTESIAN_POINT('Ctrl Pts',(-0.174981527945144,1.82923012579209,
9.61971458589249));
#64756=CARTESIAN_POINT('Ctrl Pts',(-0.167707311502605,1.82466541746763,
9.62029063096817));
#64757=CARTESIAN_POINT('Ctrl Pts',(-0.156043522334113,1.81798013377205,
9.62117671884305));
#64758=CARTESIAN_POINT('Ctrl Pts',(-0.151773515398532,1.81565937506084,
9.62149357783868));
#64759=CARTESIAN_POINT('Ctrl Pts',(-0.145376582416376,1.81236781300317,
9.62195554228492));
#64760=CARTESIAN_POINT('Ctrl Pts',(-0.143289114450342,1.81132222789547,
9.62210433035351));
#64761=CARTESIAN_POINT('Ctrl Pts',(-0.140353544793918,1.80989152931229,
9.62231064997974));
#64762=CARTESIAN_POINT('Ctrl Pts',(-0.139514912643606,1.80948729545792,
9.62236926126176));
#64763=CARTESIAN_POINT('Ctrl Pts',(-0.138056809206751,1.80879223681351,
9.62247058028614));
#64764=CARTESIAN_POINT('Ctrl Pts',(-0.137438146598455,1.80849974307325,
9.62251338692643));
#64765=CARTESIAN_POINT('Ctrl Pts',(-0.1366045121888,1.80810885803212,9.62257081835119));
#64766=CARTESIAN_POINT('Ctrl Pts',(-0.136390362850642,1.8080087322676,9.62258554959852));
#64767=CARTESIAN_POINT('Ctrl Pts',(-0.135990948615336,1.80782252096879,
9.62261298368893));
#64768=CARTESIAN_POINT('Ctrl Pts',(-0.135805711858567,1.80773637587705,
9.62262569022769));
#64769=CARTESIAN_POINT('Ctrl Pts',(-0.135420355718909,1.80755760993318,
9.62265208950303));
#64770=CARTESIAN_POINT('Ctrl Pts',(-0.135220223738272,1.80746501859875,
9.62266578031125));
#64771=CARTESIAN_POINT('Ctrl Pts',(-0.134759809839212,1.80725258090561,
9.62269723224165));
#64772=CARTESIAN_POINT('Ctrl Pts',(-0.134499462249459,1.80713287587977,
9.62271498455661));
#64773=CARTESIAN_POINT('Ctrl Pts',(-0.133692887145491,1.8067633236822,9.62276988256546));
#64774=CARTESIAN_POINT('Ctrl Pts',(-0.133146116560625,1.80651465442079,
9.62280695577378));
#64775=CARTESIAN_POINT('Ctrl Pts',(-0.128632955691229,1.80447729369562,
9.62311182498411));
#64776=CARTESIAN_POINT('Ctrl Pts',(-0.124631175558136,1.80276746166572,
9.62337489751965));
#64777=CARTESIAN_POINT('Ctrl Pts',(-0.119557146071901,1.80071999931101,
9.62370090705481));
#64778=CARTESIAN_POINT('Ctrl Pts',(-0.118516340536975,1.80030631124409,
9.62376738488982));
#64779=CARTESIAN_POINT('Ctrl Pts',(-0.115374747326695,1.79907655050822,
9.62396691745769));
#64780=CARTESIAN_POINT('Ctrl Pts',(-0.113267499666749,1.79827706622264,
9.62409924544897));
#64781=CARTESIAN_POINT('Ctrl Pts',(-0.107193139454431,1.79604507734008,
9.62447684055135));
#64782=CARTESIAN_POINT('Ctrl Pts',(-0.103205976426813,1.7946682247101,9.62472001124117));
#64783=CARTESIAN_POINT('Ctrl Pts',(-0.0838983303295262,1.78842232724667,
9.62588017845485));
#64784=CARTESIAN_POINT('Ctrl Pts',(-0.0682545337282205,1.78462571766052,
9.62676910178737));
#64785=CARTESIAN_POINT('Ctrl Pts',(-0.0502815599184166,1.78166445983123,
9.62779061851345));
#64786=CARTESIAN_POINT('Ctrl Pts',(-0.0481675119212139,1.78133773035714,
9.62791075662132));
#64787=CARTESIAN_POINT('Ctrl Pts',(-0.0361458714139469,1.77960212916412,
9.62859439336849));
#64788=CARTESIAN_POINT('Ctrl Pts',(-0.0261806462749892,1.77863436023969,
9.62916310060311));
#64789=CARTESIAN_POINT('Ctrl Pts',(-0.0076000591459639,1.77769992674078,
9.63024285808662));
#64790=CARTESIAN_POINT('Ctrl Pts',(0.00100011120099212,1.77761191297262,
9.63075026980546));
#64791=CARTESIAN_POINT('Ctrl Pts',(0.0121569598886418,1.77794416064751,
9.63142311694115));
#64792=CARTESIAN_POINT('Ctrl Pts',(0.014719855418881,1.77805112113135,9.63157867013347));
#64793=CARTESIAN_POINT('Ctrl Pts',(0.0179994393702184,1.77822723353041,
9.63177907620164));
#64794=CARTESIAN_POINT('Ctrl Pts',(0.0187175976236789,1.77826821017325,
9.63182304394822));
#64795=CARTESIAN_POINT('Ctrl Pts',(0.0198714429416238,1.77833792261787,
9.63189382141325));
#64796=CARTESIAN_POINT('Ctrl Pts',(0.0203072220930385,1.77836514026265,
9.63192058344464));
#64797=CARTESIAN_POINT('Ctrl Pts',(0.0211350983192706,1.77841853649556,
9.63197148454883));
#64798=CARTESIAN_POINT('Ctrl Pts',(0.0215272057644241,1.77844454683457,
9.63199561829509));
#64799=CARTESIAN_POINT('Ctrl Pts',(0.0224182961810345,1.77850529426981,
9.63205052208679));
#64800=CARTESIAN_POINT('Ctrl Pts',(0.0229172469440312,1.77854047594726,
9.63208130604097));
#64801=CARTESIAN_POINT('Ctrl Pts',(0.024395816212228,1.77864819170939,9.63217265407773));
#64802=CARTESIAN_POINT('Ctrl Pts',(0.0253751806253729,1.77872404273846,
9.63223332220271));
#64803=CARTESIAN_POINT('Ctrl Pts',(0.0320688451450753,1.77927325943073,
9.63264909427837));
#64804=CARTESIAN_POINT('Ctrl Pts',(0.0377696635335392,1.77989455074883,
9.63300882543525));
#64805=CARTESIAN_POINT('Ctrl Pts',(0.0437967519519885,1.78071463831535,
9.63339546789787));
#64806=CARTESIAN_POINT('Ctrl Pts',(0.0441428303656283,1.78076230142191,
9.63341769119958));
#64807=CARTESIAN_POINT('Ctrl Pts',(0.0677143896289908,1.78404772017893,
9.63493283839322));
#64808=CARTESIAN_POINT('Ctrl Pts',(0.0905134820693072,1.789809683876,9.63650595581321));
#64809=CARTESIAN_POINT('Ctrl Pts',(0.124812493549504,1.80258420156764,9.63898282532728));
#64810=CARTESIAN_POINT('Ctrl Pts',(0.136851079331668,1.80792786370775,9.63987346420303));
#64811=CARTESIAN_POINT('Ctrl Pts',(0.152804503187828,1.81621282385161,9.64105793674554));
#64812=CARTESIAN_POINT('Ctrl Pts',(0.157029198863677,1.81852848583413,9.64137195711746));
#64813=CARTESIAN_POINT('Ctrl Pts',(0.163206786996482,1.82209698088708,9.64182999402412));
#64814=CARTESIAN_POINT('Ctrl Pts',(0.165200474983747,1.82327749076189,9.6419776339886));
#64815=CARTESIAN_POINT('Ctrl Pts',(0.167972782795711,1.82495968130117,9.64218249223668));
#64816=CARTESIAN_POINT('Ctrl Pts',(0.168762181530821,1.82544334135998,9.64224077373028));
#64817=CARTESIAN_POINT('Ctrl Pts',(0.170128254952208,1.82628844443987,9.6423415281116));
#64818=CARTESIAN_POINT('Ctrl Pts',(0.170705884343607,1.8266483220269,9.64238409880506));
#64819=CARTESIAN_POINT('Ctrl Pts',(0.171536094664468,1.82716922173726,9.64244523302585));
#64820=CARTESIAN_POINT('Ctrl Pts',(0.171789592886376,1.82732876734451,9.64246389295051));
#64821=CARTESIAN_POINT('Ctrl Pts',(0.172231289517532,1.8276076209064,9.64249639348975));
#64822=CARTESIAN_POINT('Ctrl Pts',(0.172419587034698,1.82772677089896,9.64251024462435));
#64823=CARTESIAN_POINT('Ctrl Pts',(0.172782171318709,1.8279567322029,9.64253690832689));
#64824=CARTESIAN_POINT('Ctrl Pts',(0.172956474762788,1.82806751551614,9.64254972272716));
#64825=CARTESIAN_POINT('Ctrl Pts',(0.173370103738522,1.82833096728078,9.6425801237524));
#64826=CARTESIAN_POINT('Ctrl Pts',(0.173609334766229,1.8284837848445,9.64259770041354));
#64827=CARTESIAN_POINT('Ctrl Pts',(0.174451010046514,1.82902300289317,9.6426595181164));
#64828=CARTESIAN_POINT('Ctrl Pts',(0.175052374439053,1.82941109761541,9.64270364720757));
#64829=CARTESIAN_POINT('Ctrl Pts',(0.183194095914158,1.83470391641883,9.6433006448549));
#64830=CARTESIAN_POINT('Ctrl Pts',(0.190527998055029,1.83992077136793,9.64383312506809));
#64831=CARTESIAN_POINT('Ctrl Pts',(0.216893752261523,1.8603904120473,9.64576569496135));
#64832=CARTESIAN_POINT('Ctrl Pts',(0.234394833718438,1.87748059127205,9.64709132827387));
#64833=CARTESIAN_POINT('Ctrl Pts',(0.259513590099184,1.90829672842963,9.64934713552132));
#64834=CARTESIAN_POINT('Ctrl Pts',(0.268359252205346,1.92088923103108,9.65023808329113));
#64835=CARTESIAN_POINT('Ctrl Pts',(0.277530494507211,1.93615869645021,9.65131255051548));
#64836=CARTESIAN_POINT('Ctrl Pts',(0.278764921540662,1.93826791864038,9.65146081333302));
#64837=CARTESIAN_POINT('Ctrl Pts',(0.280325336210399,1.94100509040068,9.65165308969602));
#64838=CARTESIAN_POINT('Ctrl Pts',(0.280673433229465,1.94162039504213,9.65169630436787));
#64839=CARTESIAN_POINT('Ctrl Pts',(0.28123188701732,1.94261515453396,9.65176615797292));
#64840=CARTESIAN_POINT('Ctrl Pts',(0.281443508322857,1.94299389987107,9.65179275144132));
#64841=CARTESIAN_POINT('Ctrl Pts',(0.281845645913678,1.94371704375871,9.65184352221876));
#64842=CARTESIAN_POINT('Ctrl Pts',(0.282036297505233,1.94406136649512,9.65186769462323));
#64843=CARTESIAN_POINT('Ctrl Pts',(0.282470267050254,1.94484852830807,9.65192295155037));
#64844=CARTESIAN_POINT('Ctrl Pts',(0.282713174801769,1.94529159129355,9.65195405065742));
#64845=CARTESIAN_POINT('Ctrl Pts',(0.283453424575645,1.94664936981929,9.65204934708391));
#64846=CARTESIAN_POINT('Ctrl Pts',(0.283947372955939,1.94756591906286,9.65211366504469));
#64847=CARTESIAN_POINT('Ctrl Pts',(0.287576036548408,1.95437794819383,9.65259163766534));
#64848=CARTESIAN_POINT('Ctrl Pts',(0.290531097615571,1.96036680430612,9.65301159912822));
#64849=CARTESIAN_POINT('Ctrl Pts',(0.294156953708207,1.96832935245155,9.65357023009964));
#64850=CARTESIAN_POINT('Ctrl Pts',(0.29499779666557,1.97022414518271,9.65370317838104));
#64851=CARTESIAN_POINT('Ctrl Pts',(0.305847921418465,1.99532470676818,9.65546456822883));
#64852=CARTESIAN_POINT('Ctrl Pts',(0.313110758852136,2.01961877240534,9.65718200063609));
#64853=CARTESIAN_POINT('Ctrl Pts',(0.320268831644503,2.06056772313276,9.65998738362136));
#64854=CARTESIAN_POINT('Ctrl Pts',(0.321853887246089,2.07682140030427,9.66107582920751));
#64855=CARTESIAN_POINT('Ctrl Pts',(0.322215262751302,2.09376267499009,9.66214167892647));
#64856=CARTESIAN_POINT('Ctrl Pts',(0.322226939854633,2.09439830194317,9.6621815673453));
#64857=CARTESIAN_POINT('Ctrl Pts',(0.322244471416836,2.09553589239932,9.6622527692901));
#64858=CARTESIAN_POINT('Ctrl Pts',(0.322251034004431,2.0960378406693,9.6622841211853));
#64859=CARTESIAN_POINT('Ctrl Pts',(0.322259260764259,2.0968040192095,9.66233187551054));
#64860=CARTESIAN_POINT('Ctrl Pts',(0.322261772797697,2.09706823670336,9.66234832521787));
#64861=CARTESIAN_POINT('Ctrl Pts',(0.322265765375423,2.09755057736286,9.66237832088129));
#64862=CARTESIAN_POINT('Ctrl Pts',(0.322267349413251,2.09776869829432,9.66239187260473));
#64863=CARTESIAN_POINT('Ctrl Pts',(0.322270087853262,2.09820706682223,9.66241908258498));
#64864=CARTESIAN_POINT('Ctrl Pts',(0.322271237920267,2.09842731300957,9.66243274054373));
#64865=CARTESIAN_POINT('Ctrl Pts',(0.322273874681947,2.09905562592237,9.66247166713947));
#64866=CARTESIAN_POINT('Ctrl Pts',(0.32227481212114,2.09946369639774,9.66249690488908));
#64867=CARTESIAN_POINT('Ctrl Pts',(0.322275506782068,2.10120956097637,9.66260469689603));
#64868=CARTESIAN_POINT('Ctrl Pts',(0.322267709156086,2.10254736943902,9.66268683354602));
#64869=CARTESIAN_POINT('Ctrl Pts',(0.321951589917165,2.12876791924119,9.66428831208858));
#64870=CARTESIAN_POINT('Ctrl Pts',(0.318770551402111,2.15353685246092,9.66565743017571));
#64871=CARTESIAN_POINT('Ctrl Pts',(0.306800021331985,2.20172479472154,9.6684354142871));
#64872=CARTESIAN_POINT('Ctrl Pts',(0.298083129666597,2.22498148203089,9.66983795219054));
#64873=CARTESIAN_POINT('Ctrl Pts',(0.286265095832769,2.24803648785005,9.67141335290156));
#64874=CARTESIAN_POINT('Ctrl Pts',(0.285733281451517,2.24906038589736,9.67148370389835));
#64875=CARTESIAN_POINT('Ctrl Pts',(0.28495057673139,2.25054774042919,9.67158647004403));
#64876=CARTESIAN_POINT('Ctrl Pts',(0.284704025456033,2.25101348023208,9.67161873158768));
#64877=CARTESIAN_POINT('Ctrl Pts',(0.284269884461784,2.2518287382732,9.67167534896254));
#64878=CARTESIAN_POINT('Ctrl Pts',(0.284082789190552,2.25217851970955,9.6716996872001));
#64879=CARTESIAN_POINT('Ctrl Pts',(0.283718663239946,2.25285625485431,9.67174693631743));
#64880=CARTESIAN_POINT('Ctrl Pts',(0.283541708444874,2.25318424882833,9.67176984446861));
#64881=CARTESIAN_POINT('Ctrl Pts',(0.283118528240819,2.25396538753692,9.67182450147889));
#64882=CARTESIAN_POINT('Ctrl Pts',(0.28287178384129,2.25441824857883,9.67185626882006));
#64883=CARTESIAN_POINT('Ctrl Pts',(0.282124383929233,2.2557821823214,9.67195218965671));
#64884=CARTESIAN_POINT('Ctrl Pts',(0.281620409717601,2.2566914200783,9.67201646177737));
#64885=CARTESIAN_POINT('Ctrl Pts',(0.276344230003707,2.26610268074635,9.67268517407986));
#64886=CARTESIAN_POINT('Ctrl Pts',(0.271193412625119,2.27438558959964,9.67330326804845));
#64887=CARTESIAN_POINT('Ctrl Pts',(0.261509293112508,2.28848936287505,9.67441054044638));
#64888=CARTESIAN_POINT('Ctrl Pts',(0.257136625599697,2.29441217568341,9.67489382549423));
#64889=CARTESIAN_POINT('Ctrl Pts',(0.238615214911081,2.31778049432349,9.67687366376702));
#64890=CARTESIAN_POINT('Ctrl Pts',(0.222864766559749,2.33387339158329,9.67841484158103));
#64891=CARTESIAN_POINT('Ctrl Pts',(0.197911726851365,2.35454078085146,9.68057325155991));
#64892=CARTESIAN_POINT('Ctrl Pts',(0.189963004524117,2.3605266976066,9.6812247720704));
#64893=CARTESIAN_POINT('Ctrl Pts',(0.180958338940764,2.36667615704189,9.68191393890143));
#64894=CARTESIAN_POINT('Ctrl Pts',(0.180164898438415,2.36721284136648,9.68197426281579));
#64895=CARTESIAN_POINT('Ctrl Pts',(0.178787591654736,2.36813553018986,9.68207826765918));
#64896=CARTESIAN_POINT('Ctrl Pts',(0.178204844040433,2.3685231816104,9.68212205462098));
#64897=CARTESIAN_POINT('Ctrl Pts',(0.177368225348745,2.36907578841551,9.6821845999154));
#64898=CARTESIAN_POINT('Ctrl Pts',(0.177115382723512,2.36924228583061,9.68220346099222));
#64899=CARTESIAN_POINT('Ctrl Pts',(0.176678980784834,2.36952877669255,9.6822359431325));
#64900=CARTESIAN_POINT('Ctrl Pts',(0.176495533225426,2.36964893930644,9.68224957563233));
#64901=CARTESIAN_POINT('Ctrl Pts',(0.176140324807471,2.36988109167672,9.68227592976769));
#64902=CARTESIAN_POINT('Ctrl Pts',(0.175968579954325,2.36999310461074,9.68228865298913));
#64903=CARTESIAN_POINT('Ctrl Pts',(0.17556363916719,2.37025665870057,9.68231860712343));
#64904=CARTESIAN_POINT('Ctrl Pts',(0.175330353299151,2.37040806234831,9.68233582875854));
#64905=CARTESIAN_POINT('Ctrl Pts',(0.174640333455753,2.37085462018545,9.68238666526919));
#64906=CARTESIAN_POINT('Ctrl Pts',(0.174183045180023,2.37114892241593,9.68242022347555));
#64907=CARTESIAN_POINT('Ctrl Pts',(0.170154189514572,2.37372742101109,9.68271474276128));
#64908=CARTESIAN_POINT('Ctrl Pts',(0.166538410301764,2.37594222461734,9.68297120683739));
#64909=CARTESIAN_POINT('Ctrl Pts',(0.162356524760671,2.37839163458479,9.68326020257542));
#64910=CARTESIAN_POINT('Ctrl Pts',(0.161832410481271,2.37869663483361,9.68329628750687));
#64911=CARTESIAN_POINT('Ctrl Pts',(0.15904979780779,2.38030543720248,9.68348717209885));
#64912=CARTESIAN_POINT('Ctrl Pts',(0.15677633734971,2.38158330403717,9.68364070339821));
#64913=CARTESIAN_POINT('Ctrl Pts',(0.149981342156572,2.3852948244332,9.68409317572655));
#64914=CARTESIAN_POINT('Ctrl Pts',(0.145416761874995,2.38764823919489,9.68438882259132));
#64915=CARTESIAN_POINT('Ctrl Pts',(0.121561678236722,2.39923443416423,9.68590119894104));
#64916=CARTESIAN_POINT('Ctrl Pts',(0.101443229204911,2.406639562047,9.68707168908333));
#64917=CARTESIAN_POINT('Ctrl Pts',(0.0695304733343461,2.41489797057564,
9.6889442843749));
#64918=CARTESIAN_POINT('Ctrl Pts',(0.0581748171368487,2.41719216728342,
9.68961281322766));
#64919=CARTESIAN_POINT('Ctrl Pts',(0.0413260937403642,2.41966085187465,
9.69062409246578));
#64920=CARTESIAN_POINT('Ctrl Pts',(0.0359121933148562,2.42031424441174,
9.69095186100929));
#64921=CARTESIAN_POINT('Ctrl Pts',(0.0295793738233886,2.42091597502776,
9.69133939689434));
#64922=CARTESIAN_POINT('Ctrl Pts',(0.0286738354842033,2.42099815188848,
9.69139490884812));
#64923=CARTESIAN_POINT('Ctrl Pts',(0.0272915038827543,2.42111770140799,
9.69147980256366));
#64924=CARTESIAN_POINT('Ctrl Pts',(0.0268149499466486,2.42115784716734,
9.69150909710441));
#64925=CARTESIAN_POINT('Ctrl Pts',(0.0259861122009029,2.42122581228064,
9.69156009594456));
#64926=CARTESIAN_POINT('Ctrl Pts',(0.0256338678025295,2.42125411331618,
9.69158178506865));
#64927=CARTESIAN_POINT('Ctrl Pts',(0.0248995719417467,2.42131189485429,
9.69162703090765));
#64928=CARTESIAN_POINT('Ctrl Pts',(0.0245175132111387,2.42134127341768,
9.69165059079047));
#64929=CARTESIAN_POINT('Ctrl Pts',(0.0235826274313552,2.42141148485099,
9.69170828600677));
#64930=CARTESIAN_POINT('Ctrl Pts',(0.0230297471775385,2.42145157279051,
9.69174244468525));
#64931=CARTESIAN_POINT('Ctrl Pts',(0.0209124089596778,2.42159960503841,
9.69187340946448));
#64932=CARTESIAN_POINT('Ctrl Pts',(0.0193472941819304,2.42169755497616,
9.69197052875342));
#64933=CARTESIAN_POINT('Ctrl Pts',(-0.00686478916152614,2.42314601520544,
9.69360243189247));
#64934=CARTESIAN_POINT('Ctrl Pts',(-0.0315806032064484,2.42167164901584,
9.69523050539107));
#64935=CARTESIAN_POINT('Ctrl Pts',(-0.0716019339014607,2.41462541349623,
9.6979739930568));
#64936=CARTESIAN_POINT('Ctrl Pts',(-0.0870959446429602,2.41069327699743,
9.69906119939571));
#64937=CARTESIAN_POINT('Ctrl Pts',(-0.110216104805449,2.40295941855171,
9.70067542809187));
#64938=CARTESIAN_POINT('Ctrl Pts',(-0.118090272894714,2.39997785619139,
9.70122338454239));
#64939=CARTESIAN_POINT('Ctrl Pts',(-0.127048357691948,2.39617835001626,
9.70183762162377));
#64940=CARTESIAN_POINT('Ctrl Pts',(-0.128254220233477,2.39565817313808,
9.70192010783991));
#64941=CARTESIAN_POINT('Ctrl Pts',(-0.129812836578354,2.39497449746875,
9.70202643575861));
#64942=CARTESIAN_POINT('Ctrl Pts',(-0.130168498951857,2.39481772094273,
9.70205067931136));
#64943=CARTESIAN_POINT('Ctrl Pts',(-0.130743614574762,2.39456296547718,
9.70208984911431));
#64944=CARTESIAN_POINT('Ctrl Pts',(-0.130963242017428,2.39446538442401,
9.70210479970951));
#64945=CARTESIAN_POINT('Ctrl Pts',(-0.131384167197612,2.39427780217893,
9.70213343803841));
#64946=CARTESIAN_POINT('Ctrl Pts',(-0.131585481074299,2.39418784036079,
9.70214712808035));
#64947=CARTESIAN_POINT('Ctrl Pts',(-0.132048121301452,2.39398052885806,
9.70217857413504));
#64948=CARTESIAN_POINT('Ctrl Pts',(-0.132309384380341,2.39386303696335,
9.7021963213514));
#64949=CARTESIAN_POINT('Ctrl Pts',(-0.133117600435273,2.39349828002055,
9.7022511890696));
#64950=CARTESIAN_POINT('Ctrl Pts',(-0.133664023498712,2.39324983334435,
9.70228823720047));
#64951=CARTESIAN_POINT('Ctrl Pts',(-0.138156680864627,2.39119195371399,
9.70259248181589));
#64952=CARTESIAN_POINT('Ctrl Pts',(-0.142066911009777,2.38930437203179,
9.70285497621379));
#64953=CARTESIAN_POINT('Ctrl Pts',(-0.14689292630858,2.38685325666065,9.70317750791687));
#64954=CARTESIAN_POINT('Ctrl Pts',(-0.14784540715445,2.38636350727143,9.7032410929945));
#64955=CARTESIAN_POINT('Ctrl Pts',(-0.149430478977077,2.38553847395275,
9.70334681858821));
#64956=CARTESIAN_POINT('Ctrl Pts',(-0.150064419122236,2.38520581740939,
9.70338907886743));
#64957=CARTESIAN_POINT('Ctrl Pts',(-0.152724417639674,2.38379867384474,
9.70356632267326));
#64958=CARTESIAN_POINT('Ctrl Pts',(-0.154740126592792,2.38270466695156,
9.70370044158105));
#64959=CARTESIAN_POINT('Ctrl Pts',(-0.161481743353048,2.37895200834256,
9.7041489224728));
#64960=CARTESIAN_POINT('Ctrl Pts',(-0.166152336016913,2.37619555069267,
9.70445949578441));
#64961=CARTESIAN_POINT('Ctrl Pts',(-0.179231155407598,2.36802488752522,
9.70533497675114));
#64962=CARTESIAN_POINT('Ctrl Pts',(-0.187460092760589,2.36233541870357,
9.70589297686367));
#64963=CARTESIAN_POINT('Ctrl Pts',(-0.203056072827663,2.3504432621868,9.70698924188116));
#64964=CARTESIAN_POINT('Ctrl Pts',(-0.210435944569906,2.34427505366086,
9.70752688782505));
#64965=CARTESIAN_POINT('Ctrl Pts',(-0.228924020742574,2.32736201188725,
9.70894832220236));
#64966=CARTESIAN_POINT('Ctrl Pts',(-0.239553668861767,2.3161333811544,9.70984326695604));
#64967=CARTESIAN_POINT('Ctrl Pts',(-0.250889476024387,2.30229100929007,
9.71092249646669));
#64968=CARTESIAN_POINT('Ctrl Pts',(-0.252420486900822,2.30037734128407,
9.71107117090017));
#64969=CARTESIAN_POINT('Ctrl Pts',(-0.25436524669452,2.29788885184356,9.71126390705666));
#64970=CARTESIAN_POINT('Ctrl Pts',(-0.254799161135035,2.29732983525618,
9.71130716515514));
#64971=CARTESIAN_POINT('Ctrl Pts',(-0.255496223572909,2.29642566974901,
9.71137707203077));
#64972=CARTESIAN_POINT('Ctrl Pts',(-0.255760523333499,2.29608140834261,
9.71140367521613));
#64973=CARTESIAN_POINT('Ctrl Pts',(-0.256263148569348,2.29542397290897,
9.71145445334595));
#64974=CARTESIAN_POINT('Ctrl Pts',(-0.25650159757932,2.29511089395335,9.71147862336127));
#64975=CARTESIAN_POINT('Ctrl Pts',(-0.25704470366133,2.2943950898266,9.71153385915595));
#64976=CARTESIAN_POINT('Ctrl Pts',(-0.257348988279848,2.29399208451827,
9.71156493947937));
#64977=CARTESIAN_POINT('Ctrl Pts',(-0.258276833755342,2.29275718830385,
9.71166012255043));
#64978=CARTESIAN_POINT('Ctrl Pts',(-0.258897312791394,2.2919229998888,9.71172434552073));
#64979=CARTESIAN_POINT('Ctrl Pts',(-0.263452869759912,2.28573609627654,
9.71220014117438));
#64980=CARTESIAN_POINT('Ctrl Pts',(-0.267225378558869,2.28026618793135,
9.71261795633226));
#64981=CARTESIAN_POINT('Ctrl Pts',(-0.271829750123041,2.27312767567176,
9.7131602462047));
#64982=CARTESIAN_POINT('Ctrl Pts',(-0.272820089718979,2.27156282685928,
9.71327894152324));
#64983=CARTESIAN_POINT('Ctrl Pts',(-0.281416262211291,2.25771724002261,
9.71432756605408));
#64984=CARTESIAN_POINT('Ctrl Pts',(-0.288201062742526,2.24494792928204,
9.71528495834222));
#64985=CARTESIAN_POINT('Ctrl Pts',(-0.300859456614982,2.21669440842931,
9.7173676534232));
#64986=CARTESIAN_POINT('Ctrl Pts',(-0.306444003449681,2.20112404943818,
9.71849456135099));
#64987=CARTESIAN_POINT('Ctrl Pts',(-0.312946266858358,2.17740212115723,
9.72013459231386));
#64988=CARTESIAN_POINT('Ctrl Pts',(-0.314788507213134,2.16953179872205,
9.72066632354187));
#64989=CARTESIAN_POINT('Ctrl Pts',(-0.316979362341212,2.15828114388953,
9.72140167119534));
#64990=CARTESIAN_POINT('Ctrl Pts',(-0.31757340398167,2.15495219027247,9.72161621065504));
#64991=CARTESIAN_POINT('Ctrl Pts',(-0.31819849644698,2.15109955449355,9.72186051960799));
#64992=CARTESIAN_POINT('Ctrl Pts',(-0.318280772477322,2.15058455783018,
9.72189309549596));
#64993=CARTESIAN_POINT('Ctrl Pts',(-0.318403650038842,2.14980325121976,
9.72194239029906));
#64994=CARTESIAN_POINT('Ctrl Pts',(-0.318445167899288,2.14953708946823,
9.72195916095425));
#64995=CARTESIAN_POINT('Ctrl Pts',(-0.318516492815986,2.14907604605006,
9.72198817209834));
#64996=CARTESIAN_POINT('Ctrl Pts',(-0.318546454713478,2.14888118944879,
9.72200042141288));
#64997=CARTESIAN_POINT('Ctrl Pts',(-0.318608694726064,2.14847392523885,
9.72202599815512));
#64998=CARTESIAN_POINT('Ctrl Pts',(-0.318640939144057,2.14826151349862,
9.72203932361471));
#64999=CARTESIAN_POINT('Ctrl Pts',(-0.318719844368782,2.14773819508709,
9.72207211869405));
#65000=CARTESIAN_POINT('Ctrl Pts',(-0.318766262804444,2.14742725128325,
9.72209157450558));
#65001=CARTESIAN_POINT('Ctrl Pts',(-0.318945597953094,2.14621377924434,
9.72216738532989));
#65002=CARTESIAN_POINT('Ctrl Pts',(-0.319075138935293,2.1453107449331,9.7222235507548));
#65003=CARTESIAN_POINT('Ctrl Pts',(-0.321235572864455,2.12978143980146,
9.7231852928539));
#65004=CARTESIAN_POINT('Ctrl Pts',(-0.322262972831485,2.11503094359889,
9.7240362840308));
#65005=CARTESIAN_POINT('Ctrl Pts',(-0.322300767273116,2.06820607996235,
9.72668330494058));
#65006=CARTESIAN_POINT('Ctrl Pts',(-0.317544968751828,2.03633060995106,
9.72842447962931));
#65007=CARTESIAN_POINT('Ctrl Pts',(-0.307477373763807,2.00343735682915,
9.7304832467373));
#65008=CARTESIAN_POINT('Ctrl Pts',(-0.306766309896965,2.00120166950783,
9.73062441121389));
#65009=CARTESIAN_POINT('Ctrl Pts',(-0.305444310734931,1.99719703144561,
9.73087960000979));
#65010=CARTESIAN_POINT('Ctrl Pts',(-0.304842251356212,1.99542524748887,
9.730993331519));
#65011=CARTESIAN_POINT('Ctrl Pts',(-0.304006080716402,1.99303309904718,
9.73114804232437));
#65012=CARTESIAN_POINT('Ctrl Pts',(-0.303785427008262,1.9924080424053,9.73118857507883));
#65013=CARTESIAN_POINT('Ctrl Pts',(-0.303434701125111,1.99142420426905,
9.7312525448391));
#65014=CARTESIAN_POINT('Ctrl Pts',(-0.303305916509385,1.99106496305656,
9.7312759389906));
#65015=CARTESIAN_POINT('Ctrl Pts',(-0.303056524254529,1.99037316079052,
9.73132105974718));
#65016=CARTESIAN_POINT('Ctrl Pts',(-0.302936006472565,1.99004056771163,
9.73134278333345));
#65017=CARTESIAN_POINT('Ctrl Pts',(-0.302650155580088,1.9892557414458,9.73139411890376));
#65018=CARTESIAN_POINT('Ctrl Pts',(-0.302484356422846,1.98880367995816,
9.73142374640063));
#65019=CARTESIAN_POINT('Ctrl Pts',(-0.301997176602442,1.9874845072084,9.73151037401496));
#65020=CARTESIAN_POINT('Ctrl Pts',(-0.301673078094324,1.98661841102477,
9.73156746486838));
#65021=CARTESIAN_POINT('Ctrl Pts',(-0.299281311234648,1.98030969217412,
9.73198491353995));
#65022=CARTESIAN_POINT('Ctrl Pts',(-0.297070335008483,1.97492289594797,
9.73235006275498));
#65023=CARTESIAN_POINT('Ctrl Pts',(-0.289269990753396,1.95729357993644,
9.73357532485345));
#65024=CARTESIAN_POINT('Ctrl Pts',(-0.283060489148429,1.94534253341921,
9.73445601783751));
#65025=CARTESIAN_POINT('Ctrl Pts',(-0.261621058323524,1.90971991670575,
9.73723009563142));
#65026=CARTESIAN_POINT('Ctrl Pts',(-0.244028179681372,1.88762691483951,
9.73917902711662));
#65027=CARTESIAN_POINT('Ctrl Pts',(-0.221170331638683,1.8655684991073,9.74122155877672));
#65028=CARTESIAN_POINT('Ctrl Pts',(-0.218506355108674,1.86308351732256,
9.74145307689391));
#65029=CARTESIAN_POINT('Ctrl Pts',(-0.215371676566136,1.86025732501612,
9.74171745831677));
#65030=CARTESIAN_POINT('Ctrl Pts',(-0.214941627583548,1.85987168842602,
9.74175355710316));
#65031=CARTESIAN_POINT('Ctrl Pts',(-0.214300963401061,1.85930028755412,
9.74180707716083));
#65032=CARTESIAN_POINT('Ctrl Pts',(-0.214091141458655,1.8591136416554,9.74182456441686));
#65033=CARTESIAN_POINT('Ctrl Pts',(-0.213717169702861,1.85878185182211,
9.74185565924366));
#65034=CARTESIAN_POINT('Ctrl Pts',(-0.213553115917034,1.85863660111901,
9.74186927488278));
#65035=CARTESIAN_POINT('Ctrl Pts',(-0.213204708513569,1.85832875985435,
9.74189813777571));
#65036=CARTESIAN_POINT('Ctrl Pts',(-0.213020317505783,1.85816621332701,
9.74191338170609));
#65037=CARTESIAN_POINT('Ctrl Pts',(-0.212525516932343,1.85773103591591,
9.74195420407385));
#65038=CARTESIAN_POINT('Ctrl Pts',(-0.212214767481759,1.85745878953687,
9.74197975365453));
#65039=CARTESIAN_POINT('Ctrl Pts',(-0.210729671253993,1.85616274171573,
9.74210144243915));
#65040=CARTESIAN_POINT('Ctrl Pts',(-0.209548408523966,1.85514684484544,
9.74219700117327));
#65041=CARTESIAN_POINT('Ctrl Pts',(-0.199734165937715,1.84682955171127,
9.74298125232645));
#65042=CARTESIAN_POINT('Ctrl Pts',(-0.19072877516724,1.83997768036777,9.74363963203563));
#65043=CARTESIAN_POINT('Ctrl Pts',(-0.15892139623462,1.81832030671233,9.74583449180678));
#65044=CARTESIAN_POINT('Ctrl Pts',(-0.134618638082729,1.80592964816968,
9.74730762375319));
#65045=CARTESIAN_POINT('Ctrl Pts',(-0.106281484435177,1.79574013115965,
9.74905205083636));
#65046=CARTESIAN_POINT('Ctrl Pts',(-0.103501078798846,1.79478311366284,
9.74922335098398));
#65047=CARTESIAN_POINT('Ctrl Pts',(-0.0990619497888775,1.79332279428349,
9.74949733525782));
#65048=CARTESIAN_POINT('Ctrl Pts',(-0.0974115587450161,1.79279458587281,
9.74959930415271));
#65049=CARTESIAN_POINT('Ctrl Pts',(-0.0896109569113862,1.79036717906932,
9.75008190877611));
#65050=CARTESIAN_POINT('Ctrl Pts',(-0.0834093462170028,1.78863930956249,
9.75046751725774));
#65051=CARTESIAN_POINT('Ctrl Pts',(-0.076160367902026,1.78685173636693,
9.75092193315365));
#65052=CARTESIAN_POINT('Ctrl Pts',(-0.0751590965736733,1.78660991269828,
9.75098477934524));
#65053=CARTESIAN_POINT('Ctrl Pts',(-0.073667119580352,1.78625713681564,
9.75107854952184));
#65054=CARTESIAN_POINT('Ctrl Pts',(-0.0731772788433954,1.78614252508037,
9.75110935569268));
#65055=CARTESIAN_POINT('Ctrl Pts',(-0.0723039980370705,1.78594035250311,
9.75116431261855));
#65056=CARTESIAN_POINT('Ctrl Pts',(-0.0719206614173105,1.78585234558072,
9.75118844898208));
#65057=CARTESIAN_POINT('Ctrl Pts',(-0.0711129818411954,1.7856684732704,
9.75123933012168));
#65058=CARTESIAN_POINT('Ctrl Pts',(-0.0706886042531613,1.78557276500231,
9.75126607988946));
#65059=CARTESIAN_POINT('Ctrl Pts',(-0.0695689524903573,1.78532263550188,
9.75133669605044));
#65060=CARTESIAN_POINT('Ctrl Pts',(-0.0688733608220415,1.78516965992118,
9.75138060872165));
#65061=CARTESIAN_POINT('Ctrl Pts',(-0.0657389434237606,1.78449121892634,
9.75157867745487));
#65062=CARTESIAN_POINT('Ctrl Pts',(-0.0632946256190451,1.78399178899606,
9.75173366448414));
#65063=CARTESIAN_POINT('Ctrl Pts',(-0.0452105093404361,1.78051502144944,
9.75288447522972));
#65064=CARTESIAN_POINT('Ctrl Pts',(-0.0293774122755313,1.77867232730593,
9.75391655261541));
#65065=CARTESIAN_POINT('Ctrl Pts',(0.0182164670955005,1.7766805863597,9.75708440028588));
#65066=CARTESIAN_POINT('Ctrl Pts',(0.0499282451455137,1.78003998795388,
9.75929698971051));
#65067=CARTESIAN_POINT('Ctrl Pts',(0.0821433670759884,1.78836550093969,
9.76140249415399));
#65068=CARTESIAN_POINT('Ctrl Pts',(0.0836461376065765,1.78876549411481,
9.7615003284772));
#65069=CARTESIAN_POINT('Ctrl Pts',(0.0855581871992815,1.78928927458937,
9.76162426648897));
#65070=CARTESIAN_POINT('Ctrl Pts',(0.0859701627662228,1.78940301128151,
9.76165093837499));
#65071=CARTESIAN_POINT('Ctrl Pts',(0.0866241935255073,1.78958497464807,
9.76169322881389));
#65072=CARTESIAN_POINT('Ctrl Pts',(0.086866395380693,1.78965266519142,9.7617088784478));
#65073=CARTESIAN_POINT('Ctrl Pts',(0.0873186854715271,1.78977964211888,
9.7617380810263));
#65074=CARTESIAN_POINT('Ctrl Pts',(0.0875287911310894,1.78983885801099,
9.76175163792258));
#65075=CARTESIAN_POINT('Ctrl Pts',(0.0880006895482849,1.78997237491008,
9.76178206715779));
#65076=CARTESIAN_POINT('Ctrl Pts',(0.0882624478338104,1.79004679388081,
9.76179893247027));
#65077=CARTESIAN_POINT('Ctrl Pts',(0.0890383013993388,1.79026843480901,
9.76184888207946));
#65078=CARTESIAN_POINT('Ctrl Pts',(0.0895521280628243,1.79041660580567,
9.76188191113579));
#65079=CARTESIAN_POINT('Ctrl Pts',(0.0936629554860278,1.79161312640784,
9.76214576469217));
#65080=CARTESIAN_POINT('Ctrl Pts',(0.0972419811627356,1.79272290501854,
9.76237307565771));
#65081=CARTESIAN_POINT('Ctrl Pts',(0.11156924178437,1.79744090082164,9.76327632329368));
#65082=CARTESIAN_POINT('Ctrl Pts',(0.122143946869559,1.80155300183936,9.76392779428118));
#65083=CARTESIAN_POINT('Ctrl Pts',(0.163961068408712,1.82041017204418,9.76652284785366));
#65084=CARTESIAN_POINT('Ctrl Pts',(0.192951955020495,1.83957111075647,9.76839450543246));
#65085=CARTESIAN_POINT('Ctrl Pts',(0.218703677811659,1.86329320329376,9.77051183125216));
#65086=CARTESIAN_POINT('Ctrl Pts',(0.219056193903442,1.86361939545728,9.77054090819852));
#65087=CARTESIAN_POINT('Ctrl Pts',(0.22058720489933,1.86504244508946,9.77066759887071));
#65088=CARTESIAN_POINT('Ctrl Pts',(0.221758184847625,1.86614732226996,9.7707655495504));
#65089=CARTESIAN_POINT('Ctrl Pts',(0.223370552162238,1.86769167069714,9.77090191309662));
#65090=CARTESIAN_POINT('Ctrl Pts',(0.223819031526821,1.86812373007451,9.77094000462172));
#65091=CARTESIAN_POINT('Ctrl Pts',(0.224534650771843,1.86881715914905,9.77100104697609));
#65092=CARTESIAN_POINT('Ctrl Pts',(0.224802594727857,1.86907769985801,9.77102396159791));
#65093=CARTESIAN_POINT('Ctrl Pts',(0.225347931006958,1.86960981723044,9.77107071967927));
#65094=CARTESIAN_POINT('Ctrl Pts',(0.225625286996249,1.86988143014629,9.7710945647096));
#65095=CARTESIAN_POINT('Ctrl Pts',(0.226264064954431,1.87050924628127,9.77114963059154));
#65096=CARTESIAN_POINT('Ctrl Pts',(0.22662513699759,1.87086580262165,9.77118086696125));
#65097=CARTESIAN_POINT('Ctrl Pts',(0.227382268672478,1.87161700560702,9.77124659932501));
#65098=CARTESIAN_POINT('Ctrl Pts',(0.227778146090162,1.8720118327808,9.77128110326399));
#65099=CARTESIAN_POINT('Ctrl Pts',(0.228825916945846,1.87306227691534,9.77137278497359));
#65100=CARTESIAN_POINT('Ctrl Pts',(0.22947601639894,1.87371966878665,9.77143004166578));
#65101=CARTESIAN_POINT('Ctrl Pts',(0.243259384165461,1.88777813655942,9.7726519915521));
#65102=CARTESIAN_POINT('Ctrl Pts',(0.255197887340063,1.90229551906481,9.77386903115211));
#65103=CARTESIAN_POINT('Ctrl Pts',(0.281626223112089,1.94084367876889,9.77698851182424));
#65104=CARTESIAN_POINT('Ctrl Pts',(0.294374741620874,1.9658822423925,9.77892701233516));
#65105=CARTESIAN_POINT('Ctrl Pts',(0.304950197733185,1.99569331770424,9.78096102740234));
#65106=CARTESIAN_POINT('Ctrl Pts',(0.3061124275919,1.99915511147793,9.78119310223587));
#65107=CARTESIAN_POINT('Ctrl Pts',(0.307390263170965,2.00318710904358,9.78145805059677));
#65108=CARTESIAN_POINT('Ctrl Pts',(0.307563414212104,2.00373860587871,9.78149417505562));
#65109=CARTESIAN_POINT('Ctrl Pts',(0.307818505013988,2.00455880081039,9.78154772576481));
#65110=CARTESIAN_POINT('Ctrl Pts',(0.307901577571977,2.00482714114871,9.78156521810957));
#65111=CARTESIAN_POINT('Ctrl Pts',(0.308048827702213,2.00530499806484,9.78159631860327));
#65112=CARTESIAN_POINT('Ctrl Pts',(0.308113142402317,2.00551447137122,9.78160993483173));
#65113=CARTESIAN_POINT('Ctrl Pts',(0.308249136583684,2.00595902053908,9.78163879538399));
#65114=CARTESIAN_POINT('Ctrl Pts',(0.30832076062506,2.00619411217248,9.78165403639164));
#65115=CARTESIAN_POINT('Ctrl Pts',(0.30851200583889,2.00682442174181,9.78169484274036));
#65116=CARTESIAN_POINT('Ctrl Pts',(0.308631136977836,2.00721978970296,9.78172037926421));
#65117=CARTESIAN_POINT('Ctrl Pts',(0.309195461631544,2.00910576352573,9.78184191345836));
#65118=CARTESIAN_POINT('Ctrl Pts',(0.309630627898888,2.01059938359611,9.7819373324459));
#65119=CARTESIAN_POINT('Ctrl Pts',(0.313130584089651,2.02294444683579,9.78271959206433));
#65120=CARTESIAN_POINT('Ctrl Pts',(0.315635098361298,2.03394801525893,9.78337628213403));
#65121=CARTESIAN_POINT('Ctrl Pts',(0.322155219336695,2.07163582938955,9.78555813824877));
#65122=CARTESIAN_POINT('Ctrl Pts',(0.323398923842031,2.09868184702976,9.78702067276346));
#65123=CARTESIAN_POINT('Ctrl Pts',(0.320378619023862,2.13663214696955,9.78922402044224));
#65124=CARTESIAN_POINT('Ctrl Pts',(0.318927124970838,2.14764264086941,9.7898800679227));
#65125=CARTESIAN_POINT('Ctrl Pts',(0.316694071962356,2.15972823985174,9.7906272109261));
#65126=CARTESIAN_POINT('Ctrl Pts',(0.316470883100705,2.16089973679362,9.79069991398587));
#65127=CARTESIAN_POINT('Ctrl Pts',(0.316148607372668,2.16254170449757,9.79080221637746));
#65128=CARTESIAN_POINT('Ctrl Pts',(0.31605496024707,2.16301324340491,9.79083164208852));
#65129=CARTESIAN_POINT('Ctrl Pts',(0.315881412704016,2.16387698285339,9.79088562862509));
#65130=CARTESIAN_POINT('Ctrl Pts',(0.315801835935989,2.16426924807016,9.79091017906894));
#65131=CARTESIAN_POINT('Ctrl Pts',(0.315640920104777,2.16505495053901,9.79095941904348));
#65132=CARTESIAN_POINT('Ctrl Pts',(0.315559575688438,2.16544838594824,9.79098410870578));
#65133=CARTESIAN_POINT('Ctrl Pts',(0.315359149252482,2.16640872053921,9.79104445484282));
#65134=CARTESIAN_POINT('Ctrl Pts',(0.315239274383579,2.16697545117448,9.79108013664686));
#65135=CARTESIAN_POINT('Ctrl Pts',(0.314979858368417,2.16818576181493,9.79115648794718));
#65136=CARTESIAN_POINT('Ctrl Pts',(0.314839871428315,2.16882924262811,9.79119717161536));
#65137=CARTESIAN_POINT('Ctrl Pts',(0.314446231074637,2.1706123680326,9.79131016129677));
#65138=CARTESIAN_POINT('Ctrl Pts',(0.314188357284911,2.17175106163078,9.79138260254216));
#65139=CARTESIAN_POINT('Ctrl Pts',(0.313346532433743,2.17537673570273,9.79161418765129));
#65140=CARTESIAN_POINT('Ctrl Pts',(0.312739206997953,2.17785813685601,9.79177407938707));
#65141=CARTESIAN_POINT('Ctrl Pts',(0.310268245600061,2.18745821073826,9.79239822090368));
#65142=CARTESIAN_POINT('Ctrl Pts',(0.308190632893165,2.19451900712157,9.79286924683453));
#65143=CARTESIAN_POINT('Ctrl Pts',(0.301226618323582,2.21550484502384,9.79430584212117));
#65144=CARTESIAN_POINT('Ctrl Pts',(0.29562429095259,2.22917059562471,9.7952918092807));
#65145=CARTESIAN_POINT('Ctrl Pts',(0.278418297757441,2.26410209784424,9.79792124053179));
#65146=CARTESIAN_POINT('Ctrl Pts',(0.265320475326925,2.28453050723108,9.79957735230041));
#65147=CARTESIAN_POINT('Ctrl Pts',(0.249241907795073,2.30430693640791,9.80118637676125));
#65148=CARTESIAN_POINT('Ctrl Pts',(0.248418858778753,2.30530690101256,9.80126773464385));
#65149=CARTESIAN_POINT('Ctrl Pts',(0.247331879236521,2.30661142141867,9.80137384056511));
#65150=CARTESIAN_POINT('Ctrl Pts',(0.247073388823163,2.30692046415704,9.80139897491786));
#65151=CARTESIAN_POINT('Ctrl Pts',(0.246673365335428,2.30739690091608,9.80143771872869));
#65152=CARTESIAN_POINT('Ctrl Pts',(0.246532241046418,2.30756463523639,9.80145135798197));
#65153=CARTESIAN_POINT('Ctrl Pts',(0.246250265723156,2.30789908583057,9.80147855169367));
#65154=CARTESIAN_POINT('Ctrl Pts',(0.246109417455107,2.30806580184707,9.80149210610182));
#65155=CARTESIAN_POINT('Ctrl Pts',(0.245792941783322,2.30843962946974,9.80152249697373));
#65156=CARTESIAN_POINT('Ctrl Pts',(0.245617222328977,2.30864666175303,9.80153932648921));
#65157=CARTESIAN_POINT('Ctrl Pts',(0.245096504855787,2.30925860054939,9.80158906704795));
#65158=CARTESIAN_POINT('Ctrl Pts',(0.244750763626019,2.30966287775965,9.80162192354511));
#65159=CARTESIAN_POINT('Ctrl Pts',(0.242015102189969,2.31284571408807,9.80188058045424));
#65160=CARTESIAN_POINT('Ctrl Pts',(0.239578821676315,2.31558431919263,9.8021030208893));
#65161=CARTESIAN_POINT('Ctrl Pts',(0.230729078116558,2.32519689068969,9.8028858984349));
#65162=CARTESIAN_POINT('Ctrl Pts',(0.224061794823854,2.33183159833205,9.80343025197276));
#65163=CARTESIAN_POINT('Ctrl Pts',(0.205783185856824,2.34849449029425,9.80483885472536));
#65164=CARTESIAN_POINT('Ctrl Pts',(0.193730038034315,2.35800181279671,9.80568719428609));
#65165=CARTESIAN_POINT('Ctrl Pts',(0.162787017217855,2.37901372553495,9.80778553300111));
#65166=CARTESIAN_POINT('Ctrl Pts',(0.143306339627397,2.38950189517053,9.80904601614843));
#65167=CARTESIAN_POINT('Ctrl Pts',(0.121694501942709,2.39841807773674,9.81046581508964));
#65168=CARTESIAN_POINT('Ctrl Pts',(0.120477235076516,2.3989115867137,9.81054583182497));
#65169=CARTESIAN_POINT('Ctrl Pts',(0.118779274795616,2.3995879235457,9.81065752485154));
#65170=CARTESIAN_POINT('Ctrl Pts',(0.118301097827358,2.39977706767429,9.81068898823407));
#65171=CARTESIAN_POINT('Ctrl Pts',(0.117475953634054,2.40010117384551,9.81074329712354));
#65172=CARTESIAN_POINT('Ctrl Pts',(0.117129200448578,2.40023668101362,9.81076612425621));
#65173=CARTESIAN_POINT('Ctrl Pts',(0.116419688903491,2.40051253376765,9.81081284214876));
#65174=CARTESIAN_POINT('Ctrl Pts',(0.116056909790656,2.40065282404065,9.81083673472225));
#65175=CARTESIAN_POINT('Ctrl Pts',(0.115225767745568,2.40097250641598,9.8108914862161));
#65176=CARTESIAN_POINT('Ctrl Pts',(0.114757239124534,2.40115146228244,9.81092235970036));
#65177=CARTESIAN_POINT('Ctrl Pts',(0.113764403587105,2.40152802531138,9.8109878023171));
#65178=CARTESIAN_POINT('Ctrl Pts',(0.113239995765255,2.40172536009499,9.81102238046181));
#65179=CARTESIAN_POINT('Ctrl Pts',(0.11184622637586,2.40224569043652,9.8111143149589));
#65180=CARTESIAN_POINT('Ctrl Pts',(0.110975985405429,2.40256630079437,9.81117175081183));
#65181=CARTESIAN_POINT('Ctrl Pts',(0.108346120928033,2.40352231171719,9.81134542986833));
#65182=CARTESIAN_POINT('Ctrl Pts',(0.106582360375462,2.40414614225624,9.81146205638334));
#65183=CARTESIAN_POINT('Ctrl Pts',(0.10025131831194,2.40632355799008,9.8118812592682));
#65184=CARTESIAN_POINT('Ctrl Pts',(0.0956548951231364,2.40778984065767,
9.81218667542687));
#65185=CARTESIAN_POINT('Ctrl Pts',(0.080153260606281,2.41235417541674,9.81322065839277));
#65186=CARTESIAN_POINT('Ctrl Pts',(0.0691187538204526,2.41497972720595,
9.81396350932832));
#65187=CARTESIAN_POINT('Ctrl Pts',(0.0305340384473812,2.42203530744081,
9.81657670303438));
#65188=CARTESIAN_POINT('Ctrl Pts',(0.00256458125903367,2.42346938800602,
9.81850897116996));
#65189=CARTESIAN_POINT('Ctrl Pts',(-0.0262775840383949,2.42120359299221,
9.82037856688336));
#65190=CARTESIAN_POINT('Ctrl Pts',(-0.0273151276336311,2.42111702451621,
9.82044563888817));
#65191=CARTESIAN_POINT('Ctrl Pts',(-0.0317707886967957,2.42072351050581,
9.82073283700814));
#65192=CARTESIAN_POINT('Ctrl Pts',(-0.0351844622785023,2.4203669913696,
9.82095075277452));
#65193=CARTESIAN_POINT('Ctrl Pts',(-0.0391551363605281,2.41988806278194,
9.8212012476538));
#65194=CARTESIAN_POINT('Ctrl Pts',(-0.0397181435593944,2.41981864626323,
9.82123669569291));
#65195=CARTESIAN_POINT('Ctrl Pts',(-0.0405575357942016,2.41971290186362,
9.82128943812064));
#65196=CARTESIAN_POINT('Ctrl Pts',(-0.0408340579087389,2.41967770182461,
9.82130679574245));
#65197=CARTESIAN_POINT('Ctrl Pts',(-0.0413276357228092,2.41961422068304,
9.82133774673884));
#65198=CARTESIAN_POINT('Ctrl Pts',(-0.0415447080740114,2.4195860772458,
9.82135134789764));
#65199=CARTESIAN_POINT('Ctrl Pts',(-0.0420067188432984,2.41952569885671,
9.82138027294159));
#65200=CARTESIAN_POINT('Ctrl Pts',(-0.0422516482006496,2.41949340350492,
9.82139559331395));
#65201=CARTESIAN_POINT('Ctrl Pts',(-0.0429115727820625,2.41940561649061,
9.82143683486676));
#65202=CARTESIAN_POINT('Ctrl Pts',(-0.0433264991968739,2.41934959745774,
9.82146272614848));
#65203=CARTESIAN_POINT('Ctrl Pts',(-0.0453456446989847,2.41907298585237,
9.82158853414293));
#65204=CARTESIAN_POINT('Ctrl Pts',(-0.0469483314443001,2.41884110811782,
9.82168782168162));
#65205=CARTESIAN_POINT('Ctrl Pts',(-0.0561712425098101,2.4174356801978,
9.82225624082922));
#65206=CARTESIAN_POINT('Ctrl Pts',(-0.0637497986412662,2.41600095528132,
9.82271172595628));
#65207=CARTESIAN_POINT('Ctrl Pts',(-0.0876204508400575,2.41058800460521,
9.82413005955618));
#65208=CARTESIAN_POINT('Ctrl Pts',(-0.103657548743789,2.40560994981487,
9.82505945897578));
#65209=CARTESIAN_POINT('Ctrl Pts',(-0.127451694350232,2.3961341862218,9.82649228668662));
#65210=CARTESIAN_POINT('Ctrl Pts',(-0.135529663329763,2.39252537164029,
9.82698860603385));
#65211=CARTESIAN_POINT('Ctrl Pts',(-0.157593381427512,2.38155817281449,
9.82839101693977));
#65212=CARTESIAN_POINT('Ctrl Pts',(-0.171200041977602,2.37349793258629,
9.82931164810513));
#65213=CARTESIAN_POINT('Ctrl Pts',(-0.184664880412759,2.364122009939,9.83030846627022));
#65214=CARTESIAN_POINT('Ctrl Pts',(-0.185168795053712,2.36376897376731,
9.83034590089087));
#65215=CARTESIAN_POINT('Ctrl Pts',(-0.186323926310053,2.36295476203241,
9.83043201224257));
#65216=CARTESIAN_POINT('Ctrl Pts',(-0.186974445283326,2.36249260786568,
9.83048072605661));
#65217=CARTESIAN_POINT('Ctrl Pts',(-0.188031682064817,2.36173558131828,
9.83056025861495));
#65218=CARTESIAN_POINT('Ctrl Pts',(-0.188439441338247,2.36144216364572,
9.83059102129112));
#65219=CARTESIAN_POINT('Ctrl Pts',(-0.189152804213951,2.36092630215752,
9.83064499532782));
#65220=CARTESIAN_POINT('Ctrl Pts',(-0.189458706395216,2.36070427128975,
9.83066819068289));
#65221=CARTESIAN_POINT('Ctrl Pts',(-0.190105498825275,2.36023307482224,
9.83071734153009));
#65222=CARTESIAN_POINT('Ctrl Pts',(-0.190446291167721,2.35998377659539,
9.83074330214249));
#65223=CARTESIAN_POINT('Ctrl Pts',(-0.191326213007467,2.359337432986,9.8308104964579));
#65224=CARTESIAN_POINT('Ctrl Pts',(-0.191864594848648,2.35893937739228,
9.83085176945416));
#65225=CARTESIAN_POINT('Ctrl Pts',(-0.193033805870256,2.35806926627845,
9.83094175359172));
#65226=CARTESIAN_POINT('Ctrl Pts',(-0.193664150981611,2.35759657026664,
9.83099048967102));
#65227=CARTESIAN_POINT('Ctrl Pts',(-0.195487387279479,2.3562188500057,9.83113211065772));
#65228=CARTESIAN_POINT('Ctrl Pts',(-0.196675700259383,2.3553078269252,9.83122523124823));
#65229=CARTESIAN_POINT('Ctrl Pts',(-0.200677259442015,2.35219550578571,
9.83154161715574));
#65230=CARTESIAN_POINT('Ctrl Pts',(-0.203460160790687,2.349955789927,9.83176640025358));
#65231=CARTESIAN_POINT('Ctrl Pts',(-0.215004127988372,2.34034452341427,
9.83271936626098));
#65232=CARTESIAN_POINT('Ctrl Pts',(-0.22340551048689,2.33255578609056,9.83346416268097));
#65233=CARTESIAN_POINT('Ctrl Pts',(-0.25249579373195,2.30255304101051,9.83623390624631));
#65234=CARTESIAN_POINT('Ctrl Pts',(-0.270433535774029,2.27789720867154,
9.83834498563828));
#65235=CARTESIAN_POINT('Ctrl Pts',(-0.286458392377609,2.24770748579684,
9.84054561332755));
#65236=CARTESIAN_POINT('Ctrl Pts',(-0.28819757730976,2.24428468938073,9.84078981356777));
#65237=CARTESIAN_POINT('Ctrl Pts',(-0.2901316535362,2.24030375416991,9.84106708524926));
#65238=CARTESIAN_POINT('Ctrl Pts',(-0.290386588485125,2.23977535211428,
9.84110375283607));
#65239=CARTESIAN_POINT('Ctrl Pts',(-0.290762191932402,2.23899137829089,
9.84115795153868));
#65240=CARTESIAN_POINT('Ctrl Pts',(-0.290883967651328,2.23873634297265,
9.84117555108893));
#65241=CARTESIAN_POINT('Ctrl Pts',(-0.291099651241241,2.23828310372187,
9.84120677131972));
#65242=CARTESIAN_POINT('Ctrl Pts',(-0.291193692243867,2.23808496415691,
9.84122040031466));
#65243=CARTESIAN_POINT('Ctrl Pts',(-0.291392261997477,2.23766548292999,
9.8412492132196));
#65244=CARTESIAN_POINT('Ctrl Pts',(-0.291496740571661,2.23744411875162,
9.84126439396475));
#65245=CARTESIAN_POINT('Ctrl Pts',(-0.291774925424906,2.236852970124,9.84130487012847));
#65246=CARTESIAN_POINT('Ctrl Pts',(-0.291948181635381,2.23648297250073,
9.84133013753929));
#65247=CARTESIAN_POINT('Ctrl Pts',(-0.292758067308076,2.23474482098909,
9.84144853012219));
#65248=CARTESIAN_POINT('Ctrl Pts',(-0.293385799449378,2.23337250709149,
9.84154111229115));
#65249=CARTESIAN_POINT('Ctrl Pts',(-0.298375254537974,2.22225912972098,
9.8422840919691));
#65250=CARTESIAN_POINT('Ctrl Pts',(-0.302260753147022,2.21231017605921,
9.84290744226122));
#65251=CARTESIAN_POINT('Ctrl Pts',(-0.3166513036255,2.16926687404924,9.84550322046113));
#65252=CARTESIAN_POINT('Ctrl Pts',(-0.322266174513031,2.1347901479798,9.84736301833545));
#65253=CARTESIAN_POINT('Ctrl Pts',(-0.322274989605974,2.10008185028294,
9.84943323242055));
#65254=CARTESIAN_POINT('',(-0.322761847823037,2.10004974457569,10.0997435871451));
#65255=CARTESIAN_POINT('Ctrl Pts',(-0.322274989668007,2.10008160567334,
9.84943324701056));
#65256=CARTESIAN_POINT('Ctrl Pts',(-0.322276075480573,2.09579354310276,
9.84968901325225));
#65257=CARTESIAN_POINT('Ctrl Pts',(-0.322191578554922,2.09150600937965,
9.84994727655726));
#65258=CARTESIAN_POINT('Ctrl Pts',(-0.321992795503579,2.08649660667005,
9.85025238532329));
#65259=CARTESIAN_POINT('Ctrl Pts',(-0.321961580811205,2.08577177257329,
9.85029661511192));
#65260=CARTESIAN_POINT('Ctrl Pts',(-0.321905854955554,2.08457202841941,
9.85036996250775));
#65261=CARTESIAN_POINT('Ctrl Pts',(-0.321882739602497,2.08409705360839,
9.85039903640613));
#65262=CARTESIAN_POINT('Ctrl Pts',(-0.321839399303173,2.08324532807595,
9.85045123682059));
#65263=CARTESIAN_POINT('Ctrl Pts',(-0.321819563820713,2.08286855769527,
9.85047435109949));
#65264=CARTESIAN_POINT('Ctrl Pts',(-0.32177812602574,2.08210693387075,9.85052112207276));
#65265=CARTESIAN_POINT('Ctrl Pts',(-0.321756494791382,2.08172208267726,
9.85054477963659));
#65266=CARTESIAN_POINT('Ctrl Pts',(-0.321708563443494,2.08089577512828,
9.85059562638415));
#65267=CARTESIAN_POINT('Ctrl Pts',(-0.321682045016571,2.08045433266224,
9.85062282237284));
#65268=CARTESIAN_POINT('Ctrl Pts',(-0.321608451333084,2.07926997850794,
9.8506958732354));
#65269=CARTESIAN_POINT('Ctrl Pts',(-0.321559710766366,2.0785271763172,9.85074178029472));
#65270=CARTESIAN_POINT('Ctrl Pts',(-0.32133604818166,2.07529026623484,9.85094223178424));
#65271=CARTESIAN_POINT('Ctrl Pts',(-0.321134682523868,2.07279812658345,
9.8510976042842));
#65272=CARTESIAN_POINT('Ctrl Pts',(-0.320836937763716,2.06958010023945,
9.85129962789211));
#65273=CARTESIAN_POINT('Ctrl Pts',(-0.320767050268643,2.06885179968644,
9.85134544216127));
#65274=CARTESIAN_POINT('Ctrl Pts',(-0.320468730706367,2.06585052154357,
9.85153462404034));
#65275=CARTESIAN_POINT('Ctrl Pts',(-0.320218618402679,2.06357981003516,
9.85167866540678));
#65276=CARTESIAN_POINT('Ctrl Pts',(-0.315533855977145,2.02483747949882,
9.85415209806566));
#65277=CARTESIAN_POINT('Ctrl Pts',(-0.304917763229506,1.98938860429618,
9.85670064504704));
#65278=CARTESIAN_POINT('Ctrl Pts',(-0.285754470621778,1.95085087955732,
9.85954762836783));
#65279=CARTESIAN_POINT('Ctrl Pts',(-0.28277602106689,1.94527827982151,9.85996014309698));
#65280=CARTESIAN_POINT('Ctrl Pts',(-0.278165236209072,1.93723014821545,
9.86055343052394));
#65281=CARTESIAN_POINT('Ctrl Pts',(-0.276659661824865,1.93468407115852,
9.86074074043838));
#65282=CARTESIAN_POINT('Ctrl Pts',(-0.274856854593043,1.93172897211034,
9.86095736729327));
#65283=CARTESIAN_POINT('Ctrl Pts',(-0.274593514779189,1.93129958211901,
9.86098882484963));
#65284=CARTESIAN_POINT('Ctrl Pts',(-0.274189766800146,1.93064469903557,
9.86103677051984));
#65285=CARTESIAN_POINT('Ctrl Pts',(-0.274050086284967,1.9304187616772,9.86105330618524));
#65286=CARTESIAN_POINT('Ctrl Pts',(-0.273806455055637,1.93002576810647,
9.86108205774386));
#65287=CARTESIAN_POINT('Ctrl Pts',(-0.273702630986612,1.92985863486613,
9.86109428196359));
#65288=CARTESIAN_POINT('Ctrl Pts',(-0.273467238821166,1.92948047983886,
9.86112193289518));
#65289=CARTESIAN_POINT('Ctrl Pts',(-0.273335579777427,1.92926951563005,
9.86113735345064));
#65290=CARTESIAN_POINT('Ctrl Pts',(-0.272977728863717,1.92869758721397,
9.86117914516922));
#65291=CARTESIAN_POINT('Ctrl Pts',(-0.272751064283301,1.92833691713364,
9.86120548504222));
#65292=CARTESIAN_POINT('Ctrl Pts',(-0.271725910058636,1.92671284180386,
9.86132402980173));
#65293=CARTESIAN_POINT('Ctrl Pts',(-0.270919336085076,1.92545452474796,
9.86141570736903));
#65294=CARTESIAN_POINT('Ctrl Pts',(-0.254033039025549,1.89950967639892,
9.86330344367826));
#65295=CARTESIAN_POINT('Ctrl Pts',(-0.234649100297479,1.87713319544882,
9.86489286782279));
#65296=CARTESIAN_POINT('Ctrl Pts',(-0.203010029153907,1.84938654639059,
9.8672636296581));
#65297=CARTESIAN_POINT('Ctrl Pts',(-0.193050708013449,1.84163677184903,
9.86798330521246));
#65298=CARTESIAN_POINT('Ctrl Pts',(-0.178484854515807,1.83161583639994,
9.86902257548378));
#65299=CARTESIAN_POINT('Ctrl Pts',(-0.174238991980849,1.82884013555731,
9.869323965932));
#65300=CARTESIAN_POINT('Ctrl Pts',(-0.168279932652965,1.8251422020362,9.86974581259091));
#65301=CARTESIAN_POINT('Ctrl Pts',(-0.16662111599647,1.8241334592818,9.86986311894782));
#65302=CARTESIAN_POINT('Ctrl Pts',(-0.164134544812902,1.82265196020739,
9.87003882571773));
#65303=CARTESIAN_POINT('Ctrl Pts',(-0.163313623156456,1.82216777645696,
9.87009681200351));
#65304=CARTESIAN_POINT('Ctrl Pts',(-0.161997496540433,1.82139936694686,
9.8701897476582));
#65305=CARTESIAN_POINT('Ctrl Pts',(-0.161503658796771,1.82111280091829,
9.87022461236561));
#65306=CARTESIAN_POINT('Ctrl Pts',(-0.160561846611432,1.82056962303987,
9.87029109244038));
#65307=CARTESIAN_POINT('Ctrl Pts',(-0.160114011548544,1.82031277208945,
9.8703226990605));
#65308=CARTESIAN_POINT('Ctrl Pts',(-0.159327204175501,1.81986401629918,
9.87037822138686));
#65309=CARTESIAN_POINT('Ctrl Pts',(-0.158988496644061,1.81967164737203,
9.87040212031164));
#65310=CARTESIAN_POINT('Ctrl Pts',(-0.158326312022943,1.81929714579968,
9.87044883897443));
#65311=CARTESIAN_POINT('Ctrl Pts',(-0.158002867224354,1.81911495699827,
9.87047165664716));
#65312=CARTESIAN_POINT('Ctrl Pts',(-0.157234172910046,1.81868371755589,
9.87052588017673));
#65313=CARTESIAN_POINT('Ctrl Pts',(-0.156788646388517,1.81843516509024,
9.87055730384404));
#65314=CARTESIAN_POINT('Ctrl Pts',(-0.155214953969575,1.81756211932166,
9.87066828720677));
#65315=CARTESIAN_POINT('Ctrl Pts',(-0.154083643474161,1.81694334645859,
9.87074805108102));
#65316=CARTESIAN_POINT('Ctrl Pts',(-0.136406860190665,1.80741236473101,
9.87199413054736));
#65317=CARTESIAN_POINT('Ctrl Pts',(-0.119119718695546,1.79995896382205,
9.8732128517394));
#65318=CARTESIAN_POINT('Ctrl Pts',(-0.0929608241397392,1.79129894940395,
9.8750518601239));
#65319=CARTESIAN_POINT('Ctrl Pts',(-0.0845283854181895,1.78888427311213,
9.87564335847589));
#65320=CARTESIAN_POINT('Ctrl Pts',(-0.0735270853278912,1.78621430509336,
9.87640915894608));
#65321=CARTESIAN_POINT('Ctrl Pts',(-0.0710388166221223,1.78564163583795,
9.87658197292038));
#65322=CARTESIAN_POINT('Ctrl Pts',(-0.0605914599342707,1.78336757895998,
9.87730545787967));
#65323=CARTESIAN_POINT('Ctrl Pts',(-0.0525759843857189,1.7819383900288,
9.87785553570679));
#65324=CARTESIAN_POINT('Ctrl Pts',(-0.0358680333711405,1.77960823825756,
9.87898304808197));
#65325=CARTESIAN_POINT('Ctrl Pts',(-0.0271750550664454,1.77875408388538,
9.87955912624351));
#65326=CARTESIAN_POINT('Ctrl Pts',(-0.0149468507266521,1.77805259405645,
9.88034564956765));
#65327=CARTESIAN_POINT('Ctrl Pts',(-0.0114330013516283,1.77790866273691,
9.88056890195889));
#65328=CARTESIAN_POINT('Ctrl Pts',(-0.00739085921732094,1.77780932949561,
9.88082201302364));
#65329=CARTESIAN_POINT('Ctrl Pts',(-0.00686435670550724,1.77779768222994,
9.8808549093006));
#65330=CARTESIAN_POINT('Ctrl Pts',(-0.00606743225273874,1.77778200697258,
9.88090458992848));
#65331=CARTESIAN_POINT('Ctrl Pts',(-0.00579703313422386,1.77777702879389,
9.88092142724901));
#65332=CARTESIAN_POINT('Ctrl Pts',(-0.00532938696109524,1.77776900804757,
9.88095051276104));
#65333=CARTESIAN_POINT('Ctrl Pts',(-0.00513214369712841,1.77776580621873,
9.8809627699194));
#65334=CARTESIAN_POINT('Ctrl Pts',(-0.00472059483463152,1.77775950356115,
9.88098832256555));
#65335=CARTESIAN_POINT('Ctrl Pts',(-0.00450628973259388,1.77775643541844,
9.88100161615761));
#65336=CARTESIAN_POINT('Ctrl Pts',(-0.00391332761659985,1.7777485377911,
9.88103836438608));
#65337=CARTESIAN_POINT('Ctrl Pts',(-0.0035346633455427,1.77774416190341,
9.88106179348087));
#65338=CARTESIAN_POINT('Ctrl Pts',(-0.00204854543050816,1.77772960787937,
9.88115359704473));
#65339=CARTESIAN_POINT('Ctrl Pts',(-0.000941033447506969,1.77772447080819,
9.88122169219538));
#65340=CARTESIAN_POINT('Ctrl Pts',(0.0194687415531727,1.77773501542436,
9.88247103936936));
#65341=CARTESIAN_POINT('Ctrl Pts',(0.0387343882509863,1.77947911042484,
9.88356014564101));
#65342=CARTESIAN_POINT('Ctrl Pts',(0.0739802413587024,1.78589666372575,
9.88556630697484));
#65343=CARTESIAN_POINT('Ctrl Pts',(0.0899781765223071,1.7901002019261,9.88648275333677));
#65344=CARTESIAN_POINT('Ctrl Pts',(0.111817456346848,1.79767306215114,9.88780643457743));
#65345=CARTESIAN_POINT('Ctrl Pts',(0.117983986742064,1.80002584716446,9.88818847242845));
#65346=CARTESIAN_POINT('Ctrl Pts',(0.128819480882107,1.80454584366554,9.88887828701004));
#65347=CARTESIAN_POINT('Ctrl Pts',(0.133516984408784,1.80663874198001,9.8891837318254));
#65348=CARTESIAN_POINT('Ctrl Pts',(0.13993405414394,1.80968382338513,9.8896109025952));
#65349=CARTESIAN_POINT('Ctrl Pts',(0.141698139353985,1.8105407473271,9.88972938775935));
#65350=CARTESIAN_POINT('Ctrl Pts',(0.144314100417334,1.81184112359528,9.88990671319791));
#65351=CARTESIAN_POINT('Ctrl Pts',(0.145172014790615,1.81227237928788,9.88996513019462));
#65352=CARTESIAN_POINT('Ctrl Pts',(0.14653960323938,1.81296751108813,9.89005867740894));
#65353=CARTESIAN_POINT('Ctrl Pts',(0.147050526379472,1.81322892807446,9.89009372147586));
#65354=CARTESIAN_POINT('Ctrl Pts',(0.148021778848039,1.81372915352097,9.89016052244851));
#65355=CARTESIAN_POINT('Ctrl Pts',(0.148482235835225,1.81396771127447,9.89019227046276));
#65356=CARTESIAN_POINT('Ctrl Pts',(0.149287847022244,1.81438755917555,9.89024795520635));
#65357=CARTESIAN_POINT('Ctrl Pts',(0.149633252687581,1.81456836666163,9.89027187484308));
#65358=CARTESIAN_POINT('Ctrl Pts',(0.150306412628952,1.81492229946361,9.89031857961225));
#65359=CARTESIAN_POINT('Ctrl Pts',(0.150634198124144,1.81509536442133,9.89034136257993));
#65360=CARTESIAN_POINT('Ctrl Pts',(0.151410524137539,1.81550696512249,9.89039541875431));
#65361=CARTESIAN_POINT('Ctrl Pts',(0.151858799630959,1.81574599618765,9.89042670951346));
#65362=CARTESIAN_POINT('Ctrl Pts',(0.15343178422973,1.81658953157698,9.89053678000544));
#65363=CARTESIAN_POINT('Ctrl Pts',(0.154553452938725,1.81719965323017,9.89061575952742));
#65364=CARTESIAN_POINT('Ctrl Pts',(0.170842968429254,1.82618604616891,9.89176998977606));
#65365=CARTESIAN_POINT('Ctrl Pts',(0.185312173956877,1.83576408018195,9.89288948426452));
#65366=CARTESIAN_POINT('Ctrl Pts',(0.21179508236492,1.8565435983744,9.89512724377984));
#65367=CARTESIAN_POINT('Ctrl Pts',(0.223864112527872,1.86759306457073,9.89623844810752));
#65368=CARTESIAN_POINT('Ctrl Pts',(0.237721011914614,1.8823644708832,9.89760519421292));
#65369=CARTESIAN_POINT('Ctrl Pts',(0.240347348290867,1.88526840880596,9.89786869226733));
#65370=CARTESIAN_POINT('Ctrl Pts',(0.250516385788705,1.89693267694138,9.89890494401018));
#65371=CARTESIAN_POINT('Ctrl Pts',(0.257639237428898,1.90604927942632,9.89966704432621));
#65372=CARTESIAN_POINT('Ctrl Pts',(0.265159879357793,1.91682276380576,9.90049838079363));
#65373=CARTESIAN_POINT('Ctrl Pts',(0.266052881237803,1.91812222206426,9.90059755897435));
#65374=CARTESIAN_POINT('Ctrl Pts',(0.267168773655424,1.91977182764946,9.90072203198418));
#65375=CARTESIAN_POINT('Ctrl Pts',(0.267400553280895,1.92011589332288,9.90074791593235));
#65376=CARTESIAN_POINT('Ctrl Pts',(0.267768822149501,1.92066485531472,9.9007890888712));
#65377=CARTESIAN_POINT('Ctrl Pts',(0.267905741099022,1.92086946066687,9.90080440691191));
#65378=CARTESIAN_POINT('Ctrl Pts',(0.268164037732097,1.9212564057875,9.90083332352173));
#65379=CARTESIAN_POINT('Ctrl Pts',(0.268285462971969,1.92143871090572,9.90084692525057));
#65380=CARTESIAN_POINT('Ctrl Pts',(0.268561777972551,1.9218544821409,9.90087789584407));
#65381=CARTESIAN_POINT('Ctrl Pts',(0.268716548942019,1.92208802612757,9.90089525660364));
#65382=CARTESIAN_POINT('Ctrl Pts',(0.269177175995301,1.92278506856004,9.90094696627878));
#65383=CARTESIAN_POINT('Ctrl Pts',(0.269482140843537,1.92324915904211,9.90098125533155));
#65384=CARTESIAN_POINT('Ctrl Pts',(0.271609373003768,1.92650464947872,9.90122082926981));
#65385=CARTESIAN_POINT('Ctrl Pts',(0.273389517539276,1.92932351666184,9.90142336071257));
#65386=CARTESIAN_POINT('Ctrl Pts',(0.282846026764444,1.94482564885782,9.90251358000512));
#65387=CARTESIAN_POINT('Ctrl Pts',(0.289684835359071,1.95800086894476,9.90335578426171));
#65388=CARTESIAN_POINT('Ctrl Pts',(0.307616996932311,1.99928342431079,9.90588331071758));
#65389=CARTESIAN_POINT('Ctrl Pts',(0.315692156896018,2.02851332731368,9.90754137125232));
#65390=CARTESIAN_POINT('Ctrl Pts',(0.319839763281418,2.0604065994335,9.9094752219177));
#65391=CARTESIAN_POINT('Ctrl Pts',(0.320077433658286,2.06237623438598,9.90959506280617));
#65392=CARTESIAN_POINT('Ctrl Pts',(0.320404029791101,2.06531036012148,9.90977424880363));
#65393=CARTESIAN_POINT('Ctrl Pts',(0.32050682061774,2.06627328467042,9.90983315998312));
#65394=CARTESIAN_POINT('Ctrl Pts',(0.32066395980513,2.06781096781645,9.90992740869623));
#65395=CARTESIAN_POINT('Ctrl Pts',(0.320721106995287,2.06838543956142,9.9099626583548));
#65396=CARTESIAN_POINT('Ctrl Pts',(0.320826887074585,2.06947860483655,9.91002981009851));
#65397=CARTESIAN_POINT('Ctrl Pts',(0.320875806472424,2.0699972693188,9.91006170308344));
#65398=CARTESIAN_POINT('Ctrl Pts',(0.320959176359397,2.07090472409303,9.91011755995921));
#65399=CARTESIAN_POINT('Ctrl Pts',(0.320994178664902,2.07129346362793,9.91014150644712));
#65400=CARTESIAN_POINT('Ctrl Pts',(0.321060986415239,2.07205084022368,9.91018819705763));
#65401=CARTESIAN_POINT('Ctrl Pts',(0.321092863393407,2.07241947052397,9.91021093889342));
#65402=CARTESIAN_POINT('Ctrl Pts',(0.321166785292379,2.07329181499574,9.9102647958708));
#65403=CARTESIAN_POINT('Ctrl Pts',(0.321208280027281,2.07379557368435,9.91029592825864));
#65404=CARTESIAN_POINT('Ctrl Pts',(0.321349224621394,2.07555733400026,9.91040491591632));
#65405=CARTESIAN_POINT('Ctrl Pts',(0.321442469587056,2.07681580799171,9.91048296583224));
#65406=CARTESIAN_POINT('Ctrl Pts',(0.32262236244452,2.09411866833812,9.91155886056253));
#65407=CARTESIAN_POINT('Ctrl Pts',(0.322513876835275,2.11021932538932,9.91259461139189));
#65408=CARTESIAN_POINT('Ctrl Pts',(0.319449043936508,2.14773230764201,9.91508747392847));
#65409=CARTESIAN_POINT('Ctrl Pts',(0.31554110726248,2.1689910424194,9.91656371437978));
#65410=CARTESIAN_POINT('Ctrl Pts',(0.306331142177803,2.20077393989518,9.91877942206794));
#65411=CARTESIAN_POINT('Ctrl Pts',(0.302528988629397,2.21167106943813,9.91953961106161));
#65412=CARTESIAN_POINT('Ctrl Pts',(0.297552562134759,2.2237987392997,9.92036904579229));
#65413=CARTESIAN_POINT('Ctrl Pts',(0.296944118203446,2.2252511316899,9.9204680952189));
#65414=CARTESIAN_POINT('Ctrl Pts',(0.2961620178131,2.22708031624389,9.92059242944381));
#65415=CARTESIAN_POINT('Ctrl Pts',(0.295998259941087,2.2274612791722,9.92061830178424));
#65416=CARTESIAN_POINT('Ctrl Pts',(0.295736122410401,2.22806788089092,9.92065946055417));
#65417=CARTESIAN_POINT('Ctrl Pts',(0.295638219438636,2.22829372323835,9.92067477599926));
#65418=CARTESIAN_POINT('Ctrl Pts',(0.295452702632546,2.22872033295208,9.92070369048485));
#65419=CARTESIAN_POINT('Ctrl Pts',(0.295365143574476,2.22892112150346,9.9207172926788));
#65420=CARTESIAN_POINT('Ctrl Pts',(0.295165098370304,2.2293785873482,9.92074826804565));
#65421=CARTESIAN_POINT('Ctrl Pts',(0.295052482293247,2.22963520684671,9.92076563310412));
#65422=CARTESIAN_POINT('Ctrl Pts',(0.2947078976741,2.23041764053126,9.92081854708047));
#65423=CARTESIAN_POINT('Ctrl Pts',(0.294474855631371,2.23094298502076,9.9208540304404));
#65424=CARTESIAN_POINT('Ctrl Pts',(0.292779812831057,2.23473669293124,9.92110996780169));
#65425=CARTESIAN_POINT('Ctrl Pts',(0.291264768321077,2.23798127608504,9.9213272407064));
#65426=CARTESIAN_POINT('Ctrl Pts',(0.278666561604475,2.2638286286931,9.92305030691874));
#65427=CARTESIAN_POINT('Ctrl Pts',(0.265022357965995,2.28509021679271,9.92442435825353));
#65428=CARTESIAN_POINT('Ctrl Pts',(0.235344627055456,2.32122316266972,9.92704919348635));
#65429=CARTESIAN_POINT('Ctrl Pts',(0.220011460893924,2.33647733566107,9.92828313599592));
#65430=CARTESIAN_POINT('Ctrl Pts',(0.202532675550062,2.35068425519987,9.92965049157533));
#65431=CARTESIAN_POINT('Ctrl Pts',(0.201791875006027,2.35128095753941,9.9297083666877));
#65432=CARTESIAN_POINT('Ctrl Pts',(0.200602810351679,2.35223007994785,9.92980114446508));
#65433=CARTESIAN_POINT('Ctrl Pts',(0.200156230012903,2.35258460826414,9.92983596285092));
#65434=CARTESIAN_POINT('Ctrl Pts',(0.199303744449869,2.35325769348716,9.92990237933494));
#65435=CARTESIAN_POINT('Ctrl Pts',(0.198898010065265,2.35357646469923,9.92993396877016));
#65436=CARTESIAN_POINT('Ctrl Pts',(0.198184731015751,2.35413409778234,9.92998946684694));
#65437=CARTESIAN_POINT('Ctrl Pts',(0.197877514914445,2.35437337980331,9.93001335873649));
#65438=CARTESIAN_POINT('Ctrl Pts',(0.197276422359329,2.35483980608267,9.93006008272068));
#65439=CARTESIAN_POINT('Ctrl Pts',(0.196982585302058,2.35506700035299,9.93008291278487));
#65440=CARTESIAN_POINT('Ctrl Pts',(0.19628361481496,2.35560551487419,9.93013719591712));
#65441=CARTESIAN_POINT('Ctrl Pts',(0.195878133424185,2.35591637993763,9.93016866688768));
#65442=CARTESIAN_POINT('Ctrl Pts',(0.194443131470358,2.35701112550417,9.93027997609215));
#65443=CARTESIAN_POINT('Ctrl Pts',(0.193409641273601,2.35778976045026,9.93036002008375));
#65444=CARTESIAN_POINT('Ctrl Pts',(0.176726594643034,2.37020202900604,9.93165028138012));
#65445=CARTESIAN_POINT('Ctrl Pts',(0.16006056982947,2.38039577286334,9.93291711967311));
#65446=CARTESIAN_POINT('Ctrl Pts',(0.127597832294581,2.39641019621713,9.93533714572109));
#65447=CARTESIAN_POINT('Ctrl Pts',(0.112065407743267,2.40262439505264,9.93647616678091));
#65448=CARTESIAN_POINT('Ctrl Pts',(0.0860523836713744,2.41075306387351,
9.93830713282158));
#65449=CARTESIAN_POINT('Ctrl Pts',(0.0758331156550389,2.41340366642323,
9.93900768035754));
#65450=CARTESIAN_POINT('Ctrl Pts',(0.0618442749261837,2.41630746455329,
9.93992647390684));
#65451=CARTESIAN_POINT('Ctrl Pts',(0.0581740305197722,2.41700301519994,
9.94016383877853));
#65452=CARTESIAN_POINT('Ctrl Pts',(0.0539656603337894,2.4177249890654,9.94043115520065));
#65453=CARTESIAN_POINT('Ctrl Pts',(0.0534387602673929,2.41781403380391,
9.94046453738085));
#65454=CARTESIAN_POINT('Ctrl Pts',(0.0526432792788163,2.41794643382568,
9.94051480256152));
#65455=CARTESIAN_POINT('Ctrl Pts',(0.0523748642389889,2.417990759666,9.94053174042147));
#65456=CARTESIAN_POINT('Ctrl Pts',(0.0519115275516,2.41806667213618,9.94056093864365));
#65457=CARTESIAN_POINT('Ctrl Pts',(0.0517166332464374,2.41809841946003,
9.94057320818576));
#65458=CARTESIAN_POINT('Ctrl Pts',(0.0513108815777127,2.41816413165286,
9.94059872682051));
#65459=CARTESIAN_POINT('Ctrl Pts',(0.0511000202553528,2.418198065942,9.94061197412402));
#65460=CARTESIAN_POINT('Ctrl Pts',(0.0505188924337464,2.41829099533184,
9.94064844447225));
#65461=CARTESIAN_POINT('Ctrl Pts',(0.050148554969326,2.41834955416954,9.94067164262755));
#65462=CARTESIAN_POINT('Ctrl Pts',(0.0487080625215991,2.41857475302515,
9.94076170999835));
#65463=CARTESIAN_POINT('Ctrl Pts',(0.0476371567331209,2.41873664677367,
9.94082831289414));
#65464=CARTESIAN_POINT('Ctrl Pts',(0.0281230779108912,2.42158613299846,
9.94203580996059));
#65465=CARTESIAN_POINT('Ctrl Pts',(0.00947872784101369,2.42267464108025,
9.9430906431631));
#65466=CARTESIAN_POINT('Ctrl Pts',(-0.0258971944186755,2.421669007309,9.94507415722131));
#65467=CARTESIAN_POINT('Ctrl Pts',(-0.0425735994511782,2.41988917303906,
9.94600210184314));
#65468=CARTESIAN_POINT('Ctrl Pts',(-0.0732644266709059,2.41417030179155,
9.94778708822536));
#65469=CARTESIAN_POINT('Ctrl Pts',(-0.0872963369329439,2.41056387395722,
9.94863438715372));
#65470=CARTESIAN_POINT('Ctrl Pts',(-0.102181929484982,2.40564927937652,
9.94958726974118));
#65471=CARTESIAN_POINT('Ctrl Pts',(-0.103324448849124,2.40526494542432,
9.94966075252034));
#65472=CARTESIAN_POINT('Ctrl Pts',(-0.104972315384738,2.40470030599128,
9.94976724728498));
#65473=CARTESIAN_POINT('Ctrl Pts',(-0.105479420156125,2.40452513096039,
9.94980008937827));
#65474=CARTESIAN_POINT('Ctrl Pts',(-0.10636216686101,2.40421772413405,9.94985738251494));
#65475=CARTESIAN_POINT('Ctrl Pts',(-0.106738006570783,2.40408606046261,
9.94988181466686));
#65476=CARTESIAN_POINT('Ctrl Pts',(-0.107462669458365,2.40383068850838,
9.94992899826131));
#65477=CARTESIAN_POINT('Ctrl Pts',(-0.107811525671363,2.4037070752176,9.94995174651599));
#65478=CARTESIAN_POINT('Ctrl Pts',(-0.108636693031225,2.40341308550093,
9.95000563464235));
#65479=CARTESIAN_POINT('Ctrl Pts',(-0.10911281643243,2.40324218837669,9.95003679180811));
#65480=CARTESIAN_POINT('Ctrl Pts',(-0.110777452670948,2.40264026492484,
9.95014594843901));
#65481=CARTESIAN_POINT('Ctrl Pts',(-0.11196381814408,2.4022033708078,9.95022414334812));
#65482=CARTESIAN_POINT('Ctrl Pts',(-0.128368697873202,2.39605220677752,
9.95131104490252));
#65483=CARTESIAN_POINT('Ctrl Pts',(-0.143133699455842,2.38920239935996,
9.952358514376));
#65484=CARTESIAN_POINT('Ctrl Pts',(-0.161735498329928,2.37879819084325,
9.95377093461385));
#65485=CARTESIAN_POINT('Ctrl Pts',(-0.166094720906318,2.37622335781735,
9.95410890814488));
#65486=CARTESIAN_POINT('Ctrl Pts',(-0.1773944440358,2.36918480387902,9.95500239195419));
#65487=CARTESIAN_POINT('Ctrl Pts',(-0.184227280524771,2.36455538343687,
9.95556058283267));
#65488=CARTESIAN_POINT('Ctrl Pts',(-0.196980720924983,2.35518071683819,
9.95663172144273));
#65489=CARTESIAN_POINT('Ctrl Pts',(-0.2029265615126,2.35047837784963,9.9571443138424));
#65490=CARTESIAN_POINT('Ctrl Pts',(-0.217822841365875,2.33781859729511,
9.95845490429192));
#65491=CARTESIAN_POINT('Ctrl Pts',(-0.226506590135773,2.32956329579587,
9.95924533382984));
#65492=CARTESIAN_POINT('Ctrl Pts',(-0.23581215421961,2.31967335462556,9.96010477741338));
#65493=CARTESIAN_POINT('Ctrl Pts',(-0.236903944096473,2.31849548355999,
9.96020581620743));
#65494=CARTESIAN_POINT('Ctrl Pts',(-0.238268428881213,2.31700116527138,
9.96033229292212));
#65495=CARTESIAN_POINT('Ctrl Pts',(-0.238549350450033,2.31669231028167,
9.96035834297832));
#65496=CARTESIAN_POINT('Ctrl Pts',(-0.238995368527162,2.31620002393444,
9.96039971865969));
#65497=CARTESIAN_POINT('Ctrl Pts',(-0.239160854681028,2.31601694867743,
9.96041507382979));
#65498=CARTESIAN_POINT('Ctrl Pts',(-0.239472756486994,2.3156710978745,9.96044402103891));
#65499=CARTESIAN_POINT('Ctrl Pts',(-0.239619215357413,2.31550836454692,
9.96045761632779));
#65500=CARTESIAN_POINT('Ctrl Pts',(-0.239952063011153,2.31513777219875,
9.96048851964247));
#65501=CARTESIAN_POINT('Ctrl Pts',(-0.240138347255088,2.31492982052045,
9.96050581969523));
#65502=CARTESIAN_POINT('Ctrl Pts',(-0.240703754211891,2.31429699620476,
9.96055834303852));
#65503=CARTESIAN_POINT('Ctrl Pts',(-0.241082023882774,2.31387135770453,
9.96059350218161));
#65504=CARTESIAN_POINT('Ctrl Pts',(-0.243760405447751,2.31084144065498,
9.96084261094786));
#65505=CARTESIAN_POINT('Ctrl Pts',(-0.246019506756295,2.30820099191381,
9.96105356744091));
#65506=CARTESIAN_POINT('Ctrl Pts',(-0.267991281892727,2.28166313904493,
9.96311981497746));
#65507=CARTESIAN_POINT('Ctrl Pts',(-0.284206343142693,2.25507481408311,
9.96477620875413));
#65508=CARTESIAN_POINT('Ctrl Pts',(-0.302128827212125,2.21310964691832,
9.96737142239807));
#65509=CARTESIAN_POINT('Ctrl Pts',(-0.306955121896611,2.19926777803044,
9.9682223365515));
#65510=CARTESIAN_POINT('Ctrl Pts',(-0.311237435956427,2.18363545863939,
9.96920044902112));
#65511=CARTESIAN_POINT('Ctrl Pts',(-0.311640441698801,2.18212104752749,
9.96929536633618));
#65512=CARTESIAN_POINT('Ctrl Pts',(-0.312328031226317,2.17945925916442,
9.96946250560583));
#65513=CARTESIAN_POINT('Ctrl Pts',(-0.312617379242658,2.17831313487435,
9.96953457310703));
#65514=CARTESIAN_POINT('Ctrl Pts',(-0.313027849879069,2.1766487057733,9.96963938468727));
#65515=CARTESIAN_POINT('Ctrl Pts',(-0.31315400664538,2.17613164265411,9.96967196633314));
#65516=CARTESIAN_POINT('Ctrl Pts',(-0.313372151010175,2.17522784472116,
9.96972895552328));
#65517=CARTESIAN_POINT('Ctrl Pts',(-0.313464705242304,2.17484124675072,
9.96975334476004));
#65518=CARTESIAN_POINT('Ctrl Pts',(-0.313642307090249,2.17409329684037,
9.96980055453524));
#65519=CARTESIAN_POINT('Ctrl Pts',(-0.31372744614752,2.17373196705319,9.96982337208892));
#65520=CARTESIAN_POINT('Ctrl Pts',(-0.313928106322365,2.17287372607629,
9.96987759504555));
#65521=CARTESIAN_POINT('Ctrl Pts',(-0.314043071939718,2.17237668722231,
9.96990901825806));
#65522=CARTESIAN_POINT('Ctrl Pts',(-0.314383795249423,2.17088751794692,
9.97000322793127));
#65523=CARTESIAN_POINT('Ctrl Pts',(-0.314606033473852,2.1698945962138,9.97006612723546));
#65524=CARTESIAN_POINT('Ctrl Pts',(-0.316740867253675,2.16014002929923,
9.970684906583));
#65525=CARTESIAN_POINT('Ctrl Pts',(-0.318291493428664,2.15130399091243,
9.97125231117246));
#65526=CARTESIAN_POINT('Ctrl Pts',(-0.320070783976515,2.13790244324655,
9.97212438986133));
#65527=CARTESIAN_POINT('Ctrl Pts',(-0.320574246079929,2.13337741258019,
9.97242076883965));
#65528=CARTESIAN_POINT('Ctrl Pts',(-0.321852373819689,2.11915385970834,
9.97335807673244));
#65529=CARTESIAN_POINT('Ctrl Pts',(-0.322283826669288,2.10943047574389,
9.97400729087377));
#65530=CARTESIAN_POINT('Ctrl Pts',(-0.322250579164992,2.0733493113159,9.97643634402248));
#65531=CARTESIAN_POINT('Ctrl Pts',(-0.318993923940641,2.04709668394773,
9.97825145316637));
#65532=CARTESIAN_POINT('Ctrl Pts',(-0.31223920016274,2.02018912324031,9.98000427312217));
#65533=CARTESIAN_POINT('Ctrl Pts',(-0.311893288057679,2.01884785156172,
9.98009133286119));
#65534=CARTESIAN_POINT('Ctrl Pts',(-0.311432852017357,2.01710895455509,
9.9802037562032));
#65535=CARTESIAN_POINT('Ctrl Pts',(-0.311326201769074,2.01670928726914,
9.98022956487852));
#65536=CARTESIAN_POINT('Ctrl Pts',(-0.311161294179648,2.01609604517341,
9.98026911696058));
#65537=CARTESIAN_POINT('Ctrl Pts',(-0.311103586287571,2.01588232509867,
9.98028289218651));
#65538=CARTESIAN_POINT('Ctrl Pts',(-0.310988606913736,2.01545823796048,
9.98031020839601));
#65539=CARTESIAN_POINT('Ctrl Pts',(-0.310931342532343,2.01524787087951,
9.98032374961862));
#65540=CARTESIAN_POINT('Ctrl Pts',(-0.310803261417333,2.01477922766307,
9.98035389621517));
#65541=CARTESIAN_POINT('Ctrl Pts',(-0.310732336388528,2.01452098228729,
9.98037049514583));
#65542=CARTESIAN_POINT('Ctrl Pts',(-0.310524339961979,2.01376732559113,
9.98041889894385));
#65543=CARTESIAN_POINT('Ctrl Pts',(-0.310386404303334,2.01327215051197,
9.9804506536021));
#65544=CARTESIAN_POINT('Ctrl Pts',(-0.309382772373545,2.00970227601466,
9.98067924995945));
#65545=CARTESIAN_POINT('Ctrl Pts',(-0.30847255199729,2.00664012995879,9.98087355011733));
#65546=CARTESIAN_POINT('Ctrl Pts',(-0.305795756082405,1.99810184441902,
9.98141161832246));
#65547=CARTESIAN_POINT('Ctrl Pts',(-0.303927780068221,1.99265852929653,
9.98175034146277));
#65548=CARTESIAN_POINT('Ctrl Pts',(-0.298970432652464,1.97938195352247,
9.98257245907948));
#65549=CARTESIAN_POINT('Ctrl Pts',(-0.295717932675965,1.97161405236998,
9.98304995743626));
#65550=CARTESIAN_POINT('Ctrl Pts',(-0.281756877286434,1.94162587728681,
9.98491068472604));
#65551=CARTESIAN_POINT('Ctrl Pts',(-0.268818199870231,1.92053962821151,
9.9862646134698));
#65552=CARTESIAN_POINT('Ctrl Pts',(-0.252089269540585,1.89920611414663,
9.98784895971462));
#65553=CARTESIAN_POINT('Ctrl Pts',(-0.250554736038744,1.89729452837739,
9.98799294140806));
#65554=CARTESIAN_POINT('Ctrl Pts',(-0.244885185310744,1.89039465229281,
9.98852038512737));
#65555=CARTESIAN_POINT('Ctrl Pts',(-0.240622011560437,1.88551411621042,
9.9889084893278));
#65556=CARTESIAN_POINT('Ctrl Pts',(-0.235512787001667,1.8800091640062,9.98936560320263));
#65557=CARTESIAN_POINT('Ctrl Pts',(-0.234807086604242,1.87925609226046,
9.9894285702673));
#65558=CARTESIAN_POINT('Ctrl Pts',(-0.233751762674211,1.87814071452223,
9.98952248603017));
#65559=CARTESIAN_POINT('Ctrl Pts',(-0.233404882920069,1.8777758120039,9.98955331637382));
#65560=CARTESIAN_POINT('Ctrl Pts',(-0.232785466982795,1.87712726340465,
9.98960830039701));
#65561=CARTESIAN_POINT('Ctrl Pts',(-0.232513263285326,1.87684330001067,
9.98963243963232));
#65562=CARTESIAN_POINT('Ctrl Pts',(-0.231939069307073,1.87624649092155,
9.9896833103864));
#65563=CARTESIAN_POINT('Ctrl Pts',(-0.231636964606391,1.87593375684647,
9.98971004686416));
#65564=CARTESIAN_POINT('Ctrl Pts',(-0.23083902742191,1.87511108312504,9.98978059054528));
#65565=CARTESIAN_POINT('Ctrl Pts',(-0.230342140133861,1.87460217396817,
9.98982444385522));
#65566=CARTESIAN_POINT('Ctrl Pts',(-0.228101341536908,1.87232230866073,
9.99002187534543));
#65567=CARTESIAN_POINT('Ctrl Pts',(-0.22633870052059,1.87056995568458,9.99017627794503));
#65568=CARTESIAN_POINT('Ctrl Pts',(-0.213209513221816,1.85781595430748,
9.99132007996892));
#65569=CARTESIAN_POINT('Ctrl Pts',(-0.201068667300165,1.84764575309584,
9.9923452550347));
#65570=CARTESIAN_POINT('Ctrl Pts',(-0.162384402036427,1.81980987897678,
9.99551361721086));
#65571=CARTESIAN_POINT('Ctrl Pts',(-0.133924730622777,1.8051452683665,9.99773546654406));
#65572=CARTESIAN_POINT('Ctrl Pts',(-0.102314385090887,1.7943935011591,9.99984809662761));
#65573=CARTESIAN_POINT('Ctrl Pts',(-0.100847200872162,1.79390621072366,
9.99994535328652));
#65574=CARTESIAN_POINT('Ctrl Pts',(-0.0989708781197706,1.79329799029727,
10.0000686610128));
#65575=CARTESIAN_POINT('Ctrl Pts',(-0.0985649603050398,1.7931672995319,
10.000095273368));
#65576=CARTESIAN_POINT('Ctrl Pts',(-0.0979194594167723,1.79296088486271,
10.000137490571));
#65577=CARTESIAN_POINT('Ctrl Pts',(-0.0976800469248476,1.79288463537205,
10.0001531263191));
#65578=CARTESIAN_POINT('Ctrl Pts',(-0.097232447600714,1.79274265766306,
10.0001823163973));
#65579=CARTESIAN_POINT('Ctrl Pts',(-0.0970242847209387,1.79267686149397,
10.0001958746464));
#65580=CARTESIAN_POINT('Ctrl Pts',(-0.0965562015934771,1.79252943266054,
10.0002263240949));
#65581=CARTESIAN_POINT('Ctrl Pts',(-0.0962962452092579,1.79244791822177,
10.0002432082268));
#65582=CARTESIAN_POINT('Ctrl Pts',(-0.0955243096152806,1.79220693729672,
10.0002932679086));
#65583=CARTESIAN_POINT('Ctrl Pts',(-0.0950120322138111,1.79204841789635,
10.0003263878507));
#65584=CARTESIAN_POINT('Ctrl Pts',(-0.0908753458001397,1.79077966420559,
10.000593037779));
#65585=CARTESIAN_POINT('Ctrl Pts',(-0.08723181153509,1.78973211789303,10.0008229701226));
#65586=CARTESIAN_POINT('Ctrl Pts',(-0.0739276427774553,1.78615996693607,
10.0016475816422));
#65587=CARTESIAN_POINT('Ctrl Pts',(-0.0641688221698824,1.78402015758211,
10.0022240770525));
#65588=CARTESIAN_POINT('Ctrl Pts',(-0.0231551310390569,1.7770061473479,
10.0045877304807));
#65589=CARTESIAN_POINT('Ctrl Pts',(0.00862809475382032,1.77629211274213,
10.006297304328));
#65590=CARTESIAN_POINT('Ctrl Pts',(0.0455835936598826,1.7809155383611,10.0085061184341));
#65591=CARTESIAN_POINT('Ctrl Pts',(0.0511404263871118,1.78175888303605,
10.0088435882033));
#65592=CARTESIAN_POINT('Ctrl Pts',(0.0576333180037274,1.78291873335546,
10.0092451504272));
#65593=CARTESIAN_POINT('Ctrl Pts',(0.0585937186121705,1.78309480107246,
10.0093047342403));
#65594=CARTESIAN_POINT('Ctrl Pts',(0.0600436272590493,1.78336742527747,
10.0093949743796));
#65595=CARTESIAN_POINT('Ctrl Pts',(0.0605337415108948,1.78346075964565,
10.0094255279822));
#65596=CARTESIAN_POINT('Ctrl Pts',(0.0614093543027511,1.78362961399434,
10.0094802029463));
#65597=CARTESIAN_POINT('Ctrl Pts',(0.061794936038622,1.78370470156029,10.0095043104668));
#65598=CARTESIAN_POINT('Ctrl Pts',(0.0626095111423033,1.78386487696688,
10.0095553057556));
#65599=CARTESIAN_POINT('Ctrl Pts',(0.0630384701982962,1.78395013340819,
10.0095821988651));
#65600=CARTESIAN_POINT('Ctrl Pts',(0.0641756528600635,1.78417855791006,
10.0096535967567));
#65601=CARTESIAN_POINT('Ctrl Pts',(0.0648835678082039,1.78432323443327,
10.0096981496821));
#65602=CARTESIAN_POINT('Ctrl Pts',(0.0681341695864665,1.78499895582335,
10.0099032226238));
#65603=CARTESIAN_POINT('Ctrl Pts',(0.0706708067876858,1.78555833715908,
10.0100646474071));
#65604=CARTESIAN_POINT('Ctrl Pts',(0.0898402821141142,1.79002927764957,
10.0112954443779));
#65605=CARTESIAN_POINT('Ctrl Pts',(0.106142484036681,1.79522675361664,10.0124067915338));
#65606=CARTESIAN_POINT('Ctrl Pts',(0.150179965491559,1.81323002052585,10.0155814421998));
#65607=CARTESIAN_POINT('Ctrl Pts',(0.176624734051185,1.82871641425103,10.0177028746455));
#65608=CARTESIAN_POINT('Ctrl Pts',(0.201671789353781,1.84861999108225,10.0197262758824));
#65609=CARTESIAN_POINT('Ctrl Pts',(0.202838069695964,1.84956011261482,10.0198204890985));
#65610=CARTESIAN_POINT('Ctrl Pts',(0.204327838149167,1.85077822736923,10.0199407825683));
#65611=CARTESIAN_POINT('Ctrl Pts',(0.204657363582775,1.85104875792182,10.0199673873037));
#65612=CARTESIAN_POINT('Ctrl Pts',(0.205178304540571,1.85147816826047,10.0200094397432));
#65613=CARTESIAN_POINT('Ctrl Pts',(0.205370073154367,1.85163661590547,10.0200249186697));
#65614=CARTESIAN_POINT('Ctrl Pts',(0.205726712068326,1.85193198211999,10.0200537024504));
#65615=CARTESIAN_POINT('Ctrl Pts',(0.205891627962975,1.85206884203781,10.0200670113537));
#65616=CARTESIAN_POINT('Ctrl Pts',(0.206262723577866,1.85237743138563,10.0200969566319));
#65617=CARTESIAN_POINT('Ctrl Pts',(0.206468824965786,1.85254925349993,10.0201135860709));
#65618=CARTESIAN_POINT('Ctrl Pts',(0.206898908070391,1.85290871557259,10.0201482845458));
#65619=CARTESIAN_POINT('Ctrl Pts',(0.207122849832648,1.85309640326738,10.0201663500833));
#65620=CARTESIAN_POINT('Ctrl Pts',(0.207706270799739,1.85358672619504,10.0202134114093));
#65621=CARTESIAN_POINT('Ctrl Pts',(0.20806534550537,1.8538898449006,10.0202423723477));
#65622=CARTESIAN_POINT('Ctrl Pts',(0.209125658827076,1.85478890457828,10.0203278849192));
#65623=CARTESIAN_POINT('Ctrl Pts',(0.209825016394904,1.85538707098831,10.0203842787865));
#65624=CARTESIAN_POINT('Ctrl Pts',(0.21753954073014,1.8620427977235,10.0210063854916));
#65625=CARTESIAN_POINT('Ctrl Pts',(0.224293554856847,1.86839793062974,10.0215513762008));
#65626=CARTESIAN_POINT('Ctrl Pts',(0.250570037705361,1.89535197081546,10.023718920552));
#65627=CARTESIAN_POINT('Ctrl Pts',(0.267606251569835,1.91819448574496,10.0252490948596));
#65628=CARTESIAN_POINT('Ctrl Pts',(0.287218367823149,1.95334456810785,10.027571557539));
#65629=CARTESIAN_POINT('Ctrl Pts',(0.292426433353957,1.96402596669467,10.0282718903007));
#65630=CARTESIAN_POINT('Ctrl Pts',(0.297456134115654,1.97597494648757,10.0290599145351));
#65631=CARTESIAN_POINT('Ctrl Pts',(0.297874238444646,1.97698250674355,10.0291263925352));
#65632=CARTESIAN_POINT('Ctrl Pts',(0.298487274332091,1.97848126919075,10.0292253316143));
#65633=CARTESIAN_POINT('Ctrl Pts',(0.298686129149449,1.97897086663054,10.0292576600168));
#65634=CARTESIAN_POINT('Ctrl Pts',(0.299024442254204,1.97980973418222,10.0293130657912));
#65635=CARTESIAN_POINT('Ctrl Pts',(0.299164495439643,1.9801587644874,10.0293361230424));
#65636=CARTESIAN_POINT('Ctrl Pts',(0.299435754494424,1.98083821523551,10.0293810170383));
#65637=CARTESIAN_POINT('Ctrl Pts',(0.29956702524685,1.98116860936139,10.0294028515589));
#65638=CARTESIAN_POINT('Ctrl Pts',(0.299879677716944,1.9819593319255,10.0294551175539));
#65639=CARTESIAN_POINT('Ctrl Pts',(0.300060546166007,1.98241986112747,10.0294855662441));
#65640=CARTESIAN_POINT('Ctrl Pts',(0.300599729566863,1.98380208213375,10.0295769797203));
#65641=CARTESIAN_POINT('Ctrl Pts',(0.300954861026685,1.98472500218336,10.0296380512263));
#65642=CARTESIAN_POINT('Ctrl Pts',(0.304058379934767,1.99290256438331,10.030179501053));
#65643=CARTESIAN_POINT('Ctrl Pts',(0.306548023346412,2.00025205919967,10.030668467506));
#65644=CARTESIAN_POINT('Ctrl Pts',(0.310662501093312,2.01401374049299,10.0315895083546));
#65645=CARTESIAN_POINT('Ctrl Pts',(0.312359840783128,2.02040008244564,10.0320190321001));
#65646=CARTESIAN_POINT('Ctrl Pts',(0.31761456941973,2.04294117313595,10.0335414190866));
#65647=CARTESIAN_POINT('Ctrl Pts',(0.320123685651727,2.05931257776974,10.0346599663261));
#65648=CARTESIAN_POINT('Ctrl Pts',(0.322808464585944,2.09496919208831,10.0370793280725));
#65649=CARTESIAN_POINT('Ctrl Pts',(0.322534243252063,2.11422892232142,10.0383756988085));
#65650=CARTESIAN_POINT('Ctrl Pts',(0.32042751547386,2.13447700439629,10.0396588409609));
#65651=CARTESIAN_POINT('Ctrl Pts',(0.320304461898369,2.13560208256892,10.0397298679327));
#65652=CARTESIAN_POINT('Ctrl Pts',(0.320131972249648,2.13710581810401,10.0398244168798));
#65653=CARTESIAN_POINT('Ctrl Pts',(0.320087788372978,2.1374850521102,10.039848229011));
#65654=CARTESIAN_POINT('Ctrl Pts',(0.320017675697562,2.13807767154349,10.0398853877054));
#65655=CARTESIAN_POINT('Ctrl Pts',(0.31999220734791,2.13829110949441,10.0398987602574));
#65656=CARTESIAN_POINT('Ctrl Pts',(0.319940871747783,2.13871770025601,10.039925466224));
#65657=CARTESIAN_POINT('Ctrl Pts',(0.319915005221037,2.13893085103824,10.039938799498));
#65658=CARTESIAN_POINT('Ctrl Pts',(0.31985584637584,2.13941430367954,10.0399690170347));
#65659=CARTESIAN_POINT('Ctrl Pts',(0.319822424494001,2.13968458879009,10.0399858938383));
#65660=CARTESIAN_POINT('Ctrl Pts',(0.319751749917167,2.1402502507352,10.0400211792267));
#65661=CARTESIAN_POINT('Ctrl Pts',(0.319714430431215,2.14054561918466,10.0400395840306));
#65662=CARTESIAN_POINT('Ctrl Pts',(0.319615473795863,2.14132018835923,10.040087797096));
#65663=CARTESIAN_POINT('Ctrl Pts',(0.319553167957908,2.14179930514878,10.0401175681276));
#65664=CARTESIAN_POINT('Ctrl Pts',(0.319364365143869,2.14322605583921,10.0402060736799));
#65665=CARTESIAN_POINT('Ctrl Pts',(0.319234727294358,2.14417327890292,10.0402646369325));
#65666=CARTESIAN_POINT('Ctrl Pts',(0.317713408985149,2.1549324724664,10.0409277538621));
#65667=CARTESIAN_POINT('Ctrl Pts',(0.315873912944015,2.16467689009704,10.0415086670916));
#65668=CARTESIAN_POINT('Ctrl Pts',(0.306566166799982,2.20394921670598,10.0438252563361));
#65669=CARTESIAN_POINT('Ctrl Pts',(0.295381578901694,2.23243173423859,10.0454630598711));
#65670=CARTESIAN_POINT('Ctrl Pts',(0.275823699545849,2.26693496690597,10.0477766090386));
#65671=CARTESIAN_POINT('Ctrl Pts',(0.270941100815863,2.27474808060135,10.0483239516167));
#65672=CARTESIAN_POINT('Ctrl Pts',(0.265086969010754,2.28327948655966,10.0489531946683));
#65673=CARTESIAN_POINT('Ctrl Pts',(0.264437970117213,2.28421463362371,10.0490226066098));
#65674=CARTESIAN_POINT('Ctrl Pts',(0.263486216019777,2.28557062896258,10.0491239055313));
#65675=CARTESIAN_POINT('Ctrl Pts',(0.263187372965285,2.28599422322389,10.0491556427783));
#65676=CARTESIAN_POINT('Ctrl Pts',(0.262658014215155,2.28674073097179,10.0492117389238));
#65677=CARTESIAN_POINT('Ctrl Pts',(0.262427921269005,2.28706394407133,10.0492360815443));
#65678=CARTESIAN_POINT('Ctrl Pts',(0.261950830653486,2.28773150382335,10.049286472444));
#65679=CARTESIAN_POINT('Ctrl Pts',(0.261703749579431,2.28807578967311,10.0493125239089));
#65680=CARTESIAN_POINT('Ctrl Pts',(0.261069126621931,2.28895640924114,10.0493793208585));
#65681=CARTESIAN_POINT('Ctrl Pts',(0.260680612075579,2.28949203662928,10.0494201039213));
#65682=CARTESIAN_POINT('Ctrl Pts',(0.259085279263435,2.2916772580937,10.0495871250029));
#65683=CARTESIAN_POINT('Ctrl Pts',(0.257864451417593,2.2933165217645,10.0497139069075));
#65684=CARTESIAN_POINT('Ctrl Pts',(0.249691029458126,2.30407617424146,10.0505561218514));
#65685=CARTESIAN_POINT('Ctrl Pts',(0.242272222905628,2.31283047775968,10.0512900464087));
#65686=CARTESIAN_POINT('Ctrl Pts',(0.230993583310355,2.32478395707709,10.0523655881955));
#65687=CARTESIAN_POINT('Ctrl Pts',(0.227500733080137,2.32831836522635,10.0526936302465));
#65688=CARTESIAN_POINT('Ctrl Pts',(0.221149700209213,2.334454487639,10.0532808609856));
#65689=CARTESIAN_POINT('Ctrl Pts',(0.218323735815392,2.33708825744754,10.0535390780551));
#65690=CARTESIAN_POINT('Ctrl Pts',(0.194683860401407,2.35833925820666,10.0556724792574));
#65691=CARTESIAN_POINT('Ctrl Pts',(0.171577836929273,2.37423013679064,10.0576037036079));
#65692=CARTESIAN_POINT('Ctrl Pts',(0.145370249745591,2.38762986132018,10.0594654836716));
#65693=CARTESIAN_POINT('Ctrl Pts',(0.144023647930538,2.38830649607923,10.0595602695413));
#65694=CARTESIAN_POINT('Ctrl Pts',(0.142293638560569,2.38916063771463,10.0596808774873));
#65695=CARTESIAN_POINT('Ctrl Pts',(0.141914588918462,2.38934685661899,10.0597072317602));
#65696=CARTESIAN_POINT('Ctrl Pts',(0.141310303128175,2.38964225607499,10.0597491313995));
#65697=CARTESIAN_POINT('Ctrl Pts',(0.14108530559608,2.38975191944191,10.0597647068882));
#65698=CARTESIAN_POINT('Ctrl Pts',(0.140667597538195,2.3899549076566,10.0597935756167));
#65699=CARTESIAN_POINT('Ctrl Pts',(0.140474923219946,2.39004830187067,10.0598068731337));
#65700=CARTESIAN_POINT('Ctrl Pts',(0.140042562181576,2.39025734654998,10.0598366711179));
#65701=CARTESIAN_POINT('Ctrl Pts',(0.139802825765173,2.39037289191299,10.0598531649365));
#65702=CARTESIAN_POINT('Ctrl Pts',(0.139302312836595,2.39061335976269,10.0598875409973));
#65703=CARTESIAN_POINT('Ctrl Pts',(0.139041510597097,2.39073822859509,10.059905419894));
#65704=CARTESIAN_POINT('Ctrl Pts',(0.138362997413867,2.39106197038264,10.059951848352));
#65705=CARTESIAN_POINT('Ctrl Pts',(0.137945023846851,2.39126029605574,10.0599803643388));
#65706=CARTESIAN_POINT('Ctrl Pts',(0.136712012319527,2.39184210225519,10.0600642409506));
#65707=CARTESIAN_POINT('Ctrl Pts',(0.135895784014709,2.39222307043142,10.060119450942));
#65708=CARTESIAN_POINT('Ctrl Pts',(0.133051519628272,2.39353611423178,10.0603107826097));
#65709=CARTESIAN_POINT('Ctrl Pts',(0.131015354820701,2.39445056401582,10.0604458944035));
#65710=CARTESIAN_POINT('Ctrl Pts',(0.121643065576511,2.39854322530255,10.0610600536024));
#65711=CARTESIAN_POINT('Ctrl Pts',(0.114199220759256,2.40146915449024,10.0615262725987));
#65712=CARTESIAN_POINT('Ctrl Pts',(0.0785255281206204,2.41397996879105,
10.0636941082193));
#65713=CARTESIAN_POINT('Ctrl Pts',(0.0491651148219065,2.41989473106437,
10.0652998090308));
#65714=CARTESIAN_POINT('Ctrl Pts',(0.00981194732096487,2.42226903786307,
10.0675955972732));
#65715=CARTESIAN_POINT('Ctrl Pts',(0.000195004456875578,2.42241827066467,
10.0681663027694));
#65716=CARTESIAN_POINT('Ctrl Pts',(-0.0105491199298504,2.42210430337797,
10.0688199306789));
#65717=CARTESIAN_POINT('Ctrl Pts',(-0.0116844687873054,2.42206511658875,
10.0688891979826));
#65718=CARTESIAN_POINT('Ctrl Pts',(-0.0132980408704505,2.4220008804739,
10.0689879297154));
#65719=CARTESIAN_POINT('Ctrl Pts',(-0.0137764611758626,2.42198076655372,
10.0690172394603));
#65720=CARTESIAN_POINT('Ctrl Pts',(-0.0146542047701276,2.42194190425937,
10.0690710799557));
#65721=CARTESIAN_POINT('Ctrl Pts',(-0.0150535420119537,2.42192347896077,
10.0690956005338));
#65722=CARTESIAN_POINT('Ctrl Pts',(-0.0158629427642707,2.42188462411497,
10.0691453521569));
#65723=CARTESIAN_POINT('Ctrl Pts',(-0.0162730034983033,2.42186415387464,
10.0691705844336));
#65724=CARTESIAN_POINT('Ctrl Pts',(-0.0172828762691735,2.42181180619153,
10.0692327919395));
#65725=CARTESIAN_POINT('Ctrl Pts',(-0.0178826386742273,2.42177903543059,
10.069269795128));
#65726=CARTESIAN_POINT('Ctrl Pts',(-0.0200732184320803,2.42165319972201,
10.069405161047));
#65727=CARTESIAN_POINT('Ctrl Pts',(-0.0216634109427543,2.42155001394733,
10.0695038407802));
#65728=CARTESIAN_POINT('Ctrl Pts',(-0.0308585546252037,2.42088483326614,
10.0700769067982));
#65729=CARTESIAN_POINT('Ctrl Pts',(-0.0384418589597235,2.42006489058921,
10.0705593454794));
#65730=CARTESIAN_POINT('Ctrl Pts',(-0.0572952377763669,2.41734670606582,
10.0717846142746));
#65731=CARTESIAN_POINT('Ctrl Pts',(-0.0685062651080066,2.41511668192953,
10.0725367942953));
#65732=CARTESIAN_POINT('Ctrl Pts',(-0.0827250179006591,2.41149368892836,
10.0735176224775));
#65733=CARTESIAN_POINT('Ctrl Pts',(-0.0858633084840799,2.41064326558604,
10.0737357880406));
#65734=CARTESIAN_POINT('Ctrl Pts',(-0.0915917984008716,2.40899750260009,
10.0741368471783));
#65735=CARTESIAN_POINT('Ctrl Pts',(-0.0941858918084206,2.40821669598797,
10.074319538732));
#65736=CARTESIAN_POINT('Ctrl Pts',(-0.0989884622834605,2.40670485841018,
10.0746595819456));
#65737=CARTESIAN_POINT('Ctrl Pts',(-0.101199478592809,2.40598243623779,
10.074816855182));
#65738=CARTESIAN_POINT('Ctrl Pts',(-0.107818674728302,2.40374010271626,
10.0752896496324));
#65739=CARTESIAN_POINT('Ctrl Pts',(-0.11220189867558,2.40214839191601,10.0756053726803));
#65740=CARTESIAN_POINT('Ctrl Pts',(-0.129177695927073,2.39556349220256,
10.0768358176508));
#65741=CARTESIAN_POINT('Ctrl Pts',(-0.141486106149191,2.38987307802758,
10.0777452325721));
#65742=CARTESIAN_POINT('Ctrl Pts',(-0.157296139880944,2.38131604874326,
10.0789071394773));
#65743=CARTESIAN_POINT('Ctrl Pts',(-0.161147908016124,2.37912748255708,
10.0791896371829));
#65744=CARTESIAN_POINT('Ctrl Pts',(-0.165478887266146,2.37654707994299,
10.079505567464));
#65745=CARTESIAN_POINT('Ctrl Pts',(-0.16600332705698,2.37623259216902,10.0795437944543));
#65746=CARTESIAN_POINT('Ctrl Pts',(-0.166770336862275,2.37576967061939,
10.0795996562494));
#65747=CARTESIAN_POINT('Ctrl Pts',(-0.167013606618918,2.37562240782694,
10.0796173668758));
#65748=CARTESIAN_POINT('Ctrl Pts',(-0.167440375738403,2.37536329163493,
10.0796484242046));
#65749=CARTESIAN_POINT('Ctrl Pts',(-0.167623958324693,2.37525157656968,
10.0796617800078));
#65750=CARTESIAN_POINT('Ctrl Pts',(-0.168007895648443,2.37501741355672,
10.0796897031084));
#65751=CARTESIAN_POINT('Ctrl Pts',(-0.168208227897725,2.37489493052437,
10.0797042680053));
#65752=CARTESIAN_POINT('Ctrl Pts',(-0.168617436603636,2.37464412572187,
10.0797340093067));
#65753=CARTESIAN_POINT('Ctrl Pts',(-0.168826300927369,2.37451578431203,
10.0797491844028));
#65754=CARTESIAN_POINT('Ctrl Pts',(-0.169339320966691,2.37419974059354,
10.0797864458234));
#65755=CARTESIAN_POINT('Ctrl Pts',(-0.169643312154016,2.37401176984087,
10.0798085146099));
#65756=CARTESIAN_POINT('Ctrl Pts',(-0.170481351914948,2.37349164485476,
10.0798693262738));
#65757=CARTESIAN_POINT('Ctrl Pts',(-0.171014745343242,2.37315843030494,
10.0799080008233));
#65758=CARTESIAN_POINT('Ctrl Pts',(-0.172706811089052,2.37209448633088,
10.080030600397));
#65759=CARTESIAN_POINT('Ctrl Pts',(-0.17386181949199,2.37135791855282,10.0801141580076));
#65760=CARTESIAN_POINT('Ctrl Pts',(-0.178340812662885,2.36846125354458,
10.080437824106));
#65761=CARTESIAN_POINT('Ctrl Pts',(-0.181629668934853,2.36624717197366,
10.0806747085568));
#65762=CARTESIAN_POINT('Ctrl Pts',(-0.190121772504208,2.36029961146984,
10.0812866340461));
#65763=CARTESIAN_POINT('Ctrl Pts',(-0.195256212302711,2.35647065480835,
10.0816568964678));
#65764=CARTESIAN_POINT('Ctrl Pts',(-0.223204838544721,2.33430207943499,
10.083694306211));
#65765=CARTESIAN_POINT('Ctrl Pts',(-0.243551203222896,2.31307461682332,
10.0852752850844));
#65766=CARTESIAN_POINT('Ctrl Pts',(-0.266156278462439,2.28195204779663,
10.0875192617124));
#65767=CARTESIAN_POINT('Ctrl Pts',(-0.271238260151538,2.27428566776057,
10.0880657110223));
#65768=CARTESIAN_POINT('Ctrl Pts',(-0.276572796725634,2.26543868447924,
10.0886939876289));
#65769=CARTESIAN_POINT('Ctrl Pts',(-0.277155151356056,2.26446121802928,
10.0887633696755));
#65770=CARTESIAN_POINT('Ctrl Pts',(-0.277995235659732,2.26303402473525,
10.0888646329674));
#65771=CARTESIAN_POINT('Ctrl Pts',(-0.278257080324322,2.26258671998448,
10.0888963646294));
#65772=CARTESIAN_POINT('Ctrl Pts',(-0.278717443517387,2.26179591991917,
10.0889524542699));
#65773=CARTESIAN_POINT('Ctrl Pts',(-0.278916409446151,2.26145268521394,
10.0889767959825));
#65774=CARTESIAN_POINT('Ctrl Pts',(-0.279326607812478,2.26074203372973,
10.0890271882922));
#65775=CARTESIAN_POINT('Ctrl Pts',(-0.279537750199431,2.26037456609545,
10.0890532420813));
#65776=CARTESIAN_POINT('Ctrl Pts',(-0.280076777295388,2.25943215645658,
10.0891200518152));
#65777=CARTESIAN_POINT('Ctrl Pts',(-0.280403615619079,2.25885662098217,
10.0891608453661));
#65778=CARTESIAN_POINT('Ctrl Pts',(-0.28173318929537,2.25649846293582,10.0893279624801));
#65779=CARTESIAN_POINT('Ctrl Pts',(-0.282720699522567,2.25470735148448,
10.0894548307171));
#65780=CARTESIAN_POINT('Ctrl Pts',(-0.289138256698171,2.24280074309152,
10.0902979225703));
#65781=CARTESIAN_POINT('Ctrl Pts',(-0.294040889921586,2.23241180373817,
10.0910326791248));
#65782=CARTESIAN_POINT('Ctrl Pts',(-0.311442017544307,2.18977810527554,
10.0940464125566));
#65783=CARTESIAN_POINT('Ctrl Pts',(-0.319268929465149,2.15588456150291,
10.0964678626981));
#65784=CARTESIAN_POINT('Ctrl Pts',(-0.321696806114809,2.11939981487197,
10.0988163687835));
#65785=CARTESIAN_POINT('Ctrl Pts',(-0.321811173040243,2.11739992055465,
10.0989441957669));
#65786=CARTESIAN_POINT('Ctrl Pts',(-0.321987311309268,2.11371786375243,
10.0991777192447));
#65787=CARTESIAN_POINT('Ctrl Pts',(-0.322054564250783,2.11203604448895,
10.0992836849202));
#65788=CARTESIAN_POINT('Ctrl Pts',(-0.322122783971838,2.10991370253467,
10.0994164600543));
#65789=CARTESIAN_POINT('Ctrl Pts',(-0.322136026533639,2.10947364060515,
10.0994439393119));
#65790=CARTESIAN_POINT('Ctrl Pts',(-0.322155500553171,2.10877917124101,
10.0994872223651));
#65791=CARTESIAN_POINT('Ctrl Pts',(-0.322162332459915,2.10852478324684,
10.0995030597352));
#65792=CARTESIAN_POINT('Ctrl Pts',(-0.322173911592672,2.10807372378392,
10.0995311099667));
#65793=CARTESIAN_POINT('Ctrl Pts',(-0.322178780022493,2.10787705721271,
10.0995433295934));
#65794=CARTESIAN_POINT('Ctrl Pts',(-0.32218840795021,2.1074731765057,10.0995684025574));
#65795=CARTESIAN_POINT('Ctrl Pts',(-0.322193147609165,2.10726596303698,
10.0995812547188));
#65796=CARTESIAN_POINT('Ctrl Pts',(-0.322203252332036,2.10680473110434,
10.0996098363601));
#65797=CARTESIAN_POINT('Ctrl Pts',(-0.322208516919066,2.10655071023746,
10.0996255601846));
#65798=CARTESIAN_POINT('Ctrl Pts',(-0.322220884430889,2.10591784060842,
10.0996646920056));
#65799=CARTESIAN_POINT('Ctrl Pts',(-0.32222761964591,2.10553898381157,10.0996880795481));
#65800=CARTESIAN_POINT('Ctrl Pts',(-0.322260867011647,2.10346278515451,
10.0998160428866));
#65801=CARTESIAN_POINT('Ctrl Pts',(-0.322274636765795,2.10176523081878,
10.0999199208158));
#65802=CARTESIAN_POINT('Ctrl Pts',(-0.322274992908106,2.10006760976513,
10.1000231250268));
#65803=CARTESIAN_POINT('',(-0.322021890547819,2.10026805526597,10.2247225257975));
#65804=CARTESIAN_POINT('Ctrl Pts',(-0.32279818296466,2.10004841125406,10.0997227245674));
#65805=CARTESIAN_POINT('Ctrl Pts',(-0.32257517298749,1.99588884229921,10.1061816902479));
#65806=CARTESIAN_POINT('Ctrl Pts',(-0.21115554484217,1.78450861019514,10.1192641037693));
#65807=CARTESIAN_POINT('Ctrl Pts',(0.14909372275915,1.74930620373942,10.1389699651317));
#65808=CARTESIAN_POINT('Ctrl Pts',(0.375576748934469,2.03552378297651,10.1588403086545));
#65809=CARTESIAN_POINT('Ctrl Pts',(0.25751923811976,2.38088951368832,10.1787106521773));
#65810=CARTESIAN_POINT('Ctrl Pts',(-0.0967771155912757,2.46857735524538,
10.1985809957001));
#65811=CARTESIAN_POINT('Ctrl Pts',(-0.301720943666828,2.27527702420129,
10.2139182869069));
#65812=CARTESIAN_POINT('Ctrl Pts',(-0.322284932565275,2.13418886036719,
10.2226321302726));
#65813=CARTESIAN_POINT('Ctrl Pts',(-0.322021890547819,2.10026805526597,
10.2247225257975));
#65814=CARTESIAN_POINT('',(-0.32227501893165,2.09982663045473,10.4749490325485));
#65815=CARTESIAN_POINT('Ctrl Pts',(-0.322274896795217,2.10025791594028,
10.2245769286166));
#65816=CARTESIAN_POINT('Ctrl Pts',(-0.322289186763215,2.08240210618882,
10.2255878655148));
#65817=CARTESIAN_POINT('Ctrl Pts',(-0.320819566308015,2.06457809785206,
10.2266228926931));
#65818=CARTESIAN_POINT('Ctrl Pts',(-0.317749005383167,2.04617253167104,
10.2277574470772));
#65819=CARTESIAN_POINT('Ctrl Pts',(-0.317613233356406,2.04537710418631,
10.2278066036694));
#65820=CARTESIAN_POINT('Ctrl Pts',(-0.317386802593762,2.04407993994302,
10.2278869741934));
#65821=CARTESIAN_POINT('Ctrl Pts',(-0.317297937453292,2.04357789032069,
10.2279181312054));
#65822=CARTESIAN_POINT('Ctrl Pts',(-0.317139251707659,2.04269361622364,
10.2279730991149));
#65823=CARTESIAN_POINT('Ctrl Pts',(-0.317069930372312,2.04231130226097,
10.2279968941079));
#65824=CARTESIAN_POINT('Ctrl Pts',(-0.316928446102455,2.04153896165246,
10.2280450246363));
#65825=CARTESIAN_POINT('Ctrl Pts',(-0.316856254180393,2.04114894106235,
10.2280693610562));
#65826=CARTESIAN_POINT('Ctrl Pts',(-0.316714825281104,2.04039266817819,
10.2281166117624));
#65827=CARTESIAN_POINT('Ctrl Pts',(-0.316645672528919,2.04002640058617,
10.2281395233296));
#65828=CARTESIAN_POINT('Ctrl Pts',(-0.316479287063874,2.03915344983397,
10.228194196631));
#65829=CARTESIAN_POINT('Ctrl Pts',(-0.316381472969988,2.03864687975364,
10.2282259768727));
#65830=CARTESIAN_POINT('Ctrl Pts',(-0.316082741725912,2.03711949070694,
10.2283219620967));
#65831=CARTESIAN_POINT('Ctrl Pts',(-0.315878098760873,2.0360994151166,10.2283862859247));
#65832=CARTESIAN_POINT('Ctrl Pts',(-0.313698295684725,2.02550023138706,
10.2290569653176));
#65833=CARTESIAN_POINT('Ctrl Pts',(-0.311293176051704,2.01601570756492,
10.2296770624348));
#65834=CARTESIAN_POINT('Ctrl Pts',(-0.306633324098645,2.00061695603321,
10.2307184494957));
#65835=CARTESIAN_POINT('Ctrl Pts',(-0.304628990680189,1.9946332347348,10.2311319335632));
#65836=CARTESIAN_POINT('Ctrl Pts',(-0.301630268935016,1.98648349238708,
10.2317067818988));
#65837=CARTESIAN_POINT('Ctrl Pts',(-0.300785506333512,1.98426368122619,
10.2318645692362));
#65838=CARTESIAN_POINT('Ctrl Pts',(-0.291491246625091,1.96063009646229,
10.2335570552045));
#65839=CARTESIAN_POINT('Ctrl Pts',(-0.280795620286707,1.94017235607578,
10.2351395371016));
#65840=CARTESIAN_POINT('Ctrl Pts',(-0.264497698000053,1.91576592051357,
10.2370810044563));
#65841=CARTESIAN_POINT('Ctrl Pts',(-0.260828605663076,1.9106070804191,10.237494330679));
#65842=CARTESIAN_POINT('Ctrl Pts',(-0.255220716385519,1.90319462967187,
10.2380888941103));
#65843=CARTESIAN_POINT('Ctrl Pts',(-0.253399087442226,1.9008546463468,10.2382766871127));
#65844=CARTESIAN_POINT('Ctrl Pts',(-0.251230253392885,1.8981466139241,10.2384938075672));
#65845=CARTESIAN_POINT('Ctrl Pts',(-0.250914238234083,1.89775392525496,
10.2385252866926));
#65846=CARTESIAN_POINT('Ctrl Pts',(-0.250430235487796,1.89715537134316,
10.2385732584181));
#65847=CARTESIAN_POINT('Ctrl Pts',(-0.250262914271691,1.89694897202214,
10.238589798649));
#65848=CARTESIAN_POINT('Ctrl Pts',(-0.249971239873216,1.89659008486088,
10.2386185552105));
#65849=CARTESIAN_POINT('Ctrl Pts',(-0.249847002642167,1.89643750440697,
10.2386307798773));
#65850=CARTESIAN_POINT('Ctrl Pts',(-0.249565467325961,1.89609238622371,
10.2386584279182));
#65851=CARTESIAN_POINT('Ctrl Pts',(-0.2494080864596,1.89589991708202,10.2386738451439));
#65852=CARTESIAN_POINT('Ctrl Pts',(-0.248980605991111,1.89537836205425,
10.2387156185595));
#65853=CARTESIAN_POINT('Ctrl Pts',(-0.248710075562783,1.89504962748558,
10.238741943506));
#65854=CARTESIAN_POINT('Ctrl Pts',(-0.247488309677663,1.89357098234382,
10.2388603366209));
#65855=CARTESIAN_POINT('Ctrl Pts',(-0.24652972554941,1.89242712754289,10.2389518791127));
#65856=CARTESIAN_POINT('Ctrl Pts',(-0.2270735993675,1.86953551928615,10.2407839546233));
#65857=CARTESIAN_POINT('Ctrl Pts',(-0.205771740181726,1.85033042717011,
10.2423300020338));
#65858=CARTESIAN_POINT('Ctrl Pts',(-0.174358043342163,1.8287968143773,10.2444717581156));
#65859=CARTESIAN_POINT('Ctrl Pts',(-0.166267415039652,1.82376273558261,
10.2450120249765));
#65860=CARTESIAN_POINT('Ctrl Pts',(-0.152254961981358,1.8158828869014,10.2459416839309));
#65861=CARTESIAN_POINT('Ctrl Pts',(-0.146447500848813,1.81284633238072,
10.2463252832646));
#65862=CARTESIAN_POINT('Ctrl Pts',(-0.135862035555112,1.80771616098096,
10.2470246592357));
#65863=CARTESIAN_POINT('Ctrl Pts',(-0.131118066165703,1.80555750440072,
10.2473381415954));
#65864=CARTESIAN_POINT('Ctrl Pts',(-0.125500300067949,1.80316393068865,
10.2477101674222));
#65865=CARTESIAN_POINT('Ctrl Pts',(-0.124675103988472,1.80281639382124,
10.2477648339227));
#65866=CARTESIAN_POINT('Ctrl Pts',(-0.123489723870174,1.80232296909608,
10.2478433929205));
#65867=CARTESIAN_POINT('Ctrl Pts',(-0.123130702395561,1.80217428459787,
10.2478671905697));
#65868=CARTESIAN_POINT('Ctrl Pts',(-0.122404655649986,1.80187513816042,
10.2479153251275));
#65869=CARTESIAN_POINT('Ctrl Pts',(-0.12203761980767,1.80172470380358,10.2479396629184));
#65870=CARTESIAN_POINT('Ctrl Pts',(-0.121325191944509,1.80143424119896,
10.2479869124249));
#65871=CARTESIAN_POINT('Ctrl Pts',(-0.120979832739626,1.80129413364098,
10.2480098214143));
#65872=CARTESIAN_POINT('Ctrl Pts',(-0.120155957729404,1.80096156188959,
10.2480644824227));
#65873=CARTESIAN_POINT('Ctrl Pts',(-0.119677222516891,1.80076964717615,
10.24809625293));
#65874=CARTESIAN_POINT('Ctrl Pts',(-0.118231989138262,1.80019430708374,
10.2481921895673));
#65875=CARTESIAN_POINT('Ctrl Pts',(-0.117264101098603,1.79981441188242,
10.2482564743766));
#65876=CARTESIAN_POINT('Ctrl Pts',(-0.10719448462534,1.79591822830214,10.2489256687463));
#65877=CARTESIAN_POINT('Ctrl Pts',(-0.0979402591169397,1.79281267297462,
10.2495442535744));
#65878=CARTESIAN_POINT('Ctrl Pts',(-0.0825642552487831,1.78841821766854,
10.2505792789928));
#65879=CARTESIAN_POINT('Ctrl Pts',(-0.0765201606717785,1.78687906346459,
10.250987854762));
#65880=CARTESIAN_POINT('Ctrl Pts',(-0.0516971704430958,1.7813194123793,
10.2526712626576));
#65881=CARTESIAN_POINT('Ctrl Pts',(-0.0326220444416347,1.77880594115431,
10.2539802864642));
#65882=CARTESIAN_POINT('Ctrl Pts',(-0.0107480220564935,1.77789301861101,
10.2554546940015));
#65883=CARTESIAN_POINT('Ctrl Pts',(-0.00805610718413378,1.77781445259254,
10.2556356211309));
#65884=CARTESIAN_POINT('Ctrl Pts',(0.00385066369330159,1.77761626566589,
10.2564328642348));
#65885=CARTESIAN_POINT('Ctrl Pts',(0.013067981666414,1.77785817320986,10.2570421222263));
#65886=CARTESIAN_POINT('Ctrl Pts',(0.0258782267889083,1.77874523224125,
10.257867300995));
#65887=CARTESIAN_POINT('Ctrl Pts',(0.0294892036004231,1.77905655007578,
10.2580974898134));
#65888=CARTESIAN_POINT('Ctrl Pts',(0.0336220472947169,1.77948320636909,
10.2583575906857));
#65889=CARTESIAN_POINT('Ctrl Pts',(0.0341496198844267,1.7795389874961,10.2583907306631));
#65890=CARTESIAN_POINT('Ctrl Pts',(0.0349467321499745,1.7796252583088,10.2584407045574));
#65891=CARTESIAN_POINT('Ctrl Pts',(0.0352163717474638,1.77965478563913,
10.2584575923881));
#65892=CARTESIAN_POINT('Ctrl Pts',(0.0357028758430757,1.77970868275124,
10.2584880318516));
#65893=CARTESIAN_POINT('Ctrl Pts',(0.0359197522951721,1.7797329323137,10.2585015902357));
#65894=CARTESIAN_POINT('Ctrl Pts',(0.0363545920404164,1.77978200021622,
10.2585287526718));
#65895=CARTESIAN_POINT('Ctrl Pts',(0.0365725536536326,1.77980682070367,
10.2585423565409));
#65896=CARTESIAN_POINT('Ctrl Pts',(0.0371915625517916,1.77987795095816,
10.2585809600463));
#65897=CARTESIAN_POINT('Ctrl Pts',(0.0375925502096143,1.77992479199297,
10.2586059296149));
#65898=CARTESIAN_POINT('Ctrl Pts',(0.0392861385887283,1.78012585360475,
10.2587112356613));
#65899=CARTESIAN_POINT('Ctrl Pts',(0.0405779098421487,1.78028715448827,
10.2587911779562));
#65900=CARTESIAN_POINT('Ctrl Pts',(0.0658722427759269,1.78360138231084,
10.2603497261576));
#65901=CARTESIAN_POINT('Ctrl Pts',(0.0894494086236765,1.78944170706587,
10.2616856986518));
#65902=CARTESIAN_POINT('Ctrl Pts',(0.125252625922606,1.80273210048699,10.2638213674105));
#65903=CARTESIAN_POINT('Ctrl Pts',(0.138021612273087,1.80844138989162,10.2646057966907));
#65904=CARTESIAN_POINT('Ctrl Pts',(0.157349493077741,1.81863827322671,10.2658689643433));
#65905=CARTESIAN_POINT('Ctrl Pts',(0.164182145611151,1.82256984103195,10.2663312666692));
#65906=CARTESIAN_POINT('Ctrl Pts',(0.1731426001874,1.82817277370093,10.2669631005404));
#65907=CARTESIAN_POINT('Ctrl Pts',(0.175403742118743,1.8296263186784,10.267124799998));
#65908=CARTESIAN_POINT('Ctrl Pts',(0.179153710418547,1.83210377500325,10.2673969205519));
#65909=CARTESIAN_POINT('Ctrl Pts',(0.18065260914817,1.83311224470635,10.2675067658514));
#65910=CARTESIAN_POINT('Ctrl Pts',(0.182662229796387,1.83448901778054,10.2676555281578));
#65911=CARTESIAN_POINT('Ctrl Pts',(0.183180486756208,1.8348463065763,10.2676940270045));
#65912=CARTESIAN_POINT('Ctrl Pts',(0.183998891571361,1.8354140632816,10.2677550375467));
#65913=CARTESIAN_POINT('Ctrl Pts',(0.184299734682345,1.83562353016409,10.2677775110391));
#65914=CARTESIAN_POINT('Ctrl Pts',(0.184922829725932,1.83605895057268,10.2678241535532));
#65915=CARTESIAN_POINT('Ctrl Pts',(0.185245026296541,1.83628498192774,10.2678483255271));
#65916=CARTESIAN_POINT('Ctrl Pts',(0.185979875680278,1.83680251383722,10.2679035786525));
#65917=CARTESIAN_POINT('Ctrl Pts',(0.186392257934494,1.83709439515692,10.267934674381));
#65918=CARTESIAN_POINT('Ctrl Pts',(0.18765215391923,1.83799059513652,10.2680299504132));
#65919=CARTESIAN_POINT('Ctrl Pts',(0.18849742138888,1.83859804668583,10.2680942512828));
#65920=CARTESIAN_POINT('Ctrl Pts',(0.194738023071094,1.84312886412046,10.2685718315196));
#65921=CARTESIAN_POINT('Ctrl Pts',(0.200012973693616,1.84721456190441,10.2689914060697));
#65922=CARTESIAN_POINT('Ctrl Pts',(0.206600154996923,1.85265195961018,10.2695367547646));
#65923=CARTESIAN_POINT('Ctrl Pts',(0.208032826312183,1.85385569257473,10.2696567094761));
#65924=CARTESIAN_POINT('Ctrl Pts',(0.210842751077901,1.8562586521992,10.2698946569848));
#65925=CARTESIAN_POINT('Ctrl Pts',(0.212220457098058,1.85745724563736,10.2700126231219));
#65926=CARTESIAN_POINT('Ctrl Pts',(0.215518019065318,1.86037570532157,10.2702981294229));
#65927=CARTESIAN_POINT('Ctrl Pts',(0.217427552842903,1.86210700333985,10.2704660834801));
#65928=CARTESIAN_POINT('Ctrl Pts',(0.237790579035869,1.88101933340853,10.2722855149302));
#65929=CARTESIAN_POINT('Ctrl Pts',(0.254186611715538,1.90028570784347,10.2740151155493));
#65930=CARTESIAN_POINT('Ctrl Pts',(0.273084475597025,1.92863884876591,10.2762957974566));
#65931=CARTESIAN_POINT('Ctrl Pts',(0.27769539110461,1.93621639172546,10.2768820103732));
#65932=CARTESIAN_POINT('Ctrl Pts',(0.283866325917067,1.94736929244823,10.2777025005035));
#65933=CARTESIAN_POINT('Ctrl Pts',(0.285683058870289,1.95079739580824,10.2779491786113));
#65934=CARTESIAN_POINT('Ctrl Pts',(0.287681366006325,1.95473851866833,10.2782258366814));
#65935=CARTESIAN_POINT('Ctrl Pts',(0.287923979962347,1.95522000110996,10.2782595191284));
#65936=CARTESIAN_POINT('Ctrl Pts',(0.28828763770042,1.95594623183476,10.2783101451791));
#65937=CARTESIAN_POINT('Ctrl Pts',(0.288409579060359,1.95619052576048,10.2783271448254));
#65938=CARTESIAN_POINT('Ctrl Pts',(0.288628484209064,1.95663047252122,10.2783577045202));
#65939=CARTESIAN_POINT('Ctrl Pts',(0.288725559394213,1.9568260685049,10.2783712715666));
#65940=CARTESIAN_POINT('Ctrl Pts',(0.28893371816455,1.95724655854101,10.2784003959263));
#65941=CARTESIAN_POINT('Ctrl Pts',(0.28904473767325,1.95747148297549,10.2784159491646));
#65942=CARTESIAN_POINT('Ctrl Pts',(0.28934297783424,1.95807749620927,10.2784577857074));
#65943=CARTESIAN_POINT('Ctrl Pts',(0.289529708970822,1.95845882743037,10.278484038322));
#65944=CARTESIAN_POINT('Ctrl Pts',(0.290385141304568,1.96021451668704,10.278604578435));
#65945=CARTESIAN_POINT('Ctrl Pts',(0.291044828172861,1.9615932810663,10.2786983121904));
#65946=CARTESIAN_POINT('Ctrl Pts',(0.304007117161189,1.98918735780193,10.2805568443567));
#65947=CARTESIAN_POINT('Ctrl Pts',(0.312732948275626,2.01694278963421,10.2821222149668));
#65948=CARTESIAN_POINT('Ctrl Pts',(0.31958088425493,2.05684955171536,10.2844011476943));
#65949=CARTESIAN_POINT('Ctrl Pts',(0.320918958240834,2.06829992143884,10.2850568632171));
#65950=CARTESIAN_POINT('Ctrl Pts',(0.32215558256936,2.08798724773891,10.2862088087062));
#65951=CARTESIAN_POINT('Ctrl Pts',(0.322356978497306,2.09619387131056,10.2866961407268));
#65952=CARTESIAN_POINT('Ctrl Pts',(0.322229719012095,2.1055166859955,10.2872611755887));
#65953=CARTESIAN_POINT('Ctrl Pts',(0.322208641537457,2.10663452399926,10.2873291097527));
#65954=CARTESIAN_POINT('Ctrl Pts',(0.322160317794637,2.10864285582931,10.287451502947));
#65955=CARTESIAN_POINT('Ctrl Pts',(0.322135194773617,2.10953339297213,10.287505895282));
#65956=CARTESIAN_POINT('Ctrl Pts',(0.322091101520321,2.11089591987457,10.2875893042163));
#65957=CARTESIAN_POINT('Ctrl Pts',(0.322074785431026,2.11136799605421,10.2876182376057));
#65958=CARTESIAN_POINT('Ctrl Pts',(0.32204305676644,2.11223103862364,10.287671197105));
#65959=CARTESIAN_POINT('Ctrl Pts',(0.32202796991844,2.11262201668986,10.287695212959));
#65960=CARTESIAN_POINT('Ctrl Pts',(0.321996399459953,2.11340324310042,10.2877432481592));
#65961=CARTESIAN_POINT('Ctrl Pts',(0.321979918313899,2.1137934909015,10.2877672673893));
#65962=CARTESIAN_POINT('Ctrl Pts',(0.321931587402049,2.11489057735698,10.2878348598585));
#65963=CARTESIAN_POINT('Ctrl Pts',(0.321898119373994,2.11559733925875,10.2878784837748));
#65964=CARTESIAN_POINT('Ctrl Pts',(0.321751176765813,2.11849818232091,10.2880578657236));
#65965=CARTESIAN_POINT('Ctrl Pts',(0.32161759690553,2.12069114486311,10.2881942528057));
#65966=CARTESIAN_POINT('Ctrl Pts',(0.321317544338146,2.12490638643325,10.2884579600083));
#65967=CARTESIAN_POINT('Ctrl Pts',(0.321154373679745,2.12692880145859,10.2885851701079));
#65968=CARTESIAN_POINT('Ctrl Pts',(0.318270792049573,2.15889996398606,10.2906072660428));
#65969=CARTESIAN_POINT('Ctrl Pts',(0.311391022411776,2.18831958361098,10.2926433544757));
#65970=CARTESIAN_POINT('Ctrl Pts',(0.294416785485336,2.2321645713901,10.295817557353));
#65971=CARTESIAN_POINT('Ctrl Pts',(0.287055325469245,2.24747242954231,10.2969505211211));
#65972=CARTESIAN_POINT('Ctrl Pts',(0.278167041848874,2.26274142260704,10.2980589376631));
#65973=CARTESIAN_POINT('Ctrl Pts',(0.277809949407753,2.26335025508241,10.2981030946836));
#65974=CARTESIAN_POINT('Ctrl Pts',(0.277295758445557,2.26422037301077,10.2981661395487));
#65975=CARTESIAN_POINT('Ctrl Pts',(0.277140288112532,2.26448261084514,10.2981851319739));
#65976=CARTESIAN_POINT('Ctrl Pts',(0.276870611608382,2.26493601680645,10.2982179549739));
#65977=CARTESIAN_POINT('Ctrl Pts',(0.276756579164224,2.26512728757804,10.2982317969315));
#65978=CARTESIAN_POINT('Ctrl Pts',(0.27653629923257,2.26549590197447,10.2982584640149));
#65979=CARTESIAN_POINT('Ctrl Pts',(0.27643007958993,2.26567326115612,10.2982712909328));
#65980=CARTESIAN_POINT('Ctrl Pts',(0.276177199620714,2.26609458468611,10.2983017526148));
#65981=CARTESIAN_POINT('Ctrl Pts',(0.276030386288819,2.26633845766714,10.2983193773212));
#65982=CARTESIAN_POINT('Ctrl Pts',(0.275588863886564,2.26706968033769,10.2983722018605));
#65983=CARTESIAN_POINT('Ctrl Pts',(0.275293183875609,2.26755644693569,10.2984073385962));
#65984=CARTESIAN_POINT('Ctrl Pts',(0.272389903116128,2.27230757559489,10.2987500460582));
#65985=CARTESIAN_POINT('Ctrl Pts',(0.269684541971895,2.27651179699531,10.299051350106));
#65986=CARTESIAN_POINT('Ctrl Pts',(0.266574439471851,2.28110644785504,10.2993804241255));
#65987=CARTESIAN_POINT('Ctrl Pts',(0.266265426526621,2.28156045791568,10.2994129384818));
#65988=CARTESIAN_POINT('Ctrl Pts',(0.265374717851849,2.28286194609129,10.299506145785));
#65989=CARTESIAN_POINT('Ctrl Pts',(0.264790121657977,2.28370744057338,10.2995666966828));
#65990=CARTESIAN_POINT('Ctrl Pts',(0.263806564645909,2.28511549820027,10.2996675618232));
#65991=CARTESIAN_POINT('Ctrl Pts',(0.263409828921515,2.28567959840798,10.2997079776702));
#65992=CARTESIAN_POINT('Ctrl Pts',(0.260709261774106,2.28949333542838,10.299981297453));
#65993=CARTESIAN_POINT('Ctrl Pts',(0.258347086209562,2.2927013973038,10.3002116002105));
#65994=CARTESIAN_POINT('Ctrl Pts',(0.242452856737662,2.31346951408991,10.3017108681893));
#65995=CARTESIAN_POINT('Ctrl Pts',(0.22719890564693,2.32963747778471,10.302922037766));
#65996=CARTESIAN_POINT('Ctrl Pts',(0.204405324288364,2.34928374436306,10.3046290045851));
#65997=CARTESIAN_POINT('Ctrl Pts',(0.198216914756707,2.35423210914159,10.3050831683033));
#65998=CARTESIAN_POINT('Ctrl Pts',(0.185041992381582,2.36399334526722,10.3060394604555));
#65999=CARTESIAN_POINT('Ctrl Pts',(0.178035295499419,2.36876837572816,10.3065423531545));
#66000=CARTESIAN_POINT('Ctrl Pts',(0.16988337951624,2.37386513074081,10.3071248670226));
#66001=CARTESIAN_POINT('Ctrl Pts',(0.168914598959794,2.37446371468405,10.3071940511584));
#66002=CARTESIAN_POINT('Ctrl Pts',(0.167169924400801,2.37552896719064,10.3073185792449));
#66003=CARTESIAN_POINT('Ctrl Pts',(0.166395194463173,2.37599752647189,10.3073738534692));
#66004=CARTESIAN_POINT('Ctrl Pts',(0.16521104767199,2.37670690442477,10.307458307176));
#66005=CARTESIAN_POINT('Ctrl Pts',(0.164803051474384,2.37695009559504,10.3074874000111));
#66006=CARTESIAN_POINT('Ctrl Pts',(0.164089914202477,2.37737303600528,10.3075382423271));
#66007=CARTESIAN_POINT('Ctrl Pts',(0.163785010927808,2.37755318632567,10.3075599771664));
#66008=CARTESIAN_POINT('Ctrl Pts',(0.163152176645483,2.37792568686343,10.3076050826588));
#66009=CARTESIAN_POINT('Ctrl Pts',(0.162824201111661,2.37811796003331,10.3076284560666));
#66010=CARTESIAN_POINT('Ctrl Pts',(0.162026556817637,2.3785836784028,10.307685293474));
#66011=CARTESIAN_POINT('Ctrl Pts',(0.161556536328935,2.378856516062,10.3077187794156));
#66012=CARTESIAN_POINT('Ctrl Pts',(0.159790137367185,2.3798759110276,10.3078446028563));
#66013=CARTESIAN_POINT('Ctrl Pts',(0.15848927163179,2.38061461870304,10.3079372231037));
#66014=CARTESIAN_POINT('Ctrl Pts',(0.135182726994371,2.39363567905473,10.3095960238398));
#66015=CARTESIAN_POINT('Ctrl Pts',(0.111821227939386,2.40330145987106,10.3112598357882));
#66016=CARTESIAN_POINT('Ctrl Pts',(0.0723803038835808,2.41443864390435,
10.314027925672));
#66017=CARTESIAN_POINT('Ctrl Pts',(0.0568871147793168,2.4176073937109,10.3151029889319));
#66018=CARTESIAN_POINT('Ctrl Pts',(0.0349587514689426,2.42043558379176,
10.316565528261));
#66019=CARTESIAN_POINT('Ctrl Pts',(0.0286709789840776,2.42105928394083,
10.3169780432867));
#66020=CARTESIAN_POINT('Ctrl Pts',(0.0194180102140337,2.42170306834132,
10.3175713311735));
#66021=CARTESIAN_POINT('Ctrl Pts',(0.0164646793796068,2.42186773550386,
10.3177586412581));
#66022=CARTESIAN_POINT('Ctrl Pts',(0.0130061121029357,2.42201284196738,
10.3179752682868));
#66023=CARTESIAN_POINT('Ctrl Pts',(0.0125027967532464,2.42203277694278,
10.3180067258508));
#66024=CARTESIAN_POINT('Ctrl Pts',(0.011733989911379,2.42206142219062,10.3180546715302));
#66025=CARTESIAN_POINT('Ctrl Pts',(0.0114685338580242,2.42207098427995,
10.3180712071972));
#66026=CARTESIAN_POINT('Ctrl Pts',(0.010987316294063,2.42208772269296,10.318101147863));
#66027=CARTESIAN_POINT('Ctrl Pts',(0.0107715602575569,2.42209501039176,
10.3181145590702));
#66028=CARTESIAN_POINT('Ctrl Pts',(0.0103337797621303,2.42210935715143,
10.3181417450994));
#66029=CARTESIAN_POINT('Ctrl Pts',(0.010111756290258,2.42211640342295,10.3181555191432));
#66030=CARTESIAN_POINT('Ctrl Pts',(0.00947249210757115,2.42213602990904,
10.3181951397135));
#66031=CARTESIAN_POINT('Ctrl Pts',(0.00905523204150777,2.42214802909473,
10.3182209535599));
#66032=CARTESIAN_POINT('Ctrl Pts',(0.00722050985474629,2.42219722288538,
10.3183342556767));
#66033=CARTESIAN_POINT('Ctrl Pts',(0.00580280664003967,2.42222587389353,
10.3184212718284));
#66034=CARTESIAN_POINT('Ctrl Pts',(-0.0204808567483181,2.42258352712238,
10.3200253944839));
#66035=CARTESIAN_POINT('Ctrl Pts',(-0.0453068091482655,2.42004269421073,
10.3213932681915));
#66036=CARTESIAN_POINT('Ctrl Pts',(-0.0835976613275468,2.41157378620364,
10.3235874985344));
#66037=CARTESIAN_POINT('Ctrl Pts',(-0.0973756250825092,2.40754631841912,
10.3243944364557));
#66038=CARTESIAN_POINT('Ctrl Pts',(-0.118841462392824,2.39968402662316,
10.3257218652746));
#66039=CARTESIAN_POINT('Ctrl Pts',(-0.126724072873708,2.39643683906635,
10.3262250370146));
#66040=CARTESIAN_POINT('Ctrl Pts',(-0.135980944302133,2.39218680479038,
10.3268391887076));
#66041=CARTESIAN_POINT('Ctrl Pts',(-0.137488183678816,2.39148060878248,
10.3269399379096));
#66042=CARTESIAN_POINT('Ctrl Pts',(-0.14010928043266,2.39022767715955,10.3271164891046));
#66043=CARTESIAN_POINT('Ctrl Pts',(-0.141225585360997,2.38968612156072,
10.3271921115397));
#66044=CARTESIAN_POINT('Ctrl Pts',(-0.142825784352268,2.3888983656394,10.3273011454233));
#66045=CARTESIAN_POINT('Ctrl Pts',(-0.143312236546422,2.38865736296745,
10.3273343753931));
#66046=CARTESIAN_POINT('Ctrl Pts',(-0.144155450027245,2.38823695342095,
10.3273921233431));
#66047=CARTESIAN_POINT('Ctrl Pts',(-0.144512492158249,2.38805810993242,
10.3274166215567));
#66048=CARTESIAN_POINT('Ctrl Pts',(-0.145198421853844,2.38771292941303,
10.3274637750717));
#66049=CARTESIAN_POINT('Ctrl Pts',(-0.145527358498768,2.38754669079455,
10.327486426891));
#66050=CARTESIAN_POINT('Ctrl Pts',(-0.146301701700489,2.3871536827492,10.3275398443999));
#66051=CARTESIAN_POINT('Ctrl Pts',(-0.146746866352384,2.38692644117988,
10.3275706266635));
#66052=CARTESIAN_POINT('Ctrl Pts',(-0.148060545011294,2.3862519955314,10.3276616816947));
#66053=CARTESIAN_POINT('Ctrl Pts',(-0.148927550505155,2.38580187998264,
10.3277220570389));
#66054=CARTESIAN_POINT('Ctrl Pts',(-0.156622937781367,2.38176220953369,
10.3282604625113));
#66055=CARTESIAN_POINT('Ctrl Pts',(-0.163321915227626,2.37793276676771,
10.3287469856543));
#66056=CARTESIAN_POINT('Ctrl Pts',(-0.18264423861435,2.36594734366647,10.3302056700982));
#66057=CARTESIAN_POINT('Ctrl Pts',(-0.194840867457226,2.35714557268727,
10.3312002394182));
#66058=CARTESIAN_POINT('Ctrl Pts',(-0.214612880909925,2.34066042891563,
10.3329315992068));
#66059=CARTESIAN_POINT('Ctrl Pts',(-0.222499947271515,2.33338787014627,
10.3336592954323));
#66060=CARTESIAN_POINT('Ctrl Pts',(-0.241942571303382,2.31357714498271,
10.3355336234373));
#66061=CARTESIAN_POINT('Ctrl Pts',(-0.25289427796135,2.30048952352188,10.3366724815783));
#66062=CARTESIAN_POINT('Ctrl Pts',(-0.263197843587707,2.28598021525638,
10.3377895501186));
#66063=CARTESIAN_POINT('Ctrl Pts',(-0.263632706327043,2.28536326906358,
10.3378367887308));
#66064=CARTESIAN_POINT('Ctrl Pts',(-0.264245010490872,2.28448807067453,
10.337903427729));
#66065=CARTESIAN_POINT('Ctrl Pts',(-0.264424244695574,2.28423108480846,
10.3379229496669));
#66066=CARTESIAN_POINT('Ctrl Pts',(-0.264731105215501,2.2837897381052,10.3379563982328));
#66067=CARTESIAN_POINT('Ctrl Pts',(-0.264858914170717,2.28360550505589,
10.3379703374296));
#66068=CARTESIAN_POINT('Ctrl Pts',(-0.265103093514358,2.28325274180215,
10.3379969828344));
#66069=CARTESIAN_POINT('Ctrl Pts',(-0.26521949537384,2.28308423428333,10.3380096912342));
#66070=CARTESIAN_POINT('Ctrl Pts',(-0.265493044182715,2.28268742685574,
10.3380395717475));
#66071=CARTESIAN_POINT('Ctrl Pts',(-0.265650057713977,2.28245903452138,
10.3380567346961));
#66072=CARTESIAN_POINT('Ctrl Pts',(-0.266112174803341,2.28178497669168,
10.3381072842279));
#66073=CARTESIAN_POINT('Ctrl Pts',(-0.2664164548113,2.28133874364045,10.3381406150405));
#66074=CARTESIAN_POINT('Ctrl Pts',(-0.26904252835157,2.27746667459992,10.33842869963));
#66075=CARTESIAN_POINT('Ctrl Pts',(-0.27129938664848,2.27399698097526,10.338679170051));
#66076=CARTESIAN_POINT('Ctrl Pts',(-0.281104644147349,2.25826752817198,
10.3397852614992));
#66077=CARTESIAN_POINT('Ctrl Pts',(-0.28789405549644,2.24555251049751,10.3406013622875));
#66078=CARTESIAN_POINT('Ctrl Pts',(-0.306530683079391,2.20420343675961,
10.3431464018821));
#66079=CARTESIAN_POINT('Ctrl Pts',(-0.315116785478717,2.17430091953921,
10.3448499312024));
#66080=CARTESIAN_POINT('Ctrl Pts',(-0.319580938659845,2.14163265865075,
10.3468437847235));
#66081=CARTESIAN_POINT('Ctrl Pts',(-0.319835563553847,2.13962911327923,
10.3469664948881));
#66082=CARTESIAN_POINT('Ctrl Pts',(-0.320148235054558,2.13696913730879,
10.3471300167791));
#66083=CARTESIAN_POINT('Ctrl Pts',(-0.320223128285117,2.1363147025741,10.3471702967699));
#66084=CARTESIAN_POINT('Ctrl Pts',(-0.320342831839338,2.13523953372498,
10.3472365541192));
#66085=CARTESIAN_POINT('Ctrl Pts',(-0.320388821146545,2.13481893062148,
10.3472624942729));
#66086=CARTESIAN_POINT('Ctrl Pts',(-0.320476358109924,2.13400348721692,
10.3473128258209));
#66087=CARTESIAN_POINT('Ctrl Pts',(-0.320518004716193,2.13360865812287,
10.3473372140497));
#66088=CARTESIAN_POINT('Ctrl Pts',(-0.320612516783115,2.13269648523803,
10.3473936006653));
#66089=CARTESIAN_POINT('Ctrl Pts',(-0.320664859722767,2.13217908946577,
10.3474256154448));
#66090=CARTESIAN_POINT('Ctrl Pts',(-0.320828646004199,2.1305200160197,10.3475283761459));
#66091=CARTESIAN_POINT('Ctrl Pts',(-0.320935245268407,2.1293778788327,10.3475992742476));
#66092=CARTESIAN_POINT('Ctrl Pts',(-0.32186721319046,2.11878135662402,10.3482585339651));
#66093=CARTESIAN_POINT('Ctrl Pts',(-0.322280608452412,2.10929629717948,
10.3488597856719));
#66094=CARTESIAN_POINT('Ctrl Pts',(-0.322270166261914,2.09180868584661,
10.3499903677247));
#66095=CARTESIAN_POINT('Ctrl Pts',(-0.321967595462726,2.08381328509359,
10.3505157288825));
#66096=CARTESIAN_POINT('Ctrl Pts',(-0.318973647345409,2.04399231676612,
10.3531699568388));
#66097=CARTESIAN_POINT('Ctrl Pts',(-0.311859686864174,2.01268146281999,
10.3553986265746));
#66098=CARTESIAN_POINT('Ctrl Pts',(-0.299701487269705,1.98149873776168,
10.3575161254572));
#66099=CARTESIAN_POINT('Ctrl Pts',(-0.29913380087351,1.98007293874681,10.3576126631307));
#66100=CARTESIAN_POINT('Ctrl Pts',(-0.298395816820164,1.97825726730662,
10.357735185896));
#66101=CARTESIAN_POINT('Ctrl Pts',(-0.29823491475411,1.97786363323736,10.3577617237329));
#66102=CARTESIAN_POINT('Ctrl Pts',(-0.297977808701813,1.97723818126699,
10.3578038492537));
#66103=CARTESIAN_POINT('Ctrl Pts',(-0.297882112935714,1.9770061570185,10.3578194676126));
#66104=CARTESIAN_POINT('Ctrl Pts',(-0.297702659138811,1.97657249074447,
10.3578486420955));
#66105=CARTESIAN_POINT('Ctrl Pts',(-0.297618967871208,1.97637082357697,
10.3578622020975));
#66106=CARTESIAN_POINT('Ctrl Pts',(-0.297430242059429,1.9759173615482,10.3578926771343));
#66107=CARTESIAN_POINT('Ctrl Pts',(-0.297325092936461,1.97566561550265,
10.3579095850496));
#66108=CARTESIAN_POINT('Ctrl Pts',(-0.297011599905573,1.97491772824144,
10.3579597840054));
#66109=CARTESIAN_POINT('Ctrl Pts',(-0.296802331604503,1.97442197186298,
10.3579930189716));
#66110=CARTESIAN_POINT('Ctrl Pts',(-0.295086771549548,1.97038605598993,
10.3582632685398));
#66111=CARTESIAN_POINT('Ctrl Pts',(-0.293518358746154,1.96687241643497,
10.3584965757081));
#66112=CARTESIAN_POINT('Ctrl Pts',(-0.288118582297884,1.95533521092282,
10.359258787464));
#66113=CARTESIAN_POINT('Ctrl Pts',(-0.284017927955936,1.94744161309117,
10.3597740438604));
#66114=CARTESIAN_POINT('Ctrl Pts',(-0.267022939846461,1.91779388855637,
10.3617225464507));
#66115=CARTESIAN_POINT('Ctrl Pts',(-0.251913169269096,1.8974163128423,10.3630973811836));
#66116=CARTESIAN_POINT('Ctrl Pts',(-0.230792491949408,1.87499676659573,
10.3648696769891));
#66117=CARTESIAN_POINT('Ctrl Pts',(-0.226906024345914,1.87107800239181,
10.3651903363216));
#66118=CARTESIAN_POINT('Ctrl Pts',(-0.222333881607314,1.86669873196306,
10.3655627832236));
#66119=CARTESIAN_POINT('Ctrl Pts',(-0.221744638254826,1.8661386052228,10.3656106942259));
#66120=CARTESIAN_POINT('Ctrl Pts',(-0.216380868404734,1.86107837591119,
10.3660460453336));
#66121=CARTESIAN_POINT('Ctrl Pts',(-0.211472359255203,1.85672309064134,
10.3664389571224));
#66122=CARTESIAN_POINT('Ctrl Pts',(-0.205639159019191,1.85185732953281,
10.3669012678651));
#66123=CARTESIAN_POINT('Ctrl Pts',(-0.204840522495499,1.8511976508688,10.3669644657762));
#66124=CARTESIAN_POINT('Ctrl Pts',(-0.203648428635293,1.8502226043387,10.3670586595194));
#66125=CARTESIAN_POINT('Ctrl Pts',(-0.203257383641885,1.8499042866032,10.3670895359617));
#66126=CARTESIAN_POINT('Ctrl Pts',(-0.202559876788322,1.8493392197724,10.3671445717128));
#66127=CARTESIAN_POINT('Ctrl Pts',(-0.202253706391801,1.84909211116944,
10.3671687164767));
#66128=CARTESIAN_POINT('Ctrl Pts',(-0.20160853659243,1.84857334605037,10.3672195676775));
#66129=CARTESIAN_POINT('Ctrl Pts',(-0.201269439127227,1.84830181324905,
10.3672462790114));
#66130=CARTESIAN_POINT('Ctrl Pts',(-0.200375118144687,1.84758864730866,
10.3673166855608));
#66131=CARTESIAN_POINT('Ctrl Pts',(-0.199818985819162,1.84714816229201,
10.3673604265592));
#66132=CARTESIAN_POINT('Ctrl Pts',(-0.197321776417721,1.84518362947927,
10.3675566579049));
#66133=CARTESIAN_POINT('Ctrl Pts',(-0.19536472741941,1.84368010442129,10.3677099604148));
#66134=CARTESIAN_POINT('Ctrl Pts',(-0.180888730686399,1.83282085663207,
10.3688406686116));
#66135=CARTESIAN_POINT('Ctrl Pts',(-0.167723113800082,1.82436572137034,
10.3698529667051));
#66136=CARTESIAN_POINT('Ctrl Pts',(-0.12580003502154,1.80156084868131,10.3730238363504));
#66137=CARTESIAN_POINT('Ctrl Pts',(-0.0954707291611789,1.7905216495933,
10.3752647326888));
#66138=CARTESIAN_POINT('Ctrl Pts',(-0.0625320003943831,1.7838462348125,
10.3773905632051));
#66139=CARTESIAN_POINT('Ctrl Pts',(-0.0610504204559197,1.78355679705627,
10.3774855106009));
#66140=CARTESIAN_POINT('Ctrl Pts',(-0.0591515178741482,1.78319966518136,
10.3776062952398));
#66141=CARTESIAN_POINT('Ctrl Pts',(-0.058736052186312,1.78312237316838,
10.3776326665586));
#66142=CARTESIAN_POINT('Ctrl Pts',(-0.0580742042754473,1.78300059131918,
10.3776745871755));
#66143=CARTESIAN_POINT('Ctrl Pts',(-0.05782792197665,1.78295557133565,10.3776901666471));
#66144=CARTESIAN_POINT('Ctrl Pts',(-0.0573687337082872,1.78287218536047,
10.3777191771398));
#66145=CARTESIAN_POINT('Ctrl Pts',(-0.0571558431921249,1.78283374704308,
10.3777326121902));
#66146=CARTESIAN_POINT('Ctrl Pts',(-0.0566745345987861,1.78274734500622,
10.3777629529841));
#66147=CARTESIAN_POINT('Ctrl Pts',(-0.0564060948498825,1.78269950766238,
10.3777798514007));
#66148=CARTESIAN_POINT('Ctrl Pts',(-0.0556084473500054,1.7825584070011,
10.3778299947104));
#66149=CARTESIAN_POINT('Ctrl Pts',(-0.0550790633735103,1.78246612594857,
10.3778631837158));
#66150=CARTESIAN_POINT('Ctrl Pts',(-0.0507801159260038,1.78172781716147,
10.3781319867265));
#66151=CARTESIAN_POINT('Ctrl Pts',(-0.046999356795059,1.78114757935618,
10.3783639376251));
#66152=CARTESIAN_POINT('Ctrl Pts',(-0.0346098940189089,1.77947132978813,
10.3791121556485));
#66153=CARTESIAN_POINT('Ctrl Pts',(-0.0259666172483175,1.77865558582802,
10.379615516642));
#66154=CARTESIAN_POINT('Ctrl Pts',(0.0112969168478374,1.77665232392053,
10.3817452230985));
#66155=CARTESIAN_POINT('Ctrl Pts',(0.039970835702141,1.7789333776358,10.383294139838));
#66156=CARTESIAN_POINT('Ctrl Pts',(0.0773610490664642,1.78700031958462,
10.3855215895428));
#66157=CARTESIAN_POINT('Ctrl Pts',(0.086658937365287,1.78944608733933,10.3860920692034));
#66158=CARTESIAN_POINT('Ctrl Pts',(0.096917573850852,1.79264117094517,10.386745452651));
#66159=CARTESIAN_POINT('Ctrl Pts',(0.0980002965777421,1.79298467833339,
10.3868147128344));
#66160=CARTESIAN_POINT('Ctrl Pts',(0.0995368021366322,1.79348111001578,
10.3869134361264));
#66161=CARTESIAN_POINT('Ctrl Pts',(0.0999921037531905,1.79362933547767,
10.3869427445868));
#66162=CARTESIAN_POINT('Ctrl Pts',(0.100826915903225,1.79390317142987,10.3869965834661));
#66163=CARTESIAN_POINT('Ctrl Pts',(0.101206526870368,1.79402847461275,10.3870211037148));
#66164=CARTESIAN_POINT('Ctrl Pts',(0.101975550583113,1.79428390411406,10.3870708554381));
#66165=CARTESIAN_POINT('Ctrl Pts',(0.102364949679723,1.79441406891832,10.3870960881458));
#66166=CARTESIAN_POINT('Ctrl Pts',(0.103323438938877,1.79473650165447,10.3871582981351));
#66167=CARTESIAN_POINT('Ctrl Pts',(0.103892240639572,1.79492961667281,10.387195303381));
#66168=CARTESIAN_POINT('Ctrl Pts',(0.105968210452394,1.79564091262227,10.3873306850688));
#66169=CARTESIAN_POINT('Ctrl Pts',(0.107472049770653,1.79616867497327,10.3874293786102));
#66170=CARTESIAN_POINT('Ctrl Pts',(0.116150065628597,1.79928665512679,10.3880025688954));
#66171=CARTESIAN_POINT('Ctrl Pts',(0.123233874051823,1.80211957113634,10.3884851218318));
#66172=CARTESIAN_POINT('Ctrl Pts',(0.136852446194015,1.80813477037234,10.3894427799752));
#66173=CARTESIAN_POINT('Ctrl Pts',(0.143393343232581,1.81129211774023,10.3899168529905));
#66174=CARTESIAN_POINT('Ctrl Pts',(0.167065995390002,1.82372209393221,10.3916835908986));
#66175=CARTESIAN_POINT('Ctrl Pts',(0.183453123415775,1.83432091460619,10.3930109872827));
#66176=CARTESIAN_POINT('Ctrl Pts',(0.210712546858192,1.85568226252787,10.3953441616867));
#66177=CARTESIAN_POINT('Ctrl Pts',(0.221970678282373,1.86586312692097,10.3963521235913));
#66178=CARTESIAN_POINT('Ctrl Pts',(0.233109304943099,1.8774644390391,10.3973636821887));
#66179=CARTESIAN_POINT('Ctrl Pts',(0.233744354697579,1.87813156907901,10.3974214049744));
#66180=CARTESIAN_POINT('Ctrl Pts',(0.234593198227199,1.87903098269818,10.3974986172242));
#66181=CARTESIAN_POINT('Ctrl Pts',(0.234809515413488,1.87926086270181,10.3975182987843));
#66182=CARTESIAN_POINT('Ctrl Pts',(0.235172740797678,1.87964799996004,10.3975513545586));
#66183=CARTESIAN_POINT('Ctrl Pts',(0.235319829251599,1.87980508657664,10.3975647426871));
#66184=CARTESIAN_POINT('Ctrl Pts',(0.235613315132623,1.88011915174055,10.3975914601518));
#66185=CARTESIAN_POINT('Ctrl Pts',(0.235759711938809,1.88027612800174,10.3976047893837));
#66186=CARTESIAN_POINT('Ctrl Pts',(0.236091131045357,1.88063220988054,10.3976349693831));
#66187=CARTESIAN_POINT('Ctrl Pts',(0.236276058013356,1.88083140299955,10.3976518127614));
#66188=CARTESIAN_POINT('Ctrl Pts',(0.236662503945287,1.88124871877441,10.3976870184341));
#66189=CARTESIAN_POINT('Ctrl Pts',(0.236863974012249,1.88146688665493,10.3977053769873));
#66190=CARTESIAN_POINT('Ctrl Pts',(0.237391211102245,1.8820394067626,10.397753432931));
#66191=CARTESIAN_POINT('Ctrl Pts',(0.237716487809621,1.88239421252312,10.3977830934207));
#66192=CARTESIAN_POINT('Ctrl Pts',(0.238682143848504,1.88345228126765,10.3978711894635));
#66193=CARTESIAN_POINT('Ctrl Pts',(0.239320212813764,1.88415765922584,10.3979294556308));
#66194=CARTESIAN_POINT('Ctrl Pts',(0.246510880413049,1.89217794740038,10.3985868551063));
#66195=CARTESIAN_POINT('Ctrl Pts',(0.252729669881703,1.89978667654771,10.3991627665697));
#66196=CARTESIAN_POINT('Ctrl Pts',(0.276855734981084,1.93222440850118,10.4014841485089));
#66197=CARTESIAN_POINT('Ctrl Pts',(0.291529037378584,1.95925639656827,10.4031295816653));
#66198=CARTESIAN_POINT('Ctrl Pts',(0.305353509151775,1.99653867211054,10.405449618392));
#66199=CARTESIAN_POINT('Ctrl Pts',(0.308169308093801,2.00525473494782,10.4059938592449));
#66200=CARTESIAN_POINT('Ctrl Pts',(0.31091311697873,2.01517370029135,10.4066197466409));
#66201=CARTESIAN_POINT('Ctrl Pts',(0.311210339524429,2.01627072224747,10.4066890545838));
#66202=CARTESIAN_POINT('Ctrl Pts',(0.311634585424211,2.01787004686112,10.406790229551));
#66203=CARTESIAN_POINT('Ctrl Pts',(0.311766212643437,2.01837112836667,10.4068219473626));
#66204=CARTESIAN_POINT('Ctrl Pts',(0.311996492487229,2.01925644502881,10.4068780208743));
#66205=CARTESIAN_POINT('Ctrl Pts',(0.312095645243799,2.01964054995619,10.4069023603386));
#66206=CARTESIAN_POINT('Ctrl Pts',(0.312299283119881,2.02043547850106,10.4069527561596));
#66207=CARTESIAN_POINT('Ctrl Pts',(0.312403667329038,2.02084632696341,10.4069788157244));
#66208=CARTESIAN_POINT('Ctrl Pts',(0.312669059344056,2.02189959296783,10.407045657224));
#66209=CARTESIAN_POINT('Ctrl Pts',(0.31282889742508,2.02254230073753,10.4070864768347));
#66210=CARTESIAN_POINT('Ctrl Pts',(0.313475068905385,2.02517517726691,10.4072538327746));
#66211=CARTESIAN_POINT('Ctrl Pts',(0.313944392191883,2.0271694348365,10.4073809157409));
#66212=CARTESIAN_POINT('Ctrl Pts',(0.316924870372072,2.04039857370554,10.408226190087));
#66213=CARTESIAN_POINT('Ctrl Pts',(0.318851226726684,2.05175536018906,10.408963017709));
#66214=CARTESIAN_POINT('Ctrl Pts',(0.323918924248395,2.09583290568706,10.4118671565514));
#66215=CARTESIAN_POINT('Ctrl Pts',(0.322657621397719,2.12885198904343,10.4141594439876));
#66216=CARTESIAN_POINT('Ctrl Pts',(0.3154722993399,2.16605938354124,10.4166179188866));
#66217=CARTESIAN_POINT('Ctrl Pts',(0.314399777879935,2.17098873523387,10.4169404385053));
#66218=CARTESIAN_POINT('Ctrl Pts',(0.313062595447996,2.17650744409736,10.41729638456));
#66219=CARTESIAN_POINT('Ctrl Pts',(0.312911460864029,2.17712324777334,10.4173360301406));
#66220=CARTESIAN_POINT('Ctrl Pts',(0.312688888666618,2.17801870179066,10.4173935699488));
#66221=CARTESIAN_POINT('Ctrl Pts',(0.312618892470348,2.17829870367279,10.4174115465898));
#66222=CARTESIAN_POINT('Ctrl Pts',(0.312494675248389,2.17879278097519,10.4174432392002));
#66223=CARTESIAN_POINT('Ctrl Pts',(0.312440610255716,2.1790068949942,10.4174569642303));
#66224=CARTESIAN_POINT('Ctrl Pts',(0.312328686608581,2.17944823550562,10.4174852354168));
#66225=CARTESIAN_POINT('Ctrl Pts',(0.312270800180339,2.17967545393137,10.4174997798989));
#66226=CARTESIAN_POINT('Ctrl Pts',(0.312120730378924,2.18026183894202,10.417537288182));
#66227=CARTESIAN_POINT('Ctrl Pts',(0.31202817468496,2.18062091123695,10.4175602303556));
#66228=CARTESIAN_POINT('Ctrl Pts',(0.311824977726453,2.18140362770902,10.4176101852892));
#66229=CARTESIAN_POINT('Ctrl Pts',(0.311714092212591,2.18182720855345,10.4176371840414));
#66230=CARTESIAN_POINT('Ctrl Pts',(0.311389253565988,2.18305784427461,10.4177155249283));
#66231=CARTESIAN_POINT('Ctrl Pts',(0.311173025036667,2.18386430263709,10.4177667392737));
#66232=CARTESIAN_POINT('Ctrl Pts',(0.30889618123039,2.19222610225664,10.4182965572304));
#66233=CARTESIAN_POINT('Ctrl Pts',(0.306563766631296,2.19970548765169,10.4187602954756));
#66234=CARTESIAN_POINT('Ctrl Pts',(0.298665152302906,2.22212401915989,10.4201398569616));
#66235=CARTESIAN_POINT('Ctrl Pts',(0.292261379047564,2.23674248361303,10.4210258221697));
#66236=CARTESIAN_POINT('Ctrl Pts',(0.277245670525367,2.26509599250208,10.4228195801948));
#66237=CARTESIAN_POINT('Ctrl Pts',(0.26862836638918,2.27877526057871,10.4237253341536));
#66238=CARTESIAN_POINT('Ctrl Pts',(0.25318096909016,2.2996421329099,10.4252358722444));
#66239=CARTESIAN_POINT('Ctrl Pts',(0.246981805578643,2.30726201430168,10.4258183828522));
#66240=CARTESIAN_POINT('Ctrl Pts',(0.239751532301661,2.31536355997245,10.4264786716171));
#66241=CARTESIAN_POINT('Ctrl Pts',(0.239054340033127,2.31613718485374,10.4265421541153));
#66242=CARTESIAN_POINT('Ctrl Pts',(0.238005997112949,2.3172891792323,10.4266373383659));
#66243=CARTESIAN_POINT('Ctrl Pts',(0.237657662538449,2.31767011164844,10.426668920926));
#66244=CARTESIAN_POINT('Ctrl Pts',(0.237056175502255,2.3183247220695,10.4267233805703));
#66245=CARTESIAN_POINT('Ctrl Pts',(0.236803459823008,2.31859880151647,10.4267462390423));
#66246=CARTESIAN_POINT('Ctrl Pts',(0.236280913422218,2.31916355280118,10.4267934573859));
#66247=CARTESIAN_POINT('Ctrl Pts',(0.236011020653077,2.3194541661764,10.4268178198894));
#66248=CARTESIAN_POINT('Ctrl Pts',(0.235381564498682,2.32012944367354,10.4268745803274));
#66249=CARTESIAN_POINT('Ctrl Pts',(0.235021594251671,2.32051372544135,10.4269069956926));
#66250=CARTESIAN_POINT('Ctrl Pts',(0.23387141535911,2.32173556919203,10.4270104293539));
#66251=CARTESIAN_POINT('Ctrl Pts',(0.23307766549747,2.32256977188756,10.4270816003023));
#66252=CARTESIAN_POINT('Ctrl Pts',(0.215871308497118,2.34046005370663,10.4286199904444));
#66253=CARTESIAN_POINT('Ctrl Pts',(0.197637211132556,2.355657101423,10.4301727128665));
#66254=CARTESIAN_POINT('Ctrl Pts',(0.158220874573533,2.38175310302006,10.4333572861666));
#66255=CARTESIAN_POINT('Ctrl Pts',(0.137160007867019,2.39258487758418,10.4349779958288));
#66256=CARTESIAN_POINT('Ctrl Pts',(0.111902726607968,2.40224278500013,10.4367141485652));
#66257=CARTESIAN_POINT('Ctrl Pts',(0.108682093079082,2.40341576472092,10.4369317644403));
#66258=CARTESIAN_POINT('Ctrl Pts',(0.104907386525659,2.40472272215475,10.437181952391));
#66259=CARTESIAN_POINT('Ctrl Pts',(0.104371074400361,2.40490683164731,10.4372173855491));
#66260=CARTESIAN_POINT('Ctrl Pts',(0.103570431817143,2.40517932261941,10.4372701101793));
#66261=CARTESIAN_POINT('Ctrl Pts',(0.103306471742261,2.40526877697991,10.4372874648222));
#66262=CARTESIAN_POINT('Ctrl Pts',(0.102835000865762,2.40542787386226,10.4373184125258));
#66263=CARTESIAN_POINT('Ctrl Pts',(0.102627535356699,2.40549764732767,10.4373320133643));
#66264=CARTESIAN_POINT('Ctrl Pts',(0.102190452345232,2.40564414878222,10.4373606306271));
#66265=CARTESIAN_POINT('Ctrl Pts',(0.101960820147184,2.40572082917454,10.4373756441786));
#66266=CARTESIAN_POINT('Ctrl Pts',(0.101346897423774,2.40592506591728,10.4374157268217));
#66267=CARTESIAN_POINT('Ctrl Pts',(0.100962450961458,2.40605215744057,10.437440768345));
#66268=CARTESIAN_POINT('Ctrl Pts',(0.100115069881432,2.40633051691694,10.4374958366018));
#66269=CARTESIAN_POINT('Ctrl Pts',(0.0996520287937277,2.40648146106491,
10.4375258444693));
#66270=CARTESIAN_POINT('Ctrl Pts',(0.0982690068269478,2.40692883890308,
10.4376152285617));
#66271=CARTESIAN_POINT('Ctrl Pts',(0.0973480228500361,2.40722218727596,
10.4376744294435));
#66272=CARTESIAN_POINT('Ctrl Pts',(0.0940811866091533,2.40824656245011,
10.4378833292304));
#66273=CARTESIAN_POINT('Ctrl Pts',(0.0917282437612715,2.4089549207262,10.4380317992542));
#66274=CARTESIAN_POINT('Ctrl Pts',(0.084505548079991,2.4110395378678,10.4384821330487));
#66275=CARTESIAN_POINT('Ctrl Pts',(0.0796111009683528,2.41232812863234,
10.4387798217001));
#66276=CARTESIAN_POINT('Ctrl Pts',(0.0641925383506842,2.41600142768055,
10.4397000778383));
#66277=CARTESIAN_POINT('Ctrl Pts',(0.0535773906457115,2.41797338797259,
10.4403085006574));
#66278=CARTESIAN_POINT('Ctrl Pts',(0.0191642312316019,2.42259357846918,
10.4422542619353));
#66279=CARTESIAN_POINT('Ctrl Pts',(-0.00483297969329889,2.42312602856722,
10.443576694952));
#66280=CARTESIAN_POINT('Ctrl Pts',(-0.030440004569496,2.42083913226407,
10.4450886510365));
#66281=CARTESIAN_POINT('Ctrl Pts',(-0.0322112026507477,2.42066615181653,
10.4451937127245));
#66282=CARTESIAN_POINT('Ctrl Pts',(-0.0396785979762269,2.41987437185192,
10.445638826916));
#66283=CARTESIAN_POINT('Ctrl Pts',(-0.0453589210570994,2.41911842144803,
10.4459827853222));
#66284=CARTESIAN_POINT('Ctrl Pts',(-0.0519855170223322,2.4180560424297,
10.4463913642048));
#66285=CARTESIAN_POINT('Ctrl Pts',(-0.0529544899626497,2.41789614981222,
10.4464512921979));
#66286=CARTESIAN_POINT('Ctrl Pts',(-0.0544158016741092,2.41764814858091,
10.4465419522384));
#66287=CARTESIAN_POINT('Ctrl Pts',(-0.054908697067118,2.41756331770318,
10.4465725801213));
#66288=CARTESIAN_POINT('Ctrl Pts',(-0.0557885055890453,2.41740978669611,
10.4466273377849));
#66289=CARTESIAN_POINT('Ctrl Pts',(-0.0561754951234036,2.41734152547657,
10.4466514535628));
#66290=CARTESIAN_POINT('Ctrl Pts',(-0.0569922359181447,2.41719591948637,
10.4467024141892));
#66291=CARTESIAN_POINT('Ctrl Pts',(-0.0574219564553425,2.41711840881224,
10.4467292642746));
#66292=CARTESIAN_POINT('Ctrl Pts',(-0.0585592784539783,2.41691087727973,
10.4468004275212));
#66293=CARTESIAN_POINT('Ctrl Pts',(-0.0592666013618192,2.41677936040857,
10.4468447882625));
#66294=CARTESIAN_POINT('Ctrl Pts',(-0.0624949398894309,2.41616790473061,
10.4470477332154));
#66295=CARTESIAN_POINT('Ctrl Pts',(-0.0650105511544492,2.41566024317196,
10.4472071994173));
#66296=CARTESIAN_POINT('Ctrl Pts',(-0.075929102684722,2.41332077871046,
10.4479052882282));
#66297=CARTESIAN_POINT('Ctrl Pts',(-0.0842622238161775,2.41118321637384,
10.4484536176869));
#66298=CARTESIAN_POINT('Ctrl Pts',(-0.108203743666885,2.40400969737504,
10.4500756115429));
#66299=CARTESIAN_POINT('Ctrl Pts',(-0.123524558398253,2.39811326873441,
10.4511738834494));
#66300=CARTESIAN_POINT('Ctrl Pts',(-0.144863899821745,2.38797218474657,
10.4527712166224));
#66301=CARTESIAN_POINT('Ctrl Pts',(-0.151292590798713,2.38464729286863,
10.4532615940045));
#66302=CARTESIAN_POINT('Ctrl Pts',(-0.166601572640246,2.37606429770608,
10.454445646444));
#66303=CARTESIAN_POINT('Ctrl Pts',(-0.175352472452942,2.37059031752537,
10.4551364626226));
#66304=CARTESIAN_POINT('Ctrl Pts',(-0.184092010063403,2.36452109963622,
10.4558310234848));
#66305=CARTESIAN_POINT('Ctrl Pts',(-0.184357501475641,2.36433613444458,
10.4558521273706));
#66306=CARTESIAN_POINT('Ctrl Pts',(-0.189391370235722,2.36081781602418,
10.4562523457996));
#66307=CARTESIAN_POINT('Ctrl Pts',(-0.194069280840105,2.35735607447334,
10.4566255851434));
#66308=CARTESIAN_POINT('Ctrl Pts',(-0.199169778810791,2.35336339216137,
10.4570317344039));
#66309=CARTESIAN_POINT('Ctrl Pts',(-0.199687081178477,2.35295588332282,
10.4570729172066));
#66310=CARTESIAN_POINT('Ctrl Pts',(-0.200412175015025,2.35238107474349,
10.4571306244766));
#66311=CARTESIAN_POINT('Ctrl Pts',(-0.200621008910719,2.35221510178386,
10.4571472426149));
#66312=CARTESIAN_POINT('Ctrl Pts',(-0.201003625326346,2.35191023742833,
10.4571776854075));
#66313=CARTESIAN_POINT('Ctrl Pts',(-0.201177470485556,2.35177142507748,
10.4571915157491));
#66314=CARTESIAN_POINT('Ctrl Pts',(-0.201510824402877,2.35150468202842,
10.4572180325739));
#66315=CARTESIAN_POINT('Ctrl Pts',(-0.201670355025856,2.35137677963179,
10.4572307210795));
#66316=CARTESIAN_POINT('Ctrl Pts',(-0.202078550105742,2.35104887382148,
10.4572631840884));
#66317=CARTESIAN_POINT('Ctrl Pts',(-0.202327040168917,2.35084865213602,
10.4572829428178));
#66318=CARTESIAN_POINT('Ctrl Pts',(-0.203188037817808,2.3501527887829,10.457351395591));
#66319=CARTESIAN_POINT('Ctrl Pts',(-0.203799031112506,2.34965526510846,
10.4573999551223));
#66320=CARTESIAN_POINT('Ctrl Pts',(-0.205270308511925,2.34844822305168,
10.4575168630094));
#66321=CARTESIAN_POINT('Ctrl Pts',(-0.206128753494383,2.34773646513873,
10.4575850552738));
#66322=CARTESIAN_POINT('Ctrl Pts',(-0.209273320324868,2.34510156601223,
10.4578348501145));
#66323=CARTESIAN_POINT('Ctrl Pts',(-0.211536441011745,2.34315105550405,
10.4580146257314));
#66324=CARTESIAN_POINT('Ctrl Pts',(-0.219839210484209,2.33579148931068,
10.4586755949131));
#66325=CARTESIAN_POINT('Ctrl Pts',(-0.225701593183277,2.33018626187017,
10.4591451741325));
#66326=CARTESIAN_POINT('Ctrl Pts',(-0.25075357951981,2.30435477352191,10.4611980795352));
#66327=CARTESIAN_POINT('Ctrl Pts',(-0.267482002121666,2.28191125638656,
10.4627076759838));
#66328=CARTESIAN_POINT('Ctrl Pts',(-0.28205751679078,2.25591168619819,10.464438727284));
#66329=CARTESIAN_POINT('Ctrl Pts',(-0.28298567018958,2.25422064368605,10.4645511841005));
#66330=CARTESIAN_POINT('Ctrl Pts',(-0.284778784891755,2.2508829957844,10.4647729768903));
#66331=CARTESIAN_POINT('Ctrl Pts',(-0.285644783813262,2.2492370330387,10.4648822760457));
#66332=CARTESIAN_POINT('Ctrl Pts',(-0.289545410307402,2.24166495139706,
10.465384918935));
#66333=CARTESIAN_POINT('Ctrl Pts',(-0.29241001677758,2.23565351250714,10.4657835195678));
#66334=CARTESIAN_POINT('Ctrl Pts',(-0.295504479684383,2.22860544448502,
10.4662519794118));
#66335=CARTESIAN_POINT('Ctrl Pts',(-0.295918075819724,2.22765089199882,
10.4663154472849));
#66336=CARTESIAN_POINT('Ctrl Pts',(-0.296525610459625,2.22622992158104,
10.4664099660043));
#66337=CARTESIAN_POINT('Ctrl Pts',(-0.296723088645769,2.22576501668084,
10.4664408962446));
#66338=CARTESIAN_POINT('Ctrl Pts',(-0.297072487496587,2.22493705490202,
10.4664959924483));
#66339=CARTESIAN_POINT('Ctrl Pts',(-0.297224837952698,2.22457417957511,
10.4665201437492));
#66340=CARTESIAN_POINT('Ctrl Pts',(-0.297543775112242,2.2238106046695,10.4665709725445));
#66341=CARTESIAN_POINT('Ctrl Pts',(-0.297710217843865,2.22340984614323,
10.4665976548638));
#66342=CARTESIAN_POINT('Ctrl Pts',(-0.298145839210858,2.22235495305218,
10.466667903162));
#66343=CARTESIAN_POINT('Ctrl Pts',(-0.29841367343731,2.22170026897278,10.4667115145513));
#66344=CARTESIAN_POINT('Ctrl Pts',(-0.29959871652637,2.21877616026796,10.4669063698174));
#66345=CARTESIAN_POINT('Ctrl Pts',(-0.300492188249824,2.21649725945899,
10.4670584119241));
#66346=CARTESIAN_POINT('Ctrl Pts',(-0.306821695442285,2.1997957133266,10.4681742695162));
#66347=CARTESIAN_POINT('Ctrl Pts',(-0.311242013049874,2.18501189589775,
10.4691719910449));
#66348=CARTESIAN_POINT('Ctrl Pts',(-0.319710188476083,2.14693893366483,
10.4717616584561));
#66349=CARTESIAN_POINT('Ctrl Pts',(-0.322287609168167,2.12341734939115,
10.4733837697346));
#66350=CARTESIAN_POINT('Ctrl Pts',(-0.322274953623987,2.09982710796216,
10.4749491144816));
#66351=CARTESIAN_POINT('',(-0.322274999420556,2.10001932564221,10.7244193016094));
#66352=CARTESIAN_POINT('Ctrl Pts',(-0.322274953371521,2.09982663799766,
10.4749491456664));
#66353=CARTESIAN_POINT('Ctrl Pts',(-0.322269664666157,2.08999508753374,
10.4756015237701));
#66354=CARTESIAN_POINT('Ctrl Pts',(-0.321814482242808,2.08016755982393,
10.4762419206767));
#66355=CARTESIAN_POINT('Ctrl Pts',(-0.320868210385068,2.0699171372135,10.4768874415527));
#66356=CARTESIAN_POINT('Ctrl Pts',(-0.320824960434261,2.0694593412374,10.4769162240009));
#66357=CARTESIAN_POINT('Ctrl Pts',(-0.320753030884765,2.06871499184235,
10.4769629439478));
#66358=CARTESIAN_POINT('Ctrl Pts',(-0.320724946944098,2.06842838353156,
10.4769809142826));
#66359=CARTESIAN_POINT('Ctrl Pts',(-0.320674946744877,2.06792506275924,
10.4770124387095));
#66360=CARTESIAN_POINT('Ctrl Pts',(-0.320653194935537,2.06770833471107,
10.477026002008));
#66361=CARTESIAN_POINT('Ctrl Pts',(-0.320610240716335,2.06728467572564,
10.4770524937478));
#66362=CARTESIAN_POINT('Ctrl Pts',(-0.320589057628016,2.0670777427154,10.4770654232931));
#66363=CARTESIAN_POINT('Ctrl Pts',(-0.320546460293919,2.06666555828951,
10.4770911569344));
#66364=CARTESIAN_POINT('Ctrl Pts',(-0.320525049291612,2.06646030727147,
10.4771039611912));
#66365=CARTESIAN_POINT('Ctrl Pts',(-0.320473783551785,2.06597339415416,
10.4771343129506));
#66366=CARTESIAN_POINT('Ctrl Pts',(-0.320443754554873,2.06569175000694,
10.4771518505655));
#66367=CARTESIAN_POINT('Ctrl Pts',(-0.320336934899071,2.06470225630211,
10.477213400517));
#66368=CARTESIAN_POINT('Ctrl Pts',(-0.320258169087202,2.06399461531421,
10.4772573021753));
#66369=CARTESIAN_POINT('Ctrl Pts',(-0.319176293521734,2.05455943060468,
10.477841176338));
#66370=CARTESIAN_POINT('Ctrl Pts',(-0.317818968337538,2.04587526089332,
10.4783617059311));
#66371=CARTESIAN_POINT('Ctrl Pts',(-0.315809565456272,2.03575166984567,
10.4789599322486));
#66372=CARTESIAN_POINT('Ctrl Pts',(-0.315500116371917,2.03424890687167,
10.4790485086148));
#66373=CARTESIAN_POINT('Ctrl Pts',(-0.310390827631978,2.01030382358679,
10.480457083047));
#66374=CARTESIAN_POINT('Ctrl Pts',(-0.303217832213464,1.98843417167246,
10.4817088251937));
#66375=CARTESIAN_POINT('Ctrl Pts',(-0.287422327018391,1.95340910052672,
10.4838882489798));
#66376=CARTESIAN_POINT('Ctrl Pts',(-0.280056399379121,1.93978512656579,
10.4847846032852));
#66377=CARTESIAN_POINT('Ctrl Pts',(-0.270422667165388,1.924675231332,10.4858655124247));
#66378=CARTESIAN_POINT('Ctrl Pts',(-0.269080314765277,1.92262193732711,
10.4860143316882));
#66379=CARTESIAN_POINT('Ctrl Pts',(-0.267320574075358,1.91999614603866,
10.4862072296032));
#66380=CARTESIAN_POINT('Ctrl Pts',(-0.26692453357615,1.91940938527299,10.4862505029552));
#66381=CARTESIAN_POINT('Ctrl Pts',(-0.26628253854229,1.9184649518342,10.4863204285422));
#66382=CARTESIAN_POINT('Ctrl Pts',(-0.266037787509282,1.91810646064433,
10.4863470351407));
#66383=CARTESIAN_POINT('Ctrl Pts',(-0.265569765885311,1.9174239064406,10.486397815858));
#66384=CARTESIAN_POINT('Ctrl Pts',(-0.26534662436447,1.91709975552781,10.4864219850389));
#66385=CARTESIAN_POINT('Ctrl Pts',(-0.264835853514157,1.91636067628332,
10.4864772134339));
#66386=CARTESIAN_POINT('Ctrl Pts',(-0.264547842273797,1.9159460142639,10.4865082871779));
#66387=CARTESIAN_POINT('Ctrl Pts',(-0.263664077137738,1.91467998000386,
10.4866034305609));
#66388=CARTESIAN_POINT('Ctrl Pts',(-0.263065183361337,1.91383081713983,
10.4866676202762));
#66389=CARTESIAN_POINT('Ctrl Pts',(-0.258613769537593,1.90758358993761,
10.4871426560152));
#66390=CARTESIAN_POINT('Ctrl Pts',(-0.254599797432523,1.90230303676831,
10.4875597221389));
#66391=CARTESIAN_POINT('Ctrl Pts',(-0.246932825620288,1.89283785243854,
10.4883372930651));
#66392=CARTESIAN_POINT('Ctrl Pts',(-0.243328985047084,1.88861652141776,
10.4886957894891));
#66393=CARTESIAN_POINT('Ctrl Pts',(-0.224499516469823,1.86768063502768,
10.4905340921578));
#66394=CARTESIAN_POINT('Ctrl Pts',(-0.207655182980231,1.85250974497609,
10.4920742201139));
#66395=CARTESIAN_POINT('Ctrl Pts',(-0.184401597531442,1.83562364735243,
10.4940114888477));
#66396=CARTESIAN_POINT('Ctrl Pts',(-0.179335906894013,1.83216153611763,
10.4944230000212));
#66397=CARTESIAN_POINT('Ctrl Pts',(-0.168464327424338,1.82517823468396,
10.4952802265356));
#66398=CARTESIAN_POINT('Ctrl Pts',(-0.162639472269889,1.82169145236355,
10.4957247331461));
#66399=CARTESIAN_POINT('Ctrl Pts',(-0.154840600597502,1.81735157296715,
10.4962967116169));
#66400=CARTESIAN_POINT('Ctrl Pts',(-0.152962391732179,1.81633073453648,
10.496432742654));
#66401=CARTESIAN_POINT('Ctrl Pts',(-0.150303320436226,1.81491957462676,
10.4966227739306));
#66402=CARTESIAN_POINT('Ctrl Pts',(-0.149530863688142,1.8145136467174,10.496677677098));
#66403=CARTESIAN_POINT('Ctrl Pts',(-0.148181292869036,1.81381142425413,
10.496773063602));
#66404=CARTESIAN_POINT('Ctrl Pts',(-0.147604919549748,1.81351372775322,
10.4968136317398));
#66405=CARTESIAN_POINT('Ctrl Pts',(-0.146766192832983,1.81308372895409,
10.496872415544));
#66406=CARTESIAN_POINT('Ctrl Pts',(-0.146504555871096,1.81295004431243,
10.4968907176244));
#66407=CARTESIAN_POINT('Ctrl Pts',(-0.146057926309308,1.81272260653101,
10.4969218997645));
#66408=CARTESIAN_POINT('Ctrl Pts',(-0.145873025719352,1.81262867400431,
10.4969347912038));
#66409=CARTESIAN_POINT('Ctrl Pts',(-0.14550481741615,1.81244206510033,10.4969604276663));
#66410=CARTESIAN_POINT('Ctrl Pts',(-0.145321511995711,1.81234938559609,
10.4969731728897));
#66411=CARTESIAN_POINT('Ctrl Pts',(-0.144888553296427,1.81213100049349,
10.4970032357463));
#66412=CARTESIAN_POINT('Ctrl Pts',(-0.144638824354234,1.81200544407228,
10.4970205439356));
#66413=CARTESIAN_POINT('Ctrl Pts',(-0.143771658359252,1.81157087075749,
10.4970805356722));
#66414=CARTESIAN_POINT('Ctrl Pts',(-0.143153386215205,1.81126351048257,
10.4971231157937));
#66415=CARTESIAN_POINT('Ctrl Pts',(-0.135662536049415,1.80756957578739,
10.4976367360521));
#66416=CARTESIAN_POINT('Ctrl Pts',(-0.128671631440922,1.80442681077598,
10.4980930063276));
#66417=CARTESIAN_POINT('Ctrl Pts',(-0.106573022092281,1.7954252840235,10.4994846545273));
#66418=CARTESIAN_POINT('Ctrl Pts',(-0.0911307722786908,1.79045382964229,
10.5003863743916));
#66419=CARTESIAN_POINT('Ctrl Pts',(-0.0735248795059124,1.78621838016865,
10.501398571833));
#66420=CARTESIAN_POINT('Ctrl Pts',(-0.0716667096891907,1.78578877239762,
10.5015051947685));
#66421=CARTESIAN_POINT('Ctrl Pts',(-0.0676339574842302,1.78489403666191,
10.5017363156833));
#66422=CARTESIAN_POINT('Ctrl Pts',(-0.0654581575823177,1.7844348722277,
10.5018608370571));
#66423=CARTESIAN_POINT('Ctrl Pts',(-0.0413701404003216,1.77961136561737,
10.5032387443593));
#66424=CARTESIAN_POINT('Ctrl Pts',(-0.0190694523605319,1.77751512097902,
10.5045143456594));
#66425=CARTESIAN_POINT('Ctrl Pts',(0.00451678436843235,1.77775422956733,
10.505947698763));
#66426=CARTESIAN_POINT('Ctrl Pts',(0.00576653294046906,1.77777417091147,
10.5060238771631));
#66427=CARTESIAN_POINT('Ctrl Pts',(0.00756050901915792,1.77781323610676,
10.5061335697268));
#66428=CARTESIAN_POINT('Ctrl Pts',(0.00810486417989138,1.77782647021286,
10.50616689934));
#66429=CARTESIAN_POINT('Ctrl Pts',(0.00904865474546904,1.7778518086859,
10.5062247645166));
#66430=CARTESIAN_POINT('Ctrl Pts',(0.00944810719990214,1.77786327656155,
10.5062492800873));
#66431=CARTESIAN_POINT('Ctrl Pts',(0.0102155435385683,1.77788673754187,
10.5062964274895));
#66432=CARTESIAN_POINT('Ctrl Pts',(0.0105835304636266,1.77789861834759,
10.5063190557647));
#66433=CARTESIAN_POINT('Ctrl Pts',(0.0114495260047386,1.77792806346895,
10.5063723574571));
#66434=CARTESIAN_POINT('Ctrl Pts',(0.0119475147749535,1.77794615227753,
10.5064030472718));
#66435=CARTESIAN_POINT('Ctrl Pts',(0.0134158190744853,1.77800289685818,
10.5064936507183));
#66436=CARTESIAN_POINT('Ctrl Pts',(0.0143859976958136,1.77804478312911,
10.5065536654983));
#66437=CARTESIAN_POINT('Ctrl Pts',(0.0229042000524346,1.77845112538205,
10.5070819258858));
#66438=CARTESIAN_POINT('Ctrl Pts',(0.0304368681016007,1.77907654702705,
10.5075583165908));
#66439=CARTESIAN_POINT('Ctrl Pts',(0.0409692202001078,1.78032516045509,
10.5082382436887));
#66440=CARTESIAN_POINT('Ctrl Pts',(0.0439929903616167,1.78072723905905,
10.5084350461257));
#66441=CARTESIAN_POINT('Ctrl Pts',(0.0750860518564352,1.78531184831656,
10.5104751526767));
#66442=CARTESIAN_POINT('Ctrl Pts',(0.102490002526301,1.79314187201147,10.5124272195866));
#66443=CARTESIAN_POINT('Ctrl Pts',(0.136250253933023,1.80782143212454,10.5148851567934));
#66444=CARTESIAN_POINT('Ctrl Pts',(0.143857689417009,1.81149101253808,10.5154415694871));
#66445=CARTESIAN_POINT('Ctrl Pts',(0.15333709739228,1.81653189453997,10.5161307112324));
#66446=CARTESIAN_POINT('Ctrl Pts',(0.155349929378248,1.81762997260444,10.5162767887091));
#66447=CARTESIAN_POINT('Ctrl Pts',(0.158152677303352,1.81919802302192,10.5164796567165));
#66448=CARTESIAN_POINT('Ctrl Pts',(0.15895250940828,1.81965000550513,10.5165374881731));
#66449=CARTESIAN_POINT('Ctrl Pts',(0.160158014229074,1.82033804983997,10.5166245452301));
#66450=CARTESIAN_POINT('Ctrl Pts',(0.160565113825703,1.82057158319565,10.5166539260257));
#66451=CARTESIAN_POINT('Ctrl Pts',(0.161311633573284,1.82100199559477,10.5167077671956));
#66452=CARTESIAN_POINT('Ctrl Pts',(0.161651206251521,1.82119860633508,10.516732244468));
#66453=CARTESIAN_POINT('Ctrl Pts',(0.162197430194848,1.82151620046571,10.5167715945562));
#66454=CARTESIAN_POINT('Ctrl Pts',(0.162404305844222,1.82163679408186,10.5167864925645));
#66455=CARTESIAN_POINT('Ctrl Pts',(0.162800479435068,1.82186832675622,10.5168150121731));
#66456=CARTESIAN_POINT('Ctrl Pts',(0.162989796923876,1.82197922763819,10.5168286360262));
#66457=CARTESIAN_POINT('Ctrl Pts',(0.163423320083916,1.82223377752504,10.5168598231647));
#66458=CARTESIAN_POINT('Ctrl Pts',(0.163667449323333,1.82237755507033,10.516877377923));
#66459=CARTESIAN_POINT('Ctrl Pts',(0.164419600876964,1.82282186436041,10.5169314409022));
#66460=CARTESIAN_POINT('Ctrl Pts',(0.164926991014534,1.82312347214489,10.5169678793259));
#66461=CARTESIAN_POINT('Ctrl Pts',(0.168797030039666,1.82543835138596,10.5172455881328));
#66462=CARTESIAN_POINT('Ctrl Pts',(0.172123710437412,1.82751152702084,10.517483037393));
#66463=CARTESIAN_POINT('Ctrl Pts',(0.176237549213364,1.8301806706476,10.5177761492502));
#66464=CARTESIAN_POINT('Ctrl Pts',(0.17706072897645,1.83072014084796,10.5178347743073));
#66465=CARTESIAN_POINT('Ctrl Pts',(0.201711597453075,1.84703697863535,10.5195899606402));
#66466=CARTESIAN_POINT('Ctrl Pts',(0.223340684507864,1.86591190641704,10.5211285623242));
#66467=CARTESIAN_POINT('Ctrl Pts',(0.252408971761341,1.89902627697551,10.5236278863721));
#66468=CARTESIAN_POINT('Ctrl Pts',(0.261767007933318,1.91137691964034,10.5245246670195));
#66469=CARTESIAN_POINT('Ctrl Pts',(0.271538418164638,1.92640828229311,10.52560608421));
#66470=CARTESIAN_POINT('Ctrl Pts',(0.27285226477248,1.92848079381511,10.5257549472457));
#66471=CARTESIAN_POINT('Ctrl Pts',(0.274514504462495,1.93117031152111,10.525947894047));
#66472=CARTESIAN_POINT('Ctrl Pts',(0.274884732165576,1.93177378063503,10.5259911720064));
#66473=CARTESIAN_POINT('Ctrl Pts',(0.275478745136297,1.93274921513507,10.5260611032453));
#66474=CARTESIAN_POINT('Ctrl Pts',(0.275703774055899,1.93312042357371,10.5260877108749));
#66475=CARTESIAN_POINT('Ctrl Pts',(0.276131372795722,1.93382901743504,10.5261384923742));
#66476=CARTESIAN_POINT('Ctrl Pts',(0.276334076130049,1.9341663217081,10.5261626613036));
#66477=CARTESIAN_POINT('Ctrl Pts',(0.276795408427319,1.93493718661414,10.5262178874658));
#66478=CARTESIAN_POINT('Ctrl Pts',(0.27705363699152,1.93537098459127,10.5262489592243));
#66479=CARTESIAN_POINT('Ctrl Pts',(0.277840176126017,1.93669938279737,10.5263440906324));
#66480=CARTESIAN_POINT('Ctrl Pts',(0.278365176968788,1.93759592597739,10.5264082703141));
#66481=CARTESIAN_POINT('Ctrl Pts',(0.282207533088732,1.94423088193846,10.5268830769975));
#66482=CARTESIAN_POINT('Ctrl Pts',(0.285351273774903,1.95006751548306,10.5272999173633));
#66483=CARTESIAN_POINT('Ctrl Pts',(0.289290629753467,1.95795459399824,10.527862693549));
#66484=CARTESIAN_POINT('Ctrl Pts',(0.290248603942787,1.95992247370025,10.5280030644539));
#66485=CARTESIAN_POINT('Ctrl Pts',(0.301821281773637,1.98432366824271,10.5297430823078));
#66486=CARTESIAN_POINT('Ctrl Pts',(0.309828958062536,2.00789811863785,10.5314280909666));
#66487=CARTESIAN_POINT('Ctrl Pts',(0.318347059231642,2.04745229743454,10.5341599592961));
#66488=CARTESIAN_POINT('Ctrl Pts',(0.32052344195725,2.06297361398135,10.5352066821043));
#66489=CARTESIAN_POINT('Ctrl Pts',(0.32164225185983,2.07977991494844,10.5362745133951));
#66490=CARTESIAN_POINT('Ctrl Pts',(0.321714680829075,2.08096702174728,10.5363495845125));
#66491=CARTESIAN_POINT('Ctrl Pts',(0.32181192666296,2.08272050904744,10.5364599223271));
#66492=CARTESIAN_POINT('Ctrl Pts',(0.321841822342641,2.08328658165731,10.5364954576631));
#66493=CARTESIAN_POINT('Ctrl Pts',(0.321886872663395,2.08418458866005,10.5365516928382));
#66494=CARTESIAN_POINT('Ctrl Pts',(0.32190300761598,2.08451646942695,10.5365724461804));
#66495=CARTESIAN_POINT('Ctrl Pts',(0.32193259837074,2.08514516872753,10.5366117032035));
#66496=CARTESIAN_POINT('Ctrl Pts',(0.321946157007971,2.08544198174986,10.536630212584));
#66497=CARTESIAN_POINT('Ctrl Pts',(0.321968970378172,2.08595701444704,10.5366622878935));
#66498=CARTESIAN_POINT('Ctrl Pts',(0.321978413769105,2.08617522522909,10.5366758644792));
#66499=CARTESIAN_POINT('Ctrl Pts',(0.321996350456338,2.08659968184639,10.5367022473699));
#66500=CARTESIAN_POINT('Ctrl Pts',(0.322004867418532,2.08680592583026,10.5367150550038));
#66501=CARTESIAN_POINT('Ctrl Pts',(0.322024609421249,2.08729539862132,10.5367454231772));
#66502=CARTESIAN_POINT('Ctrl Pts',(0.322035658987624,2.08757863490053,10.5367629738036));
#66503=CARTESIAN_POINT('Ctrl Pts',(0.322073198118167,2.08857461665292,10.536824612895));
#66504=CARTESIAN_POINT('Ctrl Pts',(0.322097695508164,2.08928744185935,10.5368685902591));
#66505=CARTESIAN_POINT('Ctrl Pts',(0.322394574180558,2.0988508277221,10.5374568198488));
#66506=CARTESIAN_POINT('Ctrl Pts',(0.322304473587786,2.1077098242799,10.5379813178887));
#66507=CARTESIAN_POINT('Ctrl Pts',(0.320543344624518,2.14194887734258,10.5399677603813));
#66508=CARTESIAN_POINT('Ctrl Pts',(0.316236397413458,2.16710050031738,10.5413468143285));
#66509=CARTESIAN_POINT('Ctrl Pts',(0.304438959983997,2.20694942041212,10.5437109711794));
#66510=CARTESIAN_POINT('Ctrl Pts',(0.298707296777487,2.2220454769318,10.5446506404175));
#66511=CARTESIAN_POINT('Ctrl Pts',(0.291369965154471,2.23771751407591,10.5457027066269));
#66512=CARTESIAN_POINT('Ctrl Pts',(0.290863358505971,2.23878428188328,10.545774705388));
#66513=CARTESIAN_POINT('Ctrl Pts',(0.290120038527578,2.24032755224431,10.54587943514));
#66514=CARTESIAN_POINT('Ctrl Pts',(0.289887986375206,2.24080629966053,10.5459120040562));
#66515=CARTESIAN_POINT('Ctrl Pts',(0.289480492622174,2.24164172412853,10.5459689784225));
#66516=CARTESIAN_POINT('Ctrl Pts',(0.289305574159119,2.24199865626495,10.5459933655934));
#66517=CARTESIAN_POINT('Ctrl Pts',(0.288965993843291,2.24268835929184,10.5460405767786));
#66518=CARTESIAN_POINT('Ctrl Pts',(0.288801416301194,2.24302117121557,10.5460633978182));
#66519=CARTESIAN_POINT('Ctrl Pts',(0.288409239192875,2.24381080230298,10.5461176375502));
#66520=CARTESIAN_POINT('Ctrl Pts',(0.288181129362104,2.24426736562937,10.546149074078));
#66521=CARTESIAN_POINT('Ctrl Pts',(0.287372324604835,2.24587662110384,10.5462601459671));
#66522=CARTESIAN_POINT('Ctrl Pts',(0.286785796323622,2.24702635302132,10.5463399859354));
#66523=CARTESIAN_POINT('Ctrl Pts',(0.277473990296513,2.26501192831503,10.5475966630482));
#66524=CARTESIAN_POINT('Ctrl Pts',(0.267288070416979,2.28104587333796,10.5488268991088));
#66525=CARTESIAN_POINT('Ctrl Pts',(0.242114820432351,2.31387863424393,10.5515892470896));
#66526=CARTESIAN_POINT('Ctrl Pts',(0.226657609926543,2.33019544606607,10.5531291554941));
#66527=CARTESIAN_POINT('Ctrl Pts',(0.20347539793629,2.35004931177874,10.5551473341641));
#66528=CARTESIAN_POINT('Ctrl Pts',(0.197120678219569,2.3550889241483,10.555674495576));
#66529=CARTESIAN_POINT('Ctrl Pts',(0.189895166827062,2.36038764720717,10.5562399506711));
#66530=CARTESIAN_POINT('Ctrl Pts',(0.18920626158819,2.360888657891,10.5562935330643));
#66531=CARTESIAN_POINT('Ctrl Pts',(0.188155054648464,2.36164680084135,10.5563747839907));
#66532=CARTESIAN_POINT('Ctrl Pts',(0.187794200757419,2.36190592041364,10.5564025843925));
#66533=CARTESIAN_POINT('Ctrl Pts',(0.187127349168036,2.36238268200749,10.5564537894692));
#66534=CARTESIAN_POINT('Ctrl Pts',(0.186821505342916,2.36260053649778,10.5564772085336));
#66535=CARTESIAN_POINT('Ctrl Pts',(0.186323273899272,2.36295411892931,10.5565152516241));
#66536=CARTESIAN_POINT('Ctrl Pts',(0.186131118183713,2.36309017066962,10.5565298979796));
#66537=CARTESIAN_POINT('Ctrl Pts',(0.185758703992458,2.36335323833534,10.5565582334004));
#66538=CARTESIAN_POINT('Ctrl Pts',(0.185578464815048,2.36348027942862,10.5565719241584));
#66539=CARTESIAN_POINT('Ctrl Pts',(0.185163715864568,2.3637719773942,10.5566033757038));
#66540=CARTESIAN_POINT('Ctrl Pts',(0.184929116103176,2.36393650704296,10.5566211276847));
#66541=CARTESIAN_POINT('Ctrl Pts',(0.184202088224695,2.36444494147689,10.5566760237087));
#66542=CARTESIAN_POINT('Ctrl Pts',(0.183708914321381,2.36478778520095,10.5567130952737));
#66543=CARTESIAN_POINT('Ctrl Pts',(0.179637343743088,2.36760140121782,10.5570178070266));
#66544=CARTESIAN_POINT('Ctrl Pts',(0.176010022518462,2.37000104018423,10.5572807293496));
#66545=CARTESIAN_POINT('Ctrl Pts',(0.172160430631532,2.37243715686939,10.5575521722855));
#66546=CARTESIAN_POINT('Ctrl Pts',(0.171985724289401,2.37254748019269,10.5575644750564));
#66547=CARTESIAN_POINT('Ctrl Pts',(0.16118216205862,2.37935517464807,10.5583242693841));
#66548=CARTESIAN_POINT('Ctrl Pts',(0.150169800502539,2.38542616349531,10.5590398337862));
#66549=CARTESIAN_POINT('Ctrl Pts',(0.117976353414167,2.40079349279074,10.5610469234844));
#66550=CARTESIAN_POINT('Ctrl Pts',(0.096113673907244,2.40847572411003,10.5623166835501));
#66551=CARTESIAN_POINT('Ctrl Pts',(0.065274844612407,2.41571158265307,10.5641554768292));
#66552=CARTESIAN_POINT('Ctrl Pts',(0.0568579670839611,2.4173354081519,10.564661284396));
#66553=CARTESIAN_POINT('Ctrl Pts',(0.0458654961957418,2.41900475848226,
10.5653315777093));
#66554=CARTESIAN_POINT('Ctrl Pts',(0.0433397028400127,2.419357713633,10.5654862416734));
#66555=CARTESIAN_POINT('Ctrl Pts',(0.0400979718247462,2.41977154905724,
10.5656856576872));
#66556=CARTESIAN_POINT('Ctrl Pts',(0.0393856053207816,2.41986007098623,
10.5657295353681));
#66557=CARTESIAN_POINT('Ctrl Pts',(0.0382398082148054,2.41999856726033,
10.5658002023354));
#66558=CARTESIAN_POINT('Ctrl Pts',(0.0378065587415218,2.42005004310909,
10.5658269442029));
#66559=CARTESIAN_POINT('Ctrl Pts',(0.0369828209617547,2.42014621824729,
10.5658778294155));
#66560=CARTESIAN_POINT('Ctrl Pts',(0.0365923524976448,2.42019108332501,
10.5659019674842));
#66561=CARTESIAN_POINT('Ctrl Pts',(0.035704192363729,2.42029148764023,10.5659569120619));
#66562=CARTESIAN_POINT('Ctrl Pts',(0.0352064522332342,2.42034658125813,
10.565987732558));
#66563=CARTESIAN_POINT('Ctrl Pts',(0.0337292669033049,2.42050660290181,
10.5660792871369));
#66564=CARTESIAN_POINT('Ctrl Pts',(0.0327494734469116,2.42060819999485,
10.5661401259636));
#66565=CARTESIAN_POINT('Ctrl Pts',(0.0260113855047616,2.42127567857826,
10.5665593061371));
#66566=CARTESIAN_POINT('Ctrl Pts',(0.0202395431237707,2.42169085735756,
10.5669223609759));
#66567=CARTESIAN_POINT('Ctrl Pts',(-0.0172178028731702,2.42337320013905,
10.5693063371594));
#66568=CARTESIAN_POINT('Ctrl Pts',(-0.0489280897835026,2.4201123125505,
10.5714783113904));
#66569=CARTESIAN_POINT('Ctrl Pts',(-0.0880236101749342,2.41014165716153,
10.5741841571817));
#66570=CARTESIAN_POINT('Ctrl Pts',(-0.0963168031990844,2.40766718858197,
10.5747580994913));
#66571=CARTESIAN_POINT('Ctrl Pts',(-0.109057063921883,2.40330006584989,
10.5756301787366));
#66572=CARTESIAN_POINT('Ctrl Pts',(-0.113577934620847,2.40163625797509,
10.5759376712134));
#66573=CARTESIAN_POINT('Ctrl Pts',(-0.118586076441395,2.39966454183678,
10.5762747683519));
#66574=CARTESIAN_POINT('Ctrl Pts',(-0.119111513942201,2.39945607761063,
10.5763100914047));
#66575=CARTESIAN_POINT('Ctrl Pts',(-0.119894867027678,2.39914289890518,
10.5763626843279));
#66576=CARTESIAN_POINT('Ctrl Pts',(-0.120153196292357,2.39903923242129,
10.5763800169092));
#66577=CARTESIAN_POINT('Ctrl Pts',(-0.120595346399146,2.39886113394254,
10.5764096633702));
#66578=CARTESIAN_POINT('Ctrl Pts',(-0.120779232835042,2.3987868669657,10.5764219872662));
#66579=CARTESIAN_POINT('Ctrl Pts',(-0.12115854960684,2.3986332633328,10.576447396615));
#66580=CARTESIAN_POINT('Ctrl Pts',(-0.121353970099612,2.3985539047698,10.5764604806711));
#66581=CARTESIAN_POINT('Ctrl Pts',(-0.121884230864947,2.39833796383233,
10.5764959658328));
#66582=CARTESIAN_POINT('Ctrl Pts',(-0.122218920670413,2.39820100910352,
10.5765183443094));
#66583=CARTESIAN_POINT('Ctrl Pts',(-0.123470866648126,2.3976862522899,10.5766019848372));
#66584=CARTESIAN_POINT('Ctrl Pts',(-0.124386619531889,2.39730477402026,
10.5766630265201));
#66585=CARTESIAN_POINT('Ctrl Pts',(-0.141116613272475,2.39024467361929,
10.5777759245174));
#66586=CARTESIAN_POINT('Ctrl Pts',(-0.156376640253126,2.38231613100658,
10.5787543278887));
#66587=CARTESIAN_POINT('Ctrl Pts',(-0.179136967381346,2.36807601148445,
10.5802630195009));
#66588=CARTESIAN_POINT('Ctrl Pts',(-0.187104549930598,2.36257701927363,
10.5808015566657));
#66589=CARTESIAN_POINT('Ctrl Pts',(-0.203188372799222,2.35037213921557,
10.5819329174542));
#66590=CARTESIAN_POINT('Ctrl Pts',(-0.211247659363526,2.34361061522045,
10.5825257741194));
#66591=CARTESIAN_POINT('Ctrl Pts',(-0.227386279839951,2.32866674752519,
10.5837914802736));
#66592=CARTESIAN_POINT('Ctrl Pts',(-0.235387082588142,2.320422047849,10.5844658289547));
#66593=CARTESIAN_POINT('Ctrl Pts',(-0.244274463793905,2.31022689081575,
10.5852835815859));
#66594=CARTESIAN_POINT('Ctrl Pts',(-0.245603773718876,2.30867233961381,
10.5854078444174));
#66595=CARTESIAN_POINT('Ctrl Pts',(-0.247343519735688,2.30659815331847,
10.5855731266076));
#66596=CARTESIAN_POINT('Ctrl Pts',(-0.247767301216633,2.30608973324105,
10.585613599555));
#66597=CARTESIAN_POINT('Ctrl Pts',(-0.248459862033337,2.30525362895798,
10.5856800930083));
#66598=CARTESIAN_POINT('Ctrl Pts',(-0.248729567957947,2.30492671193083,
10.5857060757857));
#66599=CARTESIAN_POINT('Ctrl Pts',(-0.249250497121747,2.30429273777351,
10.5857564321111));
#66600=CARTESIAN_POINT('Ctrl Pts',(-0.249501799890435,2.30398574673646,
10.5857808023739));
#66601=CARTESIAN_POINT('Ctrl Pts',(-0.250080102888337,2.30327662532351,
10.5858370638657));
#66602=CARTESIAN_POINT('Ctrl Pts',(-0.250406700518736,2.30287416936089,
10.5858689712581));
#66603=CARTESIAN_POINT('Ctrl Pts',(-0.251447128460819,2.30158574283301,
10.5859710467707));
#66604=CARTESIAN_POINT('Ctrl Pts',(-0.252157232493726,2.30069678665248,
10.586041364226));
#66605=CARTESIAN_POINT('Ctrl Pts',(-0.258562226195379,2.29259092985175,
10.5866815882502));
#66606=CARTESIAN_POINT('Ctrl Pts',(-0.263950066744734,2.28513785547657,
10.5872635778829));
#66607=CARTESIAN_POINT('Ctrl Pts',(-0.28512229784868,2.25304382565872,10.5897461654487));
#66608=CARTESIAN_POINT('Ctrl Pts',(-0.297830858428574,2.22654401784866,
10.5917569510796));
#66609=CARTESIAN_POINT('Ctrl Pts',(-0.310491968264639,2.18719026581581,
10.5945207747618));
#66610=CARTESIAN_POINT('Ctrl Pts',(-0.313545147746194,2.17547794401441,
10.5953150983829));
#66611=CARTESIAN_POINT('Ctrl Pts',(-0.31606938711927,2.16294279820265,10.5961171699345));
#66612=CARTESIAN_POINT('Ctrl Pts',(-0.316203649537132,2.16226480032803,
10.596160404658));
#66613=CARTESIAN_POINT('Ctrl Pts',(-0.316393491237794,2.16128968660102,
10.5962223688447));
#66614=CARTESIAN_POINT('Ctrl Pts',(-0.316450834122996,2.16099292226107,
10.5962411980469));
#66615=CARTESIAN_POINT('Ctrl Pts',(-0.316549613774467,2.16047782263469,
10.5962738296575));
#66616=CARTESIAN_POINT('Ctrl Pts',(-0.316591242288312,2.16025952471552,
10.596287643086));
#66617=CARTESIAN_POINT('Ctrl Pts',(-0.316671285119646,2.15983741155213,
10.5963143228405));
#66618=CARTESIAN_POINT('Ctrl Pts',(-0.31670972839222,2.15963360280017,10.59632719083));
#66619=CARTESIAN_POINT('Ctrl Pts',(-0.316800935970401,2.15914748578624,
10.5963578505104));
#66620=CARTESIAN_POINT('Ctrl Pts',(-0.31685351981461,2.15886514324398,10.5963756318366));
#66621=CARTESIAN_POINT('Ctrl Pts',(-0.31703935137816,2.15785987962582,10.5964388492212));
#66622=CARTESIAN_POINT('Ctrl Pts',(-0.317170504314376,2.15713656632056,
10.5964841665712));
#66623=CARTESIAN_POINT('Ctrl Pts',(-0.319092072746676,2.14632852151334,
10.5971588772194));
#66624=CARTESIAN_POINT('Ctrl Pts',(-0.320403414841058,2.13616328860763,
10.5977618094621));
#66625=CARTESIAN_POINT('Ctrl Pts',(-0.321918157653852,2.11741394208228,
10.5988441931149));
#66626=CARTESIAN_POINT('Ctrl Pts',(-0.322267290657169,2.10885164379212,
10.5993272535047));
#66627=CARTESIAN_POINT('Ctrl Pts',(-0.322296636588479,2.07570046651955,
10.601186051383));
#66628=CARTESIAN_POINT('Ctrl Pts',(-0.319505367940961,2.0511961850701,10.602542691801));
#66629=CARTESIAN_POINT('Ctrl Pts',(-0.312340037700187,2.02027477169855,
10.6044113735494));
#66630=CARTESIAN_POINT('Ctrl Pts',(-0.31049241481586,2.01335786510524,10.6048392905674));
#66631=CARTESIAN_POINT('Ctrl Pts',(-0.308107975234007,2.00549190605433,
10.605339434162));
#66632=CARTESIAN_POINT('Ctrl Pts',(-0.307794765507169,2.00447677503312,
10.6054042398864));
#66633=CARTESIAN_POINT('Ctrl Pts',(-0.307325575837745,2.00298237238634,
10.6055000329622));
#66634=CARTESIAN_POINT('Ctrl Pts',(-0.307173479392267,2.00250188111931,
10.6055308927902));
#66635=CARTESIAN_POINT('Ctrl Pts',(-0.306900312063915,2.00164589620389,
10.6055859762537));
#66636=CARTESIAN_POINT('Ctrl Pts',(-0.306779677323799,2.00127026356069,
10.6056101855034));
#66637=CARTESIAN_POINT('Ctrl Pts',(-0.306526043773771,2.0004854521705,10.6056608436686));
#66638=CARTESIAN_POINT('Ctrl Pts',(-0.306392914790433,2.00007631659774,
10.6056872968324));
#66639=CARTESIAN_POINT('Ctrl Pts',(-0.306043897466262,1.99901096257498,
10.605756294479));
#66640=CARTESIAN_POINT('Ctrl Pts',(-0.305826718586659,1.99835517207938,
10.6057988814705));
#66641=CARTESIAN_POINT('Ctrl Pts',(-0.304879275481652,1.99552481129498,
10.6059831852163));
#66642=CARTESIAN_POINT('Ctrl Pts',(-0.304127928140794,1.99335741675813,
10.6061255976407));
#66643=CARTESIAN_POINT('Ctrl Pts',(-0.298682269830024,1.9781742054304,10.6071324663503));
#66644=CARTESIAN_POINT('Ctrl Pts',(-0.293177774983284,1.96546627276261,
10.6080240757013));
#66645=CARTESIAN_POINT('Ctrl Pts',(-0.271213723579515,1.92255826332494,
10.6112075045243));
#66646=CARTESIAN_POINT('Ctrl Pts',(-0.25076190532429,1.8946693392804,10.6136178430061));
#66647=CARTESIAN_POINT('Ctrl Pts',(-0.225367068715988,1.86962519463814,
10.6158695597912));
#66648=CARTESIAN_POINT('Ctrl Pts',(-0.22443565534175,1.86871769770558,10.615951252841));
#66649=CARTESIAN_POINT('Ctrl Pts',(-0.223208023036623,1.86753598789736,
10.6160577312765));
#66650=CARTESIAN_POINT('Ctrl Pts',(-0.222916762839665,1.8672566750257,10.6160829063184));
#66651=CARTESIAN_POINT('Ctrl Pts',(-0.222466385788397,1.86682639315913,
10.6161216989087));
#66652=CARTESIAN_POINT('Ctrl Pts',(-0.222307639481643,1.86667503956559,
10.6161353463728));
#66653=CARTESIAN_POINT('Ctrl Pts',(-0.221990636653397,1.86637341656219,
10.6161625472941));
#66654=CARTESIAN_POINT('Ctrl Pts',(-0.22183238311201,1.86622314688169,10.6161761007187));
#66655=CARTESIAN_POINT('Ctrl Pts',(-0.221477040660004,1.86588641710555,
10.6162064759576));
#66656=CARTESIAN_POINT('Ctrl Pts',(-0.221279869335252,1.86570004553253,
10.6162232908556));
#66657=CARTESIAN_POINT('Ctrl Pts',(-0.220696249650655,1.86514978652333,
10.6162729461702));
#66658=CARTESIAN_POINT('Ctrl Pts',(-0.220309134979495,1.86478660235013,
10.6163057323226));
#66659=CARTESIAN_POINT('Ctrl Pts',(-0.217265954467987,1.86194564770577,
10.6165623119707));
#66660=CARTESIAN_POINT('Ctrl Pts',(-0.214568933619921,1.85951186088423,
10.6167828058736));
#66661=CARTESIAN_POINT('Ctrl Pts',(-0.204857607450188,1.85104184937922,
10.6175550935828));
#66662=CARTESIAN_POINT('Ctrl Pts',(-0.197624665123048,1.845262249667,10.6180913142792));
#66663=CARTESIAN_POINT('Ctrl Pts',(-0.174733631410519,1.8285335379895,10.619707080129));
#66664=CARTESIAN_POINT('Ctrl Pts',(-0.158343497741734,1.81865809511967,
10.6207566475133));
#66665=CARTESIAN_POINT('Ctrl Pts',(-0.133136484103511,1.80637470779252,
10.6223407512847));
#66666=CARTESIAN_POINT('Ctrl Pts',(-0.124938929559806,1.80279403674246,
10.6228512335219));
#66667=CARTESIAN_POINT('Ctrl Pts',(-0.107467592621994,1.79601327518428,
10.623941705396));
#66668=CARTESIAN_POINT('Ctrl Pts',(-0.0981755345735269,1.79288642586867,
10.6245231228728));
#66669=CARTESIAN_POINT('Ctrl Pts',(-0.0877554484144572,1.78990124086157,
10.6251822306309));
#66670=CARTESIAN_POINT('Ctrl Pts',(-0.0867534059837163,1.78961941804284,
10.6252456822977));
#66671=CARTESIAN_POINT('Ctrl Pts',(-0.0852525691471043,1.78920514580274,
10.6253408278287));
#66672=CARTESIAN_POINT('Ctrl Pts',(-0.0847547865849184,1.78906903002799,
10.6253724026358));
#66673=CARTESIAN_POINT('Ctrl Pts',(-0.0838968731253664,1.78883665179657,
10.625426852469));
#66674=CARTESIAN_POINT('Ctrl Pts',(-0.0835368971228926,1.78873981719055,
10.6254497088985));
#66675=CARTESIAN_POINT('Ctrl Pts',(-0.0827935649358112,1.7885412410224,
10.625496926344));
#66676=CARTESIAN_POINT('Ctrl Pts',(-0.0824101874477816,1.78843958219748,
10.6255212899976));
#66677=CARTESIAN_POINT('Ctrl Pts',(-0.0815173047724491,1.78820458306228,
10.6255780587906));
#66678=CARTESIAN_POINT('Ctrl Pts',(-0.0810076595440639,1.78807178375359,
10.6256104813763));
#66679=CARTESIAN_POINT('Ctrl Pts',(-0.0793820940251987,1.78765245934999,
10.6257139607775));
#66680=CARTESIAN_POINT('Ctrl Pts',(-0.0782649712204857,1.78737067119903,
10.6257851704363));
#66681=CARTESIAN_POINT('Ctrl Pts',(-0.0539025035305845,1.78136413467667,
10.6273403146344));
#66682=CARTESIAN_POINT('Ctrl Pts',(-0.0300976181337822,1.77824236614711,
10.6289118564704));
#66683=CARTESIAN_POINT('Ctrl Pts',(0.0194202162551432,1.77729392558828,
10.6322496605817));
#66684=CARTESIAN_POINT('Ctrl Pts',(0.0449808675715732,1.77985429211685,
10.634009325584));
#66685=CARTESIAN_POINT('Ctrl Pts',(0.0713675412905889,1.78572321458893,
10.635717942723));
#66686=CARTESIAN_POINT('Ctrl Pts',(0.0727624928167553,1.78604324562439,
10.6358079194757));
#66687=CARTESIAN_POINT('Ctrl Pts',(0.074562984093129,1.78646896082003,10.6359235592042));
#66688=CARTESIAN_POINT('Ctrl Pts',(0.074970486011003,1.78656615154366,10.6359496988704));
#66689=CARTESIAN_POINT('Ctrl Pts',(0.0755940662386094,1.78671616343589,
10.6359896475533));
#66690=CARTESIAN_POINT('Ctrl Pts',(0.0758102793292276,1.78676841370714,
10.6360034894033));
#66691=CARTESIAN_POINT('Ctrl Pts',(0.0762362066212751,1.78687181056222,
10.6360307380852));
#66692=CARTESIAN_POINT('Ctrl Pts',(0.0764459223098293,1.786922943697,10.6360441455386));
#66693=CARTESIAN_POINT('Ctrl Pts',(0.0769131365888853,1.78703735789413,
10.636073995078));
#66694=CARTESIAN_POINT('Ctrl Pts',(0.0771706078483092,1.78710074589516,
10.6360904308459));
#66695=CARTESIAN_POINT('Ctrl Pts',(0.0779148099409177,1.78728493877614,
10.6361378985708));
#66696=CARTESIAN_POINT('Ctrl Pts',(0.0784013401768999,1.78740656278343,
10.6361688832511));
#66697=CARTESIAN_POINT('Ctrl Pts',(0.0817089081797216,1.78824160454065,
10.6363792123137));
#66698=CARTESIAN_POINT('Ctrl Pts',(0.0845205709420133,1.78899209442381,
10.6365564546037));
#66699=CARTESIAN_POINT('Ctrl Pts',(0.0933128253739693,1.79146697340311,
10.6371069265859));
#66700=CARTESIAN_POINT('Ctrl Pts',(0.0992541580732603,1.79332666479782,
10.6374733897348));
#66701=CARTESIAN_POINT('Ctrl Pts',(0.119215023012988,1.80021556029978,10.6386973012408));
#66702=CARTESIAN_POINT('Ctrl Pts',(0.132939064138795,1.80604388748199,10.639527016108));
#66703=CARTESIAN_POINT('Ctrl Pts',(0.169542697212373,1.82467860025403,10.641822881413));
#66704=CARTESIAN_POINT('Ctrl Pts',(0.191335748512181,1.83935279048595,10.6432943581486));
#66705=CARTESIAN_POINT('Ctrl Pts',(0.212279481607717,1.8575108658658,10.6449751645429));
#66706=CARTESIAN_POINT('Ctrl Pts',(0.213438517119665,1.85853042062116,10.6450691072026));
#66707=CARTESIAN_POINT('Ctrl Pts',(0.215001014936618,1.85992492331234,10.6451970344123));
#66708=CARTESIAN_POINT('Ctrl Pts',(0.21541091963552,1.86029264807644,10.6452307158567));
#66709=CARTESIAN_POINT('Ctrl Pts',(0.216103699136472,1.86091735131971,10.6452878474066));
#66710=CARTESIAN_POINT('Ctrl Pts',(0.216387063987401,1.86117378657834,10.645311274568));
#66711=CARTESIAN_POINT('Ctrl Pts',(0.216954906414712,1.86168950429582,10.6453583396015));
#66712=CARTESIAN_POINT('Ctrl Pts',(0.217239376954549,1.8619487935788,10.6453819777428));
#66713=CARTESIAN_POINT('Ctrl Pts',(0.217881641035293,1.86253631461306,10.6454354833417));
#66714=CARTESIAN_POINT('Ctrl Pts',(0.21823915807105,1.86286484600949,10.645465363519));
#66715=CARTESIAN_POINT('Ctrl Pts',(0.218983914879014,1.8635523325278,10.6455278100063));
#66716=CARTESIAN_POINT('Ctrl Pts',(0.219371017367135,1.86391143364668,10.6455603825151));
#66717=CARTESIAN_POINT('Ctrl Pts',(0.22037907645848,1.8648511938419,10.6456455061342));
#66718=CARTESIAN_POINT('Ctrl Pts',(0.22099861800348,1.86543335873016,10.6456981218718));
#66719=CARTESIAN_POINT('Ctrl Pts',(0.222822318519872,1.86716067479155,10.6458538967324));
#66720=CARTESIAN_POINT('Ctrl Pts',(0.224019918100671,1.86831268243233,10.6459573520598));
#66721=CARTESIAN_POINT('Ctrl Pts',(0.231298667419133,1.87542353177667,10.6465933494701));
#66722=CARTESIAN_POINT('Ctrl Pts',(0.237150126908992,1.88161167821181,10.6471359483214));
#66723=CARTESIAN_POINT('Ctrl Pts',(0.252169280378877,1.89881119941972,10.6486170249649));
#66724=CARTESIAN_POINT('Ctrl Pts',(0.260858721349144,1.91021346007024,10.6495720562922));
#66725=CARTESIAN_POINT('Ctrl Pts',(0.282501343320614,1.94291984497887,10.6522176987259));
#66726=CARTESIAN_POINT('Ctrl Pts',(0.293790414935612,1.96520912059328,10.6539263126378));
#66727=CARTESIAN_POINT('Ctrl Pts',(0.302891766995221,1.98991017059744,10.6555900763948));
#66728=CARTESIAN_POINT('Ctrl Pts',(0.303374033980378,1.99124620128637,10.6556793697068));
#66729=CARTESIAN_POINT('Ctrl Pts',(0.303986684019226,1.99297922612357,10.6557942567575));
#66730=CARTESIAN_POINT('Ctrl Pts',(0.304125140544139,1.99337331949361,10.6558203196843));
#66731=CARTESIAN_POINT('Ctrl Pts',(0.30433607238275,1.99397745503928,10.6558601764265));
#66732=CARTESIAN_POINT('Ctrl Pts',(0.304409096665997,1.99418730293108,10.6558740028388));
#66733=CARTESIAN_POINT('Ctrl Pts',(0.304552642169033,1.99460118418463,10.6559012370012));
#66734=CARTESIAN_POINT('Ctrl Pts',(0.30462317498462,1.99480521167726,10.6559146453406));
#66735=CARTESIAN_POINT('Ctrl Pts',(0.304780011128814,1.99526036589225,10.6559445193687));
#66736=CARTESIAN_POINT('Ctrl Pts',(0.304866208885128,1.99551152782277,10.6559609786875));
#66737=CARTESIAN_POINT('Ctrl Pts',(0.305114883856299,1.9962390411451,10.6560085810441));
#66738=CARTESIAN_POINT('Ctrl Pts',(0.305276556676943,1.99671566970388,10.6560396763884));
#66739=CARTESIAN_POINT('Ctrl Pts',(0.30637777793519,1.99998736124088,10.6562525096066));
#66740=CARTESIAN_POINT('Ctrl Pts',(0.307280082143515,2.00279494187017,10.6564320877241));
#66741=CARTESIAN_POINT('Ctrl Pts',(0.309989318788065,2.011639897083,10.6569894177268));
#66742=CARTESIAN_POINT('Ctrl Pts',(0.311657886227521,2.01771842015475,10.6573602506798));
#66743=CARTESIAN_POINT('Ctrl Pts',(0.316814249258722,2.0389205061916,10.6586241857859));
#66744=CARTESIAN_POINT('Ctrl Pts',(0.319387696355035,2.0542448223527,10.6594871295216));
#66745=CARTESIAN_POINT('Ctrl Pts',(0.323242548071882,2.09505818281226,10.6617790406768));
#66746=CARTESIAN_POINT('Ctrl Pts',(0.322622227332921,2.1206108252254,10.6632148622806));
#66747=CARTESIAN_POINT('Ctrl Pts',(0.318785689652102,2.14731963711145,10.6648513518471));
#66748=CARTESIAN_POINT('Ctrl Pts',(0.318560066550367,2.14881544695234,10.6649434247268));
#66749=CARTESIAN_POINT('Ctrl Pts',(0.318238675818512,2.1508489827476,10.6650691896555));
#66750=CARTESIAN_POINT('Ctrl Pts',(0.318152057451664,2.15138815200677,10.6651025916431));
#66751=CARTESIAN_POINT('Ctrl Pts',(0.318002696188449,2.15230302025392,10.6651593659371));
#66752=CARTESIAN_POINT('Ctrl Pts',(0.317940656624139,2.15267883421451,10.6651827158922));
#66753=CARTESIAN_POINT('Ctrl Pts',(0.317814554358334,2.15343437997761,10.6652297157877));
#66754=CARTESIAN_POINT('Ctrl Pts',(0.317750476992271,2.15381410869614,10.6652533661601));
#66755=CARTESIAN_POINT('Ctrl Pts',(0.317603577694458,2.15467523815503,10.6653070649342));
#66756=CARTESIAN_POINT('Ctrl Pts',(0.317520341721644,2.15515656643058,10.6653371264502));
#66757=CARTESIAN_POINT('Ctrl Pts',(0.317344161921807,2.15616174478203,10.6654000032942));
#66758=CARTESIAN_POINT('Ctrl Pts',(0.317251014614405,2.15668555727431,10.6654328250236));
#66759=CARTESIAN_POINT('Ctrl Pts',(0.317003956941087,2.15805519807774,10.6655187927285));
#66760=CARTESIAN_POINT('Ctrl Pts',(0.316847959092205,2.15890064122136,10.6655720050934));
#66761=CARTESIAN_POINT('Ctrl Pts',(0.316375773450556,2.16140352331891,10.6657299770651));
#66762=CARTESIAN_POINT('Ctrl Pts',(0.316049953459208,2.16305909487507,10.6658350429276));
#66763=CARTESIAN_POINT('Ctrl Pts',(0.313985769809988,2.17312964953418,10.6664776997566));
#66764=CARTESIAN_POINT('Ctrl Pts',(0.311924574635606,2.18147420811947,10.6670255271976));
#66765=CARTESIAN_POINT('Ctrl Pts',(0.305501076672879,2.20363372966154,10.6685227574027));
#66766=CARTESIAN_POINT('Ctrl Pts',(0.3005371700682,2.21725267244046,10.6694890652514));
#66767=CARTESIAN_POINT('Ctrl Pts',(0.284694823309773,2.25302803402335,10.6721293955553));
#66768=CARTESIAN_POINT('Ctrl Pts',(0.272161205444852,2.27434795152359,10.673819509377));
#66769=CARTESIAN_POINT('Ctrl Pts',(0.256480566732366,2.29514310635147,10.6754651586792));
#66770=CARTESIAN_POINT('Ctrl Pts',(0.255635325303682,2.29624906035773,10.6755526496523));
#66771=CARTESIAN_POINT('Ctrl Pts',(0.254529139669122,2.29767717228812,10.675665549127));
#66772=CARTESIAN_POINT('Ctrl Pts',(0.254274718886656,2.29800433006433,10.6756914073089));
#66773=CARTESIAN_POINT('Ctrl Pts',(0.253883333029285,2.29850561178841,10.6757310187178));
#66774=CARTESIAN_POINT('Ctrl Pts',(0.253746819537513,2.29868008525477,10.6757448039148));
#66775=CARTESIAN_POINT('Ctrl Pts',(0.253475606289268,2.29902597863009,10.6757721293538));
#66776=CARTESIAN_POINT('Ctrl Pts',(0.25334091333697,2.29919740154807,10.6757856698557));
#66777=CARTESIAN_POINT('Ctrl Pts',(0.25304053294945,2.29957889640688,10.6758157996974));
#66778=CARTESIAN_POINT('Ctrl Pts',(0.252874758251384,2.29978889820728,10.6758323826292));
#66779=CARTESIAN_POINT('Ctrl Pts',(0.252390492903354,2.30040079258708,10.6758806942903));
#66780=CARTESIAN_POINT('Ctrl Pts',(0.252071302452214,2.30080213411753,10.6759123731031));
#66781=CARTESIAN_POINT('Ctrl Pts',(0.249775341585834,2.30367491241943,10.6761390787685));
#66782=CARTESIAN_POINT('Ctrl Pts',(0.247763131919493,2.30611798440837,10.6763316115882));
#66783=CARTESIAN_POINT('Ctrl Pts',(0.242982958190087,2.31175053055,10.6767759438701));
#66784=CARTESIAN_POINT('Ctrl Pts',(0.240187605164842,2.31491608346832,10.6770260078519));
#66785=CARTESIAN_POINT('Ctrl Pts',(0.236070163782979,2.31939809758182,10.6773821157901));
#66786=CARTESIAN_POINT('Ctrl Pts',(0.234797714351001,2.32075932828418,10.6774905507741));
#66787=CARTESIAN_POINT('Ctrl Pts',(0.221179417581971,2.33507684602119,10.6786350476556));
#66788=CARTESIAN_POINT('Ctrl Pts',(0.207785796953426,2.34699515946784,10.6796240725259));
#66789=CARTESIAN_POINT('Ctrl Pts',(0.174864977644883,2.37170695202786,10.6819295707037));
#66790=CARTESIAN_POINT('Ctrl Pts',(0.154804513776457,2.3836155056448,10.6832522843232));
#66791=CARTESIAN_POINT('Ctrl Pts',(0.132384573503583,2.39383226526825,10.6847478978134));
#66792=CARTESIAN_POINT('Ctrl Pts',(0.131126697112627,2.39439576190327,10.6848318390195));
#66793=CARTESIAN_POINT('Ctrl Pts',(0.129384850896691,2.39516268652608,10.6849481306165));
#66794=CARTESIAN_POINT('Ctrl Pts',(0.128903928264723,2.39537303267501,10.6849802442848));
#66795=CARTESIAN_POINT('Ctrl Pts',(0.128078434539242,2.39573168743855,10.6850353772197));
#66796=CARTESIAN_POINT('Ctrl Pts',(0.127734113380773,2.39588057155916,10.6850583768034));
#66797=CARTESIAN_POINT('Ctrl Pts',(0.12703355943618,2.39618203960731,10.6851051783191));
#66798=CARTESIAN_POINT('Ctrl Pts',(0.126677309862307,2.39633458281642,10.6851289815937));
#66799=CARTESIAN_POINT('Ctrl Pts',(0.125857034529815,2.39668406865077,10.685183797833));
#66800=CARTESIAN_POINT('Ctrl Pts',(0.125392821014815,2.39688056548915,10.6852148258958));
#66801=CARTESIAN_POINT('Ctrl Pts',(0.124417825513626,2.39729057638326,10.6852800085365));
#66802=CARTESIAN_POINT('Ctrl Pts',(0.123906950977858,2.39750386485739,10.6853141706643));
#66803=CARTESIAN_POINT('Ctrl Pts',(0.122553639292316,2.39806477763315,10.6854046888093));
#66804=CARTESIAN_POINT('Ctrl Pts',(0.121710277337476,2.39841014482141,10.6854611211099));
#66805=CARTESIAN_POINT('Ctrl Pts',(0.104502349013638,2.40537192190849,10.6866130685066));
#66806=CARTESIAN_POINT('Ctrl Pts',(0.0876259173606703,2.41063525641142,
10.6877546825072));
#66807=CARTESIAN_POINT('Ctrl Pts',(0.0396795872400225,2.42136915630836,
10.6910242769546));
#66808=CARTESIAN_POINT('Ctrl Pts',(0.00811265859031779,2.42370783364828,
10.6932195853288));
#66809=CARTESIAN_POINT('Ctrl Pts',(-0.0248352673564854,2.42132037092403,
10.6953098178013));
#66810=CARTESIAN_POINT('Ctrl Pts',(-0.0263782197607249,2.42119738639265,
10.6954071922975));
#66811=CARTESIAN_POINT('Ctrl Pts',(-0.0283452870637515,2.42102632655017,
10.695530628623));
#66812=CARTESIAN_POINT('Ctrl Pts',(-0.0287702407712169,2.42098852142714,
10.6955572531464));
#66813=CARTESIAN_POINT('Ctrl Pts',(-0.0294453934027655,2.42092710634487,
10.6955994853193));
#66814=CARTESIAN_POINT('Ctrl Pts',(-0.0296956400592102,2.42090404756258,
10.6956151239062));
#66815=CARTESIAN_POINT('Ctrl Pts',(-0.0301632261325376,2.4208604105738,
10.6956443165365));
#66816=CARTESIAN_POINT('Ctrl Pts',(-0.0303805699767417,2.42083990439567,
10.6956578745056));
#66817=CARTESIAN_POINT('Ctrl Pts',(-0.0308690375485982,2.42079331715749,
10.6956883198061));
#66818=CARTESIAN_POINT('Ctrl Pts',(-0.0311401485078071,2.42076711328361,
10.6957052000784));
#66819=CARTESIAN_POINT('Ctrl Pts',(-0.0319446094951967,2.42068832965132,
10.6957552371758));
#66820=CARTESIAN_POINT('Ctrl Pts',(-0.0324778652822323,2.42063476281721,
10.6957883384688));
#66821=CARTESIAN_POINT('Ctrl Pts',(-0.0367726541316475,2.42019251661014,
10.6960544111927));
#66822=CARTESIAN_POINT('Ctrl Pts',(-0.0405274109805555,2.41973896820824,
10.6962838024268));
#66823=CARTESIAN_POINT('Ctrl Pts',(-0.0541199133891425,2.41785378269916,
10.697105310293));
#66824=CARTESIAN_POINT('Ctrl Pts',(-0.0638987778620044,2.41603318470171,
10.6976794049073));
#66825=CARTESIAN_POINT('Ctrl Pts',(-0.0883490186137163,2.41029951428344,
10.6991062673484));
#66826=CARTESIAN_POINT('Ctrl Pts',(-0.102856753168576,2.4057970769823,10.699945623268));
#66827=CARTESIAN_POINT('Ctrl Pts',(-0.137106292330893,2.39245334591317,
10.7020093375182));
#66828=CARTESIAN_POINT('Ctrl Pts',(-0.156377485599329,2.38261805928396,
10.7032442401006));
#66829=CARTESIAN_POINT('Ctrl Pts',(-0.17561307943088,2.37022752149179,10.7046339209849));
#66830=CARTESIAN_POINT('Ctrl Pts',(-0.176702141183835,2.36951664190246,
10.7047131527609));
#66831=CARTESIAN_POINT('Ctrl Pts',(-0.178213932620552,2.36851672578854,
10.7048239229565));
#66832=CARTESIAN_POINT('Ctrl Pts',(-0.178640331559171,2.3682332375824,10.7048552530785));
#66833=CARTESIAN_POINT('Ctrl Pts',(-0.179375106664404,2.36774219859225,
10.7049093935526));
#66834=CARTESIAN_POINT('Ctrl Pts',(-0.179683803582517,2.36753512764891,
10.7049321857958));
#66835=CARTESIAN_POINT('Ctrl Pts',(-0.18031505475115,2.36711010501215,10.7049788890919));
#66836=CARTESIAN_POINT('Ctrl Pts',(-0.180637573651193,2.36689210208032,
10.7050028020579));
#66837=CARTESIAN_POINT('Ctrl Pts',(-0.181385962907543,2.36638425902912,
10.7050584107111));
#66838=CARTESIAN_POINT('Ctrl Pts',(-0.181811533996101,2.3660939817047,10.7050901229393));
#66839=CARTESIAN_POINT('Ctrl Pts',(-0.182705622995961,2.36548098727846,
10.7051569390628));
#66840=CARTESIAN_POINT('Ctrl Pts',(-0.183173985591036,2.36515804773142,
10.7051920513624));
#66841=CARTESIAN_POINT('Ctrl Pts',(-0.184420619600864,2.3642936049633,10.7052858074805));
#66842=CARTESIAN_POINT('Ctrl Pts',(-0.185197356223901,2.36374990763086,
10.705344535034));
#66843=CARTESIAN_POINT('Ctrl Pts',(-0.203196940280945,2.35103190892641,
10.706712755718));
#66844=CARTESIAN_POINT('Ctrl Pts',(-0.219182381455994,2.33720199514564,
10.7080891514079));
#66845=CARTESIAN_POINT('Ctrl Pts',(-0.248567640916915,2.30625586813309,
10.7109528096696));
#66846=CARTESIAN_POINT('Ctrl Pts',(-0.261823764726807,2.28914461730038,
10.7124343056609));
#66847=CARTESIAN_POINT('Ctrl Pts',(-0.274078660937576,2.26954171839249,
10.7139536215175));
#66848=CARTESIAN_POINT('Ctrl Pts',(-0.274878797931887,2.2682413541729,10.7140536067864));
#66849=CARTESIAN_POINT('Ctrl Pts',(-0.276346327984832,2.26581793949615,
10.7142384018279));
#66850=CARTESIAN_POINT('Ctrl Pts',(-0.277016190000943,2.26469642567655,
10.7143233161256));
#66851=CARTESIAN_POINT('Ctrl Pts',(-0.277825243331271,2.26332297009478,
10.7144265419354));
#66852=CARTESIAN_POINT('Ctrl Pts',(-0.2779709307249,2.26307489097193,10.714445156741));
#66853=CARTESIAN_POINT('Ctrl Pts',(-0.278331126464863,2.26245965800917,
10.7144912456802));
#66854=CARTESIAN_POINT('Ctrl Pts',(-0.27854524135384,2.26209227298867,10.7145187010535));
#66855=CARTESIAN_POINT('Ctrl Pts',(-0.280800362596487,2.25820520176694,
10.7148084784105));
#66856=CARTESIAN_POINT('Ctrl Pts',(-0.282775387957434,2.25464738370695,
10.7150675629167));
#66857=CARTESIAN_POINT('Ctrl Pts',(-0.284934457358211,2.25057828308921,
10.7153561810135));
#66858=CARTESIAN_POINT('Ctrl Pts',(-0.285185114169217,2.25010301460757,
10.715389774017));
#66859=CARTESIAN_POINT('Ctrl Pts',(-0.28556292910928,2.24938227994497,10.7154405369427));
#66860=CARTESIAN_POINT('Ctrl Pts',(-0.285690960411689,2.24913727630437,
10.7154577616426));
#66861=CARTESIAN_POINT('Ctrl Pts',(-0.285913212403205,2.24871063333872,
10.7154877011998));
#66862=CARTESIAN_POINT('Ctrl Pts',(-0.286007575378837,2.24852906894342,
10.7155004251011));
#66863=CARTESIAN_POINT('Ctrl Pts',(-0.286205055633203,2.24814820993236,
10.715527078906));
#66864=CARTESIAN_POINT('Ctrl Pts',(-0.286308137666018,2.24794889753811,
10.7155410065065));
#66865=CARTESIAN_POINT('Ctrl Pts',(-0.286555054845509,2.24747025084163,
10.7155744035995));
#66866=CARTESIAN_POINT('Ctrl Pts',(-0.286698690340707,2.24719081255205,
10.7155938603938));
#66867=CARTESIAN_POINT('Ctrl Pts',(-0.287188368144886,2.24623472373415,
10.7156602935379));
#66868=CARTESIAN_POINT('Ctrl Pts',(-0.287532428853326,2.24555705276143,
10.7157071456582));
#66869=CARTESIAN_POINT('Ctrl Pts',(-0.297370732583404,2.22600826288821,
10.7170521064542));
#66870=CARTESIAN_POINT('Ctrl Pts',(-0.304990758557198,2.20624680751465,
10.7182370965088));
#66871=CARTESIAN_POINT('Ctrl Pts',(-0.317150367442741,2.16226567269911,
10.7207893142002));
#66872=CARTESIAN_POINT('Ctrl Pts',(-0.320964350568361,2.13798819359144,
10.7221516127689));
#66873=CARTESIAN_POINT('Ctrl Pts',(-0.322180229001526,2.10901803356642,
10.7238757771092));
#66874=CARTESIAN_POINT('Ctrl Pts',(-0.322274729601769,2.10451883197574,
10.7241460642757));
#66875=CARTESIAN_POINT('Ctrl Pts',(-0.322274999420556,2.10001932564221,
10.7244193016094));
#66876=CARTESIAN_POINT('',(-0.322274972444447,2.10013327014249,10.9749989620444));
#66877=CARTESIAN_POINT('Ctrl Pts',(-0.322274999426371,2.10001922843493,
10.7244193075124));
#66878=CARTESIAN_POINT('Ctrl Pts',(-0.322275071231016,2.09881575857202,
10.724492389518));
#66879=CARTESIAN_POINT('Ctrl Pts',(-0.322268401869339,2.09761230732818,
10.7245656794142));
#66880=CARTESIAN_POINT('Ctrl Pts',(-0.322249745832144,2.09593815378055,
10.724667934721));
#66881=CARTESIAN_POINT('Ctrl Pts',(-0.322243468099963,2.09546739072966,
10.7246967213388));
#66882=CARTESIAN_POINT('Ctrl Pts',(-0.32223032281347,2.09462078146521,10.7247485504602));
#66883=CARTESIAN_POINT('Ctrl Pts',(-0.322223829186279,2.09424492961336,
10.7247715812266));
#66884=CARTESIAN_POINT('Ctrl Pts',(-0.322209296423054,2.09348114419906,
10.7248184266186));
#66885=CARTESIAN_POINT('Ctrl Pts',(-0.322201214246663,2.09309321216156,
10.7248422425534));
#66886=CARTESIAN_POINT('Ctrl Pts',(-0.322183613877894,2.09231583909616,
10.7248900131817));
#66887=CARTESIAN_POINT('Ctrl Pts',(-0.322174090116559,2.0919263988397,10.7249139680112));
#66888=CARTESIAN_POINT('Ctrl Pts',(-0.322145415167206,2.09083482274152,
10.7249811773983));
#66889=CARTESIAN_POINT('Ctrl Pts',(-0.322124674678532,2.09013273400593,
10.7250244816914));
#66890=CARTESIAN_POINT('Ctrl Pts',(-0.322030837631842,2.08727302403359,
10.7252011801512));
#66891=CARTESIAN_POINT('Ctrl Pts',(-0.321938358205441,2.08511613442245,
10.7253351802876));
#66892=CARTESIAN_POINT('Ctrl Pts',(-0.319893129560837,2.04648827570738,
10.7277484858106));
#66893=CARTESIAN_POINT('Ctrl Pts',(-0.311775686476974,2.01061565133469,
10.7302506036039));
#66894=CARTESIAN_POINT('Ctrl Pts',(-0.293430908289663,1.9662386319519,10.7334657931135));
#66895=CARTESIAN_POINT('Ctrl Pts',(-0.288463479569405,1.95583799611667,
10.7342249254026));
#66896=CARTESIAN_POINT('Ctrl Pts',(-0.282196014634781,1.94434313099519,
10.7350533084369));
#66897=CARTESIAN_POINT('Ctrl Pts',(-0.281432640259525,1.94296713471299,
10.7351522865069));
#66898=CARTESIAN_POINT('Ctrl Pts',(-0.280455436392794,1.94123572289609,
10.7352765438088));
#66899=CARTESIAN_POINT('Ctrl Pts',(-0.280250974865409,1.94087508498612,
10.7353024097097));
#66900=CARTESIAN_POINT('Ctrl Pts',(-0.279924015668816,1.94030096539189,
10.7353435606193));
#66901=CARTESIAN_POINT('Ctrl Pts',(-0.279801969214595,1.94008722931695,
10.7353588746244));
#66902=CARTESIAN_POINT('Ctrl Pts',(-0.279570837359988,1.9396835301415,10.7353877879324));
#66903=CARTESIAN_POINT('Ctrl Pts',(-0.279461804032013,1.93949354001307,
10.7354013903852));
#66904=CARTESIAN_POINT('Ctrl Pts',(-0.279212819747438,1.93906070874216,
10.7354323684042));
#66905=CARTESIAN_POINT('Ctrl Pts',(-0.279072745893889,1.93881793932771,
10.7354497358507));
#66906=CARTESIAN_POINT('Ctrl Pts',(-0.278653946759488,1.93809427890708,
10.7355014835879));
#66907=CARTESIAN_POINT('Ctrl Pts',(-0.278374292100854,1.93761392277815,
10.7355358038853));
#66908=CARTESIAN_POINT('Ctrl Pts',(-0.27640369126366,1.93424911953815,10.7357760234984));
#66909=CARTESIAN_POINT('Ctrl Pts',(-0.274669110858645,1.93139028324105,
10.7359791525689));
#66910=CARTESIAN_POINT('Ctrl Pts',(-0.264994806037818,1.9159912772424,10.7370709058047));
#66911=CARTESIAN_POINT('Ctrl Pts',(-0.256239619859653,1.90398260881372,
10.7379139780569));
#66912=CARTESIAN_POINT('Ctrl Pts',(-0.227230156318473,1.86947483551174,
10.7404454445568));
#66913=CARTESIAN_POINT('Ctrl Pts',(-0.204616214479551,1.84918645442211,
10.7421067196102));
#66914=CARTESIAN_POINT('Ctrl Pts',(-0.177897636787063,1.83126711826859,
10.744041884923));
#66915=CARTESIAN_POINT('Ctrl Pts',(-0.176278550159977,1.83020229170451,
10.7441589768219));
#66916=CARTESIAN_POINT('Ctrl Pts',(-0.173850089544586,1.82863635492723,
10.7443343890193));
#66917=CARTESIAN_POINT('Ctrl Pts',(-0.173047919611941,1.82812411105513,
10.7443922968442));
#66918=CARTESIAN_POINT('Ctrl Pts',(-0.171761381140242,1.82731056317374,
10.7444851210777));
#66919=CARTESIAN_POINT('Ctrl Pts',(-0.171278457192703,1.82700697609108,
10.7445199530947));
#66920=CARTESIAN_POINT('Ctrl Pts',(-0.170357014085049,1.82643112420485,
10.7445863944146));
#66921=CARTESIAN_POINT('Ctrl Pts',(-0.169918641423097,1.82615862740662,
10.7446179950448));
#66922=CARTESIAN_POINT('Ctrl Pts',(-0.169148383254385,1.82568238896164,
10.7446735058839));
#66923=CARTESIAN_POINT('Ctrl Pts',(-0.168816778715979,1.82547819302436,
10.7446973993161));
#66924=CARTESIAN_POINT('Ctrl Pts',(-0.168168216441499,1.8250804398906,10.7447441222339));
#66925=CARTESIAN_POINT('Ctrl Pts',(-0.167851292509247,1.82488682846319,
10.7447669496817));
#66926=CARTESIAN_POINT('Ctrl Pts',(-0.167097703197015,1.82442824146782,
10.7448212202359));
#66927=CARTESIAN_POINT('Ctrl Pts',(-0.166660742142921,1.82416375593876,
10.7448526812252));
#66928=CARTESIAN_POINT('Ctrl Pts',(-0.165115391301949,1.82323339236031,
10.7449639216238));
#66929=CARTESIAN_POINT('Ctrl Pts',(-0.16400363594759,1.82257315402616,10.7450439064569));
#66930=CARTESIAN_POINT('Ctrl Pts',(-0.146216114275567,1.81215396132018,
10.7463230212281));
#66931=CARTESIAN_POINT('Ctrl Pts',(-0.128703039825372,1.80390917296598,
10.7475776898895));
#66932=CARTESIAN_POINT('Ctrl Pts',(-0.10122452635352,1.7938733127751,10.7495326277874));
#66933=CARTESIAN_POINT('Ctrl Pts',(-0.0917365454891338,1.79089751362767,
10.7502046010085));
#66934=CARTESIAN_POINT('Ctrl Pts',(-0.0792810318761317,1.78761505619139,
10.751076284176));
#66935=CARTESIAN_POINT('Ctrl Pts',(-0.0764253359104456,1.78690416281836,
10.7512754185548));
#66936=CARTESIAN_POINT('Ctrl Pts',(-0.0645557636823324,1.78412143610218,
10.7520994078017));
#66937=CARTESIAN_POINT('Ctrl Pts',(-0.0554640918823204,1.78239889135977,
10.7527218807366));
#66938=CARTESIAN_POINT('Ctrl Pts',(-0.0404041775757072,1.78021210346509,
10.7537277357974));
#66939=CARTESIAN_POINT('Ctrl Pts',(-0.0344747202440961,1.77951864414725,
10.7541173818149));
#66940=CARTESIAN_POINT('Ctrl Pts',(-0.0254375787758044,1.77871548758478,
10.7546983185686));
#66941=CARTESIAN_POINT('Ctrl Pts',(-0.0223421527856966,1.77848539956211,
10.7548950059402));
#66942=CARTESIAN_POINT('Ctrl Pts',(-0.0187344709486156,1.7782695918707,
10.755121197609));
#66943=CARTESIAN_POINT('Ctrl Pts',(-0.0182251175399177,1.77824033656169,
10.7551530620477));
#66944=CARTESIAN_POINT('Ctrl Pts',(-0.0174490977715468,1.77819761358838,
10.7552014989999));
#66945=CARTESIAN_POINT('Ctrl Pts',(-0.017182483583713,1.77818326772464,
10.7552181205703));
#66946=CARTESIAN_POINT('Ctrl Pts',(-0.0167192312684698,1.7781589185688,
10.7552469665411));
#66947=CARTESIAN_POINT('Ctrl Pts',(-0.0165226022818038,1.77814876416959,
10.7552591994507));
#66948=CARTESIAN_POINT('Ctrl Pts',(-0.0161101781189644,1.77812784452729,
10.7552848348399));
#66949=CARTESIAN_POINT('Ctrl Pts',(-0.015894382099532,1.77811711613384,
10.7552982351843));
#66950=CARTESIAN_POINT('Ctrl Pts',(-0.015291720758094,1.77808776209614,
10.7553356227266));
#66951=CARTESIAN_POINT('Ctrl Pts',(-0.0149048307575997,1.77806961674947,
10.7553595828572));
#66952=CARTESIAN_POINT('Ctrl Pts',(-0.0133463366482733,1.77799933805927,
10.7554559366748));
#66953=CARTESIAN_POINT('Ctrl Pts',(-0.0121744659209222,1.7779529017814,
10.755528014592));
#66954=CARTESIAN_POINT('Ctrl Pts',(0.00903217720685857,1.77722849271919,
10.756826039568));
#66955=CARTESIAN_POINT('Ctrl Pts',(0.0290903524390058,1.7784148001388,10.7579530513595));
#66956=CARTESIAN_POINT('Ctrl Pts',(0.0649687280313703,1.78392378279875,
10.7599840783063));
#66957=CARTESIAN_POINT('Ctrl Pts',(0.0808168358435746,1.78760006349287,
10.760886989693));
#66958=CARTESIAN_POINT('Ctrl Pts',(0.101692487984703,1.79413807960347,10.7621420781163));
#66959=CARTESIAN_POINT('Ctrl Pts',(0.107020254088062,1.79596129022122,10.7624682339063));
#66960=CARTESIAN_POINT('Ctrl Pts',(0.117375475337941,1.79981085195418,10.7631161872089));
#66961=CARTESIAN_POINT('Ctrl Pts',(0.122404960042232,1.80182631309415,10.7634375768791));
#66962=CARTESIAN_POINT('Ctrl Pts',(0.129253350831111,1.80477313558491,10.7638856613695));
#66963=CARTESIAN_POINT('Ctrl Pts',(0.131117928720049,1.80559650367018,10.7640087444872));
#66964=CARTESIAN_POINT('Ctrl Pts',(0.133874424361935,1.80684510907278,10.7641923755897));
#66965=CARTESIAN_POINT('Ctrl Pts',(0.134772422951401,1.80725686079639,10.7642524636148));
#66966=CARTESIAN_POINT('Ctrl Pts',(0.136199478095798,1.8079191542628,10.7643483820709));
#66967=CARTESIAN_POINT('Ctrl Pts',(0.13672977459112,1.80816702206007,10.7643841204526));
#66968=CARTESIAN_POINT('Ctrl Pts',(0.137736167825031,1.80864076917502,10.7644521264135));
#66969=CARTESIAN_POINT('Ctrl Pts',(0.138212392101161,1.80886637435961,10.7644843844402));
#66970=CARTESIAN_POINT('Ctrl Pts',(0.139041197517942,1.80926150225879,10.7645406616215));
#66971=CARTESIAN_POINT('Ctrl Pts',(0.139394028259233,1.80943050132624,10.7645646625604));
#66972=CARTESIAN_POINT('Ctrl Pts',(0.140078642529937,1.80975995218214,10.764611317028));
#66973=CARTESIAN_POINT('Ctrl Pts',(0.140410460431428,1.80992033154662,10.7646339680096));
#66974=CARTESIAN_POINT('Ctrl Pts',(0.141191584680361,1.81029953089555,10.7646873814043));
#66975=CARTESIAN_POINT('Ctrl Pts',(0.1416406576133,1.81051882705386,10.7647181603851));
#66976=CARTESIAN_POINT('Ctrl Pts',(0.143192286539123,1.81128101022069,10.764824755585));
#66977=CARTESIAN_POINT('Ctrl Pts',(0.144292235541167,1.81182915366252,10.7649007553378));
#66978=CARTESIAN_POINT('Ctrl Pts',(0.15783027375413,1.81867258041363,10.765841590102));
#66979=CARTESIAN_POINT('Ctrl Pts',(0.1698486129835,1.82576129681626,10.7667346747713));
#66980=CARTESIAN_POINT('Ctrl Pts',(0.197570455402011,1.84463508076959,10.7689403637104));
#66981=CARTESIAN_POINT('Ctrl Pts',(0.212730673774667,1.85711965645391,10.770273185989));
#66982=CARTESIAN_POINT('Ctrl Pts',(0.229498787228987,1.87370944920864,10.7718653456669));
#66983=CARTESIAN_POINT('Ctrl Pts',(0.232283817602781,1.87656916981761,10.772134070984));
#66984=CARTESIAN_POINT('Ctrl Pts',(0.243001812815436,1.88799166851324,10.7731833122818));
#66985=CARTESIAN_POINT('Ctrl Pts',(0.250521232929412,1.89693205973604,10.7739531628135));
#66986=CARTESIAN_POINT('Ctrl Pts',(0.258492362605685,1.90752822086026,10.774792203657));
#66987=CARTESIAN_POINT('Ctrl Pts',(0.259435760607198,1.90880174254579,10.7748918997785));
#66988=CARTESIAN_POINT('Ctrl Pts',(0.260614658193905,1.91041796425722,10.7750169309105));
#66989=CARTESIAN_POINT('Ctrl Pts',(0.260858920101935,1.91075420176454,10.7750428614043));
#66990=CARTESIAN_POINT('Ctrl Pts',(0.26124694007584,1.91129050734682,10.7750840911573));
#66991=CARTESIAN_POINT('Ctrl Pts',(0.261391119279807,1.91149026794609,10.7750994196049));
#66992=CARTESIAN_POINT('Ctrl Pts',(0.261663041772791,1.91186792893938,10.7751283447513));
#66993=CARTESIAN_POINT('Ctrl Pts',(0.261790831721598,1.91204579276277,10.7751419446351));
#66994=CARTESIAN_POINT('Ctrl Pts',(0.26208152337631,1.91245126214818,10.7751728961832));
#66995=CARTESIAN_POINT('Ctrl Pts',(0.262244309660165,1.91267894934807,10.7751902397797));
#66996=CARTESIAN_POINT('Ctrl Pts',(0.262739426309118,1.91337337335538,10.7752430246139));
#66997=CARTESIAN_POINT('Ctrl Pts',(0.263070811067957,1.91384078780257,10.7752784007617));
#66998=CARTESIAN_POINT('Ctrl Pts',(0.265443659316382,1.91720665248914,10.7755320661917));
#66999=CARTESIAN_POINT('Ctrl Pts',(0.267438519436596,1.92013787222983,10.7757472375644));
#67000=CARTESIAN_POINT('Ctrl Pts',(0.284868547498301,1.9466806888883,10.7776505903795));
#67001=CARTESIAN_POINT('Ctrl Pts',(0.297191888038881,1.9721940208487,10.7791735754917));
#67002=CARTESIAN_POINT('Ctrl Pts',(0.311383905834111,2.01519216786424,10.781730448985));
#67003=CARTESIAN_POINT('Ctrl Pts',(0.315435945604865,2.03179184338841,10.7827136778393));
#67004=CARTESIAN_POINT('Ctrl Pts',(0.318427311624856,2.05031960030041,10.7838448242673));
#67005=CARTESIAN_POINT('Ctrl Pts',(0.318686220057063,2.05200846036615,10.7839482138366));
#67006=CARTESIAN_POINT('Ctrl Pts',(0.319056336079188,2.05455791775516,10.7841047438543));
#67007=CARTESIAN_POINT('Ctrl Pts',(0.319177520085052,2.05541705392875,10.784157570415));
#67008=CARTESIAN_POINT('Ctrl Pts',(0.319367864126841,2.05680706549928,10.7842431691628));
#67009=CARTESIAN_POINT('Ctrl Pts',(0.319439173841702,2.0573376461311,10.7842758735413));
#67010=CARTESIAN_POINT('Ctrl Pts',(0.319573262441995,2.05835452029766,10.7843386119768));
#67011=CARTESIAN_POINT('Ctrl Pts',(0.319636254253694,2.05884078462938,10.7843686392312));
#67012=CARTESIAN_POINT('Ctrl Pts',(0.319746816419192,2.05970982999606,10.7844223507599));
#67013=CARTESIAN_POINT('Ctrl Pts',(0.319794809844953,2.06009255704398,10.7844460216299));
#67014=CARTESIAN_POINT('Ctrl Pts',(0.319888703606981,2.06085236625626,10.7844930470443));
#67015=CARTESIAN_POINT('Ctrl Pts',(0.319934624587577,2.0612294453074,10.7845164008981));
#67016=CARTESIAN_POINT('Ctrl Pts',(0.32004448721629,2.06214506709988,10.7845731479283));
#67017=CARTESIAN_POINT('Ctrl Pts',(0.320107736194813,2.06268369036332,10.7846065629006));
#67018=CARTESIAN_POINT('Ctrl Pts',(0.320339488150029,2.06470122478588,10.7847318514268));
#67019=CARTESIAN_POINT('Ctrl Pts',(0.320499102103547,2.06618112019379,10.7848240046562));
#67020=CARTESIAN_POINT('Ctrl Pts',(0.323161621160324,2.09258145131041,10.7864725971496));
#67021=CARTESIAN_POINT('Ctrl Pts',(0.322760823560495,2.11770335857479,10.7881253734787));
#67022=CARTESIAN_POINT('Ctrl Pts',(0.317370000806845,2.1582051174682,10.7908846012924));
#67023=CARTESIAN_POINT('Ctrl Pts',(0.314129935263931,2.1737154431584,10.7919619721888));
#67024=CARTESIAN_POINT('Ctrl Pts',(0.308007233188501,2.19504332688944,10.7934305446403));
#67025=CARTESIAN_POINT('Ctrl Pts',(0.306069928919368,2.20110835592257,10.7938464622694));
#67026=CARTESIAN_POINT('Ctrl Pts',(0.302944530816949,2.20997733351943,10.7944482968885));
#67027=CARTESIAN_POINT('Ctrl Pts',(0.301894443458182,2.21282796327431,10.7946407403734));
#67028=CARTESIAN_POINT('Ctrl Pts',(0.300622092144337,2.21613694802083,10.7948626076759));
#67029=CARTESIAN_POINT('Ctrl Pts',(0.30043890366985,2.21661002594482,10.7948942910111));
#67030=CARTESIAN_POINT('Ctrl Pts',(0.300157818160025,2.21733086032883,10.7949425093532));
#67031=CARTESIAN_POINT('Ctrl Pts',(0.300060730798659,2.21757892847742,10.7949590927445));
#67032=CARTESIAN_POINT('Ctrl Pts',(0.299891372668915,2.21801007993265,10.7949878966836));
#67033=CARTESIAN_POINT('Ctrl Pts',(0.299819241944028,2.21819321692788,10.7950001256592));
#67034=CARTESIAN_POINT('Ctrl Pts',(0.299655806368628,2.21860706090262,10.7950277468018));
#67035=CARTESIAN_POINT('Ctrl Pts',(0.299564403033707,2.21883772811042,10.7950431328937));
#67036=CARTESIAN_POINT('Ctrl Pts',(0.299316277833658,2.21946179629435,10.7950847352356));
#67037=CARTESIAN_POINT('Ctrl Pts',(0.299159046126975,2.21985499603826,10.7951109206773));
#67038=CARTESIAN_POINT('Ctrl Pts',(0.298451903872994,2.22161333269684,10.7952279047314));
#67039=CARTESIAN_POINT('Ctrl Pts',(0.297893409748926,2.22297503094965,10.7953181927988));
#67040=CARTESIAN_POINT('Ctrl Pts',(0.285909481187194,2.25163300556032,10.7972128404567));
#67041=CARTESIAN_POINT('Ctrl Pts',(0.270785710903568,2.27723590320793,10.7988084950194));
#67042=CARTESIAN_POINT('Ctrl Pts',(0.24122658197557,2.31445832677159,10.8014868305058));
#67043=CARTESIAN_POINT('Ctrl Pts',(0.228925952603847,2.32754211943909,10.8025169019109));
#67044=CARTESIAN_POINT('Ctrl Pts',(0.214298546585514,2.34070809314253,10.8037025636924));
#67045=CARTESIAN_POINT('Ctrl Pts',(0.212985107102912,2.34187103410509,10.8038086875691));
#67046=CARTESIAN_POINT('Ctrl Pts',(0.210995186752885,2.34360416524386,10.8039689954851));
#67047=CARTESIAN_POINT('Ctrl Pts',(0.2103257315894,2.34418240060269,10.8040228470717));
#67048=CARTESIAN_POINT('Ctrl Pts',(0.20924193374412,2.34511075668446,10.8041099048132));
#67049=CARTESIAN_POINT('Ctrl Pts',(0.208829069788589,2.34546260302739,10.8041430399556));
#67050=CARTESIAN_POINT('Ctrl Pts',(0.208037002557996,2.34613416504979,10.8042065548076));
#67051=CARTESIAN_POINT('Ctrl Pts',(0.20765794534745,2.34645405123024,10.8042369274126));
#67052=CARTESIAN_POINT('Ctrl Pts',(0.206982296850754,2.34702156525532,10.8042910238912));
#67053=CARTESIAN_POINT('Ctrl Pts',(0.206685995220396,2.34726953772846,10.8043147336184));
#67054=CARTESIAN_POINT('Ctrl Pts',(0.206098948599138,2.34775903995795,10.8043616812232));
#67055=CARTESIAN_POINT('Ctrl Pts',(0.205808223139834,2.34800059229907,10.8043849181289));
#67056=CARTESIAN_POINT('Ctrl Pts',(0.205104635561037,2.34858308629771,10.8044411226769));
#67057=CARTESIAN_POINT('Ctrl Pts',(0.204691348444434,2.34892351071844,10.804474111242));
#67058=CARTESIAN_POINT('Ctrl Pts',(0.203160106725728,2.35017840181598,10.8045962407549));
#67059=CARTESIAN_POINT('Ctrl Pts',(0.202036869694835,2.35108636935311,10.8046856436219));
#67060=CARTESIAN_POINT('Ctrl Pts',(0.183212918503481,2.36609459736832,10.8061809839103));
#67061=CARTESIAN_POINT('Ctrl Pts',(0.164085273225239,2.37829651302239,10.8076644148569));
#67062=CARTESIAN_POINT('Ctrl Pts',(0.13053103940573,2.39503232310662,10.8101881365517));
#67063=CARTESIAN_POINT('Ctrl Pts',(0.116776874677528,2.40074172530887,10.8112014203117));
#67064=CARTESIAN_POINT('Ctrl Pts',(0.0943347948087751,2.40828491315693,
10.8127862245283));
#67065=CARTESIAN_POINT('Ctrl Pts',(0.0858799204869176,2.41074636828859,
10.8133683030458));
#67066=CARTESIAN_POINT('Ctrl Pts',(0.0734880712214339,2.41380945811665,
10.8141904316879));
#67067=CARTESIAN_POINT('Ctrl Pts',(0.0696244618758618,2.41468922841304,
10.8144424608387));
#67068=CARTESIAN_POINT('Ctrl Pts',(0.065215004831091,2.41560809923774,10.8147244750418));
#67069=CARTESIAN_POINT('Ctrl Pts',(0.0646843278196683,2.41571728952382,
10.8147583232459));
#67070=CARTESIAN_POINT('Ctrl Pts',(0.0638852701128547,2.41587960164093,
10.8148091483914));
#67071=CARTESIAN_POINT('Ctrl Pts',(0.0636170963927311,2.41593372013465,
10.8148261820332));
#67072=CARTESIAN_POINT('Ctrl Pts',(0.0631366636616038,2.41603003680119,
10.814856654556));
#67073=CARTESIAN_POINT('Ctrl Pts',(0.0629244314745457,2.41607236257451,
10.8148701007417));
#67074=CARTESIAN_POINT('Ctrl Pts',(0.0624672025695226,2.41616306961944,
10.8148990363215));
#67075=CARTESIAN_POINT('Ctrl Pts',(0.0622221929196218,2.41621137977204,
10.8149145215638));
#67076=CARTESIAN_POINT('Ctrl Pts',(0.0615650924013758,2.41634015128421,
10.8149559986977));
#67077=CARTESIAN_POINT('Ctrl Pts',(0.0611528982619297,2.4164200925286,10.8149819607921));
#67078=CARTESIAN_POINT('Ctrl Pts',(0.0592829254556997,2.41677896597784,
10.8150994913233));
#67079=CARTESIAN_POINT('Ctrl Pts',(0.0578233566397278,2.41704863690329,
10.8151905390028));
#67080=CARTESIAN_POINT('Ctrl Pts',(0.0265580188201806,2.42260214956994,
10.8171271643803));
#67081=CARTESIAN_POINT('Ctrl Pts',(-0.00384872525162251,2.4236716980109,
10.8187548963342));
#67082=CARTESIAN_POINT('Ctrl Pts',(-0.0530840573723664,2.41845409433168,
10.8215490266969));
#67083=CARTESIAN_POINT('Ctrl Pts',(-0.0719831599756393,2.41472080240122,
10.822659071048));
#67084=CARTESIAN_POINT('Ctrl Pts',(-0.091524759306847,2.40900757677434,
10.8238972788867));
#67085=CARTESIAN_POINT('Ctrl Pts',(-0.0926125469361866,2.40868330076067,
10.8239664970896));
#67086=CARTESIAN_POINT('Ctrl Pts',(-0.0941994387379478,2.40820109568343,
10.8240679109315));
#67087=CARTESIAN_POINT('Ctrl Pts',(-0.094699915616857,2.40804768399724,
10.8240999586601));
#67088=CARTESIAN_POINT('Ctrl Pts',(-0.0955784662769301,2.40777603761185,
10.8241563288398));
#67089=CARTESIAN_POINT('Ctrl Pts',(-0.09595670094703,2.40765832360753,10.824180634172));
#67090=CARTESIAN_POINT('Ctrl Pts',(-0.0966913457913917,2.40742820127332,
10.8242279142929));
#67091=CARTESIAN_POINT('Ctrl Pts',(-0.0970477795345313,2.4073158697085,
10.8242508865286));
#67092=CARTESIAN_POINT('Ctrl Pts',(-0.0979975577110319,2.40701472605729,
10.8243121882635));
#67093=CARTESIAN_POINT('Ctrl Pts',(-0.0985905494928701,2.40682481463428,
10.8243505538678));
#67094=CARTESIAN_POINT('Ctrl Pts',(-0.100714310377563,2.40613786700255,
10.8244882904055));
#67095=CARTESIAN_POINT('Ctrl Pts',(-0.102241882122486,2.40563109023276,
10.8245879818237));
#67096=CARTESIAN_POINT('Ctrl Pts',(-0.127946706426711,2.39688915963633,
10.8262761910808));
#67097=CARTESIAN_POINT('Ctrl Pts',(-0.151059162560088,2.38582184079047,
10.8279651261308));
#67098=CARTESIAN_POINT('Ctrl Pts',(-0.184131832636683,2.36484433623847,
10.8306116114405));
#67099=CARTESIAN_POINT('Ctrl Pts',(-0.195170152865896,2.35681838654928,
10.8315382837865));
#67100=CARTESIAN_POINT('Ctrl Pts',(-0.210789316526204,2.34387148828902,
10.8328885251643));
#67101=CARTESIAN_POINT('Ctrl Pts',(-0.215779104269205,2.33946780280964,
10.8333263034291));
#67102=CARTESIAN_POINT('Ctrl Pts',(-0.223697172863672,2.332031171653,10.8340270430967));
#67103=CARTESIAN_POINT('Ctrl Pts',(-0.226708509838199,2.32908981985936,
10.8342950598146));
#67104=CARTESIAN_POINT('Ctrl Pts',(-0.230046852423466,2.32569874386905,
10.8345930303718));
#67105=CARTESIAN_POINT('Ctrl Pts',(-0.230431173545317,2.32530635047225,
10.834627346729));
#67106=CARTESIAN_POINT('Ctrl Pts',(-0.23100648633209,2.3247159419805,10.8346787337311));
#67107=CARTESIAN_POINT('Ctrl Pts',(-0.231198228158653,2.32451866426945,
10.8346958629541));
#67108=CARTESIAN_POINT('Ctrl Pts',(-0.23152743898233,2.3241790796921,10.8347252774116));
#67109=CARTESIAN_POINT('Ctrl Pts',(-0.231665029448718,2.32403689183852,
10.8347375722316));
#67110=CARTESIAN_POINT('Ctrl Pts',(-0.231949932871431,2.32374192568121,
10.8347630333303));
#67111=CARTESIAN_POINT('Ctrl Pts',(-0.232097225443932,2.32358912900327,
10.834776198015));
#67112=CARTESIAN_POINT('Ctrl Pts',(-0.232499656477737,2.32317083354989,
10.8348121709493));
#67113=CARTESIAN_POINT('Ctrl Pts',(-0.232754492031633,2.3229050417822,10.8348349554606));
#67114=CARTESIAN_POINT('Ctrl Pts',(-0.23372454376118,2.3218898070262,10.8349217083476));
#67115=CARTESIAN_POINT('Ctrl Pts',(-0.23443661033113,2.32113734334974,10.8349854347236));
#67116=CARTESIAN_POINT('Ctrl Pts',(-0.247795835104529,2.30688316912171,
10.8361821808254));
#67117=CARTESIAN_POINT('Ctrl Pts',(-0.259262987732564,2.29231833894362,
10.8372301352378));
#67118=CARTESIAN_POINT('Ctrl Pts',(-0.278643658436492,2.26279292648151,
10.8392101534994));
#67119=CARTESIAN_POINT('Ctrl Pts',(-0.286755077178749,2.24803827813328,
10.8401414151025));
#67120=CARTESIAN_POINT('Ctrl Pts',(-0.299756742200531,2.21926828385461,
10.8419457599582));
#67121=CARTESIAN_POINT('Ctrl Pts',(-0.304903156312032,2.20541823329652,
10.8428097187293));
#67122=CARTESIAN_POINT('Ctrl Pts',(-0.309394616577889,2.19020734037224,
10.8437745034147));
#67123=CARTESIAN_POINT('Ctrl Pts',(-0.309701638749541,2.18914756268587,
10.8438417966249));
#67124=CARTESIAN_POINT('Ctrl Pts',(-0.310144633697823,2.18758852399087,
10.8439409079549));
#67125=CARTESIAN_POINT('Ctrl Pts',(-0.310284858175825,2.18709047093874,
10.8439725876028));
#67126=CARTESIAN_POINT('Ctrl Pts',(-0.310530075467895,2.18621139170129,
10.8440285346253));
#67127=CARTESIAN_POINT('Ctrl Pts',(-0.310635568186558,2.18583050509191,
10.8440527856941));
#67128=CARTESIAN_POINT('Ctrl Pts',(-0.310839950692917,2.18508725969011,
10.8441001288166));
#67129=CARTESIAN_POINT('Ctrl Pts',(-0.310938908203602,2.18472492001555,
10.844123218628));
#67130=CARTESIAN_POINT('Ctrl Pts',(-0.311202776233992,2.18375206039317,
10.844185239422));
#67131=CARTESIAN_POINT('Ctrl Pts',(-0.311366522910841,2.18314122898511,
10.8442242080835));
#67132=CARTESIAN_POINT('Ctrl Pts',(-0.311956201487708,2.18091534947454,
10.8443663133828));
#67133=CARTESIAN_POINT('Ctrl Pts',(-0.312371368305348,2.17929750009675,
10.8444697977315));
#67134=CARTESIAN_POINT('Ctrl Pts',(-0.319109652835105,2.15216497995407,
10.8462087973236));
#67135=CARTESIAN_POINT('Ctrl Pts',(-0.322298967491384,2.12597977636967,
10.8479511623769));
#67136=CARTESIAN_POINT('Ctrl Pts',(-0.322261340588192,2.08496170084742,
10.8507246764572));
#67137=CARTESIAN_POINT('Ctrl Pts',(-0.321236218004765,2.07023679775949,
10.8517263176096));
#67138=CARTESIAN_POINT('Ctrl Pts',(-0.318013606332761,2.04705094368035,
10.8532730678785));
#67139=CARTESIAN_POINT('Ctrl Pts',(-0.316474955975911,2.03851918886136,
10.8538353008064));
#67140=CARTESIAN_POINT('Ctrl Pts',(-0.31444002312565,2.02936607487704,10.8544236901166));
#67141=CARTESIAN_POINT('Ctrl Pts',(-0.314283677364257,2.02867363960958,
10.8544681089694));
#67142=CARTESIAN_POINT('Ctrl Pts',(-0.314061830390749,2.02770600071265,
10.8545300462583));
#67143=CARTESIAN_POINT('Ctrl Pts',(-0.313998254241525,2.02743036464106,
10.8545476739591));
#67144=CARTESIAN_POINT('Ctrl Pts',(-0.313887691233006,2.02695388125218,
10.8545781193426));
#67145=CARTESIAN_POINT('Ctrl Pts',(-0.313840874447394,2.02675299529436,
10.8545909468267));
#67146=CARTESIAN_POINT('Ctrl Pts',(-0.313743037445857,2.02633500276789,
10.854617620023));
#67147=CARTESIAN_POINT('Ctrl Pts',(-0.313691984790493,2.0261179044596,10.8546314637561));
#67148=CARTESIAN_POINT('Ctrl Pts',(-0.313570175067326,2.02560231835343,
10.8546643180725));
#67149=CARTESIAN_POINT('Ctrl Pts',(-0.313499216860585,2.02530387723714,
10.854683317005));
#67150=CARTESIAN_POINT('Ctrl Pts',(-0.313261068712301,2.02430857365992,
10.8547466185388));
#67151=CARTESIAN_POINT('Ctrl Pts',(-0.313091978983786,2.02361216123397,
10.8547908122397));
#67152=CARTESIAN_POINT('Ctrl Pts',(-0.310092295551753,2.01143497243676,
10.8555619368634));
#67153=CARTESIAN_POINT('Ctrl Pts',(-0.306633895325478,2.00011645781304,
10.856253425238));
#67154=CARTESIAN_POINT('Ctrl Pts',(-0.292518746355445,1.96163749784622,
10.8585962757962));
#67155=CARTESIAN_POINT('Ctrl Pts',(-0.27880864834607,1.93575243663756,10.8601708704603));
#67156=CARTESIAN_POINT('Ctrl Pts',(-0.256261597751206,1.90434346911651,
10.8624234177236));
#67157=CARTESIAN_POINT('Ctrl Pts',(-0.250381539066271,1.8968730875613,10.8629877131863));
#67158=CARTESIAN_POINT('Ctrl Pts',(-0.243431566881132,1.88880443984327,
10.8636353048508));
#67159=CARTESIAN_POINT('Ctrl Pts',(-0.242678043332475,1.88793901911214,
10.8637052752765));
#67160=CARTESIAN_POINT('Ctrl Pts',(-0.241576291273093,1.88668722111408,
10.8638072395696));
#67161=CARTESIAN_POINT('Ctrl Pts',(-0.241231718005775,1.8862976266761,10.8638390808942));
#67162=CARTESIAN_POINT('Ctrl Pts',(-0.240622451104511,1.88561210555517,
10.8638952983856));
#67163=CARTESIAN_POINT('Ctrl Pts',(-0.240358150248578,1.88531582995742,
10.8639196580485));
#67164=CARTESIAN_POINT('Ctrl Pts',(-0.239811078399718,1.88470485072827,
10.863970023294));
#67165=CARTESIAN_POINT('Ctrl Pts',(-0.239528233964862,1.88439021415036,
10.8639960319446));
#67166=CARTESIAN_POINT('Ctrl Pts',(-0.238803526882096,1.88358723490584,
10.8640625932487));
#67167=CARTESIAN_POINT('Ctrl Pts',(-0.238360786972351,1.88309968978662,
10.8641031829652));
#67168=CARTESIAN_POINT('Ctrl Pts',(-0.23655494989471,1.88112330874004,10.8642684425734));
#67169=CARTESIAN_POINT('Ctrl Pts',(-0.235179396245872,1.87964596309556,
10.8643936420003));
#67170=CARTESIAN_POINT('Ctrl Pts',(-0.212496239219926,1.85573857485373,
10.8664474989823));
#67171=CARTESIAN_POINT('Ctrl Pts',(-0.188086092579508,1.83648340023354,
10.8685289412811));
#67172=CARTESIAN_POINT('Ctrl Pts',(-0.145843842433668,1.81205871572784,
10.8718279115494));
#67173=CARTESIAN_POINT('Ctrl Pts',(-0.129651809717556,1.80441382868556,
10.8730280100167));
#67174=CARTESIAN_POINT('Ctrl Pts',(-0.111895017570926,1.79777185905241,
10.8742223714685));
#67175=CARTESIAN_POINT('Ctrl Pts',(-0.110880635296253,1.79739823375761,
10.8742901895303));
#67176=CARTESIAN_POINT('Ctrl Pts',(-0.109512171682685,1.79690199565565,
10.8743811085517));
#67177=CARTESIAN_POINT('Ctrl Pts',(-0.109159743472639,1.79677489155321,
10.8744044725445));
#67178=CARTESIAN_POINT('Ctrl Pts',(-0.108606114174695,1.79657631407934,
10.8744410942665));
#67179=CARTESIAN_POINT('Ctrl Pts',(-0.108405063751985,1.79650442611567,
10.8744543767429));
#67180=CARTESIAN_POINT('Ctrl Pts',(-0.108017925339663,1.79636643395622,
10.8744799208599));
#67181=CARTESIAN_POINT('Ctrl Pts',(-0.107831849433781,1.79630030149659,
10.8744921841024));
#67182=CARTESIAN_POINT('Ctrl Pts',(-0.107389166940257,1.79614342770171,
10.8745213248039));
#67183=CARTESIAN_POINT('Ctrl Pts',(-0.107132506356514,1.79605284046718,
10.8745381929596));
#67184=CARTESIAN_POINT('Ctrl Pts',(-0.106371022967843,1.79578516258503,
10.874588159191));
#67185=CARTESIAN_POINT('Ctrl Pts',(-0.105865870471747,1.79560900258117,
10.874621201971));
#67186=CARTESIAN_POINT('Ctrl Pts',(-0.101813268529822,1.79420706210006,
10.8748854751099));
#67187=CARTESIAN_POINT('Ctrl Pts',(-0.0982449064654422,1.79304201614351,
10.8751131793803));
#67188=CARTESIAN_POINT('Ctrl Pts',(-0.0852828923600123,1.78905921700752,
10.8759251296168));
#67189=CARTESIAN_POINT('Ctrl Pts',(-0.0757815139115759,1.78660801116049,
10.8764918455314));
#67190=CARTESIAN_POINT('Ctrl Pts',(-0.0352192502788053,1.77809674492801,
10.8788479777394));
#67191=CARTESIAN_POINT('Ctrl Pts',(-0.00347017465484709,1.77619431317332,
10.8805571999396));
#67192=CARTESIAN_POINT('Ctrl Pts',(0.0288798137658721,1.77902051645085,
10.8824813382952));
#67193=CARTESIAN_POINT('Ctrl Pts',(0.0297111471255038,1.77909640042432,
10.8825308945931));
#67194=CARTESIAN_POINT('Ctrl Pts',(0.0355616695097354,1.77965336431316,
10.882880441744));
#67195=CARTESIAN_POINT('Ctrl Pts',(0.040569032653257,1.78024892712483,10.8831837450786));
#67196=CARTESIAN_POINT('Ctrl Pts',(0.0464111151192779,1.78108320378603,
10.8835431284651));
#67197=CARTESIAN_POINT('Ctrl Pts',(0.0472615724770881,1.78120812705068,
10.8835955825203));
#67198=CARTESIAN_POINT('Ctrl Pts',(0.0486211417301354,1.78141339349703,
10.8836796602766));
#67199=CARTESIAN_POINT('Ctrl Pts',(0.0491305823272808,1.78149155875938,
10.8837112149715));
#67200=CARTESIAN_POINT('Ctrl Pts',(0.0500313645639767,1.78163198149173,
10.8837670988584));
#67201=CARTESIAN_POINT('Ctrl Pts',(0.0504227839274482,1.78169373944612,
10.8837914121679));
#67202=CARTESIAN_POINT('Ctrl Pts',(0.0512337911253736,1.78182323322659,
10.8838418509587));
#67203=CARTESIAN_POINT('Ctrl Pts',(0.0516533606498985,1.78189107746202,
10.8838679798364));
#67204=CARTESIAN_POINT('Ctrl Pts',(0.0527313552383046,1.78206757773024,
10.8839352021998));
#67205=CARTESIAN_POINT('Ctrl Pts',(0.0533895768346469,1.782177448833,10.8839763341998));
#67206=CARTESIAN_POINT('Ctrl Pts',(0.0561081615480556,1.78263992175687,
10.8841465771644));
#67207=CARTESIAN_POINT('Ctrl Pts',(0.058165374948528,1.78301051455767,10.8842762587965));
#67208=CARTESIAN_POINT('Ctrl Pts',(0.0719027439351294,1.78562343530252,
10.8851481079116));
#67209=CARTESIAN_POINT('Ctrl Pts',(0.0834533185927601,1.78849058779111,
10.8859101941257));
#67210=CARTESIAN_POINT('Ctrl Pts',(0.128326777924193,1.80230441663914,10.888988199625));
#67211=CARTESIAN_POINT('Ctrl Pts',(0.159922118083132,1.8180161936087,10.8914480006426));
#67212=CARTESIAN_POINT('Ctrl Pts',(0.190235096140064,1.8398517811264,10.8938322911741));
#67213=CARTESIAN_POINT('Ctrl Pts',(0.192090755508233,1.84121895363696,10.8939782256543));
#67214=CARTESIAN_POINT('Ctrl Pts',(0.194489892606779,1.84302656588351,10.894166698071));
#67215=CARTESIAN_POINT('Ctrl Pts',(0.195046771873976,1.84344898953423,10.8942104311826));
#67216=CARTESIAN_POINT('Ctrl Pts',(0.195825597072403,1.8440437730517,10.8942715687392));
#67217=CARTESIAN_POINT('Ctrl Pts',(0.196048693471399,1.84421461266912,10.8942890787938));
#67218=CARTESIAN_POINT('Ctrl Pts',(0.196434784587293,1.84451106995502,10.8943193761975));
#67219=CARTESIAN_POINT('Ctrl Pts',(0.196597882464655,1.84463655198454,10.8943321731249));
#67220=CARTESIAN_POINT('Ctrl Pts',(0.196934062000048,1.84489571019799,10.8943585465853));
#67221=CARTESIAN_POINT('Ctrl Pts',(0.19710712760593,1.84502940620839,10.8943721215994));
#67222=CARTESIAN_POINT('Ctrl Pts',(0.197516812198245,1.84534656065699,10.8944042520772));
#67223=CARTESIAN_POINT('Ctrl Pts',(0.197753312654186,1.84553017348571,10.8944227965578));
#67224=CARTESIAN_POINT('Ctrl Pts',(0.198254369210672,1.84592030118297,10.8944620785442));
#67225=CARTESIAN_POINT('Ctrl Pts',(0.198518859564754,1.84612690047666,10.8944828100633));
#67226=CARTESIAN_POINT('Ctrl Pts',(0.199235655516072,1.84668861084085,10.8945389850039));
#67227=CARTESIAN_POINT('Ctrl Pts',(0.199687336793267,1.84704452201451,10.8945743726409));
#67228=CARTESIAN_POINT('Ctrl Pts',(0.212941385742961,1.85754593529842,10.8956125547702));
#67229=CARTESIAN_POINT('Ctrl Pts',(0.224956979001012,1.86865063590422,10.8965480141698));
#67230=CARTESIAN_POINT('Ctrl Pts',(0.253256335860199,1.89910428734379,10.8988893224661));
#67231=CARTESIAN_POINT('Ctrl Pts',(0.268201510462072,1.91954012300735,10.9002722466885));
#67232=CARTESIAN_POINT('Ctrl Pts',(0.281774268365464,1.94357097186685,10.9018853522377));
#67233=CARTESIAN_POINT('Ctrl Pts',(0.282915646310602,1.94564483865028,10.9020243886057));
#67234=CARTESIAN_POINT('Ctrl Pts',(0.287118611846333,1.95348481774788,10.9025496488998));
#67235=CARTESIAN_POINT('Ctrl Pts',(0.290027441447156,1.95933063614475,10.9029406451016));
#67236=CARTESIAN_POINT('Ctrl Pts',(0.29318905587905,1.96620006347498,10.9034008851928));
#67237=CARTESIAN_POINT('Ctrl Pts',(0.293616975175867,1.96714173962145,10.9034639914284));
#67238=CARTESIAN_POINT('Ctrl Pts',(0.294246618215615,1.96854522741762,10.903558074788));
#67239=CARTESIAN_POINT('Ctrl Pts',(0.294451806911116,1.9690054849689,10.9035889329338));
#67240=CARTESIAN_POINT('Ctrl Pts',(0.294815262256672,1.96982591832359,10.903643948146));
#67241=CARTESIAN_POINT('Ctrl Pts',(0.2949739508228,1.97018590703018,10.9036680907075));
#67242=CARTESIAN_POINT('Ctrl Pts',(0.295306543653845,1.97094416031045,10.9037189496296));
#67243=CARTESIAN_POINT('Ctrl Pts',(0.295480302190845,1.97134248759977,10.9037456709116));
#67244=CARTESIAN_POINT('Ctrl Pts',(0.295935884318789,1.97239266349623,10.9038161317182));
#67245=CARTESIAN_POINT('Ctrl Pts',(0.296216358738336,1.97304509162687,10.9038599171535));
#67246=CARTESIAN_POINT('Ctrl Pts',(0.297464574525642,1.97597529552459,10.9040566224848));
#67247=CARTESIAN_POINT('Ctrl Pts',(0.298408194869985,1.97826319741798,10.9042103593725));
#67248=CARTESIAN_POINT('Ctrl Pts',(0.305145194551675,1.99514684885435,10.9053462226367));
#67249=CARTESIAN_POINT('Ctrl Pts',(0.309890359206995,2.01013561618187,10.9063635876285));
#67250=CARTESIAN_POINT('Ctrl Pts',(0.319342784572609,2.04986621749384,10.9090776630549));
#67251=CARTESIAN_POINT('Ctrl Pts',(0.322279455761842,2.07491881408578,10.9108109894218));
#67252=CARTESIAN_POINT('Ctrl Pts',(0.322273592482529,2.10796044840965,10.9129869508134));
#67253=CARTESIAN_POINT('Ctrl Pts',(0.321981467241188,2.11586179408585,10.9134982412682));
#67254=CARTESIAN_POINT('Ctrl Pts',(0.321347810561823,2.12443857123039,10.9140378168913));
#67255=CARTESIAN_POINT('Ctrl Pts',(0.321294333757685,2.12513185693778,10.91408132207));
#67256=CARTESIAN_POINT('Ctrl Pts',(0.321216146366285,2.12610443531726,10.9141421935344));
#67257=CARTESIAN_POINT('Ctrl Pts',(0.321193314990505,2.12638387076451,10.9141596642279));
#67258=CARTESIAN_POINT('Ctrl Pts',(0.321153106963466,2.12686819295285,10.9141899121766));
#67259=CARTESIAN_POINT('Ctrl Pts',(0.321135898874397,2.12707309290631,10.9142026989355));
#67260=CARTESIAN_POINT('Ctrl Pts',(0.321099968102112,2.12749607278979,10.9142290738959));
#67261=CARTESIAN_POINT('Ctrl Pts',(0.321081219364787,2.12771414991567,10.9142426605403));
#67262=CARTESIAN_POINT('Ctrl Pts',(0.321036260027539,2.12823092774375,10.9142748297268));
#67263=CARTESIAN_POINT('Ctrl Pts',(0.321009854612441,2.12852961228594,10.9142934012386));
#67264=CARTESIAN_POINT('Ctrl Pts',(0.320952934379791,2.12916338027077,10.9143327627248));
#67265=CARTESIAN_POINT('Ctrl Pts',(0.320922311548323,2.12949845400558,10.9143535466324));
#67266=CARTESIAN_POINT('Ctrl Pts',(0.320837736757134,2.13040814681732,10.9144099023265));
#67267=CARTESIAN_POINT('Ctrl Pts',(0.320782765574531,2.13098267326406,10.9144454178637));
#67268=CARTESIAN_POINT('Ctrl Pts',(0.320606908573613,2.13276997433638,10.91455567401));
#67269=CARTESIAN_POINT('Ctrl Pts',(0.320480684622271,2.13398222968042,10.9146301273247));
#67270=CARTESIAN_POINT('Ctrl Pts',(0.319454339014239,2.14332443472775,10.9152015612954));
#67271=CARTESIAN_POINT('Ctrl Pts',(0.318251788945937,2.15141891176627,10.9156830338338));
#67272=CARTESIAN_POINT('Ctrl Pts',(0.313730137988612,2.17550585337633,10.9170979416891));
#67273=CARTESIAN_POINT('Ctrl Pts',(0.309502699192559,2.19130102853537,10.9180028538564));
#67274=CARTESIAN_POINT('Ctrl Pts',(0.299047824853666,2.22109514109726,10.9197697354791));
#67275=CARTESIAN_POINT('Ctrl Pts',(0.292985262477462,2.23510446761896,10.9206284530444));
#67276=CARTESIAN_POINT('Ctrl Pts',(0.281663860477681,2.25688592850269,10.9220598444195));
#67277=CARTESIAN_POINT('Ctrl Pts',(0.27701823389186,2.26495028832841,10.9226125870655));
#67278=CARTESIAN_POINT('Ctrl Pts',(0.271418718418372,2.27376523640135,10.923247673354));
#67279=CARTESIAN_POINT('Ctrl Pts',(0.270801677535746,2.27472529719778,10.9233172650414));
#67280=CARTESIAN_POINT('Ctrl Pts',(0.26989665885054,2.27611711580354,10.9234187781613));
#67281=CARTESIAN_POINT('Ctrl Pts',(0.269612712191117,2.27655149491753,10.9234505489591));
#67282=CARTESIAN_POINT('Ctrl Pts',(0.269109784217348,2.27731682702414,10.9235066841963));
#67283=CARTESIAN_POINT('Ctrl Pts',(0.268891237945403,2.27764806574058,10.923531032285));
#67284=CARTESIAN_POINT('Ctrl Pts',(0.268438173528964,2.27833199940078,10.9235814147865));
#67285=CARTESIAN_POINT('Ctrl Pts',(0.268203570893212,2.27868463721106,10.9236074523469));
#67286=CARTESIAN_POINT('Ctrl Pts',(0.267601237897133,2.27958616206266,10.923674172798));
#67287=CARTESIAN_POINT('Ctrl Pts',(0.267232514896873,2.28013438067171,10.9237148930991));
#67288=CARTESIAN_POINT('Ctrl Pts',(0.265720830930905,2.28236710105095,10.9238813405545));
#67289=CARTESIAN_POINT('Ctrl Pts',(0.264563627137085,2.28404186052861,10.9240076068985));
#67290=CARTESIAN_POINT('Ctrl Pts',(0.256825522724552,2.29501700255983,10.924844591866));
#67291=CARTESIAN_POINT('Ctrl Pts',(0.249771992862943,2.30397274367543,10.9255735559959));
#67292=CARTESIAN_POINT('Ctrl Pts',(0.239105141218199,2.31613141821105,10.9266317562559));
#67293=CARTESIAN_POINT('Ctrl Pts',(0.235870867762312,2.31965652538539,10.9269473918592));
#67294=CARTESIAN_POINT('Ctrl Pts',(0.21283791635488,2.34366518889734,10.9291580803373));
#67295=CARTESIAN_POINT('Ctrl Pts',(0.190479444856319,2.36151517768232,10.9311336135066));
#67296=CARTESIAN_POINT('Ctrl Pts',(0.165772275101214,2.37637084979726,10.9330007166504));
#67297=CARTESIAN_POINT('Ctrl Pts',(0.165477366585806,2.37654752748797,10.9330229590571));
#67298=CARTESIAN_POINT('Ctrl Pts',(0.16465254870239,2.37703987850495,10.9330850450253));
#67299=CARTESIAN_POINT('Ctrl Pts',(0.164122012053392,2.37735450464635,10.9331248382677));
#67300=CARTESIAN_POINT('Ctrl Pts',(0.160271490278829,2.37962307699123,10.9334126080442));
#67301=CARTESIAN_POINT('Ctrl Pts',(0.156917427912352,2.3815189866872,10.933657681958));
#67302=CARTESIAN_POINT('Ctrl Pts',(0.153013637944836,2.38363417835583,10.9339358398401));
#67303=CARTESIAN_POINT('Ctrl Pts',(0.152496509678359,2.38391254829179,10.9339725454677));
#67304=CARTESIAN_POINT('Ctrl Pts',(0.151731962159788,2.38432141235384,10.9340266010447));
#67305=CARTESIAN_POINT('Ctrl Pts',(0.151485133033698,2.38445299846359,10.9340440200348));
#67306=CARTESIAN_POINT('Ctrl Pts',(0.15105061491398,2.38468391674351,10.9340746268837));
#67307=CARTESIAN_POINT('Ctrl Pts',(0.150862998977748,2.38478338480114,10.934087823434));
#67308=CARTESIAN_POINT('Ctrl Pts',(0.150466061533849,2.3849933261858,10.9341157032804));
#67309=CARTESIAN_POINT('Ctrl Pts',(0.150256717099342,2.38510375411654,10.9341303836514));
#67310=CARTESIAN_POINT('Ctrl Pts',(0.149710045158083,2.38539135092291,10.9341686586376));
#67311=CARTESIAN_POINT('Ctrl Pts',(0.149372523518038,2.38556815302874,10.9341922298953));
#67312=CARTESIAN_POINT('Ctrl Pts',(0.148633746319999,2.38595347447336,10.9342436936415));
#67313=CARTESIAN_POINT('Ctrl Pts',(0.148232363050393,2.38616174911893,10.9342715708207));
#67314=CARTESIAN_POINT('Ctrl Pts',(0.147054897629151,2.3867695846028,10.9343531086353));
#67315=CARTESIAN_POINT('Ctrl Pts',(0.146277621545877,2.38716684182743,10.934406628531));
#67316=CARTESIAN_POINT('Ctrl Pts',(0.143590535186885,2.388526441128,10.9345906314389));
#67317=CARTESIAN_POINT('Ctrl Pts',(0.141672719740869,2.38947295219074,10.9347201892511));
#67318=CARTESIAN_POINT('Ctrl Pts',(0.133607087817728,2.39335427117415,10.935258287291));
#67319=CARTESIAN_POINT('Ctrl Pts',(0.127376041355683,2.39611305215611,10.935657659415));
#67320=CARTESIAN_POINT('Ctrl Pts',(0.105820504938987,2.4048502236292,10.9369995364899));
#67321=CARTESIAN_POINT('Ctrl Pts',(0.0901277915379695,2.40985268145701,
10.9379105683123));
#67322=CARTESIAN_POINT('Ctrl Pts',(0.0585939231336889,2.41730503161373,
10.939724164058));
#67323=CARTESIAN_POINT('Ctrl Pts',(0.0428168215292512,2.41981617630719,
10.9406238840494));
#67324=CARTESIAN_POINT('Ctrl Pts',(0.0250778754289856,2.42130311589696,
10.9416660801061));
#67325=CARTESIAN_POINT('Ctrl Pts',(0.0232346903394261,2.42144166048897,
10.9417747160147));
#67326=CARTESIAN_POINT('Ctrl Pts',(0.0147657889760138,2.42200501129435,
10.9422756274501));
#67327=CARTESIAN_POINT('Ctrl Pts',(0.00812950234340606,2.4222408375359,
10.9426731362181));
#67328=CARTESIAN_POINT('Ctrl Pts',(0.000451560457815039,2.42227635996316,
10.9431404158847));
#67329=CARTESIAN_POINT('Ctrl Pts',(-0.000587893916345153,2.42227614003989,
10.9432038322062));
#67330=CARTESIAN_POINT('Ctrl Pts',(-0.00213225426868554,2.42226834173135,
10.9432982888775));
#67331=CARTESIAN_POINT('Ctrl Pts',(-0.0026371799767455,2.42226460535982,
10.9433292088539));
#67332=CARTESIAN_POINT('Ctrl Pts',(-0.00353561351639392,2.42225584546371,
10.9433842935171));
#67333=CARTESIAN_POINT('Ctrl Pts',(-0.00392912572336737,2.42225128776676,
10.9434084435639));
#67334=CARTESIAN_POINT('Ctrl Pts',(-0.0047566259865352,2.42224018762881,
10.9434592765997));
#67335=CARTESIAN_POINT('Ctrl Pts',(-0.00519061085343672,2.42223348921219,
10.9434859644275));
#67336=CARTESIAN_POINT('Ctrl Pts',(-0.0063322228811744,2.42221356192837,
10.9435562427709));
#67337=CARTESIAN_POINT('Ctrl Pts',(-0.00703981941321461,2.42219887874889,
10.9435998787676));
#67338=CARTESIAN_POINT('Ctrl Pts',(-0.0101982263588391,2.42212293000704,
10.9437949945642));
#67339=CARTESIAN_POINT('Ctrl Pts',(-0.012648286661351,2.4220360324057,10.9439472752221));
#67340=CARTESIAN_POINT('Ctrl Pts',(-0.0305337345986822,2.42119726268091,
10.9450659315417));
#67341=CARTESIAN_POINT('Ctrl Pts',(-0.0458959992238623,2.41936409121903,
10.946066397893));
#67342=CARTESIAN_POINT('Ctrl Pts',(-0.0645551773513158,2.41576325716946,
10.9473283150609));
#67343=CARTESIAN_POINT('Ctrl Pts',(-0.0680331992839133,2.41503220198344,
10.9475654933345));
#67344=CARTESIAN_POINT('Ctrl Pts',(-0.074307969169397,2.41360453432287,
10.9479966685379));
#67345=CARTESIAN_POINT('Ctrl Pts',(-0.0771088526425831,2.41292763168831,
10.9481903264274));
#67346=CARTESIAN_POINT('Ctrl Pts',(-0.08225352289581,2.41161103027343,10.9485480461931));
#67347=CARTESIAN_POINT('Ctrl Pts',(-0.0845998964871797,2.41098220780366,
10.9487119712565));
#67348=CARTESIAN_POINT('Ctrl Pts',(-0.088958974454173,2.40976100041126,
10.9490178211939));
#67349=CARTESIAN_POINT('Ctrl Pts',(-0.0909734478491825,2.40917536810437,
10.9491596906761));
#67350=CARTESIAN_POINT('Ctrl Pts',(-0.0947473084584657,2.40803818308583,
10.9494263536089));
#67351=CARTESIAN_POINT('Ctrl Pts',(-0.0965079658691028,2.40749111729511,
10.9495511287727));
#67352=CARTESIAN_POINT('Ctrl Pts',(-0.116662664991957,2.40103855624245,
10.9509832100453));
#67353=CARTESIAN_POINT('Ctrl Pts',(-0.134496813281154,2.39350497703906,
10.9522889214736));
#67354=CARTESIAN_POINT('Ctrl Pts',(-0.152971177015249,2.38366104242875,
10.9536141979254));
#67355=CARTESIAN_POINT('Ctrl Pts',(-0.154386468234403,2.38289324253364,
10.9537155263969));
#67356=CARTESIAN_POINT('Ctrl Pts',(-0.156175044295363,2.38190551373694,
10.9538432696754));
#67357=CARTESIAN_POINT('Ctrl Pts',(-0.156553688728325,2.38169541296712,
10.9538702953475));
#67358=CARTESIAN_POINT('Ctrl Pts',(-0.157152711796571,2.38136144850785,
10.9539130208945));
#67359=CARTESIAN_POINT('Ctrl Pts',(-0.157373368413679,2.38123808854179,
10.9539287529331));
#67360=CARTESIAN_POINT('Ctrl Pts',(-0.157783734795642,2.38100803552845,
10.9539579984019));
#67361=CARTESIAN_POINT('Ctrl Pts',(-0.157973480259551,2.38090141069915,
10.953971516037));
#67362=CARTESIAN_POINT('Ctrl Pts',(-0.158393747014589,2.38066468712013,
10.9540014454602));
#67363=CARTESIAN_POINT('Ctrl Pts',(-0.158624215498863,2.38053449689501,
10.9540178512001));
#67364=CARTESIAN_POINT('Ctrl Pts',(-0.159294454143511,2.38015479320819,
10.9540655416513));
#67365=CARTESIAN_POINT('Ctrl Pts',(-0.159733800374228,2.37990452712422,
10.9540967779604));
#67366=CARTESIAN_POINT('Ctrl Pts',(-0.160728233209435,2.37933496154287,
10.9541674266003));
#67367=CARTESIAN_POINT('Ctrl Pts',(-0.161282962752072,2.37901503836335,
10.9542067994757));
#67368=CARTESIAN_POINT('Ctrl Pts',(-0.163050744685599,2.37798849089676,
10.9543321632354));
#67369=CARTESIAN_POINT('Ctrl Pts',(-0.164260154428481,2.37727558176294,
10.9544177673243));
#67370=CARTESIAN_POINT('Ctrl Pts',(-0.16898370950396,2.37444944173226,10.9547516262125));
#67371=CARTESIAN_POINT('Ctrl Pts',(-0.172462205319981,2.37227703041422,
10.954996432063));
#67372=CARTESIAN_POINT('Ctrl Pts',(-0.181939370062623,2.36610377217654,
10.9556631878612));
#67373=CARTESIAN_POINT('Ctrl Pts',(-0.187846909062409,2.36196698860046,
10.9560785793407));
#67374=CARTESIAN_POINT('Ctrl Pts',(-0.219072103021601,2.33850148411132,
10.9583009966784));
#67375=CARTESIAN_POINT('Ctrl Pts',(-0.241555082508471,2.31570063702235,
10.960020041645));
#67376=CARTESIAN_POINT('Ctrl Pts',(-0.263772148334165,2.28525530336174,
10.9622529216656));
#67377=CARTESIAN_POINT('Ctrl Pts',(-0.267085267268975,2.28044591165535,
10.9626033508674));
#67378=CARTESIAN_POINT('Ctrl Pts',(-0.270803857736533,2.27472098350322,
10.9630189369418));
#67379=CARTESIAN_POINT('Ctrl Pts',(-0.271338133537857,2.27389010522579,
10.9630792141947));
#67380=CARTESIAN_POINT('Ctrl Pts',(-0.272137808888918,2.27263383207967,
10.9631703001465));
#67381=CARTESIAN_POINT('Ctrl Pts',(-0.272406052927599,2.27221024745726,
10.9632010032093));
#67382=CARTESIAN_POINT('Ctrl Pts',(-0.272882849420923,2.27145343581024,
10.9632558447674));
#67383=CARTESIAN_POINT('Ctrl Pts',(-0.273091783146859,2.27112044920089,
10.9632799690961));
#67384=CARTESIAN_POINT('Ctrl Pts',(-0.273531142866867,2.27041736875368,
10.9633308955763));
#67385=CARTESIAN_POINT('Ctrl Pts',(-0.273761428011194,2.27004718821927,
10.9633577028604));
#67386=CARTESIAN_POINT('Ctrl Pts',(-0.274368122860366,2.26906750710678,
10.9634286326884));
#67387=CARTESIAN_POINT('Ctrl Pts',(-0.274743251130419,2.26845721933555,
10.9634728022551));
#67388=CARTESIAN_POINT('Ctrl Pts',(-0.276436894559954,2.26568116365865,
10.9636736522902));
#67389=CARTESIAN_POINT('Ctrl Pts',(-0.277731827901016,2.26350117994996,
10.9638311926291));
#67390=CARTESIAN_POINT('Ctrl Pts',(-0.283275559870006,2.25391254579048,
10.9645235048124));
#67391=CARTESIAN_POINT('Ctrl Pts',(-0.287254297008239,2.24635252434112,
10.9650678601259));
#67392=CARTESIAN_POINT('Ctrl Pts',(-0.294913678652514,2.23028022388178,
10.9662228655744));
#67393=CARTESIAN_POINT('Ctrl Pts',(-0.298536681400055,2.2217490934837,10.9668347079274));
#67394=CARTESIAN_POINT('Ctrl Pts',(-0.310613646588465,2.1895165660611,10.969135254109));
#67395=CARTESIAN_POINT('Ctrl Pts',(-0.316651403064107,2.16500717140273,
10.9708704080542));
#67396=CARTESIAN_POINT('Ctrl Pts',(-0.319949542429548,2.13867022547181,
10.9725997397257));
#67397=CARTESIAN_POINT('Ctrl Pts',(-0.320112869977615,2.13729405635418,
10.9726896947713));
#67398=CARTESIAN_POINT('Ctrl Pts',(-0.320317146764235,2.13547253885684,
10.9728081870754));
#67399=CARTESIAN_POINT('Ctrl Pts',(-0.320366050795247,2.13502811765518,
10.9728370522035));
#67400=CARTESIAN_POINT('Ctrl Pts',(-0.320847886025833,2.13056395555407,
10.9731265370863));
#67401=CARTESIAN_POINT('Ctrl Pts',(-0.321206088488374,2.12653627360764,
10.9733839585624));
#67402=CARTESIAN_POINT('Ctrl Pts',(-0.321530009532216,2.12190852265042,
10.9736746182531));
#67403=CARTESIAN_POINT('Ctrl Pts',(-0.321569951881506,2.12131423127655,
10.973711847856));
#67404=CARTESIAN_POINT('Ctrl Pts',(-0.321626334010426,2.12043908122525,
10.9737665262981));
#67405=CARTESIAN_POINT('Ctrl Pts',(-0.321644053705415,2.12015831063642,
10.9737840464796));
#67406=CARTESIAN_POINT('Ctrl Pts',(-0.321674558231837,2.11966468110594,
10.9738148099156));
#67407=CARTESIAN_POINT('Ctrl Pts',(-0.321687499459502,2.11945183254085,
10.9738280620025));
#67408=CARTESIAN_POINT('Ctrl Pts',(-0.321712427713363,2.11903500018582,
10.973853989));
#67409=CARTESIAN_POINT('Ctrl Pts',(-0.321724431955575,2.11883101857893,
10.9738666648614));
#67410=CARTESIAN_POINT('Ctrl Pts',(-0.321749941839371,2.11839039780635,
10.97389402076));
#67411=CARTESIAN_POINT('Ctrl Pts',(-0.321763380448994,2.11815375465339,
10.9739086970079));
#67412=CARTESIAN_POINT('Ctrl Pts',(-0.321795326792112,2.11758002415924,
10.9739442412565));
#67413=CARTESIAN_POINT('Ctrl Pts',(-0.32181356600365,2.11724292124719,10.9739650942513));
#67414=CARTESIAN_POINT('Ctrl Pts',(-0.3218616962146,2.11632667843549,10.974021688422));
#67415=CARTESIAN_POINT('Ctrl Pts',(-0.321890553974519,2.11574748211461,
10.9740573727328));
#67416=CARTESIAN_POINT('Ctrl Pts',(-0.322153811874418,2.11016030736698,
10.9744007455043));
#67417=CARTESIAN_POINT('Ctrl Pts',(-0.322272898997973,2.10514729573573,
10.9747022220165));
#67418=CARTESIAN_POINT('Ctrl Pts',(-0.322274972444447,2.10013327014249,
10.9749989620444));
#67419=CARTESIAN_POINT('',(-0.322274851933155,2.09976304472565,11.2245150602744));
#67420=CARTESIAN_POINT('Ctrl Pts',(-0.322274972285662,2.10013365356628,
10.9749989393526));
#67421=CARTESIAN_POINT('Ctrl Pts',(-0.322286505590925,2.07232372871807,
10.9766447874895));
#67422=CARTESIAN_POINT('Ctrl Pts',(-0.318698447630823,2.0446243611031,10.9781452314249));
#67423=CARTESIAN_POINT('Ctrl Pts',(-0.307582929054177,2.00252678812056,
10.980613112068));
#67424=CARTESIAN_POINT('Ctrl Pts',(-0.30246370257334,1.98764388337767,10.9815231732153));
#67425=CARTESIAN_POINT('Ctrl Pts',(-0.295305324641373,1.97091834625809,
10.9826204205879));
#67426=CARTESIAN_POINT('Ctrl Pts',(-0.294304759986646,1.96865307078078,
10.98277063913));
#67427=CARTESIAN_POINT('Ctrl Pts',(-0.292983742380287,1.96575318668376,
10.9829650992664));
#67428=CARTESIAN_POINT('Ctrl Pts',(-0.292687140388391,1.96510775402837,
10.9830085192869));
#67429=CARTESIAN_POINT('Ctrl Pts',(-0.292205626817879,1.96406900217425,
10.9830786247952));
#67430=CARTESIAN_POINT('Ctrl Pts',(-0.292022048046513,1.96367506476905,
10.9831052642163));
#67431=CARTESIAN_POINT('Ctrl Pts',(-0.291670779306314,1.96292525071276,
10.9831560699419));
#67432=CARTESIAN_POINT('Ctrl Pts',(-0.291503233346953,1.9625693071421,10.9831802312259));
#67433=CARTESIAN_POINT('Ctrl Pts',(-0.291119615562072,1.96175818673965,
10.9832353890754));
#67434=CARTESIAN_POINT('Ctrl Pts',(-0.290903127566555,1.96130320888384,
10.9832664000362));
#67435=CARTESIAN_POINT('Ctrl Pts',(-0.29023911087759,1.95991608471161,10.9833611651593));
#67436=CARTESIAN_POINT('Ctrl Pts',(-0.28978816549436,1.95898558972559,10.983425038007));
#67437=CARTESIAN_POINT('Ctrl Pts',(-0.286460554789652,1.95220266464841,
10.9838928902086));
#67438=CARTESIAN_POINT('Ctrl Pts',(-0.283411501660716,1.94643694292837,
10.9843028802144));
#67439=CARTESIAN_POINT('Ctrl Pts',(-0.279294527895826,1.9391925816273,10.9848345157245));
#67440=CARTESIAN_POINT('Ctrl Pts',(-0.278385964976796,1.93762477586695,
10.9849505817826));
#67441=CARTESIAN_POINT('Ctrl Pts',(-0.276190157854215,1.9339083212073,10.9852281369164));
#67442=CARTESIAN_POINT('Ctrl Pts',(-0.274891004631814,1.93176687572201,
10.9853900192953));
#67443=CARTESIAN_POINT('Ctrl Pts',(-0.258638755590362,1.90566860378542,
10.9873869655372));
#67444=CARTESIAN_POINT('Ctrl Pts',(-0.240624897632953,1.8837641769449,10.9893295095311));
#67445=CARTESIAN_POINT('Ctrl Pts',(-0.216796979188666,1.86150602677445,
10.9915064069956));
#67446=CARTESIAN_POINT('Ctrl Pts',(-0.213540201652061,1.85858564558906,
10.9917964689506));
#67447=CARTESIAN_POINT('Ctrl Pts',(-0.206372239800927,1.85241665856006,
10.9924173105733));
#67448=CARTESIAN_POINT('Ctrl Pts',(-0.202441458342558,1.84919235544017,
10.9927469917213));
#67449=CARTESIAN_POINT('Ctrl Pts',(-0.197142943171452,1.84505191155942,
10.9931756268706));
#67450=CARTESIAN_POINT('Ctrl Pts',(-0.195842342519386,1.84405147983064,
10.9932796230344));
#67451=CARTESIAN_POINT('Ctrl Pts',(-0.193961465477244,1.84262742674652,
10.9934282078485));
#67452=CARTESIAN_POINT('Ctrl Pts',(-0.193387349586159,1.84219576303671,
10.9934733217587));
#67453=CARTESIAN_POINT('Ctrl Pts',(-0.192367766777382,1.84143448606023,
10.9935530093519));
#67454=CARTESIAN_POINT('Ctrl Pts',(-0.191922886322869,1.84110409734757,
10.9935876354554));
#67455=CARTESIAN_POINT('Ctrl Pts',(-0.191255678264736,1.8406112628323,10.9936393472546));
#67456=CARTESIAN_POINT('Ctrl Pts',(-0.191033993975276,1.84044795399541,
10.993656492858));
#67457=CARTESIAN_POINT('Ctrl Pts',(-0.19064074625559,1.8401590357485,10.9936868434776));
#67458=CARTESIAN_POINT('Ctrl Pts',(-0.19046926782256,1.84003331203363,10.9937000565092));
#67459=CARTESIAN_POINT('Ctrl Pts',(-0.190125726777528,1.83978195867729,
10.9937264843247));
#67460=CARTESIAN_POINT('Ctrl Pts',(-0.189953664640784,1.83965633039631,
10.993739699024));
#67461=CARTESIAN_POINT('Ctrl Pts',(-0.18953259415636,1.83934953250683,10.9937719854924));
#67462=CARTESIAN_POINT('Ctrl Pts',(-0.18928344986884,1.83916854856127,10.9937910442971));
#67463=CARTESIAN_POINT('Ctrl Pts',(-0.188330687951089,1.838478525171,10.9938637581903));
#67464=CARTESIAN_POINT('Ctrl Pts',(-0.187625264868729,1.83797196744496,
10.9939172427132));
#67465=CARTESIAN_POINT('Ctrl Pts',(-0.171601045978219,1.82656301689355,
10.9951244317931));
#67466=CARTESIAN_POINT('Ctrl Pts',(-0.155356641582743,1.81701723021737,
10.9961892365301));
#67467=CARTESIAN_POINT('Ctrl Pts',(-0.127038638249114,1.80355476045963,
10.9979468928977));
#67468=CARTESIAN_POINT('Ctrl Pts',(-0.1154023415154,1.79883411312044,10.9986438678778));
#67469=CARTESIAN_POINT('Ctrl Pts',(-0.0908192867085159,1.79049568797157,
11.0001099554788));
#67470=CARTESIAN_POINT('Ctrl Pts',(-0.0778625531357536,1.78698493563875,
11.0008794379299));
#67471=CARTESIAN_POINT('Ctrl Pts',(-0.0590317109278613,1.78312428875382,
11.0020190229934));
#67472=CARTESIAN_POINT('Ctrl Pts',(-0.0533075363000413,1.78211124699869,
11.0023680606024));
#67473=CARTESIAN_POINT('Ctrl Pts',(-0.0466451239344354,1.7811171649638,
11.0027783817122));
#67474=CARTESIAN_POINT('Ctrl Pts',(-0.0457303090077639,1.78098468864694,
11.0028348106505));
#67475=CARTESIAN_POINT('Ctrl Pts',(-0.0443381956867634,1.78078920475774,
11.0029208186924));
#67476=CARTESIAN_POINT('Ctrl Pts',(-0.0438612997994791,1.78072332723506,
11.0029503069855));
#67477=CARTESIAN_POINT('Ctrl Pts',(-0.0430337339081151,1.78061089795157,
11.003001521745));
#67478=CARTESIAN_POINT('Ctrl Pts',(-0.0426831306197502,1.78056385439297,
11.0030232326285));
#67479=CARTESIAN_POINT('Ctrl Pts',(-0.0419540916280925,1.78046725443173,
11.0030684061299));
#67480=CARTESIAN_POINT('Ctrl Pts',(-0.0415756440955298,1.7804177928751,
11.0030918717088));
#67481=CARTESIAN_POINT('Ctrl Pts',(-0.0406527590303697,1.78029884258931,
11.0031491339876));
#67482=CARTESIAN_POINT('Ctrl Pts',(-0.0401082315710116,1.78023007236325,
11.0031829533213));
#67483=CARTESIAN_POINT('Ctrl Pts',(-0.038043606937609,1.77997468049737,
11.0033113093046));
#67484=CARTESIAN_POINT('Ctrl Pts',(-0.0365223807408191,1.77979750668268,
11.0034061434928));
#67485=CARTESIAN_POINT('Ctrl Pts',(-0.0344065489643755,1.77956635419292,
11.0035384208527));
#67486=CARTESIAN_POINT('Ctrl Pts',(-0.0338129519234283,1.7795031727905,
11.0035755722486));
#67487=CARTESIAN_POINT('Ctrl Pts',(0.00112730891194376,1.7758823437247,
11.0057648121165));
#67488=CARTESIAN_POINT('Ctrl Pts',(0.0358162906273977,1.77786733165216,
11.0081134930966));
#67489=CARTESIAN_POINT('Ctrl Pts',(0.0791987263826779,1.78745069442327,
11.0111031474422));
#67490=CARTESIAN_POINT('Ctrl Pts',(0.0887783865065095,1.79003559102699,
11.011764032059));
#67491=CARTESIAN_POINT('Ctrl Pts',(0.10150815450842,1.79410923732769,11.012630987656));
#67492=CARTESIAN_POINT('Ctrl Pts',(0.104775151156336,1.79521280541231,11.0128524443016));
#67493=CARTESIAN_POINT('Ctrl Pts',(0.10919022981537,1.79678357282061,11.0131497184835));
#67494=CARTESIAN_POINT('Ctrl Pts',(0.110354129889588,1.79720522770592,11.0132278941916));
#67495=CARTESIAN_POINT('Ctrl Pts',(0.112063308930015,1.79783558909977,11.0133423821373));
#67496=CARTESIAN_POINT('Ctrl Pts',(0.112610480119193,1.79803908166318,11.0133789866153));
#67497=CARTESIAN_POINT('Ctrl Pts',(0.113474674488532,1.7983631506095,11.0134367208747));
#67498=CARTESIAN_POINT('Ctrl Pts',(0.113792062177418,1.79848274137554,11.0134579078631));
#67499=CARTESIAN_POINT('Ctrl Pts',(0.114391741679551,1.79870978062201,11.013497906566));
#67500=CARTESIAN_POINT('Ctrl Pts',(0.114674072055389,1.79881712522565,11.0135167244092));
#67501=CARTESIAN_POINT('Ctrl Pts',(0.115161179424897,1.7990031121493,11.0135491669555));
#67502=CARTESIAN_POINT('Ctrl Pts',(0.115366027466735,1.7990815667827,11.0135628029791));
#67503=CARTESIAN_POINT('Ctrl Pts',(0.115762385097162,1.7992338317814,11.0135891726748));
#67504=CARTESIAN_POINT('Ctrl Pts',(0.115953904001306,1.79930761583351,11.0136019079176));
#67505=CARTESIAN_POINT('Ctrl Pts',(0.116405490607794,1.79948208846341,11.0136319215314));
#67506=CARTESIAN_POINT('Ctrl Pts',(0.116665498857491,1.79958293195018,11.0136491905337));
#67507=CARTESIAN_POINT('Ctrl Pts',(0.117434918962496,1.79988249897222,11.013700259126));
#67508=CARTESIAN_POINT('Ctrl Pts',(0.117943959583554,1.80008218288509,11.0137340013147));
#67509=CARTESIAN_POINT('Ctrl Pts',(0.122473263983379,1.80187223047611,11.0140338562746));
#67510=CARTESIAN_POINT('Ctrl Pts',(0.126461891364466,1.80354214154966,11.0142952907844));
#67511=CARTESIAN_POINT('Ctrl Pts',(0.144029989661839,1.81131647862155,11.0154401865152));
#67512=CARTESIAN_POINT('Ctrl Pts',(0.157211761980527,1.81827784859222,11.0162819372703));
#67513=CARTESIAN_POINT('Ctrl Pts',(0.182288593846631,1.83383139104344,11.0179360459235));
#67514=CARTESIAN_POINT('Ctrl Pts',(0.194172430617465,1.84237252236545,11.0187469857272));
#67515=CARTESIAN_POINT('Ctrl Pts',(0.218344214336702,1.86237068973899,11.0205284698258));
#67516=CARTESIAN_POINT('Ctrl Pts',(0.230398962818633,1.87403964793668,11.0215028961044));
#67517=CARTESIAN_POINT('Ctrl Pts',(0.242267860162846,1.8874703898857,11.0225926581617));
#67518=CARTESIAN_POINT('Ctrl Pts',(0.243039713951109,1.88835348188817,11.0226641666582));
#67519=CARTESIAN_POINT('Ctrl Pts',(0.244153673844902,1.8896421129742,11.0227683125976));
#67520=CARTESIAN_POINT('Ctrl Pts',(0.24449963233475,1.89004432165627,11.0228007905086));
#67521=CARTESIAN_POINT('Ctrl Pts',(0.245102895285899,1.89074918362958,11.0228576589865));
#67522=CARTESIAN_POINT('Ctrl Pts',(0.24536063694186,1.89105146263633,11.0228820314777));
#67523=CARTESIAN_POINT('Ctrl Pts',(0.245858454383012,1.89163749333182,11.022929253109));
#67524=CARTESIAN_POINT('Ctrl Pts',(0.246098599593246,1.89192118547748,11.0229520993466));
#67525=CARTESIAN_POINT('Ctrl Pts',(0.246668331848672,1.89259659655669,11.0230064601568));
#67526=CARTESIAN_POINT('Ctrl Pts',(0.246997476611873,1.89298868572125,11.0230379927519));
#67527=CARTESIAN_POINT('Ctrl Pts',(0.248159056598995,1.89437911611605,11.0231497273836));
#67528=CARTESIAN_POINT('Ctrl Pts',(0.248986376023775,1.89538169745484,11.0232301372489));
#67529=CARTESIAN_POINT('Ctrl Pts',(0.263090155004585,1.91268545502951,11.0246153598456));
#67530=CARTESIAN_POINT('Ctrl Pts',(0.274743587065271,1.93023893518118,11.0259865192235));
#67531=CARTESIAN_POINT('Ctrl Pts',(0.297624392304764,1.97330706051475,11.0292580007473));
#67532=CARTESIAN_POINT('Ctrl Pts',(0.307425042725117,1.99939509541718,11.0311773524713));
#67533=CARTESIAN_POINT('Ctrl Pts',(0.314047052837155,2.0276316273834,11.0330174070865));
#67534=CARTESIAN_POINT('Ctrl Pts',(0.314324914044205,2.02884818148198,11.0330962190931));
#67535=CARTESIAN_POINT('Ctrl Pts',(0.314723135176345,2.03063957436843,11.0332115561625));
#67536=CARTESIAN_POINT('Ctrl Pts',(0.314848997305213,2.03121315992428,11.0332483784213));
#67537=CARTESIAN_POINT('Ctrl Pts',(0.315045377313401,2.03211994515133,11.0333064177723));
#67538=CARTESIAN_POINT('Ctrl Pts',(0.31511693523804,2.03245291463347,11.0333276928405));
#67539=CARTESIAN_POINT('Ctrl Pts',(0.31525112495666,2.03308217317511,11.0333678288733));
#67540=CARTESIAN_POINT('Ctrl Pts',(0.315313867131693,2.03337843795238,11.0333866960886));
#67541=CARTESIAN_POINT('Ctrl Pts',(0.315421382194234,2.03388967179714,11.0334192019865));
#67542=CARTESIAN_POINT('Ctrl Pts',(0.315466353070964,2.03410459863101,11.033432852088));
#67543=CARTESIAN_POINT('Ctrl Pts',(0.31555288081542,2.03452025463806,11.0334592201462));
#67544=CARTESIAN_POINT('Ctrl Pts',(0.31559446577971,2.03472097723323,11.0334719397283));
#67545=CARTESIAN_POINT('Ctrl Pts',(0.315691971851304,2.03519389111773,11.0335018758161));
#67546=CARTESIAN_POINT('Ctrl Pts',(0.315747732592164,2.0354661158454,11.0335190830717));
#67547=CARTESIAN_POINT('Ctrl Pts',(0.315911394195508,2.036270404244,11.0335698492085));
#67548=CARTESIAN_POINT('Ctrl Pts',(0.316018303468171,2.03680267220058,11.0336033516415));
#67549=CARTESIAN_POINT('Ctrl Pts',(0.316943371249401,2.04146934412526,11.0338962822342));
#67550=CARTESIAN_POINT('Ctrl Pts',(0.317681746909734,2.04561939614342,11.0341512666328));
#67551=CARTESIAN_POINT('Ctrl Pts',(0.318487897271585,2.0507297891205,11.0344598276248));
#67552=CARTESIAN_POINT('Ctrl Pts',(0.318633031377166,2.05167727506182,11.0345168080056));
#67553=CARTESIAN_POINT('Ctrl Pts',(0.318790664114814,2.05273795343883,11.0345803547889));
#67554=CARTESIAN_POINT('Ctrl Pts',(0.318807330912431,2.05285051083551,11.0345870952348));
#67555=CARTESIAN_POINT('Ctrl Pts',(0.323594825879833,2.08530093292347,11.0365295054938));
#67556=CARTESIAN_POINT('Ctrl Pts',(0.323418871791408,2.1181796131024,11.0382671601089));
#67557=CARTESIAN_POINT('Ctrl Pts',(0.316499908032065,2.16181264824939,11.040809420811));
#67558=CARTESIAN_POINT('Ctrl Pts',(0.314097276321906,2.17304691931913,11.0414837537174));
#67559=CARTESIAN_POINT('Ctrl Pts',(0.310566713491625,2.18610270396061,11.0423014877548));
#67560=CARTESIAN_POINT('Ctrl Pts',(0.310014005571546,2.18807198878652,11.0424257487357));
#67561=CARTESIAN_POINT('Ctrl Pts',(0.309257687246741,2.19067136584204,11.0425910288291));
#67562=CARTESIAN_POINT('Ctrl Pts',(0.309070818809496,2.19130631224068,11.0426315015477));
#67563=CARTESIAN_POINT('Ctrl Pts',(0.308761089093054,2.19234687381505,11.0426979947211));
#67564=CARTESIAN_POINT('Ctrl Pts',(0.308639380696337,2.19275283242039,11.0427239774479));
#67565=CARTESIAN_POINT('Ctrl Pts',(0.308402190327191,2.19353834520715,11.0427743337435));
#67566=CARTESIAN_POINT('Ctrl Pts',(0.308286807508776,2.19391792872775,11.0427987040273));
#67567=CARTESIAN_POINT('Ctrl Pts',(0.308019068861919,2.19479291895021,11.0428549656657));
#67568=CARTESIAN_POINT('Ctrl Pts',(0.307866218534672,2.19528817211921,11.0428868731841));
#67569=CARTESIAN_POINT('Ctrl Pts',(0.307374018766481,2.19686941073919,11.042988949499));
#67570=CARTESIAN_POINT('Ctrl Pts',(0.307030115601695,2.19795395964441,11.0430592676338));
#67571=CARTESIAN_POINT('Ctrl Pts',(0.303855251642027,2.20778535809125,11.043699513596));
#67572=CARTESIAN_POINT('Ctrl Pts',(0.300657221435879,2.21640835345211,11.0442815254013));
#67573=CARTESIAN_POINT('Ctrl Pts',(0.285742114969969,2.25189144740712,11.0467668190956));
#67574=CARTESIAN_POINT('Ctrl Pts',(0.270759418599727,2.27722408076043,11.0487806693746));
#67575=CARTESIAN_POINT('Ctrl Pts',(0.248599651072349,2.3051832800998,11.0511655147813));
#67576=CARTESIAN_POINT('Ctrl Pts',(0.244484503756594,2.31006975374366,11.0515885027043));
#67577=CARTESIAN_POINT('Ctrl Pts',(0.23672517478167,2.31874633191602,11.0523466005296));
#67578=CARTESIAN_POINT('Ctrl Pts',(0.233128257590068,2.32257580577685,11.0526838601655));
#67579=CARTESIAN_POINT('Ctrl Pts',(0.228972287035158,2.32678912949382,11.0530562838448));
#67580=CARTESIAN_POINT('Ctrl Pts',(0.228504018334942,2.32726093177172,11.0530980069804));
#67581=CARTESIAN_POINT('Ctrl Pts',(0.227771615230126,2.32799430935568,11.0531628878784));
#67582=CARTESIAN_POINT('Ctrl Pts',(0.227508485623431,2.32825687892315,11.0531861222213));
#67583=CARTESIAN_POINT('Ctrl Pts',(0.2270668660611,2.32869603626308,11.0532249902718));
#67584=CARTESIAN_POINT('Ctrl Pts',(0.226888623818351,2.32887287093074,11.0532406433113));
#67585=CARTESIAN_POINT('Ctrl Pts',(0.226540279482203,2.32921765756393,11.0532711669051));
#67586=CARTESIAN_POINT('Ctrl Pts',(0.226370196877471,2.32938562887312,11.0532860389899));
#67587=CARTESIAN_POINT('Ctrl Pts',(0.22604755403463,2.32970355831272,11.0533141913446));
#67588=CARTESIAN_POINT('Ctrl Pts',(0.225895032625989,2.32985355255407,11.0533274744534));
#67589=CARTESIAN_POINT('Ctrl Pts',(0.225541776537568,2.33020026423165,11.053358181479));
#67590=CARTESIAN_POINT('Ctrl Pts',(0.225340934053014,2.33039687076347,11.0533755965801));
#67591=CARTESIAN_POINT('Ctrl Pts',(0.224725701221314,2.33099755373371,11.0534288123423));
#67592=CARTESIAN_POINT('Ctrl Pts',(0.224310476424354,2.33140077959882,11.053464546345));
#67593=CARTESIAN_POINT('Ctrl Pts',(0.221256457636975,2.33435060040325,11.0537260645824));
#67594=CARTESIAN_POINT('Ctrl Pts',(0.218575320882135,2.33685323690722,11.0539485093795));
#67595=CARTESIAN_POINT('Ctrl Pts',(0.198326479432866,2.35511723274437,11.0555814939783));
#67596=CARTESIAN_POINT('Ctrl Pts',(0.179115160409457,2.36895402044413,11.0568769247291));
#67597=CARTESIAN_POINT('Ctrl Pts',(0.147215452101506,2.38698198964458,11.0589296486043));
#67598=CARTESIAN_POINT('Ctrl Pts',(0.135490552676234,2.39270006243359,11.059665335046));
#67599=CARTESIAN_POINT('Ctrl Pts',(0.115554219353248,2.40096761646637,11.0609183459603));
#67600=CARTESIAN_POINT('Ctrl Pts',(0.107529464692874,2.40392709493348,11.0614230845691));
#67601=CARTESIAN_POINT('Ctrl Pts',(0.0978051816322179,2.40707999350992,
11.062039403416));
#67602=CARTESIAN_POINT('Ctrl Pts',(0.0962093673241007,2.4075837015274,11.0621406881873));
#67603=CARTESIAN_POINT('Ctrl Pts',(0.0934185450418449,2.40844076221392,
11.0623181014675));
#67604=CARTESIAN_POINT('Ctrl Pts',(0.0922252666255146,2.40879965751356,
11.0623940480093));
#67605=CARTESIAN_POINT('Ctrl Pts',(0.0905082591785677,2.4093052317748,11.0625034659324));
#67606=CARTESIAN_POINT('Ctrl Pts',(0.08998618313039,2.40945752248523,11.0625367540473));
#67607=CARTESIAN_POINT('Ctrl Pts',(0.0890799301691933,2.40971939116687,
11.0625945703844));
#67608=CARTESIAN_POINT('Ctrl Pts',(0.0886959292143868,2.4098295779331,11.062619078708));
#67609=CARTESIAN_POINT('Ctrl Pts',(0.0879574884210784,2.41003998375589,
11.0626662285788));
#67610=CARTESIAN_POINT('Ctrl Pts',(0.0876030794755914,2.41014030979758,
11.0626888666004));
#67611=CARTESIAN_POINT('Ctrl Pts',(0.0867681950696272,2.4103751035249,11.0627422162835));
#67612=CARTESIAN_POINT('Ctrl Pts',(0.0862875788253872,2.4105090631523,11.0627729444155));
#67613=CARTESIAN_POINT('Ctrl Pts',(0.0848683063736579,2.41090109983592,
11.0628637349262));
#67614=CARTESIAN_POINT('Ctrl Pts',(0.0839287959360401,2.4111560388058,11.0629238990436));
#67615=CARTESIAN_POINT('Ctrl Pts',(0.0756229958424341,2.41336948821514,
11.0634563689979));
#67616=CARTESIAN_POINT('Ctrl Pts',(0.0681910842962278,2.41507020443631,
11.0639369634235));
#67617=CARTESIAN_POINT('Ctrl Pts',(0.0556381306158246,2.41747788255345,
11.0647566078587));
#67618=CARTESIAN_POINT('Ctrl Pts',(0.050547519747401,2.41832805591596,11.0650911187698));
#67619=CARTESIAN_POINT('Ctrl Pts',(0.0203676535977019,2.4226261780475,11.0670861740336));
#67620=CARTESIAN_POINT('Ctrl Pts',(-0.0050358085002599,2.42322881557018,
11.0688234755355));
#67621=CARTESIAN_POINT('Ctrl Pts',(-0.0390981100356025,2.42001815879886,
11.0711134265003));
#67622=CARTESIAN_POINT('Ctrl Pts',(-0.0479155718867667,2.41881720162864,
11.0717014867406));
#67623=CARTESIAN_POINT('Ctrl Pts',(-0.0604554131837114,2.41657713777353,
11.0725212685571));
#67624=CARTESIAN_POINT('Ctrl Pts',(-0.0642259500314016,2.41583377232668,
11.0727655796292));
#67625=CARTESIAN_POINT('Ctrl Pts',(-0.0685083407886799,2.41490962554986,
11.0730398658279));
#67626=CARTESIAN_POINT('Ctrl Pts',(-0.0690339110882322,2.41479482866049,
11.0730734734072));
#67627=CARTESIAN_POINT('Ctrl Pts',(-0.0698255561840318,2.41461983685557,
11.0731240095053));
#67628=CARTESIAN_POINT('Ctrl Pts',(-0.0700918427085674,2.414560619955,11.0731409937705));
#67629=CARTESIAN_POINT('Ctrl Pts',(-0.0705711293419392,2.41445339718521,
11.073171536866));
#67630=CARTESIAN_POINT('Ctrl Pts',(-0.0707841553714158,2.41440551306747,
11.0731851026602));
#67631=CARTESIAN_POINT('Ctrl Pts',(-0.0712419734018721,2.4143021155744,
11.0732142365868));
#67632=CARTESIAN_POINT('Ctrl Pts',(-0.0714867485126919,2.41424653286369,
11.0732298006185));
#67633=CARTESIAN_POINT('Ctrl Pts',(-0.0721461328219506,2.41409599179341,
11.0732716942551));
#67634=CARTESIAN_POINT('Ctrl Pts',(-0.0725606211979494,2.41400049808581,
11.0732979930275));
#67635=CARTESIAN_POINT('Ctrl Pts',(-0.0744705605062103,2.41355648465866,
11.073419017539));
#67636=CARTESIAN_POINT('Ctrl Pts',(-0.0759637296475638,2.41319809298793,
11.073513184125));
#67637=CARTESIAN_POINT('Ctrl Pts',(-0.107942151474649,2.40528045594786,
11.0755213688631));
#67638=CARTESIAN_POINT('Ctrl Pts',(-0.137168483565152,2.39331424067264,
11.0772023830586));
#67639=CARTESIAN_POINT('Ctrl Pts',(-0.170823547680819,2.37338555260755,
11.0794161170358));
#67640=CARTESIAN_POINT('Ctrl Pts',(-0.177299603940018,2.36923072925723,
11.0798557117326));
#67641=CARTESIAN_POINT('Ctrl Pts',(-0.190568968560996,2.36003101958675,
11.0807933381482));
#67642=CARTESIAN_POINT('Ctrl Pts',(-0.197324598403303,2.35494243947079,
11.0812924888056));
#67643=CARTESIAN_POINT('Ctrl Pts',(-0.20586390398981,2.3479674246868,11.0819571186211));
#67644=CARTESIAN_POINT('Ctrl Pts',(-0.207836242385954,2.34631663855998,
11.0821130853541));
#67645=CARTESIAN_POINT('Ctrl Pts',(-0.210335139219411,2.34417375628028,
11.0823139517104));
#67646=CARTESIAN_POINT('Ctrl Pts',(-0.210880134570738,2.34370322705424,
11.0823579611775));
#67647=CARTESIAN_POINT('Ctrl Pts',(-0.21175319877268,2.34294433357055,11.082428789828));
#67648=CARTESIAN_POINT('Ctrl Pts',(-0.212082268297347,2.34265711997669,
11.0824555611999));
#67649=CARTESIAN_POINT('Ctrl Pts',(-0.212706264277336,2.34211025414729,
11.0825064696922));
#67650=CARTESIAN_POINT('Ctrl Pts',(-0.213001301961375,2.34185072955579,
11.082530601463));
#67651=CARTESIAN_POINT('Ctrl Pts',(-0.213670623451771,2.34125979818048,
11.0825854864903));
#67652=CARTESIAN_POINT('Ctrl Pts',(-0.214044611588771,2.3409280593656,11.0826162536195));
#67653=CARTESIAN_POINT('Ctrl Pts',(-0.215150220485708,2.33994274459153,
11.0827075066318));
#67654=CARTESIAN_POINT('Ctrl Pts',(-0.215879625557522,2.33928670103503,
11.0827680962354));
#67655=CARTESIAN_POINT('Ctrl Pts',(-0.220834003862298,2.33478952925394,
11.0831823111476));
#67656=CARTESIAN_POINT('Ctrl Pts',(-0.22495901039486,2.33084024175663,11.0835405245172));
#67657=CARTESIAN_POINT('Ctrl Pts',(-0.251185289099338,2.30436034631158,
11.0859092796138));
#67658=CARTESIAN_POINT('Ctrl Pts',(-0.269976449189104,2.2787990379345,11.0880695269971));
#67659=CARTESIAN_POINT('Ctrl Pts',(-0.289414584760995,2.24212520419406,
11.0908546960212));
#67660=CARTESIAN_POINT('Ctrl Pts',(-0.293668901525981,2.2331126833806,11.0915150774641));
#67661=CARTESIAN_POINT('Ctrl Pts',(-0.298954795570931,2.22042232468121,
11.0923994514248));
#67662=CARTESIAN_POINT('Ctrl Pts',(-0.300348763214145,2.2169022225204,11.0926400767577));
#67663=CARTESIAN_POINT('Ctrl Pts',(-0.301869012781538,2.21285637827059,
11.0929106664692));
#67664=CARTESIAN_POINT('Ctrl Pts',(-0.302056320621364,2.21235409283417,
11.0929441555249));
#67665=CARTESIAN_POINT('Ctrl Pts',(-0.302336917480526,2.21159586979602,
11.0929945491833));
#67666=CARTESIAN_POINT('Ctrl Pts',(-0.302431135537317,2.21134028060896,
11.0930115090652));
#67667=CARTESIAN_POINT('Ctrl Pts',(-0.302593108131419,2.21089916837023,
11.0930407320606));
#67668=CARTESIAN_POINT('Ctrl Pts',(-0.302661016100332,2.21071370270996,
11.0930530044007));
#67669=CARTESIAN_POINT('Ctrl Pts',(-0.302801946771057,2.2103277036916,11.0930785159454));
#67670=CARTESIAN_POINT('Ctrl Pts',(-0.302874940562762,2.21012716081844,
11.0930917533838));
#67671=CARTESIAN_POINT('Ctrl Pts',(-0.303075351311409,2.20957484670271,
11.0931281644425));
#67672=CARTESIAN_POINT('Ctrl Pts',(-0.30320235550609,2.20922292443155,11.0931513133117));
#67673=CARTESIAN_POINT('Ctrl Pts',(-0.303692695285387,2.20785677135116,
11.0932409800713));
#67674=CARTESIAN_POINT('Ctrl Pts',(-0.304051562363496,2.20684092753995,
11.0933072346486));
#67675=CARTESIAN_POINT('Ctrl Pts',(-0.310770061875346,2.18751486839519,
11.0945600868534));
#67676=CARTESIAN_POINT('Ctrl Pts',(-0.315471163088868,2.16866639143661,
11.0956535704891));
#67677=CARTESIAN_POINT('Ctrl Pts',(-0.320984911269382,2.1331996890645,11.0976634125365));
#67678=CARTESIAN_POINT('Ctrl Pts',(-0.322263687232037,2.11672194114262,
11.0985791771401));
#67679=CARTESIAN_POINT('Ctrl Pts',(-0.322279119157057,2.09406097418821,
11.0998769815226));
#67680=CARTESIAN_POINT('Ctrl Pts',(-0.322106784972583,2.08790389574324,
11.1002333037848));
#67681=CARTESIAN_POINT('Ctrl Pts',(-0.321662121054868,2.08006173344352,
11.100693995383));
#67682=CARTESIAN_POINT('Ctrl Pts',(-0.321552690927278,2.07836850894687,
11.1007938705203));
#67683=CARTESIAN_POINT('Ctrl Pts',(-0.320967512822546,2.07030403697101,
11.1012716286859));
#67684=CARTESIAN_POINT('Ctrl Pts',(-0.320315770191979,2.06394735442926,
11.1016544275016));
#67685=CARTESIAN_POINT('Ctrl Pts',(-0.319340408853926,2.05659567667398,
11.1021058058224));
#67686=CARTESIAN_POINT('Ctrl Pts',(-0.319200360194628,2.05557746040996,
11.1021685150284));
#67687=CARTESIAN_POINT('Ctrl Pts',(-0.318984575929597,2.05406234036855,
11.1022621201842));
#67688=CARTESIAN_POINT('Ctrl Pts',(-0.318912543737527,2.05356490878941,
11.1022928989308));
#67689=CARTESIAN_POINT('Ctrl Pts',(-0.318782079289554,2.05267858625138,
11.1023478251374));
#67690=CARTESIAN_POINT('Ctrl Pts',(-0.318724098206761,2.05228962905771,
11.1023719582658));
#67691=CARTESIAN_POINT('Ctrl Pts',(-0.31860044012786,2.05147037352446,11.1024228512993));
#67692=CARTESIAN_POINT('Ctrl Pts',(-0.318534603035533,2.0510401004744,11.1024496162334));
#67693=CARTESIAN_POINT('Ctrl Pts',(-0.318358576800999,2.04990507995941,
11.1025203151052));
#67694=CARTESIAN_POINT('Ctrl Pts',(-0.318246919680029,2.04920056557668,
11.1025642955169));
#67695=CARTESIAN_POINT('Ctrl Pts',(-0.317732518027707,2.0460231526446,11.1027630939253));
#67696=CARTESIAN_POINT('Ctrl Pts',(-0.317303291637972,2.04355468479851,
11.1029187504209));
#67697=CARTESIAN_POINT('Ctrl Pts',(-0.313913752637339,2.02532369735203,
11.1040776362655));
#67698=CARTESIAN_POINT('Ctrl Pts',(-0.309809723394746,2.00979916520171,
11.1051176746206));
#67699=CARTESIAN_POINT('Ctrl Pts',(-0.294241904758251,1.96479393743857,
11.108285739829));
#67700=CARTESIAN_POINT('Ctrl Pts',(-0.279583656067169,1.9366233733669,11.110488570131));
#67701=CARTESIAN_POINT('Ctrl Pts',(-0.260150544648588,1.9097756882248,11.112585806053));
#67702=CARTESIAN_POINT('Ctrl Pts',(-0.259229454663409,1.90852236491617,
11.1126836589867));
#67703=CARTESIAN_POINT('Ctrl Pts',(-0.258043706543295,1.90693316229477,
11.1128076172985));
#67704=CARTESIAN_POINT('Ctrl Pts',(-0.257787424646087,1.90659110152979,
11.1128342910974));
#67705=CARTESIAN_POINT('Ctrl Pts',(-0.257379267004166,1.90604858394906,
11.1128765838894));
#67706=CARTESIAN_POINT('Ctrl Pts',(-0.257227836950572,1.90584779483474,
11.1128922339694));
#67707=CARTESIAN_POINT('Ctrl Pts',(-0.256944527580794,1.90547305322312,
11.1129214369502));
#67708=CARTESIAN_POINT('Ctrl Pts',(-0.256812707547586,1.90529905876304,
11.1129349938037));
#67709=CARTESIAN_POINT('Ctrl Pts',(-0.256516162449057,1.9049084623133,11.1129654223928));
#67710=CARTESIAN_POINT('Ctrl Pts',(-0.256351340160191,1.90469193546109,
11.1129822871032));
#67711=CARTESIAN_POINT('Ctrl Pts',(-0.255861833515929,1.90405055832936,
11.1130322331928));
#67712=CARTESIAN_POINT('Ctrl Pts',(-0.255536363815494,1.90362630441212,
11.1130652593433));
#67713=CARTESIAN_POINT('Ctrl Pts',(-0.252922796162288,1.9002369859955,11.1133290241799));
#67714=CARTESIAN_POINT('Ctrl Pts',(-0.250584106784911,1.89731104871572,
11.1135562519831));
#67715=CARTESIAN_POINT('Ctrl Pts',(-0.241048559871339,1.88579851360797,
11.1144514044096));
#67716=CARTESIAN_POINT('Ctrl Pts',(-0.233456541942335,1.877548259749,11.115095504736));
#67717=CARTESIAN_POINT('Ctrl Pts',(-0.200685871950773,1.84546646406922,
11.117690914745));
#67718=CARTESIAN_POINT('Ctrl Pts',(-0.172177353774156,1.82537831924969,
11.1195680576262));
#67719=CARTESIAN_POINT('Ctrl Pts',(-0.140584914647754,1.81000467626274,
11.1216926054115));
#67720=CARTESIAN_POINT('Ctrl Pts',(-0.140152846737291,1.80979561415512,
11.1217216627831));
#67721=CARTESIAN_POINT('Ctrl Pts',(-0.138259922433071,1.80888490956204,
11.1218489735811));
#67722=CARTESIAN_POINT('Ctrl Pts',(-0.13679427193258,1.80819333618129,11.1219475688659));
#67723=CARTESIAN_POINT('Ctrl Pts',(-0.134756737461304,1.80725064082534,
11.1220846867209));
#67724=CARTESIAN_POINT('Ctrl Pts',(-0.13418922897129,1.8069900745575,11.1221228832378));
#67725=CARTESIAN_POINT('Ctrl Pts',(-0.133280570599592,1.80657606598691,
11.122184051147));
#67726=CARTESIAN_POINT('Ctrl Pts',(-0.132939902700795,1.80642156445158,
11.1222069860545));
#67727=CARTESIAN_POINT('Ctrl Pts',(-0.132238082429994,1.80610474321743,
11.12225423995));
#67728=CARTESIAN_POINT('Ctrl Pts',(-0.131876898473017,1.80594249533295,
11.1222785613567));
#67729=CARTESIAN_POINT('Ctrl Pts',(-0.131038579711416,1.80556776831032,
11.1223350188168));
#67730=CARTESIAN_POINT('Ctrl Pts',(-0.130561226541323,1.80535578310536,
11.1223671717287));
#67731=CARTESIAN_POINT('Ctrl Pts',(-0.129050429952884,1.80468925388385,
11.1224689512538));
#67732=CARTESIAN_POINT('Ctrl Pts',(-0.128015120729468,1.80423898320546,
11.1225387236975));
#67733=CARTESIAN_POINT('Ctrl Pts',(-0.110311589729551,1.79664983588963,
11.1237323178894));
#67734=CARTESIAN_POINT('Ctrl Pts',(-0.0930755304292735,1.79092604324175,
11.1249048460923));
#67735=CARTESIAN_POINT('Ctrl Pts',(-0.0449721212638717,1.7793419217712,
11.1281989993795));
#67736=CARTESIAN_POINT('Ctrl Pts',(-0.0135855239974599,1.77648877419941,
11.1303842054922));
#67737=CARTESIAN_POINT('Ctrl Pts',(0.0192291216163404,1.77829562354102,
11.1324630413769));
#67738=CARTESIAN_POINT('Ctrl Pts',(0.0207393158627849,1.77838944989073,
11.1325582119755));
#67739=CARTESIAN_POINT('Ctrl Pts',(0.0226707846860111,1.77852311117779,
11.1326792407297));
#67740=CARTESIAN_POINT('Ctrl Pts',(0.0230926863436832,1.77855314223438,
11.1327056355626));
#67741=CARTESIAN_POINT('Ctrl Pts',(0.0237643128038553,1.77860227787508,
11.1327475851168));
#67742=CARTESIAN_POINT('Ctrl Pts',(0.0240140747259697,1.77862084298106,
11.1327631700821));
#67743=CARTESIAN_POINT('Ctrl Pts',(0.0244816004614455,1.77865614279342,
11.1327923148035));
#67744=CARTESIAN_POINT('Ctrl Pts',(0.0246993672333281,1.77867280758666,
11.1328058783589));
#67745=CARTESIAN_POINT('Ctrl Pts',(0.0251898742010052,1.77871084564593,
11.1328364034087));
#67746=CARTESIAN_POINT('Ctrl Pts',(0.0254626036031507,1.7787323447857,11.1328533576827));
#67747=CARTESIAN_POINT('Ctrl Pts',(0.026275343225585,1.77879745412792,11.1329038286545));
#67748=CARTESIAN_POINT('Ctrl Pts',(0.0268152746379742,1.7788420790444,11.1329372883614));
#67749=CARTESIAN_POINT('Ctrl Pts',(0.0313020651314989,1.779224302717,11.133214773746));
#67750=CARTESIAN_POINT('Ctrl Pts',(0.0352427199463631,1.77963330163458,
11.1334548661034));
#67751=CARTESIAN_POINT('Ctrl Pts',(0.047911748249203,1.78118482665181,11.1342179552807));
#67752=CARTESIAN_POINT('Ctrl Pts',(0.0566016863271637,1.78261234316721,
11.1347279086689));
#67753=CARTESIAN_POINT('Ctrl Pts',(0.0895115152696047,1.78941346595069,
11.1366437919211));
#67754=CARTESIAN_POINT('Ctrl Pts',(0.113139435671579,1.79721980039706,11.1379936325884));
#67755=CARTESIAN_POINT('Ctrl Pts',(0.1407353486564,1.81002361846842,11.1397412842303));
#67756=CARTESIAN_POINT('Ctrl Pts',(0.145768833303795,1.81252098725543,11.1400672070263));
#67757=CARTESIAN_POINT('Ctrl Pts',(0.157494543444109,1.8187258588255,11.1408464662675));
#67758=CARTESIAN_POINT('Ctrl Pts',(0.164124831897628,1.82254243790705,11.14130306007));
#67759=CARTESIAN_POINT('Ctrl Pts',(0.171439417038848,1.82710688635928,11.1418276163898));
#67760=CARTESIAN_POINT('Ctrl Pts',(0.17226376568294,1.82762650608545,11.1418870388028));
#67761=CARTESIAN_POINT('Ctrl Pts',(0.173506818849672,1.82841795231551,11.1419771111624));
#67762=CARTESIAN_POINT('Ctrl Pts',(0.173927274350962,1.82868702934756,11.1420076590608));
#67763=CARTESIAN_POINT('Ctrl Pts',(0.174656936134254,1.82915638090702,11.1420608146164));
#67764=CARTESIAN_POINT('Ctrl Pts',(0.17496642814806,1.82935621129893,11.1420834057006));
#67765=CARTESIAN_POINT('Ctrl Pts',(0.17560395929017,1.82976939803651,11.1421300343566));
#67766=CARTESIAN_POINT('Ctrl Pts',(0.17593195371403,1.82998282199794,11.1421540744307));
#67767=CARTESIAN_POINT('Ctrl Pts',(0.176700603101929,1.83048497253621,11.1422105315963));
#67768=CARTESIAN_POINT('Ctrl Pts',(0.177140939442664,1.83077418263936,11.1422429667704));
#67769=CARTESIAN_POINT('Ctrl Pts',(0.178069410538245,1.83138726049994,11.1423115546311));
#67770=CARTESIAN_POINT('Ctrl Pts',(0.178557374861144,1.8317113817796,11.1423477167863));
#67771=CARTESIAN_POINT('Ctrl Pts',(0.179866742980831,1.8325862598275,11.1424450638094));
#67772=CARTESIAN_POINT('Ctrl Pts',(0.180686494911895,1.83313946679022,11.1425063410808));
#67773=CARTESIAN_POINT('Ctrl Pts',(0.195021465764697,1.84290970756538,11.143583771011));
#67774=CARTESIAN_POINT('Ctrl Pts',(0.207815921021083,1.85313731898319,11.1446392699356));
#67775=CARTESIAN_POINT('Ctrl Pts',(0.237178893393102,1.88051555649975,11.1473024126867));
#67776=CARTESIAN_POINT('Ctrl Pts',(0.252728699838661,1.89861643817499,11.1489383549451));
#67777=CARTESIAN_POINT('Ctrl Pts',(0.271690434451924,1.92638487766024,11.1511705096389));
#67778=CARTESIAN_POINT('Ctrl Pts',(0.276862542093809,1.93475751247217,11.1518115320709));
#67779=CARTESIAN_POINT('Ctrl Pts',(0.281998506430586,1.94399182776937,11.152474737774));
#67780=CARTESIAN_POINT('Ctrl Pts',(0.28235080702904,1.94463034650834,11.1525203771726));
#67781=CARTESIAN_POINT('Ctrl Pts',(0.282838351275772,1.94552111929646,11.1525837369018));
#67782=CARTESIAN_POINT('Ctrl Pts',(0.282975427445434,1.94577235980716,11.1526015731464));
#67783=CARTESIAN_POINT('Ctrl Pts',(0.283211136270214,1.94620575165398,11.1526322814067));
#67784=CARTESIAN_POINT('Ctrl Pts',(0.283309928013786,1.94638781551856,11.1526451636222));
#67785=CARTESIAN_POINT('Ctrl Pts',(0.283514427702919,1.94676555748459,11.1526718537622));
#67786=CARTESIAN_POINT('Ctrl Pts',(0.283620108458385,1.94696124945941,11.1526856598679));
#67787=CARTESIAN_POINT('Ctrl Pts',(0.283869410557732,1.94742403419987,11.1527182603433));
#67788=CARTESIAN_POINT('Ctrl Pts',(0.284012858109618,1.94769122145967,11.1527370435491));
#67789=CARTESIAN_POINT('Ctrl Pts',(0.284484656637369,1.94857298366152,11.1527989054581));
#67790=CARTESIAN_POINT('Ctrl Pts',(0.284811394511033,1.94918842644795,11.1528418819509));
#67791=CARTESIAN_POINT('Ctrl Pts',(0.29165395039516,1.96217859959539,11.153744858478));
#67792=CARTESIAN_POINT('Ctrl Pts',(0.297360377069753,1.97496527303764,11.1545550935495));
#67793=CARTESIAN_POINT('Ctrl Pts',(0.313884725756788,2.01958768505058,11.1572540602539));
#67794=CARTESIAN_POINT('Ctrl Pts',(0.320553073793347,2.05271880752622,11.1590699414324));
#67795=CARTESIAN_POINT('Ctrl Pts',(0.322085127160976,2.08868147677592,11.1612285137931));
#67796=CARTESIAN_POINT('Ctrl Pts',(0.32216049744579,2.09108083412663,11.1613732673326));
#67797=CARTESIAN_POINT('Ctrl Pts',(0.322239605059702,2.09499067569081,11.1616104480026));
#67798=CARTESIAN_POINT('Ctrl Pts',(0.322259540798553,2.09650076545826,11.1617023692229));
#67799=CARTESIAN_POINT('Ctrl Pts',(0.32227222932597,2.09855654849124,11.1618279543588));
#67800=CARTESIAN_POINT('Ctrl Pts',(0.322274211292739,2.099102182169,11.1618613292478));
#67801=CARTESIAN_POINT('Ctrl Pts',(0.322275223682472,2.10002859379283,11.1619180689192));
#67802=CARTESIAN_POINT('Ctrl Pts',(0.322274964945271,2.10040937110595,11.1619414114075));
#67803=CARTESIAN_POINT('Ctrl Pts',(0.322273095781549,2.10117174049117,11.1619881889911));
#67804=CARTESIAN_POINT('Ctrl Pts',(0.322271482446517,2.10155333196045,11.1620116241413));
#67805=CARTESIAN_POINT('Ctrl Pts',(0.322266267738438,2.10242186458755,11.162065013517));
#67806=CARTESIAN_POINT('Ctrl Pts',(0.322262240451007,2.10290880138403,11.1620949810332));
#67807=CARTESIAN_POINT('Ctrl Pts',(0.322246977394136,2.10435727807169,11.1621842300725));
#67808=CARTESIAN_POINT('Ctrl Pts',(0.3222325417138,2.10531877245459,11.1622436116892));
#67809=CARTESIAN_POINT('Ctrl Pts',(0.322189905118657,2.10750630536493,11.1623790335668));
#67810=CARTESIAN_POINT('Ctrl Pts',(0.32215900881206,2.10873227089407,11.1624551575809));
#67811=CARTESIAN_POINT('Ctrl Pts',(0.321503220180181,2.12994566825458,11.1637764065909));
#67812=CARTESIAN_POINT('Ctrl Pts',(0.319026501717544,2.14982859651757,11.1650811496727));
#67813=CARTESIAN_POINT('Ctrl Pts',(0.308585551081056,2.19721124704738,11.1683336249915));
#67814=CARTESIAN_POINT('Ctrl Pts',(0.298774269560823,2.22413351992096,11.1703094168567));
#67815=CARTESIAN_POINT('Ctrl Pts',(0.284856885159457,2.25073136570968,11.1722078420144));
#67816=CARTESIAN_POINT('Ctrl Pts',(0.284157902583248,2.25204498095543,11.1723014206999));
#67817=CARTESIAN_POINT('Ctrl Pts',(0.283247475481208,2.25372775968843,11.1724210184171));
#67818=CARTESIAN_POINT('Ctrl Pts',(0.283044378329125,2.25410138340238,11.1724475546315));
#67819=CARTESIAN_POINT('Ctrl Pts',(0.282721421815863,2.25469271162721,11.1724895234929));
#67820=CARTESIAN_POINT('Ctrl Pts',(0.282602050054987,2.25491067971539,11.1725049871528));
#67821=CARTESIAN_POINT('Ctrl Pts',(0.282387706101224,2.25530099094743,11.1725326658846));
#67822=CARTESIAN_POINT('Ctrl Pts',(0.282292828877308,2.25547338393156,11.1725448869095));
#67823=CARTESIAN_POINT('Ctrl Pts',(0.282069400650137,2.2558784767551,11.172573594508));
#67824=CARTESIAN_POINT('Ctrl Pts',(0.28194071975812,2.25611110416018,11.1725900725981));
#67825=CARTESIAN_POINT('Ctrl Pts',(0.28156689170883,2.25678493510139,11.1726377823765));
#67826=CARTESIAN_POINT('Ctrl Pts',(0.281320994312782,2.25722572483017,11.172668966038));
#67827=CARTESIAN_POINT('Ctrl Pts',(0.279616040169678,2.26026517893233,11.172883825757));
#67828=CARTESIAN_POINT('Ctrl Pts',(0.278121972265919,2.26284418187908,11.1730652947945));
#67829=CARTESIAN_POINT('Ctrl Pts',(0.273333523543109,2.27085162051902,11.1736272681463));
#67830=CARTESIAN_POINT('Ctrl Pts',(0.269914203680284,2.27620393033147,11.174000771798));
#67831=CARTESIAN_POINT('Ctrl Pts',(0.257752745426355,2.29405474722714,11.1752514271106));
#67832=CARTESIAN_POINT('Ctrl Pts',(0.248282504099237,2.30603296205102,11.1760999098117));
#67833=CARTESIAN_POINT('Ctrl Pts',(0.221156571177228,2.33574332645426,11.1783489491363));
#67834=CARTESIAN_POINT('Ctrl Pts',(0.202229380756787,2.35216697703358,11.1797551868193));
#67835=CARTESIAN_POINT('Ctrl Pts',(0.179922596490352,2.36738201859145,11.1813875425534));
#67836=CARTESIAN_POINT('Ctrl Pts',(0.178237281197064,2.36850839073381,11.1815106690491));
#67837=CARTESIAN_POINT('Ctrl Pts',(0.175968427178553,2.36999399520502,11.1816762042101));
#67838=CARTESIAN_POINT('Ctrl Pts',(0.175394181580329,2.37036739053891,11.1817180820357));
#67839=CARTESIAN_POINT('Ctrl Pts',(0.174494435259594,2.37094836542319,11.1817836695924));
#67840=CARTESIAN_POINT('Ctrl Pts',(0.174169742201446,2.37115719714116,11.1818073326218));
#67841=CARTESIAN_POINT('Ctrl Pts',(0.173520135129708,2.3715733545157,11.1818546638438));
#67842=CARTESIAN_POINT('Ctrl Pts',(0.173195222840069,2.37178068173016,11.1818783319284));
#67843=CARTESIAN_POINT('Ctrl Pts',(0.172466555108044,2.37224380883074,11.1819313995992));
#67844=CARTESIAN_POINT('Ctrl Pts',(0.172062601591138,2.37249929395738,11.1819608107834));
#67845=CARTESIAN_POINT('Ctrl Pts',(0.170880352858381,2.37324334405928,11.1820468657141));
#67846=CARTESIAN_POINT('Ctrl Pts',(0.17010053937595,2.37372947693246,11.1821035991339));
#67847=CARTESIAN_POINT('Ctrl Pts',(0.168331705417179,2.37482168410834,11.1822322267473));
#67848=CARTESIAN_POINT('Ctrl Pts',(0.167341474578119,2.37542576483375,11.1823041933915));
#67849=CARTESIAN_POINT('Ctrl Pts',(0.164179170187885,2.37733154889983,11.1825338985548));
#67850=CARTESIAN_POINT('Ctrl Pts',(0.161995047655948,2.37861297867182,11.1826923710873));
#67851=CARTESIAN_POINT('Ctrl Pts',(0.153481426301801,2.38347398822047,11.1833095203347));
#67852=CARTESIAN_POINT('Ctrl Pts',(0.147046978135979,2.38686446794562,11.1837748103081));
#67853=CARTESIAN_POINT('Ctrl Pts',(0.128654760880419,2.3957743667495,11.185101971699));
#67854=CARTESIAN_POINT('Ctrl Pts',(0.116466245112043,2.40078244236685,11.1859787824058));
#67855=CARTESIAN_POINT('Ctrl Pts',(0.0796325709258978,2.41334166493395,
11.1886009359856));
#67856=CARTESIAN_POINT('Ctrl Pts',(0.0543486863065345,2.41870168158942,
11.1903719732322));
#67857=CARTESIAN_POINT('Ctrl Pts',(0.0272812749704597,2.42112135170366,
11.1920895017625));
#67858=CARTESIAN_POINT('Ctrl Pts',(0.0258666048432852,2.42123839965724,
11.192178737775));
#67859=CARTESIAN_POINT('Ctrl Pts',(0.02403477896752,2.42137778301569,11.1922935616967));
#67860=CARTESIAN_POINT('Ctrl Pts',(0.023618317034262,2.42140865750825,11.1923196181675));
#67861=CARTESIAN_POINT('Ctrl Pts',(0.0229802009126081,2.42145471741773,
11.1923594671744));
#67862=CARTESIAN_POINT('Ctrl Pts',(0.0227585910815346,2.42147048311903,
11.1923732922878));
#67863=CARTESIAN_POINT('Ctrl Pts',(0.0223216154817358,2.42150111618827,
11.1924005252316));
#67864=CARTESIAN_POINT('Ctrl Pts',(0.0221062523520976,2.42151599623583,
11.1924139336489));
#67865=CARTESIAN_POINT('Ctrl Pts',(0.0216259129545834,2.42154869933305,
11.1924438097529));
#67866=CARTESIAN_POINT('Ctrl Pts',(0.0213609302254168,2.42156641120462,
11.1924602710655));
#67867=CARTESIAN_POINT('Ctrl Pts',(0.0205935547748246,2.42161675110045,
11.1925078848268));
#67868=CARTESIAN_POINT('Ctrl Pts',(0.0200911042269686,2.42164852964958,
11.1925389895467));
#67869=CARTESIAN_POINT('Ctrl Pts',(0.0166419652946308,2.42185856417759,
11.1927520367056));
#67870=CARTESIAN_POINT('Ctrl Pts',(0.0136929007994413,2.42199750977293,
11.1929318144236));
#67871=CARTESIAN_POINT('Ctrl Pts',(0.0044383185330517,2.4223061592897,11.193489681011));
#67872=CARTESIAN_POINT('Ctrl Pts',(-0.00187083683493692,2.42233130450191,
11.1938608401677));
#67873=CARTESIAN_POINT('Ctrl Pts',(-0.0163995557725327,2.4219625489532,
11.1947026508984));
#67874=CARTESIAN_POINT('Ctrl Pts',(-0.0246114516756555,2.42143913584733,
11.1951689748867));
#67875=CARTESIAN_POINT('Ctrl Pts',(-0.0351547796587503,2.42036064899454,
11.1957650207563));
#67876=CARTESIAN_POINT('Ctrl Pts',(-0.0375121522217631,2.42009317789086,
11.195898112615));
#67877=CARTESIAN_POINT('Ctrl Pts',(-0.0418937100685406,2.41954697097701,
11.1961454641326));
#67878=CARTESIAN_POINT('Ctrl Pts',(-0.0439186067174756,2.41927496869533,
11.1962597668203));
#67879=CARTESIAN_POINT('Ctrl Pts',(-0.0638294318043176,2.41640736494172,
11.1973846302653));
#67880=CARTESIAN_POINT('Ctrl Pts',(-0.0814690164902492,2.41233085379869,
11.1983907870723));
#67881=CARTESIAN_POINT('Ctrl Pts',(-0.100618705595673,2.40617189574131,
11.1995566211787));
#67882=CARTESIAN_POINT('Ctrl Pts',(-0.102558538860407,2.40552757572936,
11.1996755550277));
#67883=CARTESIAN_POINT('Ctrl Pts',(-0.106836055389708,2.40406146176682,
11.199939800347));
#67884=CARTESIAN_POINT('Ctrl Pts',(-0.109170637815719,2.40323107797723,
11.2000853432664));
#67885=CARTESIAN_POINT('Ctrl Pts',(-0.11755954849835,2.40013780571722,11.2006134550837));
#67886=CARTESIAN_POINT('Ctrl Pts',(-0.123554730358445,2.39771995155523,
11.2010006241662));
#67887=CARTESIAN_POINT('Ctrl Pts',(-0.130417294100534,2.39470929511149,
11.2014567271557));
#67888=CARTESIAN_POINT('Ctrl Pts',(-0.131359714293648,2.39429044267108,
11.2015196490164));
#67889=CARTESIAN_POINT('Ctrl Pts',(-0.132759053095792,2.39366045490954,
11.2016135103359));
#67890=CARTESIAN_POINT('Ctrl Pts',(-0.133217520149066,2.39345275816962,
11.2016443316423));
#67891=CARTESIAN_POINT('Ctrl Pts',(-0.134033404477511,2.39308083667459,
11.2016993055327));
#67892=CARTESIAN_POINT('Ctrl Pts',(-0.134391011972061,2.39291702961872,
11.2017234436921));
#67893=CARTESIAN_POINT('Ctrl Pts',(-0.135081400093194,2.39259925738513,
11.2017701272468));
#67894=CARTESIAN_POINT('Ctrl Pts',(-0.135414219765039,2.39244537807448,
11.2017926696489));
#67895=CARTESIAN_POINT('Ctrl Pts',(-0.13632040550142,2.39202452413079,11.2018541493673));
#67896=CARTESIAN_POINT('Ctrl Pts',(-0.136893247206196,2.3917564301093,11.2018931253493));
#67897=CARTESIAN_POINT('Ctrl Pts',(-0.1391180957658,2.39070719009987,11.2020449417559));
#67898=CARTESIAN_POINT('Ctrl Pts',(-0.140764211166632,2.38991369677706,
11.20215820977));
#67899=CARTESIAN_POINT('Ctrl Pts',(-0.144850628005584,2.3879008731621,11.2024417902872));
#67900=CARTESIAN_POINT('Ctrl Pts',(-0.147282327270247,2.38666449472945,
11.202612693031));
#67901=CARTESIAN_POINT('Ctrl Pts',(-0.156816333497679,2.38166367362775,
11.2032914477006));
#67902=CARTESIAN_POINT('Ctrl Pts',(-0.16379195800011,2.37766520122641,11.2038074154449));
#67903=CARTESIAN_POINT('Ctrl Pts',(-0.176650172920616,2.36964156864037,
11.2047957960116));
#67904=CARTESIAN_POINT('Ctrl Pts',(-0.182563094925284,2.36567379508756,
11.2052661636137));
#67905=CARTESIAN_POINT('Ctrl Pts',(-0.210308784578101,2.34569163092447,
11.2075470149174));
#67906=CARTESIAN_POINT('Ctrl Pts',(-0.230195878789479,2.32716512388663,
11.2094200873821));
#67907=CARTESIAN_POINT('Ctrl Pts',(-0.247662065263262,2.30621522266743,
11.2111860568691));
#67908=CARTESIAN_POINT('Ctrl Pts',(-0.247791589476958,2.30605956618204,
11.2111991598836));
#67909=CARTESIAN_POINT('Ctrl Pts',(-0.248089630244186,2.30570070656009,
11.2112293266428));
#67910=CARTESIAN_POINT('Ctrl Pts',(-0.248258044236419,2.30549741795663,
11.2112463849195));
#67911=CARTESIAN_POINT('Ctrl Pts',(-0.251145595213711,2.30200319204345,
11.2115390605021));
#67912=CARTESIAN_POINT('Ctrl Pts',(-0.253799495321363,2.29865855167063,
11.2118111382571));
#67913=CARTESIAN_POINT('Ctrl Pts',(-0.256716433460838,2.29482850226574,
11.2121128142802));
#67914=CARTESIAN_POINT('Ctrl Pts',(-0.257045463295528,2.29439419310629,
11.2121468821952));
#67915=CARTESIAN_POINT('Ctrl Pts',(-0.257540935355721,2.29373672790081,
11.212198239991));
#67916=CARTESIAN_POINT('Ctrl Pts',(-0.257708190424643,2.29351418994768,
11.2122155864644));
#67917=CARTESIAN_POINT('Ctrl Pts',(-0.257998178775376,2.29312730890536,
11.2122456785265));
#67918=CARTESIAN_POINT('Ctrl Pts',(-0.258121043541063,2.29296306532144,
11.2122584333852));
#67919=CARTESIAN_POINT('Ctrl Pts',(-0.258377728025089,2.29261924991804,
11.2122850910418));
#67920=CARTESIAN_POINT('Ctrl Pts',(-0.258511517298682,2.2924396560033,11.2122989916365));
#67921=CARTESIAN_POINT('Ctrl Pts',(-0.258831157502417,2.29200964761838,
11.2123322169018));
#67922=CARTESIAN_POINT('Ctrl Pts',(-0.259016833025361,2.29175910169806,
11.2123515292061));
#67923=CARTESIAN_POINT('Ctrl Pts',(-0.259645523864615,2.29090818282496,
11.2124169626358));
#67924=CARTESIAN_POINT('Ctrl Pts',(-0.260086822032264,2.29030653526275,
11.2124629645414));
#67925=CARTESIAN_POINT('Ctrl Pts',(-0.268088613375624,2.27931740455733,
11.213298517819));
#67926=CARTESIAN_POINT('Ctrl Pts',(-0.275024432899713,2.26848705185273,
11.2140462713635));
#67927=CARTESIAN_POINT('Ctrl Pts',(-0.292880680164075,2.23654908737248,
11.2161293400547));
#67928=CARTESIAN_POINT('Ctrl Pts',(-0.302140674970359,2.21461159974322,
11.2174241064268));
#67929=CARTESIAN_POINT('Ctrl Pts',(-0.309548391236215,2.18969965145635,
11.2189136991572));
#67930=CARTESIAN_POINT('Ctrl Pts',(-0.310166834987415,2.18753723888272,
11.2190430949091));
#67931=CARTESIAN_POINT('Ctrl Pts',(-0.313810715440795,2.1742726163118,11.2198379475692));
#67932=CARTESIAN_POINT('Ctrl Pts',(-0.316262076377164,2.16302253524376,
11.2205172739084));
#67933=CARTESIAN_POINT('Ctrl Pts',(-0.318299394224182,2.15047889144871,
11.2212897620399));
#67934=CARTESIAN_POINT('Ctrl Pts',(-0.318485604562547,2.14929038922978,
11.2213630975516));
#67935=CARTESIAN_POINT('Ctrl Pts',(-0.318737164351746,2.14762382239962,
11.2214661403069));
#67936=CARTESIAN_POINT('Ctrl Pts',(-0.318808102795438,2.1471466010113,11.221495670528));
#67937=CARTESIAN_POINT('Ctrl Pts',(-0.318935995832331,2.14627274307627,
11.2215497889005));
#67938=CARTESIAN_POINT('Ctrl Pts',(-0.318993282907696,2.14587615553678,
11.2215743664815));
#67939=CARTESIAN_POINT('Ctrl Pts',(-0.319101766146809,2.14511511843883,
11.2216215625014));
#67940=CARTESIAN_POINT('Ctrl Pts',(-0.319153077988528,2.14475068578719,
11.2216441772396));
#67941=CARTESIAN_POINT('Ctrl Pts',(-0.319258908054122,2.14398960733594,
11.221691435867));
#67942=CARTESIAN_POINT('Ctrl Pts',(-0.319313311565178,2.14359294645298,
11.2217160833448));
#67943=CARTESIAN_POINT('Ctrl Pts',(-0.319439626120075,2.14265905157697,
11.2217741538407));
#67944=CARTESIAN_POINT('Ctrl Pts',(-0.319510921106644,2.14212173672847,
11.221807596281));
#67945=CARTESIAN_POINT('Ctrl Pts',(-0.319694872427188,2.1407080446414,11.2218956688574));
#67946=CARTESIAN_POINT('Ctrl Pts',(-0.319805280096866,2.13983138400767,
11.2219503698759));
#67947=CARTESIAN_POINT('Ctrl Pts',(-0.321495713817078,2.12594869728428,
11.222817986632));
#67948=CARTESIAN_POINT('Ctrl Pts',(-0.32228455980763,2.11286066814297,11.2236558602518));
#67949=CARTESIAN_POINT('Ctrl Pts',(-0.322274912584447,2.09976263174766,
11.2245149816093));
#67950=CARTESIAN_POINT('',(-0.322274869595754,2.100295846535,11.4747410785928));
#67951=CARTESIAN_POINT('Ctrl Pts',(-0.322274912883247,2.0997630377757,11.2245149549773));
#67952=CARTESIAN_POINT('Ctrl Pts',(-0.322257167869846,2.07562934868397,
11.2260979218609));
#67953=CARTESIAN_POINT('Ctrl Pts',(-0.319528452590636,2.05157412299925,
11.2277513364805));
#67954=CARTESIAN_POINT('Ctrl Pts',(-0.311483480343985,2.01644805456151,
11.2301667567537));
#67955=CARTESIAN_POINT('Ctrl Pts',(-0.308184629440469,2.00499902034208,
11.2309525967105));
#67956=CARTESIAN_POINT('Ctrl Pts',(-0.303911148762247,1.99276052604722,
11.2317729952443));
#67957=CARTESIAN_POINT('Ctrl Pts',(-0.303558063396941,1.99176510112813,
11.2318395761317));
#67958=CARTESIAN_POINT('Ctrl Pts',(-0.302942032987554,1.99005510487359,
11.2319536776715));
#67959=CARTESIAN_POINT('Ctrl Pts',(-0.302681440042532,1.98933970361187,
11.2320013305429));
#67960=CARTESIAN_POINT('Ctrl Pts',(-0.302309650396511,1.98833017523488,
11.2320684508034));
#67961=CARTESIAN_POINT('Ctrl Pts',(-0.302200557391591,1.98803528412861,
11.2320880421188));
#67962=CARTESIAN_POINT('Ctrl Pts',(-0.302012854502684,1.98753017422174,
11.2321215731145));
#67963=CARTESIAN_POINT('Ctrl Pts',(-0.301934456415664,1.98731987741595,
11.2321355255213));
#67964=CARTESIAN_POINT('Ctrl Pts',(-0.301784177725824,1.9869180494076,11.2321621700806));
#67965=CARTESIAN_POINT('Ctrl Pts',(-0.301712334521615,1.98672650498237,
11.2321748644755));
#67966=CARTESIAN_POINT('Ctrl Pts',(-0.301543047730908,1.98627646547573,
11.2322046751093));
#67967=CARTESIAN_POINT('Ctrl Pts',(-0.301445453870973,1.98601802650689,
11.2322217822912));
#67968=CARTESIAN_POINT('Ctrl Pts',(-0.301157318252216,1.98525797103119,
11.2322720596991));
#67969=CARTESIAN_POINT('Ctrl Pts',(-0.300965854689481,1.98475670141155,
11.2323051749995));
#67970=CARTESIAN_POINT('Ctrl Pts',(-0.299318688184017,1.98047636682896,
11.2325875928504));
#67971=CARTESIAN_POINT('Ctrl Pts',(-0.29779304371687,1.97672436254925,11.2328327953071));
#67972=CARTESIAN_POINT('Ctrl Pts',(-0.296023082510531,1.97259629120257,
11.2331010007329));
#67973=CARTESIAN_POINT('Ctrl Pts',(-0.295848336032624,1.97219103135824,
11.2331273139276));
#67974=CARTESIAN_POINT('Ctrl Pts',(-0.283624759562947,1.94400236081858,
11.2349564830699));
#67975=CARTESIAN_POINT('Ctrl Pts',(-0.267719471077407,1.91805198310139,
11.2365783853178));
#67976=CARTESIAN_POINT('Ctrl Pts',(-0.243934627392196,1.88927101815344,
11.2387041703094));
#67977=CARTESIAN_POINT('Ctrl Pts',(-0.239270176327684,1.88398939690268,
11.2391094837015));
#67978=CARTESIAN_POINT('Ctrl Pts',(-0.228471273512003,1.8725409209569,11.2400288599434));
#67979=CARTESIAN_POINT('Ctrl Pts',(-0.22225296988535,1.86646124084567,11.2405458271256));
#67980=CARTESIAN_POINT('Ctrl Pts',(-0.214875712963193,1.85981019588915,
11.2411494126321));
#67981=CARTESIAN_POINT('Ctrl Pts',(-0.213949728487726,1.85898500537721,
11.2412250040009));
#67982=CARTESIAN_POINT('Ctrl Pts',(-0.212699250071877,1.85788352756138,
11.2413268671389));
#67983=CARTESIAN_POINT('Ctrl Pts',(-0.212378929457911,1.85760250098894,
11.2413529411975));
#67984=CARTESIAN_POINT('Ctrl Pts',(-0.211781971716141,1.85708086427266,
11.2414014986026));
#67985=CARTESIAN_POINT('Ctrl Pts',(-0.211505479232515,1.85684008903736,
11.2414239750444));
#67986=CARTESIAN_POINT('Ctrl Pts',(-0.210931433715147,1.85634191848747,
11.2414706116191));
#67987=CARTESIAN_POINT('Ctrl Pts',(-0.21063381914024,1.85608459530462,11.2414947746824));
#67988=CARTESIAN_POINT('Ctrl Pts',(-0.209953811668142,1.85549882066492,
11.2415499485096));
#67989=CARTESIAN_POINT('Ctrl Pts',(-0.209571118545734,1.85517072071112,
11.2415809736993));
#67990=CARTESIAN_POINT('Ctrl Pts',(-0.2084002012148,1.85417159779695,11.241675824477));
#67991=CARTESIAN_POINT('Ctrl Pts',(-0.207609518140649,1.85350347845571,
11.2417397690647));
#67992=CARTESIAN_POINT('Ctrl Pts',(-0.201795264100384,1.84863831137625,
11.2422092385638));
#67993=CARTESIAN_POINT('Ctrl Pts',(-0.196648388665452,1.84459164417501,
11.2426208209571));
#67994=CARTESIAN_POINT('Ctrl Pts',(-0.189495550032751,1.83931223572083,
11.2431881050269));
#67995=CARTESIAN_POINT('Ctrl Pts',(-0.187593837865329,1.83794041617636,
11.2433384873584));
#67996=CARTESIAN_POINT('Ctrl Pts',(-0.184035739725214,1.83543232224418,
11.2436190439595));
#67997=CARTESIAN_POINT('Ctrl Pts',(-0.182383362731027,1.83429053773368,
11.243749016994));
#67998=CARTESIAN_POINT('Ctrl Pts',(-0.168332390862551,1.82477420293039,
11.2448515396291));
#67999=CARTESIAN_POINT('Ctrl Pts',(-0.155376344667364,1.81725781901964,
11.2458517930096));
#68000=CARTESIAN_POINT('Ctrl Pts',(-0.13079968673523,1.80520045178729,11.2477007096753));
#68001=CARTESIAN_POINT('Ctrl Pts',(-0.119346105964983,1.8003804960653,11.2485444080226));
#68002=CARTESIAN_POINT('Ctrl Pts',(-0.0970106230450789,1.79246568542562,
11.2501299296301));
#68003=CARTESIAN_POINT('Ctrl Pts',(-0.086186609550036,1.7892584001102,11.2508728244769));
#68004=CARTESIAN_POINT('Ctrl Pts',(-0.0737025519997631,1.78626200338303,
11.2516850210315));
#68005=CARTESIAN_POINT('Ctrl Pts',(-0.0721868982699399,1.78590980810848,
11.2517828872688));
#68006=CARTESIAN_POINT('Ctrl Pts',(-0.0702658157767175,1.78547804323444,
11.2519059453327));
#68007=CARTESIAN_POINT('Ctrl Pts',(-0.0698627378677819,1.78538826465537,
11.2519317103064));
#68008=CARTESIAN_POINT('Ctrl Pts',(-0.0692194963123179,1.7852462909575,
11.2519727380133));
#68009=CARTESIAN_POINT('Ctrl Pts',(-0.0689794453095743,1.78519359575845,
11.2519880294441));
#68010=CARTESIAN_POINT('Ctrl Pts',(-0.0685252521055096,1.78509443722911,
11.2520169243712));
#68011=CARTESIAN_POINT('Ctrl Pts',(-0.0683111245664494,1.78504791808762,
11.2520305309624));
#68012=CARTESIAN_POINT('Ctrl Pts',(-0.0678223976239946,1.78494226417037,
11.2520615509351));
#68013=CARTESIAN_POINT('Ctrl Pts',(-0.0675477687064621,1.78488327008905,
11.2520789561148));
#68014=CARTESIAN_POINT('Ctrl Pts',(-0.0667078168726211,1.78470398535475,
11.2521321119707));
#68015=CARTESIAN_POINT('Ctrl Pts',(-0.06614224326597,1.78458485554578,11.2521677962077));
#68016=CARTESIAN_POINT('Ctrl Pts',(-0.0620026591585345,1.78372453660465,
11.2524282111753));
#68017=CARTESIAN_POINT('Ctrl Pts',(-0.0584164268455472,1.78304255442916,
11.2526496340625));
#68018=CARTESIAN_POINT('Ctrl Pts',(-0.03055591582342,1.77823337656398,11.2543429452643));
#68019=CARTESIAN_POINT('Ctrl Pts',(-0.00588914584610395,1.7768389150058,
11.2556894071172));
#68020=CARTESIAN_POINT('Ctrl Pts',(0.0300302398492489,1.77892648370263,
11.2577077226902));
#68021=CARTESIAN_POINT('Ctrl Pts',(0.0413187149275944,1.78018324381883,
11.2583496134809));
#68022=CARTESIAN_POINT('Ctrl Pts',(0.0586195670072356,1.78304072566145,
11.2593649253089));
#68023=CARTESIAN_POINT('Ctrl Pts',(0.0646917388519135,1.78422411853641,
11.259727309717));
#68024=CARTESIAN_POINT('Ctrl Pts',(0.0740938039734348,1.78633903505189,
11.2603001699505));
#68025=CARTESIAN_POINT('Ctrl Pts',(0.077449270889123,1.7871506723797,11.260506972013));
#68026=CARTESIAN_POINT('Ctrl Pts',(0.0829176465982549,1.78856675578361,
11.2608481862337));
#68027=CARTESIAN_POINT('Ctrl Pts',(0.0850386049789374,1.78913919993995,
11.2609815698259));
#68028=CARTESIAN_POINT('Ctrl Pts',(0.0877992221061013,1.78991465356809,
11.2611565962173));
#68029=CARTESIAN_POINT('Ctrl Pts',(0.0884443672169454,1.79009804877814,
11.2611976005212));
#68030=CARTESIAN_POINT('Ctrl Pts',(0.0894979249321199,1.79040110114194,
11.2612647303043));
#68031=CARTESIAN_POINT('Ctrl Pts',(0.0899066835533084,1.79051955636749,
11.261290816564));
#68032=CARTESIAN_POINT('Ctrl Pts',(0.0906929159306681,1.79074908981536,
11.2613410725349));
#68033=CARTESIAN_POINT('Ctrl Pts',(0.0910704234621937,1.79086005043303,
11.2613652383682));
#68034=CARTESIAN_POINT('Ctrl Pts',(0.0919314357614094,1.7911148413918,11.261420436972));
#68035=CARTESIAN_POINT('Ctrl Pts',(0.0924148070601843,1.79125911589007,
11.2614514842156));
#68036=CARTESIAN_POINT('Ctrl Pts',(0.0938907790914673,1.79170343415643,
11.2615464678369));
#68037=CARTESIAN_POINT('Ctrl Pts',(0.0948822648417215,1.79200713208325,
11.2616105237025));
#68038=CARTESIAN_POINT('Ctrl Pts',(0.102159028085886,1.79427451951713,11.262082512362));
#68039=CARTESIAN_POINT('Ctrl Pts',(0.10838387406563,1.79642552484246,11.2624965759582));
#68040=CARTESIAN_POINT('Ctrl Pts',(0.116248919051294,1.79941604432397,11.2630335978392));
#68041=CARTESIAN_POINT('Ctrl Pts',(0.117954114325009,1.80008109047539,11.263150871693));
#68042=CARTESIAN_POINT('Ctrl Pts',(0.146771383088917,1.81160393129525,11.2651471377833));
#68043=CARTESIAN_POINT('Ctrl Pts',(0.172286652735094,1.82608235507904,11.2671494677046));
#68044=CARTESIAN_POINT('Ctrl Pts',(0.204971970430768,1.85102267464569,11.2699053832089));
#68045=CARTESIAN_POINT('Ctrl Pts',(0.214039640544268,1.85877331096139,11.2706921812367));
#68046=CARTESIAN_POINT('Ctrl Pts',(0.223816313852621,1.86811640709246,11.271548030196));
#68047=CARTESIAN_POINT('Ctrl Pts',(0.224966466390309,1.86923208139158,11.2716488355227));
#68048=CARTESIAN_POINT('Ctrl Pts',(0.226405540697228,1.87064900088079,11.2717750610047));
#68049=CARTESIAN_POINT('Ctrl Pts',(0.226702236821778,1.87094226605491,11.271801090384));
#68050=CARTESIAN_POINT('Ctrl Pts',(0.227173488688738,1.87140988095001,11.2718424408301));
#68051=CARTESIAN_POINT('Ctrl Pts',(0.227348413830684,1.87158385516791,11.2718577913799));
#68052=CARTESIAN_POINT('Ctrl Pts',(0.227678203862228,1.87191260655261,11.2718867347598));
#68053=CARTESIAN_POINT('Ctrl Pts',(0.227833109527904,1.87206733940324,11.2719003308286));
#68054=CARTESIAN_POINT('Ctrl Pts',(0.22818526800376,1.87241982269153,11.2719312424145));
#68055=CARTESIAN_POINT('Ctrl Pts',(0.22838242114157,1.87261767141523,11.2719485499423));
#68056=CARTESIAN_POINT('Ctrl Pts',(0.228981157206632,1.8732200842038,11.2720011181253));
#68057=CARTESIAN_POINT('Ctrl Pts',(0.229381926927629,1.87362546040922,11.272036314472));
#68058=CARTESIAN_POINT('Ctrl Pts',(0.232226322258109,1.87651785884341,11.2722862001482));
#68059=CARTESIAN_POINT('Ctrl Pts',(0.234630639580509,1.879043448759,11.2724978752574));
#68060=CARTESIAN_POINT('Ctrl Pts',(0.257991289299909,1.90439381299478,11.2745651011999));
#68061=CARTESIAN_POINT('Ctrl Pts',(0.275596164965768,1.9300922031378,11.2762218342607));
#68062=CARTESIAN_POINT('Ctrl Pts',(0.295710064412846,1.97104014851827,11.2788165890518));
#68063=CARTESIAN_POINT('Ctrl Pts',(0.301256481100086,1.9845897037151,11.2796664942681));
#68064=CARTESIAN_POINT('Ctrl Pts',(0.306356744928255,1.99995414673547,11.2806434453885));
#68065=CARTESIAN_POINT('Ctrl Pts',(0.306839257642292,2.00144393598077,11.2807382945257));
#68066=CARTESIAN_POINT('Ctrl Pts',(0.307664227776886,2.00405587594661,11.2809048243429));
#68067=CARTESIAN_POINT('Ctrl Pts',(0.308011453500283,2.00517649843207,11.2809763480761));
#68068=CARTESIAN_POINT('Ctrl Pts',(0.308506226462004,2.00680470380926,11.2810803869012));
#68069=CARTESIAN_POINT('Ctrl Pts',(0.308658658701833,2.00731080213404,11.2811127420596));
#68070=CARTESIAN_POINT('Ctrl Pts',(0.30892184219017,2.00819246025817,11.2811691366466));
#68071=CARTESIAN_POINT('Ctrl Pts',(0.309033155635182,2.00856785219853,11.2811931576518));
#68072=CARTESIAN_POINT('Ctrl Pts',(0.309247806959349,2.00929660942484,11.2812398086958));
#68073=CARTESIAN_POINT('Ctrl Pts',(0.309351224022832,2.00964995094177,11.2812624361087));
#68074=CARTESIAN_POINT('Ctrl Pts',(0.309593177179976,2.01048190945071,11.2813157335523));
#68075=CARTESIAN_POINT('Ctrl Pts',(0.309731208926827,2.01096067102533,11.2813464199739));
#68076=CARTESIAN_POINT('Ctrl Pts',(0.31020349724187,2.01261318549312,11.2814523939515));
#68077=CARTESIAN_POINT('Ctrl Pts',(0.310532193280485,2.01378850470286,11.2815278622122));
#68078=CARTESIAN_POINT('Ctrl Pts',(0.314402545366612,2.02793708354436,11.2824375688188));
#68079=CARTESIAN_POINT('Ctrl Pts',(0.317135030240786,2.04111611572456,11.2832980494071));
#68080=CARTESIAN_POINT('Ctrl Pts',(0.322742264988997,2.0803688734147,11.2859013645669));
#68081=CARTESIAN_POINT('Ctrl Pts',(0.323269632531096,2.10666646822778,11.2877051827109));
#68082=CARTESIAN_POINT('Ctrl Pts',(0.319617273894639,2.14244057510283,11.29009909489));
#68083=CARTESIAN_POINT('Ctrl Pts',(0.318185586963727,2.15209968310979,11.2907379834616));
#68084=CARTESIAN_POINT('Ctrl Pts',(0.316043172614847,2.16308679297468,11.2914453740954));
#68085=CARTESIAN_POINT('Ctrl Pts',(0.315759436189301,2.16449193006609,11.2915354728));
#68086=CARTESIAN_POINT('Ctrl Pts',(0.31538429782932,2.16628786658685,11.2916501158366));
#68087=CARTESIAN_POINT('Ctrl Pts',(0.315301534410007,2.16668042423969,11.2916751431238));
#68088=CARTESIAN_POINT('Ctrl Pts',(0.315167436732576,2.16731063482504,11.2917152700823));
#68089=CARTESIAN_POINT('Ctrl Pts',(0.315116566530907,2.16754838440588,11.2917303963055));
#68090=CARTESIAN_POINT('Ctrl Pts',(0.315019214972943,2.16800086833013,11.2917591616201));
#68091=CARTESIAN_POINT('Ctrl Pts',(0.314972783464189,2.16821561091787,11.2917728033984));
#68092=CARTESIAN_POINT('Ctrl Pts',(0.314866479012346,2.16870483931604,11.2918038600185));
#68093=CARTESIAN_POINT('Ctrl Pts',(0.31480646681093,2.16897929404199,11.291821266724));
#68094=CARTESIAN_POINT('Ctrl Pts',(0.314618535360809,2.16983341035285,11.2918753886939));
#68095=CARTESIAN_POINT('Ctrl Pts',(0.31448937248105,2.17041280142002,11.2919120327856));
#68096=CARTESIAN_POINT('Ctrl Pts',(0.313478347910406,2.17488971435916,11.2921946636391));
#68097=CARTESIAN_POINT('Ctrl Pts',(0.312525617069997,2.17877109973992,11.2924366761619));
#68098=CARTESIAN_POINT('Ctrl Pts',(0.30799726752279,2.19584137804758,11.2934916812047));
#68099=CARTESIAN_POINT('Ctrl Pts',(0.303656822016394,2.20881406188279,11.294268873093));
#68100=CARTESIAN_POINT('Ctrl Pts',(0.290351415807177,2.24151046574074,11.2962528514013));
#68101=CARTESIAN_POINT('Ctrl Pts',(0.280201191802749,2.2606748753388,11.2974441550979));
#68102=CARTESIAN_POINT('Ctrl Pts',(0.262493935972236,2.28725469291956,11.2992912576973));
#68103=CARTESIAN_POINT('Ctrl Pts',(0.256372492668453,2.29555178005256,11.2998989495893));
#68104=CARTESIAN_POINT('Ctrl Pts',(0.249059496054933,2.3045291371305,11.3005995906683));
#68105=CARTESIAN_POINT('Ctrl Pts',(0.248248573686606,2.30551264219229,11.3006769543108));
#68106=CARTESIAN_POINT('Ctrl Pts',(0.246982526573189,2.30702970550629,11.3007972441958));
#68107=CARTESIAN_POINT('Ctrl Pts',(0.246531453051886,2.30756663999412,11.3008400059698));
#68108=CARTESIAN_POINT('Ctrl Pts',(0.245700304824471,2.30854946441163,11.3009186261479));
#68109=CARTESIAN_POINT('Ctrl Pts',(0.24532075895096,2.30899579928265,11.3009544628246));
#68110=CARTESIAN_POINT('Ctrl Pts',(0.244671769330094,2.30975478843058,11.3010156303718));
#68111=CARTESIAN_POINT('Ctrl Pts',(0.244402937250365,2.31006796575765,11.3010409359902));
#68112=CARTESIAN_POINT('Ctrl Pts',(0.243873813643848,2.31068198047981,11.3010906811962));
#68113=CARTESIAN_POINT('Ctrl Pts',(0.243613565174485,2.31098285413941,11.3011151189757));
#68114=CARTESIAN_POINT('Ctrl Pts',(0.24300875987902,2.31167945949151,11.3011718438711));
#68115=CARTESIAN_POINT('Ctrl Pts',(0.242663793045512,2.31207483228363,11.3012041479994));
#68116=CARTESIAN_POINT('Ctrl Pts',(0.241544851271979,2.31335096725937,11.3013087690935));
#68117=CARTESIAN_POINT('Ctrl Pts',(0.240767041588981,2.31422834087198,11.3013812461048));
#68118=CARTESIAN_POINT('Ctrl Pts',(0.23307386710797,2.32281146512357,11.3020957210278));
#68119=CARTESIAN_POINT('Ctrl Pts',(0.225796459080732,2.33018317935379,11.3027531061938));
#68120=CARTESIAN_POINT('Ctrl Pts',(0.197347848397992,2.35635129128395,11.3052610380192));
#68121=CARTESIAN_POINT('Ctrl Pts',(0.174086138107179,2.37268248188999,11.3072069488528));
#68122=CARTESIAN_POINT('Ctrl Pts',(0.138576019735989,2.39119753100971,11.3098822932387));
#68123=CARTESIAN_POINT('Ctrl Pts',(0.127863449913641,2.39605797217822,11.3106536980132));
#68124=CARTESIAN_POINT('Ctrl Pts',(0.116213653022638,2.40059294347934,11.3114383495289));
#68125=CARTESIAN_POINT('Ctrl Pts',(0.115518351187812,2.40086083391411,11.311484978988));
#68126=CARTESIAN_POINT('Ctrl Pts',(0.114530898660844,2.40123735826879,11.3115509095041));
#68127=CARTESIAN_POINT('Ctrl Pts',(0.114239516564171,2.40134798094888,11.3115703286612));
#68128=CARTESIAN_POINT('Ctrl Pts',(0.11373852004471,2.40153735228262,11.3116036552946));
#68129=CARTESIAN_POINT('Ctrl Pts',(0.113528983575527,2.40161630535005,11.3116175751078));
#68130=CARTESIAN_POINT('Ctrl Pts',(0.113127313881231,2.40176717609063,11.3116442225777));
#68131=CARTESIAN_POINT('Ctrl Pts',(0.112935194565043,2.40183912857819,11.3116569523507));
#68132=CARTESIAN_POINT('Ctrl Pts',(0.112482077369429,2.40200833676204,11.3116869389236));
#68133=CARTESIAN_POINT('Ctrl Pts',(0.112221021355397,2.40210543783657,11.3117041863963));
#68134=CARTESIAN_POINT('Ctrl Pts',(0.111448374755254,2.40239168786539,11.3117551494511));
#68135=CARTESIAN_POINT('Ctrl Pts',(0.110936426235142,2.4025798778341,11.3117888079655));
#68136=CARTESIAN_POINT('Ctrl Pts',(0.106398522394149,2.40423492566739,11.3120862116029));
#68137=CARTESIAN_POINT('Ctrl Pts',(0.102343927612831,2.40562274192891,11.3123453622156));
#68138=CARTESIAN_POINT('Ctrl Pts',(0.0980224894931366,2.40700623894997,
11.3126158478163));
#68139=CARTESIAN_POINT('Ctrl Pts',(0.0977822626798492,2.40708283622927,
11.3126308654065));
#68140=CARTESIAN_POINT('Ctrl Pts',(0.0966090843650532,2.40745539258839,
11.3127041161562));
#68141=CARTESIAN_POINT('Ctrl Pts',(0.0956748679776952,2.40774738551964,
11.3127621702724));
#68142=CARTESIAN_POINT('Ctrl Pts',(0.0703085130019445,2.41554906524073,
11.3143313667764));
#68143=CARTESIAN_POINT('Ctrl Pts',(0.0450678822283201,2.42013075071515,
11.3157200024032));
#68144=CARTESIAN_POINT('Ctrl Pts',(0.00560066933125505,2.42252918148792,
11.3179496253073));
#68145=CARTESIAN_POINT('Ctrl Pts',(-0.00838631442558622,2.42246868166866,
11.3187497060787));
#68146=CARTESIAN_POINT('Ctrl Pts',(-0.0282407562157118,2.42109003106072,
11.3199289193568));
#68147=CARTESIAN_POINT('Ctrl Pts',(-0.0341443830088618,2.42051599415301,
11.3202849405618));
#68148=CARTESIAN_POINT('Ctrl Pts',(-0.0409504086324087,2.41966404680808,
11.3207027368468));
#68149=CARTESIAN_POINT('Ctrl Pts',(-0.0418717694873003,2.41954466617439,
11.3207594515585));
#68150=CARTESIAN_POINT('Ctrl Pts',(-0.0432707353759901,2.41935724793347,
11.3208458066171));
#68151=CARTESIAN_POINT('Ctrl Pts',(-0.0437487305075147,2.41929211847863,
11.3208753550211));
#68152=CARTESIAN_POINT('Ctrl Pts',(-0.0445770921586413,2.41917735461621,
11.3209266370696));
#68153=CARTESIAN_POINT('Ctrl Pts',(-0.0449275274405052,2.419128215803,11.3209483550046));
#68154=CARTESIAN_POINT('Ctrl Pts',(-0.0456553103582945,2.41902494194536,
11.3209935073609));
#68155=CARTESIAN_POINT('Ctrl Pts',(-0.0460326441284862,2.41897071436066,
11.3210169446802));
#68156=CARTESIAN_POINT('Ctrl Pts',(-0.046951383250179,2.41883701584333,
11.3210740768854));
#68157=CARTESIAN_POINT('Ctrl Pts',(-0.0474926826939706,2.41875683544925,
11.3211077941926));
#68158=CARTESIAN_POINT('Ctrl Pts',(-0.0495373726868952,2.41844864030113,
11.3212353718955));
#68159=CARTESIAN_POINT('Ctrl Pts',(-0.0510393287386378,2.41821136779986,
11.3213295252425));
#68160=CARTESIAN_POINT('Ctrl Pts',(-0.0770921258318028,2.41390646556157,
11.3229704965056));
#68161=CARTESIAN_POINT('Ctrl Pts',(-0.101086797606177,2.40702023379844,
11.3246122974463));
#68162=CARTESIAN_POINT('Ctrl Pts',(-0.138710738571104,2.39132966209393,
11.327364818185));
#68163=CARTESIAN_POINT('Ctrl Pts',(-0.152903697696493,2.38413751822651,
11.328446828231));
#68164=CARTESIAN_POINT('Ctrl Pts',(-0.173666221616018,2.37160837115654,
11.3300520978402));
#68165=CARTESIAN_POINT('Ctrl Pts',(-0.180653825076045,2.3670117722686,11.330596297387));
#68166=CARTESIAN_POINT('Ctrl Pts',(-0.188519344907763,2.36138734314269,
11.3312066561789));
#68167=CARTESIAN_POINT('Ctrl Pts',(-0.189578713243375,2.36062002644359,
11.3312888128107));
#68168=CARTESIAN_POINT('Ctrl Pts',(-0.190946334140453,2.35961668616787,
11.3313947790735));
#68169=CARTESIAN_POINT('Ctrl Pts',(-0.191258853566124,2.3593865401188,11.3314189872067));
#68170=CARTESIAN_POINT('Ctrl Pts',(-0.191764115654627,2.35901304459273,
11.3314581137563));
#68171=CARTESIAN_POINT('Ctrl Pts',(-0.191957113952789,2.35887004408742,
11.3314730564196));
#68172=CARTESIAN_POINT('Ctrl Pts',(-0.192327006519708,2.35859533411609,
11.3315016893146));
#68173=CARTESIAN_POINT('Ctrl Pts',(-0.192503924903201,2.35846365926477,
11.3315153818342));
#68174=CARTESIAN_POINT('Ctrl Pts',(-0.192910549194887,2.35816037234505,
11.3315468468583));
#68175=CARTESIAN_POINT('Ctrl Pts',(-0.193140162007362,2.3579886347522,11.3315646105313));
#68176=CARTESIAN_POINT('Ctrl Pts',(-0.193850792248245,2.35745564249114,
11.3316195760497));
#68177=CARTESIAN_POINT('Ctrl Pts',(-0.194331031122767,2.35709334464808,
11.3316567051538));
#68178=CARTESIAN_POINT('Ctrl Pts',(-0.198295633680705,2.35408494615743,
11.3319631153394));
#68179=CARTESIAN_POINT('Ctrl Pts',(-0.201727001701122,2.35136932905977,
11.332227619736));
#68180=CARTESIAN_POINT('Ctrl Pts',(-0.20587752965679,2.34794480990606,11.3325481729399));
#68181=CARTESIAN_POINT('Ctrl Pts',(-0.206649866688878,2.34730147314956,
11.3326078487002));
#68182=CARTESIAN_POINT('Ctrl Pts',(-0.20837924623776,2.3458471860078,11.3327415645579));
#68183=CARTESIAN_POINT('Ctrl Pts',(-0.209334593514034,2.34503423673766,
11.3328154966818));
#68184=CARTESIAN_POINT('Ctrl Pts',(-0.210800206431039,2.34377225130663,
11.3329290602555));
#68185=CARTESIAN_POINT('Ctrl Pts',(-0.211313829647995,2.34332715210315,
11.3329688859367));
#68186=CARTESIAN_POINT('Ctrl Pts',(-0.212446244318525,2.34233952653793,
11.3330567624215));
#68187=CARTESIAN_POINT('Ctrl Pts',(-0.213064374936227,2.34179624687297,
11.3331047768513));
#68188=CARTESIAN_POINT('Ctrl Pts',(-0.236477748626727,2.32105855934872,
11.3349255390429));
#68189=CARTESIAN_POINT('Ctrl Pts',(-0.256299221631263,2.29773633896801,
11.3365569851879));
#68190=CARTESIAN_POINT('Ctrl Pts',(-0.278381798287223,2.26273919428442,
11.338943891826));
#68191=CARTESIAN_POINT('Ctrl Pts',(-0.283736358910085,2.25321263410087,
11.33958659776));
#68192=CARTESIAN_POINT('Ctrl Pts',(-0.2894794297308,2.24165722459343,11.3403670821373));
#68193=CARTESIAN_POINT('Ctrl Pts',(-0.290345742613333,2.23987301022815,
11.3404876059498));
#68194=CARTESIAN_POINT('Ctrl Pts',(-0.291475806249693,2.23748984672977,
11.3406486459071));
#68195=CARTESIAN_POINT('Ctrl Pts',(-0.29175429411947,2.23689790150177,11.3406886506411));
#68196=CARTESIAN_POINT('Ctrl Pts',(-0.292209507155768,2.23592261670422,
11.3407545713113));
#68197=CARTESIAN_POINT('Ctrl Pts',(-0.292387285852208,2.23553976860403,
11.3407804507856));
#68198=CARTESIAN_POINT('Ctrl Pts',(-0.292730993831924,2.2347957671431,11.3408307481886));
#68199=CARTESIAN_POINT('Ctrl Pts',(-0.292897008268704,2.23443465377095,
11.3408551631245));
#68200=CARTESIAN_POINT('Ctrl Pts',(-0.293279756734901,2.23359802768407,
11.3409117332416));
#68201=CARTESIAN_POINT('Ctrl Pts',(-0.2934960025927,2.23312229403271,11.3409439051514));
#68202=CARTESIAN_POINT('Ctrl Pts',(-0.294074930190123,2.23184040535424,
11.3410306065643));
#68203=CARTESIAN_POINT('Ctrl Pts',(-0.29443545179984,2.23103328488892,11.3410852100494));
#68204=CARTESIAN_POINT('Ctrl Pts',(-0.297016792335192,2.22518984491185,
11.3414806416937));
#68205=CARTESIAN_POINT('Ctrl Pts',(-0.299111467723363,2.22009910922912,
11.3418257499965));
#68206=CARTESIAN_POINT('Ctrl Pts',(-0.312392693735311,2.18531545867443,
11.3441898417103));
#68207=CARTESIAN_POINT('Ctrl Pts',(-0.319269283773583,2.15416829051745,
11.3463611927753));
#68208=CARTESIAN_POINT('Ctrl Pts',(-0.322014613897808,2.11499428314519,
11.348996619342));
#68209=CARTESIAN_POINT('Ctrl Pts',(-0.322277630461605,2.10744195239842,
11.3494990518891));
#68210=CARTESIAN_POINT('Ctrl Pts',(-0.322274760262603,2.09926006986015,
11.3500329025093));
#68211=CARTESIAN_POINT('Ctrl Pts',(-0.322272711291937,2.0986331910827,11.3500737381608));
#68212=CARTESIAN_POINT('Ctrl Pts',(-0.322262647519997,2.09700643224205,
11.3501795272261));
#68213=CARTESIAN_POINT('Ctrl Pts',(-0.322251808357313,2.09600656880701,
11.3502443724598));
#68214=CARTESIAN_POINT('Ctrl Pts',(-0.322231286061559,2.0946821723725,11.3503300176523));
#68215=CARTESIAN_POINT('Ctrl Pts',(-0.322225765931273,2.09435759100465,
11.3503509877838));
#68216=CARTESIAN_POINT('Ctrl Pts',(-0.322142162270717,2.08984295570853,
11.3506423847816));
#68217=CARTESIAN_POINT('Ctrl Pts',(-0.321982842034037,2.08565455274893,
11.3509093892228));
#68218=CARTESIAN_POINT('Ctrl Pts',(-0.321710696427258,2.08092915467588,
11.3512059711591));
#68219=CARTESIAN_POINT('Ctrl Pts',(-0.321678170886067,2.08038817390923,
11.3512398558992));
#68220=CARTESIAN_POINT('Ctrl Pts',(-0.321626919389701,2.07957018283672,
11.3512909843371));
#68221=CARTESIAN_POINT('Ctrl Pts',(-0.32160920007326,2.0792931138242,11.351308283924));
#68222=CARTESIAN_POINT('Ctrl Pts',(-0.321577779737462,2.07881157869098,
11.3513383172269));
#68223=CARTESIAN_POINT('Ctrl Pts',(-0.321564241736346,2.0786071026854,11.3513510601254));
#68224=CARTESIAN_POINT('Ctrl Pts',(-0.321535489433735,2.07817902642415,
11.3513777160785));
#68225=CARTESIAN_POINT('Ctrl Pts',(-0.32152023692546,2.07795542921854,11.3513916268917));
#68226=CARTESIAN_POINT('Ctrl Pts',(-0.321483142001477,2.07741985742535,
11.3514249174701));
#68227=CARTESIAN_POINT('Ctrl Pts',(-0.321461078615877,2.07710789728034,
11.3514442847425));
#68228=CARTESIAN_POINT('Ctrl Pts',(-0.321384460829354,2.07604653384006,
11.3515100972263));
#68229=CARTESIAN_POINT('Ctrl Pts',(-0.321327739172489,2.0752972821618,11.3515564213311));
#68230=CARTESIAN_POINT('Ctrl Pts',(-0.321186363489505,2.07351274876815,
11.3516664465324));
#68231=CARTESIAN_POINT('Ctrl Pts',(-0.321099323082241,2.07247765721126,
11.3517300183183));
#68232=CARTESIAN_POINT('Ctrl Pts',(-0.319985740555356,2.05995995741967,
11.3524960223014));
#68233=CARTESIAN_POINT('Ctrl Pts',(-0.318348655376113,2.04853860388575,
11.3531666224636));
#68234=CARTESIAN_POINT('Ctrl Pts',(-0.312585255584749,2.01951552768629,
11.3548528312258));
#68235=CARTESIAN_POINT('Ctrl Pts',(-0.307585194892534,2.00212924602347,
11.3558471779224));
#68236=CARTESIAN_POINT('Ctrl Pts',(-0.294198592816751,1.96699598748604,
11.3579662293857));
#68237=CARTESIAN_POINT('Ctrl Pts',(-0.285597735543596,1.94941234818879,
11.3590915593017));
#68238=CARTESIAN_POINT('Ctrl Pts',(-0.27478706982546,1.93161081744876,11.3603565552511));
#68239=CARTESIAN_POINT('Ctrl Pts',(-0.274108648226786,1.93050870395655,
11.3604354020208));
#68240=CARTESIAN_POINT('Ctrl Pts',(-0.273153143741806,1.92897720392091,
11.3605457199085));
#68241=CARTESIAN_POINT('Ctrl Pts',(-0.272881643774218,1.92854433459032,
11.3605769849733));
#68242=CARTESIAN_POINT('Ctrl Pts',(-0.272411008231611,1.9277979204997,11.360631043289));
#68243=CARTESIAN_POINT('Ctrl Pts',(-0.272212357359613,1.92748407004326,
11.3606538185599));
#68244=CARTESIAN_POINT('Ctrl Pts',(-0.27180004984217,1.92683514659664,11.3607010026624));
#68245=CARTESIAN_POINT('Ctrl Pts',(-0.271586315203881,1.92650012409172,
11.3607254143657));
#68246=CARTESIAN_POINT('Ctrl Pts',(-0.271085298505831,1.92571799002968,
11.360782526825));
#68247=CARTESIAN_POINT('Ctrl Pts',(-0.270797529683122,1.92527119305217,
11.3608152456765));
#68248=CARTESIAN_POINT('Ctrl Pts',(-0.269868427986225,1.92383645513704,
11.3609206127401));
#68249=CARTESIAN_POINT('Ctrl Pts',(-0.26922278931383,1.92285132623277,11.3609934217841));
#68250=CARTESIAN_POINT('Ctrl Pts',(-0.267709438798386,1.92056960668969,
11.3611631456716));
#68251=CARTESIAN_POINT('Ctrl Pts',(-0.26683768871196,1.91927574205359,11.3612602116797));
#68252=CARTESIAN_POINT('Ctrl Pts',(-0.257749077940783,1.90599541108135,
11.3622651230337));
#68253=CARTESIAN_POINT('Ctrl Pts',(-0.248740970689,1.8945731459135,11.3632034653423));
#68254=CARTESIAN_POINT('Ctrl Pts',(-0.218226273014972,1.86084144644508,
11.3662147778078));
#68255=CARTESIAN_POINT('Ctrl Pts',(-0.19426128068826,1.84099825800115,11.3683709608921));
#68256=CARTESIAN_POINT('Ctrl Pts',(-0.164748890010322,1.82299448536771,
11.370593445208));
#68257=CARTESIAN_POINT('Ctrl Pts',(-0.161630216819241,1.821163259902,11.3708232524154));
#68258=CARTESIAN_POINT('Ctrl Pts',(-0.157979280602623,1.81910134419536,
11.371085897172));
#68259=CARTESIAN_POINT('Ctrl Pts',(-0.157476572978896,1.8188192095686,11.3711219228752));
#68260=CARTESIAN_POINT('Ctrl Pts',(-0.156728050133536,1.81840175309935,
11.3711753556645));
#68261=CARTESIAN_POINT('Ctrl Pts',(-0.156482814323158,1.81826540294255,
11.3711928284236));
#68262=CARTESIAN_POINT('Ctrl Pts',(-0.156045778826928,1.81802315957682,
11.3712239071148));
#68263=CARTESIAN_POINT('Ctrl Pts',(-0.155854049346688,1.81791714173303,
11.3712375210835));
#68264=CARTESIAN_POINT('Ctrl Pts',(-0.155446859434647,1.81769252577277,
11.3712663906848));
#68265=CARTESIAN_POINT('Ctrl Pts',(-0.155231371927921,1.81757397909718,
11.3712816429731));
#68266=CARTESIAN_POINT('Ctrl Pts',(-0.154653012969298,1.81725666694516,
11.3713225111528));
#68267=CARTESIAN_POINT('Ctrl Pts',(-0.154289892564901,1.81705835254545,
11.3713480980743));
#68268=CARTESIAN_POINT('Ctrl Pts',(-0.152551827026258,1.81611346716004,
11.3714702300917));
#68269=CARTESIAN_POINT('Ctrl Pts',(-0.151171809089077,1.81537619947339,
11.3715661895778));
#68270=CARTESIAN_POINT('Ctrl Pts',(-0.139697066005331,1.80935287758154,
11.3723561844237));
#68271=CARTESIAN_POINT('Ctrl Pts',(-0.12933267025224,1.80459495419969,11.3730194368098));
#68272=CARTESIAN_POINT('Ctrl Pts',(-0.0849952756713622,1.78702350160199,
11.3757387256628));
#68273=CARTESIAN_POINT('Ctrl Pts',(-0.0492400728219842,1.7794472788211,
11.3776858655186));
#68274=CARTESIAN_POINT('Ctrl Pts',(-0.0105334510163253,1.77788793613816,
11.3800220205265));
#68275=CARTESIAN_POINT('Ctrl Pts',(-0.00809320590537355,1.77781738906632,
11.3801700830293));
#68276=CARTESIAN_POINT('Ctrl Pts',(-0.00491502393441853,1.77776163772369,
11.3803640108235));
#68277=CARTESIAN_POINT('Ctrl Pts',(-0.004177565082357,1.77775123348794,
11.380409085805));
#68278=CARTESIAN_POINT('Ctrl Pts',(-0.00299940278673548,1.77773865663401,
11.3804812216926));
#68279=CARTESIAN_POINT('Ctrl Pts',(-0.00255871632707988,1.77773485634833,
11.3805082315666));
#68280=CARTESIAN_POINT('Ctrl Pts',(-0.00176502681447951,1.77772964002475,
11.380556927659));
#68281=CARTESIAN_POINT('Ctrl Pts',(-0.00141202599249764,1.77772790002978,
11.3805786036913));
#68282=CARTESIAN_POINT('Ctrl Pts',(-0.000584296812591893,1.77772518002378,
11.3806294729498));
#68283=CARTESIAN_POINT('Ctrl Pts',(-0.000109568635152322,1.77772466897949,
11.3806586808236));
#68284=CARTESIAN_POINT('Ctrl Pts',(0.00125787086624673,1.77772621837162,
11.380742908553));
#68285=CARTESIAN_POINT('Ctrl Pts',(0.00215056945188629,1.77773093913696,
11.3807980116101));
#68286=CARTESIAN_POINT('Ctrl Pts',(0.0081326857779983,1.77778743053788,
11.3811680640883));
#68287=CARTESIAN_POINT('Ctrl Pts',(0.0132200369947419,1.77795604905191,
11.381486655182));
#68288=CARTESIAN_POINT('Ctrl Pts',(0.0278436129398111,1.77878782063104,
11.3824143393393));
#68289=CARTESIAN_POINT('Ctrl Pts',(0.0373564599011915,1.77975478698624,
11.3830325667887));
#68290=CARTESIAN_POINT('Ctrl Pts',(0.0766474732230871,1.78552312003411,
11.3856457197092));
#68291=CARTESIAN_POINT('Ctrl Pts',(0.105716704378513,1.79406826305974,11.387740093877));
#68292=CARTESIAN_POINT('Ctrl Pts',(0.133983641781497,1.80689532244629,11.3897667565093));
#68293=CARTESIAN_POINT('Ctrl Pts',(0.134792858967848,1.80726658292542,11.3898247507822));
#68294=CARTESIAN_POINT('Ctrl Pts',(0.136146108144932,1.80789424082443,11.3899216813483));
#68295=CARTESIAN_POINT('Ctrl Pts',(0.136690975470414,1.8081488143903,11.3899606946782));
#68296=CARTESIAN_POINT('Ctrl Pts',(0.137494730866613,1.80852709057561,11.3900182201424));
#68297=CARTESIAN_POINT('Ctrl Pts',(0.137754168508875,1.80864961471797,11.3900367845145));
#68298=CARTESIAN_POINT('Ctrl Pts',(0.13839585018029,1.80895370925731,11.3900826907974));
#68299=CARTESIAN_POINT('Ctrl Pts',(0.138777901985562,1.80913568691488,11.3901100141952));
#68300=CARTESIAN_POINT('Ctrl Pts',(0.142831562103555,1.81107631796754,11.3903998199027));
#68301=CARTESIAN_POINT('Ctrl Pts',(0.146470105386644,1.81290374222548,11.3906590610497));
#68302=CARTESIAN_POINT('Ctrl Pts',(0.150548826194132,1.81504997743624,11.3909478367668));
#68303=CARTESIAN_POINT('Ctrl Pts',(0.151023783824546,1.81530142052213,11.3909814355843));
#68304=CARTESIAN_POINT('Ctrl Pts',(0.15174212484499,1.81568401451245,11.391032205797));
#68305=CARTESIAN_POINT('Ctrl Pts',(0.151985969156564,1.8158142909343,11.3910494319919));
#68306=CARTESIAN_POINT('Ctrl Pts',(0.152410005983539,1.81604153900037,11.3910793734193));
#68307=CARTESIAN_POINT('Ctrl Pts',(0.152590273849286,1.81613836852379,11.3910920976985));
#68308=CARTESIAN_POINT('Ctrl Pts',(0.15296802205246,1.81634173693857,11.3911187515392));
#68309=CARTESIAN_POINT('Ctrl Pts',(0.15316548329971,1.81644831035666,11.3911326787989));
#68310=CARTESIAN_POINT('Ctrl Pts',(0.15363914237129,1.8167045918943,11.3911660737386));
#68311=CARTESIAN_POINT('Ctrl Pts',(0.153915233883513,1.81685449835297,11.3911855287245));
#68312=CARTESIAN_POINT('Ctrl Pts',(0.154842833757168,1.81735990500328,11.3912508584859));
#68313=CARTESIAN_POINT('Ctrl Pts',(0.155493339355823,1.81771725538503,11.3912966159694));
#68314=CARTESIAN_POINT('Ctrl Pts',(0.157045116931194,1.81857670452074,11.3914056481177));
#68315=CARTESIAN_POINT('Ctrl Pts',(0.157945230156048,1.81908089362418,11.3914687936616));
#68316=CARTESIAN_POINT('Ctrl Pts',(0.168745359740301,1.82519879412834,11.3922254513136));
#68317=CARTESIAN_POINT('Ctrl Pts',(0.178344914343773,1.83132947468025,11.3928879275854));
#68318=CARTESIAN_POINT('Ctrl Pts',(0.20869985926452,1.85306099628176,11.3950166235831));
#68319=CARTESIAN_POINT('Ctrl Pts',(0.227897196189615,1.87065865649994,11.3964262556818));
#68320=CARTESIAN_POINT('Ctrl Pts',(0.248366278791247,1.89455946420404,11.3982412623956));
#68321=CARTESIAN_POINT('Ctrl Pts',(0.251847116713623,1.89884173553397,11.3985627468047));
#68322=CARTESIAN_POINT('Ctrl Pts',(0.259313591127547,1.90852503108503,11.3992841385145));
#68323=CARTESIAN_POINT('Ctrl Pts',(0.26324378173639,1.91396531586363,11.3996858096092));
#68324=CARTESIAN_POINT('Ctrl Pts',(0.267585024537801,1.92038786939276,11.400157588205));
#68325=CARTESIAN_POINT('Ctrl Pts',(0.26816473361342,1.92125454292723,11.4002212003856));
#68326=CARTESIAN_POINT('Ctrl Pts',(0.269019271110226,1.92254560301677,11.4003158927731));
#68327=CARTESIAN_POINT('Ctrl Pts',(0.269297327119056,1.92296785365566,11.4003468517216));
#68328=CARTESIAN_POINT('Ctrl Pts',(0.269790093827069,1.92372000727747,11.4004019802214));
#68329=CARTESIAN_POINT('Ctrl Pts',(0.27000519637855,1.9240496533454,11.4004261350477));
#68330=CARTESIAN_POINT('Ctrl Pts',(0.27045603463757,1.92474333949884,11.4004769520664));
#68331=CARTESIAN_POINT('Ctrl Pts',(0.27069164032874,1.92510746278041,11.400503619046));
#68332=CARTESIAN_POINT('Ctrl Pts',(0.271301335856536,1.92605391685708,11.4005729150985));
#68333=CARTESIAN_POINT('Ctrl Pts',(0.271674284558492,1.92663697690686,11.4006155865113));
#68334=CARTESIAN_POINT('Ctrl Pts',(0.273285967541569,1.92917462005297,11.4008012298959));
#68335=CARTESIAN_POINT('Ctrl Pts',(0.274505483292307,1.93114127300455,11.4009449107577));
#68336=CARTESIAN_POINT('Ctrl Pts',(0.283023197408598,1.94521352336701,11.4019718709127));
#68337=CARTESIAN_POINT('Ctrl Pts',(0.289538172460316,1.95777295085765,11.4028835285566));
#68338=CARTESIAN_POINT('Ctrl Pts',(0.30440342555142,1.99171679812595,11.4053333954308));
#68339=CARTESIAN_POINT('Ctrl Pts',(0.311332480722723,2.01363654946929,11.4069056397352));
#68340=CARTESIAN_POINT('Ctrl Pts',(0.316736882305902,2.04035329504781,11.4087269090854));
#68341=CARTESIAN_POINT('Ctrl Pts',(0.317510852410453,2.04462091306966,11.4090148190689));
#68342=CARTESIAN_POINT('Ctrl Pts',(0.319393179477519,2.05634280540895,11.4097953207747));
#68343=CARTESIAN_POINT('Ctrl Pts',(0.320326704382693,2.06382296571582,11.4102820877981));
#68344=CARTESIAN_POINT('Ctrl Pts',(0.321058357966574,2.07201465751626,11.4107980363229));
#68345=CARTESIAN_POINT('Ctrl Pts',(0.321117348903699,2.07269987421677,11.4108410637669));
#68346=CARTESIAN_POINT('Ctrl Pts',(0.321197190871934,2.07366337027746,11.4109013770768));
#68347=CARTESIAN_POINT('Ctrl Pts',(0.321219874124523,2.07394148971953,11.4109187648537));
#68348=CARTESIAN_POINT('Ctrl Pts',(0.321258617694233,2.07442426300877,11.4109489087156));
#68349=CARTESIAN_POINT('Ctrl Pts',(0.321274843696754,2.07462890279038,11.4109616741484));
#68350=CARTESIAN_POINT('Ctrl Pts',(0.321308351169368,2.07505668060003,11.4109883335251));
#68351=CARTESIAN_POINT('Ctrl Pts',(0.321325595718477,2.07527982098841,11.4110022252993));
#68352=CARTESIAN_POINT('Ctrl Pts',(0.321366253171583,2.07581315001459,11.4110353938813));
#68353=CARTESIAN_POINT('Ctrl Pts',(0.321389449521425,2.0761233560143,11.4110546584326));
#68354=CARTESIAN_POINT('Ctrl Pts',(0.321464784825603,2.07715082233046,11.4111183764601));
#68355=CARTESIAN_POINT('Ctrl Pts',(0.321514972572268,2.07786823011169,11.411162720841));
#68356=CARTESIAN_POINT('Ctrl Pts',(0.32162883875125,2.07957808321426,11.4112680764456));
#68357=CARTESIAN_POINT('Ctrl Pts',(0.321690326159174,2.08057067380755,11.4113289688813));
#68358=CARTESIAN_POINT('Ctrl Pts',(0.322355582655625,2.09218052293047,11.4120382332205));
#68359=CARTESIAN_POINT('Ctrl Pts',(0.322438135198141,2.10282233956264,11.4126594456948));
#68360=CARTESIAN_POINT('Ctrl Pts',(0.321142405703716,2.13384257073631,11.41443548328));
#68361=CARTESIAN_POINT('Ctrl Pts',(0.318355255251917,2.15410883659745,11.4155545094065));
#68362=CARTESIAN_POINT('Ctrl Pts',(0.309497782562498,2.19166588644357,11.4177362954637));
#68363=CARTESIAN_POINT('Ctrl Pts',(0.303837524600769,2.20896845452589,11.4187877654759));
#68364=CARTESIAN_POINT('Ctrl Pts',(0.296248992178024,2.22688325539048,11.4199695504907));
#68365=CARTESIAN_POINT('Ctrl Pts',(0.295740877035584,2.22806310725788,11.4200478176743));
#68366=CARTESIAN_POINT('Ctrl Pts',(0.295021468249988,2.22970646987592,11.4201574536801));
#68367=CARTESIAN_POINT('Ctrl Pts',(0.294816104463046,2.2301725762232,11.420188619804));
#68368=CARTESIAN_POINT('Ctrl Pts',(0.294459243057607,2.23097735473361,11.4202425532499));
#68369=CARTESIAN_POINT('Ctrl Pts',(0.294308263554812,2.23131625671087,11.4202653027877));
#68370=CARTESIAN_POINT('Ctrl Pts',(0.293994250533588,2.23201785639865,11.4203124773208));
#68371=CARTESIAN_POINT('Ctrl Pts',(0.293831130325233,2.23238051444411,11.4203369052638));
#68372=CARTESIAN_POINT('Ctrl Pts',(0.293447786975302,2.23322858578083,11.4203941317023));
#68373=CARTESIAN_POINT('Ctrl Pts',(0.293227030418377,2.23371375537482,11.4204269485085));
#68374=CARTESIAN_POINT('Ctrl Pts',(0.292523891044995,2.23524897073322,11.4205310402435));
#68375=CARTESIAN_POINT('Ctrl Pts',(0.292037067877216,2.23629696198534,11.4206024681837));
#68376=CARTESIAN_POINT('Ctrl Pts',(0.288152271303356,2.24454344936577,11.4211674933057));
#68377=CARTESIAN_POINT('Ctrl Pts',(0.284494553420535,2.25161586709843,11.421670086572));
#68378=CARTESIAN_POINT('Ctrl Pts',(0.277531053500126,2.26393924564599,11.4225795579248));
#68379=CARTESIAN_POINT('Ctrl Pts',(0.274328306406912,2.26924400883745,11.4229827547632));
#68380=CARTESIAN_POINT('Ctrl Pts',(0.260528830244049,2.29067850604845,11.4246598769326));
#68381=CARTESIAN_POINT('Ctrl Pts',(0.248647277148233,2.30593196769664,11.4259716245397));
#68382=CARTESIAN_POINT('Ctrl Pts',(0.232954964968058,2.32272578851382,11.4275234458375));
#68383=CARTESIAN_POINT('Ctrl Pts',(0.230389420628076,2.32537858867961,11.4277720321297));
#68384=CARTESIAN_POINT('Ctrl Pts',(0.220784360342617,2.33497488884179,11.4286826959563));
#68385=CARTESIAN_POINT('Ctrl Pts',(0.213471340959871,2.34163806224665,11.4293378125982));
#68386=CARTESIAN_POINT('Ctrl Pts',(0.203086352975509,2.35026012890085,11.4302055166265));
#68387=CARTESIAN_POINT('Ctrl Pts',(0.200271129216339,2.35251866542901,11.4304348499554));
#68388=CARTESIAN_POINT('Ctrl Pts',(0.196963062473938,2.35508245635267,11.4306970112674));
#68389=CARTESIAN_POINT('Ctrl Pts',(0.196506756064167,2.35543414484239,11.4307330143777));
#68390=CARTESIAN_POINT('Ctrl Pts',(0.19582686122584,2.35595525925136,11.4307864201857));
#68391=CARTESIAN_POINT('Ctrl Pts',(0.195603993844891,2.35612561744066,11.4308038884601));
#68392=CARTESIAN_POINT('Ctrl Pts',(0.195206675191319,2.3564285038407,11.4308349621622));
#68393=CARTESIAN_POINT('Ctrl Pts',(0.195032311319071,2.35656114507822,11.4308485756167));
#68394=CARTESIAN_POINT('Ctrl Pts',(0.194661882860758,2.35684233976215,11.4308774473053));
#68395=CARTESIAN_POINT('Ctrl Pts',(0.194465783973343,2.35699084613658,11.4308927021888));
#68396=CARTESIAN_POINT('Ctrl Pts',(0.194065529267228,2.35729323997252,11.4309237794022));
#68397=CARTESIAN_POINT('Ctrl Pts',(0.193861359922479,2.35744710935531,11.4309396004527));
#68398=CARTESIAN_POINT('Ctrl Pts',(0.192953573085077,2.35812955803287,11.431009806456));
#68399=CARTESIAN_POINT('Ctrl Pts',(0.192247966515316,2.35865550353666,11.4310640078875));
#68400=CARTESIAN_POINT('Ctrl Pts',(0.190511285100771,2.35993895967821,11.431196534431));
#68401=CARTESIAN_POINT('Ctrl Pts',(0.189477827138661,2.36069324052468,11.4312746445315));
#68402=CARTESIAN_POINT('Ctrl Pts',(0.185512878239694,2.36355106880785,11.4315715704013));
#68403=CARTESIAN_POINT('Ctrl Pts',(0.182550512776564,2.36561157079062,11.4317877151375));
#68404=CARTESIAN_POINT('Ctrl Pts',(0.175001473048611,2.37067640342882,11.4323260228765));
#68405=CARTESIAN_POINT('Ctrl Pts',(0.170371475048728,2.37361432270027,11.4326448646238));
#68406=CARTESIAN_POINT('Ctrl Pts',(0.151255883351461,2.38507045976688,11.4339253876778));
#68407=CARTESIAN_POINT('Ctrl Pts',(0.136189064409516,2.39256812394989,11.4348542788846));
#68408=CARTESIAN_POINT('Ctrl Pts',(0.108011185590584,2.40393948673635,11.4365572958474));
#68409=CARTESIAN_POINT('Ctrl Pts',(0.0951088359956848,2.40822053020989,
11.4373250345767));
#68410=CARTESIAN_POINT('Ctrl Pts',(0.0728200079417232,2.41408286838521,
11.4386679479792));
#68411=CARTESIAN_POINT('Ctrl Pts',(0.0635634144105625,2.41608617101461,
11.4392301645112));
#68412=CARTESIAN_POINT('Ctrl Pts',(0.0531026622613474,2.41787198223381,
11.4398755053916));
#68413=CARTESIAN_POINT('Ctrl Pts',(0.0519716139524046,2.41805886423508,
11.4399454082582));
#68414=CARTESIAN_POINT('Ctrl Pts',(0.0503262083653341,2.41832172197047,
11.4400472920871));
#68415=CARTESIAN_POINT('Ctrl Pts',(0.0498126174761309,2.41840249537629,
11.4400791208478));
#68416=CARTESIAN_POINT('Ctrl Pts',(0.0489065097601256,2.41854275464342,
11.4401353236783));
#68417=CARTESIAN_POINT('Ctrl Pts',(0.0485140732948712,2.41860275881235,
11.4401596812714));
#68418=CARTESIAN_POINT('Ctrl Pts',(0.0477031080657034,2.41872522362356,
11.4402100495519));
#68419=CARTESIAN_POINT('Ctrl Pts',(0.0472845653396324,2.41878758534633,
11.4402360633213));
#68420=CARTESIAN_POINT('Ctrl Pts',(0.0462139581986469,2.41894494808144,
11.4403026528132));
#68421=CARTESIAN_POINT('Ctrl Pts',(0.0455617253508072,2.41903877352418,
11.4403432656603));
#68422=CARTESIAN_POINT('Ctrl Pts',(0.0429493223209359,2.41940640033758,
11.4405061180151));
#68423=CARTESIAN_POINT('Ctrl Pts',(0.0409869685045067,2.41966413780157,
11.4406288641107));
#68424=CARTESIAN_POINT('Ctrl Pts',(0.0279561741863934,2.42125365595445,
11.4414468333331));
#68425=CARTESIAN_POINT('Ctrl Pts',(0.0168285981275828,2.42202827323941,
11.4421595293942));
#68426=CARTESIAN_POINT('Ctrl Pts',(-0.0118298918335914,2.42253382824022,
11.444032691079));
#68427=CARTESIAN_POINT('Ctrl Pts',(-0.0293384821624809,2.42141430629471,
11.4452145718946));
#68428=CARTESIAN_POINT('Ctrl Pts',(-0.0665240705506868,2.415972231577,11.4477578117019));
#68429=CARTESIAN_POINT('Ctrl Pts',(-0.0860683125025795,2.4112175228195,
11.449114888552));
#68430=CARTESIAN_POINT('Ctrl Pts',(-0.106121627391803,2.40430358617244,
11.4504519737043));
#68431=CARTESIAN_POINT('Ctrl Pts',(-0.10719622394402,2.40392670501595,11.4505234420489));
#68432=CARTESIAN_POINT('Ctrl Pts',(-0.108629373528265,2.40341552592135,
11.4506184916307));
#68433=CARTESIAN_POINT('Ctrl Pts',(-0.108989700695743,2.40328627946075,
11.4506423668456));
#68434=CARTESIAN_POINT('Ctrl Pts',(-0.109552188931617,2.40308338756261,
11.4506796011478));
#68435=CARTESIAN_POINT('Ctrl Pts',(-0.109754506487611,2.40301018171417,
11.450692986401));
#68436=CARTESIAN_POINT('Ctrl Pts',(-0.110142003605072,2.40286953215308,
11.4507186088649));
#68437=CARTESIAN_POINT('Ctrl Pts',(-0.110327193273273,2.40280212167267,
11.4507308479087));
#68438=CARTESIAN_POINT('Ctrl Pts',(-0.110764785458685,2.40264237997746,
11.4507597533917));
#68439=CARTESIAN_POINT('Ctrl Pts',(-0.111017134075308,2.40254990298973,
11.45077641097));
#68440=CARTESIAN_POINT('Ctrl Pts',(-0.1115392958736,2.4023578076107,11.4508108557249));
#68441=CARTESIAN_POINT('Ctrl Pts',(-0.111809092120167,2.40225814342697,
11.4508286401532));
#68442=CARTESIAN_POINT('Ctrl Pts',(-0.113289902190313,2.40170887024669,
11.4509261833984));
#68443=CARTESIAN_POINT('Ctrl Pts',(-0.114498360508774,2.40125233591932,
11.4510055335957));
#68444=CARTESIAN_POINT('Ctrl Pts',(-0.117660610527874,2.40003591596145,
11.4512125911184));
#68445=CARTESIAN_POINT('Ctrl Pts',(-0.119609823440329,2.39926419897227,
11.4513396346509));
#68446=CARTESIAN_POINT('Ctrl Pts',(-0.122305406930449,2.39816643981833,
11.4515146902266));
#68447=CARTESIAN_POINT('Ctrl Pts',(-0.123058231790622,2.39785652588867,
11.4515635107545));
#68448=CARTESIAN_POINT('Ctrl Pts',(-0.133771613180375,2.39339861862727,
11.4522573943448));
#68449=CARTESIAN_POINT('Ctrl Pts',(-0.143519862387249,2.38875540943751,
11.4528780562243));
#68450=CARTESIAN_POINT('Ctrl Pts',(-0.162018124310045,2.37877570012278,
11.4540683483744));
#68451=CARTESIAN_POINT('Ctrl Pts',(-0.170782634744406,2.3734941770556,11.4546382976379));
#68452=CARTESIAN_POINT('Ctrl Pts',(-0.191790201953743,2.35943070424253,
11.4560518017516));
#68453=CARTESIAN_POINT('Ctrl Pts',(-0.2036963572905,2.35019096949125,11.4568964773903));
#68454=CARTESIAN_POINT('Ctrl Pts',(-0.216439868090448,2.3387868502637,11.4578879684261));
#68455=CARTESIAN_POINT('Ctrl Pts',(-0.217954075312678,2.33740555422382,
11.4580072722552));
#68456=CARTESIAN_POINT('Ctrl Pts',(-0.221083807544876,2.33449535743689,
11.4582571241224));
#68457=CARTESIAN_POINT('Ctrl Pts',(-0.22269688148436,2.33296399135776,11.458387757009));
#68458=CARTESIAN_POINT('Ctrl Pts',(-0.229037555234947,2.3268184599815,11.4589089661364));
#68459=CARTESIAN_POINT('Ctrl Pts',(-0.233638391883418,2.3220763558671,11.4593045225998));
#68460=CARTESIAN_POINT('Ctrl Pts',(-0.238789550991669,2.31642967280185,
11.4597696920269));
#68461=CARTESIAN_POINT('Ctrl Pts',(-0.239485349140365,2.31565950115755,
11.4598330158626));
#68462=CARTESIAN_POINT('Ctrl Pts',(-0.240513890358391,2.31450990380329,
11.4599273612062));
#68463=CARTESIAN_POINT('Ctrl Pts',(-0.240849487050015,2.31413303077337,
11.4599582627578));
#68464=CARTESIAN_POINT('Ctrl Pts',(-0.241445193846402,2.31346088362359,
11.4600133267127));
#68465=CARTESIAN_POINT('Ctrl Pts',(-0.241705651510153,2.31316591776071,
11.4600374745164));
#68466=CARTESIAN_POINT('Ctrl Pts',(-0.242252365654404,2.3125444788454,11.4600883152048));
#68467=CARTESIAN_POINT('Ctrl Pts',(-0.242538503691286,2.31221790305502,
11.4601150129529));
#68468=CARTESIAN_POINT('Ctrl Pts',(-0.243117828666712,2.31155400434653,
11.4601692473874));
#68469=CARTESIAN_POINT('Ctrl Pts',(-0.243410975560251,2.31121664788614,
11.4601967856532));
#68470=CARTESIAN_POINT('Ctrl Pts',(-0.244133539122185,2.3103816122781,11.4602648989441));
#68471=CARTESIAN_POINT('Ctrl Pts',(-0.244562135298083,2.30988322867072,
11.4603055077896));
#68472=CARTESIAN_POINT('Ctrl Pts',(-0.248500652182109,2.30527496717996,
11.4606805967958));
#68473=CARTESIAN_POINT('Ctrl Pts',(-0.251908008977126,2.30107892873676,
11.461019251086));
#68474=CARTESIAN_POINT('Ctrl Pts',(-0.26349469955704,2.28605338878381,11.4622230154228));
#68475=CARTESIAN_POINT('Ctrl Pts',(-0.271093300244179,2.27479606001237,
11.4631099453408));
#68476=CARTESIAN_POINT('Ctrl Pts',(-0.280346600429231,2.25902582795637,
11.4643290027014));
#68477=CARTESIAN_POINT('Ctrl Pts',(-0.28264431077338,2.2549052030052,11.4646454138578));
#68478=CARTESIAN_POINT('Ctrl Pts',(-0.287116581784,2.24645379221042,11.4652892583565));
#68479=CARTESIAN_POINT('Ctrl Pts',(-0.289285605294081,2.24212136470088,
11.4656166806061));
#68480=CARTESIAN_POINT('Ctrl Pts',(-0.299422882711818,2.22067864346843,
11.467221393532));
#68481=CARTESIAN_POINT('Ctrl Pts',(-0.305975819114873,2.20293842151257,
11.4685028272173));
#68482=CARTESIAN_POINT('Ctrl Pts',(-0.311884705337857,2.18125305061516,
11.4699476056887));
#68483=CARTESIAN_POINT('Ctrl Pts',(-0.312772665988365,2.17776496481335,
11.4701763008842));
#68484=CARTESIAN_POINT('Ctrl Pts',(-0.313734693619783,2.17370243536213,
11.4704378110769));
#68485=CARTESIAN_POINT('Ctrl Pts',(-0.31386583448979,2.17314195041977,11.4704737836992));
#68486=CARTESIAN_POINT('Ctrl Pts',(-0.314058629481986,2.17230789382675,
11.4705271530946));
#68487=CARTESIAN_POINT('Ctrl Pts',(-0.314121428440611,2.17203459209038,
11.4705446153147));
#68488=CARTESIAN_POINT('Ctrl Pts',(-0.314232651272593,2.17154763791132,
11.4705756822835));
#68489=CARTESIAN_POINT('Ctrl Pts',(-0.314281213988249,2.17133401819357,
11.4705892950457));
#68490=CARTESIAN_POINT('Ctrl Pts',(-0.314383856272639,2.17088037158899,
11.4706181695613));
#68491=CARTESIAN_POINT('Ctrl Pts',(-0.314437878643613,2.17064033293045,
11.4706334279553));
#68492=CARTESIAN_POINT('Ctrl Pts',(-0.314547491622685,2.1701506702798,11.4706645136694));
#68493=CARTESIAN_POINT('Ctrl Pts',(-0.314603060113425,2.16990104144555,
11.4706803397064));
#68494=CARTESIAN_POINT('Ctrl Pts',(-0.314741085308612,2.16927749602512,
11.4707198186209));
#68495=CARTESIAN_POINT('Ctrl Pts',(-0.314823173155208,2.16890349689813,
11.4707434504841));
#68496=CARTESIAN_POINT('Ctrl Pts',(-0.315051943684686,2.16785225548443,
11.4708097444342));
#68497=CARTESIAN_POINT('Ctrl Pts',(-0.315197110005239,2.16717468018985,
11.4708523216657));
#68498=CARTESIAN_POINT('Ctrl Pts',(-0.315662529000211,2.16496757198191,
11.4709905310224));
#68499=CARTESIAN_POINT('Ctrl Pts',(-0.315973848210064,2.16343614972098,
11.4710856792933));
#68500=CARTESIAN_POINT('Ctrl Pts',(-0.320245880130619,2.1416093583186,11.4724319212824));
#68501=CARTESIAN_POINT('Ctrl Pts',(-0.322255880839034,2.12097861176568,
11.4735849954418));
#68502=CARTESIAN_POINT('Ctrl Pts',(-0.322274864254423,2.10029579518797,
11.4747410908026));
#68503=CARTESIAN_POINT('',(-0.322274879003935,2.09972073668561,11.7247944044677));
#68504=CARTESIAN_POINT('Ctrl Pts',(-0.322274864206818,2.10029584705048,
11.4747410879037));
#68505=CARTESIAN_POINT('Ctrl Pts',(-0.322300036387824,2.07287505241094,
11.4762738121076));
#68506=CARTESIAN_POINT('Ctrl Pts',(-0.318825877456706,2.04556637550985,
11.4778092777199));
#68507=CARTESIAN_POINT('Ctrl Pts',(-0.311694069518997,2.01809202581767,
11.4795321329028));
#68508=CARTESIAN_POINT('Ctrl Pts',(-0.311447100466804,2.01715790449816,
11.4795909126418));
#68509=CARTESIAN_POINT('Ctrl Pts',(-0.311046099801683,2.01566832345317,
11.4796849747927));
#68510=CARTESIAN_POINT('Ctrl Pts',(-0.310894770908584,2.01511213699265,
11.4797201697899));
#68511=CARTESIAN_POINT('Ctrl Pts',(-0.310602184302145,2.01404805620748,
11.4797876462982));
#68512=CARTESIAN_POINT('Ctrl Pts',(-0.310461170783618,2.01354009619816,
11.479819919803));
#68513=CARTESIAN_POINT('Ctrl Pts',(-0.310211858606244,2.01265049638237,
11.4798765510346));
#68514=CARTESIAN_POINT('Ctrl Pts',(-0.310104100144894,2.01226870528007,
11.4799008911412));
#68515=CARTESIAN_POINT('Ctrl Pts',(-0.309893757497413,2.01152868520873,
11.4799481386391));
#68516=CARTESIAN_POINT('Ctrl Pts',(-0.309791256362075,2.01117043309485,
11.479971043292));
#68517=CARTESIAN_POINT('Ctrl Pts',(-0.309517377810665,2.01021943878283,
11.4800319289907));
#68518=CARTESIAN_POINT('Ctrl Pts',(-0.309344919677988,2.00962701177772,
11.4800699452409));
#68519=CARTESIAN_POINT('Ctrl Pts',(-0.308726236192182,2.00752423567982,
11.4802051935106));
#68520=CARTESIAN_POINT('Ctrl Pts',(-0.308270647798801,2.00601668518114,
11.4803027310344));
#68521=CARTESIAN_POINT('Ctrl Pts',(-0.300012608945608,1.97939687465801,
11.4820353647899));
#68522=CARTESIAN_POINT('Ctrl Pts',(-0.289178276617797,1.95533480414639,
11.4837774849787));
#68523=CARTESIAN_POINT('Ctrl Pts',(-0.273220773402468,1.92902723115153,
11.4858578169994));
#68524=CARTESIAN_POINT('Ctrl Pts',(-0.27081570574098,1.92524264784903,11.4861614143527));
#68525=CARTESIAN_POINT('Ctrl Pts',(-0.266047539806185,1.91807445896218,
11.4867437230064));
#68526=CARTESIAN_POINT('Ctrl Pts',(-0.263696839886045,1.91468358601546,
11.4870224336136));
#68527=CARTESIAN_POINT('Ctrl Pts',(-0.255164453629505,1.90286687206271,
11.48800344053));
#68528=CARTESIAN_POINT('Ctrl Pts',(-0.248638295625961,1.89469680465762,
11.4886998085046));
#68529=CARTESIAN_POINT('Ctrl Pts',(-0.239451881133808,1.88427842600382,
11.4895986227768));
#68530=CARTESIAN_POINT('Ctrl Pts',(-0.23713633480027,1.88173556913315,11.4898188986773));
#68531=CARTESIAN_POINT('Ctrl Pts',(-0.233735433919225,1.87811883907701,
11.4901328964604));
#68532=CARTESIAN_POINT('Ctrl Pts',(-0.232682540074257,1.8770149368117,11.4902288313966));
#68533=CARTESIAN_POINT('Ctrl Pts',(-0.231411835578182,1.87570147306234,
11.4903430482569));
#68534=CARTESIAN_POINT('Ctrl Pts',(-0.231201541992224,1.87548471362899,
11.4903618996373));
#68535=CARTESIAN_POINT('Ctrl Pts',(-0.230835446840317,1.87510842205462,
11.4903946288729));
#68536=CARTESIAN_POINT('Ctrl Pts',(-0.230679784274552,1.87494875588769,
11.4904085174729));
#68537=CARTESIAN_POINT('Ctrl Pts',(-0.230367275548818,1.87462887440837,
11.4904363443925));
#68538=CARTESIAN_POINT('Ctrl Pts',(-0.230210427414233,1.874468660703,11.4904502825807));
#68539=CARTESIAN_POINT('Ctrl Pts',(-0.229909974599999,1.87416240092585,
11.4904769280684));
#68540=CARTESIAN_POINT('Ctrl Pts',(-0.229766398081505,1.87401632826821,
11.4904896375556));
#68541=CARTESIAN_POINT('Ctrl Pts',(-0.22942816148061,1.87367286685185,11.4905195234819));
#68542=CARTESIAN_POINT('Ctrl Pts',(-0.229233385390726,1.87347559181608,
11.4905366907478));
#68543=CARTESIAN_POINT('Ctrl Pts',(-0.22865820303797,1.87289453153451,11.4905872613698));
#68544=CARTESIAN_POINT('Ctrl Pts',(-0.228277083400759,1.87251144901886,
11.4906206088896));
#68545=CARTESIAN_POINT('Ctrl Pts',(-0.224963595263786,1.86919760720726,
11.4909091629549));
#68546=CARTESIAN_POINT('Ctrl Pts',(-0.221975723413425,1.86632256018818,
11.4911600707356));
#68547=CARTESIAN_POINT('Ctrl Pts',(-0.218668300037411,1.86326073344151,
11.4914290154668));
#68548=CARTESIAN_POINT('Ctrl Pts',(-0.218403152916785,1.86301610060982,
11.4914505158638));
#68549=CARTESIAN_POINT('Ctrl Pts',(-0.217945850173143,1.86259559846163,
11.4914874955826));
#68550=CARTESIAN_POINT('Ctrl Pts',(-0.217753891632086,1.86241951646358,
11.4915029873584));
#68551=CARTESIAN_POINT('Ctrl Pts',(-0.205505824868496,1.85121177942031,
11.492489499747));
#68552=CARTESIAN_POINT('Ctrl Pts',(-0.192626928169415,1.84111159791732,
11.4934071571877));
#68553=CARTESIAN_POINT('Ctrl Pts',(-0.168119893824159,1.82473788067897,
11.4950559483026));
#68554=CARTESIAN_POINT('Ctrl Pts',(-0.156768373938024,1.81811847014041,
11.4957866415096));
#68555=CARTESIAN_POINT('Ctrl Pts',(-0.134914282452979,1.80710408576295,
11.4971779421657));
#68556=CARTESIAN_POINT('Ctrl Pts',(-0.124521756421104,1.8025371014388,11.4978335105095));
#68557=CARTESIAN_POINT('Ctrl Pts',(-0.110577280362001,1.79726820581965,
11.4987189037373));
#68558=CARTESIAN_POINT('Ctrl Pts',(-0.107223247718585,1.79606407288629,
11.4989322532449));
#68559=CARTESIAN_POINT('Ctrl Pts',(-0.101718662701923,1.79419032324544,
11.4992833833423));
#68560=CARTESIAN_POINT('Ctrl Pts',(-0.0995797905910993,1.79348717865874,
11.499420057571));
#68561=CARTESIAN_POINT('Ctrl Pts',(-0.0969471876172316,1.79265218560044,
11.4995886273974));
#68562=CARTESIAN_POINT('Ctrl Pts',(-0.0964602437650322,1.792499012081,11.4996198216239));
#68563=CARTESIAN_POINT('Ctrl Pts',(-0.0955151720130558,1.79220419514818,
11.4996803929389));
#68564=CARTESIAN_POINT('Ctrl Pts',(-0.0950570876118069,1.79206241596736,
11.4997097654923));
#68565=CARTESIAN_POINT('Ctrl Pts',(-0.0942607389623816,1.79181788874921,
11.4997608510882));
#68566=CARTESIAN_POINT('Ctrl Pts',(-0.0939226180269496,1.79171467367697,
11.4997825487915));
#68567=CARTESIAN_POINT('Ctrl Pts',(-0.0932182483540775,1.79150092357473,
11.49982776472));
#68568=CARTESIAN_POINT('Ctrl Pts',(-0.0928519714335364,1.7913904839763,
11.499851286029));
#68569=CARTESIAN_POINT('Ctrl Pts',(-0.0919566267182979,1.79112225843007,
11.499908804359));
#68570=CARTESIAN_POINT('Ctrl Pts',(-0.0914273498627072,1.7909651797519,
11.4999428244338));
#68571=CARTESIAN_POINT('Ctrl Pts',(-0.0894075920349929,1.79037139932322,
11.5000727198406));
#68572=CARTESIAN_POINT('Ctrl Pts',(-0.0879143836163184,1.78994411973268,
11.5001689018952));
#68573=CARTESIAN_POINT('Ctrl Pts',(-0.0626760899065705,1.78291918791218,
11.5017972692741));
#68574=CARTESIAN_POINT('Ctrl Pts',(-0.0382595575110669,1.77905724232482,
11.5034224355678));
#68575=CARTESIAN_POINT('Ctrl Pts',(0.00195367112345285,1.77735286556368,
11.5061395770682));
#68576=CARTESIAN_POINT('Ctrl Pts',(0.017581956956381,1.77782630548259,11.5072028867821));
#68577=CARTESIAN_POINT('Ctrl Pts',(0.0424096820951024,1.78039099817006,
11.5088581357477));
#68578=CARTESIAN_POINT('Ctrl Pts',(0.0516596151429787,1.78175509859245,
11.5094668303981));
#68579=CARTESIAN_POINT('Ctrl Pts',(0.0617159469430251,1.78368826036074,
11.5101106670232));
#68580=CARTESIAN_POINT('Ctrl Pts',(0.0625931131909332,1.78386066842813,
11.5101666741714));
#68581=CARTESIAN_POINT('Ctrl Pts',(0.0637222040510651,1.7840874761284,11.5102385611435));
#68582=CARTESIAN_POINT('Ctrl Pts',(0.0639747852367891,1.78413852896711,
11.5102546292145));
#68583=CARTESIAN_POINT('Ctrl Pts',(0.0644697565418142,1.78423919285321,
11.5102860906599));
#68584=CARTESIAN_POINT('Ctrl Pts',(0.0647121512356568,1.7842887801772,11.5103014853775));
#68585=CARTESIAN_POINT('Ctrl Pts',(0.0651688274105437,1.78438275166764,
11.5103304656057));
#68586=CARTESIAN_POINT('Ctrl Pts',(0.0653831190488537,1.7844270745854,11.5103440544618));
#68587=CARTESIAN_POINT('Ctrl Pts',(0.0658697065494724,1.78452823460986,
11.5103748881207));
#68588=CARTESIAN_POINT('Ctrl Pts',(0.0661419735546816,1.78458520590344,
11.5103921250876));
#68589=CARTESIAN_POINT('Ctrl Pts',(0.0669663848953701,1.78475882662979,
11.510444270816));
#68590=CARTESIAN_POINT('Ctrl Pts',(0.0675183006269034,1.78487657467964,
11.5104791167787));
#68591=CARTESIAN_POINT('Ctrl Pts',(0.0713664729464188,1.78570813412444,
11.5107216487909));
#68592=CARTESIAN_POINT('Ctrl Pts',(0.0746518098132963,1.78647223426109,
11.5109265173873));
#68593=CARTESIAN_POINT('Ctrl Pts',(0.0923436990885821,1.79088087327393,
11.5120208548015));
#68594=CARTESIAN_POINT('Ctrl Pts',(0.106498699583136,1.79546736880027,11.5128647754025));
#68595=CARTESIAN_POINT('Ctrl Pts',(0.136216340816891,1.80742340489367,11.5146633473693));
#68596=CARTESIAN_POINT('Ctrl Pts',(0.151606717232641,1.81509414483439,11.5156128191301));
#68597=CARTESIAN_POINT('Ctrl Pts',(0.17245749060505,1.82765636836675,11.5170013797609));
#68598=CARTESIAN_POINT('Ctrl Pts',(0.17847664634258,1.8315624515842,11.5174151494616));
#68599=CARTESIAN_POINT('Ctrl Pts',(0.191008502118423,1.84030281480634,11.5183104835166));
#68600=CARTESIAN_POINT('Ctrl Pts',(0.197479005921777,1.84518849907411,11.5187935646229));
#68601=CARTESIAN_POINT('Ctrl Pts',(0.204638500756096,1.85103102420079,11.5193555072261));
#68602=CARTESIAN_POINT('Ctrl Pts',(0.205515085251483,1.85175412070992,11.5194247946692));
#68603=CARTESIAN_POINT('Ctrl Pts',(0.206795589068756,1.85282184188117,11.5195267314757));
#68604=CARTESIAN_POINT('Ctrl Pts',(0.207202516891855,1.85316285835057,11.5195592336723));
#68605=CARTESIAN_POINT('Ctrl Pts',(0.207912485053595,1.85376082350786,11.519616130392));
#68606=CARTESIAN_POINT('Ctrl Pts',(0.208215897196949,1.85401733062496,11.5196405067851));
#68607=CARTESIAN_POINT('Ctrl Pts',(0.208802151316757,1.85451481653447,11.5196877255656));
#68608=CARTESIAN_POINT('Ctrl Pts',(0.209085052539872,1.8547557248411,11.5197105650311));
#68609=CARTESIAN_POINT('Ctrl Pts',(0.209756402796594,1.85532942809465,11.5197648933318));
#68610=CARTESIAN_POINT('Ctrl Pts',(0.210144476511901,1.85566265889679,11.5197964001392));
#68611=CARTESIAN_POINT('Ctrl Pts',(0.211514048391049,1.85684435807869,11.519907956616));
#68612=CARTESIAN_POINT('Ctrl Pts',(0.212491204601813,1.85769781933947,11.5199882132454));
#68613=CARTESIAN_POINT('Ctrl Pts',(0.228594145571592,1.87193466580153,11.5213219443861));
#68614=CARTESIAN_POINT('Ctrl Pts',(0.24243115815712,1.88670223451989,11.5226363767671));
#68615=CARTESIAN_POINT('Ctrl Pts',(0.265174715581445,1.91606804183148,11.5251235949813));
#68616=CARTESIAN_POINT('Ctrl Pts',(0.274481470815994,1.93026934932985,11.5262803806405));
#68617=CARTESIAN_POINT('Ctrl Pts',(0.287252231163573,1.95357615037385,11.5280619158883));
#68618=CARTESIAN_POINT('Ctrl Pts',(0.291496720035063,1.9622194415589,11.5286991731304));
#68619=CARTESIAN_POINT('Ctrl Pts',(0.296337184543605,1.97330526426592,11.5294769840491));
#68620=CARTESIAN_POINT('Ctrl Pts',(0.297300039901078,1.97558147194635,11.5296346488267));
#68621=CARTESIAN_POINT('Ctrl Pts',(0.298786006309718,1.97921010199178,11.5298825157586));
#68622=CARTESIAN_POINT('Ctrl Pts',(0.299326318979447,1.98055531832086,11.5299736556224));
#68623=CARTESIAN_POINT('Ctrl Pts',(0.300008135942414,1.98228652215027,11.5300899439757));
#68624=CARTESIAN_POINT('Ctrl Pts',(0.300157993173823,1.98266917013226,11.530115584587));
#68625=CARTESIAN_POINT('Ctrl Pts',(0.300396822814261,1.98328245386878,11.5301565783158));
#68626=CARTESIAN_POINT('Ctrl Pts',(0.300486261856708,1.98351290557249,11.5301719595071));
#68627=CARTESIAN_POINT('Ctrl Pts',(0.300654388543525,1.98394758866713,11.5302009283933));
#68628=CARTESIAN_POINT('Ctrl Pts',(0.300733132652277,1.98415179564563,11.5302145194011));
#68629=CARTESIAN_POINT('Ctrl Pts',(0.300911608721305,1.98461604561564,11.5302453766564));
#68630=CARTESIAN_POINT('Ctrl Pts',(0.301011211464575,1.98487613728402,11.5302626350216));
#68631=CARTESIAN_POINT('Ctrl Pts',(0.301312228593085,1.98566524174221,11.5303149086718));
#68632=CARTESIAN_POINT('Ctrl Pts',(0.301512587849395,1.9861946599431,11.5303498607029));
#68633=CARTESIAN_POINT('Ctrl Pts',(0.302909493931732,1.98991535069655,11.5305946840036));
#68634=CARTESIAN_POINT('Ctrl Pts',(0.304056802264673,1.9931250507782,11.5308016771025));
#68635=CARTESIAN_POINT('Ctrl Pts',(0.30835246401238,2.0057720920444,11.531603122784));
#68636=CARTESIAN_POINT('Ctrl Pts',(0.311114334807051,2.01533567591138,11.5321786276792));
#68637=CARTESIAN_POINT('Ctrl Pts',(0.318089201093232,2.04448893066623,11.5338836486623));
#68638=CARTESIAN_POINT('Ctrl Pts',(0.320923469273321,2.06435747231275,11.5349826079845));
#68639=CARTESIAN_POINT('Ctrl Pts',(0.322651337208529,2.09992202811594,11.5370016500021));
#68640=CARTESIAN_POINT('Ctrl Pts',(0.322277938761377,2.11551537065162,11.5379040195773));
#68641=CARTESIAN_POINT('Ctrl Pts',(0.320542517469727,2.13346179084894,11.5389915232467));
#68642=CARTESIAN_POINT('Ctrl Pts',(0.320278449922763,2.13590140601419,11.5391403776386));
#68643=CARTESIAN_POINT('Ctrl Pts',(0.319901635130056,2.13904649854756,11.5393336711109));
#68644=CARTESIAN_POINT('Ctrl Pts',(0.319814361532946,2.13975499153655,11.5393773056542));
#68645=CARTESIAN_POINT('Ctrl Pts',(0.319670068310917,2.14089514185,11.5394476743335));
#68646=CARTESIAN_POINT('Ctrl Pts',(0.319614526238513,2.14132698652482,11.5394743617711));
#68647=CARTESIAN_POINT('Ctrl Pts',(0.31950715678073,2.14214863011245,11.5395252044871));
#68648=CARTESIAN_POINT('Ctrl Pts',(0.31945549072856,2.14253844961513,11.5395493546247));
#68649=CARTESIAN_POINT('Ctrl Pts',(0.319336190075152,2.14342609513884,11.5396044112339));
#68650=CARTESIAN_POINT('Ctrl Pts',(0.319268104684871,2.14392385863166,11.539635331907));
#68651=CARTESIAN_POINT('Ctrl Pts',(0.319057339008716,2.14543835556062,11.5397295545003));
#68652=CARTESIAN_POINT('Ctrl Pts',(0.318910964799818,2.1464545608391,11.5397929731253));
#68653=CARTESIAN_POINT('Ctrl Pts',(0.317822100641731,2.15376624741762,11.5402507139636));
#68654=CARTESIAN_POINT('Ctrl Pts',(0.316698182763316,2.16003289707887,11.5406507583335));
#68655=CARTESIAN_POINT('Ctrl Pts',(0.315175392709095,2.16728099301359,11.5411229586531));
#68656=CARTESIAN_POINT('Ctrl Pts',(0.314956332180802,2.16829911397336,11.5411895062166));
#68657=CARTESIAN_POINT('Ctrl Pts',(0.314119814477821,2.17209735134805,11.5414385905456));
#68658=CARTESIAN_POINT('Ctrl Pts',(0.31347046354994,2.17487024517658,11.541622078546));
#68659=CARTESIAN_POINT('Ctrl Pts',(0.311389630989868,2.18325383010857,11.5421818236745));
#68660=CARTESIAN_POINT('Ctrl Pts',(0.309843664500307,2.1888346787487,11.5425612800199));
#68661=CARTESIAN_POINT('Ctrl Pts',(0.301398072630265,2.21641206096363,11.5444690840411));
#68662=CARTESIAN_POINT('Ctrl Pts',(0.292302442066179,2.2376652227163,11.5460507612595));
#68663=CARTESIAN_POINT('Ctrl Pts',(0.275853287058625,2.26696557423439,11.5482939167655));
#68664=CARTESIAN_POINT('Ctrl Pts',(0.270237857399356,2.27590931943745,11.548986980369));
#68665=CARTESIAN_POINT('Ctrl Pts',(0.263625931597988,2.28537401226372,11.5497170074157));
#68666=CARTESIAN_POINT('Ctrl Pts',(0.263055078675454,2.28618319439693,11.5497793911423));
#68667=CARTESIAN_POINT('Ctrl Pts',(0.26206333046707,2.28757532722642,11.5498866475975));
#68668=CARTESIAN_POINT('Ctrl Pts',(0.261644201190781,2.28815951893643,11.549931635104));
#68669=CARTESIAN_POINT('Ctrl Pts',(0.261043913400579,2.28899032919334,11.5499955779287));
#68670=CARTESIAN_POINT('Ctrl Pts',(0.260864357140167,2.28923809454706,11.5500146424192));
#68671=CARTESIAN_POINT('Ctrl Pts',(0.260552727305522,2.28966681867745,11.5500476223554));
#68672=CARTESIAN_POINT('Ctrl Pts',(0.260420817620313,2.28984789586578,11.5500615492034));
#68673=CARTESIAN_POINT('Ctrl Pts',(0.26016782755644,2.29019442463864,11.5500881958069));
#68674=CARTESIAN_POINT('Ctrl Pts',(0.260046778287583,2.29035989798773,11.5501009177061));
#68675=CARTESIAN_POINT('Ctrl Pts',(0.259761206078221,2.29074949210748,11.5501308652863));
#68676=CARTESIAN_POINT('Ctrl Pts',(0.259596550546737,2.2909735161431,11.5501480816996));
#68677=CARTESIAN_POINT('Ctrl Pts',(0.259109177083391,2.29163482287312,11.5501988926499));
#68678=CARTESIAN_POINT('Ctrl Pts',(0.258785640650641,2.29207150540782,11.5502324305982));
#68679=CARTESIAN_POINT('Ctrl Pts',(0.255933988083595,2.29590014305912,11.5505263717919));
#68680=CARTESIAN_POINT('Ctrl Pts',(0.253340269676402,2.29924302811231,11.5507822974457));
#68681=CARTESIAN_POINT('Ctrl Pts',(0.250496953269214,2.30276226991565,11.5510521042505));
#68682=CARTESIAN_POINT('Ctrl Pts',(0.250312264312243,2.30299022645092,11.551069582536));
#68683=CARTESIAN_POINT('Ctrl Pts',(0.250049060513017,2.30331418627907,11.5510944247329));
#68684=CARTESIAN_POINT('Ctrl Pts',(0.249970801676966,2.3034103962801,11.5511018027744));
#68685=CARTESIAN_POINT('Ctrl Pts',(0.248304773843184,2.30545616736796,11.551258695054));
#68686=CARTESIAN_POINT('Ctrl Pts',(0.246694255513354,2.30738717995559,11.5514069518324));
#68687=CARTESIAN_POINT('Ctrl Pts',(0.228128425389095,2.32912527432822,11.5530803943711));
#68688=CARTESIAN_POINT('Ctrl Pts',(0.208850918622891,2.34682490214154,11.5544926725794));
#68689=CARTESIAN_POINT('Ctrl Pts',(0.174907822703956,2.37113475499553,11.5568594392085));
#68690=CARTESIAN_POINT('Ctrl Pts',(0.161519081643916,2.37931754651797,11.5577669120608));
#68691=CARTESIAN_POINT('Ctrl Pts',(0.145399318262787,2.38762177142336,11.5588605686963));
#68692=CARTESIAN_POINT('Ctrl Pts',(0.143196393845611,2.38872484724655,11.5590100136225));
#68693=CARTESIAN_POINT('Ctrl Pts',(0.140338885087336,2.39011494787469,11.5592039233685));
#68694=CARTESIAN_POINT('Ctrl Pts',(0.139695652374363,2.39042522332378,11.5592475766606));
#68695=CARTESIAN_POINT('Ctrl Pts',(0.138658546069605,2.39092124855844,11.559317968341));
#68696=CARTESIAN_POINT('Ctrl Pts',(0.13826531554256,2.39110834370712,11.5593446599755));
#68697=CARTESIAN_POINT('Ctrl Pts',(0.137516293855436,2.39146286069906,11.5593955059471));
#68698=CARTESIAN_POINT('Ctrl Pts',(0.137160572858918,2.39163042964247,11.559419655133));
#68699=CARTESIAN_POINT('Ctrl Pts',(0.136349773670778,2.39201055995282,11.5594747030017));
#68700=CARTESIAN_POINT('Ctrl Pts',(0.135894504258505,2.39222270892559,11.5595056158694));
#68701=CARTESIAN_POINT('Ctrl Pts',(0.134507686132918,2.39286500440821,11.5595997916401));
#68702=CARTESIAN_POINT('Ctrl Pts',(0.13357458417131,2.39329176405129,11.5596631710777));
#68703=CARTESIAN_POINT('Ctrl Pts',(0.126850040042698,2.39632852698699,11.5601200505271));
#68704=CARTESIAN_POINT('Ctrl Pts',(0.12098493897138,2.39877108937195,11.5605192484609));
#68705=CARTESIAN_POINT('Ctrl Pts',(0.112561613054045,2.40199034050775,11.5610941373801));
#68706=CARTESIAN_POINT('Ctrl Pts',(0.110059756970473,2.40291109542363,11.5612650743948));
#68707=CARTESIAN_POINT('Ctrl Pts',(0.0790684922863867,2.41388214388985,
11.5633848410861));
#68708=CARTESIAN_POINT('Ctrl Pts',(0.0493160837766237,2.41990805106609,
11.5654644547761));
#68709=CARTESIAN_POINT('Ctrl Pts',(0.00779220350546494,2.4223823083516,
11.5682405252315));
#68710=CARTESIAN_POINT('Ctrl Pts',(-0.00361422939399656,2.4224563113289,
11.5689876574152));
#68711=CARTESIAN_POINT('Ctrl Pts',(-0.0157565970924718,2.42189047226933,
11.5697506937988));
#68712=CARTESIAN_POINT('Ctrl Pts',(-0.0165112169790477,2.42185264676695,
11.569797980487));
#68713=CARTESIAN_POINT('Ctrl Pts',(-0.0175786983845659,2.42179537478719,
11.5698646753597));
#68714=CARTESIAN_POINT('Ctrl Pts',(-0.0178916678621757,2.42177812556858,
11.5698842053705));
#68715=CARTESIAN_POINT('Ctrl Pts',(-0.0184285035061297,2.42174775239437,
11.5699176635231));
#68716=CARTESIAN_POINT('Ctrl Pts',(-0.0186523816238351,2.42173485134996,
11.5699316042519));
#68717=CARTESIAN_POINT('Ctrl Pts',(-0.0190806710450227,2.42170972249897,
11.5699582495359));
#68718=CARTESIAN_POINT('Ctrl Pts',(-0.0192850838892537,2.42169753355886,
11.5699709562888));
#68719=CARTESIAN_POINT('Ctrl Pts',(-0.0197660285946986,2.4216683952385,
11.5700008286008));
#68720=CARTESIAN_POINT('Ctrl Pts',(-0.0200425510249569,2.4216512840507,
11.5700179850077));
#68721=CARTESIAN_POINT('Ctrl Pts',(-0.0208576627637052,2.42159978978246,
11.5700685025891));
#68722=CARTESIAN_POINT('Ctrl Pts',(-0.0213961915499814,2.42156441015942,
11.5701018080924));
#68723=CARTESIAN_POINT('Ctrl Pts',(-0.0260523959849527,2.42124676367071,
11.5703891825053));
#68724=CARTESIAN_POINT('Ctrl Pts',(-0.0301646190358144,2.42088675597886,
11.5706389913146));
#68725=CARTESIAN_POINT('Ctrl Pts',(-0.063066890822936,2.4173681530483,11.5726137822695));
#68726=CARTESIAN_POINT('Ctrl Pts',(-0.0913219801422467,2.41042029982934,
11.5741721611729));
#68727=CARTESIAN_POINT('Ctrl Pts',(-0.132986146390127,2.39398315379957,
11.5767100861028));
#68728=CARTESIAN_POINT('Ctrl Pts',(-0.147251921351612,2.38710308795363,
11.5776255706286));
#68729=CARTESIAN_POINT('Ctrl Pts',(-0.163107234313584,2.37796291748983,
11.5787292850434));
#68730=CARTESIAN_POINT('Ctrl Pts',(-0.165246085137236,2.37669673687579,
11.5788800525975));
#68731=CARTESIAN_POINT('Ctrl Pts',(-0.1679778548328,2.37503658267105,11.5790751253761));
#68732=CARTESIAN_POINT('Ctrl Pts',(-0.16858445010462,2.37466518653035,11.5791186025966));
#68733=CARTESIAN_POINT('Ctrl Pts',(-0.169559890647617,2.37406351121688,
11.5791887782749));
#68734=CARTESIAN_POINT('Ctrl Pts',(-0.169929510345819,2.37383448688515,
11.5792154304981));
#68735=CARTESIAN_POINT('Ctrl Pts',(-0.170632616863394,2.37339685517219,
11.5792662460395));
#68736=CARTESIAN_POINT('Ctrl Pts',(-0.170966187720178,2.37318838373902,
11.5792904043049));
#68737=CARTESIAN_POINT('Ctrl Pts',(-0.171725830636405,2.37271169427819,
11.5793455349365));
#68738=CARTESIAN_POINT('Ctrl Pts',(-0.172151656749483,2.3724430879609,11.5793765216458));
#68739=CARTESIAN_POINT('Ctrl Pts',(-0.173448450451586,2.37162083089572,
11.5794711408778));
#68740=CARTESIAN_POINT('Ctrl Pts',(-0.174317383146928,2.37106399730259,
11.5795348915516));
#68741=CARTESIAN_POINT('Ctrl Pts',(-0.180621804251176,2.36698111733284,
11.5800000019099));
#68742=CARTESIAN_POINT('Ctrl Pts',(-0.185952200698111,2.36329626357821,
11.5804072932857));
#68743=CARTESIAN_POINT('Ctrl Pts',(-0.192610371048218,2.35839046437724,
11.5809348582146));
#68744=CARTESIAN_POINT('Ctrl Pts',(-0.194044190173149,2.35731544682622,
11.5810496175182));
#68745=CARTESIAN_POINT('Ctrl Pts',(-0.200437187080528,2.35243842432353,
11.5815664929444));
#68746=CARTESIAN_POINT('Ctrl Pts',(-0.205293871926056,2.34850481347523,
11.581973364511));
#68747=CARTESIAN_POINT('Ctrl Pts',(-0.218592929113318,2.33707737508756,
11.5831275501657));
#68748=CARTESIAN_POINT('Ctrl Pts',(-0.226760106438218,2.32927793946239,
11.58388435836));
#68749=CARTESIAN_POINT('Ctrl Pts',(-0.245321299615967,2.30958878761414,
11.5857118133949));
#68750=CARTESIAN_POINT('Ctrl Pts',(-0.255284670277783,2.29733161726445,
11.5867857237935));
#68751=CARTESIAN_POINT('Ctrl Pts',(-0.267955254158262,2.27916956648074,
11.5882511730193));
#68752=CARTESIAN_POINT('Ctrl Pts',(-0.271444472905799,2.27383803183175,
11.588667332731));
#68753=CARTESIAN_POINT('Ctrl Pts',(-0.276342307012434,2.26584666768287,
11.5892670505577));
#68754=CARTESIAN_POINT('Ctrl Pts',(-0.277875262406565,2.26326520744194,
11.5894572100316));
#68755=CARTESIAN_POINT('Ctrl Pts',(-0.27962410035098,2.26022419878823,11.5896767470799));
#68756=CARTESIAN_POINT('Ctrl Pts',(-0.279875183294306,2.25978520944908,
11.5897083308891));
#68757=CARTESIAN_POINT('Ctrl Pts',(-0.280256781289631,2.25911437066009,
11.5897564290526));
#68758=CARTESIAN_POINT('Ctrl Pts',(-0.280388042836235,2.25888295013964,
11.5897729914233));
#68759=CARTESIAN_POINT('Ctrl Pts',(-0.280615898526883,2.25848006766776,
11.5898017722693));
#68760=CARTESIAN_POINT('Ctrl Pts',(-0.280712621932126,2.25830868025067,
11.5898139991277));
#68761=CARTESIAN_POINT('Ctrl Pts',(-0.280931057294658,2.25792079772892,
11.5898416332746));
#68762=CARTESIAN_POINT('Ctrl Pts',(-0.281052675761352,2.25770425091423,
11.5898570344523));
#68763=CARTESIAN_POINT('Ctrl Pts',(-0.281381518936521,2.25711714318444,
11.5898987196739));
#68764=CARTESIAN_POINT('Ctrl Pts',(-0.281588262819436,2.2567463113719,11.5899249726992));
#68765=CARTESIAN_POINT('Ctrl Pts',(-0.282513225566171,2.25507949065013,
11.5900426375257));
#68766=CARTESIAN_POINT('Ctrl Pts',(-0.283223249255329,2.25377893977755,
11.5901335315008));
#68767=CARTESIAN_POINT('Ctrl Pts',(-0.297898443549344,2.22645193587756,
11.5920252812356));
#68768=CARTESIAN_POINT('Ctrl Pts',(-0.30823167155431,2.19862796003161,11.593618310384));
#68769=CARTESIAN_POINT('Ctrl Pts',(-0.318520117292683,2.15223947607352,
11.5962955128742));
#68770=CARTESIAN_POINT('Ctrl Pts',(-0.320936382997456,2.13440545864712,
11.5973276698267));
#68771=CARTESIAN_POINT('Ctrl Pts',(-0.321990560442423,2.11379795139737,
11.5985708108872));
#68772=CARTESIAN_POINT('Ctrl Pts',(-0.322093819741655,2.11112991915533,
11.5987326684898));
#68773=CARTESIAN_POINT('Ctrl Pts',(-0.322183069083759,2.10773161967271,
11.5989400820847));
#68774=CARTESIAN_POINT('Ctrl Pts',(-0.322199747055235,2.10700220899107,
11.5989846747466));
#68775=CARTESIAN_POINT('Ctrl Pts',(-0.32222249118166,2.10583390614677,11.5990562189057));
#68776=CARTESIAN_POINT('Ctrl Pts',(-0.322230137909884,2.1053950443746,11.5990831208393));
#68777=CARTESIAN_POINT('Ctrl Pts',(-0.322242924628796,2.10456368619702,
11.5991341343135));
#68778=CARTESIAN_POINT('Ctrl Pts',(-0.322248244140542,2.10417119301832,
11.5991582401835));
#68779=CARTESIAN_POINT('Ctrl Pts',(-0.322258664822077,2.1032825008821,11.5992128711703));
#68780=CARTESIAN_POINT('Ctrl Pts',(-0.322263337039576,2.10278629874118,
11.5992434096704));
#68781=CARTESIAN_POINT('Ctrl Pts',(-0.32227239197695,2.1015120666034,11.5993219230351));
#68782=CARTESIAN_POINT('Ctrl Pts',(-0.322275103222484,2.10073403126868,
11.5993699501528));
#68783=CARTESIAN_POINT('Ctrl Pts',(-0.322274377752403,2.09542047604823,
11.599698555776));
#68784=CARTESIAN_POINT('Ctrl Pts',(-0.322178013225252,2.09088567023784,
11.5999820311716));
#68785=CARTESIAN_POINT('Ctrl Pts',(-0.321605378908561,2.07737342051489,
11.6008362740597));
#68786=CARTESIAN_POINT('Ctrl Pts',(-0.320849202675792,2.06841288027864,
11.6014155175924));
#68787=CARTESIAN_POINT('Ctrl Pts',(-0.315383956854345,2.02527246823403,
11.6042653785859));
#68788=CARTESIAN_POINT('Ctrl Pts',(-0.305582855616318,1.99197271155528,
11.606682232021));
#68789=CARTESIAN_POINT('Ctrl Pts',(-0.289313275863257,1.95798168310811,
11.6090977647223));
#68790=CARTESIAN_POINT('Ctrl Pts',(-0.287891731459744,1.95512168285173,
11.6093003244147));
#68791=CARTESIAN_POINT('Ctrl Pts',(-0.286176650735651,1.95179608461336,
11.6095346450617));
#68792=CARTESIAN_POINT('Ctrl Pts',(-0.285924213285312,1.95130964984272,
11.6095688883125));
#68793=CARTESIAN_POINT('Ctrl Pts',(-0.285541569005008,1.95057689061059,
11.6096204226893));
#68794=CARTESIAN_POINT('Ctrl Pts',(-0.285412283173555,1.95033009031703,
11.6096377715127));
#68795=CARTESIAN_POINT('Ctrl Pts',(-0.285180860618937,1.94988970632409,
11.6096687127855));
#68796=CARTESIAN_POINT('Ctrl Pts',(-0.285078846836794,1.94969605920642,
11.6096823129997));
#68797=CARTESIAN_POINT('Ctrl Pts',(-0.284861226729738,1.94928398158569,
11.6097112424425));
#68798=CARTESIAN_POINT('Ctrl Pts',(-0.284745566745866,1.9490655807306,11.6097265681452));
#68799=CARTESIAN_POINT('Ctrl Pts',(-0.284433101514647,1.94847718979725,
11.6097678389454));
#68800=CARTESIAN_POINT('Ctrl Pts',(-0.284235824768456,1.94810744859642,
11.609793754071));
#68801=CARTESIAN_POINT('Ctrl Pts',(-0.283270702998693,1.94630705681918,
11.609919854892));
#68802=CARTESIAN_POINT('Ctrl Pts',(-0.282492757320223,1.94488180544531,
11.6100194078714));
#68803=CARTESIAN_POINT('Ctrl Pts',(-0.277953886764267,1.93671368019125,
11.6105887253818));
#68804=CARTESIAN_POINT('Ctrl Pts',(-0.273962069616423,1.93010123335591,
11.6110448102347));
#68805=CARTESIAN_POINT('Ctrl Pts',(-0.261347311798038,1.91080763514703,
11.6123804553721));
#68806=CARTESIAN_POINT('Ctrl Pts',(-0.252053084280766,1.89859127761922,
11.6132334581119));
#68807=CARTESIAN_POINT('Ctrl Pts',(-0.232263507153112,1.8761057188586,11.6149079425629));
#68808=CARTESIAN_POINT('Ctrl Pts',(-0.221867601011758,1.86579983858226,
11.6157272450068));
#68809=CARTESIAN_POINT('Ctrl Pts',(-0.202071096458281,1.84867971434771,
11.617239284847));
#68810=CARTESIAN_POINT('Ctrl Pts',(-0.192934642654253,1.8415995521945,11.6179211527213));
#68811=CARTESIAN_POINT('Ctrl Pts',(-0.182461551238716,1.8343491575479,11.6186954510481));
#68812=CARTESIAN_POINT('Ctrl Pts',(-0.181480775372377,1.83367817234211,
11.6187678895224));
#68813=CARTESIAN_POINT('Ctrl Pts',(-0.180091934526216,1.83273924902574,
11.6188703738423));
#68814=CARTESIAN_POINT('Ctrl Pts',(-0.17968692915405,1.8324667845299,11.6189002485926));
#68815=CARTESIAN_POINT('Ctrl Pts',(-0.17897746753938,1.83199183700675,11.6189525624917));
#68816=CARTESIAN_POINT('Ctrl Pts',(-0.178673282048293,1.83178894952271,
11.6189749863637));
#68817=CARTESIAN_POINT('Ctrl Pts',(-0.178034119153083,1.83136420664323,
11.619022091784));
#68818=CARTESIAN_POINT('Ctrl Pts',(-0.177699071003547,1.83114245925169,
11.619046777338));
#68819=CARTESIAN_POINT('Ctrl Pts',(-0.176899006707475,1.83061509564786,
11.6191057079155));
#68820=CARTESIAN_POINT('Ctrl Pts',(-0.176433613140975,1.83031005688991,
11.619139974486));
#68821=CARTESIAN_POINT('Ctrl Pts',(-0.1748631052955,1.82928648426307,11.6192555675552));
#68822=CARTESIAN_POINT('Ctrl Pts',(-0.173754384360246,1.82857353292461,
11.6193371018863));
#68823=CARTESIAN_POINT('Ctrl Pts',(-0.158515211917701,1.8189057784121,11.6204569039393));
#68824=CARTESIAN_POINT('Ctrl Pts',(-0.143715155243382,1.81105912853269,
11.6215362852948));
#68825=CARTESIAN_POINT('Ctrl Pts',(-0.100861560692302,1.79244856020525,
11.6246370316621));
#68826=CARTESIAN_POINT('Ctrl Pts',(-0.0718168907659464,1.78440031422148,
11.6267228143369));
#68827=CARTESIAN_POINT('Ctrl Pts',(-0.0383846183829855,1.77999736653987,
11.6288923096056));
#68828=CARTESIAN_POINT('Ctrl Pts',(-0.0346814010707901,1.77957486406645,
11.6291292652265));
#68829=CARTESIAN_POINT('Ctrl Pts',(-0.0303926174221089,1.7791607837939,
11.6293991796128));
#68830=CARTESIAN_POINT('Ctrl Pts',(-0.029813582926488,1.77910645981082,
11.6294355262708));
#68831=CARTESIAN_POINT('Ctrl Pts',(-0.0289539546364591,1.77902815787421,
11.6294893421895));
#68832=CARTESIAN_POINT('Ctrl Pts',(-0.0286734754234494,1.77900298017691,
11.6295068784974));
#68833=CARTESIAN_POINT('Ctrl Pts',(-0.0281746103864681,1.77895885776884,
11.6295380280129));
#68834=CARTESIAN_POINT('Ctrl Pts',(-0.0279562383214456,1.77893976824352,
11.6295516493964));
#68835=CARTESIAN_POINT('Ctrl Pts',(-0.0274934026084197,1.77889978412336,
11.6295804900284));
#68836=CARTESIAN_POINT('Ctrl Pts',(-0.0272489352186839,1.77887894595118,
11.6295957060232));
#68837=CARTESIAN_POINT('Ctrl Pts',(-0.0265947813079852,1.77882393887186,
11.6296363753008));
#68838=CARTESIAN_POINT('Ctrl Pts',(-0.0261850510851788,1.77879027452655,
11.6296618001036));
#68839=CARTESIAN_POINT('Ctrl Pts',(-0.0242440437561171,1.77863453566225,
11.629782019799));
#68840=CARTESIAN_POINT('Ctrl Pts',(-0.0227119380452166,1.77852262378633,
11.6298762510855));
#68841=CARTESIAN_POINT('Ctrl Pts',(-0.0101836873572701,1.7776975168496,
11.6306418095175));
#68842=CARTESIAN_POINT('Ctrl Pts',(0.000842895172138619,1.77753768701612,
11.6312843275724));
#68843=CARTESIAN_POINT('Ctrl Pts',(0.0404173256039185,1.77899469635037,
11.6335458604291));
#68844=CARTESIAN_POINT('Ctrl Pts',(0.0687102306005357,1.78384026189208,
11.6350912251872));
#68845=CARTESIAN_POINT('Ctrl Pts',(0.105375118861746,1.79528074083744,11.6373258087251));
#68846=CARTESIAN_POINT('Ctrl Pts',(0.114616287970004,1.79863507244393,11.6379087836228));
#68847=CARTESIAN_POINT('Ctrl Pts',(0.12465104495111,1.80280582501161,11.63856957402));
#68848=CARTESIAN_POINT('Ctrl Pts',(0.12561096622351,1.80321026672242,11.6386330695936));
#68849=CARTESIAN_POINT('Ctrl Pts',(0.12704366217022,1.80382209732776,11.6387282702642));
#68850=CARTESIAN_POINT('Ctrl Pts',(0.127517933146498,1.80402598281251,11.6387598561118));
#68851=CARTESIAN_POINT('Ctrl Pts',(0.128333868553212,1.80437907245378,11.6388143199164));
#68852=CARTESIAN_POINT('Ctrl Pts',(0.128675768744317,1.80452773199962,11.6388371792547));
#68853=CARTESIAN_POINT('Ctrl Pts',(0.129380842810447,1.80483575685466,11.6388843979801));
#68854=CARTESIAN_POINT('Ctrl Pts',(0.129743981882299,1.8049951999017,11.6389087599966));
#68855=CARTESIAN_POINT('Ctrl Pts',(0.130588510369989,1.80536786701859,11.6389655168954));
#68856=CARTESIAN_POINT('Ctrl Pts',(0.131069672395004,1.80558160078071,11.6389979292017));
#68857=CARTESIAN_POINT('Ctrl Pts',(0.132601260817074,1.80626643605271,11.6391013434893));
#68858=CARTESIAN_POINT('Ctrl Pts',(0.133649678736999,1.80674198343807,11.6391724980422));
#68859=CARTESIAN_POINT('Ctrl Pts',(0.140013600139703,1.80966978194355,11.6396066556019));
#68860=CARTESIAN_POINT('Ctrl Pts',(0.1452637304307,1.8122607341547,11.6399744335374));
#68861=CARTESIAN_POINT('Ctrl Pts',(0.155182720155349,1.81749644611086,11.6406885216269));
#68862=CARTESIAN_POINT('Ctrl Pts',(0.15986185199902,1.82011767187691,11.641033930799));
#68863=CARTESIAN_POINT('Ctrl Pts',(0.177432588813707,1.83054509460032,11.6423638753915));
#68864=CARTESIAN_POINT('Ctrl Pts',(0.189835326956287,1.83913464139733,11.643372984266));
#68865=CARTESIAN_POINT('Ctrl Pts',(0.217442502888987,1.86126847913411,11.6457642146428));
#68866=CARTESIAN_POINT('Ctrl Pts',(0.232058102594201,1.8754490358269,11.6471497636331));
#68867=CARTESIAN_POINT('Ctrl Pts',(0.247857831656728,1.89398075368579,11.6487197220496));
#68868=CARTESIAN_POINT('Ctrl Pts',(0.250416228320391,1.89709817427318,11.6489764471714));
#68869=CARTESIAN_POINT('Ctrl Pts',(0.253284449496401,1.90073003866605,11.649266402911));
#68870=CARTESIAN_POINT('Ctrl Pts',(0.253652025246222,1.90119813897083,11.6493036036124));
#68871=CARTESIAN_POINT('Ctrl Pts',(0.254191384182196,1.90188893284851,11.6493582477198));
#68872=CARTESIAN_POINT('Ctrl Pts',(0.254364173301848,1.90211083389363,11.6493757623403));
#68873=CARTESIAN_POINT('Ctrl Pts',(0.25467145326886,1.90250651959351,11.6494069248232));
#68874=CARTESIAN_POINT('Ctrl Pts',(0.254806056900456,1.90268021568752,11.6494205807547));
#68875=CARTESIAN_POINT('Ctrl Pts',(0.255089115037092,1.9030462540395,11.6494493087416));
#68876=CARTESIAN_POINT('Ctrl Pts',(0.255237529325224,1.90323862603861,11.6494643779174));
#68877=CARTESIAN_POINT('Ctrl Pts',(0.255625086304347,1.90374214696252,11.649503745614));
#68878=CARTESIAN_POINT('Ctrl Pts',(0.255863879390579,1.90405356636553,11.6495280192667));
#68879=CARTESIAN_POINT('Ctrl Pts',(0.25692093544817,1.90543734159228,11.6496355511383));
#68880=CARTESIAN_POINT('Ctrl Pts',(0.257733045384272,1.90651441246081,11.6497183804235));
#68881=CARTESIAN_POINT('Ctrl Pts',(0.263834334288215,1.91471290146194,11.6503425793381));
#68882=CARTESIAN_POINT('Ctrl Pts',(0.268834751355689,1.92204558785675,11.6508651865999));
#68883=CARTESIAN_POINT('Ctrl Pts',(0.285445062684285,1.94870475716014,11.6526776442871));
#68884=CARTESIAN_POINT('Ctrl Pts',(0.29532459810369,1.96903189587887,11.6539081582701));
#68885=CARTESIAN_POINT('Ctrl Pts',(0.309133039964591,2.00714606197448,11.6562012862632));
#68886=CARTESIAN_POINT('Ctrl Pts',(0.313834413111732,2.02454863896376,11.6572430729892));
#68887=CARTESIAN_POINT('Ctrl Pts',(0.317288633751638,2.04351332247817,11.6584139948067));
#68888=CARTESIAN_POINT('Ctrl Pts',(0.317511002865627,2.04477695380665,11.6584921671831));
#68889=CARTESIAN_POINT('Ctrl Pts',(0.317811052036545,2.04654375632469,11.6586016916113));
#68890=CARTESIAN_POINT('Ctrl Pts',(0.317895096510152,2.04704584629552,11.6586328415039));
#68891=CARTESIAN_POINT('Ctrl Pts',(0.318038323393932,2.04791412786243,11.6586867544743));
#68892=CARTESIAN_POINT('Ctrl Pts',(0.318098064042576,2.04828022743618,11.6587094997998));
#68893=CARTESIAN_POINT('Ctrl Pts',(0.318220544424159,2.04903904538053,11.6587566728148));
#68894=CARTESIAN_POINT('Ctrl Pts',(0.318283189524069,2.04943177822474,11.6587811034646));
#68895=CARTESIAN_POINT('Ctrl Pts',(0.318428136743616,2.05035141734731,11.6588383488025));
#68896=CARTESIAN_POINT('Ctrl Pts',(0.318509858077849,2.05087841277801,11.6588711818371));
#68897=CARTESIAN_POINT('Ctrl Pts',(0.318769383208879,2.05257988850592,11.6589772821713));
#68898=CARTESIAN_POINT('Ctrl Pts',(0.318942000137274,2.05375513938439,11.6590507134631));
#68899=CARTESIAN_POINT('Ctrl Pts',(0.319328600653571,2.05649245765527,11.6592220930409));
#68900=CARTESIAN_POINT('Ctrl Pts',(0.319537624892319,2.05805518420373,11.6593201965411));
#68901=CARTESIAN_POINT('Ctrl Pts',(0.32158934226764,2.07430074640087,11.6603428715395));
#68902=CARTESIAN_POINT('Ctrl Pts',(0.322429874233752,2.08909025726703,11.6612990911777));
#68903=CARTESIAN_POINT('Ctrl Pts',(0.321975591097415,2.12678690609023,11.6637971479464));
#68904=CARTESIAN_POINT('Ctrl Pts',(0.319258802395855,2.14959353172216,11.6653691607795));
#68905=CARTESIAN_POINT('Ctrl Pts',(0.313256289760883,2.17581316446439,11.6671624285807));
#68906=CARTESIAN_POINT('Ctrl Pts',(0.312292296682133,2.1796910446217,11.6674270968607));
#68907=CARTESIAN_POINT('Ctrl Pts',(0.311072082449083,2.1842368130202,11.6677359799147));
#68908=CARTESIAN_POINT('Ctrl Pts',(0.310885481460665,2.18492289784849,11.6677825619809));
#68909=CARTESIAN_POINT('Ctrl Pts',(0.31029683662742,2.18705925397643,11.6679274840545));
#68910=CARTESIAN_POINT('Ctrl Pts',(0.309886898089565,2.18850735038045,11.6680255347787));
#68911=CARTESIAN_POINT('Ctrl Pts',(0.30806018014137,2.19479187066617,11.6684501151593));
#68912=CARTESIAN_POINT('Ctrl Pts',(0.306540116345514,2.19959787870943,11.6687723726319));
#68913=CARTESIAN_POINT('Ctrl Pts',(0.304702551508788,2.20496634030109,11.6691280575734));
#68914=CARTESIAN_POINT('Ctrl Pts',(0.304495486311521,2.20556550726584,11.6691676942922));
#68915=CARTESIAN_POINT('Ctrl Pts',(0.304191584724653,2.2064365477278,11.6692252236362));
#68916=CARTESIAN_POINT('Ctrl Pts',(0.304096150606751,2.2067089035518,11.6692431986329));
#68917=CARTESIAN_POINT('Ctrl Pts',(0.303927044721102,2.20718943920772,11.6692748893394));
#68918=CARTESIAN_POINT('Ctrl Pts',(0.303853524718333,2.20739767179972,11.6692886141064));
#68919=CARTESIAN_POINT('Ctrl Pts',(0.30369987500955,2.20783143710921,11.6693171872511));
#68920=CARTESIAN_POINT('Ctrl Pts',(0.303619708251891,2.20805695568442,11.6693320333437));
#68921=CARTESIAN_POINT('Ctrl Pts',(0.303412767844019,2.20863705506181,11.669370198254));
#68922=CARTESIAN_POINT('Ctrl Pts',(0.30328562337729,2.20899150462009,11.669393494926));
#68923=CARTESIAN_POINT('Ctrl Pts',(0.302747497313431,2.2104834434498,11.6694914622987));
#68924=CARTESIAN_POINT('Ctrl Pts',(0.302330728541014,2.21161885635859,11.669565792367));
#68925=CARTESIAN_POINT('Ctrl Pts',(0.301234494287541,2.21455416271915,11.6697574315919));
#68926=CARTESIAN_POINT('Ctrl Pts',(0.300545275993852,2.21635039417139,11.6698741931758));
#68927=CARTESIAN_POINT('Ctrl Pts',(0.297556638115072,2.22393554887978,11.6703655206203));
#68928=CARTESIAN_POINT('Ctrl Pts',(0.295105593015899,2.22966369072847,11.6707322610364));
#68929=CARTESIAN_POINT('Ctrl Pts',(0.284879350479015,2.25176778895219,11.6721438452319));
#68930=CARTESIAN_POINT('Ctrl Pts',(0.275894079011462,2.26754777038506,11.6731451304909));
#68931=CARTESIAN_POINT('Ctrl Pts',(0.252564213523024,2.30150640374914,11.675452940969));
#68932=CARTESIAN_POINT('Ctrl Pts',(0.237497327138924,2.31906232258689,11.6767650541417));
#68933=CARTESIAN_POINT('Ctrl Pts',(0.219635087677082,2.33584674485049,11.6782522888263));
#68934=CARTESIAN_POINT('Ctrl Pts',(0.218576652532869,2.33682800859974,11.6783401630285));
#68935=CARTESIAN_POINT('Ctrl Pts',(0.217116698444672,2.33816339224909,11.678461043699));
#68936=CARTESIAN_POINT('Ctrl Pts',(0.216720824415134,2.33852368102661,11.6784937883162));
#68937=CARTESIAN_POINT('Ctrl Pts',(0.216043914286319,2.33913666712065,11.678549723828));
#68938=CARTESIAN_POINT('Ctrl Pts',(0.215763326998765,2.33938986023259,11.6785728937459));
#68939=CARTESIAN_POINT('Ctrl Pts',(0.215218433398933,2.33987981879738,11.6786178584926));
#68940=CARTESIAN_POINT('Ctrl Pts',(0.2149541800147,2.34011664255857,11.678639650824));
#68941=CARTESIAN_POINT('Ctrl Pts',(0.214324081043995,2.34067946324338,11.6786915807907));
#68942=CARTESIAN_POINT('Ctrl Pts',(0.213957882815853,2.34100506243483,11.6787217350297));
#68943=CARTESIAN_POINT('Ctrl Pts',(0.212867825331273,2.34196982677535,11.6788114181472));
#68944=CARTESIAN_POINT('Ctrl Pts',(0.21214183913221,2.34260657078502,11.6788710478177));
#68945=CARTESIAN_POINT('Ctrl Pts',(0.206255398754909,2.34772279295457,11.6793537533184));
#68946=CARTESIAN_POINT('Ctrl Pts',(0.200956867167417,2.35204007158081,11.6797834652237));
#68947=CARTESIAN_POINT('Ctrl Pts',(0.187643444634022,2.36220112035548,11.6808529751251));
#68948=CARTESIAN_POINT('Ctrl Pts',(0.179488730895552,2.36784931207831,11.6814996458115));
#68949=CARTESIAN_POINT('Ctrl Pts',(0.155240465916205,2.38303929248595,11.6833958241118));
#68950=CARTESIAN_POINT('Ctrl Pts',(0.138560330615208,2.3915678244327,11.6846703045923));
#68951=CARTESIAN_POINT('Ctrl Pts',(0.107339552280378,2.40424391470092,11.6869397568061));
#68952=CARTESIAN_POINT('Ctrl Pts',(0.0930636111457863,2.40891005785235,
11.6879365643188));
#68953=CARTESIAN_POINT('Ctrl Pts',(0.0776272905968485,2.41278748864775,
11.6889375328384));
#68954=CARTESIAN_POINT('Ctrl Pts',(0.0767407883785567,2.41300616726648,
11.6889947521092));
#68955=CARTESIAN_POINT('Ctrl Pts',(0.0755476888938698,2.41329510248296,
11.6890713923113));
#68956=CARTESIAN_POINT('Ctrl Pts',(0.075241911878687,2.41336867941118,11.6890910017969));
#68957=CARTESIAN_POINT('Ctrl Pts',(0.0747270389134289,2.41349177254316,
11.6891239653934));
#68958=CARTESIAN_POINT('Ctrl Pts',(0.0745180011093741,2.41354152724687,
11.6891373332667));
#68959=CARTESIAN_POINT('Ctrl Pts',(0.0741170851783154,2.41363652876188,
11.689162942107));
#68960=CARTESIAN_POINT('Ctrl Pts',(0.0739252166960136,2.41368180824816,
11.6891751848684));
#68961=CARTESIAN_POINT('Ctrl Pts',(0.0735290342556281,2.41377492056864,
11.6892004377969));
#68962=CARTESIAN_POINT('Ctrl Pts',(0.0733247158077496,2.41382272975159,
11.6892134465479));
#68963=CARTESIAN_POINT('Ctrl Pts',(0.0727010144003571,2.41396802944874,
11.6892531127247));
#68964=CARTESIAN_POINT('Ctrl Pts',(0.072281480449289,2.41406487960281,11.6892797332001));
#68965=CARTESIAN_POINT('Ctrl Pts',(0.0701513391982144,2.41455213210589,
11.6894145920859));
#68966=CARTESIAN_POINT('Ctrl Pts',(0.0684377157826533,2.41492941048388,
11.6895220874162));
#68967=CARTESIAN_POINT('Ctrl Pts',(0.0636351078458215,2.41594572030417,
11.6898207961471));
#68968=CARTESIAN_POINT('Ctrl Pts',(0.0605396151090193,2.41655344220464,
11.6900103777501));
#68969=CARTESIAN_POINT('Ctrl Pts',(0.0493213918298268,2.418585272238,11.6906884293629));
#68970=CARTESIAN_POINT('Ctrl Pts',(0.0411531768135743,2.41974303959515,
11.691165193645));
#68971=CARTESIAN_POINT('Ctrl Pts',(0.0219252772709739,2.42171923116479,
11.6922663191834));
#68972=CARTESIAN_POINT('Ctrl Pts',(0.0108500919752149,2.42228290911793,
11.6928844785792));
#68973=CARTESIAN_POINT('Ctrl Pts',(-0.026349379231974,2.42225608012335,
11.6949638055561));
#68974=CARTESIAN_POINT('Ctrl Pts',(-0.0523627545378986,2.41906292409022,
11.696432267091));
#68975=CARTESIAN_POINT('Ctrl Pts',(-0.0791787362356968,2.41240072264719,
11.6981080005207));
#68976=CARTESIAN_POINT('Ctrl Pts',(-0.080650547254897,2.41202399408809,
11.6982004683781));
#68977=CARTESIAN_POINT('Ctrl Pts',(-0.08264857140053,2.41149749354986,11.6983266872025));
#68978=CARTESIAN_POINT('Ctrl Pts',(-0.0831771643241079,2.41135676349097,
11.6983601453683));
#68979=CARTESIAN_POINT('Ctrl Pts',(-0.0840734690315348,2.41111569023454,
11.6984169914503));
#68980=CARTESIAN_POINT('Ctrl Pts',(-0.0844413670449397,2.41101603887046,
11.6984403568963));
#68981=CARTESIAN_POINT('Ctrl Pts',(-0.085150492101369,2.41082260945812,
11.6984854566663));
#68982=CARTESIAN_POINT('Ctrl Pts',(-0.0854917433633932,2.41072892152256,
11.6985071880369));
#68983=CARTESIAN_POINT('Ctrl Pts',(-0.0862979438368308,2.41050615670808,
11.6985585947473));
#68984=CARTESIAN_POINT('Ctrl Pts',(-0.086762757867981,2.41037659755082,
11.6985882857314));
#68985=CARTESIAN_POINT('Ctrl Pts',(-0.0881222202801561,2.40999437761453,
11.6986752790105));
#68986=CARTESIAN_POINT('Ctrl Pts',(-0.0890160628457078,2.40973889065822,
11.6987326732174));
#68987=CARTESIAN_POINT('Ctrl Pts',(-0.0955137384121603,2.4078512114935,
11.6991513405159));
#68988=CARTESIAN_POINT('Ctrl Pts',(-0.101073105861682,2.40607100927709,
11.6995174282468));
#68989=CARTESIAN_POINT('Ctrl Pts',(-0.119370659259948,2.39965895631597,
11.7007498438901));
#68990=CARTESIAN_POINT('Ctrl Pts',(-0.131863520340114,2.39437523243346,
11.7016370915332));
#68991=CARTESIAN_POINT('Ctrl Pts',(-0.156027163894041,2.38230809878514,
11.7034397379492));
#68992=CARTESIAN_POINT('Ctrl Pts',(-0.16767985280604,2.37554632807435,11.7043531213799));
#68993=CARTESIAN_POINT('Ctrl Pts',(-0.191221103348493,2.35983831857301,
11.7062658056417));
#68994=CARTESIAN_POINT('Ctrl Pts',(-0.202984559992781,2.35075649383721,
11.7072620933955));
#68995=CARTESIAN_POINT('Ctrl Pts',(-0.216576113052761,2.33867782766144,
11.708428811427));
#68996=CARTESIAN_POINT('Ctrl Pts',(-0.219036767035541,2.33642168895417,
11.7086406807862));
#68997=CARTESIAN_POINT('Ctrl Pts',(-0.221865632774627,2.3337458561133,11.7088845507742));
#68998=CARTESIAN_POINT('Ctrl Pts',(-0.222268243982232,2.33336304759886,
11.7089192660681));
#68999=CARTESIAN_POINT('Ctrl Pts',(-0.222872443920402,2.33278558350855,
11.7089713713294));
#69000=CARTESIAN_POINT('Ctrl Pts',(-0.223074769299489,2.33259170546664,
11.7089888208954));
#69001=CARTESIAN_POINT('Ctrl Pts',(-0.223434800798351,2.33224580383475,
11.709019873798));
#69002=CARTESIAN_POINT('Ctrl Pts',(-0.223592604692754,2.33209388344898,
11.7090334851205));
#69003=CARTESIAN_POINT('Ctrl Pts',(-0.223927417576696,2.3317708952344,11.7090623655788));
#69004=CARTESIAN_POINT('Ctrl Pts',(-0.224104384985417,2.33159978594896,
11.7090776313369));
#69005=CARTESIAN_POINT('Ctrl Pts',(-0.224464926652284,2.33125037906326,
11.7091087348809));
#69006=CARTESIAN_POINT('Ctrl Pts',(-0.224648484985861,2.33107206518433,
11.7091245713763));
#69007=CARTESIAN_POINT('Ctrl Pts',(-0.225106451055752,2.33062612220227,
11.7091640857884));
#69008=CARTESIAN_POINT('Ctrl Pts',(-0.225380594993654,2.33035822093609,
11.7091877426331));
#69009=CARTESIAN_POINT('Ctrl Pts',(-0.228482204711251,2.32731640264702,
11.7094554352374));
#69010=CARTESIAN_POINT('Ctrl Pts',(-0.231258934104973,2.32449092110601,
11.7096955018236));
#69011=CARTESIAN_POINT('Ctrl Pts',(-0.240431501661529,2.31480643737695,
11.7104929587089));
#69012=CARTESIAN_POINT('Ctrl Pts',(-0.246580321137079,2.30771925200631,
11.7110351008034));
#69013=CARTESIAN_POINT('Ctrl Pts',(-0.256877153641243,2.29474826262257,
11.7119772671885));
#69014=CARTESIAN_POINT('Ctrl Pts',(-0.261153422113637,2.28897527214057,
11.7123805541285));
#69015=CARTESIAN_POINT('Ctrl Pts',(-0.278346260679777,2.26406534111136,
11.7140747231586));
#69016=CARTESIAN_POINT('Ctrl Pts',(-0.289378786448976,2.24371461358229,
11.7153544460444));
#69017=CARTESIAN_POINT('Ctrl Pts',(-0.298348076118668,2.22186014041684,
11.7167446716449));
#69018=CARTESIAN_POINT('Ctrl Pts',(-0.298552234293598,2.22135910241772,
11.7167765487307));
#69019=CARTESIAN_POINT('Ctrl Pts',(-0.299422126779447,2.21920876235513,
11.7169133816852));
#69020=CARTESIAN_POINT('Ctrl Pts',(-0.300075454400406,2.21755450020109,
11.7170187078431));
#69021=CARTESIAN_POINT('Ctrl Pts',(-0.302547578480107,2.21114002754951,
11.7174274673825));
#69022=CARTESIAN_POINT('Ctrl Pts',(-0.304266991499749,2.20634254274059,
11.7177339474231));
#69023=CARTESIAN_POINT('Ctrl Pts',(-0.306143539801097,2.20068789692954,
11.7180967647819));
#69024=CARTESIAN_POINT('Ctrl Pts',(-0.306411914166872,2.19986820507022,
11.7181493963221));
#69025=CARTESIAN_POINT('Ctrl Pts',(-0.306835661514563,2.19855617169906,
11.7182337047387));
#69026=CARTESIAN_POINT('Ctrl Pts',(-0.306993148798102,2.19806451316955,
11.7182653120054));
#69027=CARTESIAN_POINT('Ctrl Pts',(-0.307269468453475,2.19719468357653,
11.718321256941));
#69028=CARTESIAN_POINT('Ctrl Pts',(-0.307388786045428,2.1968166668013,11.7183455786138));
#69029=CARTESIAN_POINT('Ctrl Pts',(-0.307634480680699,2.19603323515355,
11.7183960032265));
#69030=CARTESIAN_POINT('Ctrl Pts',(-0.307760754392193,2.19562778890543,
11.7184221095017));
#69031=CARTESIAN_POINT('Ctrl Pts',(-0.3080829155303,2.19458612965494,11.7184892077374));
#69032=CARTESIAN_POINT('Ctrl Pts',(-0.308277633036435,2.19394955946454,
11.7185302379382));
#69033=CARTESIAN_POINT('Ctrl Pts',(-0.30869366980271,2.19257423286936,11.71861894199));
#69034=CARTESIAN_POINT('Ctrl Pts',(-0.308914312006688,2.19183527747259,
11.7186666377402));
#69035=CARTESIAN_POINT('Ctrl Pts',(-0.310021486365612,2.18807808644813,
11.718909331594));
#69036=CARTESIAN_POINT('Ctrl Pts',(-0.310866420089562,2.18504786329901,
11.7191056804272));
#69037=CARTESIAN_POINT('Ctrl Pts',(-0.318735136329981,2.15514245817528,
11.7210500832756));
#69038=CARTESIAN_POINT('Ctrl Pts',(-0.322298937199578,2.12748432642362,
11.7229160354673));
#69039=CARTESIAN_POINT('Ctrl Pts',(-0.322274879003935,2.09972073668561,
11.7247944044677));
#69040=CARTESIAN_POINT('',(-0.322274882473144,2.10017262650289,11.9744806947813));
#69041=CARTESIAN_POINT('Ctrl Pts',(-0.322274878830663,2.09972053679725,
11.7247944179913));
#69042=CARTESIAN_POINT('Ctrl Pts',(-0.322258357831344,2.08066864373516,
11.7260833897981));
#69043=CARTESIAN_POINT('Ctrl Pts',(-0.320552428193726,2.0616526188374,11.7273676966839));
#69044=CARTESIAN_POINT('Ctrl Pts',(-0.317040312090144,2.04214501967275,
11.7286169371805));
#69045=CARTESIAN_POINT('Ctrl Pts',(-0.31690239481546,2.04139427991564,11.7286649034451));
#69046=CARTESIAN_POINT('Ctrl Pts',(-0.316686225496915,2.04024066078012,
11.7287384336421));
#69047=CARTESIAN_POINT('Ctrl Pts',(-0.316609870106264,2.03983743523448,
11.7287641014531));
#69048=CARTESIAN_POINT('Ctrl Pts',(-0.316482519396665,2.03917186535682,
11.7288064129159));
#69049=CARTESIAN_POINT('Ctrl Pts',(-0.316431967886135,2.03890943813674,
11.7288230814444));
#69050=CARTESIAN_POINT('Ctrl Pts',(-0.316340940502728,2.03844003359228,
11.7288528702927));
#69051=CARTESIAN_POINT('Ctrl Pts',(-0.316300587867842,2.03823303295985,
11.7288659976201));
#69052=CARTESIAN_POINT('Ctrl Pts',(-0.316222029871392,2.03783214253678,
11.7288914029485));
#69053=CARTESIAN_POINT('Ctrl Pts',(-0.316183849369666,2.03763824829164,
11.7289036823447));
#69054=CARTESIAN_POINT('Ctrl Pts',(-0.316104141202829,2.03723541669019,
11.7289291768685));
#69055=CARTESIAN_POINT('Ctrl Pts',(-0.316062584844273,2.0370264859976,11.7289423902863));
#69056=CARTESIAN_POINT('Ctrl Pts',(-0.315947853945584,2.036452633936,11.7289786568704));
#69057=CARTESIAN_POINT('Ctrl Pts',(-0.315874254068038,2.03608779641753,
11.7290016856212));
#69058=CARTESIAN_POINT('Ctrl Pts',(-0.315588033875181,2.03468156304085,
11.7290903410722));
#69059=CARTESIAN_POINT('Ctrl Pts',(-0.315370891194541,2.0336410790217,11.7291557120302));
#69060=CARTESIAN_POINT('Ctrl Pts',(-0.311263355965539,2.01443460896736,
11.730358545139));
#69061=CARTESIAN_POINT('Ctrl Pts',(-0.30581382126515,1.9966344346182,11.7314103826875));
#69062=CARTESIAN_POINT('Ctrl Pts',(-0.297707451480833,1.97654584893946,
11.7326246449452));
#69063=CARTESIAN_POINT('Ctrl Pts',(-0.296514504510577,1.97370747109345,
11.7327968396689));
#69064=CARTESIAN_POINT('Ctrl Pts',(-0.294235888609452,1.96849629863782,
11.7331147972916));
#69065=CARTESIAN_POINT('Ctrl Pts',(-0.293161724471731,1.96611876563191,
11.733260570526));
#69066=CARTESIAN_POINT('Ctrl Pts',(-0.289843927380256,1.95900666174207,
11.733699385616));
#69067=CARTESIAN_POINT('Ctrl Pts',(-0.287513617992391,1.95431354882682,
11.7339926716667));
#69068=CARTESIAN_POINT('Ctrl Pts',(-0.278203408493568,1.93665754731237,
11.735116110529));
#69069=CARTESIAN_POINT('Ctrl Pts',(-0.270453392731345,1.92412280084275,
11.7359567844403));
#69070=CARTESIAN_POINT('Ctrl Pts',(-0.258376519481509,1.90728579213341,
11.7371836552982));
#69071=CARTESIAN_POINT('Ctrl Pts',(-0.254743302284678,1.90250814072322,
11.7375437221857));
#69072=CARTESIAN_POINT('Ctrl Pts',(-0.250366235949369,1.89707420643385,
11.7379685736147));
#69073=CARTESIAN_POINT('Ctrl Pts',(-0.249750022135621,1.89631628389044,
11.738028187837));
#69074=CARTESIAN_POINT('Ctrl Pts',(-0.24881807558594,1.89518060820616,11.738118056729));
#69075=CARTESIAN_POINT('Ctrl Pts',(-0.24850490354374,1.89480075316036,11.7381482075975));
#69076=CARTESIAN_POINT('Ctrl Pts',(-0.247964305069852,1.89414809892012,
11.7382001711221));
#69077=CARTESIAN_POINT('Ctrl Pts',(-0.247737295154548,1.89387495456681,
11.738221966796));
#69078=CARTESIAN_POINT('Ctrl Pts',(-0.247268371999136,1.89331262742267,
11.7382669378538));
#69079=CARTESIAN_POINT('Ctrl Pts',(-0.247026401956639,1.89302349285848,
11.7382901155404));
#69080=CARTESIAN_POINT('Ctrl Pts',(-0.246372562586775,1.89224498766539,
11.7383526704311));
#69081=CARTESIAN_POINT('Ctrl Pts',(-0.245959744420385,1.89175641940034,
11.7383920864978));
#69082=CARTESIAN_POINT('Ctrl Pts',(-0.244433787483275,1.88996132438122,
11.7385374963559));
#69083=CARTESIAN_POINT('Ctrl Pts',(-0.243311685935253,1.88866248552757,
11.7386438592414));
#69084=CARTESIAN_POINT('Ctrl Pts',(-0.224173958965546,1.866864904691,11.7404486931334));
#69085=CARTESIAN_POINT('Ctrl Pts',(-0.203640703875255,1.84873171117412,
11.742263101875));
#69086=CARTESIAN_POINT('Ctrl Pts',(-0.174853944328719,1.82917933412451,
11.7446174232807));
#69087=CARTESIAN_POINT('Ctrl Pts',(-0.168486629653042,1.82517279446666,
11.7451268872452));
#69088=CARTESIAN_POINT('Ctrl Pts',(-0.154874298789226,1.81725845766967,
11.7461865073697));
#69089=CARTESIAN_POINT('Ctrl Pts',(-0.147607568234485,1.81339774973521,
11.7467356447559));
#69090=CARTESIAN_POINT('Ctrl Pts',(-0.13600980730416,1.80779429961115,11.7475787927971));
#69091=CARTESIAN_POINT('Ctrl Pts',(-0.131775305159434,1.80586038529376,
11.7478799431085));
#69092=CARTESIAN_POINT('Ctrl Pts',(-0.126086839063073,1.80340995838733,
11.748274292824));
#69093=CARTESIAN_POINT('Ctrl Pts',(-0.124669140740509,1.80281125638688,
11.7483717432364));
#69094=CARTESIAN_POINT('Ctrl Pts',(-0.122307174138058,1.80183366093716,
11.7485326603685));
#69095=CARTESIAN_POINT('Ctrl Pts',(-0.121365319681414,1.80144904984179,
11.748596449517));
#69096=CARTESIAN_POINT('Ctrl Pts',(-0.120173618139414,1.80096898383512,
11.7486766692601));
#69097=CARTESIAN_POINT('Ctrl Pts',(-0.119925466091536,1.8008693768447,11.7486933468897));
#69098=CARTESIAN_POINT('Ctrl Pts',(-0.119481332684988,1.8006917454184,11.7487231476064));
#69099=CARTESIAN_POINT('Ctrl Pts',(-0.119285398542744,1.80061360449083,
11.7487362777163));
#69100=CARTESIAN_POINT('Ctrl Pts',(-0.118905737971855,1.80046262309496,
11.7487616871518));
#69101=CARTESIAN_POINT('Ctrl Pts',(-0.118722021266612,1.80038975926554,
11.7487739678759));
#69102=CARTESIAN_POINT('Ctrl Pts',(-0.118340213229229,1.80023873681532,
11.7487994593262));
#69103=CARTESIAN_POINT('Ctrl Pts',(-0.118142112032152,1.80016060575966,
11.7488126683528));
#69104=CARTESIAN_POINT('Ctrl Pts',(-0.117597900401303,1.79994659191713,
11.7488489085078));
#69105=CARTESIAN_POINT('Ctrl Pts',(-0.117251630629727,1.79981111113348,
11.748871915282));
#69106=CARTESIAN_POINT('Ctrl Pts',(-0.115917086858522,1.79929162176353,
11.7489603873084));
#69107=CARTESIAN_POINT('Ctrl Pts',(-0.114927140457945,1.79891188627372,
11.7490255981782));
#69108=CARTESIAN_POINT('Ctrl Pts',(-0.0975638905877046,1.79234959602426,
11.7501623926708));
#69109=CARTESIAN_POINT('Ctrl Pts',(-0.0807129274239811,1.78750504435862,
11.7511579841937));
#69110=CARTESIAN_POINT('Ctrl Pts',(-0.0449280728360833,1.78030728269999,
11.7532075353054));
#69111=CARTESIAN_POINT('Ctrl Pts',(-0.0260126232552263,1.77821546568542,
11.7542565112898));
#69112=CARTESIAN_POINT('Ctrl Pts',(0.00478950206968854,1.77754404360837,
11.7560245429554));
#69113=CARTESIAN_POINT('Ctrl Pts',(0.0166062876633351,1.77793639184922,
11.7567164723318));
#69114=CARTESIAN_POINT('Ctrl Pts',(0.0307648249340058,1.77918780903631,
11.7575740533033));
#69115=CARTESIAN_POINT('Ctrl Pts',(0.033153163073487,1.77942582196759,11.7577196781388));
#69116=CARTESIAN_POINT('Ctrl Pts',(0.0362418092435508,1.77976850948186,
11.7579093222204));
#69117=CARTESIAN_POINT('Ctrl Pts',(0.0369447840398306,1.7798488494845,11.757952573734));
#69118=CARTESIAN_POINT('Ctrl Pts',(0.0380785062502868,1.77998220153079,
11.7580224725321));
#69119=CARTESIAN_POINT('Ctrl Pts',(0.0385094237913649,1.78003377013867,
11.758049074244));
#69120=CARTESIAN_POINT('Ctrl Pts',(0.039330900900313,1.7801337611734,11.7580998512577));
#69121=CARTESIAN_POINT('Ctrl Pts',(0.0397214787946563,1.78018202891819,
11.758124021634));
#69122=CARTESIAN_POINT('Ctrl Pts',(0.0406130640235536,1.78029386977093,
11.7581792606267));
#69123=CARTESIAN_POINT('Ctrl Pts',(0.0411140113856175,1.78035790524622,
11.7582103437934));
#69124=CARTESIAN_POINT('Ctrl Pts',(0.0426459795508157,1.78055739575476,
11.758305544018));
#69125=CARTESIAN_POINT('Ctrl Pts',(0.0436764894256331,1.78069666270193,
11.758369781362));
#69126=CARTESIAN_POINT('Ctrl Pts',(0.0512906053982372,1.78176321211027,
11.7588459058248));
#69127=CARTESIAN_POINT('Ctrl Pts',(0.0578443630311506,1.78288898091934,
11.7592640451124));
#69128=CARTESIAN_POINT('Ctrl Pts',(0.0661755824306511,1.78458692513058,
11.7598068497073));
#69129=CARTESIAN_POINT('Ctrl Pts',(0.067989654627021,1.78497298187326,11.7599257278585));
#69130=CARTESIAN_POINT('Ctrl Pts',(0.0722858348494677,1.78592609812625,
11.7602088936562));
#69131=CARTESIAN_POINT('Ctrl Pts',(0.0747647285274502,1.78650694971935,
11.7603735796461));
#69132=CARTESIAN_POINT('Ctrl Pts',(0.0916792670192907,1.79068237296024,
11.7615061557513));
#69133=CARTESIAN_POINT('Ctrl Pts',(0.105856486095041,1.79524303949041,11.7625009824833));
#69134=CARTESIAN_POINT('Ctrl Pts',(0.134850615103314,1.80683808428629,11.7646101919796));
#69135=CARTESIAN_POINT('Ctrl Pts',(0.149550754543677,1.81405733675741,11.7657237341072));
#69136=CARTESIAN_POINT('Ctrl Pts',(0.167951729265524,1.82490284665707,11.7671330871891));
#69137=CARTESIAN_POINT('Ctrl Pts',(0.172204100899809,1.82754453513131,11.7674598126102));
#69138=CARTESIAN_POINT('Ctrl Pts',(0.178407147214478,1.83160131354508,11.7679360941594));
#69139=CARTESIAN_POINT('Ctrl Pts',(0.180406118597845,1.83294083385767,11.7680895264074));
#69140=CARTESIAN_POINT('Ctrl Pts',(0.183572549349485,1.83511445440992,11.768332246967));
#69141=CARTESIAN_POINT('Ctrl Pts',(0.184749726214653,1.83593415218344,11.7684224106087));
#69142=CARTESIAN_POINT('Ctrl Pts',(0.186248715108876,1.83699286643263,11.7685370892849));
#69143=CARTESIAN_POINT('Ctrl Pts',(0.186575584211952,1.83722464429261,11.7685620878989));
#69144=CARTESIAN_POINT('Ctrl Pts',(0.187101497838295,1.8375990375636,11.7686022948937));
#69145=CARTESIAN_POINT('Ctrl Pts',(0.187300812286686,1.83774127031004,11.7686175294956));
#69146=CARTESIAN_POINT('Ctrl Pts',(0.187678335107111,1.83801132419063,11.7686463788368));
#69147=CARTESIAN_POINT('Ctrl Pts',(0.187856573624218,1.83813909900984,11.7686599965318));
#69148=CARTESIAN_POINT('Ctrl Pts',(0.188264093107926,1.83843186993913,11.7686911253479));
#69149=CARTESIAN_POINT('Ctrl Pts',(0.188493287310915,1.83859698537034,11.7687086280551));
#69150=CARTESIAN_POINT('Ctrl Pts',(0.189197254081118,1.83910554235006,11.7687623744014));
#69151=CARTESIAN_POINT('Ctrl Pts',(0.189671310653218,1.83944998001894,11.7687985494251));
#69152=CARTESIAN_POINT('Ctrl Pts',(0.193231114661388,1.84205130879584,11.7690700810946));
#69153=CARTESIAN_POINT('Ctrl Pts',(0.196277585772294,1.84436177238076,11.7693018043733));
#69154=CARTESIAN_POINT('Ctrl Pts',(0.205983871660226,1.85199892397352,11.7700405502315));
#69155=CARTESIAN_POINT('Ctrl Pts',(0.212473999017151,1.85753616329091,11.7705352656361));
#69156=CARTESIAN_POINT('Ctrl Pts',(0.230085147851148,1.87381253880505,11.7719042433702));
#69157=CARTESIAN_POINT('Ctrl Pts',(0.240664423655455,1.88510324536843,11.7727594998356));
#69158=CARTESIAN_POINT('Ctrl Pts',(0.264782072222983,1.91486758388619,11.7749071415005));
#69159=CARTESIAN_POINT('Ctrl Pts',(0.277238784185174,1.93410250623397,11.7762105954028));
#69160=CARTESIAN_POINT('Ctrl Pts',(0.288071407502033,1.95551005780231,11.7776695524184));
#69161=CARTESIAN_POINT('Ctrl Pts',(0.288581490011106,1.95653152685366,11.7777391689828));
#69162=CARTESIAN_POINT('Ctrl Pts',(0.289320578544577,1.95803148301144,11.7778414067238));
#69163=CARTESIAN_POINT('Ctrl Pts',(0.289553852210817,1.95850786718032,11.7778738788605));
#69164=CARTESIAN_POINT('Ctrl Pts',(0.289959760409528,1.95934200783372,11.777930740625));
#69165=CARTESIAN_POINT('Ctrl Pts',(0.290132912040883,1.95969951259745,11.77795511219));
#69166=CARTESIAN_POINT('Ctrl Pts',(0.290466812210881,1.96039217500428,11.778002334506));
#69167=CARTESIAN_POINT('Ctrl Pts',(0.290627642816581,1.96072729260524,11.7780251823591));
#69168=CARTESIAN_POINT('Ctrl Pts',(0.291008635641253,1.96152468891259,11.7780795509204));
#69169=CARTESIAN_POINT('Ctrl Pts',(0.291228276144563,1.96198721447788,11.7781110896634));
#69170=CARTESIAN_POINT('Ctrl Pts',(0.292001854695574,1.9636263088293,11.7782228667951));
#69171=CARTESIAN_POINT('Ctrl Pts',(0.292549766802917,1.96480569297037,11.7783033132202));
#69172=CARTESIAN_POINT('Ctrl Pts',(0.302002168028159,1.9854785906559,11.7797138555546));
#69173=CARTESIAN_POINT('Ctrl Pts',(0.308945720199433,2.00580511466784,11.7811130502327));
#69174=CARTESIAN_POINT('Ctrl Pts',(0.318545781976656,2.04688721452165,11.7839454490837));
#69175=CARTESIAN_POINT('Ctrl Pts',(0.321305555521644,2.0675171414673,11.7853688126219));
#69176=CARTESIAN_POINT('Ctrl Pts',(0.322329488724655,2.09562862630801,11.7872223375088));
#69177=CARTESIAN_POINT('Ctrl Pts',(0.322345239189801,2.1029957365363,11.7876996961705));
#69178=CARTESIAN_POINT('Ctrl Pts',(0.322069741459443,2.11156343222941,11.7882402996076));
#69179=CARTESIAN_POINT('Ctrl Pts',(0.32202419281672,2.11276912991203,11.788316039976));
#69180=CARTESIAN_POINT('Ctrl Pts',(0.321955555706071,2.11435051851738,11.788414914027));
#69181=CARTESIAN_POINT('Ctrl Pts',(0.321938579642829,2.1147264446734,11.7884383836547));
#69182=CARTESIAN_POINT('Ctrl Pts',(0.32190973176689,2.11534136487403,11.7884767164492));
#69183=CARTESIAN_POINT('Ctrl Pts',(0.321898252215036,2.11558037561262,11.7884916016271));
#69184=CARTESIAN_POINT('Ctrl Pts',(0.321875665641876,2.11603995846333,11.788520195994));
#69185=CARTESIAN_POINT('Ctrl Pts',(0.321864598119062,2.11626053128858,11.7885339073225));
#69186=CARTESIAN_POINT('Ctrl Pts',(0.321838538878732,2.11676943275992,11.7885655137618));
#69187=CARTESIAN_POINT('Ctrl Pts',(0.321823386384843,2.1170577536633,11.7885833997797));
#69188=CARTESIAN_POINT('Ctrl Pts',(0.3217736892413,2.11797974604633,11.788640530314));
#69189=CARTESIAN_POINT('Ctrl Pts',(0.321737660071789,2.11861334100938,11.78867969178));
#69190=CARTESIAN_POINT('Ctrl Pts',(0.32139742612532,2.12430015637966,11.7890303309067));
#69191=CARTESIAN_POINT('Ctrl Pts',(0.320976046170345,2.12934600283102,11.7893353986273));
#69192=CARTESIAN_POINT('Ctrl Pts',(0.320313048749553,2.13552538623077,11.78970384451));
#69193=CARTESIAN_POINT('Ctrl Pts',(0.320184035140333,2.1366699601125,11.789771871841));
#69194=CARTESIAN_POINT('Ctrl Pts',(0.319931153549727,2.13881030048345,11.7898987147928));
#69195=CARTESIAN_POINT('Ctrl Pts',(0.319808766330212,2.13980622381987,11.7899575870811));
#69196=CARTESIAN_POINT('Ctrl Pts',(0.316843118895036,2.16304217557256,11.7913279905411));
#69197=CARTESIAN_POINT('Ctrl Pts',(0.311691099760403,2.18492775296392,11.7925550281665));
#69198=CARTESIAN_POINT('Ctrl Pts',(0.297747301946518,2.22491927571672,11.7949365619973));
#69199=CARTESIAN_POINT('Ctrl Pts',(0.289456582201734,2.24308388088151,11.7960789470654));
#69200=CARTESIAN_POINT('Ctrl Pts',(0.278615209895248,2.26198214311942,11.7973974035842));
#69201=CARTESIAN_POINT('Ctrl Pts',(0.277673715326556,2.26359082329075,11.7975106943063));
#69202=CARTESIAN_POINT('Ctrl Pts',(0.276380174828903,2.26575768404406,11.79766476984));
#69203=CARTESIAN_POINT('Ctrl Pts',(0.276040278957232,2.26632310495274,11.7977051114966));
#69204=CARTESIAN_POINT('Ctrl Pts',(0.27547943067571,2.26724962813779,11.7977714442932));
#69205=CARTESIAN_POINT('Ctrl Pts',(0.275259497501414,2.2676113476773,11.7977973980613));
#69206=CARTESIAN_POINT('Ctrl Pts',(0.274831970781404,2.26831138111555,11.7978477374538));
#69207=CARTESIAN_POINT('Ctrl Pts',(0.274624463568972,2.26864974706126,11.7978721198744));
#69208=CARTESIAN_POINT('Ctrl Pts',(0.274143938595106,2.26943006349542,11.7979284661934));
#69209=CARTESIAN_POINT('Ctrl Pts',(0.273870476845853,2.26987173806047,11.7979604464106));
#69210=CARTESIAN_POINT('Ctrl Pts',(0.272991330782801,2.27128402695609,11.7980629862771));
#69211=CARTESIAN_POINT('Ctrl Pts',(0.272381550396838,2.27225206971811,11.7981336971865));
#69212=CARTESIAN_POINT('Ctrl Pts',(0.266717805087173,2.28113814017874,11.7987867538698));
#69213=CARTESIAN_POINT('Ctrl Pts',(0.261325544388627,2.28883416953473,11.7993817237438));
#69214=CARTESIAN_POINT('Ctrl Pts',(0.251872262981872,2.30114449346192,11.8003847679703));
#69215=CARTESIAN_POINT('Ctrl Pts',(0.248001440858772,2.30589808711745,11.8007857119392));
#69216=CARTESIAN_POINT('Ctrl Pts',(0.227662105725203,2.32946981486172,11.8028429286825));
#69217=CARTESIAN_POINT('Ctrl Pts',(0.209180734789248,2.34643393556545,11.8045639601435));
#69218=CARTESIAN_POINT('Ctrl Pts',(0.181555619120013,2.36642351475296,11.8068281901526));
#69219=CARTESIAN_POINT('Ctrl Pts',(0.173962360821164,2.37144255925349,11.8074221833282));
#69220=CARTESIAN_POINT('Ctrl Pts',(0.164991719543398,2.37684072475377,11.8080834490993));
#69221=CARTESIAN_POINT('Ctrl Pts',(0.163812758172484,2.37753996976898,11.8081695761182));
#69222=CARTESIAN_POINT('Ctrl Pts',(0.162289313951313,2.37843043893781,11.8082798330742));
#69223=CARTESIAN_POINT('Ctrl Pts',(0.161948915003612,2.37862856939478,11.8083044027569));
#69224=CARTESIAN_POINT('Ctrl Pts',(0.161397657919383,2.37894807910312,11.8083440839672));
#69225=CARTESIAN_POINT('Ctrl Pts',(0.161187025374068,2.37906984371154,11.8083592205061));
#69226=CARTESIAN_POINT('Ctrl Pts',(0.160785955008397,2.37930109299815,11.8083879936448));
#69227=CARTESIAN_POINT('Ctrl Pts',(0.160595544725543,2.37941062057926,11.8084016329572));
#69228=CARTESIAN_POINT('Ctrl Pts',(0.160161617150881,2.37965963379146,11.8084326683852));
#69229=CARTESIAN_POINT('Ctrl Pts',(0.15991802990074,2.37979899587893,11.8084500564044));
#69230=CARTESIAN_POINT('Ctrl Pts',(0.159159996015875,2.38023137191248,11.8085040629998));
#69231=CARTESIAN_POINT('Ctrl Pts',(0.158644920066477,2.38052328866954,11.8085406108402));
#69232=CARTESIAN_POINT('Ctrl Pts',(0.154678558884764,2.38275678611862,11.8088209274459));
#69233=CARTESIAN_POINT('Ctrl Pts',(0.151192369877625,2.3846361316279,11.8090607943519));
#69234=CARTESIAN_POINT('Ctrl Pts',(0.146594411267985,2.38700648888283,11.8093698981345));
#69235=CARTESIAN_POINT('Ctrl Pts',(0.145513441970028,2.38755605430353,11.8094420517271));
#69236=CARTESIAN_POINT('Ctrl Pts',(0.144323493189536,2.38815259667175,11.8095209427483));
#69237=CARTESIAN_POINT('Ctrl Pts',(0.144217575896015,2.38820562183606,11.809527960182));
#69238=CARTESIAN_POINT('Ctrl Pts',(0.143194695477665,2.38871699936055,11.8095956853169));
#69239=CARTESIAN_POINT('Ctrl Pts',(0.142275569439957,2.38917103748531,11.8096561943016));
#69240=CARTESIAN_POINT('Ctrl Pts',(0.126043049663522,2.39709359372834,11.8107190102569));
#69241=CARTESIAN_POINT('Ctrl Pts',(0.110161823517475,2.40334128709682,11.811668806838));
#69242=CARTESIAN_POINT('Ctrl Pts',(0.0777240397127478,2.41321660566566,
11.8135640327894));
#69243=CARTESIAN_POINT('Ctrl Pts',(0.061228309141513,2.41685439574087,11.8145069310016));
#69244=CARTESIAN_POINT('Ctrl Pts',(0.0360242051667638,2.42037025066754,
11.8159840525524));
#69245=CARTESIAN_POINT('Ctrl Pts',(0.0274803215562856,2.42121589880442,
11.8164906218053));
#69246=CARTESIAN_POINT('Ctrl Pts',(0.0163604997795346,2.42186961553835,
11.8171621255569));
#69247=CARTESIAN_POINT('Ctrl Pts',(0.0138059799212023,2.42198930059415,
11.8173172095709));
#69248=CARTESIAN_POINT('Ctrl Pts',(0.0105322509925847,2.42210365354363,
11.8175170933146));
#69249=CARTESIAN_POINT('Ctrl Pts',(0.00981406307787783,2.42212633560431,
11.8175610136008));
#69250=CARTESIAN_POINT('Ctrl Pts',(0.00865952887527339,2.42215893387814,
11.8176317328388));
#69251=CARTESIAN_POINT('Ctrl Pts',(0.00822322502517501,2.42217036593247,
11.8176584842447));
#69252=CARTESIAN_POINT('Ctrl Pts',(0.00739400962481082,2.42219040752398,
11.8177093769649));
#69253=CARTESIAN_POINT('Ctrl Pts',(0.00700110260858537,2.42219918472722,
11.817733512979));
#69254=CARTESIAN_POINT('Ctrl Pts',(0.00610778547895219,2.42221750586125,
11.8177884382155));
#69255=CARTESIAN_POINT('Ctrl Pts',(0.00560736809805012,2.42222660278972,
11.8178192413877));
#69256=CARTESIAN_POINT('Ctrl Pts',(0.00412331072681669,2.42225012287198,
11.8179106980219));
#69257=CARTESIAN_POINT('Ctrl Pts',(0.0031396302956104,2.4222612078262,11.8179714558947));
#69258=CARTESIAN_POINT('Ctrl Pts',(-0.00360499709869908,2.42230632837212,
11.8183890043709));
#69259=CARTESIAN_POINT('Ctrl Pts',(-0.00936558974634618,2.42219038490161,
11.8187504670316));
#69260=CARTESIAN_POINT('Ctrl Pts',(-0.0162913166439642,2.42186510272379,
11.819191244171));
#69261=CARTESIAN_POINT('Ctrl Pts',(-0.0174626163683917,2.42180367978286,
11.8192660025406));
#69262=CARTESIAN_POINT('Ctrl Pts',(-0.0513626445563393,2.4198403375196,
11.8214358662419));
#69263=CARTESIAN_POINT('Ctrl Pts',(-0.083607918300789,2.41296138676534,
11.8236957992876));
#69264=CARTESIAN_POINT('Ctrl Pts',(-0.124568318091742,2.39743179102914,
11.8266152975117));
#69265=CARTESIAN_POINT('Ctrl Pts',(-0.134679767225662,2.39299207485365,
11.827337462497));
#69266=CARTESIAN_POINT('Ctrl Pts',(-0.145179240796961,2.38772324883421,
11.8280744936241));
#69267=CARTESIAN_POINT('Ctrl Pts',(-0.14581287106627,2.38740265575012,11.8281189205441));
#69268=CARTESIAN_POINT('Ctrl Pts',(-0.146717682533934,2.3869410926603,11.8281822812153));
#69269=CARTESIAN_POINT('Ctrl Pts',(-0.146989725126854,2.38680183007471,
11.8282013209847));
#69270=CARTESIAN_POINT('Ctrl Pts',(-0.147459763948895,2.38656036587058,
11.8282341996362));
#69271=CARTESIAN_POINT('Ctrl Pts',(-0.147657852710915,2.38645834567303,
11.8282480500063));
#69272=CARTESIAN_POINT('Ctrl Pts',(-0.148039362459526,2.38626135863725,
11.8282747139783));
#69273=CARTESIAN_POINT('Ctrl Pts',(-0.148222797553566,2.38616642111238,
11.8282875294092));
#69274=CARTESIAN_POINT('Ctrl Pts',(-0.14865818230571,2.38594055514912,11.8283179354342));
#69275=CARTESIAN_POINT('Ctrl Pts',(-0.148910050957868,2.38580946970068,
11.8283355160567));
#69276=CARTESIAN_POINT('Ctrl Pts',(-0.149664084723506,2.38541576429168,
11.8283881217005));
#69277=CARTESIAN_POINT('Ctrl Pts',(-0.1501657340924,2.38515215075168,11.8284230843498));
#69278=CARTESIAN_POINT('Ctrl Pts',(-0.155006881105659,2.38259184069591,
11.8287601743047));
#69279=CARTESIAN_POINT('Ctrl Pts',(-0.159294341576421,2.3801974317452,11.8290562566643));
#69280=CARTESIAN_POINT('Ctrl Pts',(-0.165386879340408,2.37660987133092,
11.8294758619985));
#69281=CARTESIAN_POINT('Ctrl Pts',(-0.167237050380818,2.37549520901356,
11.8296031327435));
#69282=CARTESIAN_POINT('Ctrl Pts',(-0.16965739164014,2.3740036707823,11.8297696084987));
#69283=CARTESIAN_POINT('Ctrl Pts',(-0.170237728877009,2.37364348671123,
11.8298095239649));
#69284=CARTESIAN_POINT('Ctrl Pts',(-0.182206386362924,2.36616237464167,
11.8306327922391));
#69285=CARTESIAN_POINT('Ctrl Pts',(-0.193140532014059,2.35833769497382,
11.8313865547347));
#69286=CARTESIAN_POINT('Ctrl Pts',(-0.212647012642128,2.34244577287646,
11.8327939443665));
#69287=CARTESIAN_POINT('Ctrl Pts',(-0.221327718684909,2.33454794245605,
11.8334470657655));
#69288=CARTESIAN_POINT('Ctrl Pts',(-0.236672016406793,2.31897546261698,
11.834685523274));
#69289=CARTESIAN_POINT('Ctrl Pts',(-0.243440550226437,2.3114250962219,11.8352672648673));
#69290=CARTESIAN_POINT('Ctrl Pts',(-0.254753569990906,2.29754052727777,
11.836319382539));
#69291=CARTESIAN_POINT('Ctrl Pts',(-0.259445219213881,2.29133688695115,
11.8367837582573));
#69292=CARTESIAN_POINT('Ctrl Pts',(-0.26447554142552,2.2841598286851,11.8373173544009));
#69293=CARTESIAN_POINT('Ctrl Pts',(-0.265039662540447,2.28334702550041,
11.8373777317379));
#69294=CARTESIAN_POINT('Ctrl Pts',(-0.265880317129291,2.28212379715537,
11.8374685232586));
#69295=CARTESIAN_POINT('Ctrl Pts',(-0.266159666204504,2.28171530647875,
11.8374988304081));
#69296=CARTESIAN_POINT('Ctrl Pts',(-0.266638088351222,2.28101224231749,
11.8375509726073));
#69297=CARTESIAN_POINT('Ctrl Pts',(-0.266837617456695,2.28071797900809,
11.8375727903431));
#69298=CARTESIAN_POINT('Ctrl Pts',(-0.26724718425741,2.28011179733906,11.8376177226416));
#69299=CARTESIAN_POINT('Ctrl Pts',(-0.267457163715863,2.27979984040434,
11.8376408393615));
#69300=CARTESIAN_POINT('Ctrl Pts',(-0.268020039298423,2.27896043389243,
11.8377030239784));
#69301=CARTESIAN_POINT('Ctrl Pts',(-0.268371922898259,2.27843231028932,
11.837742129916));
#69302=CARTESIAN_POINT('Ctrl Pts',(-0.269652033914422,2.276498705992,11.8378852432835));
#69303=CARTESIAN_POINT('Ctrl Pts',(-0.270570786436317,2.27508701255458,
11.8379896048751));
#69304=CARTESIAN_POINT('Ctrl Pts',(-0.285988659492705,2.25098576838733,
11.8397694514625));
#69305=CARTESIAN_POINT('Ctrl Pts',(-0.297595819282992,2.2265793046525,11.8415575433361));
#69306=CARTESIAN_POINT('Ctrl Pts',(-0.306993897314332,2.19810874971128,
11.8435855798235));
#69307=CARTESIAN_POINT('Ctrl Pts',(-0.307913549237319,2.19518311788768,
11.8437931629675));
#69308=CARTESIAN_POINT('Ctrl Pts',(-0.311247655873619,2.18402213070639,
11.8445812641169));
#69309=CARTESIAN_POINT('Ctrl Pts',(-0.313374665135546,2.17570435945351,
11.8451608812378));
#69310=CARTESIAN_POINT('Ctrl Pts',(-0.3174896470563,2.1564370796737,11.8464743064071));
#69311=CARTESIAN_POINT('Ctrl Pts',(-0.319248051768745,2.14544845427597,
11.8472022648895));
#69312=CARTESIAN_POINT('Ctrl Pts',(-0.320510752778471,2.13368290768133,
11.8479446849101));
#69313=CARTESIAN_POINT('Ctrl Pts',(-0.320584267995804,2.13297587076742,
11.8479891578022));
#69314=CARTESIAN_POINT('Ctrl Pts',(-0.320686057364261,2.13196438198879,
11.8480525722451));
#69315=CARTESIAN_POINT('Ctrl Pts',(-0.320716237875869,2.13166013058033,
11.8480716200598));
#69316=CARTESIAN_POINT('Ctrl Pts',(-0.320767666625017,2.13113405418223,
11.848104508174));
#69317=CARTESIAN_POINT('Ctrl Pts',(-0.320789117811177,2.1309122496268,11.8481183599797));
#69318=CARTESIAN_POINT('Ctrl Pts',(-0.32083000555721,2.13048484553704,11.8481450234474));
#69319=CARTESIAN_POINT('Ctrl Pts',(-0.320849474508391,2.13027925001634,
11.8481578369448));
#69320=CARTESIAN_POINT('Ctrl Pts',(-0.320895230721912,2.12979105699431,
11.8481882335886));
#69321=CARTESIAN_POINT('Ctrl Pts',(-0.320921342374644,2.12950844263593,
11.8482058067782));
#69322=CARTESIAN_POINT('Ctrl Pts',(-0.321011955699495,2.12851335989533,
11.8482676006445));
#69323=CARTESIAN_POINT('Ctrl Pts',(-0.321074459008251,2.12780070485117,
11.8483117094844));
#69324=CARTESIAN_POINT('Ctrl Pts',(-0.321889070701451,2.11814323507957,
11.8489075331983));
#69325=CARTESIAN_POINT('Ctrl Pts',(-0.322269600647659,2.10917003746095,
11.8494389452187));
#69326=CARTESIAN_POINT('Ctrl Pts',(-0.322284274189371,2.08450966955439,
11.8508668647107));
#69327=CARTESIAN_POINT('Ctrl Pts',(-0.321148945012806,2.06884677325038,
11.851738443188));
#69328=CARTESIAN_POINT('Ctrl Pts',(-0.315240713484417,2.02847994117197,
11.8540195117517));
#69329=CARTESIAN_POINT('Ctrl Pts',(-0.308712891507352,2.00414633866884,
11.8554360006477));
#69330=CARTESIAN_POINT('Ctrl Pts',(-0.298835027863087,1.97932949640279,
11.8570550188287));
#69331=CARTESIAN_POINT('Ctrl Pts',(-0.298231232476188,1.97784486851709,
11.8571525319499));
#69332=CARTESIAN_POINT('Ctrl Pts',(-0.297377942157259,1.9757908155867,11.8572883832299));
#69333=CARTESIAN_POINT('Ctrl Pts',(-0.297137828864432,1.97521749872879,
11.8573264032261));
#69334=CARTESIAN_POINT('Ctrl Pts',(-0.296750777633431,1.97430079115112,
11.8573873600653));
#69335=CARTESIAN_POINT('Ctrl Pts',(-0.296604897871146,1.973956953035,11.8574102608891));
#69336=CARTESIAN_POINT('Ctrl Pts',(-0.296303028280497,1.97324887352863,
11.8574574984729));
#69337=CARTESIAN_POINT('Ctrl Pts',(-0.296146963822613,1.97288466478659,
11.8574818377459));
#69338=CARTESIAN_POINT('Ctrl Pts',(-0.295782888023978,1.9720393281884,11.8575384280255));
#69339=CARTESIAN_POINT('Ctrl Pts',(-0.295574374208098,1.9715584191759,11.8575706961416));
#69340=CARTESIAN_POINT('Ctrl Pts',(-0.294909112237652,1.97003428108864,
11.8576731997394));
#69341=CARTESIAN_POINT('Ctrl Pts',(-0.29444801092008,1.96899297200225,11.8577435840178));
#69342=CARTESIAN_POINT('Ctrl Pts',(-0.285787813666087,1.94971226951271,
11.8590534412962));
#69343=CARTESIAN_POINT('Ctrl Pts',(-0.27591580065792,1.93227618811299,11.8603526939427));
#69344=CARTESIAN_POINT('Ctrl Pts',(-0.247643213747223,1.89166402675304,
11.8636627652313));
#69345=CARTESIAN_POINT('Ctrl Pts',(-0.227549557780284,1.86988627721789,
11.8657099719235));
#69346=CARTESIAN_POINT('Ctrl Pts',(-0.203623533619788,1.85019837393665,
11.8676695236398));
#69347=CARTESIAN_POINT('Ctrl Pts',(-0.202466377476437,1.84925957242019,
11.8677632342839));
#69348=CARTESIAN_POINT('Ctrl Pts',(-0.200970458605046,1.84806304076782,
11.8678829767281));
#69349=CARTESIAN_POINT('Ctrl Pts',(-0.200637663452224,1.84779792889735,
11.8679095272247));
#69350=CARTESIAN_POINT('Ctrl Pts',(-0.200109619252282,1.84737898406483,
11.8679515135071));
#69351=CARTESIAN_POINT('Ctrl Pts',(-0.199914717071086,1.84722471776537,
11.8679669803497));
#69352=CARTESIAN_POINT('Ctrl Pts',(-0.199565205221356,1.84694873403057,
11.867994661863));
#69353=CARTESIAN_POINT('Ctrl Pts',(-0.19941066367725,1.84682693358912,11.8680068824943));
#69354=CARTESIAN_POINT('Ctrl Pts',(-0.199047120205912,1.84654094965893,
11.8680355854545));
#69355=CARTESIAN_POINT('Ctrl Pts',(-0.198838026974118,1.84637688336367,
11.8680520593087));
#69356=CARTESIAN_POINT('Ctrl Pts',(-0.19823151483918,1.84590219092132,11.8680997448379));
#69357=CARTESIAN_POINT('Ctrl Pts',(-0.197833567044267,1.84559223712172,
11.8681309085613));
#69358=CARTESIAN_POINT('Ctrl Pts',(-0.195085038511268,1.84346181045368,
11.8683453085849));
#69359=CARTESIAN_POINT('Ctrl Pts',(-0.192709993592025,1.84167293050021,
11.8685263486336));
#69360=CARTESIAN_POINT('Ctrl Pts',(-0.185193755521249,1.83617307446806,
11.8690873647851));
#69361=CARTESIAN_POINT('Ctrl Pts',(-0.179967348573326,1.83258059491871,
11.8694603542844));
#69362=CARTESIAN_POINT('Ctrl Pts',(-0.161472693599664,1.8206559015049,11.8707346192801));
#69363=CARTESIAN_POINT('Ctrl Pts',(-0.147705132802424,1.81313798701479,
11.871605283269));
#69364=CARTESIAN_POINT('Ctrl Pts',(-0.110494886851804,1.79621103429578,
11.8738909348181));
#69365=CARTESIAN_POINT('Ctrl Pts',(-0.0864033617983778,1.78850191072719,
11.875313000937));
#69366=CARTESIAN_POINT('Ctrl Pts',(-0.0601407595611295,1.78338246264711,
11.8769353967941));
#69367=CARTESIAN_POINT('Ctrl Pts',(-0.0586179968316454,1.78309700816043,
11.8770296802902));
#69368=CARTESIAN_POINT('Ctrl Pts',(-0.0565504585056609,1.78272484269528,
11.8771580020592));
#69369=CARTESIAN_POINT('Ctrl Pts',(-0.0560074143208578,1.78262853100025,
11.8771917348199));
#69370=CARTESIAN_POINT('Ctrl Pts',(-0.0550874280701067,1.78246780143117,
11.8772489320117));
#69371=CARTESIAN_POINT('Ctrl Pts',(-0.0547106123608324,1.78240265940597,
11.8772723733894));
#69372=CARTESIAN_POINT('Ctrl Pts',(-0.0539851810074332,1.78227857978515,
11.8773175292657));
#69373=CARTESIAN_POINT('Ctrl Pts',(-0.0536365823558393,1.78221954486885,
11.8773392406389));
#69374=CARTESIAN_POINT('Ctrl Pts',(-0.0528146352802478,1.78208173976765,
11.8773904620561));
#69375=CARTESIAN_POINT('Ctrl Pts',(-0.0523412076390352,1.78200345305664,
11.8774199874018));
#69376=CARTESIAN_POINT('Ctrl Pts',(-0.0509626512087354,1.78177865481395,
11.8775060281071));
#69377=CARTESIAN_POINT('Ctrl Pts',(-0.0500570754135329,1.78163494927446,
11.8775626323308));
#69378=CARTESIAN_POINT('Ctrl Pts',(-0.0435855719649405,1.78063628247278,
11.8779677568109));
#69379=CARTESIAN_POINT('Ctrl Pts',(-0.0379989908904124,1.77992351479139,
11.8783207536229));
#69380=CARTESIAN_POINT('Ctrl Pts',(-0.0198728252425622,1.77809209464067,
11.8794776300977));
#69381=CARTESIAN_POINT('Ctrl Pts',(-0.00728683287487953,1.77756168578663,
11.8802992322672));
#69382=CARTESIAN_POINT('Ctrl Pts',(0.0368384164631355,1.77828700113255,
11.883235446806));
#69383=CARTESIAN_POINT('Ctrl Pts',(0.0681313773255557,1.78343340978731,
11.8854351470669));
#69384=CARTESIAN_POINT('Ctrl Pts',(0.0996567720394734,1.79351653253819,
11.8875295500734));
#69385=CARTESIAN_POINT('Ctrl Pts',(0.101132736536379,1.79400039563498,11.8876272676468));
#69386=CARTESIAN_POINT('Ctrl Pts',(0.103010142977465,1.7946309305739,11.8877510783012));
#69387=CARTESIAN_POINT('Ctrl Pts',(0.10341483798138,1.79476774513709,11.88777773818));
#69388=CARTESIAN_POINT('Ctrl Pts',(0.104057295772176,1.79498636416991,11.8878200138478));
#69389=CARTESIAN_POINT('Ctrl Pts',(0.104295235127536,1.79506764229351,11.8878356606814));
#69390=CARTESIAN_POINT('Ctrl Pts',(0.104739574125223,1.79522000575755,11.8878648607357));
#69391=CARTESIAN_POINT('Ctrl Pts',(0.104945995115022,1.79529102181243,11.8878784179014));
#69392=CARTESIAN_POINT('Ctrl Pts',(0.105409641091001,1.79545105930514,11.8879088511974));
#69393=CARTESIAN_POINT('Ctrl Pts',(0.105666824935934,1.79554019670479,11.8879257202929));
#69394=CARTESIAN_POINT('Ctrl Pts',(0.106429226274875,1.79580551993146,11.8879756920193));
#69395=CARTESIAN_POINT('Ctrl Pts',(0.106934121427034,1.79598263932137,11.8880087393361));
#69396=CARTESIAN_POINT('Ctrl Pts',(0.110979180094051,1.79741298688306,11.8882731513907));
#69397=CARTESIAN_POINT('Ctrl Pts',(0.114497816973326,1.79872681530517,11.8885009858784));
#69398=CARTESIAN_POINT('Ctrl Pts',(0.127127971983891,1.8036960641637,11.8893136682817));
#69399=CARTESIAN_POINT('Ctrl Pts',(0.136094933320498,1.80770606039616,11.8898809487722));
#69400=CARTESIAN_POINT('Ctrl Pts',(0.17334106174489,1.82644884197759,11.8922512176522));
#69401=CARTESIAN_POINT('Ctrl Pts',(0.199531473828622,1.84492233697124,11.8939730704327));
#69402=CARTESIAN_POINT('Ctrl Pts',(0.22661699792488,1.87079050115555,11.8961948397034));
#69403=CARTESIAN_POINT('Ctrl Pts',(0.23054799738413,1.87474487083542,11.8965296739284));
#69404=CARTESIAN_POINT('Ctrl Pts',(0.235042760660081,1.87950731347566,11.8969283760793));
#69405=CARTESIAN_POINT('Ctrl Pts',(0.235708014946101,1.88021861815218,11.8969878088939));
#69406=CARTESIAN_POINT('Ctrl Pts',(0.236708808978657,1.88129845961459,11.8970778647568));
#69407=CARTESIAN_POINT('Ctrl Pts',(0.237046738934835,1.88166478165217,11.8971083857105));
#69408=CARTESIAN_POINT('Ctrl Pts',(0.237649460408076,1.88232119106848,11.8971630243864));
#69409=CARTESIAN_POINT('Ctrl Pts',(0.237914574477576,1.88261098201822,11.8971871283389));
#69410=CARTESIAN_POINT('Ctrl Pts',(0.238467999778197,1.88321814523423,11.8972375934571));
#69411=CARTESIAN_POINT('Ctrl Pts',(0.238756208534521,1.88353560949364,11.8972639588897));
#69412=CARTESIAN_POINT('Ctrl Pts',(0.23951118487641,1.88437056413067,11.8973332475421));
#69413=CARTESIAN_POINT('Ctrl Pts',(0.23997690708086,1.88488899295959,11.8973762146872));
#69414=CARTESIAN_POINT('Ctrl Pts',(0.240992621419867,1.88602706131453,11.8974704201715));
#69415=CARTESIAN_POINT('Ctrl Pts',(0.241541911743713,1.88664731799404,11.897521687546));
#69416=CARTESIAN_POINT('Ctrl Pts',(0.243147718865144,1.8884747393112,11.8976725170221));
#69417=CARTESIAN_POINT('Ctrl Pts',(0.244197609384204,1.88968766912045,11.8977723533518));
#69418=CARTESIAN_POINT('Ctrl Pts',(0.255131809680098,1.90251212134189,11.8988251624081));
#69419=CARTESIAN_POINT('Ctrl Pts',(0.264187728835675,1.91480165729399,11.8998117902089));
#69420=CARTESIAN_POINT('Ctrl Pts',(0.289755626950704,1.95521084335876,11.9029850798514));
#69421=CARTESIAN_POINT('Ctrl Pts',(0.302897445200297,1.98521645232034,11.9052612673115));
#69422=CARTESIAN_POINT('Ctrl Pts',(0.311698195297557,2.01810025438366,11.9074136872392));
#69423=CARTESIAN_POINT('Ctrl Pts',(0.312068256596787,2.01952182467518,11.9075060574541));
#69424=CARTESIAN_POINT('Ctrl Pts',(0.312532393362588,2.02135613320944,11.9076243288732));
#69425=CARTESIAN_POINT('Ctrl Pts',(0.312635385857129,2.02176656597363,11.9076507334961));
#69426=CARTESIAN_POINT('Ctrl Pts',(0.312797468325896,2.02241790824809,11.9076925418296));
#69427=CARTESIAN_POINT('Ctrl Pts',(0.312857088609165,2.0226586833595,11.9077079761529));
#69428=CARTESIAN_POINT('Ctrl Pts',(0.312963522720707,2.02309065195168,11.9077356293546));
#69429=CARTESIAN_POINT('Ctrl Pts',(0.313010439018017,2.02328181808054,11.9077478541171));
#69430=CARTESIAN_POINT('Ctrl Pts',(0.313120459793668,2.02373189199893,11.9077766049823));
#69431=CARTESIAN_POINT('Ctrl Pts',(0.313183418214199,2.02399083478711,11.9077931225183));
#69432=CARTESIAN_POINT('Ctrl Pts',(0.313365403317879,2.02474338934705,11.9078410583693));
#69433=CARTESIAN_POINT('Ctrl Pts',(0.313483585405194,2.02523720756027,11.9078724279517));
#69434=CARTESIAN_POINT('Ctrl Pts',(0.314302998613926,2.02869719136046,11.9080916373238));
#69435=CARTESIAN_POINT('Ctrl Pts',(0.314963317101599,2.03167302164196,11.9082771668378));
#69436=CARTESIAN_POINT('Ctrl Pts',(0.316868720677611,2.0408755088131,11.9088429173463));
#69437=CARTESIAN_POINT('Ctrl Pts',(0.317972154470192,2.04713023912698,11.9092162532531));
#69438=CARTESIAN_POINT('Ctrl Pts',(0.321175562452994,2.06905813338983,11.910498907868));
#69439=CARTESIAN_POINT('Ctrl Pts',(0.322306833356607,2.08485036634992,11.9113771759143));
#69440=CARTESIAN_POINT('Ctrl Pts',(0.32222273102675,2.1257504314663,11.9136642529783));
#69441=CARTESIAN_POINT('Ctrl Pts',(0.319242167848216,2.15074204212297,11.9150806065274));
#69442=CARTESIAN_POINT('Ctrl Pts',(0.313052036700598,2.17656210544553,11.9166914055921));
#69443=CARTESIAN_POINT('Ctrl Pts',(0.312699795496268,2.17798827769494,11.9167808351785));
#69444=CARTESIAN_POINT('Ctrl Pts',(0.312204923070445,2.1799346765526,11.9169035280593));
#69445=CARTESIAN_POINT('Ctrl Pts',(0.312070714450355,2.1804570424628,11.9169365192217));
#69446=CARTESIAN_POINT('Ctrl Pts',(0.311839952112226,2.18134594990796,11.9169927690346));
#69447=CARTESIAN_POINT('Ctrl Pts',(0.311744061507356,2.18171266372291,11.9170160061959));
#69448=CARTESIAN_POINT('Ctrl Pts',(0.311549303120863,2.18245214418087,11.9170629282279));
#69449=CARTESIAN_POINT('Ctrl Pts',(0.311450412739822,2.18282490420944,11.9170866137991));
#69450=CARTESIAN_POINT('Ctrl Pts',(0.311231151082831,2.18364544949951,11.9171388251013));
#69451=CARTESIAN_POINT('Ctrl Pts',(0.311110482187376,2.18409315368016,11.9171673604459));
#69452=CARTESIAN_POINT('Ctrl Pts',(0.310851205469512,2.18504692232507,11.9172282536997));
#69453=CARTESIAN_POINT('Ctrl Pts',(0.310712327242414,2.18555291130754,11.9172606203346));
#69454=CARTESIAN_POINT('Ctrl Pts',(0.310347304674683,2.18687022212318,11.9173450470936));
#69455=CARTESIAN_POINT('Ctrl Pts',(0.31011921547614,2.18768099669506,11.9173971704074));
#69456=CARTESIAN_POINT('Ctrl Pts',(0.309437452251883,2.19006847722662,11.9175511359824));
#69457=CARTESIAN_POINT('Ctrl Pts',(0.308974918309365,2.19164260549263,11.9176532663039));
#69458=CARTESIAN_POINT('Ctrl Pts',(0.30391269167118,2.20839667470287,11.9187469789045));
#69459=CARTESIAN_POINT('Ctrl Pts',(0.298211056544918,2.22321848218613,11.919775051054));
#69460=CARTESIAN_POINT('Ctrl Pts',(0.27787342459795,2.2663073864259,11.9229431098404));
#69461=CARTESIAN_POINT('Ctrl Pts',(0.260126349595312,2.29288862247379,11.9251609732479));
#69462=CARTESIAN_POINT('Ctrl Pts',(0.237734888667022,2.31759067874664,11.9272706180569));
#69463=CARTESIAN_POINT('Ctrl Pts',(0.236685022506325,2.31873221325915,11.9273681869276));
#69464=CARTESIAN_POINT('Ctrl Pts',(0.235335654474263,2.32017830874775,11.9274918353485));
#69465=CARTESIAN_POINT('Ctrl Pts',(0.235043754869597,2.32048988913702,11.927518479916));
#69466=CARTESIAN_POINT('Ctrl Pts',(0.234579006285329,2.32098400083996,11.9275607367477));
#69467=CARTESIAN_POINT('Ctrl Pts',(0.234406562734848,2.32116691019436,11.9275763800102));
#69468=CARTESIAN_POINT('Ctrl Pts',(0.234083967020305,2.3215082835132,11.9276055768478));
#69469=CARTESIAN_POINT('Ctrl Pts',(0.233933868985738,2.3216667954898,11.9276191343596));
#69470=CARTESIAN_POINT('Ctrl Pts',(0.233596202296759,2.32202266557389,11.9276495728457));
#69471=CARTESIAN_POINT('Ctrl Pts',(0.233408544976355,2.32221993810038,11.9276664467746));
#69472=CARTESIAN_POINT('Ctrl Pts',(0.232851108099107,2.32280445187023,11.9277164467658));
#69473=CARTESIAN_POINT('Ctrl Pts',(0.232480610926652,2.32319101207061,11.9277495174197));
#69474=CARTESIAN_POINT('Ctrl Pts',(0.229496020341915,2.32628950549246,11.9280146456769));
#69475=CARTESIAN_POINT('Ctrl Pts',(0.226835392082965,2.32895648398696,11.9282431515341));
#69476=CARTESIAN_POINT('Ctrl Pts',(0.217036305224036,2.33844041663441,11.92905962284));
#69477=CARTESIAN_POINT('Ctrl Pts',(0.209631890823145,2.34497570336214,11.9296298266413));
#69478=CARTESIAN_POINT('Ctrl Pts',(0.191237395366663,2.35976523321532,11.9309712492244));
#69479=CARTESIAN_POINT('Ctrl Pts',(0.179997022229583,2.36767669349779,11.9317328745752));
#69480=CARTESIAN_POINT('Ctrl Pts',(0.148640230057736,2.38687611980003,11.9337927806612));
#69481=CARTESIAN_POINT('Ctrl Pts',(0.127764831403284,2.39676209536793,11.9351037140861));
#69482=CARTESIAN_POINT('Ctrl Pts',(0.104736435116182,2.40478400597705,11.9365842368593));
#69483=CARTESIAN_POINT('Ctrl Pts',(0.103454245097934,2.4052216083831,11.936666754527));
#69484=CARTESIAN_POINT('Ctrl Pts',(0.101675156603859,2.40581630052915,11.9367813799651));
#69485=CARTESIAN_POINT('Ctrl Pts',(0.101180566586012,2.40598029361391,11.9368132597954));
#69486=CARTESIAN_POINT('Ctrl Pts',(0.100330205310402,2.40625996388917,11.9368680960105));
#69487=CARTESIAN_POINT('Ctrl Pts',(0.0999746252684269,2.4063762227712,11.9368910331859));
#69488=CARTESIAN_POINT('Ctrl Pts',(0.0992603919978063,2.40660836953332,
11.9369371207987));
#69489=CARTESIAN_POINT('Ctrl Pts',(0.0989017362848541,2.4067242478928,11.9369602715091));
#69490=CARTESIAN_POINT('Ctrl Pts',(0.0980657832762865,2.4069927179476,11.9370142491381));
#69491=CARTESIAN_POINT('Ctrl Pts',(0.0975883327136098,2.40714482583319,
11.9370450919026));
#69492=CARTESIAN_POINT('Ctrl Pts',(0.0961293001700396,2.4076059041071,11.9371393867013));
#69493=CARTESIAN_POINT('Ctrl Pts',(0.0951465985366241,2.40791128485376,
11.9372029563425));
#69494=CARTESIAN_POINT('Ctrl Pts',(0.0928870560330176,2.40860160228108,
11.9373492659192));
#69495=CARTESIAN_POINT('Ctrl Pts',(0.0916092612740967,2.40898332846891,
11.9374321098634));
#69496=CARTESIAN_POINT('Ctrl Pts',(0.0873955585469937,2.41021368708271,
11.9377056604697));
#69497=CARTESIAN_POINT('Ctrl Pts',(0.0844500168335711,2.41102846964457,
11.9378974603774));
#69498=CARTESIAN_POINT('Ctrl Pts',(0.0724967516520152,2.41415261514852,
11.9386783188074));
#69499=CARTESIAN_POINT('Ctrl Pts',(0.0634033320567419,2.41611332574865,
11.9392782776601));
#69500=CARTESIAN_POINT('Ctrl Pts',(0.0382237152840651,2.42041235076216,
11.9409549749743));
#69501=CARTESIAN_POINT('Ctrl Pts',(0.0220263157463984,2.42193148861396,
11.9420517138141));
#69502=CARTESIAN_POINT('Ctrl Pts',(-0.0142620859097455,2.4225829854974,
11.9445078361993));
#69503=CARTESIAN_POINT('Ctrl Pts',(-0.0343015208324877,2.421071318454,11.9458638563658));
#69504=CARTESIAN_POINT('Ctrl Pts',(-0.055237241858519,2.41750813990561,
11.9472030730987));
#69505=CARTESIAN_POINT('Ctrl Pts',(-0.0564010099644147,2.41730347929402,
11.9472772506192));
#69506=CARTESIAN_POINT('Ctrl Pts',(-0.0579458128205222,2.41702304216756,
11.9473753367658));
#69507=CARTESIAN_POINT('Ctrl Pts',(-0.058327854988515,2.41695297415362,
11.9473995634741));
#69508=CARTESIAN_POINT('Ctrl Pts',(-0.0589224359550742,2.41684281425423,
11.947437219113));
#69509=CARTESIAN_POINT('Ctrl Pts',(-0.0591350610163383,2.41680319910424,
11.9474506752031));
#69510=CARTESIAN_POINT('Ctrl Pts',(-0.0595411298601977,2.41672711950472,
11.9474763546452));
#69511=CARTESIAN_POINT('Ctrl Pts',(-0.0597345787697421,2.41669069211817,
11.9474885799867));
#69512=CARTESIAN_POINT('Ctrl Pts',(-0.0601899289174849,2.41660451536295,
11.9475173374345));
#69513=CARTESIAN_POINT('Ctrl Pts',(-0.0604518015141238,2.41655461833028,
11.9475338609617));
#69514=CARTESIAN_POINT('Ctrl Pts',(-0.0612127313247458,2.41640865259135,
11.9475818311893));
#69515=CARTESIAN_POINT('Ctrl Pts',(-0.0617116264791871,2.41631172769368,
11.9476132290494));
#69516=CARTESIAN_POINT('Ctrl Pts',(-0.0652111528068321,2.41562324830059,
11.9478331101284));
#69517=CARTESIAN_POINT('Ctrl Pts',(-0.0682035880346649,2.41499016103255,
11.9480192669058));
#69518=CARTESIAN_POINT('Ctrl Pts',(-0.0773541649728065,2.41291771711632,
11.9485840471005));
#69519=CARTESIAN_POINT('Ctrl Pts',(-0.0834796232035285,2.41133957013502,
11.9489558759193));
#69520=CARTESIAN_POINT('Ctrl Pts',(-0.104267788750449,2.4053260257712,11.9502085157357));
#69521=CARTESIAN_POINT('Ctrl Pts',(-0.118659356281344,2.40002628499509,
11.9510604433797));
#69522=CARTESIAN_POINT('Ctrl Pts',(-0.139700753455025,2.39052578260807,
11.9523511284678));
#69523=CARTESIAN_POINT('Ctrl Pts',(-0.146663289992089,2.38707386884959,
11.9527860036273));
#69524=CARTESIAN_POINT('Ctrl Pts',(-0.165004478480103,2.3771390577625,11.9539657056869));
#69525=CARTESIAN_POINT('Ctrl Pts',(-0.176123148351679,2.37020940025921,
11.9547181227331));
#69526=CARTESIAN_POINT('Ctrl Pts',(-0.191249313945377,2.35945102414004,
11.9558197711838));
#69527=CARTESIAN_POINT('Ctrl Pts',(-0.195627870514173,2.35616569793313,
11.9561485939121));
#69528=CARTESIAN_POINT('Ctrl Pts',(-0.20061255038541,2.35222323222255,11.9565355474609));
#69529=CARTESIAN_POINT('Ctrl Pts',(-0.201302384122906,2.35167301080386,
11.9565893856552));
#69530=CARTESIAN_POINT('Ctrl Pts',(-0.202396779152602,2.35079272719641,
11.9566752607316));
#69531=CARTESIAN_POINT('Ctrl Pts',(-0.202802816422597,2.35046450022299,
11.9567072238346));
#69532=CARTESIAN_POINT('Ctrl Pts',(-0.203516472054414,2.34988473168529,
11.9567635836033));
#69533=CARTESIAN_POINT('Ctrl Pts',(-0.203824426925171,2.3496336045353,11.9567879634999));
#69534=CARTESIAN_POINT('Ctrl Pts',(-0.20441530110516,2.34914994363757,11.9568348565242));
#69535=CARTESIAN_POINT('Ctrl Pts',(-0.204698290214955,2.34891749581303,
11.9568573661455));
#69536=CARTESIAN_POINT('Ctrl Pts',(-0.205439747869139,2.3483063415082,11.9569164778506));
#69537=CARTESIAN_POINT('Ctrl Pts',(-0.20589756396956,2.34792684885174,11.9569531118843));
#69538=CARTESIAN_POINT('Ctrl Pts',(-0.207552874278974,2.34654698283765,
11.9570860618835));
#69539=CARTESIAN_POINT('Ctrl Pts',(-0.208744134628662,2.345539195422,11.9571826806891));
#69540=CARTESIAN_POINT('Ctrl Pts',(-0.211624607772102,2.34306624821065,
11.9574186303411));
#69541=CARTESIAN_POINT('Ctrl Pts',(-0.213305961844113,2.34159209811111,
11.9575583309558));
#69542=CARTESIAN_POINT('Ctrl Pts',(-0.21954818525648,2.33600318229971,11.9580845359022));
#69543=CARTESIAN_POINT('Ctrl Pts',(-0.224006212412139,2.33177600454659,
11.9584757180441));
#69544=CARTESIAN_POINT('Ctrl Pts',(-0.232800997142482,2.32294578708031,
11.9592797713753));
#69545=CARTESIAN_POINT('Ctrl Pts',(-0.237128531158594,2.31833730790587,
11.9596927696632));
#69546=CARTESIAN_POINT('Ctrl Pts',(-0.264136268315157,2.28782562682128,
11.9623833732619));
#69547=CARTESIAN_POINT('Ctrl Pts',(-0.282674580828835,2.25855998744229,
11.9647980413033));
#69548=CARTESIAN_POINT('Ctrl Pts',(-0.296742751309248,2.22572430624604,
11.9670532449211));
#69549=CARTESIAN_POINT('Ctrl Pts',(-0.297246903106023,2.22452766907421,
11.9671348168656));
#69550=CARTESIAN_POINT('Ctrl Pts',(-0.297898156102656,2.22295538569893,
11.9672411607182));
#69551=CARTESIAN_POINT('Ctrl Pts',(-0.298051794890168,2.2225824858971,11.9672663210735));
#69552=CARTESIAN_POINT('Ctrl Pts',(-0.298287890024066,2.22200638662459,
11.9673050960571));
#69553=CARTESIAN_POINT('Ctrl Pts',(-0.298370838962983,2.22180339145282,
11.9673187405576));
#69554=CARTESIAN_POINT('Ctrl Pts',(-0.298535926514821,2.22139820358291,
11.9673459388737));
#69555=CARTESIAN_POINT('Ctrl Pts',(-0.298618066365931,2.22119601352165,
11.9673594926504));
#69556=CARTESIAN_POINT('Ctrl Pts',(-0.2988018940132,2.22074219401556,11.9673898735181));
#69557=CARTESIAN_POINT('Ctrl Pts',(-0.298903469124256,2.22049052007669,
11.9674066936813));
#69558=CARTESIAN_POINT('Ctrl Pts',(-0.299202920669377,2.21974585621456,
11.9674563796927));
#69559=CARTESIAN_POINT('Ctrl Pts',(-0.299399897464345,2.21925250196752,
11.9674891911753));
#69560=CARTESIAN_POINT('Ctrl Pts',(-0.300938493977236,2.21537104325906,
11.9677465161175));
#69561=CARTESIAN_POINT('Ctrl Pts',(-0.302223848577097,2.21196072020821,
11.9679677083848));
#69562=CARTESIAN_POINT('Ctrl Pts',(-0.306585057431664,2.19976663452508,
11.968743790018));
#69563=CARTESIAN_POINT('Ctrl Pts',(-0.309338236253323,2.19087169219695,
11.9692829243192));
#69564=CARTESIAN_POINT('Ctrl Pts',(-0.318707330195921,2.15520055744231,
11.9713842265054));
#69565=CARTESIAN_POINT('Ctrl Pts',(-0.322260151683405,2.12774507942207,
11.9728789771032));
#69566=CARTESIAN_POINT('Ctrl Pts',(-0.322274953560087,2.10017301110915,
11.9744805487749));
#69567=CARTESIAN_POINT('',(-0.322759928630395,2.09993784294859,12.2247412594466));
#69568=CARTESIAN_POINT('Ctrl Pts',(-0.322274953770146,2.10017261938011,
11.9744805715291));
#69569=CARTESIAN_POINT('Ctrl Pts',(-0.322280140850064,2.09048850430689,
11.9750430905345));
#69570=CARTESIAN_POINT('Ctrl Pts',(-0.321848831765366,2.08080970305467,
11.9756163851485));
#69571=CARTESIAN_POINT('Ctrl Pts',(-0.320889619698775,2.07013188223727,
11.9762666160024));
#69572=CARTESIAN_POINT('Ctrl Pts',(-0.320791782188379,2.06909878755829,
11.9763297091459));
#69573=CARTESIAN_POINT('Ctrl Pts',(-0.320628924429427,2.06746332065255,
11.9764298860425));
#69574=CARTESIAN_POINT('Ctrl Pts',(-0.320567191588716,2.06686062232353,
11.9764668666521));
#69575=CARTESIAN_POINT('Ctrl Pts',(-0.320459192676731,2.06583477427253,
11.9765299208147));
#69576=CARTESIAN_POINT('Ctrl Pts',(-0.320413786902972,2.06541153400647,
11.97655596728));
#69577=CARTESIAN_POINT('Ctrl Pts',(-0.320327716372621,2.06462396092436,
11.9766044947544));
#69578=CARTESIAN_POINT('Ctrl Pts',(-0.320287268185173,2.06425960473219,
11.9766269689109));
#69579=CARTESIAN_POINT('Ctrl Pts',(-0.320202109701468,2.06350425444715,
11.9766736100176));
#69580=CARTESIAN_POINT('Ctrl Pts',(-0.320157304747916,2.06311327182989,
11.9766977799149));
#69581=CARTESIAN_POINT('Ctrl Pts',(-0.320053374576734,2.06222079889792,
11.976753014664));
#69582=CARTESIAN_POINT('Ctrl Pts',(-0.319993786735539,2.06171936442678,
11.9767840940578));
#69583=CARTESIAN_POINT('Ctrl Pts',(-0.319807920601414,2.06018605444385,
11.9768792715208));
#69584=CARTESIAN_POINT('Ctrl Pts',(-0.319677828682961,2.05915465573492,
11.9769434897918));
#69585=CARTESIAN_POINT('Ctrl Pts',(-0.318679712191136,2.05153835440923,
11.9774191779939));
#69586=CARTESIAN_POINT('Ctrl Pts',(-0.317613353017002,2.04498148074331,
11.9778368872331));
#69587=CARTESIAN_POINT('Ctrl Pts',(-0.315932899967771,2.03634277701505,
11.9783987082447));
#69588=CARTESIAN_POINT('Ctrl Pts',(-0.315499250006797,2.03422719243243,
11.9785372131014));
#69589=CARTESIAN_POINT('Ctrl Pts',(-0.314578913072934,2.02995596973158,
11.9788187064767));
#69590=CARTESIAN_POINT('Ctrl Pts',(-0.314091250581152,2.02780066014975,
11.978961716818));
#69591=CARTESIAN_POINT('Ctrl Pts',(-0.307367604592412,1.99944252826692,
11.9808560295979));
#69592=CARTESIAN_POINT('Ctrl Pts',(-0.29789291162276,1.97411874585603,11.9827037981042));
#69593=CARTESIAN_POINT('Ctrl Pts',(-0.281047570084969,1.94201107663383,
11.9851321291597));
#69594=CARTESIAN_POINT('Ctrl Pts',(-0.276355449123813,1.93393997442173,
11.9857492851136));
#69595=CARTESIAN_POINT('Ctrl Pts',(-0.269349813934889,1.92301081340079,
11.9865836565265));
#69596=CARTESIAN_POINT('Ctrl Pts',(-0.267328199079778,1.91997185991686,
11.9868154957117));
#69597=CARTESIAN_POINT('Ctrl Pts',(-0.264953485993235,1.91653036141997,
11.9870772574279));
#69598=CARTESIAN_POINT('Ctrl Pts',(-0.264650594565342,1.916093717273,11.9871104539786));
#69599=CARTESIAN_POINT('Ctrl Pts',(-0.264191359206747,1.91543517392646,
11.9871604959271));
#69600=CARTESIAN_POINT('Ctrl Pts',(-0.264035814569343,1.91521272249132,
11.9871773954587));
#69601=CARTESIAN_POINT('Ctrl Pts',(-0.263754702030048,1.91481177032229,
11.9872078474552));
#69602=CARTESIAN_POINT('Ctrl Pts',(-0.263629234181853,1.9146332010857,11.987221406697));
#69603=CARTESIAN_POINT('Ctrl Pts',(-0.263377344520193,1.91427547793548,
11.9872485636152));
#69604=CARTESIAN_POINT('Ctrl Pts',(-0.263250921824196,1.91409632638916,
11.9872621611223));
#69605=CARTESIAN_POINT('Ctrl Pts',(-0.262891507522944,1.91358810803321,
11.9873007266314));
#69606=CARTESIAN_POINT('Ctrl Pts',(-0.262658080023907,1.91325934776626,
11.9873256646614));
#69607=CARTESIAN_POINT('Ctrl Pts',(-0.261670835978958,1.9118744224225,11.9874306815702));
#69608=CARTESIAN_POINT('Ctrl Pts',(-0.260911247895749,1.91082235809651,
11.9875103689434));
#69609=CARTESIAN_POINT('Ctrl Pts',(-0.239813944938682,1.88197041301535,
11.9896941254943));
#69610=CARTESIAN_POINT('Ctrl Pts',(-0.215152759056864,1.85759965938156,
11.9915162503771));
#69611=CARTESIAN_POINT('Ctrl Pts',(-0.178630626541909,1.83155943299207,
11.9940749490111));
#69612=CARTESIAN_POINT('Ctrl Pts',(-0.169880079880557,1.82593802132801,
11.9946775529013));
#69613=CARTESIAN_POINT('Ctrl Pts',(-0.157875553349675,1.81902231789463,
11.9955010447022));
#69614=CARTESIAN_POINT('Ctrl Pts',(-0.154849820146373,1.81734353003614,
11.9957083186952));
#69615=CARTESIAN_POINT('Ctrl Pts',(-0.150507733696608,1.81502502520281,
11.9960056453086));
#69616=CARTESIAN_POINT('Ctrl Pts',(-0.149213083247758,1.81434501607311,
11.9960942813772));
#69617=CARTESIAN_POINT('Ctrl Pts',(-0.146928124361533,1.81316462405401,
11.9962507116368));
#69618=CARTESIAN_POINT('Ctrl Pts',(-0.145939769705516,1.81266049663759,
11.9963183733908));
#69619=CARTESIAN_POINT('Ctrl Pts',(-0.144487299898654,1.8119290663169,11.9964178124959));
#69620=CARTESIAN_POINT('Ctrl Pts',(-0.144025202468255,1.81169775631445,
11.9964494493051));
#69621=CARTESIAN_POINT('Ctrl Pts',(-0.143228510114815,1.81130135309551,
11.9965039955819));
#69622=CARTESIAN_POINT('Ctrl Pts',(-0.142894180152883,1.81113572718191,
11.9965268863734));
#69623=CARTESIAN_POINT('Ctrl Pts',(-0.142229191429349,1.81080773103358,
11.9965724180849));
#69624=CARTESIAN_POINT('Ctrl Pts',(-0.141898540346243,1.8106453463819,11.9965950584603));
#69625=CARTESIAN_POINT('Ctrl Pts',(-0.14111925679983,1.81026429272008,11.9966484197235));
#69626=CARTESIAN_POINT('Ctrl Pts',(-0.140670394317473,1.81004609871425,
11.9966791570994));
#69627=CARTESIAN_POINT('Ctrl Pts',(-0.139343993182991,1.80940513425141,
11.9967699927608));
#69628=CARTESIAN_POINT('Ctrl Pts',(-0.138465048435954,1.80898530146423,
11.9968301929278));
#69629=CARTESIAN_POINT('Ctrl Pts',(-0.130677267381999,1.80530869362934,
11.9973636780659));
#69630=CARTESIAN_POINT('Ctrl Pts',(-0.123657102274845,1.80229474429172,
11.9978452864166));
#69631=CARTESIAN_POINT('Ctrl Pts',(-0.0973871452182989,1.792105861998,11.9996522730904));
#69632=CARTESIAN_POINT('Ctrl Pts',(-0.077573843073094,1.78652731697814,
12.0010283370725));
#69633=CARTESIAN_POINT('Ctrl Pts',(-0.0552039993273162,1.78248066367391,
12.0025663110488));
#69634=CARTESIAN_POINT('Ctrl Pts',(-0.0530363378706432,1.78211140734768,
12.0027151318981));
#69635=CARTESIAN_POINT('Ctrl Pts',(-0.0483532023407551,1.78136288020533,
12.003036050105));
#69636=CARTESIAN_POINT('Ctrl Pts',(-0.0458366618553275,1.78099114933279,
12.0032081263859));
#69637=CARTESIAN_POINT('Ctrl Pts',(-0.0258175782646707,1.77827580842671,
12.0045730993834));
#69638=CARTESIAN_POINT('Ctrl Pts',(-0.00815113662796364,1.77734424781082,
12.0057557076176));
#69639=CARTESIAN_POINT('Ctrl Pts',(0.0102113679736316,1.77788603971825,
12.0069082379681));
#69640=CARTESIAN_POINT('Ctrl Pts',(0.0109179768508587,1.77790921582853,
12.0069524680628));
#69641=CARTESIAN_POINT('Ctrl Pts',(0.0119293765709213,1.77794572093613,
12.0070155984508));
#69642=CARTESIAN_POINT('Ctrl Pts',(0.012234227252519,1.77795715754873,12.007034603713));
#69643=CARTESIAN_POINT('Ctrl Pts',(0.0127616123662588,1.77797769257668,
12.0070674417965));
#69644=CARTESIAN_POINT('Ctrl Pts',(0.0129841540810078,1.77798658883144,
12.0070812860292));
#69645=CARTESIAN_POINT('Ctrl Pts',(0.013413196383939,1.77800418557804,12.0071079522445));
#69646=CARTESIAN_POINT('Ctrl Pts',(0.0136196973612327,1.77801285400363,
12.0071207760293));
#69647=CARTESIAN_POINT('Ctrl Pts',(0.0141103867407583,1.77803392488116,
12.0071512225435));
#69648=CARTESIAN_POINT('Ctrl Pts',(0.0143945679148747,1.7780465049772,12.0071688352387));
#69649=CARTESIAN_POINT('Ctrl Pts',(0.0152468967022026,1.77808536652297,
12.0072216001003));
#69650=CARTESIAN_POINT('Ctrl Pts',(0.0158149956011329,1.77811277591143,
12.0072566893676));
#69651=CARTESIAN_POINT('Ctrl Pts',(0.0213507606199708,1.77839455385049,
12.0075978595259));
#69652=CARTESIAN_POINT('Ctrl Pts',(0.0263123131510297,1.77876241380163,
12.0078977348205));
#69653=CARTESIAN_POINT('Ctrl Pts',(0.0316003009612357,1.77927782896817,
12.0082129091073));
#69654=CARTESIAN_POINT('Ctrl Pts',(0.0319368670015658,1.77931116866954,
12.0082329498713));
#69655=CARTESIAN_POINT('Ctrl Pts',(0.0326193524279296,1.77937985967693,
12.0082735504688));
#69656=CARTESIAN_POINT('Ctrl Pts',(0.0329652683854436,1.77941524113622,
12.0082941090338));
#69657=CARTESIAN_POINT('Ctrl Pts',(0.0337575093247992,1.7794975700599,12.0083411498375));
#69658=CARTESIAN_POINT('Ctrl Pts',(0.0342037957024968,1.77954489020023,
12.008367617034));
#69659=CARTESIAN_POINT('Ctrl Pts',(0.0360959270022173,1.77974951228507,
12.0084797007805));
#69660=CARTESIAN_POINT('Ctrl Pts',(0.0375408164208962,1.7799156704009,12.0085649696864));
#69661=CARTESIAN_POINT('Ctrl Pts',(0.0696308772562227,1.7838262169437,12.0104525461949));
#69662=CARTESIAN_POINT('Ctrl Pts',(0.0995833500407337,1.79194504281586,
12.0121040237752));
#69663=CARTESIAN_POINT('Ctrl Pts',(0.135602593779702,1.80752252732983,12.014366563192));
#69664=CARTESIAN_POINT('Ctrl Pts',(0.143146923892467,1.81114003921337,12.0148561730258));
#69665=CARTESIAN_POINT('Ctrl Pts',(0.153026876241346,1.81635964457534,12.0155236012933));
#69666=CARTESIAN_POINT('Ctrl Pts',(0.155494798840177,1.81770504279601,12.0156925699906));
#69667=CARTESIAN_POINT('Ctrl Pts',(0.159037209010758,1.81969674900383,12.0159385279017));
#69668=CARTESIAN_POINT('Ctrl Pts',(0.160126062786958,1.82031733997859,12.0160146035594));
#69669=CARTESIAN_POINT('Ctrl Pts',(0.162059132023687,1.82143407931396,12.0161505233134));
#69670=CARTESIAN_POINT('Ctrl Pts',(0.162904762613146,1.82192775628501,12.0162102780267));
#69671=CARTESIAN_POINT('Ctrl Pts',(0.164170518899697,1.82267445689397,12.0163001703966));
#69672=CARTESIAN_POINT('Ctrl Pts',(0.164592343648889,1.82292460133961,12.0163302033129));
#69673=CARTESIAN_POINT('Ctrl Pts',(0.165340284638635,1.82337044526916,12.0163835898017));
#69674=CARTESIAN_POINT('Ctrl Pts',(0.165666629225812,1.82356576146592,12.0164069293558));
#69675=CARTESIAN_POINT('Ctrl Pts',(0.166317488049061,1.82395686489884,12.016453569345));
#69676=CARTESIAN_POINT('Ctrl Pts',(0.166642004204567,1.82415264782818,12.0164768695978));
#69677=CARTESIAN_POINT('Ctrl Pts',(0.167521828158983,1.82468557112558,12.0165401655595));
#69678=CARTESIAN_POINT('Ctrl Pts',(0.168076460918846,1.82502381751995,12.0165802017942));
#69679=CARTESIAN_POINT('Ctrl Pts',(0.170148333428435,1.82629597287729,12.0167302695134));
#69680=CARTESIAN_POINT('Ctrl Pts',(0.171658821171498,1.82724076781729,12.0168407013711));
#69681=CARTESIAN_POINT('Ctrl Pts',(0.175211939345334,1.82950441148556,12.0171029417462));
#69682=CARTESIAN_POINT('Ctrl Pts',(0.177247609027421,1.83083393291993,12.017255143187));
#69683=CARTESIAN_POINT('Ctrl Pts',(0.20798603168023,1.85140949010392,12.0195837696654));
#69684=CARTESIAN_POINT('Ctrl Pts',(0.233420781080795,1.87512447848566,12.0219535093765));
#69685=CARTESIAN_POINT('Ctrl Pts',(0.261660880641864,1.91151269188097,12.0250376035386));
#69686=CARTESIAN_POINT('Ctrl Pts',(0.268231536649158,1.92098663329777,12.0257969754443));
#69687=CARTESIAN_POINT('Ctrl Pts',(0.275107559463095,1.93213254313696,12.0266255969777));
#69688=CARTESIAN_POINT('Ctrl Pts',(0.275924042788517,1.93347800386039,12.0267245912393));
#69689=CARTESIAN_POINT('Ctrl Pts',(0.276943137679035,1.93518541933912,12.0268488659962));
#69690=CARTESIAN_POINT('Ctrl Pts',(0.277154932863702,1.93554182689864,12.0268747333587));
#69691=CARTESIAN_POINT('Ctrl Pts',(0.277491370211385,1.93611047726076,12.0269158860523));
#69692=CARTESIAN_POINT('Ctrl Pts',(0.277616457102722,1.93632245434332,12.0269312003843));
#69693=CARTESIAN_POINT('Ctrl Pts',(0.277852410815398,1.93672335925277,12.0269601139595));
#69694=CARTESIAN_POINT('Ctrl Pts',(0.277963326941763,1.93691225525686,12.0269737163535));
#69695=CARTESIAN_POINT('Ctrl Pts',(0.27821571869168,1.93734309713439,12.0270046937703));
#69696=CARTESIAN_POINT('Ctrl Pts',(0.278357071102478,1.9375851141501,12.0270220606746));
#69697=CARTESIAN_POINT('Ctrl Pts',(0.278777785747945,1.93830760470921,12.0270738053249));
#69698=CARTESIAN_POINT('Ctrl Pts',(0.27905622279983,1.9387886199768,12.0271081230882));
#69699=CARTESIAN_POINT('Ctrl Pts',(0.28100055262145,1.94216768735413,12.0273482902683));
#69700=CARTESIAN_POINT('Ctrl Pts',(0.282622589395207,1.94509091834847,12.0275513708062));
#69701=CARTESIAN_POINT('Ctrl Pts',(0.29119679547267,1.96112648055801,12.0286430231439));
#69702=CARTESIAN_POINT('Ctrl Pts',(0.297283141535621,1.9746833410916,12.0294860460318));
#69703=CARTESIAN_POINT('Ctrl Pts',(0.312862952454075,2.01698221442692,12.0320172654897));
#69704=CARTESIAN_POINT('Ctrl Pts',(0.31926737670666,2.04667686674732,12.0336783332231));
#69705=CARTESIAN_POINT('Ctrl Pts',(0.321580447391477,2.07876421940431,12.035613415307));
#69706=CARTESIAN_POINT('Ctrl Pts',(0.321702502145319,2.08070123360885,12.0357306860977));
#69707=CARTESIAN_POINT('Ctrl Pts',(0.321858381398105,2.08359067671234,12.035906344017));
#69708=CARTESIAN_POINT('Ctrl Pts',(0.321905491017937,2.08454236793351,12.0359643172929));
#69709=CARTESIAN_POINT('Ctrl Pts',(0.321974074254386,2.08606454058975,12.0360572344727));
#69710=CARTESIAN_POINT('Ctrl Pts',(0.321998254030737,2.08663489934523,12.0360920937599));
#69711=CARTESIAN_POINT('Ctrl Pts',(0.322041394546881,2.08772067443161,12.03615853778));
#69712=CARTESIAN_POINT('Ctrl Pts',(0.322060633704833,2.08823607842296,12.0361901137055));
#69713=CARTESIAN_POINT('Ctrl Pts',(0.322092232953702,2.08914086258905,12.0362456083718));
#69714=CARTESIAN_POINT('Ctrl Pts',(0.322105124432119,2.08953022412738,12.0362695104124));
#69715=CARTESIAN_POINT('Ctrl Pts',(0.322128919842068,2.09029060253867,12.0363162290804));
#69716=CARTESIAN_POINT('Ctrl Pts',(0.322139888863817,2.09066161691207,12.0363390436313));
#69717=CARTESIAN_POINT('Ctrl Pts',(0.322164407076842,2.09154242853018,12.0363932521324));
#69718=CARTESIAN_POINT('Ctrl Pts',(0.322177387164284,2.09205223946233,12.0364246638698));
#69719=CARTESIAN_POINT('Ctrl Pts',(0.3222188912953,2.09385007744737,12.0365355651537));
#69720=CARTESIAN_POINT('Ctrl Pts',(0.322240901448385,2.09513822960247,12.0366152584823));
#69721=CARTESIAN_POINT('Ctrl Pts',(0.322461903787939,2.11506783318796,12.037851915141));
#69722=CARTESIAN_POINT('Ctrl Pts',(0.321050746486486,2.13368853336305,12.0390604100042));
#69723=CARTESIAN_POINT('Ctrl Pts',(0.314989707775189,2.17070158703793,12.0415625759917));
#69724=CARTESIAN_POINT('Ctrl Pts',(0.310311048848054,2.18901817897884,12.0428521251548));
#69725=CARTESIAN_POINT('Ctrl Pts',(0.300207171021233,2.21777836571666,12.0448937540188));
#69726=CARTESIAN_POINT('Ctrl Pts',(0.295767140814976,2.22852217518522,12.045659689364));
#69727=CARTESIAN_POINT('Ctrl Pts',(0.2900743104949,2.24042994220696,12.046494839577));
#69728=CARTESIAN_POINT('Ctrl Pts',(0.289382016876861,2.24185105860879,12.0465942748824));
#69729=CARTESIAN_POINT('Ctrl Pts',(0.288494693224047,2.24363899196686,12.0467190249983));
#69730=CARTESIAN_POINT('Ctrl Pts',(0.288309388200623,2.24401057152752,12.0467449320832));
#69731=CARTESIAN_POINT('Ctrl Pts',(0.288013032149422,2.24460196951414,12.0467861332633));
#69732=CARTESIAN_POINT('Ctrl Pts',(0.287902447185933,2.24482201897709,12.0468014564773));
#69733=CARTESIAN_POINT('Ctrl Pts',(0.287693034878547,2.24523753399328,12.0468303773267));
#69734=CARTESIAN_POINT('Ctrl Pts',(0.287594261319001,2.24543302394837,12.0468439781344));
#69735=CARTESIAN_POINT('Ctrl Pts',(0.287368747479664,2.24587822666639,12.0468749392419));
#69736=CARTESIAN_POINT('Ctrl Pts',(0.287241881193742,2.246127874593,12.0468922914552));
#69737=CARTESIAN_POINT('Ctrl Pts',(0.28685413169894,2.24688843331047,12.0469451281181));
#69738=CARTESIAN_POINT('Ctrl Pts',(0.286592207792514,2.24739881667687,12.0469805472902));
#69739=CARTESIAN_POINT('Ctrl Pts',(0.284695363949266,2.25107082497772,12.0472351226996));
#69740=CARTESIAN_POINT('Ctrl Pts',(0.283009448610425,2.25420602763454,12.0474511357969));
#69741=CARTESIAN_POINT('Ctrl Pts',(0.266270952339075,2.28413409169868,12.0495063196684));
#69742=CARTESIAN_POINT('Ctrl Pts',(0.247508855106342,2.30867571226429,12.051150797027));
#69743=CARTESIAN_POINT('Ctrl Pts',(0.214136164988961,2.34137584980251,12.0538068447533));
#69744=CARTESIAN_POINT('Ctrl Pts',(0.201906157376013,2.35169504278487,12.0547368060863));
#69745=CARTESIAN_POINT('Ctrl Pts',(0.188165657816019,2.3616406473426,12.055766159724));
#69746=CARTESIAN_POINT('Ctrl Pts',(0.187366235968143,2.36221372334213,12.0558259891433));
#69747=CARTESIAN_POINT('Ctrl Pts',(0.186088343661225,2.36312096945232,12.0559215407801));
#69748=CARTESIAN_POINT('Ctrl Pts',(0.185611563021663,2.36345751816512,12.0559571718738));
#69749=CARTESIAN_POINT('Ctrl Pts',(0.184703802113902,2.36409459890853,12.0560249762929));
#69750=CARTESIAN_POINT('Ctrl Pts',(0.184272995454772,2.36439537595985,12.056057140131));
#69751=CARTESIAN_POINT('Ctrl Pts',(0.183520233683676,2.36491819947496,12.0561133159111));
#69752=CARTESIAN_POINT('Ctrl Pts',(0.183198605448993,2.36514071649547,12.0561373098611));
#69753=CARTESIAN_POINT('Ctrl Pts',(0.182572876711769,2.36557194194939,12.0561839751006));
#69754=CARTESIAN_POINT('Ctrl Pts',(0.182268821258163,2.36578071498321,12.056206643887));
#69755=CARTESIAN_POINT('Ctrl Pts',(0.181551005495881,2.36627177641139,12.0562601446258));
#69756=CARTESIAN_POINT('Ctrl Pts',(0.181136945047295,2.3665536224557,12.0562909932793));
#69757=CARTESIAN_POINT('Ctrl Pts',(0.179699336113754,2.3675272892533,12.0563980575599));
#69758=CARTESIAN_POINT('Ctrl Pts',(0.178672477586694,2.36821418228663,12.0564744588725));
#69759=CARTESIAN_POINT('Ctrl Pts',(0.165716940455456,2.37677307132526,12.0574375411727));
#69760=CARTESIAN_POINT('Ctrl Pts',(0.153283084964506,2.38384790192533,12.0583539529111));
#69761=CARTESIAN_POINT('Ctrl Pts',(0.119355572243307,2.40027193455651,12.0608360518322));
#69762=CARTESIAN_POINT('Ctrl Pts',(0.0972412806432422,2.40814435526604,
12.0624400964415));
#69763=CARTESIAN_POINT('Ctrl Pts',(0.0654671569879768,2.41569116109062,
12.0646267782147));
#69764=CARTESIAN_POINT('Ctrl Pts',(0.0563724442155307,2.4174413876791,12.0652388487674));
#69765=CARTESIAN_POINT('Ctrl Pts',(0.0436204481428185,2.41932997214429,
12.0660673022455));
#69766=CARTESIAN_POINT('Ctrl Pts',(0.0400176724595867,2.41980144350143,
12.0662980795035));
#69767=CARTESIAN_POINT('Ctrl Pts',(0.0358800790211579,2.42027188033794,
12.0665587726477));
#69768=CARTESIAN_POINT('Ctrl Pts',(0.0353524950995632,2.42033054569548,
12.0665919328572));
#69769=CARTESIAN_POINT('Ctrl Pts',(0.0345550358528794,2.42041722602747,
12.0666419310906));
#69770=CARTESIAN_POINT('Ctrl Pts',(0.0342852694208972,2.42044620381582,
12.0666588231068));
#69771=CARTESIAN_POINT('Ctrl Pts',(0.0337984519812384,2.42049787502278,
12.0666892670523));
#69772=CARTESIAN_POINT('Ctrl Pts',(0.033581415087397,2.4205206885867,12.0667028257419));
#69773=CARTESIAN_POINT('Ctrl Pts',(0.0331461992642003,2.42056598884791,
12.0667299861991));
#69774=CARTESIAN_POINT('Ctrl Pts',(0.0329280215237486,2.42058847317226,
12.0667435877887));
#69775=CARTESIAN_POINT('Ctrl Pts',(0.0323083764105983,2.4206516915179,12.0667821776799));
#69776=CARTESIAN_POINT('Ctrl Pts',(0.0319068534368921,2.42069189445253,
12.066807135948));
#69777=CARTESIAN_POINT('Ctrl Pts',(0.0302112169251173,2.42085845584139,
12.0669123383206));
#69778=CARTESIAN_POINT('Ctrl Pts',(0.0289163972440879,2.42097773819712,
12.0669921892031));
#69779=CARTESIAN_POINT('Ctrl Pts',(-0.00662168824983516,2.4240348099655,
12.0691714140337));
#69780=CARTESIAN_POINT('Ctrl Pts',(-0.0411216162206596,2.42148470754561,
12.070990059537));
#69781=CARTESIAN_POINT('Ctrl Pts',(-0.0894095475321529,2.40999954039297,
12.0738207928766));
#69782=CARTESIAN_POINT('Ctrl Pts',(-0.103975881710794,2.40542216959212,
12.0747115561074));
#69783=CARTESIAN_POINT('Ctrl Pts',(-0.119291937520403,2.39938617814062,
12.0757121926381));
#69784=CARTESIAN_POINT('Ctrl Pts',(-0.120419084779609,2.39893459815941,
12.0757862095546));
#69785=CARTESIAN_POINT('Ctrl Pts',(-0.122042016027532,2.39827371911218,
12.0758933388007));
#69786=CARTESIAN_POINT('Ctrl Pts',(-0.122539879380128,2.39806952736741,
12.0759262783804));
#69787=CARTESIAN_POINT('Ctrl Pts',(-0.123405548589118,2.39771194972716,
12.0759836855929));
#69788=CARTESIAN_POINT('Ctrl Pts',(-0.123773586728971,2.39755912632428,
12.0760081341147));
#69789=CARTESIAN_POINT('Ctrl Pts',(-0.124482517695573,2.39726320844895,
12.0760553091768));
#69790=CARTESIAN_POINT('Ctrl Pts',(-0.124823449804632,2.3971202091516,12.0760780324544));
#69791=CARTESIAN_POINT('Ctrl Pts',(-0.125628853456805,2.39678076273561,
12.0761317992387));
#69792=CARTESIAN_POINT('Ctrl Pts',(-0.126093110420215,2.39658381184877,
12.0761628598533));
#69793=CARTESIAN_POINT('Ctrl Pts',(-0.12771178165399,2.39589263827053,12.0762713940251));
#69794=CARTESIAN_POINT('Ctrl Pts',(-0.128863756720793,2.39539276343199,
12.0763490601389));
#69795=CARTESIAN_POINT('Ctrl Pts',(-0.144299741416769,2.38858717106899,
12.0773955424419));
#69796=CARTESIAN_POINT('Ctrl Pts',(-0.158107807155391,2.38125924039731,
12.0784000258124));
#69797=CARTESIAN_POINT('Ctrl Pts',(-0.181182739410418,2.3667758256734,12.0802018192575));
#69798=CARTESIAN_POINT('Ctrl Pts',(-0.190693839377793,2.36006221610297,
12.0809850223607));
#69799=CARTESIAN_POINT('Ctrl Pts',(-0.208077246289068,2.34632454700014,
12.0824835445723));
#69800=CARTESIAN_POINT('Ctrl Pts',(-0.216009448452653,2.33939893363112,
12.0831972585498));
#69801=CARTESIAN_POINT('Ctrl Pts',(-0.229953559816156,2.32596602119399,
12.0844932478045));
#69802=CARTESIAN_POINT('Ctrl Pts',(-0.236064040377432,2.31957476306567,
12.0850776681776));
#69803=CARTESIAN_POINT('Ctrl Pts',(-0.242437560932519,2.31233430151985,
12.0856987385142));
#69804=CARTESIAN_POINT('Ctrl Pts',(-0.242968376089979,2.31172669836537,
12.0857505550383));
#69805=CARTESIAN_POINT('Ctrl Pts',(-0.245563076176704,2.3087340395674,12.0860042633628));
#69806=CARTESIAN_POINT('Ctrl Pts',(-0.247594244513767,2.30632066202191,
12.0862041894235));
#69807=CARTESIAN_POINT('Ctrl Pts',(-0.249913860846921,2.3034809580087,12.0864336765439));
#69808=CARTESIAN_POINT('Ctrl Pts',(-0.250237032541212,2.30308339584795,
12.0864656759506));
#69809=CARTESIAN_POINT('Ctrl Pts',(-0.250727463214252,2.30247712548755,
12.0865142757597));
#69810=CARTESIAN_POINT('Ctrl Pts',(-0.250895410818259,2.30226897930018,
12.0865309257231));
#69811=CARTESIAN_POINT('Ctrl Pts',(-0.251199785104768,2.30189079006862,
12.0865611130724));
#69812=CARTESIAN_POINT('Ctrl Pts',(-0.251336297862839,2.3017208182827,12.0865746566823));
#69813=CARTESIAN_POINT('Ctrl Pts',(-0.25161122213855,2.3013777982335,12.0866019413403));
#69814=CARTESIAN_POINT('Ctrl Pts',(-0.251749627030635,2.30120474650983,
12.0866156819177));
#69815=CARTESIAN_POINT('Ctrl Pts',(-0.252146557103133,2.30070740236997,
12.0866551023111));
#69816=CARTESIAN_POINT('Ctrl Pts',(-0.252404636135577,2.30038275196958,
12.0866807499687));
#69817=CARTESIAN_POINT('Ctrl Pts',(-0.253527704001543,2.29896437710852,
12.0867924382633));
#69818=CARTESIAN_POINT('Ctrl Pts',(-0.254386232537767,2.29786552230014,
12.0868780231181));
#69819=CARTESIAN_POINT('Ctrl Pts',(-0.271161502514037,2.27610471774014,
12.0885551521896));
#69820=CARTESIAN_POINT('Ctrl Pts',(-0.284521898853985,2.25358779823015,
12.0899825739465));
#69821=CARTESIAN_POINT('Ctrl Pts',(-0.304478988187319,2.2081933879082,12.0927603130377));
#69822=CARTESIAN_POINT('Ctrl Pts',(-0.311553286843005,2.18571795050003,
12.0940973395832));
#69823=CARTESIAN_POINT('Ctrl Pts',(-0.316345671568156,2.16154605335343,
12.0955958390002));
#69824=CARTESIAN_POINT('Ctrl Pts',(-0.316563476686372,2.16041577424569,
12.0956660262563));
#69825=CARTESIAN_POINT('Ctrl Pts',(-0.316872066876738,2.15876687866993,
12.0957685970524));
#69826=CARTESIAN_POINT('Ctrl Pts',(-0.316967645393132,2.15824915934225,
12.0958008278167));
#69827=CARTESIAN_POINT('Ctrl Pts',(-0.317132999465671,2.15734102862904,
12.0958574095478));
#69828=CARTESIAN_POINT('Ctrl Pts',(-0.317203323930711,2.15695071728576,
12.0958817429893));
#69829=CARTESIAN_POINT('Ctrl Pts',(-0.31733836036152,2.1561932350945,12.0959289963291));
#69830=CARTESIAN_POINT('Ctrl Pts',(-0.317403156032775,2.15582607962183,
12.0959519135238));
#69831=CARTESIAN_POINT('Ctrl Pts',(-0.317556157066649,2.1549502435909,12.0960066136525));
#69832=CARTESIAN_POINT('Ctrl Pts',(-0.317643777295143,2.15444146308063,
12.0960384151356));
#69833=CARTESIAN_POINT('Ctrl Pts',(-0.31790451429511,2.15290539394979,12.0961345064152));
#69834=CARTESIAN_POINT('Ctrl Pts',(-0.318073871539974,2.15187748182884,
12.096198915421));
#69835=CARTESIAN_POINT('Ctrl Pts',(-0.319789487367902,2.14114026054711,
12.0968728504719));
#69836=CARTESIAN_POINT('Ctrl Pts',(-0.320895507197951,2.13136681055273,
12.0974962639784));
#69837=CARTESIAN_POINT('Ctrl Pts',(-0.322040275759761,2.11429246827615,
12.0986041887887));
#69838=CARTESIAN_POINT('Ctrl Pts',(-0.322280985094732,2.10701205250904,
12.0990824510732));
#69839=CARTESIAN_POINT('Ctrl Pts',(-0.322247790519718,2.06737328250978,
12.1017144122446));
#69840=CARTESIAN_POINT('Ctrl Pts',(-0.317348336812178,2.03520732101442,
12.1039744415003));
#69841=CARTESIAN_POINT('Ctrl Pts',(-0.307300500071528,2.0028929287017,12.1061144844357));
#69842=CARTESIAN_POINT('Ctrl Pts',(-0.306849793355093,2.00147799657012,
12.106207871317));
#69843=CARTESIAN_POINT('Ctrl Pts',(-0.306257549281033,1.99966222201093,
12.1063272586368));
#69844=CARTESIAN_POINT('Ctrl Pts',(-0.306124986182603,1.99925850396661,
12.1063537740615));
#69845=CARTESIAN_POINT('Ctrl Pts',(-0.305913652020919,1.99861915933155,
12.1063957175632));
#69846=CARTESIAN_POINT('Ctrl Pts',(-0.305835406893998,1.99838336140965,
12.1064111765899));
#69847=CARTESIAN_POINT('Ctrl Pts',(-0.305694695923818,1.99796095240443,
12.1064388512764));
#69848=CARTESIAN_POINT('Ctrl Pts',(-0.30563233228046,1.99777430941643,12.1064510728784));
#69849=CARTESIAN_POINT('Ctrl Pts',(-0.30548528526606,1.99733556196087,12.1064797872487));
#69850=CARTESIAN_POINT('Ctrl Pts',(-0.305400460886729,1.99708350548443,
12.1064962715204));
#69851=CARTESIAN_POINT('Ctrl Pts',(-0.305153594464095,1.99635293228873,
12.106544016697));
#69852=CARTESIAN_POINT('Ctrl Pts',(-0.304990738169087,1.99587468848168,
12.1065752294648));
#69853=CARTESIAN_POINT('Ctrl Pts',(-0.303856036836927,1.99256802661997,
12.1067907625882));
#69854=CARTESIAN_POINT('Ctrl Pts',(-0.302845945008753,1.98975275439017,
12.1069728600996));
#69855=CARTESIAN_POINT('Ctrl Pts',(-0.299565469078418,1.98099509792868,
12.1075361080725));
#69856=CARTESIAN_POINT('Ctrl Pts',(-0.297158148072634,1.97510531176735,
12.1079102432682));
#69857=CARTESIAN_POINT('Ctrl Pts',(-0.288196181561464,1.95490790868862,
12.1091895043447));
#69858=CARTESIAN_POINT('Ctrl Pts',(-0.280769314203126,1.94101128607393,
12.1100638285064));
#69859=CARTESIAN_POINT('Ctrl Pts',(-0.264949236511171,1.91600255692778,
12.1117184880149));
#69860=CARTESIAN_POINT('Ctrl Pts',(-0.256794869216396,1.90478340659086,
12.1124958224374));
#69861=CARTESIAN_POINT('Ctrl Pts',(-0.240440600941432,1.88508730337559,
12.1139737063647));
#69862=CARTESIAN_POINT('Ctrl Pts',(-0.232449213616003,1.87646820261433,
12.1146666713391));
#69863=CARTESIAN_POINT('Ctrl Pts',(-0.223223726701841,1.8675488714921,12.115446673721));
#69864=CARTESIAN_POINT('Ctrl Pts',(-0.222437728606187,1.86679662061965,
12.1155129761535));
#69865=CARTESIAN_POINT('Ctrl Pts',(-0.221264844718941,1.86568541954142,
12.115611695542));
#69866=CARTESIAN_POINT('Ctrl Pts',(-0.220880856389436,1.86532341105381,
12.1156439806317));
#69867=CARTESIAN_POINT('Ctrl Pts',(-0.220221842818759,1.86470517034173,
12.1156993313465));
#69868=CARTESIAN_POINT('Ctrl Pts',(-0.219947254413533,1.86444847231994,
12.1157223769395));
#69869=CARTESIAN_POINT('Ctrl Pts',(-0.219412032312354,1.86394987365464,
12.115767263944));
#69870=CARTESIAN_POINT('Ctrl Pts',(-0.219151445996653,1.86370792271613,
12.1157891031603));
#69871=CARTESIAN_POINT('Ctrl Pts',(-0.218526944253705,1.86313000280699,
12.1158414055441));
#69872=CARTESIAN_POINT('Ctrl Pts',(-0.21816265455396,1.86279444127789,12.1158718859937));
#69873=CARTESIAN_POINT('Ctrl Pts',(-0.217066850152191,1.86178971245898,
12.1159634871017));
#69874=CARTESIAN_POINT('Ctrl Pts',(-0.216333024729269,1.86112308420092,
12.1160247151333));
#69875=CARTESIAN_POINT('Ctrl Pts',(-0.209760656893737,1.85520767838577,
12.1165721010869));
#69876=CARTESIAN_POINT('Ctrl Pts',(-0.203735656965121,1.85017090129081,
12.1170670578835));
#69877=CARTESIAN_POINT('Ctrl Pts',(-0.192306823100366,1.84130517338212,
12.1179949464548));
#69878=CARTESIAN_POINT('Ctrl Pts',(-0.186957188246556,1.83741300892228,
12.1184251378175));
#69879=CARTESIAN_POINT('Ctrl Pts',(-0.167782063506492,1.82434512488735,
12.1199519569906));
#69880=CARTESIAN_POINT('Ctrl Pts',(-0.153372223662145,1.81607517145014,
12.1210743362764));
#69881=CARTESIAN_POINT('Ctrl Pts',(-0.121137962395615,1.80074801912172,
12.1234891764099));
#69882=CARTESIAN_POINT('Ctrl Pts',(-0.103187067520866,1.79409352941735,
12.124777067591));
#69883=CARTESIAN_POINT('Ctrl Pts',(-0.083688634493038,1.78877885807314,
12.1260505124402));
#69884=CARTESIAN_POINT('Ctrl Pts',(-0.0826253754244083,1.78849488905523,
12.1261195638895));
#69885=CARTESIAN_POINT('Ctrl Pts',(-0.0811955632310493,1.78812085905379,
12.1262118778034));
#69886=CARTESIAN_POINT('Ctrl Pts',(-0.0808302922582874,1.78802599162324,
12.126235413582));
#69887=CARTESIAN_POINT('Ctrl Pts',(-0.0802575677386353,1.78787831816809,
12.1262722411104));
#69888=CARTESIAN_POINT('Ctrl Pts',(-0.0800502282704827,1.7878250772349,
12.1262855580805));
#69889=CARTESIAN_POINT('Ctrl Pts',(-0.079651652303674,1.78772315351383,
12.126311127882));
#69890=CARTESIAN_POINT('Ctrl Pts',(-0.0794604255616051,1.78767444014961,
12.1263233823936));
#69891=CARTESIAN_POINT('Ctrl Pts',(-0.0790064856221822,1.78755924674988,
12.126352441263));
#69892=CARTESIAN_POINT('Ctrl Pts',(-0.0787437335160616,1.78749292248796,
12.1263692364708));
#69893=CARTESIAN_POINT('Ctrl Pts',(-0.0779675644234021,1.78729804182714,
12.1264187770687));
#69894=CARTESIAN_POINT('Ctrl Pts',(-0.0774539108930987,1.78717041788851,
12.1264514685728));
#69895=CARTESIAN_POINT('Ctrl Pts',(-0.073454671590297,1.78618720844768,
12.126705289892));
#69896=CARTESIAN_POINT('Ctrl Pts',(-0.069955153749981,1.7853885952402,12.1269231994161));
#69897=CARTESIAN_POINT('Ctrl Pts',(-0.0575787702630422,1.7827809578194,
12.127681471899));
#69898=CARTESIAN_POINT('Ctrl Pts',(-0.0486391019565784,1.78128774523499,
12.1282069254693));
#69899=CARTESIAN_POINT('Ctrl Pts',(-0.0124974444364622,1.77680740547635,
12.1302842609111));
#69900=CARTESIAN_POINT('Ctrl Pts',(0.0149704029345457,1.77691236870578,
12.1317670682871));
#69901=CARTESIAN_POINT('Ctrl Pts',(0.0440525856281309,1.78074392552548,
12.1334674639364));
#69902=CARTESIAN_POINT('Ctrl Pts',(0.0460070073745451,1.7810197083649,12.133582317846));
#69903=CARTESIAN_POINT('Ctrl Pts',(0.0504657912932282,1.78169070521084,
12.1338457928476));
#69904=CARTESIAN_POINT('Ctrl Pts',(0.0529682478138649,1.78209755037014,
12.1339947146648));
#69905=CARTESIAN_POINT('Ctrl Pts',(0.0617980585269762,1.78364023692487,
12.1345242449501));
#69906=CARTESIAN_POINT('Ctrl Pts',(0.0680956286381113,1.78493575843284,
12.1349093614281));
#69907=CARTESIAN_POINT('Ctrl Pts',(0.0753518288853519,1.78665619883699,
12.1353632454283));
#69908=CARTESIAN_POINT('Ctrl Pts',(0.0763525683939736,1.78689854502939,
12.1354260677032));
#69909=CARTESIAN_POINT('Ctrl Pts',(0.0778404102545852,1.78726640864994,
12.1355198090705));
#69910=CARTESIAN_POINT('Ctrl Pts',(0.0783284146839475,1.78738827904912,
12.1355506104555));
#69911=CARTESIAN_POINT('Ctrl Pts',(0.0791974873826132,1.78760747719763,
12.1356055620188));
#69912=CARTESIAN_POINT('Ctrl Pts',(0.0795786673914997,1.78770436121431,
12.135629697816));
#69913=CARTESIAN_POINT('Ctrl Pts',(0.0803811435798505,1.78790989013368,
12.1356805810226));
#69914=CARTESIAN_POINT('Ctrl Pts',(0.0808023987152766,1.7880186908187,12.1357073334303));
#69915=CARTESIAN_POINT('Ctrl Pts',(0.081912840741439,1.78830789283193,12.1357779639882));
#69916=CARTESIAN_POINT('Ctrl Pts',(0.0826016491628338,1.78848972618587,
12.1358218884506));
#69917=CARTESIAN_POINT('Ctrl Pts',(0.0857016748337845,1.7893190835939,12.1360200840034));
#69918=CARTESIAN_POINT('Ctrl Pts',(0.0881058690337412,1.78999231595668,
12.1361751873675));
#69919=CARTESIAN_POINT('Ctrl Pts',(0.105801443053288,1.79516997420092,12.1373273977299));
#69920=CARTESIAN_POINT('Ctrl Pts',(0.120745335951812,1.8007748051267,12.1383608542996));
#69921=CARTESIAN_POINT('Ctrl Pts',(0.163991563556159,1.82076322136371,12.1415293385699));
#69922=CARTESIAN_POINT('Ctrl Pts',(0.190649576433447,1.83823845157279,12.1437409005924));
#69923=CARTESIAN_POINT('Ctrl Pts',(0.215482609035767,1.86035272615333,12.1458449273601));
#69924=CARTESIAN_POINT('Ctrl Pts',(0.216630955468818,1.8613902767711,12.1459422892195));
#69925=CARTESIAN_POINT('Ctrl Pts',(0.218086282725865,1.8627243566944,12.1460657117548));
#69926=CARTESIAN_POINT('Ctrl Pts',(0.21840018471435,1.86301325576943,12.1460923349739));
#69927=CARTESIAN_POINT('Ctrl Pts',(0.21889808397416,1.86347332579699,12.1461345655422));
#69928=CARTESIAN_POINT('Ctrl Pts',(0.219082454892995,1.86364408884864,12.1461502038248));
#69929=CARTESIAN_POINT('Ctrl Pts',(0.219423226082209,1.86396045005131,12.146179108353));
#69930=CARTESIAN_POINT('Ctrl Pts',(0.219579680135567,1.86410598702748,12.1461923790611));
#69931=CARTESIAN_POINT('Ctrl Pts',(0.219929615102729,1.86443215396266,12.1462220615753));
#69932=CARTESIAN_POINT('Ctrl Pts',(0.22012301782706,1.86461286630357,12.1462384668841));
#69933=CARTESIAN_POINT('Ctrl Pts',(0.22052572467431,1.86499007935451,12.1462726275565));
#69934=CARTESIAN_POINT('Ctrl Pts',(0.220734989441227,1.86518662201053,12.1462903796853));
#69935=CARTESIAN_POINT('Ctrl Pts',(0.221277199461615,1.86569723408782,12.1463363785576));
#69936=CARTESIAN_POINT('Ctrl Pts',(0.221609740203629,1.8660117349768,12.1463645925796));
#69937=CARTESIAN_POINT('Ctrl Pts',(0.222585153736869,1.86693817834692,12.1464473621812));
#69938=CARTESIAN_POINT('Ctrl Pts',(0.223226176146524,1.86755207529081,12.1465017718546));
#69939=CARTESIAN_POINT('Ctrl Pts',(0.230125938239207,1.87421473208817,12.1470876933559));
#69940=CARTESIAN_POINT('Ctrl Pts',(0.236140339687896,1.88051263229804,12.1476008962165));
#69941=CARTESIAN_POINT('Ctrl Pts',(0.252639012382195,1.89925343638975,12.1490429328214));
#69942=CARTESIAN_POINT('Ctrl Pts',(0.262446425155853,1.91225657752088,12.1499445656362));
#69943=CARTESIAN_POINT('Ctrl Pts',(0.28433442614348,1.94636479749796,12.1522121255405));
#69944=CARTESIAN_POINT('Ctrl Pts',(0.295088261136304,1.96819517835631,12.1535863466674));
#69945=CARTESIAN_POINT('Ctrl Pts',(0.303771665303652,1.99236184144264,12.1551447107973));
#69946=CARTESIAN_POINT('Ctrl Pts',(0.304243654791469,1.99370326328157,12.1552312974069));
#69947=CARTESIAN_POINT('Ctrl Pts',(0.304879957457614,1.99555063397955,12.1553506751489));
#69948=CARTESIAN_POINT('Ctrl Pts',(0.305051923788697,1.99605394519802,12.1553832127895));
#69949=CARTESIAN_POINT('Ctrl Pts',(0.305343654298555,1.99691474138801,12.15543888473));
#69950=CARTESIAN_POINT('Ctrl Pts',(0.305464038969914,1.99727201618972,12.1554619984802));
#69951=CARTESIAN_POINT('Ctrl Pts',(0.305696615527068,1.99796627505659,12.155506927252));
#69952=CARTESIAN_POINT('Ctrl Pts',(0.305808877867033,1.99830323512187,12.1555287399115));
#69953=CARTESIAN_POINT('Ctrl Pts',(0.306075431373924,1.99910773896031,12.1555808339469));
#69954=CARTESIAN_POINT('Ctrl Pts',(0.306229208255277,1.99957545103168,12.1556111322259));
#69955=CARTESIAN_POINT('Ctrl Pts',(0.306684935265848,2.00097232396216,12.1557016597356));
#69956=CARTESIAN_POINT('Ctrl Pts',(0.306983730562625,2.00190250117017,12.1557619926299));
#69957=CARTESIAN_POINT('Ctrl Pts',(0.309490836658603,2.0098309883645,12.1562767004672));
#69958=CARTESIAN_POINT('Ctrl Pts',(0.311463589293737,2.01690098117099,12.1567387472258));
#69959=CARTESIAN_POINT('Ctrl Pts',(0.315909750651387,2.03523109486856,12.1579459568555));
#69960=CARTESIAN_POINT('Ctrl Pts',(0.318023348799647,2.04656701624795,12.1587016373454));
#69961=CARTESIAN_POINT('Ctrl Pts',(0.323539167175525,2.08852075933428,12.1615225826909));
#69962=CARTESIAN_POINT('Ctrl Pts',(0.32315693868286,2.11946723999282,12.1636662977494));
#69963=CARTESIAN_POINT('Ctrl Pts',(0.31814886681069,2.15142861911134,12.1657135095731));
#69964=CARTESIAN_POINT('Ctrl Pts',(0.317896448046752,2.15296652592275,12.165811559086));
#69965=CARTESIAN_POINT('Ctrl Pts',(0.317560539174908,2.15492415263175,12.1659357318024));
#69966=CARTESIAN_POINT('Ctrl Pts',(0.317487361438907,2.15534558622842,12.1659624257878));
#69967=CARTESIAN_POINT('Ctrl Pts',(0.317369813387169,2.1560146450507,12.1660047434122));
#69968=CARTESIAN_POINT('Ctrl Pts',(0.317325992120164,2.15626236429047,12.1660203981995));
#69969=CARTESIAN_POINT('Ctrl Pts',(0.317244443217679,2.15672022969564,12.1660493083529));
#69970=CARTESIAN_POINT('Ctrl Pts',(0.317206797081795,2.15693038814862,12.1660625682373));
#69971=CARTESIAN_POINT('Ctrl Pts',(0.317122089855381,2.15740057122688,12.1660922125629));
#69972=CARTESIAN_POINT('Ctrl Pts',(0.317074917902033,2.15766057483267,12.1661085905489));
#69973=CARTESIAN_POINT('Ctrl Pts',(0.316975935576021,2.15820235365931,12.1661426875516));
#69974=CARTESIAN_POINT('Ctrl Pts',(0.316924069109392,2.15848411858298,12.1661604033609));
#69975=CARTESIAN_POINT('Ctrl Pts',(0.316788623970022,2.15921445387308,12.166206279191));
#69976=CARTESIAN_POINT('Ctrl Pts',(0.316704467899478,2.15966291849028,12.1662344067328));
#69977=CARTESIAN_POINT('Ctrl Pts',(0.316454514231153,2.16097948116525,12.1663168597775));
#69978=CARTESIAN_POINT('Ctrl Pts',(0.316286096251948,2.16184708610698,12.1663710407114));
#69979=CARTESIAN_POINT('Ctrl Pts',(0.314432769509267,2.17118890361534,12.1669528618822));
#69980=CARTESIAN_POINT('Ctrl Pts',(0.312411125221211,2.17959362252603,12.1674624570753));
#69981=CARTESIAN_POINT('Ctrl Pts',(0.305634879415968,2.20349370862875,12.1688976972309));
#69982=CARTESIAN_POINT('Ctrl Pts',(0.300046657608677,2.21872529631896,12.1697961214094));
#69983=CARTESIAN_POINT('Ctrl Pts',(0.283245103546552,2.25565047156884,12.1720657265194));
#69984=CARTESIAN_POINT('Ctrl Pts',(0.270673308898107,2.27660851819424,12.1734450973064));
#69985=CARTESIAN_POINT('Ctrl Pts',(0.254983928620161,2.29709504293656,12.1750108085516));
#69986=CARTESIAN_POINT('Ctrl Pts',(0.254098472250674,2.29823527965232,12.1750987039041));
#69987=CARTESIAN_POINT('Ctrl Pts',(0.252874219383313,2.29979011832866,12.1752196092392));
#69988=CARTESIAN_POINT('Ctrl Pts',(0.252541997182618,2.30020989452088,12.1752523572321));
#69989=CARTESIAN_POINT('Ctrl Pts',(0.251973441853097,2.30092462037754,12.175308297045));
#69990=CARTESIAN_POINT('Ctrl Pts',(0.251737632190452,2.30121998660751,12.1753314678812));
#69991=CARTESIAN_POINT('Ctrl Pts',(0.251279426017346,2.30179185215891,12.1753764332272));
#69992=CARTESIAN_POINT('Ctrl Pts',(0.251057091246833,2.30206840047481,12.1753982252374));
#69993=CARTESIAN_POINT('Ctrl Pts',(0.250526660210225,2.30272594365249,12.1754501525763));
#69994=CARTESIAN_POINT('Ctrl Pts',(0.250218151575264,2.30310660334889,12.175480304504));
#69995=CARTESIAN_POINT('Ctrl Pts',(0.249299165575879,2.30423524138608,12.1755699741035));
#69996=CARTESIAN_POINT('Ctrl Pts',(0.248686197827588,2.30498117659541,12.1756295925217));
#69997=CARTESIAN_POINT('Ctrl Pts',(0.24362552048113,2.31108352543893,12.1761202596055));
#69998=CARTESIAN_POINT('Ctrl Pts',(0.239008957799691,2.31629691364484,12.1765582023383));
#69999=CARTESIAN_POINT('Ctrl Pts',(0.227115030733097,2.32888242872741,12.1776646337308));
#70000=CARTESIAN_POINT('Ctrl Pts',(0.219644645872505,2.3360605802087,12.1783409527639));
#70001=CARTESIAN_POINT('Ctrl Pts',(0.200531663456048,2.35273206026565,12.1800245063167));
#70002=CARTESIAN_POINT('Ctrl Pts',(0.18854611791864,2.36179525696979,12.1810424146601));
#70003=CARTESIAN_POINT('Ctrl Pts',(0.174158870863387,2.3711725564389,12.1822035062334));
#70004=CARTESIAN_POINT('Ctrl Pts',(0.172332296021505,2.37233701091298,12.1823498359201));
#70005=CARTESIAN_POINT('Ctrl Pts',(0.156946852189241,2.38192856827801,12.1835727606581));
#70006=CARTESIAN_POINT('Ctrl Pts',(0.142788824312264,2.38935708268555,12.1846371156795));
#70007=CARTESIAN_POINT('Ctrl Pts',(0.127308311871691,2.39606516943603,12.1856980667814));
#70008=CARTESIAN_POINT('Ctrl Pts',(0.126478346037844,2.39642067885795,12.1857546444854));
#70009=CARTESIAN_POINT('Ctrl Pts',(0.125358628255423,2.39689474217853,12.1858305551512));
#70010=CARTESIAN_POINT('Ctrl Pts',(0.125070191960333,2.39701636435786,12.1858500722007));
#70011=CARTESIAN_POINT('Ctrl Pts',(0.124583842366009,2.3972206046707,12.1858829176177));
#70012=CARTESIAN_POINT('Ctrl Pts',(0.124386023764666,2.39730344551001,12.1858962595539));
#70013=CARTESIAN_POINT('Ctrl Pts',(0.123990143025759,2.39746876489539,12.1859229243216));
#70014=CARTESIAN_POINT('Ctrl Pts',(0.12379208277191,2.39755124247632,12.1859362469755));
#70015=CARTESIAN_POINT('Ctrl Pts',(0.123341589003261,2.39773831246295,12.1859665094598));
#70016=CARTESIAN_POINT('Ctrl Pts',(0.123089105178579,2.39784278147001,12.1859834416839));
#70017=CARTESIAN_POINT('Ctrl Pts',(0.122560065624196,2.39806089199314,12.1860188610108));
#70018=CARTESIAN_POINT('Ctrl Pts',(0.122283483791231,2.39817447009283,12.1860373442625));
#70019=CARTESIAN_POINT('Ctrl Pts',(0.121556719301025,2.39847173404023,12.1860858239132));
#70020=CARTESIAN_POINT('Ctrl Pts',(0.121106276221756,2.39865478716254,12.1861157825205));
#70021=CARTESIAN_POINT('Ctrl Pts',(0.119761188344413,2.39919786662018,12.186204983752));
#70022=CARTESIAN_POINT('Ctrl Pts',(0.118865330479024,2.39955490129152,12.1862640518854));
#70023=CARTESIAN_POINT('Ctrl Pts',(0.115688372705815,2.40080454801704,12.1864723614415));
#70024=CARTESIAN_POINT('Ctrl Pts',(0.113398650085323,2.40167519395395,12.1866203817086));
#70025=CARTESIAN_POINT('Ctrl Pts',(0.102201278301866,2.40578738418493,12.1873350184067));
#70026=CARTESIAN_POINT('Ctrl Pts',(0.0931627634098174,2.40866123273915,
12.1878836928875));
#70027=CARTESIAN_POINT('Ctrl Pts',(0.0535327939586389,2.41936185417131,
12.1902206434306));
#70028=CARTESIAN_POINT('Ctrl Pts',(0.0220135996442052,2.42306847842293,
12.1919242965977));
#70029=CARTESIAN_POINT('Ctrl Pts',(-0.0105381364554002,2.42210419953507,
12.1938498746952));
#70030=CARTESIAN_POINT('Ctrl Pts',(-0.0115335683588456,2.42207009244559,
12.1939088976496));
#70031=CARTESIAN_POINT('Ctrl Pts',(-0.0178491844456279,2.42182437971641,
12.1942842900059));
#70032=CARTESIAN_POINT('Ctrl Pts',(-0.0231633463181839,2.42148558145952,
12.1946043003191));
#70033=CARTESIAN_POINT('Ctrl Pts',(-0.0293377015159986,2.42093806246608,
12.1949817357561));
#70034=CARTESIAN_POINT('Ctrl Pts',(-0.0302086260850107,2.42085725729072,
12.1950351051084));
#70035=CARTESIAN_POINT('Ctrl Pts',(-0.0315966277756221,2.42072277589623,
12.1951203717778));
#70036=CARTESIAN_POINT('Ctrl Pts',(-0.0321139268470682,2.42067139186843,
12.1951521969492));
#70037=CARTESIAN_POINT('Ctrl Pts',(-0.033026045331891,2.42057856065976,
12.195208395592));
#70038=CARTESIAN_POINT('Ctrl Pts',(-0.0334209176978157,2.42053763504922,
12.1952327525945));
#70039=CARTESIAN_POINT('Ctrl Pts',(-0.0342365638744501,2.42045157576002,
12.1952831217451));
#70040=CARTESIAN_POINT('Ctrl Pts',(-0.034657326230079,2.42040634271012,
12.1953091369793));
#70041=CARTESIAN_POINT('Ctrl Pts',(-0.0357331371261176,2.42028854630009,
12.1953757345369));
#70042=CARTESIAN_POINT('Ctrl Pts',(-0.036388052057458,2.42021480233908,
12.1954163540023));
#70043=CARTESIAN_POINT('Ctrl Pts',(-0.0390517894580874,2.41990658592075,
12.1955818835482));
#70044=CARTESIAN_POINT('Ctrl Pts',(-0.0410585759184614,2.419655218977,12.1957073253495));
#70045=CARTESIAN_POINT('Ctrl Pts',(-0.0738055382937274,2.41523993066607,
12.1977666774738));
#70046=CARTESIAN_POINT('Ctrl Pts',(-0.103782248977166,2.40667864323254,
12.1998542954765));
#70047=CARTESIAN_POINT('Ctrl Pts',(-0.144461119167753,2.38840393394621,
12.202869108715));
#70048=CARTESIAN_POINT('Ctrl Pts',(-0.156493427571204,2.38205622275597,
12.2037827354587));
#70049=CARTESIAN_POINT('Ctrl Pts',(-0.169157401257869,2.37431462748633,
12.2047444982193));
#70050=CARTESIAN_POINT('Ctrl Pts',(-0.170221184020779,2.37365578718893,
12.2048252833724));
#70051=CARTESIAN_POINT('Ctrl Pts',(-0.174383873036224,2.37104401366694,
12.2051413099288));
#70052=CARTESIAN_POINT('Ctrl Pts',(-0.177453378384979,2.36904440868316,
12.2053741392918));
#70053=CARTESIAN_POINT('Ctrl Pts',(-0.180967550912966,2.36666881297011,
12.2056398508253));
#70054=CARTESIAN_POINT('Ctrl Pts',(-0.181445952814739,2.36634353101555,
12.2056760049753));
#70055=CARTESIAN_POINT('Ctrl Pts',(-0.182155425700699,2.36585833722564,
12.2057295911317));
#70056=CARTESIAN_POINT('Ctrl Pts',(-0.182387164269939,2.36569941079272,
12.2057470893593));
#70057=CARTESIAN_POINT('Ctrl Pts',(-0.182794936290268,2.36541897566497,
12.2057778705777));
#70058=CARTESIAN_POINT('Ctrl Pts',(-0.182971056585335,2.365297594843,12.2057911622665));
#70059=CARTESIAN_POINT('Ctrl Pts',(-0.18334378918105,2.36504016253991,12.2058192857141));
#70060=CARTESIAN_POINT('Ctrl Pts',(-0.183540370430215,2.36490406794475,
12.2058341144152));
#70061=CARTESIAN_POINT('Ctrl Pts',(-0.183943112934896,2.36462458293121,
12.20586448715));
#70062=CARTESIAN_POINT('Ctrl Pts',(-0.184149258480139,2.36448117001017,
12.2058800296304));
#70063=CARTESIAN_POINT('Ctrl Pts',(-0.184660221257112,2.36412481248137,
12.2059185447945));
#70064=CARTESIAN_POINT('Ctrl Pts',(-0.184964838935141,2.36391158035218,
12.2059414980038));
#70065=CARTESIAN_POINT('Ctrl Pts',(-0.185813214923136,2.36331552746861,
12.2060054031896));
#70066=CARTESIAN_POINT('Ctrl Pts',(-0.186356162175378,2.36293154752429,
12.2060462777403));
#70067=CARTESIAN_POINT('Ctrl Pts',(-0.188101766720825,2.36168890812007,
12.206177628532));
#70068=CARTESIAN_POINT('Ctrl Pts',(-0.189299728251979,2.36082364223252,
12.2062676741761));
#70069=CARTESIAN_POINT('Ctrl Pts',(-0.194041814136444,2.35734863709071,
12.2066239139265));
#70070=CARTESIAN_POINT('Ctrl Pts',(-0.197538433894537,2.35467453332596,
12.2068861379953));
#70071=CARTESIAN_POINT('Ctrl Pts',(-0.207413829897046,2.34679633427967,
12.2076289068151));
#70072=CARTESIAN_POINT('Ctrl Pts',(-0.213649704531986,2.34141820217246,
12.2081006662662));
#70073=CARTESIAN_POINT('Ctrl Pts',(-0.244124843119446,2.31302814833285,
12.210459137361));
#70074=CARTESIAN_POINT('Ctrl Pts',(-0.264882979066932,2.28658758370106,
12.212269165555));
#70075=CARTESIAN_POINT('Ctrl Pts',(-0.281548317275773,2.25681903024943,
12.2143184235909));
#70076=CARTESIAN_POINT('Ctrl Pts',(-0.281887433592866,2.25620863606117,
12.2143604351478));
#70077=CARTESIAN_POINT('Ctrl Pts',(-0.283461767497315,2.25335308439422,
12.2145569448378));
#70078=CARTESIAN_POINT('Ctrl Pts',(-0.28467213597157,2.25109439613411,12.2147122974484));
#70079=CARTESIAN_POINT('Ctrl Pts',(-0.2862024491468,2.24815498132722,12.2149144507731));
#70080=CARTESIAN_POINT('Ctrl Pts',(-0.28654714894836,2.24748719200055,12.2149603754758));
#70081=CARTESIAN_POINT('Ctrl Pts',(-0.287091700957168,2.24642311241345,
12.2150335536904));
#70082=CARTESIAN_POINT('Ctrl Pts',(-0.287293077144125,2.24602760160073,
12.2150607535405));
#70083=CARTESIAN_POINT('Ctrl Pts',(-0.287652968475392,2.245317134835,12.2151096139321));
#70084=CARTESIAN_POINT('Ctrl Pts',(-0.287811785250694,2.2450023317694,12.2151312638428));
#70085=CARTESIAN_POINT('Ctrl Pts',(-0.288181300273844,2.24426688854295,
12.2151818431708));
#70086=CARTESIAN_POINT('Ctrl Pts',(-0.288391594312289,2.24384604716049,
12.2152107866899));
#70087=CARTESIAN_POINT('Ctrl Pts',(-0.288989378074391,2.24264317964662,
12.2152935169491));
#70088=CARTESIAN_POINT('Ctrl Pts',(-0.289374611348188,2.24186004237497,
12.2153473823499));
#70089=CARTESIAN_POINT('Ctrl Pts',(-0.291809918762221,2.23685813026403,
12.2156914536161));
#70090=CARTESIAN_POINT('Ctrl Pts',(-0.293770775581835,2.23259677288957,
12.2159847406427));
#70091=CARTESIAN_POINT('Ctrl Pts',(-0.299365630372979,2.21970414481153,
12.2168731335076));
#70092=CARTESIAN_POINT('Ctrl Pts',(-0.302716903732548,2.21095634819819,
12.2174774693702));
#70093=CARTESIAN_POINT('Ctrl Pts',(-0.316678617351566,2.16914572635596,
12.2203718361332));
#70094=CARTESIAN_POINT('Ctrl Pts',(-0.322279760427778,2.13466281959473,
12.2228062951007));
#70095=CARTESIAN_POINT('Ctrl Pts',(-0.322274996964664,2.09995576849626,
12.2250196508122));
#70096=CARTESIAN_POINT('',(-0.322191991682866,2.10029560349716,12.3497226077682));
#70097=CARTESIAN_POINT('Ctrl Pts',(-0.32279233570592,2.09993664501779,12.2247226550727));
#70098=CARTESIAN_POINT('Ctrl Pts',(-0.322801489738851,2.09653177634649,
12.2249337817233));
#70099=CARTESIAN_POINT('Ctrl Pts',(-0.321208780390457,1.98631842288104,
12.2317683562149));
#70100=CARTESIAN_POINT('Ctrl Pts',(-0.195976803199286,1.7731848083249,12.2452263785474));
#70101=CARTESIAN_POINT('Ctrl Pts',(0.168706279937227,1.75830822659656,12.2650967220702));
#70102=CARTESIAN_POINT('Ctrl Pts',(0.378624318517414,2.05688732983139,12.284967065593));
#70103=CARTESIAN_POINT('Ctrl Pts',(0.241206089904363,2.39501643868587,12.3048374091158));
#70104=CARTESIAN_POINT('Ctrl Pts',(-0.117485888951984,2.46250812790751,
12.3247077526386));
#70105=CARTESIAN_POINT('Ctrl Pts',(-0.306416606983072,2.26292630316716,
12.3396694855227));
#70106=CARTESIAN_POINT('Ctrl Pts',(-0.322441083855502,2.12808501973466,
12.3480077705659));
#70107=CARTESIAN_POINT('Ctrl Pts',(-0.322191991682866,2.10029560349716,
12.3497226077682));
#70108=CARTESIAN_POINT('',(-0.322274943346505,2.09975100738521,12.5998588212847));
#70109=CARTESIAN_POINT('Ctrl Pts',(-0.322274867496596,2.10029224142693,
12.3496749413664));
#70110=CARTESIAN_POINT('Ctrl Pts',(-0.322296495229194,2.07644184235539,
12.3510102465589));
#70111=CARTESIAN_POINT('Ctrl Pts',(-0.319670682733467,2.05266582285634,
12.3523648898113));
#70112=CARTESIAN_POINT('Ctrl Pts',(-0.314258803938727,2.02856252633657,
12.3538660697406));
#70113=CARTESIAN_POINT('Ctrl Pts',(-0.314067932909001,2.02772799994053,
12.3539181974045));
#70114=CARTESIAN_POINT('Ctrl Pts',(-0.313753399015614,2.0263775736076,12.3540028010071));
#70115=CARTESIAN_POINT('Ctrl Pts',(-0.313631782519355,2.02586119740506,
12.3540352112806));
#70116=CARTESIAN_POINT('Ctrl Pts',(-0.31339445757114,2.02486456479613,12.3540978808206));
#70117=CARTESIAN_POINT('Ctrl Pts',(-0.313278918719662,2.02438426922169,
12.3541281345601));
#70118=CARTESIAN_POINT('Ctrl Pts',(-0.313078357963032,2.0235588872839,12.3541802156155));
#70119=CARTESIAN_POINT('Ctrl Pts',(-0.312993868440541,2.02321367143124,
12.3542020257311));
#70120=CARTESIAN_POINT('Ctrl Pts',(-0.312818728813947,2.02250316014996,
12.3542469709228));
#70121=CARTESIAN_POINT('Ctrl Pts',(-0.312728009509253,2.02213788244577,
12.3542701082055));
#70122=CARTESIAN_POINT('Ctrl Pts',(-0.312508116191336,2.02125907455914,
12.3543258476801));
#70123=CARTESIAN_POINT('Ctrl Pts',(-0.31237831630706,2.02074570345677,12.3543584700538));
#70124=CARTESIAN_POINT('Ctrl Pts',(-0.311899040870473,2.0188695918474,12.3544779137642));
#70125=CARTESIAN_POINT('Ctrl Pts',(-0.311541912255455,2.01750883907694,
12.3545649823896));
#70126=CARTESIAN_POINT('Ctrl Pts',(-0.305170201185175,1.99386263348242,
12.3560857210088));
#70127=CARTESIAN_POINT('Ctrl Pts',(-0.29678873525536,1.97228925654693,12.3576002603711));
#70128=CARTESIAN_POINT('Ctrl Pts',(-0.283828034568538,1.94726187056406,
12.3594984299381));
#70129=CARTESIAN_POINT('Ctrl Pts',(-0.281370520131295,1.94278066712219,
12.3598439200554));
#70130=CARTESIAN_POINT('Ctrl Pts',(-0.276392986878284,1.93419509174689,
12.3605154395705));
#70131=CARTESIAN_POINT('Ctrl Pts',(-0.273885423306676,1.93008494444492,
12.3608413550749));
#70132=CARTESIAN_POINT('Ctrl Pts',(-0.264809010705497,1.91593109284126,
12.3619766725555));
#70133=CARTESIAN_POINT('Ctrl Pts',(-0.257771622368049,1.90619852627263,
12.3627810833841));
#70134=CARTESIAN_POINT('Ctrl Pts',(-0.247020297585665,1.89295479670488,
12.3638885385063));
#70135=CARTESIAN_POINT('Ctrl Pts',(-0.243741184786293,1.88910432548278,
12.3642121384117));
#70136=CARTESIAN_POINT('Ctrl Pts',(-0.240048298739609,1.88496924190876,
12.3645599701792));
#70137=CARTESIAN_POINT('Ctrl Pts',(-0.239723179112611,1.88460684770286,
12.3645904564089));
#70138=CARTESIAN_POINT('Ctrl Pts',(-0.239123607778677,1.88394157530411,
12.3646464246558));
#70139=CARTESIAN_POINT('Ctrl Pts',(-0.23884939938938,1.88363848055883,12.3646719244823));
#70140=CARTESIAN_POINT('Ctrl Pts',(-0.238410022727396,1.88315467119545,
12.3647126284764));
#70141=CARTESIAN_POINT('Ctrl Pts',(-0.238245225001502,1.88297362297137,
12.3647278605627));
#70142=CARTESIAN_POINT('Ctrl Pts',(-0.23793240540446,1.88263074232285,12.3647567079094));
#70143=CARTESIAN_POINT('Ctrl Pts',(-0.237784425874324,1.88246887455684,
12.3647703261192));
#70144=CARTESIAN_POINT('Ctrl Pts',(-0.237445423005381,1.88209881470844,
12.3648014598632));
#70145=CARTESIAN_POINT('Ctrl Pts',(-0.237254291327162,1.88189072301716,
12.364818966974));
#70146=CARTESIAN_POINT('Ctrl Pts',(-0.236665690205331,1.88125158174621,
12.3648727400675));
#70147=CARTESIAN_POINT('Ctrl Pts',(-0.236267315075448,1.88082136224369,
12.3649089373353));
#70148=CARTESIAN_POINT('Ctrl Pts',(-0.233257179511233,1.87758835304452,
12.365180985109));
#70149=CARTESIAN_POINT('Ctrl Pts',(-0.230596664937258,1.87483109947546,
12.3654131867485));
#70150=CARTESIAN_POINT('Ctrl Pts',(-0.227437438966471,1.87167174493164,
12.3656804162024));
#70151=CARTESIAN_POINT('Ctrl Pts',(-0.226986067287601,1.87122302131531,
12.3657183988861));
#70152=CARTESIAN_POINT('Ctrl Pts',(-0.212302644645049,1.8567119760241,12.3669477335148));
#70153=CARTESIAN_POINT('Ctrl Pts',(-0.196791406142918,1.84400232019779,
12.3680578825385));
#70154=CARTESIAN_POINT('Ctrl Pts',(-0.171777998542755,1.82713247909485,
12.3697445288577));
#70155=CARTESIAN_POINT('Ctrl Pts',(-0.163092542719674,1.82185403690482,
12.3703132775227));
#70156=CARTESIAN_POINT('Ctrl Pts',(-0.144502965162274,1.81172700613436,
12.3715180821414));
#70157=CARTESIAN_POINT('Ctrl Pts',(-0.1345705344048,1.80695876819794,12.3721550372872));
#70158=CARTESIAN_POINT('Ctrl Pts',(-0.121148702422358,1.80134183665283,
12.3730193777702));
#70159=CARTESIAN_POINT('Ctrl Pts',(-0.117861014221769,1.80002919060396,
12.3732313416604));
#70160=CARTESIAN_POINT('Ctrl Pts',(-0.112458823734777,1.79797482585322,
12.3735803736879));
#70161=CARTESIAN_POINT('Ctrl Pts',(-0.110356981766597,1.79720051347837,
12.373716352169));
#70162=CARTESIAN_POINT('Ctrl Pts',(-0.107767211893838,1.7962769955414,12.3738841708104));
#70163=CARTESIAN_POINT('Ctrl Pts',(-0.107286741302973,1.79610694227634,
12.3739153170629));
#70164=CARTESIAN_POINT('Ctrl Pts',(-0.1064393399561,1.79580928111394,12.3739702704131));
#70165=CARTESIAN_POINT('Ctrl Pts',(-0.106072577196951,1.79568119527145,
12.3739940616255));
#70166=CARTESIAN_POINT('Ctrl Pts',(-0.105330912053665,1.79542368461445,
12.3740421864207));
#70167=CARTESIAN_POINT('Ctrl Pts',(-0.104956000617464,1.79529428810735,
12.3740665208914));
#70168=CARTESIAN_POINT('Ctrl Pts',(-0.104228228611407,1.79504460823843,
12.374113773317));
#70169=CARTESIAN_POINT('Ctrl Pts',(-0.103875396136379,1.79492424435951,
12.3741366885628));
#70170=CARTESIAN_POINT('Ctrl Pts',(-0.10303355804136,1.79463869276486,12.3741913794026));
#70171=CARTESIAN_POINT('Ctrl Pts',(-0.102544364001847,1.79447406747458,
12.3742231735311));
#70172=CARTESIAN_POINT('Ctrl Pts',(-0.101067068798483,1.79398087063957,
12.3743192280852));
#70173=CARTESIAN_POINT('Ctrl Pts',(-0.100077775815596,1.79365591457149,
12.3743836075941));
#70174=CARTESIAN_POINT('Ctrl Pts',(-0.0897483600836429,1.79031835507489,
12.3750564130522));
#70175=CARTESIAN_POINT('Ctrl Pts',(-0.0802777587900481,1.78772938492326,
12.3756786757457));
#70176=CARTESIAN_POINT('Ctrl Pts',(-0.0645588008478664,1.78419465266251,
12.3767217036889));
#70177=CARTESIAN_POINT('Ctrl Pts',(-0.0583741417256624,1.78299320495288,
12.3771345625626));
#70178=CARTESIAN_POINT('Ctrl Pts',(-0.0436968267518361,1.78058602181512,
12.3781192081937));
#70179=CARTESIAN_POINT('Ctrl Pts',(-0.0351834935626272,1.77953656837286,
12.3786941898648));
#70180=CARTESIAN_POINT('Ctrl Pts',(-0.00171687585879573,1.77676076279026,
12.3809597627853));
#70181=CARTESIAN_POINT('Ctrl Pts',(0.0233628538449163,1.77760126893881,
12.3826756874152));
#70182=CARTESIAN_POINT('Ctrl Pts',(0.0493740514826458,1.78152699786694,
12.3843360141426));
#70183=CARTESIAN_POINT('Ctrl Pts',(0.0506524070603436,1.78172781484886,
12.3844172868297));
#70184=CARTESIAN_POINT('Ctrl Pts',(0.0522134327750501,1.78198268002496,
12.3845161025249));
#70185=CARTESIAN_POINT('Ctrl Pts',(0.0524972608750805,1.78202941021471,
12.3845340520266));
#70186=CARTESIAN_POINT('Ctrl Pts',(0.0530461804847233,1.78212054076278,
12.384568732098));
#70187=CARTESIAN_POINT('Ctrl Pts',(0.0533112796173102,1.78216489285197,
12.3845854653811));
#70188=CARTESIAN_POINT('Ctrl Pts',(0.0537706615633961,1.78224234010725,
12.3846144349692));
#70189=CARTESIAN_POINT('Ctrl Pts',(0.0539649691161984,1.78227528176972,
12.3846266800205));
#70190=CARTESIAN_POINT('Ctrl Pts',(0.0543713299783697,1.78234455712618,
12.3846522708329));
#70191=CARTESIAN_POINT('Ctrl Pts',(0.0545833764672977,1.78238092480922,
12.3846656145847));
#70192=CARTESIAN_POINT('Ctrl Pts',(0.0551725576544382,1.78248258158102,
12.384702663434));
#70193=CARTESIAN_POINT('Ctrl Pts',(0.0555496142809594,1.78254833049041,
12.3847263422769));
#70194=CARTESIAN_POINT('Ctrl Pts',(0.057047607315314,1.7828122923175,12.3848202941495));
#70195=CARTESIAN_POINT('Ctrl Pts',(0.0581676246149263,1.78301577493059,
12.3848902709028));
#70196=CARTESIAN_POINT('Ctrl Pts',(0.0780643120329327,1.78673957529713,
12.3861289703446));
#70197=CARTESIAN_POINT('Ctrl Pts',(0.0964955990191437,1.79191727663207,
12.38720761918));
#70198=CARTESIAN_POINT('Ctrl Pts',(0.126063456666013,1.80314004241898,12.3889789536029));
#70199=CARTESIAN_POINT('Ctrl Pts',(0.137496310380895,1.80825938235688,12.3896746638643));
#70200=CARTESIAN_POINT('Ctrl Pts',(0.160054595676795,1.81998165338232,12.3911126450931));
#70201=CARTESIAN_POINT('Ctrl Pts',(0.17113805222637,1.82661480402884,12.391854469339));
#70202=CARTESIAN_POINT('Ctrl Pts',(0.186493905642391,1.83710533213254,12.3929575776971));
#70203=CARTESIAN_POINT('Ctrl Pts',(0.191108329838723,1.84044040505684,12.3932995378452));
#70204=CARTESIAN_POINT('Ctrl Pts',(0.196360101664941,1.84445210622024,12.3937020958421));
#70205=CARTESIAN_POINT('Ctrl Pts',(0.197086015547253,1.84501153361454,12.3937580422227));
#70206=CARTESIAN_POINT('Ctrl Pts',(0.198118067485639,1.84581392701225,12.3938380213069));
#70207=CARTESIAN_POINT('Ctrl Pts',(0.198426169771662,1.84605436898266,12.3938619538538));
#70208=CARTESIAN_POINT('Ctrl Pts',(0.199047032434409,1.84654070782728,12.3939102945346));
#70209=CARTESIAN_POINT('Ctrl Pts',(0.199359776312855,1.84678662457162,12.393934703434));
#70210=CARTESIAN_POINT('Ctrl Pts',(0.199963042964823,1.84726279558797,12.3939819004964));
#70211=CARTESIAN_POINT('Ctrl Pts',(0.200253625566472,1.84749297338201,12.3940046855803));
#70212=CARTESIAN_POINT('Ctrl Pts',(0.200941592519429,1.84803986378302,12.3940587519778));
#70213=CARTESIAN_POINT('Ctrl Pts',(0.201338625318784,1.84835701520459,12.3940900508597));
#70214=CARTESIAN_POINT('Ctrl Pts',(0.202731267096658,1.84947486886477,12.3942001770699));
#70215=CARTESIAN_POINT('Ctrl Pts',(0.203722853173014,1.850280543392,12.394279204454));
#70216=CARTESIAN_POINT('Ctrl Pts',(0.218151265596728,1.86214691846572,12.3954382437835));
#70217=CARTESIAN_POINT('Ctrl Pts',(0.230673036367228,1.87427044267747,12.3965629071262));
#70218=CARTESIAN_POINT('Ctrl Pts',(0.254494312873291,1.90139590926546,12.3989632867845));
#70219=CARTESIAN_POINT('Ctrl Pts',(0.265588036890956,1.91649558765193,12.4002397349749));
#70220=CARTESIAN_POINT('Ctrl Pts',(0.278943830835475,1.93844380037637,12.4019662753593));
#70221=CARTESIAN_POINT('Ctrl Pts',(0.282383442989657,1.94453403120263,12.4024326126142));
#70222=CARTESIAN_POINT('Ctrl Pts',(0.288520839389249,1.95627782889572,12.4033022267684));
#70223=CARTESIAN_POINT('Ctrl Pts',(0.291257401697145,1.96190772861526,12.4037067976145));
#70224=CARTESIAN_POINT('Ctrl Pts',(0.294400135273472,1.96888298102292,12.4041901062997));
#70225=CARTESIAN_POINT('Ctrl Pts',(0.294963592486101,1.97015550997893,12.4042775618792));
#70226=CARTESIAN_POINT('Ctrl Pts',(0.29567858687149,1.97179894964489,12.4043895504796));
#70227=CARTESIAN_POINT('Ctrl Pts',(0.295837689049186,1.97216652320831,12.4044145365268));
#70228=CARTESIAN_POINT('Ctrl Pts',(0.296092210538458,1.97275756398156,12.4044546131207));
#70229=CARTESIAN_POINT('Ctrl Pts',(0.296188062452622,1.97298084267734,12.4044697301013));
#70230=CARTESIAN_POINT('Ctrl Pts',(0.296370117842785,1.97340625148948,12.4044984884381));
#70231=CARTESIAN_POINT('Ctrl Pts',(0.296456366385389,1.97360835968342,12.4045121324582));
#70232=CARTESIAN_POINT('Ctrl Pts',(0.296652519571478,1.97406931534854,12.4045432082144));
#70233=CARTESIAN_POINT('Ctrl Pts',(0.296762292022528,1.97432821820365,12.4045606317783));
#70234=CARTESIAN_POINT('Ctrl Pts',(0.297103278030211,1.97513538587368,12.4046148579569));
#70235=CARTESIAN_POINT('Ctrl Pts',(0.297333313833047,1.97568415155093,12.4046515890031));
#70236=CARTESIAN_POINT('Ctrl Pts',(0.299109096770105,1.97995352542925,12.4049363269711));
#70237=CARTESIAN_POINT('Ctrl Pts',(0.30058655622867,1.98370239176844,12.4051802931541));
#70238=CARTESIAN_POINT('Ctrl Pts',(0.302292067036046,1.98827975321324,12.4054720260709));
#70239=CARTESIAN_POINT('Ctrl Pts',(0.30258753932006,1.98908251529534,12.4055229621931));
#70240=CARTESIAN_POINT('Ctrl Pts',(0.303494426500509,1.99157701145392,12.4056805650547));
#70241=CARTESIAN_POINT('Ctrl Pts',(0.304094885437384,1.99327272013194,12.4057867389432));
#70242=CARTESIAN_POINT('Ctrl Pts',(0.308161596583003,2.00507020894522,12.4065193421156));
#70243=CARTESIAN_POINT('Ctrl Pts',(0.311138282480242,2.0153345568045,12.4071260918152));
#70244=CARTESIAN_POINT('Ctrl Pts',(0.318426266125922,2.04610691562251,12.4089044964611));
#70245=CARTESIAN_POINT('Ctrl Pts',(0.321254638995248,2.06690641464713,12.4100576977834));
#70246=CARTESIAN_POINT('Ctrl Pts',(0.322466804601989,2.09899128551383,12.4119077788129));
#70247=CARTESIAN_POINT('Ctrl Pts',(0.322308138440749,2.11016271437738,12.4125642965293));
#70248=CARTESIAN_POINT('Ctrl Pts',(0.32143789833822,2.12329930318677,12.4133604680997));
#70249=CARTESIAN_POINT('Ctrl Pts',(0.321287032453841,2.12529471316311,12.413482052272));
#70250=CARTESIAN_POINT('Ctrl Pts',(0.321062111267256,2.12794146935968,12.4136442258299));
#70251=CARTESIAN_POINT('Ctrl Pts',(0.321004635739305,2.12859420964545,12.4136842937553));
#70252=CARTESIAN_POINT('Ctrl Pts',(0.32090657300441,2.12967032044656,12.4137504716847));
#70253=CARTESIAN_POINT('Ctrl Pts',(0.320867137527,2.13009379612676,12.4137765454159));
#70254=CARTESIAN_POINT('Ctrl Pts',(0.320789350985821,2.13091156510658,12.4138269566818));
#70255=CARTESIAN_POINT('Ctrl Pts',(0.320751110932969,2.13130586840005,12.413851290679));
#70256=CARTESIAN_POINT('Ctrl Pts',(0.320661513710283,2.1322123298462,12.4139072950026));
#70257=CARTESIAN_POINT('Ctrl Pts',(0.320609656468812,2.13272443648313,12.4139389810211));
#70258=CARTESIAN_POINT('Ctrl Pts',(0.320445374555601,2.13430889281329,12.414037162039));
#70259=CARTESIAN_POINT('Ctrl Pts',(0.320328795829269,2.13538079588493,12.414103787709));
#70260=CARTESIAN_POINT('Ctrl Pts',(0.319314254390294,2.14429285465081,12.4146594647908));
#70261=CARTESIAN_POINT('Ctrl Pts',(0.318134051496545,2.15209757797293,12.41515738017));
#70262=CARTESIAN_POINT('Ctrl Pts',(0.316083220083332,2.16294849729848,12.415866381315));
#70263=CARTESIAN_POINT('Ctrl Pts',(0.315452306718204,2.16603753828827,12.4160701293096));
#70264=CARTESIAN_POINT('Ctrl Pts',(0.314203529985022,2.17172480232731,12.4164487607958));
#70265=CARTESIAN_POINT('Ctrl Pts',(0.313598489190092,2.174325584479,12.4166232754865));
#70266=CARTESIAN_POINT('Ctrl Pts',(0.306756826776055,2.20216251720299,12.4185055832604));
#70267=CARTESIAN_POINT('Ctrl Pts',(0.297520827934519,2.22656239461783,12.4202941964783));
#70268=CARTESIAN_POINT('Ctrl Pts',(0.280856943656299,2.2583628436451,12.422685579553));
#70269=CARTESIAN_POINT('Ctrl Pts',(0.275853463508499,2.2669260970625,12.4233348786647));
#70270=CARTESIAN_POINT('Ctrl Pts',(0.269687353918092,2.27644245420543,12.4240515384591));
#70271=CARTESIAN_POINT('Ctrl Pts',(0.268904090720959,2.27763388945186,12.4241411693506));
#70272=CARTESIAN_POINT('Ctrl Pts',(0.267883604151819,2.27916395023983,12.4242561125363));
#70273=CARTESIAN_POINT('Ctrl Pts',(0.267653616433828,2.27950734818761,12.4242818990967));
#70274=CARTESIAN_POINT('Ctrl Pts',(0.267285771109931,2.28005430465777,12.4243229531554));
#70275=CARTESIAN_POINT('Ctrl Pts',(0.267148341053489,2.28025814804597,12.4243382494152));
#70276=CARTESIAN_POINT('Ctrl Pts',(0.266887984701972,2.28064337036095,12.4243671482616));
#70277=CARTESIAN_POINT('Ctrl Pts',(0.266765107700984,2.28082477968251,12.4243807539548));
#70278=CARTESIAN_POINT('Ctrl Pts',(0.266484355178158,2.28123835934159,12.4244117648929));
#70279=CARTESIAN_POINT('Ctrl Pts',(0.266326361474266,2.28147044838448,12.4244291619537));
#70280=CARTESIAN_POINT('Ctrl Pts',(0.265842567170203,2.28217913820726,12.4244822688146));
#70281=CARTESIAN_POINT('Ctrl Pts',(0.265515786782654,2.28265507356483,12.4245179123544));
#70282=CARTESIAN_POINT('Ctrl Pts',(0.263121545848907,2.28612213439397,12.4247774291381));
#70283=CARTESIAN_POINT('Ctrl Pts',(0.26100477081154,2.28907910811186,12.4249980201438));
#70284=CARTESIAN_POINT('Ctrl Pts',(0.258387304435151,2.29260776094619,12.4252611832714));
#70285=CARTESIAN_POINT('Ctrl Pts',(0.257934167847442,2.29321416549574,12.4253064055224));
#70286=CARTESIAN_POINT('Ctrl Pts',(0.256841326563231,2.29466595094714,12.4254146798273));
#70287=CARTESIAN_POINT('Ctrl Pts',(0.256199575322627,2.29550978785943,12.4254776200604));
#70288=CARTESIAN_POINT('Ctrl Pts',(0.25193034593304,2.30106626708438,12.4258922248953));
#70289=CARTESIAN_POINT('Ctrl Pts',(0.248176986926294,2.30568114588776,12.4262373323093));
#70290=CARTESIAN_POINT('Ctrl Pts',(0.228096784542626,2.32901982369845,12.4280018623011));
#70291=CARTESIAN_POINT('Ctrl Pts',(0.209772779032673,2.34591404382063,12.4293520112015));
#70292=CARTESIAN_POINT('Ctrl Pts',(0.179163493103398,2.36819981070686,12.4315177064403));
#70293=CARTESIAN_POINT('Ctrl Pts',(0.16818420651584,2.37521756383352,12.4322784507776));
#70294=CARTESIAN_POINT('Ctrl Pts',(0.155533648611095,2.3822633507784,12.4331531151963));
#70295=CARTESIAN_POINT('Ctrl Pts',(0.154250986585684,2.3829663373471,12.4332417693122));
#70296=CARTESIAN_POINT('Ctrl Pts',(0.151986839859772,2.38418727561975,12.4333982311474));
#70297=CARTESIAN_POINT('Ctrl Pts',(0.151007375843766,2.38470893822862,12.433465906373));
#70298=CARTESIAN_POINT('Ctrl Pts',(0.149567892297635,2.3854660895134,12.4335653592122));
#70299=CARTESIAN_POINT('Ctrl Pts',(0.149109962217914,2.38570555092768,12.4335969962124));
#70300=CARTESIAN_POINT('Ctrl Pts',(0.148299451261063,2.38612690502402,12.4336529909271));
#70301=CARTESIAN_POINT('Ctrl Pts',(0.147947105894386,2.38630925042366,12.4336773326093));
#70302=CARTESIAN_POINT('Ctrl Pts',(0.147263214897355,2.38666157743863,12.4337245787531));
#70303=CARTESIAN_POINT('Ctrl Pts',(0.146931709264649,2.38683163572428,12.4337474804682));
#70304=CARTESIAN_POINT('Ctrl Pts',(0.146140986824898,2.38723553602845,12.4338021067701));
#70305=CARTESIAN_POINT('Ctrl Pts',(0.145681503638398,2.38746885166994,12.4338338497912));
#70306=CARTESIAN_POINT('Ctrl Pts',(0.14404301408909,2.38829590406254,12.4339470451726));
#70307=CARTESIAN_POINT('Ctrl Pts',(0.142860933910683,2.38888349154305,12.4340287125573));
#70308=CARTESIAN_POINT('Ctrl Pts',(0.121467994831725,2.39935406141144,12.435506871291));
#70309=CARTESIAN_POINT('Ctrl Pts',(0.100284913931503,2.40709914814937,12.4369799693657));
#70310=CARTESIAN_POINT('Ctrl Pts',(0.0642686757891546,2.41614106449588,
12.4394780027634));
#70311=CARTESIAN_POINT('Ctrl Pts',(0.0498386451562194,2.41873459418383,
12.4404754175767));
#70312=CARTESIAN_POINT('Ctrl Pts',(0.0257344860335249,2.42138945102289,
12.4421009157807));
#70313=CARTESIAN_POINT('Ctrl Pts',(0.0161435218139634,2.42201375994364,
12.4427369405762));
#70314=CARTESIAN_POINT('Ctrl Pts',(0.00282906180194584,2.42228393656158,
12.4435932200996));
#70315=CARTESIAN_POINT('Ctrl Pts',(-0.000881350041491249,2.42229515280251,
12.4438289619597));
#70316=CARTESIAN_POINT('Ctrl Pts',(-0.00512477297303729,2.42223469235417,
12.4440946478046));
#70317=CARTESIAN_POINT('Ctrl Pts',(-0.00565821059082051,2.42222576699766,
12.4441279760569));
#70318=CARTESIAN_POINT('Ctrl Pts',(-0.00646344937015723,2.42221029369236,
12.4441781763964));
#70319=CARTESIAN_POINT('Ctrl Pts',(-0.0067352651080267,2.42220472644626,
12.4441951031318));
#70320=CARTESIAN_POINT('Ctrl Pts',(-0.00722529520009168,2.42219406943175,
12.4442255843107));
#70321=CARTESIAN_POINT('Ctrl Pts',(-0.00744351088698507,2.42218910194841,
12.4442391455913));
#70322=CARTESIAN_POINT('Ctrl Pts',(-0.00788068927321197,2.42217870558857,
12.4442662898499));
#70323=CARTESIAN_POINT('Ctrl Pts',(-0.00809965051149217,2.42217327521137,
12.4442798726902));
#70324=CARTESIAN_POINT('Ctrl Pts',(-0.00872049049333367,2.42215724466279,
12.4443183506055));
#70325=CARTESIAN_POINT('Ctrl Pts',(-0.00912235698171078,2.42214611568422,
12.4443432159289));
#70326=CARTESIAN_POINT('Ctrl Pts',(-0.0108116168559985,2.42209617111383,
12.444447568782));
#70327=CARTESIAN_POINT('Ctrl Pts',(-0.0120988151790634,2.42205038939176,
12.4445266709184));
#70328=CARTESIAN_POINT('Ctrl Pts',(-0.0474013440095872,2.42058282829831,
12.4466856093803));
#70329=CARTESIAN_POINT('Ctrl Pts',(-0.0809846619981988,2.41378766304625,
12.44848943791));
#70330=CARTESIAN_POINT('Ctrl Pts',(-0.127482796154434,2.39639866997596,
12.4513176779318));
#70331=CARTESIAN_POINT('Ctrl Pts',(-0.141662297018011,2.3898891624813,12.4522269437802));
#70332=CARTESIAN_POINT('Ctrl Pts',(-0.1563812978573,2.38179344990619,12.4532479760744));
#70333=CARTESIAN_POINT('Ctrl Pts',(-0.157445022938027,2.38120050394322,
12.4533222100742));
#70334=CARTESIAN_POINT('Ctrl Pts',(-0.158974443454908,2.38033656952996,
12.4534295970661));
#70335=CARTESIAN_POINT('Ctrl Pts',(-0.159442869042054,2.38007041506324,
12.4534625761404));
#70336=CARTESIAN_POINT('Ctrl Pts',(-0.160256707656882,2.37960529711032,
12.4535200296141));
#70337=CARTESIAN_POINT('Ctrl Pts',(-0.160602424012035,2.37940686448318,
12.4535444848135));
#70338=CARTESIAN_POINT('Ctrl Pts',(-0.161267933323786,2.37902323536221,
12.4535916566088));
#70339=CARTESIAN_POINT('Ctrl Pts',(-0.161587777828325,2.37883812910945,
12.4536143699117));
#70340=CARTESIAN_POINT('Ctrl Pts',(-0.16234280753026,2.37839942917438,12.4536680881339));
#70341=CARTESIAN_POINT('Ctrl Pts',(-0.162777717038571,2.37814536514661,
12.4536991100868));
#70342=CARTESIAN_POINT('Ctrl Pts',(-0.164291227818846,2.37725644179421,
12.4538073466104));
#70343=CARTESIAN_POINT('Ctrl Pts',(-0.165366714517951,2.37661632582565,
12.4538847523012));
#70344=CARTESIAN_POINT('Ctrl Pts',(-0.17957028612797,2.36805010313999,12.454913658068));
#70345=CARTESIAN_POINT('Ctrl Pts',(-0.192118073453158,2.35920429458674,
12.4558995252219));
#70346=CARTESIAN_POINT('Ctrl Pts',(-0.210222168886031,2.34440269060158,
12.4574447221865));
#70347=CARTESIAN_POINT('Ctrl Pts',(-0.216263545757921,2.33907342557645,
12.4579835424306));
#70348=CARTESIAN_POINT('Ctrl Pts',(-0.232464329613483,2.32366525524817,
12.4594895489275));
#70349=CARTESIAN_POINT('Ctrl Pts',(-0.24216199824409,2.31312761351484,12.4604635350252));
#70350=CARTESIAN_POINT('Ctrl Pts',(-0.25652972839462,2.29526385244901,12.4619983563205));
#70351=CARTESIAN_POINT('Ctrl Pts',(-0.261660735238953,2.28833256860578,
12.4625687258165));
#70352=CARTESIAN_POINT('Ctrl Pts',(-0.268871331443674,2.2777274604184,12.4633959688205));
#70353=CARTESIAN_POINT('Ctrl Pts',(-0.271166588380249,2.27420542075281,
12.4636636256317));
#70354=CARTESIAN_POINT('Ctrl Pts',(-0.273683143250254,2.27017348271022,
12.4639612377251));
#70355=CARTESIAN_POINT('Ctrl Pts',(-0.273972685238909,2.26970693819236,
12.4639955439658));
#70356=CARTESIAN_POINT('Ctrl Pts',(-0.274405487414254,2.26900556134797,
12.4640469188337));
#70357=CARTESIAN_POINT('Ctrl Pts',(-0.274549639733619,2.26877128491865,
12.464064045998));
#70358=CARTESIAN_POINT('Ctrl Pts',(-0.274796962691122,2.26836818009139,
12.4640934581181));
#70359=CARTESIAN_POINT('Ctrl Pts',(-0.274900277739513,2.26819944135198,
12.464105752655));
#70360=CARTESIAN_POINT('Ctrl Pts',(-0.275114099773814,2.26784949442321,
12.4641312143249));
#70361=CARTESIAN_POINT('Ctrl Pts',(-0.275224582832695,2.26766827272239,
12.464144379862));
#70362=CARTESIAN_POINT('Ctrl Pts',(-0.275493425890947,2.26722631663603,
12.464176439271));
#70363=CARTESIAN_POINT('Ctrl Pts',(-0.275651595241697,2.26696546567262,
12.4641953205501));
#70364=CARTESIAN_POINT('Ctrl Pts',(-0.276248721310408,2.2659775313998,12.4642666778783));
#70365=CARTESIAN_POINT('Ctrl Pts',(-0.276685178694181,2.26524893005533,
12.4643189913582));
#70366=CARTESIAN_POINT('Ctrl Pts',(-0.277326375818384,2.26416888349929,
12.46439609048));
#70367=CARTESIAN_POINT('Ctrl Pts',(-0.277533334290376,2.26381876997368,
12.4644210140226));
#70368=CARTESIAN_POINT('Ctrl Pts',(-0.287911081162565,2.24618653040182,
12.4656727666616));
#70369=CARTESIAN_POINT('Ctrl Pts',(-0.296449117321679,2.22799014405869,
12.4668002106639));
#70370=CARTESIAN_POINT('Ctrl Pts',(-0.308742711882082,2.19382523907905,
12.4688318487209));
#70371=CARTESIAN_POINT('Ctrl Pts',(-0.313080142218739,2.17814110839469,
12.4697349549351));
#70372=CARTESIAN_POINT('Ctrl Pts',(-0.3177109498993,2.15459778634299,12.4711115750337));
#70373=CARTESIAN_POINT('Ctrl Pts',(-0.318931222069622,2.14694708804417,
12.4715618464812));
#70374=CARTESIAN_POINT('Ctrl Pts',(-0.32062113402107,2.13317844708526,12.4723829927829));
#70375=CARTESIAN_POINT('Ctrl Pts',(-0.321193947693445,2.12707695039786,
12.4727506203706));
#70376=CARTESIAN_POINT('Ctrl Pts',(-0.321653404840576,2.1200284811212,12.4731808344414));
#70377=CARTESIAN_POINT('Ctrl Pts',(-0.321710254790034,2.11909358100029,
12.4732380085269));
#70378=CARTESIAN_POINT('Ctrl Pts',(-0.321790298535224,2.11767522689382,
12.4733249211477));
#70379=CARTESIAN_POINT('Ctrl Pts',(-0.321816480367335,2.11719194104954,
12.473354565906));
#70380=CARTESIAN_POINT('Ctrl Pts',(-0.321859929762684,2.11635501745125,
12.4734059560992));
#70381=CARTESIAN_POINT('Ctrl Pts',(-0.321877703470191,2.11600140587012,
12.4734276856215));
#70382=CARTESIAN_POINT('Ctrl Pts',(-0.32191336901801,2.11526771921309,12.4734728053105));
#70383=CARTESIAN_POINT('Ctrl Pts',(-0.321931170534929,2.11488764046356,
12.473496198276));
#70384=CARTESIAN_POINT('Ctrl Pts',(-0.32197788218834,2.11385102465628,12.4735600523362));
#70385=CARTESIAN_POINT('Ctrl Pts',(-0.322005457186875,2.11319443193811,
12.4736005552258));
#70386=CARTESIAN_POINT('Ctrl Pts',(-0.322102306447256,2.11070686971297,
12.4737542258757));
#70387=CARTESIAN_POINT('Ctrl Pts',(-0.322157972662154,2.10887543267303,
12.4738678191804));
#70388=CARTESIAN_POINT('Ctrl Pts',(-0.322250105177716,2.10466101085775,
12.4741302974112));
#70389=CARTESIAN_POINT('Ctrl Pts',(-0.322275760642569,2.102277920165,12.4742795147116));
#70390=CARTESIAN_POINT('Ctrl Pts',(-0.322272588014354,2.09255738744876,
12.4748915139082));
#70391=CARTESIAN_POINT('Ctrl Pts',(-0.322019612823381,2.08522269994397,
12.4753611513157));
#70392=CARTESIAN_POINT('Ctrl Pts',(-0.320506614220196,2.06320773342047,
12.4767947033937));
#70393=CARTESIAN_POINT('Ctrl Pts',(-0.318490374713577,2.04859998618421,
12.4777789870123));
#70394=CARTESIAN_POINT('Ctrl Pts',(-0.310549414108851,2.01053650966025,
12.4804044773017));
#70395=CARTESIAN_POINT('Ctrl Pts',(-0.302973007981674,1.98751789815905,
12.482058470587));
#70396=CARTESIAN_POINT('Ctrl Pts',(-0.29232510396039,1.96431996066291,12.4836708894387));
#70397=CARTESIAN_POINT('Ctrl Pts',(-0.291747697791952,1.96308279702549,
12.4837566894748));
#70398=CARTESIAN_POINT('Ctrl Pts',(-0.290986111659057,1.96147769986851,
12.4838677206556));
#70399=CARTESIAN_POINT('Ctrl Pts',(-0.290809075726345,1.9611064209841,12.4838933835442));
#70400=CARTESIAN_POINT('Ctrl Pts',(-0.290535868898998,1.96053626526242,
12.483932760908));
#70401=CARTESIAN_POINT('Ctrl Pts',(-0.290440204363937,1.9603371484124,12.48394650676));
#70402=CARTESIAN_POINT('Ctrl Pts',(-0.290249699192893,1.95994167181169,
12.4839737959681));
#70403=CARTESIAN_POINT('Ctrl Pts',(-0.290154864605045,1.9597453112263,12.4839873395014));
#70404=CARTESIAN_POINT('Ctrl Pts',(-0.289942778553595,1.95930731033082,
12.4840175363373));
#70405=CARTESIAN_POINT('Ctrl Pts',(-0.28982542458291,1.95906572088977,12.4840341830917));
#70406=CARTESIAN_POINT('Ctrl Pts',(-0.289480976403368,1.95835887617515,
12.4840828627687));
#70407=CARTESIAN_POINT('Ctrl Pts',(-0.289253061579566,1.95789401830503,
12.4841148446016));
#70408=CARTESIAN_POINT('Ctrl Pts',(-0.28757092281332,1.95448392135822,12.4843492324344));
#70409=CARTESIAN_POINT('Ctrl Pts',(-0.286072800309766,1.95156038351303,
12.4845489484519));
#70410=CARTESIAN_POINT('Ctrl Pts',(-0.281023014289846,1.94206641177733,
12.4851951260007));
#70411=CARTESIAN_POINT('Ctrl Pts',(-0.27728743727569,1.93559608590047,12.4856317303332));
#70412=CARTESIAN_POINT('Ctrl Pts',(-0.257917537601212,1.90458749576234,
12.4877340052729));
#70413=CARTESIAN_POINT('Ctrl Pts',(-0.23923518474163,1.88211421053499,12.4893014981543));
#70414=CARTESIAN_POINT('Ctrl Pts',(-0.215548211091604,1.86039743443793,
12.4911629641946));
#70415=CARTESIAN_POINT('Ctrl Pts',(-0.213278095052337,1.85837451681975,
12.4913401231548));
#70416=CARTESIAN_POINT('Ctrl Pts',(-0.209697335171616,1.85527345614903,
12.4916179490723));
#70417=CARTESIAN_POINT('Ctrl Pts',(-0.20840619553882,1.85417300563637,12.49171780746));
#70418=CARTESIAN_POINT('Ctrl Pts',(-0.2022109058474,1.84897658962971,12.4921955868076));
#70419=CARTESIAN_POINT('Ctrl Pts',(-0.197194617326637,1.84501710396387,
12.4925784246921));
#70420=CARTESIAN_POINT('Ctrl Pts',(-0.191238848552106,1.84059696439787,
12.4930298452525));
#70421=CARTESIAN_POINT('Ctrl Pts',(-0.190410565186254,1.83998836814056,
12.4930925563702));
#70422=CARTESIAN_POINT('Ctrl Pts',(-0.18917292871917,1.83908807750596,12.4931861638291));
#70423=CARTESIAN_POINT('Ctrl Pts',(-0.188765776049483,1.83879335757367,
12.4932169429586));
#70424=CARTESIAN_POINT('Ctrl Pts',(-0.188038840907404,1.83826974843146,
12.493271869594));
#70425=CARTESIAN_POINT('Ctrl Pts',(-0.18771932511294,1.83804048928718,12.4932960027674));
#70426=CARTESIAN_POINT('Ctrl Pts',(-0.187045268803415,1.83755870654412,
12.493346895634));
#70427=CARTESIAN_POINT('Ctrl Pts',(-0.186690634956594,1.83730631543739,
12.4933736603556));
#70428=CARTESIAN_POINT('Ctrl Pts',(-0.185753512225661,1.83664222602965,
12.493444358069));
#70429=CARTESIAN_POINT('Ctrl Pts',(-0.185170168366749,1.83623174347784,
12.493488337532));
#70430=CARTESIAN_POINT('Ctrl Pts',(-0.182531788014225,1.83438825576535,
12.4936871257023));
#70431=CARTESIAN_POINT('Ctrl Pts',(-0.180461491239928,1.83297733818936,
12.4938427728026));
#70432=CARTESIAN_POINT('Ctrl Pts',(-0.165018972382683,1.82271480386809,
12.4950015449702));
#70433=CARTESIAN_POINT('Ctrl Pts',(-0.151021187884627,1.81484950793117,
12.4960414711917));
#70434=CARTESIAN_POINT('Ctrl Pts',(-0.107832039307155,1.79465623858834,
12.4992131805885));
#70435=CARTESIAN_POINT('Ctrl Pts',(-0.0773498936013661,1.78554885740935,
12.501420192557));
#70436=CARTESIAN_POINT('Ctrl Pts',(-0.0445359051621924,1.78081352133288,
12.5035172823646));
#70437=CARTESIAN_POINT('Ctrl Pts',(-0.0430400883240043,1.78060838141668,
12.5036122444036));
#70438=CARTESIAN_POINT('Ctrl Pts',(-0.0411187908275544,1.78035863294732,
12.5037333583808));
#70439=CARTESIAN_POINT('Ctrl Pts',(-0.0406946186598991,1.78030435331775,
12.5037600434783));
#70440=CARTESIAN_POINT('Ctrl Pts',(-0.0400232456041312,1.78021979820696,
12.5038021939301));
#70441=CARTESIAN_POINT('Ctrl Pts',(-0.0397761174110584,1.78018896496181,
12.503817690753));
#70442=CARTESIAN_POINT('Ctrl Pts',(-0.0393337274287649,1.78013429035512,
12.5038453985808));
#70443=CARTESIAN_POINT('Ctrl Pts',(-0.0391384809514146,1.78011034147818,
12.5038576156164));
#70444=CARTESIAN_POINT('Ctrl Pts',(-0.0386800185379905,1.78005453263466,
12.5038862754056));
#70445=CARTESIAN_POINT('Ctrl Pts',(-0.0384167855298611,1.78002281876282,
12.5039027097675));
#70446=CARTESIAN_POINT('Ctrl Pts',(-0.0376556488705497,1.77993207107737,
12.5039501694607));
#70447=CARTESIAN_POINT('Ctrl Pts',(-0.0371576433711127,1.77987387397494,
12.5039811475399));
#70448=CARTESIAN_POINT('Ctrl Pts',(-0.0337708295416636,1.77948609936018,
12.5041913284462));
#70449=CARTESIAN_POINT('Ctrl Pts',(-0.0308776933712805,1.77919445312149,
12.504368432567));
#70450=CARTESIAN_POINT('Ctrl Pts',(-0.0217855722827214,1.77840205550125,
12.5049184716612));
#70451=CARTESIAN_POINT('Ctrl Pts',(-0.0155754981362823,1.77804151907465,
12.5052846503156));
#70452=CARTESIAN_POINT('Ctrl Pts',(0.0169904565885914,1.77709544396082,
12.5071730700716));
#70453=CARTESIAN_POINT('Ctrl Pts',(0.0433350658331552,1.7795654342851,12.5085995186846));
#70454=CARTESIAN_POINT('Ctrl Pts',(0.0838704389529214,1.78846183768363,
12.5109665164185));
#70455=CARTESIAN_POINT('Ctrl Pts',(0.0984057645377988,1.79274361160915,
12.5118504846997));
#70456=CARTESIAN_POINT('Ctrl Pts',(0.113755591282043,1.79846658377027,12.5128458100211));
#70457=CARTESIAN_POINT('Ctrl Pts',(0.114923346683233,1.79890971458748,12.512921920378));
#70458=CARTESIAN_POINT('Ctrl Pts',(0.116557941491595,1.79954089271375,12.513029015853));
#70459=CARTESIAN_POINT('Ctrl Pts',(0.117026971643791,1.79972326633693,12.5130598105164));
#70460=CARTESIAN_POINT('Ctrl Pts',(0.117839577180716,1.80004142593268,12.5131132760572));
#70461=CARTESIAN_POINT('Ctrl Pts',(0.118183350748654,1.80017670585726,12.5131359298806));
#70462=CARTESIAN_POINT('Ctrl Pts',(0.118897642899031,1.800459209627,12.5131830734801));
#70463=CARTESIAN_POINT('Ctrl Pts',(0.119268122250218,1.80060653047051,12.513207566495));
#70464=CARTESIAN_POINT('Ctrl Pts',(0.120139016006041,1.80095471376566,12.5132652402384));
#70465=CARTESIAN_POINT('Ctrl Pts',(0.120639200407508,1.80115614494308,12.5132984401233));
#70466=CARTESIAN_POINT('Ctrl Pts',(0.122269762457786,1.80181755559609,12.5134069184662));
#70467=CARTESIAN_POINT('Ctrl Pts',(0.123398022950824,1.802282696458,12.5134823713874));
#70468=CARTESIAN_POINT('Ctrl Pts',(0.139122213805027,1.80886994874965,12.5145394876793));
#70469=CARTESIAN_POINT('Ctrl Pts',(0.153248120056147,1.81605181165994,12.5155578531953));
#70470=CARTESIAN_POINT('Ctrl Pts',(0.195608380800261,1.84167263456954,12.5188332354438));
#70471=CARTESIAN_POINT('Ctrl Pts',(0.221515521738057,1.86351246144548,12.5211921398196));
#70472=CARTESIAN_POINT('Ctrl Pts',(0.244478348197526,1.89001562271875,12.5234078054523));
#70473=CARTESIAN_POINT('Ctrl Pts',(0.245380306598264,1.89107033064131,12.5234950313591));
#70474=CARTESIAN_POINT('Ctrl Pts',(0.246542445553757,1.89244718859257,12.523607638196));
#70475=CARTESIAN_POINT('Ctrl Pts',(0.246808840083189,1.89276403921107,12.5236334659714));
#70476=CARTESIAN_POINT('Ctrl Pts',(0.247216798546808,1.89325116886778,12.5236730409425));
#70477=CARTESIAN_POINT('Ctrl Pts',(0.247358797446731,1.89342108049301,12.5236868200156));
#70478=CARTESIAN_POINT('Ctrl Pts',(0.247640256400486,1.8937585721378,12.5237141397824));
#70479=CARTESIAN_POINT('Ctrl Pts',(0.247779720649175,1.89392614626721,12.5237276807231));
#70480=CARTESIAN_POINT('Ctrl Pts',(0.248086610765351,1.89429565393181,12.5237574860971));
#70481=CARTESIAN_POINT('Ctrl Pts',(0.248253959712069,1.8944976498411,12.5237737448548));
#70482=CARTESIAN_POINT('Ctrl Pts',(0.248736610432294,1.89508167574258,12.5238206539857));
#70483=CARTESIAN_POINT('Ctrl Pts',(0.249051280068474,1.89546423078148,12.5238512582981));
#70484=CARTESIAN_POINT('Ctrl Pts',(0.249760305009823,1.89633027976183,12.5239202694135));
#70485=CARTESIAN_POINT('Ctrl Pts',(0.250154142129212,1.89681419810651,12.5239586394138));
#70486=CARTESIAN_POINT('Ctrl Pts',(0.259951482425394,1.90892411975307,12.5249141670821));
#70487=CARTESIAN_POINT('Ctrl Pts',(0.2685373642032,1.92119122246392,12.5257752203212));
#70488=CARTESIAN_POINT('Ctrl Pts',(0.286771581773594,1.95153702817107,12.5277755318574));
#70489=CARTESIAN_POINT('Ctrl Pts',(0.295610331285801,1.97002409067696,12.5288986484699));
#70490=CARTESIAN_POINT('Ctrl Pts',(0.304681252318336,1.99480570790901,12.5304064257487));
#70491=CARTESIAN_POINT('Ctrl Pts',(0.306569439002036,2.0004425868955,12.5307492604118));
#70492=CARTESIAN_POINT('Ctrl Pts',(0.30907939362852,2.00868596798165,12.5312526852586));
#70493=CARTESIAN_POINT('Ctrl Pts',(0.309826294017514,2.01125321990143,12.5314097484109));
#70494=CARTESIAN_POINT('Ctrl Pts',(0.311026461653203,2.01557837856498,12.531675024557));
#70495=CARTESIAN_POINT('Ctrl Pts',(0.311496981370765,2.01733138188119,12.5317827236437));
#70496=CARTESIAN_POINT('Ctrl Pts',(0.31211902812725,2.01972966297947,12.5319303582435));
#70497=CARTESIAN_POINT('Ctrl Pts',(0.312283415266841,2.02037159260504,12.5319699028552));
#70498=CARTESIAN_POINT('Ctrl Pts',(0.312687317745546,2.02196931467299,12.532068401063));
#70499=CARTESIAN_POINT('Ctrl Pts',(0.312924430494483,2.02292570273174,12.53212742749));
#70500=CARTESIAN_POINT('Ctrl Pts',(0.313311850969022,2.02451961394665,12.5322259178452));
#70501=CARTESIAN_POINT('Ctrl Pts',(0.31346460882439,2.02515653908674,12.5322653055569));
#70502=CARTESIAN_POINT('Ctrl Pts',(0.314230002975547,2.02839130660131,12.5324655089636));
#70503=CARTESIAN_POINT('Ctrl Pts',(0.314812276794845,2.03099616343875,12.5326272641653));
#70504=CARTESIAN_POINT('Ctrl Pts',(0.315517522131463,2.03434607463527,12.5328360708784));
#70505=CARTESIAN_POINT('Ctrl Pts',(0.315670335529582,2.03508479423746,12.5328821654538));
#70506=CARTESIAN_POINT('Ctrl Pts',(0.315909927691416,2.03626386701522,12.5329558171436));
#70507=CARTESIAN_POINT('Ctrl Pts',(0.315998383270926,2.03670387982834,12.5329833206209));
#70508=CARTESIAN_POINT('Ctrl Pts',(0.316162222540064,2.03752778442171,12.5330348534106));
#70509=CARTESIAN_POINT('Ctrl Pts',(0.316237826996519,2.0379116318856,12.5330588756232));
#70510=CARTESIAN_POINT('Ctrl Pts',(0.316404903863116,2.03876811137085,12.5331125073754));
#70511=CARTESIAN_POINT('Ctrl Pts',(0.316496016451906,2.03924081188998,12.5331421283365));
#70512=CARTESIAN_POINT('Ctrl Pts',(0.316758963902753,2.04062164829004,12.5332287183438));
#70513=CARTESIAN_POINT('Ctrl Pts',(0.316927950576724,2.04153031572439,12.5332857780064));
#70514=CARTESIAN_POINT('Ctrl Pts',(0.318130666890541,2.04815593941973,12.5337024215269));
#70515=CARTESIAN_POINT('Ctrl Pts',(0.319013490500741,2.05389887619387,12.5340667758708));
#70516=CARTESIAN_POINT('Ctrl Pts',(0.321417845182028,2.07295719552124,12.5352876100207));
#70517=CARTESIAN_POINT('Ctrl Pts',(0.322264072884849,2.08634220741131,12.5361644796985));
#70518=CARTESIAN_POINT('Ctrl Pts',(0.322295136279694,2.12479830135188,12.5387298954818));
#70519=CARTESIAN_POINT('Ctrl Pts',(0.319392804474774,2.14977253846948,12.5404580627473));
#70520=CARTESIAN_POINT('Ctrl Pts',(0.313351201127258,2.1753235354817,12.5421762985306));
#70521=CARTESIAN_POINT('Ctrl Pts',(0.313069088619063,2.17648762038991,12.5422544499576));
#70522=CARTESIAN_POINT('Ctrl Pts',(0.312551633846643,2.17857196688452,12.5423941189368));
#70523=CARTESIAN_POINT('Ctrl Pts',(0.312318701699164,2.17949280728362,12.542455730133));
#70524=CARTESIAN_POINT('Ctrl Pts',(0.31203619846259,2.18058920354458,12.542528965958));
#70525=CARTESIAN_POINT('Ctrl Pts',(0.311990547680749,2.18076575411089,12.5425407552229));
#70526=CARTESIAN_POINT('Ctrl Pts',(0.310843341486386,2.18518699115654,12.5428358901318));
#70527=CARTESIAN_POINT('Ctrl Pts',(0.309655342330867,2.18940906056954,12.5431155233963));
#70528=CARTESIAN_POINT('Ctrl Pts',(0.308206622817147,2.19418182218119,12.5434280861989));
#70529=CARTESIAN_POINT('Ctrl Pts',(0.308030167174242,2.19475734326281,12.5434657173088));
#70530=CARTESIAN_POINT('Ctrl Pts',(0.307767256629074,2.19560634723978,12.5435211395322));
#70531=CARTESIAN_POINT('Ctrl Pts',(0.307682048803485,2.19588021032071,12.5435390030848));
#70532=CARTESIAN_POINT('Ctrl Pts',(0.307530671114432,2.19636446747756,12.5435705650232));
#70533=CARTESIAN_POINT('Ctrl Pts',(0.307464650791378,2.19657490762741,12.5435842722269));
#70534=CARTESIAN_POINT('Ctrl Pts',(0.30733706513423,2.19698013069461,12.5436106503663));
#70535=CARTESIAN_POINT('Ctrl Pts',(0.307275530863958,2.19717492211315,12.5436233230994));
#70536=CARTESIAN_POINT('Ctrl Pts',(0.307108982190797,2.19770040464002,12.5436574905935));
#70537=CARTESIAN_POINT('Ctrl Pts',(0.307003618512989,2.19803098607946,12.5436789647187));
#70538=CARTESIAN_POINT('Ctrl Pts',(0.306599086866941,2.19929316658817,12.5437608775598));
#70539=CARTESIAN_POINT('Ctrl Pts',(0.306296206770293,2.20022358392657,12.5438210999068));
#70540=CARTESIAN_POINT('Ctrl Pts',(0.305529788650055,2.20254201699488,12.5439707975406));
#70541=CARTESIAN_POINT('Ctrl Pts',(0.305061020356548,2.20392829760395,12.5440599793416));
#70542=CARTESIAN_POINT('Ctrl Pts',(0.301768859464088,2.21344992541272,12.5446705676976));
#70543=CARTESIAN_POINT('Ctrl Pts',(0.298629569041108,2.22147319784076,12.5451752501702));
#70544=CARTESIAN_POINT('Ctrl Pts',(0.288870577986393,2.24374086386009,12.5465732721839));
#70545=CARTESIAN_POINT('Ctrl Pts',(0.281526210377958,2.25764102310232,12.5474435574157));
#70546=CARTESIAN_POINT('Ctrl Pts',(0.267087037482708,2.28071632111964,12.5489670603575));
#70547=CARTESIAN_POINT('Ctrl Pts',(0.260457587520216,2.29014651796972,12.5496150563501));
#70548=CARTESIAN_POINT('Ctrl Pts',(0.251765092716363,2.30120136184224,12.5504240312249));
#70549=CARTESIAN_POINT('Ctrl Pts',(0.250168729705539,2.3031828146735,12.5505710660864));
#70550=CARTESIAN_POINT('Ctrl Pts',(0.247390069170748,2.30654937560533,12.5508246147971));
#70551=CARTESIAN_POINT('Ctrl Pts',(0.246219177550728,2.30794376000644,12.5509307555948));
#70552=CARTESIAN_POINT('Ctrl Pts',(0.243802889230984,2.31077223292768,12.5511484548271));
#70553=CARTESIAN_POINT('Ctrl Pts',(0.242556506964485,2.31220538093181,12.5512600450055));
#70554=CARTESIAN_POINT('Ctrl Pts',(0.23686326700206,2.31863603909449,12.5517668036554));
#70555=CARTESIAN_POINT('Ctrl Pts',(0.232274386633705,2.32350508788052,12.5521672594439));
#70556=CARTESIAN_POINT('Ctrl Pts',(0.226799831228138,2.32896309181853,12.5526377244686));
#70557=CARTESIAN_POINT('Ctrl Pts',(0.226058535982045,2.32969501328918,12.5527012796481));
#70558=CARTESIAN_POINT('Ctrl Pts',(0.224952359549989,2.33077666039275,12.5527959034412));
#70559=CARTESIAN_POINT('Ctrl Pts',(0.224590178257293,2.33112914760994,12.5528268510541));
#70560=CARTESIAN_POINT('Ctrl Pts',(0.223944462107621,2.33175462980146,12.5528819667986));
#70561=CARTESIAN_POINT('Ctrl Pts',(0.223661252829754,2.33202796065028,12.5529061202299));
#70562=CARTESIAN_POINT('Ctrl Pts',(0.223064855592406,2.33260144884772,12.5529569418838));
#70563=CARTESIAN_POINT('Ctrl Pts',(0.222751561103613,2.33290149383268,12.5529836149085));
#70564=CARTESIAN_POINT('Ctrl Pts',(0.221926300380556,2.3336886651656,12.5530538125088));
#70565=CARTESIAN_POINT('Ctrl Pts',(0.221413338110253,2.33417473971725,12.5530973823757));
#70566=CARTESIAN_POINT('Ctrl Pts',(0.219121155227616,2.33633250973028,12.5532917987959));
#70567=CARTESIAN_POINT('Ctrl Pts',(0.217324609313445,2.3379856077224,12.5534434391629));
#70568=CARTESIAN_POINT('Ctrl Pts',(0.204100285823825,2.34987939736561,12.5545545957836));
#70569=CARTESIAN_POINT('Ctrl Pts',(0.191974515974857,2.35931120804736,12.5555477092274));
#70570=CARTESIAN_POINT('Ctrl Pts',(0.161174796688992,2.3799205930671,12.5580077423645));
#70571=CARTESIAN_POINT('Ctrl Pts',(0.141951725903037,2.39014214856864,12.5594961841716));
#70572=CARTESIAN_POINT('Ctrl Pts',(0.118107681086719,2.39988009654711,12.561216351124));
#70573=CARTESIAN_POINT('Ctrl Pts',(0.114339119282427,2.4013371277777,12.561484536216));
#70574=CARTESIAN_POINT('Ctrl Pts',(0.109677219936091,2.40303949350571,12.5618110395627));
#70575=CARTESIAN_POINT('Ctrl Pts',(0.108809035160431,2.40335230524324,12.5618716223891));
#70576=CARTESIAN_POINT('Ctrl Pts',(0.107030891361815,2.40398436443888,12.5619952343106));
#70577=CARTESIAN_POINT('Ctrl Pts',(0.106120817352215,2.40430326599029,12.5620582503552));
#70578=CARTESIAN_POINT('Ctrl Pts',(0.099670602573884,2.40653104801812,12.5625030516906));
#70579=CARTESIAN_POINT('Ctrl Pts',(0.0940802971422607,2.40829275190804,
12.5628790374363));
#70580=CARTESIAN_POINT('Ctrl Pts',(0.0878102499072631,2.41008220017839,
12.5632878892984));
#70581=CARTESIAN_POINT('Ctrl Pts',(0.0871752983943934,2.41026130636021,
12.5633291473241));
#70582=CARTESIAN_POINT('Ctrl Pts',(0.0862826463464921,2.41051014770598,
12.5633869418814));
#70583=CARTESIAN_POINT('Ctrl Pts',(0.0860254078311277,2.41058151280734,
12.5634035724611));
#70584=CARTESIAN_POINT('Ctrl Pts',(0.0855535890755672,2.41071177727027,
12.5634340308768));
#70585=CARTESIAN_POINT('Ctrl Pts',(0.0853390360428728,2.41077077415099,
12.5634478644217));
#70586=CARTESIAN_POINT('Ctrl Pts',(0.0849272008447671,2.41088356018715,
12.5634743851206));
#70587=CARTESIAN_POINT('Ctrl Pts',(0.0847299287289757,2.41093738375452,
12.5634870743019));
#70588=CARTESIAN_POINT('Ctrl Pts',(0.0842249094404933,2.41107465651565,
12.5635195221701));
#70589=CARTESIAN_POINT('Ctrl Pts',(0.0839170884816694,2.4111578370529,12.5635392651269));
#70590=CARTESIAN_POINT('Ctrl Pts',(0.082851319705993,2.41144413654314,12.5636075025057));
#70591=CARTESIAN_POINT('Ctrl Pts',(0.0820927461135195,2.41164494610045,
12.5636558636874));
#70592=CARTESIAN_POINT('Ctrl Pts',(0.0802591323779252,2.41212318070828,
12.5637722776558));
#70593=CARTESIAN_POINT('Ctrl Pts',(0.0791833689253165,2.41239782718925,
12.5638401757661));
#70594=CARTESIAN_POINT('Ctrl Pts',(0.0752251546961129,2.41338661435927,
12.5640886045771));
#70595=CARTESIAN_POINT('Ctrl Pts',(0.0723341960332176,2.41406648886256,
12.5642673303035));
#70596=CARTESIAN_POINT('Ctrl Pts',(0.0621853187662264,2.41630565123588,
12.5648865874848));
#70597=CARTESIAN_POINT('Ctrl Pts',(0.054882883921114,2.41765415663696,12.5653176435627));
#70598=CARTESIAN_POINT('Ctrl Pts',(0.0374783709972437,2.42024995540952,
12.566324399971));
#70599=CARTESIAN_POINT('Ctrl Pts',(0.0273510080992763,2.42127340508745,
12.5668940777291));
#70600=CARTESIAN_POINT('Ctrl Pts',(-0.00550923410627159,2.42302884441702,
12.5687339862276));
#70601=CARTESIAN_POINT('Ctrl Pts',(-0.0282723807757971,2.42183618493003,
12.5700004848898));
#70602=CARTESIAN_POINT('Ctrl Pts',(-0.0511748427832104,2.41818630307005,
12.5713723674859));
#70603=CARTESIAN_POINT('Ctrl Pts',(-0.0516297786196632,2.4181128006728,
12.5713996559998));
#70604=CARTESIAN_POINT('Ctrl Pts',(-0.0577337106364597,2.41711317090707,
12.5717662983612));
#70605=CARTESIAN_POINT('Ctrl Pts',(-0.0633569213734242,2.41603771730515,
12.5721099455375));
#70606=CARTESIAN_POINT('Ctrl Pts',(-0.0699073248494511,2.41460309198936,
12.5725181873107));
#70607=CARTESIAN_POINT('Ctrl Pts',(-0.0708654195474081,2.4143886636566,
12.572578098328));
#70608=CARTESIAN_POINT('Ctrl Pts',(-0.0723100178329812,2.41405841340361,
12.5726687376621));
#70609=CARTESIAN_POINT('Ctrl Pts',(-0.072797262189937,2.41394583023476,
12.5726993618859));
#70610=CARTESIAN_POINT('Ctrl Pts',(-0.0736669036313325,2.41374275664988,
12.5727541154711));
#70611=CARTESIAN_POINT('Ctrl Pts',(-0.0740494017864178,2.41365269986691,
12.5727782308377));
#70612=CARTESIAN_POINT('Ctrl Pts',(-0.0748566167999468,2.4134610872894,
12.5728291931499));
#70613=CARTESIAN_POINT('Ctrl Pts',(-0.0752812935553688,2.41335936743781,
12.5728560453375));
#70614=CARTESIAN_POINT('Ctrl Pts',(-0.076405224164876,2.41308774356345,
12.5729272200487));
#70615=CARTESIAN_POINT('Ctrl Pts',(-0.0771041150161828,2.41291636084341,
12.57297159018));
#70616=CARTESIAN_POINT('Ctrl Pts',(-0.0802942833983428,2.41212272801736,
12.5731746385882));
#70617=CARTESIAN_POINT('Ctrl Pts',(-0.0827785871249266,2.41147307137411,
12.5733341999556));
#70618=CARTESIAN_POINT('Ctrl Pts',(-0.0935514061977446,2.40851794626102,
12.5740325704462));
#70619=CARTESIAN_POINT('Ctrl Pts',(-0.10175284566134,2.40591097504596,12.5745810923826));
#70620=CARTESIAN_POINT('Ctrl Pts',(-0.122889517641475,2.39824826011225,
12.5760401993752));
#70621=CARTESIAN_POINT('Ctrl Pts',(-0.135618859755706,2.39267954081438,
12.5769654559846));
#70622=CARTESIAN_POINT('Ctrl Pts',(-0.158782211372128,2.38070998396296,
12.578723633248));
#70623=CARTESIAN_POINT('Ctrl Pts',(-0.169289414434756,2.37450133157515,
12.5795525465214));
#70624=CARTESIAN_POINT('Ctrl Pts',(-0.19087785500478,2.3600328555652,12.5812981886102));
#70625=CARTESIAN_POINT('Ctrl Pts',(-0.201832975126465,2.35162470648952,
12.5822104505904));
#70626=CARTESIAN_POINT('Ctrl Pts',(-0.21281207685205,2.34201822559049,12.5831267402155));
#70627=CARTESIAN_POINT('Ctrl Pts',(-0.21340558480918,2.34149504751771,12.5831762779815));
#70628=CARTESIAN_POINT('Ctrl Pts',(-0.214218750776272,2.34077290184463,
12.5832441492252));
#70629=CARTESIAN_POINT('Ctrl Pts',(-0.214440063643184,2.34057581456429,
12.5832626211453));
#70630=CARTESIAN_POINT('Ctrl Pts',(-0.214817632419047,2.34023864066017,
12.5832941344178));
#70631=CARTESIAN_POINT('Ctrl Pts',(-0.214974023376015,2.34009870665723,
12.5833071872103));
#70632=CARTESIAN_POINT('Ctrl Pts',(-0.215278260317774,2.33982594888752,
12.5833325790823));
#70633=CARTESIAN_POINT('Ctrl Pts',(-0.215426119663416,2.33969314152092,
12.5833449192772));
#70634=CARTESIAN_POINT('Ctrl Pts',(-0.215732283546537,2.33941763277691,
12.5833704710243));
#70635=CARTESIAN_POINT('Ctrl Pts',(-0.215890569674052,2.33927491087689,
12.5833836810221));
#70636=CARTESIAN_POINT('Ctrl Pts',(-0.216252264258994,2.33894813052187,
12.5834138666154));
#70637=CARTESIAN_POINT('Ctrl Pts',(-0.216455579871819,2.3387639688494,12.5834308344189));
#70638=CARTESIAN_POINT('Ctrl Pts',(-0.217413090824135,2.33789443479493,
12.5835107448448));
#70639=CARTESIAN_POINT('Ctrl Pts',(-0.218164278656408,2.33720573718186,
12.5835734388705));
#70640=CARTESIAN_POINT('Ctrl Pts',(-0.226158458695229,2.32980648217156,
12.5842408226513));
#70641=CARTESIAN_POINT('Ctrl Pts',(-0.23309348577565,2.32276924779686,12.5848215108042));
#70642=CARTESIAN_POINT('Ctrl Pts',(-0.244154189606144,2.31046236658406,
12.5857735413746));
#70643=CARTESIAN_POINT('Ctrl Pts',(-0.248458356167264,2.30536340435532,
12.5861514178989));
#70644=CARTESIAN_POINT('Ctrl Pts',(-0.268042511844972,2.28064509320284,
12.5879256410042));
#70645=CARTESIAN_POINT('Ctrl Pts',(-0.281175425585426,2.25943577612085,
12.5892903841016));
#70646=CARTESIAN_POINT('Ctrl Pts',(-0.292647276310875,2.23499374692047,
12.5908691814638));
#70647=CARTESIAN_POINT('Ctrl Pts',(-0.293535738939955,2.2330507787122,12.5909946621733));
#70648=CARTESIAN_POINT('Ctrl Pts',(-0.297108989117396,2.22502645504214,
12.5915130422179));
#70649=CARTESIAN_POINT('Ctrl Pts',(-0.299624472669125,2.21887191249012,
12.5919110373481));
#70650=CARTESIAN_POINT('Ctrl Pts',(-0.302311188028485,2.21167006079562,
12.5923788427164));
#70651=CARTESIAN_POINT('Ctrl Pts',(-0.302669919903463,2.21069406682922,
12.5924422820164));
#70652=CARTESIAN_POINT('Ctrl Pts',(-0.303195848223308,2.2092415135678,12.5925367663454));
#70653=CARTESIAN_POINT('Ctrl Pts',(-0.303366660452299,2.20876626309599,
12.5925676908974));
#70654=CARTESIAN_POINT('Ctrl Pts',(-0.303668594193689,2.20791994906532,
12.5926227807048));
#70655=CARTESIAN_POINT('Ctrl Pts',(-0.303800154712069,2.20754904230431,
12.5926469313103));
#70656=CARTESIAN_POINT('Ctrl Pts',(-0.304075368333923,2.20676860190148,
12.5926977624537));
#70657=CARTESIAN_POINT('Ctrl Pts',(-0.304218874131501,2.20635901747682,
12.5927244478244));
#70658=CARTESIAN_POINT('Ctrl Pts',(-0.304594169369989,2.205280901745,12.5927947127654));
#70659=CARTESIAN_POINT('Ctrl Pts',(-0.304824584268628,2.20461189750278,
12.5928383377853));
#70660=CARTESIAN_POINT('Ctrl Pts',(-0.305842942400099,2.20162318686394,
12.5930333373239));
#70661=CARTESIAN_POINT('Ctrl Pts',(-0.306606605860521,2.19929534850143,
12.5931855115272));
#70662=CARTESIAN_POINT('Ctrl Pts',(-0.31198753761293,2.18223871864703,12.5943029182228));
#70663=CARTESIAN_POINT('Ctrl Pts',(-0.315567205317863,2.16720598797477,
12.5953021588895));
#70664=CARTESIAN_POINT('Ctrl Pts',(-0.320877649168001,2.13471020012158,
12.5974885280355));
#70665=CARTESIAN_POINT('Ctrl Pts',(-0.322288399277859,2.11724389580947,
12.5986797078545));
#70666=CARTESIAN_POINT('Ctrl Pts',(-0.322274904093275,2.09975137041567,
12.5998588653417));
#70667=CARTESIAN_POINT('',(-0.322274978515416,2.10011767704999,12.8494474689269));
#70668=CARTESIAN_POINT('Ctrl Pts',(-0.322274903816576,2.09975101201496,
12.5998588895012));
#70669=CARTESIAN_POINT('Ctrl Pts',(-0.322263089948684,2.08445985996148,
12.6008896539382));
#70670=CARTESIAN_POINT('Ctrl Pts',(-0.321162988197009,2.06918639405889,
12.6019079146836));
#70671=CARTESIAN_POINT('Ctrl Pts',(-0.318876035729298,2.05331166160658,
12.6029184379496));
#70672=CARTESIAN_POINT('Ctrl Pts',(-0.318767604272797,2.05257699296849,
12.6029650937256));
#70673=CARTESIAN_POINT('Ctrl Pts',(-0.318596508128715,2.05144485063174,
12.6030368143299));
#70674=CARTESIAN_POINT('Ctrl Pts',(-0.318535637745597,2.05104711436359,
12.6030619769726));
#70675=CARTESIAN_POINT('Ctrl Pts',(-0.318433613039424,2.05038871754176,
12.6031035731591));
#70676=CARTESIAN_POINT('Ctrl Pts',(-0.318392883383902,2.0501279931007,12.6031200303807));
#70677=CARTESIAN_POINT('Ctrl Pts',(-0.31831918235261,2.04965997787716,12.6031495450491));
#70678=CARTESIAN_POINT('Ctrl Pts',(-0.318286328676651,2.04945266911989,
12.6031626091511));
#70679=CARTESIAN_POINT('Ctrl Pts',(-0.31822222128866,2.0490506881614,12.6031879223878));
#70680=CARTESIAN_POINT('Ctrl Pts',(-0.318190991489702,2.04885601272614,
12.6032001728416));
#70681=CARTESIAN_POINT('Ctrl Pts',(-0.318125370277947,2.04844934010768,
12.6032257459455));
#70682=CARTESIAN_POINT('Ctrl Pts',(-0.318090945709314,2.04823734929271,
12.6032390666384));
#70683=CARTESIAN_POINT('Ctrl Pts',(-0.318005651099943,2.04771539270985,
12.6032718399029));
#70684=CARTESIAN_POINT('Ctrl Pts',(-0.317954539621869,2.04740546580883,
12.6032912787028));
#70685=CARTESIAN_POINT('Ctrl Pts',(-0.317753532353024,2.04619761118911,
12.6033669548326));
#70686=CARTESIAN_POINT('Ctrl Pts',(-0.31760028344457,2.04530023430135,12.6034230034244));
#70687=CARTESIAN_POINT('Ctrl Pts',(-0.314820562302665,2.02942866395548,
12.6044114052215));
#70688=CARTESIAN_POINT('Ctrl Pts',(-0.311141145399845,2.01465585671774,
12.60528587343));
#70689=CARTESIAN_POINT('Ctrl Pts',(-0.305523008500156,1.99740625450415,
12.6063101881615));
#70690=CARTESIAN_POINT('Ctrl Pts',(-0.304576250783404,1.99462878409233,
12.6064752060964));
#70691=CARTESIAN_POINT('Ctrl Pts',(-0.302739288953132,1.98947148721287,
12.6067823777893));
#70692=CARTESIAN_POINT('Ctrl Pts',(-0.301858621322224,1.98708852108661,
12.6069246157394));
#70693=CARTESIAN_POINT('Ctrl Pts',(-0.299197908214657,1.98014269435755,
12.6073406961287));
#70694=CARTESIAN_POINT('Ctrl Pts',(-0.297341922818261,1.975609715328,12.6076141433382));
#70695=CARTESIAN_POINT('Ctrl Pts',(-0.29090313529031,1.96085240272916,12.6085150770348));
#70696=CARTESIAN_POINT('Ctrl Pts',(-0.285890698464738,1.95082500917218,
12.609144758323));
#70697=CARTESIAN_POINT('Ctrl Pts',(-0.274407483324548,1.93056640978541,
12.6104815452582));
#70698=CARTESIAN_POINT('Ctrl Pts',(-0.267862452458586,1.92039803803896,
12.6111898610645));
#70699=CARTESIAN_POINT('Ctrl Pts',(-0.259522059347485,1.90891380859753,
12.6120476855147));
#70700=CARTESIAN_POINT('Ctrl Pts',(-0.258264861637497,1.90721801757539,
12.6121759016919));
#70701=CARTESIAN_POINT('Ctrl Pts',(-0.256586948684576,1.90500061018871,
12.6123456576193));
#70702=CARTESIAN_POINT('Ctrl Pts',(-0.256181117958024,1.90446775444153,
12.6123866126842));
#70703=CARTESIAN_POINT('Ctrl Pts',(-0.255514725921791,1.90359841759433,
12.6124536963514));
#70704=CARTESIAN_POINT('Ctrl Pts',(-0.255255152647321,1.90326117877099,
12.6124797859045));
#70705=CARTESIAN_POINT('Ctrl Pts',(-0.25475271826226,1.90261108180813,12.6125302070032));
#70706=CARTESIAN_POINT('Ctrl Pts',(-0.254509946780996,1.90229815510655,
12.612554534968));
#70707=CARTESIAN_POINT('Ctrl Pts',(-0.253950709838055,1.90158004909039,
12.6126104958646));
#70708=CARTESIAN_POINT('Ctrl Pts',(-0.253633851026828,1.901175178726,12.612642144409));
#70709=CARTESIAN_POINT('Ctrl Pts',(-0.252787314251255,1.90009882233431,
12.6127265443052));
#70710=CARTESIAN_POINT('Ctrl Pts',(-0.252255932499933,1.89942868705994,
12.6127793636404));
#70711=CARTESIAN_POINT('Ctrl Pts',(-0.248622405225213,1.89488365894975,
12.6131394679851));
#70712=CARTESIAN_POINT('Ctrl Pts',(-0.245433909520306,1.89107894942784,
12.6134502206167));
#70713=CARTESIAN_POINT('Ctrl Pts',(-0.240900564676967,1.88591653340762,
12.6138852966044));
#70714=CARTESIAN_POINT('Ctrl Pts',(-0.239629494437767,1.88449473816552,
12.6140065816338));
#70715=CARTESIAN_POINT('Ctrl Pts',(-0.237930234181469,1.88262759910436,
12.614167810379));
#70716=CARTESIAN_POINT('Ctrl Pts',(-0.237513257609106,1.88217206455459,
12.6142073021062));
#70717=CARTESIAN_POINT('Ctrl Pts',(-0.220067104520433,1.86322231050974,
12.6158566430798));
#70718=CARTESIAN_POINT('Ctrl Pts',(-0.200935907445734,1.84678554624629,
12.6175575509816));
#70719=CARTESIAN_POINT('Ctrl Pts',(-0.170915124594642,1.82655583962047,
12.6200045802552));
#70720=CARTESIAN_POINT('Ctrl Pts',(-0.161422956593141,1.82084708936651,
12.6207492092464));
#70721=CARTESIAN_POINT('Ctrl Pts',(-0.147246866025745,1.81328673149349,
12.6218033245117));
#70722=CARTESIAN_POINT('Ctrl Pts',(-0.142784051359772,1.81103830947749,
12.6221272213385));
#70723=CARTESIAN_POINT('Ctrl Pts',(-0.136806920071566,1.8081992673277,12.6225489193075));
#70724=CARTESIAN_POINT('Ctrl Pts',(-0.135338081818067,1.80751512034525,
12.6226515976927));
#70725=CARTESIAN_POINT('Ctrl Pts',(-0.13290073873828,1.80640216133249,12.6228203363655));
#70726=CARTESIAN_POINT('Ctrl Pts',(-0.131935187071276,1.80596700233786,
12.6228867591986));
#70727=CARTESIAN_POINT('Ctrl Pts',(-0.130720128499522,1.80542658483338,
12.6229698002301));
#70728=CARTESIAN_POINT('Ctrl Pts',(-0.130472625436737,1.80531687708526,
12.6229866870364));
#70729=CARTESIAN_POINT('Ctrl Pts',(-0.13003108604427,1.80512182647746,12.6230167617716));
#70730=CARTESIAN_POINT('Ctrl Pts',(-0.129837103610137,1.80503636311472,
12.6230299570727));
#70731=CARTESIAN_POINT('Ctrl Pts',(-0.129461631291973,1.80487138242886,
12.6230554638541));
#70732=CARTESIAN_POINT('Ctrl Pts',(-0.129280152267775,1.80479184103976,
12.6230677768057));
#70733=CARTESIAN_POINT('Ctrl Pts',(-0.12890491241708,1.80462778758897,12.6230932041341));
#70734=CARTESIAN_POINT('Ctrl Pts',(-0.128711142320766,1.8045432990217,12.623106317043));
#70735=CARTESIAN_POINT('Ctrl Pts',(-0.128240383177364,1.80433858736127,
12.6231381323252));
#70736=CARTESIAN_POINT('Ctrl Pts',(-0.127963307382638,1.8042185625053,12.6231568225022));
#70737=CARTESIAN_POINT('Ctrl Pts',(-0.126924893911851,1.80377047042737,
12.6232267377013));
#70738=CARTESIAN_POINT('Ctrl Pts',(-0.12616245143274,1.803444948164,12.623277808433));
#70739=CARTESIAN_POINT('Ctrl Pts',(-0.112483570691222,1.79766709770227,
12.624189493848));
#70740=CARTESIAN_POINT('Ctrl Pts',(-0.0992242532669101,1.79305962175152,
12.6250006339302));
#70741=CARTESIAN_POINT('Ctrl Pts',(-0.0691312990108737,1.78475780571472,
12.6267698960893));
#70742=CARTESIAN_POINT('Ctrl Pts',(-0.0522178637634279,1.78151907948186,
12.6277178917979));
#70743=CARTESIAN_POINT('Ctrl Pts',(-0.032582528648154,1.77936609021369,
12.6288329992982));
#70744=CARTESIAN_POINT('Ctrl Pts',(-0.0300353424680076,1.77911746198778,
12.6289778979243));
#70745=CARTESIAN_POINT('Ctrl Pts',(-0.0179680999931977,1.77808453369203,
12.6296662139752));
#70746=CARTESIAN_POINT('Ctrl Pts',(-0.00841983568812099,1.77769346042888,
12.630216509681));
#70747=CARTESIAN_POINT('Ctrl Pts',(0.00835066081367094,1.77775232614261,
12.6312041915843));
#70748=CARTESIAN_POINT('Ctrl Pts',(0.0155667529695329,1.77802024795877,
12.6316360091664));
#70749=CARTESIAN_POINT('Ctrl Pts',(0.0237383780460576,1.77859898471538,
12.6321348243136));
#70750=CARTESIAN_POINT('Ctrl Pts',(0.0247090648291275,1.77867215293273,
12.6321942337122));
#70751=CARTESIAN_POINT('Ctrl Pts',(0.0261694510710479,1.77878889006884,
12.6322838548113));
#70752=CARTESIAN_POINT('Ctrl Pts',(0.0266594127649577,1.77882918404787,
12.6323139635704));
#70753=CARTESIAN_POINT('Ctrl Pts',(0.0275030836455508,1.77890051060771,
12.6323658790763));
#70754=CARTESIAN_POINT('Ctrl Pts',(0.0278568382811187,1.77893100701354,
12.6323876689302));
#70755=CARTESIAN_POINT('Ctrl Pts',(0.0285863904456573,1.77899511489679,
12.6324326509772));
#70756=CARTESIAN_POINT('Ctrl Pts',(0.0289621806781749,1.77902880181032,
12.6324558455127));
#70757=CARTESIAN_POINT('Ctrl Pts',(0.0299762541646356,1.77912150165511,
12.6325185025269));
#70758=CARTESIAN_POINT('Ctrl Pts',(0.0306144194441522,1.77918175889387,
12.6325580040958));
#70759=CARTESIAN_POINT('Ctrl Pts',(0.0329696722154685,1.77941123948419,
12.6327040559405));
#70760=CARTESIAN_POINT('Ctrl Pts',(0.0346855484848275,1.77959234529213,
12.6328109795501));
#70761=CARTESIAN_POINT('Ctrl Pts',(0.0636346891724505,1.78288310933234,
12.6346239357937));
#70762=CARTESIAN_POINT('Ctrl Pts',(0.0903572443348884,1.78944016818164,
12.6364470189146));
#70763=CARTESIAN_POINT('Ctrl Pts',(0.129203829033449,1.80441553176713,12.6392638367271));
#70764=CARTESIAN_POINT('Ctrl Pts',(0.142132738459312,1.81041040968414,12.6402291913141));
#70765=CARTESIAN_POINT('Ctrl Pts',(0.158836856858038,1.81954485116631,12.6414835146814));
#70766=CARTESIAN_POINT('Ctrl Pts',(0.162998521407312,1.82194294717615,12.6417965570157));
#70767=CARTESIAN_POINT('Ctrl Pts',(0.16908119966043,1.82563151839742,12.6422532500383));
#70768=CARTESIAN_POINT('Ctrl Pts',(0.171044273971853,1.82685100620375,12.6424005036394));
#70769=CARTESIAN_POINT('Ctrl Pts',(0.173773732773531,1.82858754775436,12.6426048699034));
#70770=CARTESIAN_POINT('Ctrl Pts',(0.174551216280972,1.82908690991551,12.6426630402455));
#70771=CARTESIAN_POINT('Ctrl Pts',(0.17589647198174,1.8299591361978,12.6427636006482));
#70772=CARTESIAN_POINT('Ctrl Pts',(0.176465228297705,1.8303304611188,12.6428060881676));
#70773=CARTESIAN_POINT('Ctrl Pts',(0.177283037904706,1.83086808110544,12.642867135109));
#70774=CARTESIAN_POINT('Ctrl Pts',(0.17753303512872,1.83103292629707,12.6428857904756));
#70775=CARTESIAN_POINT('Ctrl Pts',(0.177968647674363,1.83132103596253,12.642918285638));
#70776=CARTESIAN_POINT('Ctrl Pts',(0.178154365334642,1.83144414475814,12.6429321359439));
#70777=CARTESIAN_POINT('Ctrl Pts',(0.178511996001877,1.83168174573787,12.6429587999387));
#70778=CARTESIAN_POINT('Ctrl Pts',(0.17868392624026,1.83179621033472,12.6429716154563));
#70779=CARTESIAN_POINT('Ctrl Pts',(0.179091948830611,1.83206842270357,12.6430020219018));
#70780=CARTESIAN_POINT('Ctrl Pts',(0.179327943455863,1.83222631767512,12.6430196028575));
#70781=CARTESIAN_POINT('Ctrl Pts',(0.180034324187824,1.83270028263979,12.6430722101546));
#70782=CARTESIAN_POINT('Ctrl Pts',(0.180504088739578,1.83301728380587,12.6431071741185));
#70783=CARTESIAN_POINT('Ctrl Pts',(0.185036141744048,1.83609298151457,12.6434443062806));
#70784=CARTESIAN_POINT('Ctrl Pts',(0.189035983359318,1.83894312582869,12.643740427882));
#70785=CARTESIAN_POINT('Ctrl Pts',(0.194286161150776,1.84286819287913,12.6441294590774));
#70786=CARTESIAN_POINT('Ctrl Pts',(0.195595413669306,1.84386270674848,12.6442265020967));
#70787=CARTESIAN_POINT('Ctrl Pts',(0.197458006305936,1.84530015016024,12.6443646914499));
#70788=CARTESIAN_POINT('Ctrl Pts',(0.198017565662223,1.84573493856557,12.6444062235031));
#70789=CARTESIAN_POINT('Ctrl Pts',(0.201721770456884,1.84863282132245,12.6446813080671));
#70790=CARTESIAN_POINT('Ctrl Pts',(0.204821927565954,1.85115243355031,12.6449122477602));
#70791=CARTESIAN_POINT('Ctrl Pts',(0.22482649081042,1.86803806472242,12.6464129843889));
#70792=CARTESIAN_POINT('Ctrl Pts',(0.240256246804799,1.88405945487228,12.6476249423491));
#70793=CARTESIAN_POINT('Ctrl Pts',(0.264450340574353,1.91501436316179,12.6498536871035));
#70794=CARTESIAN_POINT('Ctrl Pts',(0.273891385891835,1.92930422142116,12.6508472312825));
#70795=CARTESIAN_POINT('Ctrl Pts',(0.28272523996759,1.94530994264776,12.6519586851609));
#70796=CARTESIAN_POINT('Ctrl Pts',(0.283291170421165,1.94634881106424,12.652030809099));
#70797=CARTESIAN_POINT('Ctrl Pts',(0.284103475539937,1.94785968888747,12.6521356878562));
#70798=CARTESIAN_POINT('Ctrl Pts',(0.284354425214816,1.9483292383659,12.6521682799478));
#70799=CARTESIAN_POINT('Ctrl Pts',(0.284790727020741,1.94915048732087,12.6522252813045));
#70800=CARTESIAN_POINT('Ctrl Pts',(0.284976594560447,1.94950191289264,12.6522496722387));
#70801=CARTESIAN_POINT('Ctrl Pts',(0.285334741546027,1.95018211499849,12.6522968808661));
#70802=CARTESIAN_POINT('Ctrl Pts',(0.285507104276185,1.95051084719786,12.6523196955664));
#70803=CARTESIAN_POINT('Ctrl Pts',(0.285914937941978,1.95129195054275,12.6523739047866));
#70804=CARTESIAN_POINT('Ctrl Pts',(0.286149903228206,1.9517445832711,12.6524053170949));
#70805=CARTESIAN_POINT('Ctrl Pts',(0.286974679094783,1.95334268121504,12.6525162223056));
#70806=CARTESIAN_POINT('Ctrl Pts',(0.287558688072607,1.95449111219108,12.6525959190091));
#70807=CARTESIAN_POINT('Ctrl Pts',(0.296486187531674,1.97231035276441,12.6538325568906));
#70808=CARTESIAN_POINT('Ctrl Pts',(0.303373155113652,1.98966770968823,12.655041027468));
#70809=CARTESIAN_POINT('Ctrl Pts',(0.31335330594097,2.02298397179068,12.6573612594581));
#70810=CARTESIAN_POINT('Ctrl Pts',(0.31681706446449,2.0387735983825,12.6584603876228));
#70811=CARTESIAN_POINT('Ctrl Pts',(0.321209239133184,2.06974889480681,12.6605679766027));
#70812=CARTESIAN_POINT('Ctrl Pts',(0.322276106084797,2.08487587596805,12.661574888799));
#70813=CARTESIAN_POINT('Ctrl Pts',(0.322274931633552,2.10094731643302,12.6625856179645));
#70814=CARTESIAN_POINT('Ctrl Pts',(0.322270892319163,2.10187109091309,12.6626435043966));
#70815=CARTESIAN_POINT('Ctrl Pts',(0.322259938807276,2.10313409683487,12.6627223498357));
#70816=CARTESIAN_POINT('Ctrl Pts',(0.322256460944064,2.10347334210428,12.6627434984175));
#70817=CARTESIAN_POINT('Ctrl Pts',(0.322250032133136,2.10401672699517,12.6627773252712));
#70818=CARTESIAN_POINT('Ctrl Pts',(0.322247422905286,2.10422086922562,12.6627900227457));
#70819=CARTESIAN_POINT('Ctrl Pts',(0.322241578492425,2.1046464797449,12.6628164726298));
#70820=CARTESIAN_POINT('Ctrl Pts',(0.322238308986342,2.10486794670926,12.6628302229931));
#70821=CARTESIAN_POINT('Ctrl Pts',(0.322230189759312,2.10538201360899,12.6628621106337));
#70822=CARTESIAN_POINT('Ctrl Pts',(0.322225169794744,2.10567461145633,12.6628802382985));
#70823=CARTESIAN_POINT('Ctrl Pts',(0.322207606835458,2.10662298407759,12.6629389231083));
#70824=CARTESIAN_POINT('Ctrl Pts',(0.322193460340211,2.10727873289414,12.6629793906942));
#70825=CARTESIAN_POINT('Ctrl Pts',(0.322036318261357,2.11365947405338,12.6633721299591));
#70826=CARTESIAN_POINT('Ctrl Pts',(0.321742739571791,2.11938016842448,12.6637161824122));
#70827=CARTESIAN_POINT('Ctrl Pts',(0.321260061828799,2.12556112710748,12.6640820960283));
#70828=CARTESIAN_POINT('Ctrl Pts',(0.321222268926149,2.12603175936495,12.664109920897));
#70829=CARTESIAN_POINT('Ctrl Pts',(0.318902950200669,2.15413975421192,12.6657696314752));
#70830=CARTESIAN_POINT('Ctrl Pts',(0.313064695962023,2.18136982709652,12.6672652695433));
#70831=CARTESIAN_POINT('Ctrl Pts',(0.298812567944701,2.22164158169612,12.6696921560592));
#70832=CARTESIAN_POINT('Ctrl Pts',(0.292836263485593,2.23539742039894,12.6705616877709));
#70833=CARTESIAN_POINT('Ctrl Pts',(0.285192942406668,2.25009557910688,12.6715612456403));
#70834=CARTESIAN_POINT('Ctrl Pts',(0.284449915566278,2.25149898567876,12.6716574124135));
#70835=CARTESIAN_POINT('Ctrl Pts',(0.283129747846024,2.25394852665679,12.6718265720009));
#70836=CARTESIAN_POINT('Ctrl Pts',(0.282557100614126,2.25499705741575,12.6718994051566));
#70837=CARTESIAN_POINT('Ctrl Pts',(0.281719816945964,2.25651008310049,12.6720051276942));
#70838=CARTESIAN_POINT('Ctrl Pts',(0.281459829496123,2.25697715039701,12.6720378506277));
#70839=CARTESIAN_POINT('Ctrl Pts',(0.281004289498087,2.2577907577746,12.6720950045516));
#70840=CARTESIAN_POINT('Ctrl Pts',(0.280809254422768,2.2581375875105,12.6721194169179));
#70841=CARTESIAN_POINT('Ctrl Pts',(0.280431323158472,2.25880675669054,12.6721666118676));
#70842=CARTESIAN_POINT('Ctrl Pts',(0.28024851217878,2.25912914377567,12.6721893913554));
#70843=CARTESIAN_POINT('Ctrl Pts',(0.279813899048572,2.25989251199931,12.6722434307136));
#70844=CARTESIAN_POINT('Ctrl Pts',(0.279561610483123,2.2603332137568,12.6722747081106));
#70845=CARTESIAN_POINT('Ctrl Pts',(0.278671921014469,2.26187885357189,12.6723846870006));
#70846=CARTESIAN_POINT('Ctrl Pts',(0.278029008799322,2.26298059082657,12.6724635878451));
#70847=CARTESIAN_POINT('Ctrl Pts',(0.268606400872723,2.27890979248885,12.6736118254267));
#70848=CARTESIAN_POINT('Ctrl Pts',(0.258659382805385,2.29301103828681,12.6747249028285));
#70849=CARTESIAN_POINT('Ctrl Pts',(0.232617834483761,2.32427820237332,12.6774292264098));
#70850=CARTESIAN_POINT('Ctrl Pts',(0.215678009381438,2.34061311885854,12.6790425177258));
#70851=CARTESIAN_POINT('Ctrl Pts',(0.190201726535308,2.36030915232194,12.6811776633843));
#70852=CARTESIAN_POINT('Ctrl Pts',(0.183072419183627,2.36537157245333,12.6817474605309));
#70853=CARTESIAN_POINT('Ctrl Pts',(0.174999731144078,2.37062346752309,12.6823555625261));
#70854=CARTESIAN_POINT('Ctrl Pts',(0.174252003085409,2.37110552657333,12.6824115475311));
#70855=CARTESIAN_POINT('Ctrl Pts',(0.172946523591007,2.37193953468199,12.6825086894062));
#70856=CARTESIAN_POINT('Ctrl Pts',(0.172389674509169,2.37229287667165,12.6825499349618));
#70857=CARTESIAN_POINT('Ctrl Pts',(0.171581782647307,2.37280204321679,12.6826094959071));
#70858=CARTESIAN_POINT('Ctrl Pts',(0.171331608661035,2.37295923284435,12.682627901082));
#70859=CARTESIAN_POINT('Ctrl Pts',(0.170892989624312,2.37323398590605,12.682660101959));
#70860=CARTESIAN_POINT('Ctrl Pts',(0.170704638816866,2.3733516988139,12.6826739076296));
#70861=CARTESIAN_POINT('Ctrl Pts',(0.170340009620423,2.37357905592845,12.6827005914425));
#70862=CARTESIAN_POINT('Ctrl Pts',(0.170163747440561,2.37368872424305,12.6827134712121));
#70863=CARTESIAN_POINT('Ctrl Pts',(0.169742767067178,2.37395008952703,12.6827441874106));
#70864=CARTESIAN_POINT('Ctrl Pts',(0.169497950801575,2.3741016293258,12.6827620133868));
#70865=CARTESIAN_POINT('Ctrl Pts',(0.168623715633899,2.37464115651323,12.6828255401566));
#70866=CARTESIAN_POINT('Ctrl Pts',(0.167993158793409,2.37502730946052,12.6828711207182));
#70867=CARTESIAN_POINT('Ctrl Pts',(0.158338294576425,2.38089435408875,12.683565475993));
#70868=CARTESIAN_POINT('Ctrl Pts',(0.149050205269201,2.38593136066844,12.6841861260136));
#70869=CARTESIAN_POINT('Ctrl Pts',(0.115842128055158,2.40188137992821,12.6863028573398));
#70870=CARTESIAN_POINT('Ctrl Pts',(0.0908506660060515,2.41031930079258,
12.6877266112227));
#70871=CARTESIAN_POINT('Ctrl Pts',(0.0559631144688198,2.41751621407871,
12.6897700651807));
#70872=CARTESIAN_POINT('Ctrl Pts',(0.046738418792484,2.41900456779105,12.6903144461336));
#70873=CARTESIAN_POINT('Ctrl Pts',(0.0328141551664482,2.4206342329586,12.6911501882692));
#70874=CARTESIAN_POINT('Ctrl Pts',(0.0281545578310163,2.42107693395974,
12.6914321578811));
#70875=CARTESIAN_POINT('Ctrl Pts',(0.0226172468280913,2.42148156485683,
12.691770493883));
#70876=CARTESIAN_POINT('Ctrl Pts',(0.0217470962122639,2.42154159945444,
12.6918237557348));
#70877=CARTESIAN_POINT('Ctrl Pts',(0.0204073634932882,2.42162856894783,
12.6919059099216));
#70878=CARTESIAN_POINT('Ctrl Pts',(0.0199379435579667,2.42165800977303,
12.6919347235605));
#70879=CARTESIAN_POINT('Ctrl Pts',(0.0190821787669227,2.42170980065954,
12.6919873035723));
#70880=CARTESIAN_POINT('Ctrl Pts',(0.0186958542693854,2.42173248269013,
12.692011059481));
#70881=CARTESIAN_POINT('Ctrl Pts',(0.0178538189901202,2.42178039884677,
12.6920628804837));
#70882=CARTESIAN_POINT('Ctrl Pts',(0.0173980941028262,2.42180536082032,
12.6920909540651));
#70883=CARTESIAN_POINT('Ctrl Pts',(0.0161564767652849,2.42187072427285,
12.6921675148444));
#70884=CARTESIAN_POINT('Ctrl Pts',(0.0153704906936252,2.4219092152823,12.6922160618568));
#70885=CARTESIAN_POINT('Ctrl Pts',(0.0116006579549702,2.42207999194193,
12.6924493054261));
#70886=CARTESIAN_POINT('Ctrl Pts',(0.00861528837951467,2.42217366794012,
12.6926352079763));
#70887=CARTESIAN_POINT('Ctrl Pts',(0.00440153812928454,2.42224728008276,
12.6928993718858));
#70888=CARTESIAN_POINT('Ctrl Pts',(0.00317385091221689,2.42226170989115,
12.692976548198));
#70889=CARTESIAN_POINT('Ctrl Pts',(0.00129576556333843,2.42227305130751,
12.6930949384668));
#70890=CARTESIAN_POINT('Ctrl Pts',(0.00064539986456536,2.42227500997834,
12.6931359961843));
#70891=CARTESIAN_POINT('Ctrl Pts',(-0.0301634909334848,2.42227453547553,
12.6950838324592));
#70892=CARTESIAN_POINT('Ctrl Pts',(-0.0601677324211988,2.41804054828723,
12.697132098493));
#70893=CARTESIAN_POINT('Ctrl Pts',(-0.0969512851132294,2.40745363310054,
12.6997131933395));
#70894=CARTESIAN_POINT('Ctrl Pts',(-0.104677547501558,2.40490967925323,
12.7002580873391));
#70895=CARTESIAN_POINT('Ctrl Pts',(-0.11911468164049,2.39954253729782,12.7012725062849));
#70896=CARTESIAN_POINT('Ctrl Pts',(-0.125842644935426,2.39677885124912,
12.701743609366));
#70897=CARTESIAN_POINT('Ctrl Pts',(-0.133568556171125,2.39329518169239,
12.7022780409889));
#70898=CARTESIAN_POINT('Ctrl Pts',(-0.134662456122448,2.39279454540867,
12.7023535533578));
#70899=CARTESIAN_POINT('Ctrl Pts',(-0.136094799150632,2.39212929131218,
12.7024521971335));
#70900=CARTESIAN_POINT('Ctrl Pts',(-0.136435775152762,2.39197019789751,
12.7024756624557));
#70901=CARTESIAN_POINT('Ctrl Pts',(-0.136991572205964,2.39170968650625,
12.7025138821698));
#70902=CARTESIAN_POINT('Ctrl Pts',(-0.137206559894064,2.39160862809586,
12.7025286587888));
#70903=CARTESIAN_POINT('Ctrl Pts',(-0.137621794943528,2.3914128793418,12.7025571848057));
#70904=CARTESIAN_POINT('Ctrl Pts',(-0.137822055917343,2.39131822049557,
12.7025709360565));
#70905=CARTESIAN_POINT('Ctrl Pts',(-0.138286741032999,2.3910979879146,12.7026028299271));
#70906=CARTESIAN_POINT('Ctrl Pts',(-0.138551092715102,2.39097225988491,
12.7026209629229));
#70907=CARTESIAN_POINT('Ctrl Pts',(-0.139407631246628,2.39056345054624,
12.7026796823161));
#70908=CARTESIAN_POINT('Ctrl Pts',(-0.139999129554428,2.39027891791343,
12.7027201790069));
#70909=CARTESIAN_POINT('Ctrl Pts',(-0.145757603908711,2.38748718255777,
12.7031139522351));
#70910=CARTESIAN_POINT('Ctrl Pts',(-0.150857947107048,2.38484390285048,
12.7034589621373));
#70911=CARTESIAN_POINT('Ctrl Pts',(-0.156542820691324,2.38170212161456,
12.7038422749471));
#70912=CARTESIAN_POINT('Ctrl Pts',(-0.157199089401506,2.3813364291061,12.7038865059924));
#70913=CARTESIAN_POINT('Ctrl Pts',(-0.158924175049733,2.38036723910117,
12.7040027384602));
#70914=CARTESIAN_POINT('Ctrl Pts',(-0.159990841077548,2.37975992032515,
12.7040745730923));
#70915=CARTESIAN_POINT('Ctrl Pts',(-0.164589420662945,2.37710676254905,
12.7043842253612));
#70916=CARTESIAN_POINT('Ctrl Pts',(-0.168085866503903,2.37499996166468,
12.7046195658867));
#70917=CARTESIAN_POINT('Ctrl Pts',(-0.182324404307719,2.36604741173927,
12.7055814015772));
#70918=CARTESIAN_POINT('Ctrl Pts',(-0.192696375987787,2.35863400244468,
12.706290692235));
#70919=CARTESIAN_POINT('Ctrl Pts',(-0.212956776373089,2.34225575991361,
12.7077472184702));
#70920=CARTESIAN_POINT('Ctrl Pts',(-0.222781813165474,2.33325238975243,
12.7084934685184));
#70921=CARTESIAN_POINT('Ctrl Pts',(-0.239982591609493,2.31540917720707,
12.7099197394892));
#70922=CARTESIAN_POINT('Ctrl Pts',(-0.247496346665469,2.30673236935726,
12.710593488435));
#70923=CARTESIAN_POINT('Ctrl Pts',(-0.255784989053216,2.29605966919968,
12.7114105341652));
#70924=CARTESIAN_POINT('Ctrl Pts',(-0.257023449190687,2.29443328104845,
12.7115347266316));
#70925=CARTESIAN_POINT('Ctrl Pts',(-0.258642203218125,2.29226498442269,
12.7116999290876));
#70926=CARTESIAN_POINT('Ctrl Pts',(-0.259036438906985,2.29173350471078,
12.711740393335));
#70927=CARTESIAN_POINT('Ctrl Pts',(-0.259680455280729,2.29085967714637,
12.7118068761416));
#70928=CARTESIAN_POINT('Ctrl Pts',(-0.2599312038883,2.29051804234162,12.7118328569957));
#70929=CARTESIAN_POINT('Ctrl Pts',(-0.260415398671583,2.28985561136627,
12.7118832121895));
#70930=CARTESIAN_POINT('Ctrl Pts',(-0.260648927851673,2.28953487657968,
12.7119075832492));
#70931=CARTESIAN_POINT('Ctrl Pts',(-0.261186214566062,2.28879408270519,
12.7119638503217));
#70932=CARTESIAN_POINT('Ctrl Pts',(-0.261489551451457,2.28837372115173,
12.7119957625081));
#70933=CARTESIAN_POINT('Ctrl Pts',(-0.262455662772666,2.28702806246782,
12.7120978685487));
#70934=CARTESIAN_POINT('Ctrl Pts',(-0.26311454460571,2.28609999311008,12.7121682118643));
#70935=CARTESIAN_POINT('Ctrl Pts',(-0.269058100290468,2.27763352594785,
12.7128092712413));
#70936=CARTESIAN_POINT('Ctrl Pts',(-0.274021925476739,2.26987609396934,
12.7133921052078));
#70937=CARTESIAN_POINT('Ctrl Pts',(-0.293944022309454,2.23559180971319,
12.7159525583956));
#70938=CARTESIAN_POINT('Ctrl Pts',(-0.30543216780947,2.20723261627071,12.7180515638223));
#70939=CARTESIAN_POINT('Ctrl Pts',(-0.315161040815088,2.16806663384149,
12.7207397032437));
#70940=CARTESIAN_POINT('Ctrl Pts',(-0.317106723563917,2.15833452148095,
12.7213894667624));
#70941=CARTESIAN_POINT('Ctrl Pts',(-0.318818403965751,2.14709665448337,
12.7221079047565));
#70942=CARTESIAN_POINT('Ctrl Pts',(-0.319026663470127,2.14566462255405,
12.722198865012));
#70943=CARTESIAN_POINT('Ctrl Pts',(-0.319280521766391,2.14383247747162,
12.722314444726));
#70944=CARTESIAN_POINT('Ctrl Pts',(-0.319335021884388,2.14343364436722,
12.7223395567739));
#70945=CARTESIAN_POINT('Ctrl Pts',(-0.31942128154863,2.14279345485475,12.7223797872454));
#70946=CARTESIAN_POINT('Ctrl Pts',(-0.31945351491635,2.1425521643763,12.7223949324639));
#70947=CARTESIAN_POINT('Ctrl Pts',(-0.319514309987767,2.14209310604026,
12.7224237122151));
#70948=CARTESIAN_POINT('Ctrl Pts',(-0.319542922233879,2.14187534732476,
12.7224373494819));
#70949=CARTESIAN_POINT('Ctrl Pts',(-0.319607554410098,2.14137952878586,
12.7224683672128));
#70950=CARTESIAN_POINT('Ctrl Pts',(-0.319643434039418,2.14110145150065,
12.7224857396136));
#70951=CARTESIAN_POINT('Ctrl Pts',(-0.31975378018135,2.14023735388963,12.7225396498846));
#70952=CARTESIAN_POINT('Ctrl Pts',(-0.319826998900076,2.13965117117984,
12.7225761173822));
#70953=CARTESIAN_POINT('Ctrl Pts',(-0.320374987342286,2.13516373476118,
12.7228545167446));
#70954=CARTESIAN_POINT('Ctrl Pts',(-0.320779997052963,2.13125408190264,
12.7230926061921));
#70955=CARTESIAN_POINT('Ctrl Pts',(-0.321880646213262,2.11832570593583,
12.7238680874627));
#70956=CARTESIAN_POINT('Ctrl Pts',(-0.322268220777703,2.10928454586238,
12.7243915076839));
#70957=CARTESIAN_POINT('Ctrl Pts',(-0.3222980136772,2.06900520556015,12.7266854167059));
#70958=CARTESIAN_POINT('Ctrl Pts',(-0.317781127774183,2.03793606687203,
12.7283711669917));
#70959=CARTESIAN_POINT('Ctrl Pts',(-0.30696909246082,2.00163717397536,12.7306064103029));
#70960=CARTESIAN_POINT('Ctrl Pts',(-0.304877384437114,1.99533367262709,
12.7310039785322));
#70961=CARTESIAN_POINT('Ctrl Pts',(-0.30223487916569,1.98812357705959,12.7314713224698));
#70962=CARTESIAN_POINT('Ctrl Pts',(-0.301872450919865,1.98714930425478,
12.7315347416019));
#70963=CARTESIAN_POINT('Ctrl Pts',(-0.301326977087005,1.98570440306193,
12.7316292016562));
#70964=CARTESIAN_POINT('Ctrl Pts',(-0.301147526216988,1.98523241725721,
12.7316601221923));
#70965=CARTESIAN_POINT('Ctrl Pts',(-0.300826245251008,1.98439333640509,
12.7317152074847));
#70966=CARTESIAN_POINT('Ctrl Pts',(-0.300684850298476,1.98402607492126,
12.7317393575998));
#70967=CARTESIAN_POINT('Ctrl Pts',(-0.300386098065088,1.98325431014875,
12.731790190404));
#70968=CARTESIAN_POINT('Ctrl Pts',(-0.30022859571811,1.98284986419209,12.7318168779311));
#70969=CARTESIAN_POINT('Ctrl Pts',(-0.29981212319551,1.98178677192677,12.7318871546343));
#70970=CARTESIAN_POINT('Ctrl Pts',(-0.299551800644933,1.98112866104859,
12.7319307892876));
#70971=CARTESIAN_POINT('Ctrl Pts',(-0.298380125612294,1.97819488731416,
12.732125890853));
#70972=CARTESIAN_POINT('Ctrl Pts',(-0.297445013241985,1.9759288575038,12.7322781584792));
#70973=CARTESIAN_POINT('Ctrl Pts',(-0.29042747320749,1.95945888612768,12.7333966617674));
#70974=CARTESIAN_POINT('Ctrl Pts',(-0.283357282461509,1.9457001380034,12.7343969780078));
#70975=CARTESIAN_POINT('Ctrl Pts',(-0.258527893869593,1.90488600248727,
12.7375693276821));
#70976=CARTESIAN_POINT('Ctrl Pts',(-0.237669020585884,1.87995568670838,
12.7398270568302));
#70977=CARTESIAN_POINT('Ctrl Pts',(-0.212337273616127,1.85756182886676,
12.7419652587983));
#70978=CARTESIAN_POINT('Ctrl Pts',(-0.211216922126842,1.85658513480374,
12.7420587299654));
#70979=CARTESIAN_POINT('Ctrl Pts',(-0.209767496374826,1.85533910453047,
12.7421782097466));
#70980=CARTESIAN_POINT('Ctrl Pts',(-0.209444614117482,1.85506264080497,
12.7422047343115));
#70981=CARTESIAN_POINT('Ctrl Pts',(-0.208932125437122,1.85462558339571,
12.7422466889626));
#70982=CARTESIAN_POINT('Ctrl Pts',(-0.208742880082693,1.85446457001207,
12.7422621500264));
#70983=CARTESIAN_POINT('Ctrl Pts',(-0.208403424497302,1.85417643114158,
12.7422898264909));
#70984=CARTESIAN_POINT('Ctrl Pts',(-0.208253285138892,1.85404922529566,
12.7423020478385));
#70985=CARTESIAN_POINT('Ctrl Pts',(-0.207899995204906,1.85375045518358,
12.7423307592287));
#70986=CARTESIAN_POINT('Ctrl Pts',(-0.207696749043881,1.85357900502124,
12.7423472407803));
#70987=CARTESIAN_POINT('Ctrl Pts',(-0.207106884593097,1.85308266767366,
12.7423949703796));
#70988=CARTESIAN_POINT('Ctrl Pts',(-0.206719712340603,1.85275843555941,
12.7424261703386));
#70989=CARTESIAN_POINT('Ctrl Pts',(-0.204037913078161,1.85052330273849,
12.7426414067777));
#70990=CARTESIAN_POINT('Ctrl Pts',(-0.201717489824324,1.84864338423648,
12.7428232273925));
#70991=CARTESIAN_POINT('Ctrl Pts',(-0.194377244848565,1.84286372542345,
12.743385933902));
#70992=CARTESIAN_POINT('Ctrl Pts',(-0.189267727330464,1.83907986753902,
12.743759810019));
#70993=CARTESIAN_POINT('Ctrl Pts',(-0.171146198593381,1.826472622341,12.7450379286634));
#70994=CARTESIAN_POINT('Ctrl Pts',(-0.157602797201683,1.8184512994269,12.7459114119524));
#70995=CARTESIAN_POINT('Ctrl Pts',(-0.121062001803699,1.80027558308879,
12.7481933628477));
#70996=CARTESIAN_POINT('Ctrl Pts',(-0.0973724990780165,1.79176457423886,
12.7496089563464));
#70997=CARTESIAN_POINT('Ctrl Pts',(-0.071401661738542,1.78573026827096,
12.7512253491736));
#70998=CARTESIAN_POINT('Ctrl Pts',(-0.0698633049023688,1.7853847110031,
12.7513212893368));
#70999=CARTESIAN_POINT('Ctrl Pts',(-0.0677192104231427,1.78491958924006,
12.7514552975027));
#71000=CARTESIAN_POINT('Ctrl Pts',(-0.0671155541168977,1.78479045209226,
12.7514930586409));
#71001=CARTESIAN_POINT('Ctrl Pts',(-0.0661468718781647,1.78458613559324,
12.7515537061667));
#71002=CARTESIAN_POINT('Ctrl Pts',(-0.0657820780349808,1.78450985320175,
12.7515765572141));
#71003=CARTESIAN_POINT('Ctrl Pts',(-0.0650287355410895,1.78435368443279,
12.7516237723065));
#71004=CARTESIAN_POINT('Ctrl Pts',(-0.0646401702072823,1.78427388234324,
12.7516481390043));
#71005=CARTESIAN_POINT('Ctrl Pts',(-0.0637350661091332,1.78408973635926,
12.7517049298787));
#71006=CARTESIAN_POINT('Ctrl Pts',(-0.0632184178936092,1.78398594183286,
12.7517373715434));
#71007=CARTESIAN_POINT('Ctrl Pts',(-0.0615698020172943,1.78365893994127,
12.7518409718653));
#71008=CARTESIAN_POINT('Ctrl Pts',(-0.0604368988732375,1.78344054587071,
12.7519122838711));
#71009=CARTESIAN_POINT('Ctrl Pts',(-0.0349713140770128,1.77867313226768,
12.7535180205679));
#71010=CARTESIAN_POINT('Ctrl Pts',(-0.0102014481847637,1.77693749736386,
12.7551465958483));
#71011=CARTESIAN_POINT('Ctrl Pts',(0.0392963744586832,1.77916950582992,
12.7584894940021));
#71012=CARTESIAN_POINT('Ctrl Pts',(0.063865145861179,1.7831437859012,12.7601910495075));
#71013=CARTESIAN_POINT('Ctrl Pts',(0.0890940594577364,1.7902817159124,12.761848024256));
#71014=CARTESIAN_POINT('Ctrl Pts',(0.0904493874471372,1.79067480637249,
12.7619367328674));
#71015=CARTESIAN_POINT('Ctrl Pts',(0.0922015083168492,1.79119548078547,
12.762050975548));
#71016=CARTESIAN_POINT('Ctrl Pts',(0.0926006698698686,1.79131494178123,
12.7620769724326));
#71017=CARTESIAN_POINT('Ctrl Pts',(0.0932121357200198,1.79149923394967,
12.7621167500453));
#71018=CARTESIAN_POINT('Ctrl Pts',(0.0934246046612958,1.79156351035633,
12.7621305631674));
#71019=CARTESIAN_POINT('Ctrl Pts',(0.0938435847576729,1.79169073346145,
12.7621577848877));
#71020=CARTESIAN_POINT('Ctrl Pts',(0.0940500978343611,1.79175366777266,
12.7621711940475));
#71021=CARTESIAN_POINT('Ctrl Pts',(0.0945107968945404,1.79189457066812,
12.7622010894277));
#71022=CARTESIAN_POINT('Ctrl Pts',(0.0947649490451584,1.79197264610572,
12.7622175692334));
#71023=CARTESIAN_POINT('Ctrl Pts',(0.0955014279907667,1.79219988991929,
12.7622652888352));
#71024=CARTESIAN_POINT('Ctrl Pts',(0.0959835040252072,1.79234987814531,
12.7622964805738));
#71025=CARTESIAN_POINT('Ctrl Pts',(0.0993116036978307,1.79339393324283,
12.7625115268883));
#71026=CARTESIAN_POINT('Ctrl Pts',(0.102145565574032,1.79432638358897,12.7626931700653));
#71027=CARTESIAN_POINT('Ctrl Pts',(0.110972785339516,1.79736725894137,12.7632555126664));
#71028=CARTESIAN_POINT('Ctrl Pts',(0.11691720449251,1.79961372627749,12.7636292066262));
#71029=CARTESIAN_POINT('Ctrl Pts',(0.137314296259386,1.80801937979289,12.764906532903));
#71030=CARTESIAN_POINT('Ctrl Pts',(0.151380871440545,1.81505826015645,12.7657794356856));
#71031=CARTESIAN_POINT('Ctrl Pts',(0.186555291292564,1.83600234546141,12.7680684178094));
#71032=CARTESIAN_POINT('Ctrl Pts',(0.206637743401506,1.85140751406754,12.7694917914411));
#71033=CARTESIAN_POINT('Ctrl Pts',(0.22578549421405,1.87003411964847,12.771112154926));
#71034=CARTESIAN_POINT('Ctrl Pts',(0.226846237074405,1.87108040684051,12.77120284892));
#71035=CARTESIAN_POINT('Ctrl Pts',(0.228283284064847,1.87251766618022,12.7713270103677));
#71036=CARTESIAN_POINT('Ctrl Pts',(0.228665923885607,1.87290230025078,12.7713601971794));
#71037=CARTESIAN_POINT('Ctrl Pts',(0.229314857591101,1.8735579189781,12.7714166966568));
#71038=CARTESIAN_POINT('Ctrl Pts',(0.229581647797675,1.87382841256679,12.7714399874238));
#71039=CARTESIAN_POINT('Ctrl Pts',(0.230118324678067,1.87437446721308,12.7714869661206));
#71040=CARTESIAN_POINT('Ctrl Pts',(0.230388196197885,1.87465004227048,12.7715106546591));
#71041=CARTESIAN_POINT('Ctrl Pts',(0.2310005269371,1.87527756381501,12.7715645516838));
#71042=CARTESIAN_POINT('Ctrl Pts',(0.231342677152315,1.87562980925738,12.7715947735851));
#71043=CARTESIAN_POINT('Ctrl Pts',(0.232056295744779,1.87636785101841,12.7716580299529));
#71044=CARTESIAN_POINT('Ctrl Pts',(0.232427609909756,1.8767537937635,12.7716910709992));
#71045=CARTESIAN_POINT('Ctrl Pts',(0.233398298160891,1.8777677707484,12.7717777819875));
#71046=CARTESIAN_POINT('Ctrl Pts',(0.233996096589068,1.87839730132519,12.7718315198894));
#71047=CARTESIAN_POINT('Ctrl Pts',(0.235763774619217,1.88027393851874,12.7719914316652));
#71048=CARTESIAN_POINT('Ctrl Pts',(0.236926266307724,1.8815279338937,12.7720979208166));
#71049=CARTESIAN_POINT('Ctrl Pts',(0.249595770763598,1.89541474631622,12.7732733134957));
#71050=CARTESIAN_POINT('Ctrl Pts',(0.260088709742853,1.90893228567935,12.7743847600436));
#71051=CARTESIAN_POINT('Ctrl Pts',(0.284974320967406,1.94686365838458,12.7774119995573));
#71052=CARTESIAN_POINT('Ctrl Pts',(0.29730807380174,1.97244997711326,12.7793724891378));
#71053=CARTESIAN_POINT('Ctrl Pts',(0.307223558791195,2.00259978892891,12.7814106527746));
#71054=CARTESIAN_POINT('Ctrl Pts',(0.308250294919806,2.00589965854843,12.7816300947249));
#71055=CARTESIAN_POINT('Ctrl Pts',(0.309383941520664,2.00976100894052,12.7818821511715));
#71056=CARTESIAN_POINT('Ctrl Pts',(0.309542635556573,2.01030688118527,12.7819176746694));
#71057=CARTESIAN_POINT('Ctrl Pts',(0.309777060170828,2.01112128233304,12.7819705073353));
#71058=CARTESIAN_POINT('Ctrl Pts',(0.309853886670054,2.01138949058335,12.7819878800527));
#71059=CARTESIAN_POINT('Ctrl Pts',(0.309990373991858,2.01186832816303,12.7820188477439));
#71060=CARTESIAN_POINT('Ctrl Pts',(0.310050168435358,2.01207891832641,12.7820324505349));
#71061=CARTESIAN_POINT('Ctrl Pts',(0.310176945271489,2.01252715160196,12.7820613680862));
#71062=CARTESIAN_POINT('Ctrl Pts',(0.310243868966954,2.01276481011532,12.7820766793561));
#71063=CARTESIAN_POINT('Ctrl Pts',(0.310423365016631,2.01340505313477,12.7821178709696));
#71064=CARTESIAN_POINT('Ctrl Pts',(0.31053542778828,2.01380778188335,12.7821437215394));
#71065=CARTESIAN_POINT('Ctrl Pts',(0.311075787940476,2.01576444968728,12.7822690311996));
#71066=CARTESIAN_POINT('Ctrl Pts',(0.311493216388209,2.01732140435859,12.7823678671197));
#71067=CARTESIAN_POINT('Ctrl Pts',(0.314933476378884,2.03054912691521,12.7832006719247));
#71068=CARTESIAN_POINT('Ctrl Pts',(0.317311280266319,2.04237934554807,12.7839002292066));
#71069=CARTESIAN_POINT('Ctrl Pts',(0.323492491125186,2.08554427789025,12.7863799730291));
#71070=CARTESIAN_POINT('Ctrl Pts',(0.323355220399317,2.11725775562877,12.7880839641929));
#71071=CARTESIAN_POINT('Ctrl Pts',(0.318558985801885,2.14880036914511,12.789972862854));
#71072=CARTESIAN_POINT('Ctrl Pts',(0.318504648706878,2.1491537609395,12.7899940476842));
#71073=CARTESIAN_POINT('Ctrl Pts',(0.317581876958154,2.15508940739074,12.790350251868));
#71074=CARTESIAN_POINT('Ctrl Pts',(0.316567439799264,2.16064768266981,12.7906894708981));
#71075=CARTESIAN_POINT('Ctrl Pts',(0.315206716276064,2.16713313427387,12.7910929155316));
#71076=CARTESIAN_POINT('Ctrl Pts',(0.315001583337389,2.16808916334379,12.7911525832712));
#71077=CARTESIAN_POINT('Ctrl Pts',(0.314685151325108,2.16953186595057,12.7912429258181));
#71078=CARTESIAN_POINT('Ctrl Pts',(0.314577065631431,2.17001924465002,12.7912734975513));
#71079=CARTESIAN_POINT('Ctrl Pts',(0.314383700140548,2.17088168064732,12.7913276881274));
#71080=CARTESIAN_POINT('Ctrl Pts',(0.314298880333391,2.17125684096698,12.7913512921594));
#71081=CARTESIAN_POINT('Ctrl Pts',(0.314118736202303,2.17204704393086,12.7914010754268));
#71082=CARTESIAN_POINT('Ctrl Pts',(0.314023260501571,2.17246205099014,12.7914272594881));
#71083=CARTESIAN_POINT('Ctrl Pts',(0.313826419523107,2.17330997014364,12.7914808362312));
#71084=CARTESIAN_POINT('Ctrl Pts',(0.313724980388417,2.17374286399562,12.7915082312425));
#71085=CARTESIAN_POINT('Ctrl Pts',(0.313472628283032,2.17480983741991,12.7915758575303));
#71086=CARTESIAN_POINT('Ctrl Pts',(0.313320687398373,2.17544366968593,12.7916161218708));
#71087=CARTESIAN_POINT('Ctrl Pts',(0.312895170433927,2.17719528632815,12.791727648093));
#71088=CARTESIAN_POINT('Ctrl Pts',(0.312617530483398,2.17831206478821,12.7917990408456));
#71089=CARTESIAN_POINT('Ctrl Pts',(0.311716471030652,2.18185532202667,12.7920264768815));
#71090=CARTESIAN_POINT('Ctrl Pts',(0.311070747664932,2.18427598372225,12.7921832376335));
#71091=CARTESIAN_POINT('Ctrl Pts',(0.308386057660836,2.19388875078528,12.7928113962438));
#71092=CARTESIAN_POINT('Ctrl Pts',(0.306125475368093,2.20101602244717,12.7932898595829));
#71093=CARTESIAN_POINT('Ctrl Pts',(0.298664231582634,2.22198051723248,12.7947358319504));
#71094=CARTESIAN_POINT('Ctrl Pts',(0.292757874081862,2.23554451715273,12.7957235828702));
#71095=CARTESIAN_POINT('Ctrl Pts',(0.282148713797219,2.2559516743852,12.7972768004029));
#71096=CARTESIAN_POINT('Ctrl Pts',(0.27807698856887,2.26310122520011,12.7978345173346));
#71097=CARTESIAN_POINT('Ctrl Pts',(0.26509302419037,2.28399746012209,12.7994949001649));
#71098=CARTESIAN_POINT('Ctrl Pts',(0.255400828351278,2.29723067303651,12.8005883409397));
#71099=CARTESIAN_POINT('Ctrl Pts',(0.24414731898204,2.31036658771123,12.801676218175));
#71100=CARTESIAN_POINT('Ctrl Pts',(0.243548433025559,2.31105964893951,12.8017336198947));
#71101=CARTESIAN_POINT('Ctrl Pts',(0.242739674038493,2.31198755965272,12.8018104674315));
#71102=CARTESIAN_POINT('Ctrl Pts',(0.242532407297021,2.31222465976554,12.8018301030824));
#71103=CARTESIAN_POINT('Ctrl Pts',(0.242183056463924,2.31262311494563,12.8018631001392));
#71104=CARTESIAN_POINT('Ctrl Pts',(0.242041158423969,2.31278463167437,12.8018764753627));
#71105=CARTESIAN_POINT('Ctrl Pts',(0.241768853951751,2.31309395988053,12.8019020899468));
#71106=CARTESIAN_POINT('Ctrl Pts',(0.24163847448526,2.31324179263786,12.8019143311182));
#71107=CARTESIAN_POINT('Ctrl Pts',(0.241329792526146,2.31359114978668,12.8019432584471));
#71108=CARTESIAN_POINT('Ctrl Pts',(0.241151373438628,2.31379257030551,12.8019599357024));
#71109=CARTESIAN_POINT('Ctrl Pts',(0.240627361924749,2.31438264576097,12.8020087916964));
#71110=CARTESIAN_POINT('Ctrl Pts',(0.240281078635024,2.31477069020068,12.8020409187787));
#71111=CARTESIAN_POINT('Ctrl Pts',(0.237701183975946,2.31764766602275,12.8022791139228));
#71112=CARTESIAN_POINT('Ctrl Pts',(0.235429787426852,2.32010265041096,12.802482392019));
#71113=CARTESIAN_POINT('Ctrl Pts',(0.227683409815427,2.32821798143634,12.8031562362659));
#71114=CARTESIAN_POINT('Ctrl Pts',(0.222038959348495,2.33371329069305,12.8036157023208));
#71115=CARTESIAN_POINT('Ctrl Pts',(0.204369407896036,2.34969731659983,12.8049828644614));
#71116=CARTESIAN_POINT('Ctrl Pts',(0.191761730137281,2.35950547936917,12.8058659995682));
#71117=CARTESIAN_POINT('Ctrl Pts',(0.159113850783497,2.3812203234735,12.8080621591748));
#71118=CARTESIAN_POINT('Ctrl Pts',(0.138414682339636,2.39196442846323,12.8093846654114));
#71119=CARTESIAN_POINT('Ctrl Pts',(0.115476022251753,2.40087922338813,12.8108787872511));
#71120=CARTESIAN_POINT('Ctrl Pts',(0.114207518094959,2.40136300619729,12.8109614754647));
#71121=CARTESIAN_POINT('Ctrl Pts',(0.112447548335094,2.40202151661007,12.8110763006425));
#71122=CARTESIAN_POINT('Ctrl Pts',(0.111958646062443,2.40220309261958,12.8111082086231));
#71123=CARTESIAN_POINT('Ctrl Pts',(0.11111817790777,2.40251291907921,12.8111630805358));
#71124=CARTESIAN_POINT('Ctrl Pts',(0.110766824357633,2.40264174578398,12.8111860252017));
#71125=CARTESIAN_POINT('Ctrl Pts',(0.110050769624072,2.40290287922451,12.8112327982012));
#71126=CARTESIAN_POINT('Ctrl Pts',(0.109686052389334,2.40303513995334,12.8112566280242));
#71127=CARTESIAN_POINT('Ctrl Pts',(0.108847916573885,2.403337369438,12.8113114049436));
#71128=CARTESIAN_POINT('Ctrl Pts',(0.108374338020282,2.40350688870952,12.8113423669312));
#71129=CARTESIAN_POINT('Ctrl Pts',(0.107376898992149,2.40386129368629,12.8114076020985));
#71130=CARTESIAN_POINT('Ctrl Pts',(0.106852953911956,2.40404593480588,12.8114418832977));
#71131=CARTESIAN_POINT('Ctrl Pts',(0.105463882693164,2.40453141713499,12.8115328066202));
#71132=CARTESIAN_POINT('Ctrl Pts',(0.10459795160515,2.40482992482228,12.8115895259406));
#71133=CARTESIAN_POINT('Ctrl Pts',(0.101989241599399,2.40571678668166,12.811760521371));
#71134=CARTESIAN_POINT('Ctrl Pts',(0.10024270933671,2.40629390797053,12.8118751669781));
#71135=CARTESIAN_POINT('Ctrl Pts',(0.094001901231711,2.40829701564943,12.8122854558636));
#71136=CARTESIAN_POINT('Ctrl Pts',(0.0894815617570456,2.40963923141877,
12.8125838071877));
#71137=CARTESIAN_POINT('Ctrl Pts',(0.0744645067125392,2.41374192445326,
12.8135791823806));
#71138=CARTESIAN_POINT('Ctrl Pts',(0.0638586331040312,2.41607118281746,
12.814289200609));
#71139=CARTESIAN_POINT('Ctrl Pts',(0.0218867343742071,2.42309020539783,
12.8171192816193));
#71140=CARTESIAN_POINT('Ctrl Pts',(-0.00998151255418595,2.42367674683068,
12.8193307300791));
#71141=CARTESIAN_POINT('Ctrl Pts',(-0.0429644068629143,2.4194020275151,
12.8214353089777));
#71142=CARTESIAN_POINT('Ctrl Pts',(-0.0445056485663049,2.41919091922345,
12.8215331775479));
#71143=CARTESIAN_POINT('Ctrl Pts',(-0.0464683924069918,2.41890758353654,
12.8216571529156));
#71144=CARTESIAN_POINT('Ctrl Pts',(-0.0468913281886851,2.4188456706241,
12.8216838283215));
#71145=CARTESIAN_POINT('Ctrl Pts',(-0.0475629123853623,2.41874599329277,
12.8217261230904));
#71146=CARTESIAN_POINT('Ctrl Pts',(-0.0478116400495858,2.4187087792195,
12.8217417735451));
#71147=CARTESIAN_POINT('Ctrl Pts',(-0.0482761745562963,2.41863872056923,
12.8217709768639));
#71148=CARTESIAN_POINT('Ctrl Pts',(-0.0484919899745699,2.41860594813111,
12.8217845336815));
#71149=CARTESIAN_POINT('Ctrl Pts',(-0.0489767604464773,2.41853182981651,
12.8218149617279));
#71150=CARTESIAN_POINT('Ctrl Pts',(-0.0492456958901408,2.41849036266061,
12.8218318259326));
#71151=CARTESIAN_POINT('Ctrl Pts',(-0.050042902983552,2.41836640739827,
12.8218817690664));
#71152=CARTESIAN_POINT('Ctrl Pts',(-0.050571025527687,2.41828294469779,
12.8219147927766));
#71153=CARTESIAN_POINT('Ctrl Pts',(-0.0547956660277045,2.41760451633553,
12.8221784831365));
#71154=CARTESIAN_POINT('Ctrl Pts',(-0.0584819597554197,2.41694645786921,
12.8224056411284));
#71155=CARTESIAN_POINT('Ctrl Pts',(-0.0730539263277228,2.41408223375931,
12.823294935386));
#71156=CARTESIAN_POINT('Ctrl Pts',(-0.0838347996316255,2.41137806557885,
12.8239337056198));
#71157=CARTESIAN_POINT('Ctrl Pts',(-0.106968868991532,2.40428627640394,
12.8253034929775));
#71158=CARTESIAN_POINT('Ctrl Pts',(-0.119237241687734,2.39969146119117,
12.8260296159695));
#71159=CARTESIAN_POINT('Ctrl Pts',(-0.150955892785231,2.38555502753493,
12.827976551957));
#71160=CARTESIAN_POINT('Ctrl Pts',(-0.16977897136329,2.37478038180383,12.8292092669971));
#71161=CARTESIAN_POINT('Ctrl Pts',(-0.187749355614054,2.36193808772033,
12.8305450328203));
#71162=CARTESIAN_POINT('Ctrl Pts',(-0.188118697275485,2.36167296013191,
12.8305725577014));
#71163=CARTESIAN_POINT('Ctrl Pts',(-0.189802615709957,2.36045877126188,
12.8306983774857));
#71164=CARTESIAN_POINT('Ctrl Pts',(-0.191110562103236,2.35950059221636,
12.8307970179876));
#71165=CARTESIAN_POINT('Ctrl Pts',(-0.192912258236908,2.35815969158861,
12.8309341887392));
#71166=CARTESIAN_POINT('Ctrl Pts',(-0.193412224332735,2.35778533164087,
12.8309723926039));
#71167=CARTESIAN_POINT('Ctrl Pts',(-0.194209892037314,2.35718443460567,
12.8310335693012));
#71168=CARTESIAN_POINT('Ctrl Pts',(-0.194508294691635,2.35695882717436,
12.8310565056299));
#71169=CARTESIAN_POINT('Ctrl Pts',(-0.195106552992748,2.35650487453366,
12.8311025918164));
#71170=CARTESIAN_POINT('Ctrl Pts',(-0.195406402230549,2.35627652183858,
12.8311257419479));
#71171=CARTESIAN_POINT('Ctrl Pts',(-0.196104018372711,2.35574331029572,
12.8311797227165));
#71172=CARTESIAN_POINT('Ctrl Pts',(-0.196501475301194,2.35543804920737,
12.8312105692095));
#71173=CARTESIAN_POINT('Ctrl Pts',(-0.197713610744413,2.35450258272397,
12.8313049244684));
#71174=CARTESIAN_POINT('Ctrl Pts',(-0.198525975564917,2.35386940239681,
12.8313685511082));
#71175=CARTESIAN_POINT('Ctrl Pts',(-0.200384007286858,2.35240682745984,
12.8315149837187));
#71176=CARTESIAN_POINT('Ctrl Pts',(-0.201427579727765,2.35157481384962,
12.8315978938301));
#71177=CARTESIAN_POINT('Ctrl Pts',(-0.204846174536465,2.3488143484801,12.831871715925));
#71178=CARTESIAN_POINT('Ctrl Pts',(-0.207198849779643,2.34685860496231,
12.8320637236145));
#71179=CARTESIAN_POINT('Ctrl Pts',(-0.216217053397281,2.33914216102917,
12.8328138924901));
#71180=CARTESIAN_POINT('Ctrl Pts',(-0.222672618073112,2.3331430229541,12.8333816911373));
#71181=CARTESIAN_POINT('Ctrl Pts',(-0.253019398119515,2.30253054713207,
12.8362062865143));
#71182=CARTESIAN_POINT('Ctrl Pts',(-0.273118277123958,2.27448031075107,
12.8386078568072));
#71183=CARTESIAN_POINT('Ctrl Pts',(-0.289939391013341,2.24074073929259,
12.8410281140105));
#71184=CARTESIAN_POINT('Ctrl Pts',(-0.291412559951727,2.23766455011192,
12.8412446440178));
#71185=CARTESIAN_POINT('Ctrl Pts',(-0.293073091696434,2.2340509570786,12.8414937203854));
#71186=CARTESIAN_POINT('Ctrl Pts',(-0.293308139926533,2.23353587995225,
12.8415290995131));
#71187=CARTESIAN_POINT('Ctrl Pts',(-0.29365679668629,2.23276648283692,12.8415817595171));
#71188=CARTESIAN_POINT('Ctrl Pts',(-0.293771433261199,2.23251263413729,
12.8415991033384));
#71189=CARTESIAN_POINT('Ctrl Pts',(-0.293975561531511,2.23205905023668,
12.8416300390852));
#71190=CARTESIAN_POINT('Ctrl Pts',(-0.294065178765829,2.23185937268792,
12.8416436387647));
#71191=CARTESIAN_POINT('Ctrl Pts',(-0.294255575961439,2.23143398624645,
12.8416725707188));
#71192=CARTESIAN_POINT('Ctrl Pts',(-0.294356299384256,2.23120825331823,
12.8416878994601));
#71193=CARTESIAN_POINT('Ctrl Pts',(-0.294627178125342,2.23059930070285,
12.8417291869347));
#71194=CARTESIAN_POINT('Ctrl Pts',(-0.29479684617357,2.23021586280102,12.8417551156541));
#71195=CARTESIAN_POINT('Ctrl Pts',(-0.295620889582056,2.22834371708293,
12.8418813837428));
#71196=CARTESIAN_POINT('Ctrl Pts',(-0.296264754027261,2.22685036796803,
12.8419810883679));
#71197=CARTESIAN_POINT('Ctrl Pts',(-0.299902736665034,2.21823378629403,
12.8425509168014));
#71198=CARTESIAN_POINT('Ctrl Pts',(-0.302651465175548,2.21100897009397,
12.8430073420929));
#71199=CARTESIAN_POINT('Ctrl Pts',(-0.316473043909679,2.17033562215885,
12.8454962606067));
#71200=CARTESIAN_POINT('Ctrl Pts',(-0.322262114102556,2.13534866200769,
12.8473676961822));
#71201=CARTESIAN_POINT('Ctrl Pts',(-0.322274978515416,2.10011767704999,
12.8494474689269));
#71202=CARTESIAN_POINT('Ctrl Pts',(-0.322274978630497,2.10011736146139,
12.8494474875569));
#71203=CARTESIAN_POINT('Ctrl Pts',(-0.322277157687331,2.09413366386358,
12.8498007202859));
#71204=CARTESIAN_POINT('Ctrl Pts',(-0.322112687808582,2.08815130524338,
12.8501585781565));
#71205=CARTESIAN_POINT('Ctrl Pts',(-0.321727601263438,2.08119876450792,
12.8505811569999));
#71206=CARTESIAN_POINT('Ctrl Pts',(-0.321668946773117,2.08022060365881,
12.8506407635404));
#71207=CARTESIAN_POINT('Ctrl Pts',(-0.321568342069809,2.07866186951974,
12.8507359989904));
#71208=CARTESIAN_POINT('Ctrl Pts',(-0.321529278176364,2.07808111083284,
12.8507715375699));
#71209=CARTESIAN_POINT('Ctrl Pts',(-0.321459594655213,2.07708542538063,
12.8508325631538));
#71210=CARTESIAN_POINT('Ctrl Pts',(-0.321429744388672,2.07667044480597,
12.8508580260017));
#71211=CARTESIAN_POINT('Ctrl Pts',(-0.321372111330502,2.07589033860108,
12.8509059470247));
#71212=CARTESIAN_POINT('Ctrl Pts',(-0.321344509635997,2.07552519992233,
12.8509283994817));
#71213=CARTESIAN_POINT('Ctrl Pts',(-0.321285723178165,2.07476476795226,
12.8509752056234));
#71214=CARTESIAN_POINT('Ctrl Pts',(-0.321254431084157,2.0743694837902,12.8509995626424));
#71215=CARTESIAN_POINT('Ctrl Pts',(-0.321180657881334,2.07345893885342,
12.8510557309639));
#71216=CARTESIAN_POINT('Ctrl Pts',(-0.321137666298163,2.07294372155164,
12.8510875582589));
#71217=CARTESIAN_POINT('Ctrl Pts',(-0.321019430216105,2.07156675677206,
12.8511727419246));
#71218=CARTESIAN_POINT('Ctrl Pts',(-0.320941956002435,2.07070520949559,
12.8512261682936));
#71219=CARTESIAN_POINT('Ctrl Pts',(-0.320379828768282,2.06472415556308,
12.8515979688614));
#71220=CARTESIAN_POINT('Ctrl Pts',(-0.319776194024506,2.05961682662829,
12.8519200698964));
#71221=CARTESIAN_POINT('Ctrl Pts',(-0.318737431477237,2.0523286962274,12.8523866777551));
#71222=CARTESIAN_POINT('Ctrl Pts',(-0.318401512203134,2.05013437991286,
12.8525280721608));
#71223=CARTESIAN_POINT('Ctrl Pts',(-0.312433322235896,2.01367111492903,
12.8548928874559));
#71224=CARTESIAN_POINT('Ctrl Pts',(-0.301320101473062,1.98053248647146,
12.8573024756047));
#71225=CARTESIAN_POINT('Ctrl Pts',(-0.28226851332567,1.94436033833722,12.8600043028669));
#71226=CARTESIAN_POINT('Ctrl Pts',(-0.279237977056343,1.93898639626217,
12.8604067311897));
#71227=CARTESIAN_POINT('Ctrl Pts',(-0.274566052596327,1.93123097769794,
12.8609855525643));
#71228=CARTESIAN_POINT('Ctrl Pts',(-0.273044059269899,1.92877954782531,
12.861168215415));
#71229=CARTESIAN_POINT('Ctrl Pts',(-0.271219685736593,1.92592729094785,
12.8613800891526));
#71230=CARTESIAN_POINT('Ctrl Pts',(-0.270949103052731,1.92550641980074,
12.8614113356884));
#71231=CARTESIAN_POINT('Ctrl Pts',(-0.270533758567627,1.92486367801339,
12.8614590263761));
#71232=CARTESIAN_POINT('Ctrl Pts',(-0.270389703072263,1.92464135528173,
12.8614755173072));
#71233=CARTESIAN_POINT('Ctrl Pts',(-0.270138213209825,1.92425427437457,
12.8615042199367));
#71234=CARTESIAN_POINT('Ctrl Pts',(-0.270030902462749,1.92408943741881,
12.8615164398667));
#71235=CARTESIAN_POINT('Ctrl Pts',(-0.269804772373784,1.92374277999112,
12.8615421324718));
#71236=CARTESIAN_POINT('Ctrl Pts',(-0.269685920506403,1.92356098197335,
12.8615556028591));
#71237=CARTESIAN_POINT('Ctrl Pts',(-0.269351525527247,1.92305061249473,
12.8615934091016));
#71238=CARTESIAN_POINT('Ctrl Pts',(-0.269135564180713,1.92272231347581,
12.861617716871));
#71239=CARTESIAN_POINT('Ctrl Pts',(-0.268248633699049,1.92137938019784,
12.8617171066464));
#71240=CARTESIAN_POINT('Ctrl Pts',(-0.267572511905333,1.92036813678199,
12.8617918472915));
#71241=CARTESIAN_POINT('Ctrl Pts',(-0.255645037439752,1.90274554798675,
12.8630930075478));
#71242=CARTESIAN_POINT('Ctrl Pts',(-0.242870450672732,1.88721393156759,
12.8642206172097));
#71243=CARTESIAN_POINT('Ctrl Pts',(-0.2173039605043,1.86145579718763,12.8662511534273));
#71244=CARTESIAN_POINT('Ctrl Pts',(-0.205022964154451,1.85082154520588,
12.8671528932526));
#71245=CARTESIAN_POINT('Ctrl Pts',(-0.184544572071718,1.8356318740856,12.8686159991174));
#71246=CARTESIAN_POINT('Ctrl Pts',(-0.176860460505816,1.83043078686845,
12.8691567479731));
#71247=CARTESIAN_POINT('Ctrl Pts',(-0.166366454361655,1.82396978826265,
12.8698914989739));
#71248=CARTESIAN_POINT('Ctrl Pts',(-0.163747198520407,1.82240798110385,
12.8700745758402));
#71249=CARTESIAN_POINT('Ctrl Pts',(-0.159953089300008,1.82021801769047,
12.8703395129879));
#71250=CARTESIAN_POINT('Ctrl Pts',(-0.158795839397795,1.81955957903782,
12.8704202877841));
#71251=CARTESIAN_POINT('Ctrl Pts',(-0.156737349697347,1.8184051900843,12.8705639241158));
#71252=CARTESIAN_POINT('Ctrl Pts',(-0.15583774805245,1.81790634532998,12.8706266813033));
#71253=CARTESIAN_POINT('Ctrl Pts',(-0.154496907438959,1.81717119714039,
12.870720203657));
#71254=CARTESIAN_POINT('Ctrl Pts',(-0.154057475223261,1.81693159756241,
12.8707508510653));
#71255=CARTESIAN_POINT('Ctrl Pts',(-0.153285996960608,1.81651327904887,
12.870804652661));
#71256=CARTESIAN_POINT('Ctrl Pts',(-0.152954191241553,1.81633411696238,
12.8708277910155));
#71257=CARTESIAN_POINT('Ctrl Pts',(-0.15229235410508,1.8159782496852,12.8708739419111));
#71258=CARTESIAN_POINT('Ctrl Pts',(-0.151962327679417,1.8158015363603,12.8708969541191));
#71259=CARTESIAN_POINT('Ctrl Pts',(-0.151171356612527,1.81537978096935,
12.8709521051751));
#71260=CARTESIAN_POINT('Ctrl Pts',(-0.15071012412062,1.81513528364581,12.8709842632768));
#71261=CARTESIAN_POINT('Ctrl Pts',(-0.14904455937368,1.8142575524176,12.8711003854084));
#71262=CARTESIAN_POINT('Ctrl Pts',(-0.14783682672451,1.8136308333598,12.8711845792833));
#71263=CARTESIAN_POINT('Ctrl Pts',(-0.12924950651635,1.80413438370041,12.8724803171443));
#71264=CARTESIAN_POINT('Ctrl Pts',(-0.111106876040193,1.7968549693569,12.8737485197718));
#71265=CARTESIAN_POINT('Ctrl Pts',(-0.0845216063084188,1.78889671070481,
12.8756042866134));
#71266=CARTESIAN_POINT('Ctrl Pts',(-0.0765351409159154,1.7868362678772,
12.8761608906105));
#71267=CARTESIAN_POINT('Ctrl Pts',(-0.0660581444609805,1.78455803493682,
12.8768862749059));
#71268=CARTESIAN_POINT('Ctrl Pts',(-0.0636315990035245,1.78405960787905,
12.87705393976));
#71269=CARTESIAN_POINT('Ctrl Pts',(-0.0583702570241278,1.78304196951893,
12.87741653011));
#71270=CARTESIAN_POINT('Ctrl Pts',(-0.0555337376611356,1.78253270384031,
12.8776114202096));
#71271=CARTESIAN_POINT('Ctrl Pts',(-0.0492488346375455,1.78149113023244,
12.8780415504108));
#71272=CARTESIAN_POINT('Ctrl Pts',(-0.0457978278428185,1.78097663492912,
12.8782766157209));
#71273=CARTESIAN_POINT('Ctrl Pts',(-0.0324390850201182,1.77920627642581,
12.87918091445));
#71274=CARTESIAN_POINT('Ctrl Pts',(-0.0224825201446892,1.77835504281546,
12.8798431302006));
#71275=CARTESIAN_POINT('Ctrl Pts',(-0.00871348195573289,1.77782051088361,
12.8807296079082));
#71276=CARTESIAN_POINT('Ctrl Pts',(-0.00492273681241625,1.77774029453169,
12.8809705905321));
#71277=CARTESIAN_POINT('Ctrl Pts',(-0.000595009464524741,1.77772510312494,
12.8812415387497));
#71278=CARTESIAN_POINT('Ctrl Pts',(-5.87514730183204E-5,1.77772455918855,
12.8812750394004));
#71279=CARTESIAN_POINT('Ctrl Pts',(0.000749948505829715,1.7777257574283,
12.8813254469954));
#71280=CARTESIAN_POINT('Ctrl Pts',(0.00102238764228161,1.77772650656197,
12.8813424092646));
#71281=CARTESIAN_POINT('Ctrl Pts',(0.00151113897232835,1.77772847026807,
12.8813728042586));
#71282=CARTESIAN_POINT('Ctrl Pts',(0.00172745041171609,1.77772955715307,
12.8813862441318));
#71283=CARTESIAN_POINT('Ctrl Pts',(0.002194282367126,1.77773237284469,12.8814152226764));
#71284=CARTESIAN_POINT('Ctrl Pts',(0.00244480127400739,1.77773417597397,
12.8814307570786));
#71285=CARTESIAN_POINT('Ctrl Pts',(0.00311858829100794,1.77773981133,12.8814724940126));
#71286=CARTESIAN_POINT('Ctrl Pts',(0.00354185321747487,1.77774418535084,
12.8814986661032));
#71287=CARTESIAN_POINT('Ctrl Pts',(0.00548104204343319,1.77776804597079,
12.881618365286));
#71288=CARTESIAN_POINT('Ctrl Pts',(0.00699685732786645,1.77779739569885,
12.8817113479611));
#71289=CARTESIAN_POINT('Ctrl Pts',(0.0398515981020691,1.77866551064822,
12.8837151565225));
#71290=CARTESIAN_POINT('Ctrl Pts',(0.0709081183332139,1.78406201212841,
12.8853935030414));
#71291=CARTESIAN_POINT('Ctrl Pts',(0.112837519840646,1.79785413207552,12.887891218246));
#71292=CARTESIAN_POINT('Ctrl Pts',(0.124725617504497,1.80256445550007,12.8886259628782));
#71293=CARTESIAN_POINT('Ctrl Pts',(0.139682723273527,1.80954547471785,12.8896051691714));
#71294=CARTESIAN_POINT('Ctrl Pts',(0.143035650505402,1.81118189909493,12.8898283401935));
#71295=CARTESIAN_POINT('Ctrl Pts',(0.147737075016866,1.81357841606296,12.8901468478925));
#71296=CARTESIAN_POINT('Ctrl Pts',(0.149109743929759,1.81429061755591,12.8902405253662));
#71297=CARTESIAN_POINT('Ctrl Pts',(0.151190517514351,1.81538929449036,12.8903835933802));
#71298=CARTESIAN_POINT('Ctrl Pts',(0.15190239764257,1.81576860157805,12.8904327315421));
#71299=CARTESIAN_POINT('Ctrl Pts',(0.15306179238086,1.81639195505095,12.8905130757969));
#71300=CARTESIAN_POINT('Ctrl Pts',(0.153510168181661,1.81663439921752,12.8905442250222));
#71301=CARTESIAN_POINT('Ctrl Pts',(0.154372654682901,1.81710340770834,12.8906042933358));
#71302=CARTESIAN_POINT('Ctrl Pts',(0.154786846765385,1.8173298202697,12.8906332069651));
#71303=CARTESIAN_POINT('Ctrl Pts',(0.155536841321006,1.81774193746432,12.8906856843163));
#71304=CARTESIAN_POINT('Ctrl Pts',(0.155872812971644,1.81792733374395,12.8907092369769));
#71305=CARTESIAN_POINT('Ctrl Pts',(0.156598171317104,1.8183292935229,12.8907601837709));
#71306=CARTESIAN_POINT('Ctrl Pts',(0.156987441225676,1.81854606515202,12.8907875853327));
#71307=CARTESIAN_POINT('Ctrl Pts',(0.158038841204687,1.81913441509601,12.8908617602436));
#71308=CARTESIAN_POINT('Ctrl Pts',(0.158700106669771,1.81950752551983,12.8909085886042));
#71309=CARTESIAN_POINT('Ctrl Pts',(0.161647746115612,1.82118445299271,12.8911181268885));
#71310=CARTESIAN_POINT('Ctrl Pts',(0.163919362967305,1.82251388348162,12.8912817597874));
#71311=CARTESIAN_POINT('Ctrl Pts',(0.166811989138186,1.8242546651879,12.8914929586836));
#71312=CARTESIAN_POINT('Ctrl Pts',(0.167448254239965,1.82464057755743,12.8915395919473));
#71313=CARTESIAN_POINT('Ctrl Pts',(0.168890448138891,1.82552215507232,12.8916456997064));
#71314=CARTESIAN_POINT('Ctrl Pts',(0.169695539466153,1.82601917095657,12.8917052230982));
#71315=CARTESIAN_POINT('Ctrl Pts',(0.171063780029292,1.82687218624442,12.8918068794288));
#71316=CARTESIAN_POINT('Ctrl Pts',(0.171628038678842,1.82722640191287,12.8918489472837));
#71317=CARTESIAN_POINT('Ctrl Pts',(0.173716281414955,1.82854634950647,12.8920051748721));
#71318=CARTESIAN_POINT('Ctrl Pts',(0.175233224067756,1.82952311047368,12.8921197327936));
#71319=CARTESIAN_POINT('Ctrl Pts',(0.200294103798603,1.84595915003484,12.8940302719698));
#71320=CARTESIAN_POINT('Ctrl Pts',(0.221716286517478,1.86442455988885,12.8959445343833));
#71321=CARTESIAN_POINT('Ctrl Pts',(0.243047976389121,1.88833057736983,12.8981054330911));
#71322=CARTESIAN_POINT('Ctrl Pts',(0.245581536936684,1.89127536535079,12.8983666593293));
#71323=CARTESIAN_POINT('Ctrl Pts',(0.255224790608973,1.90290256154339,12.8993772063056));
#71324=CARTESIAN_POINT('Ctrl Pts',(0.261933149392528,1.91190912712761,12.9001160680041));
#71325=CARTESIAN_POINT('Ctrl Pts',(0.2687264808695,1.92210030192945,12.9008908603931));
#71326=CARTESIAN_POINT('Ctrl Pts',(0.269290364576245,1.92295502349478,12.9009553889674));
#71327=CARTESIAN_POINT('Ctrl Pts',(0.270256311907252,1.92443447551816,12.9010662844528));
#71328=CARTESIAN_POINT('Ctrl Pts',(0.270660302836582,1.92505792956902,12.9011127740866));
#71329=CARTESIAN_POINT('Ctrl Pts',(0.271230516609302,1.92594460827455,12.9011785418412));
#71330=CARTESIAN_POINT('Ctrl Pts',(0.271398515562288,1.92620667941089,12.9011979372766));
#71331=CARTESIAN_POINT('Ctrl Pts',(0.27168666666379,1.92665761946614,12.9012312358004));
#71332=CARTESIAN_POINT('Ctrl Pts',(0.271807002015925,1.9268463705599,12.9012451511724));
#71333=CARTESIAN_POINT('Ctrl Pts',(0.272037289502212,1.92720841783902,12.9012717992586));
#71334=CARTESIAN_POINT('Ctrl Pts',(0.27214727258354,1.92738169340612,12.9012845340714));
#71335=CARTESIAN_POINT('Ctrl Pts',(0.272406299548407,1.9277906467436,12.9013145455612));
#71336=CARTESIAN_POINT('Ctrl Pts',(0.272555203505363,1.92802641358001,12.9013318128729));
#71337=CARTESIAN_POINT('Ctrl Pts',(0.272995129773377,1.92872497666683,12.9013828731749));
#71338=CARTESIAN_POINT('Ctrl Pts',(0.273285282561672,1.92918832345746,12.9014166087903));
#71339=CARTESIAN_POINT('Ctrl Pts',(0.275857892501965,1.9333198750419,12.9017162692713));
#71340=CARTESIAN_POINT('Ctrl Pts',(0.278067685846616,1.93703310936577,12.9019775225503));
#71341=CARTESIAN_POINT('Ctrl Pts',(0.28044889711628,1.94122392825339,12.9022647791911));
#71342=CARTESIAN_POINT('Ctrl Pts',(0.280694517744455,1.94165855701322,12.9022944806215));
#71343=CARTESIAN_POINT('Ctrl Pts',(0.294163787079987,1.96562242778806,12.903927265826));
#71344=CARTESIAN_POINT('Ctrl Pts',(0.304381950305955,1.99072201990376,12.90538805438));
#71345=CARTESIAN_POINT('Ctrl Pts',(0.315729411381623,2.03318887370769,12.9078708907702));
#71346=CARTESIAN_POINT('Ctrl Pts',(0.318806771259509,2.04989096725383,12.9088485122852));
#71347=CARTESIAN_POINT('Ctrl Pts',(0.320731476990113,2.06845011375563,12.9099731445066));
#71348=CARTESIAN_POINT('Ctrl Pts',(0.320893710396938,2.07014531675932,12.9100761964332));
#71349=CARTESIAN_POINT('Ctrl Pts',(0.321118124014856,2.07270393401074,12.9102322595821));
#71350=CARTESIAN_POINT('Ctrl Pts',(0.321190275055793,2.07356646115116,12.910284959171));
#71351=CARTESIAN_POINT('Ctrl Pts',(0.321301357494795,2.07496204964271,12.9103703771467));
#71352=CARTESIAN_POINT('Ctrl Pts',(0.32134243928868,2.07549493944714,12.9104030281167));
#71353=CARTESIAN_POINT('Ctrl Pts',(0.32141863229049,2.07651642280567,12.9104656841865));
#71354=CARTESIAN_POINT('Ctrl Pts',(0.321453955529854,2.07700499942695,12.9104956825531));
#71355=CARTESIAN_POINT('Ctrl Pts',(0.321515095938439,2.07787834939146,12.9105493599422));
#71356=CARTESIAN_POINT('Ctrl Pts',(0.32154133670542,2.07826309291672,12.9105730256186));
#71357=CARTESIAN_POINT('Ctrl Pts',(0.321592073877392,2.07902720418058,12.9106200639299));
#71358=CARTESIAN_POINT('Ctrl Pts',(0.321616589725816,2.07940657006584,12.9106434359165));
#71359=CARTESIAN_POINT('Ctrl Pts',(0.321674517098838,2.08032829581913,12.910700266758));
#71360=CARTESIAN_POINT('Ctrl Pts',(0.321707228177452,2.08087069711788,12.9107337475446));
#71361=CARTESIAN_POINT('Ctrl Pts',(0.321824814402479,2.08290611873595,12.9108595320774));
#71362=CARTESIAN_POINT('Ctrl Pts',(0.321900668006174,2.08439962314418,12.9109521183478));
#71363=CARTESIAN_POINT('Ctrl Pts',(0.323069003507011,2.11106581421381,12.9126105730301));
#71364=CARTESIAN_POINT('Ctrl Pts',(0.321215879903872,2.13627496294571,12.9142740319504));
#71365=CARTESIAN_POINT('Ctrl Pts',(0.313471287372211,2.17644765881876,12.9170373232934));
#71366=CARTESIAN_POINT('Ctrl Pts',(0.309367967216245,2.19165142605742,12.9181078675751));
#71367=CARTESIAN_POINT('Ctrl Pts',(0.302070279286985,2.21249503317324,12.9195691186867));
#71368=CARTESIAN_POINT('Ctrl Pts',(0.299792429553495,2.21843182278065,12.9199843751127));
#71369=CARTESIAN_POINT('Ctrl Pts',(0.296188326555408,2.22705342063701,12.9205822185144));
#71370=CARTESIAN_POINT('Ctrl Pts',(0.294998055359448,2.22979308681931,12.9207713987382));
#71371=CARTESIAN_POINT('Ctrl Pts',(0.293562153519512,2.2329762862353,12.9209899360706));
#71372=CARTESIAN_POINT('Ctrl Pts',(0.293353407372075,2.23343616103362,12.9210214767567));
#71373=CARTESIAN_POINT('Ctrl Pts',(0.293033102718043,2.23413741850574,12.9210695228396));
#71374=CARTESIAN_POINT('Ctrl Pts',(0.292922326263744,2.23437915429638,12.9210860760938));
#71375=CARTESIAN_POINT('Ctrl Pts',(0.292729050111147,2.23479954588023,12.9211148469356));
#71376=CARTESIAN_POINT('Ctrl Pts',(0.292646686195391,2.23497826272417,12.921127072887));
#71377=CARTESIAN_POINT('Ctrl Pts',(0.292459954606125,2.2353824667857,12.921154712731));
#71378=CARTESIAN_POINT('Ctrl Pts',(0.292355490042023,2.23560790834051,12.9211701204974));
#71379=CARTESIAN_POINT('Ctrl Pts',(0.29207161504631,2.23621867703564,12.9212118419233));
#71380=CARTESIAN_POINT('Ctrl Pts',(0.29189170206523,2.23660377212756,12.9212381244719));
#71381=CARTESIAN_POINT('Ctrl Pts',(0.29107934984364,2.23833364053522,12.9213560877753));
#71382=CARTESIAN_POINT('Ctrl Pts',(0.290438362544747,2.23967441344406,12.9214472474941));
#71383=CARTESIAN_POINT('Ctrl Pts',(0.275645797984994,2.27007429276252,12.9235090522467));
#71384=CARTESIAN_POINT('Ctrl Pts',(0.25720920743113,2.29685052668868,12.9252328109758));
#71385=CARTESIAN_POINT('Ctrl Pts',(0.229675995362771,2.3262140827988,12.9275162367858));
#71386=CARTESIAN_POINT('Ctrl Pts',(0.224049101353253,2.3317884015734,12.927970245729));
#71387=CARTESIAN_POINT('Ctrl Pts',(0.211991142975801,2.34288402396529,12.9289259451313));
#71388=CARTESIAN_POINT('Ctrl Pts',(0.20553625112613,2.34837013561412,12.929428390533));
#71389=CARTESIAN_POINT('Ctrl Pts',(0.197977583342984,2.354297753848,12.9300104017628));
#71390=CARTESIAN_POINT('Ctrl Pts',(0.197078240135899,2.35499536923611,12.9300795501089));
#71391=CARTESIAN_POINT('Ctrl Pts',(0.195662132064026,2.3560818696166,12.9301882834839));
#71392=CARTESIAN_POINT('Ctrl Pts',(0.195147854129657,2.35647399261758,12.9302277411017));
#71393=CARTESIAN_POINT('Ctrl Pts',(0.194279705206705,2.35713180975134,12.9302942999217));
#71394=CARTESIAN_POINT('Ctrl Pts',(0.193926459447994,2.35739832898465,12.9303213687203));
#71395=CARTESIAN_POINT('Ctrl Pts',(0.19323351400758,2.35791891096481,12.9303744421324));
#71396=CARTESIAN_POINT('Ctrl Pts',(0.192893859306704,2.35817303230204,12.9304004443816));
#71397=CARTESIAN_POINT('Ctrl Pts',(0.192245273869495,2.35865629364737,12.9304500739471));
#71398=CARTESIAN_POINT('Ctrl Pts',(0.191936432483957,2.35888555280634,12.930473696555));
#71399=CARTESIAN_POINT('Ctrl Pts',(0.191223781576466,2.35941259167593,12.9305281834365));
#71400=CARTESIAN_POINT('Ctrl Pts',(0.190819686370547,2.35970998180534,12.9305590627908));
#71401=CARTESIAN_POINT('Ctrl Pts',(0.189616597940501,2.36059105988883,12.9306509505075));
#71402=CARTESIAN_POINT('Ctrl Pts',(0.188815614676009,2.36117200908226,12.93071206475));
#71403=CARTESIAN_POINT('Ctrl Pts',(0.183243356321864,2.36517450873392,12.9311368122169));
#71404=CARTESIAN_POINT('Ctrl Pts',(0.178382299333618,2.3684686120969,12.9315053016902));
#71405=CARTESIAN_POINT('Ctrl Pts',(0.171725692425987,2.37271885039723,12.9320076557367));
#71406=CARTESIAN_POINT('Ctrl Pts',(0.170006928891879,2.37379358764576,12.9321371667537));
#71407=CARTESIAN_POINT('Ctrl Pts',(0.165321328749332,2.3766623467054,12.9324897059705));
#71408=CARTESIAN_POINT('Ctrl Pts',(0.162335556255635,2.37842478625113,12.9327137894189));
#71409=CARTESIAN_POINT('Ctrl Pts',(0.153310501969327,2.38355756523765,12.9333893952023));
#71410=CARTESIAN_POINT('Ctrl Pts',(0.147190819574099,2.3867818960783,12.9338452778013));
#71411=CARTESIAN_POINT('Ctrl Pts',(0.123092617714442,2.3985041314876,12.9356292427549));
#71412=CARTESIAN_POINT('Ctrl Pts',(0.104447471556289,2.40552769177142,12.9369892070315));
#71413=CARTESIAN_POINT('Ctrl Pts',(0.0742451370356756,2.4138146673319,12.9390857024458));
#71414=CARTESIAN_POINT('Ctrl Pts',(0.0630609392872428,2.41625205712724,
12.9398393956297));
#71415=CARTESIAN_POINT('Ctrl Pts',(0.050222332347642,2.4183415627825,12.9406623620609));
#71416=CARTESIAN_POINT('Ctrl Pts',(0.0486731518091858,2.41858210525885,
12.9407609709017));
#71417=CARTESIAN_POINT('Ctrl Pts',(0.0467126612951205,2.41887187759347,
12.9408848300887));
#71418=CARTESIAN_POINT('Ctrl Pts',(0.0463029627783074,2.41893162697948,
12.9409106625966));
#71419=CARTESIAN_POINT('Ctrl Pts',(0.0456496480063069,2.41902561931791,
12.9409517727443));
#71420=CARTESIAN_POINT('Ctrl Pts',(0.0454061074671507,2.41906037289192,
12.9409670792816));
#71421=CARTESIAN_POINT('Ctrl Pts',(0.0449456108270473,2.41912554847158,
12.9409959864923));
#71422=CARTESIAN_POINT('Ctrl Pts',(0.0447286652909905,2.41915602786332,
12.9410095902974));
#71423=CARTESIAN_POINT('Ctrl Pts',(0.0442338934213134,2.41922502559751,
12.9410405821166));
#71424=CARTESIAN_POINT('Ctrl Pts',(0.0439560482497025,2.41926340241036,
12.9410579619841));
#71425=CARTESIAN_POINT('Ctrl Pts',(0.043107552813163,2.41937947052273,12.9411109651706));
#71426=CARTESIAN_POINT('Ctrl Pts',(0.0425367401493403,2.41945599548373,
12.9411465226073));
#71427=CARTESIAN_POINT('Ctrl Pts',(0.0383914749090107,2.42000041541923,
12.9414040388614));
#71428=CARTESIAN_POINT('Ctrl Pts',(0.0348094222584036,2.42040985936664,
12.9416227722865));
#71429=CARTESIAN_POINT('Ctrl Pts',(0.000411766580830305,2.42375795348819,
12.9436933755305));
#71430=CARTESIAN_POINT('Ctrl Pts',(-0.0306731658353331,2.42230288530457,
12.945348481072));
#71431=CARTESIAN_POINT('Ctrl Pts',(-0.0753521971415159,2.41367913817677,
12.9479372907939));
#71432=CARTESIAN_POINT('Ctrl Pts',(-0.0894230777536805,2.40996126869124,
12.9487824051948));
#71433=CARTESIAN_POINT('Ctrl Pts',(-0.104672267532592,2.40480703306695,
12.9497538429676));
#71434=CARTESIAN_POINT('Ctrl Pts',(-0.106146999728627,2.40429660746455,
12.9498483677315));
#71435=CARTESIAN_POINT('Ctrl Pts',(-0.108728432369929,2.40338208841053,
12.9500148718208));
#71436=CARTESIAN_POINT('Ctrl Pts',(-0.10983674049928,2.402982596782,12.9500866983085));
#71437=CARTESIAN_POINT('Ctrl Pts',(-0.11144183488985,2.40239407327635,12.950191222956));
#71438=CARTESIAN_POINT('Ctrl Pts',(-0.111940392140116,2.40220987197385,
12.9502237599366));
#71439=CARTESIAN_POINT('Ctrl Pts',(-0.112810921385648,2.40188578895137,
12.9502806971259));
#71440=CARTESIAN_POINT('Ctrl Pts',(-0.113183095571158,2.40174645056622,
12.9503050791269));
#71441=CARTESIAN_POINT('Ctrl Pts',(-0.113902612477554,2.40147555199565,
12.9503522939031));
#71442=CARTESIAN_POINT('Ctrl Pts',(-0.114249987550027,2.40134407895846,
12.9503751237288));
#71443=CARTESIAN_POINT('Ctrl Pts',(-0.115074660855946,2.40103032919098,
12.9504294057162));
#71444=CARTESIAN_POINT('Ctrl Pts',(-0.115551753352763,2.40084751778309,
12.9504608757788));
#71445=CARTESIAN_POINT('Ctrl Pts',(-0.117235533185718,2.40019773407506,
12.9505721787253));
#71446=CARTESIAN_POINT('Ctrl Pts',(-0.118439828680841,2.39972463477145,
12.9506522173366));
#71447=CARTESIAN_POINT('Ctrl Pts',(-0.137719387956688,2.39201645069858,
12.9519405801952));
#71448=CARTESIAN_POINT('Ctrl Pts',(-0.155101938164828,2.38316669458161,
12.9532053397036));
#71449=CARTESIAN_POINT('Ctrl Pts',(-0.180657036723986,2.36709410512825,
12.9552235066925));
#71450=CARTESIAN_POINT('Ctrl Pts',(-0.189445653652415,2.3609340064727,12.9559495443048));
#71451=CARTESIAN_POINT('Ctrl Pts',(-0.206554494301615,2.34762143483849,
12.95741637958));
#71452=CARTESIAN_POINT('Ctrl Pts',(-0.214850421600092,2.34045883595795,
12.9581562309807));
#71453=CARTESIAN_POINT('Ctrl Pts',(-0.227332226951529,2.32851950677843,
12.9592992967429));
#71454=CARTESIAN_POINT('Ctrl Pts',(-0.231769493215158,2.32401789996387,
12.9597122005932));
#71455=CARTESIAN_POINT('Ctrl Pts',(-0.238154782776612,2.31714704163497,
12.9603126100037));
#71456=CARTESIAN_POINT('Ctrl Pts',(-0.240205834826079,2.31487600342673,
12.9605064820318));
#71457=CARTESIAN_POINT('Ctrl Pts',(-0.242559588025475,2.31219396841813,
12.9607298057502));
#71458=CARTESIAN_POINT('Ctrl Pts',(-0.242893955028742,2.31181114369888,
12.9607615505944));
#71459=CARTESIAN_POINT('Ctrl Pts',(-0.243402317259382,2.31122632092448,
12.9608098431944));
#71460=CARTESIAN_POINT('Ctrl Pts',(-0.2435769678993,2.31102489760392,12.9608264395624));
#71461=CARTESIAN_POINT('Ctrl Pts',(-0.243880143105038,2.31067436999814,
12.9608552577744));
#71462=CARTESIAN_POINT('Ctrl Pts',(-0.244008780667505,2.31052536505823,
12.9608674880737));
#71463=CARTESIAN_POINT('Ctrl Pts',(-0.244299150901746,2.31018839639859,
12.9608951012756));
#71464=CARTESIAN_POINT('Ctrl Pts',(-0.244460802874286,2.3100003642163,12.9609104781251));
#71465=CARTESIAN_POINT('Ctrl Pts',(-0.244897492637309,2.3094912229207,12.9609520297055));
#71466=CARTESIAN_POINT('Ctrl Pts',(-0.245172117019421,2.3091697574266,12.9609781737569));
#71467=CARTESIAN_POINT('Ctrl Pts',(-0.24639591699617,2.30773149944604,12.9610947426073));
#71468=CARTESIAN_POINT('Ctrl Pts',(-0.247338119466721,2.30660875737659,
12.961184661275));
#71469=CARTESIAN_POINT('Ctrl Pts',(-0.269052163456808,2.28037256063258,
12.9632620238983));
#71470=CARTESIAN_POINT('Ctrl Pts',(-0.285907091027176,2.25225412224008,
12.9649983267579));
#71471=CARTESIAN_POINT('Ctrl Pts',(-0.304652152001445,2.20645749369945,
12.9678073309816));
#71472=CARTESIAN_POINT('Ctrl Pts',(-0.309808454080694,2.19035888983947,
12.9687887190482));
#71473=CARTESIAN_POINT('Ctrl Pts',(-0.313949349887022,2.17278982378761,
12.9698861890681));
#71474=CARTESIAN_POINT('Ctrl Pts',(-0.314212316438326,2.1716461644679,12.9699577362798));
#71475=CARTESIAN_POINT('Ctrl Pts',(-0.314585112885802,2.16998331202528,
12.970061928334));
#71476=CARTESIAN_POINT('Ctrl Pts',(-0.314699918027856,2.16946523446546,
12.9700944134444));
#71477=CARTESIAN_POINT('Ctrl Pts',(-0.314898432643307,2.16855881098179,
12.9701512902924));
#71478=CARTESIAN_POINT('Ctrl Pts',(-0.314982704799778,2.16817058837342,
12.9701756639382));
#71479=CARTESIAN_POINT('Ctrl Pts',(-0.315144426671496,2.16741887043298,
12.9702228847172));
#71480=CARTESIAN_POINT('Ctrl Pts',(-0.315221965889312,2.16705539479896,
12.9702457289421));
#71481=CARTESIAN_POINT('Ctrl Pts',(-0.315404789360231,2.16619105996187,
12.9703000800952));
#71482=CARTESIAN_POINT('Ctrl Pts',(-0.315509509331421,2.16569008362661,
12.970331605031));
#71483=CARTESIAN_POINT('Ctrl Pts',(-0.315875818968115,2.16391658901139,
12.9704432867336));
#71484=CARTESIAN_POINT('Ctrl Pts',(-0.31613090436578,2.16264275365301,12.970523651071));
#71485=CARTESIAN_POINT('Ctrl Pts',(-0.32031961774128,2.14104794318442,12.9718886281106));
#71486=CARTESIAN_POINT('Ctrl Pts',(-0.322293545820142,2.12040010805891,
12.9732374354274));
#71487=CARTESIAN_POINT('Ctrl Pts',(-0.322249124175129,2.07118859678447,
12.9765363794684));
#71488=CARTESIAN_POINT('Ctrl Pts',(-0.318437719932902,2.04279737836198,
12.978511553746));
#71489=CARTESIAN_POINT('Ctrl Pts',(-0.310548662491574,2.01384366776017,
12.9804093387725));
#71490=CARTESIAN_POINT('Ctrl Pts',(-0.310147947802387,2.01241212391825,
12.9805028263917));
#71491=CARTESIAN_POINT('Ctrl Pts',(-0.30961991595704,2.01057481353525,12.9806223242202));
#71492=CARTESIAN_POINT('Ctrl Pts',(-0.309501689790216,2.01016648535517,
12.9806488505687));
#71493=CARTESIAN_POINT('Ctrl Pts',(-0.309313077612012,2.00951985087926,
12.9806908073958));
#71494=CARTESIAN_POINT('Ctrl Pts',(-0.309243223852495,2.00928139182592,
12.9807062688572));
#71495=CARTESIAN_POINT('Ctrl Pts',(-0.309117555490014,2.00885423083842,
12.980733945671));
#71496=CARTESIAN_POINT('Ctrl Pts',(-0.309061844247845,2.00866550061113,
12.9807461669712));
#71497=CARTESIAN_POINT('Ctrl Pts',(-0.308930448566064,2.00822187475915,
12.9807748777869));
#71498=CARTESIAN_POINT('Ctrl Pts',(-0.308854621623009,2.00796702206663,
12.9807913588126));
#71499=CARTESIAN_POINT('Ctrl Pts',(-0.30863387743126,2.00722845096755,12.9808390853883));
#71500=CARTESIAN_POINT('Ctrl Pts',(-0.308488137770651,2.00674497616145,
12.9808702828592));
#71501=CARTESIAN_POINT('Ctrl Pts',(-0.307472972036128,2.00340570121056,
12.9810854615992));
#71502=CARTESIAN_POINT('Ctrl Pts',(-0.306565002898372,2.00056163905591,
12.9812672283599));
#71503=CARTESIAN_POINT('Ctrl Pts',(-0.303600862136323,1.99170373464854,
12.9818298258549));
#71504=CARTESIAN_POINT('Ctrl Pts',(-0.301406146446895,1.98573753646431,
12.9822036480554));
#71505=CARTESIAN_POINT('Ctrl Pts',(-0.293176851667434,1.96525773677546,
12.9834815315278));
#71506=CARTESIAN_POINT('Ctrl Pts',(-0.286258289494841,1.95112286813672,
12.9843548423626));
#71507=CARTESIAN_POINT('Ctrl Pts',(-0.271043546283658,1.92505475481123,
12.9860425186791));
#71508=CARTESIAN_POINT('Ctrl Pts',(-0.262918938531272,1.91306676206004,
12.9868541882073));
#71509=CARTESIAN_POINT('Ctrl Pts',(-0.251820560382959,1.89885249283377,
12.9878975425398));
#71510=CARTESIAN_POINT('Ctrl Pts',(-0.249577527498403,1.89607606618043,
12.9881054378204));
#71511=CARTESIAN_POINT('Ctrl Pts',(-0.246053203866126,1.89185891868664,
12.9884280780931));
#71512=CARTESIAN_POINT('Ctrl Pts',(-0.244804290397781,1.8903914408968,12.9885416669482));
#71513=CARTESIAN_POINT('Ctrl Pts',(-0.243330301273887,1.88869064171508,
12.9886749145883));
#71514=CARTESIAN_POINT('Ctrl Pts',(-0.243117925104523,1.88844633090246,
12.988694093829));
#71515=CARTESIAN_POINT('Ctrl Pts',(-0.239174078828746,1.88392323701485,
12.9890498982305));
#71516=CARTESIAN_POINT('Ctrl Pts',(-0.235330747341237,1.87974369309926,
12.9893907650507));
#71517=CARTESIAN_POINT('Ctrl Pts',(-0.230697537289453,1.87496493401502,
12.9897959949599));
#71518=CARTESIAN_POINT('Ctrl Pts',(-0.230012669317467,1.87426496383031,
12.9898557536156));
#71519=CARTESIAN_POINT('Ctrl Pts',(-0.228973645729901,1.87321266629227,
12.98994620709));
#71520=CARTESIAN_POINT('Ctrl Pts',(-0.228621839496334,1.87285801869761,
12.9899767984544));
#71521=CARTESIAN_POINT('Ctrl Pts',(-0.227991863930262,1.87222590144169,
12.9900315154405));
#71522=CARTESIAN_POINT('Ctrl Pts',(-0.2277140084875,1.87194811921664,12.9900556271391));
#71523=CARTESIAN_POINT('Ctrl Pts',(-0.227126038454846,1.87136245005111,
12.9901066047036));
#71524=CARTESIAN_POINT('Ctrl Pts',(-0.226815804445384,1.87105468460433,
12.9901334758577));
#71525=CARTESIAN_POINT('Ctrl Pts',(-0.225992081899213,1.87024083405121,
12.9902047539913));
#71526=CARTESIAN_POINT('Ctrl Pts',(-0.225477521590444,1.86973584155897,
12.9902492088265));
#71527=CARTESIAN_POINT('Ctrl Pts',(-0.223112734651171,1.86743055300935,
12.9904531928106));
#71528=CARTESIAN_POINT('Ctrl Pts',(-0.221242654089342,1.86565084291849,
12.9906136150321));
#71529=CARTESIAN_POINT('Ctrl Pts',(-0.206970780108064,1.85239173962067,
12.9918315826369));
#71530=CARTESIAN_POINT('Ctrl Pts',(-0.193706656717891,1.84188311887711,
12.9929301518164));
#71531=CARTESIAN_POINT('Ctrl Pts',(-0.158133572766333,1.81799162650794,
12.9957880807951));
#71532=CARTESIAN_POINT('Ctrl Pts',(-0.134916896728148,1.8061763439686,12.9975807246286));
#71533=CARTESIAN_POINT('Ctrl Pts',(-0.105047958610657,1.79527024528794,
12.9996531220359));
#71534=CARTESIAN_POINT('Ctrl Pts',(-0.0995070351941245,1.79341614908757,
13.0000278981939));
#71535=CARTESIAN_POINT('Ctrl Pts',(-0.0932877754666285,1.79152147382515,
13.0004355599173));
#71536=CARTESIAN_POINT('Ctrl Pts',(-0.0926565991362059,1.79133130249855,
13.0004767848727));
#71537=CARTESIAN_POINT('Ctrl Pts',(-0.0917690824540835,1.79106686427661,
13.0005345410591));
#71538=CARTESIAN_POINT('Ctrl Pts',(-0.0915132320466128,1.79099097876599,
13.0005511661722));
#71539=CARTESIAN_POINT('Ctrl Pts',(-0.0910438998521653,1.79085240834202,
13.0005816177234));
#71540=CARTESIAN_POINT('Ctrl Pts',(-0.090830446945182,1.79078962656966,
13.000595449861));
#71541=CARTESIAN_POINT('Ctrl Pts',(-0.0903952048889321,1.7906621007059,
13.0006236189108));
#71542=CARTESIAN_POINT('Ctrl Pts',(-0.0901734110855543,1.79059737405672,
13.0006379547816));
#71543=CARTESIAN_POINT('Ctrl Pts',(-0.0896186778656303,1.79043613200863,
13.000673764191));
#71544=CARTESIAN_POINT('Ctrl Pts',(-0.0892856509545071,1.79033991486716,
13.0006952201981));
#71545=CARTESIAN_POINT('Ctrl Pts',(-0.0880185743581929,1.78997604887177,
13.0007766981902));
#71546=CARTESIAN_POINT('Ctrl Pts',(-0.0870834589533761,1.78971208380125,
13.0008365071011));
#71547=CARTESIAN_POINT('Ctrl Pts',(-0.0722725922572282,1.78560349065665,
13.0017789041796));
#71548=CARTESIAN_POINT('Ctrl Pts',(-0.0581536240978287,1.78268821968073,
13.0026097704631));
#71549=CARTESIAN_POINT('Ctrl Pts',(-0.00962500357097965,1.77601778957087,
13.0053814187414));
#71550=CARTESIAN_POINT('Ctrl Pts',(0.0251659925638299,1.7768533616894,13.007255240017));
#71551=CARTESIAN_POINT('Ctrl Pts',(0.0596921708261186,1.78330091048652,
13.0093791054892));
#71552=CARTESIAN_POINT('Ctrl Pts',(0.0602239513661011,1.78340160418447,
13.0094118750788));
#71553=CARTESIAN_POINT('Ctrl Pts',(0.0623020787287461,1.78380052697147,
13.0095401609234));
#71554=CARTESIAN_POINT('Ctrl Pts',(0.0638464653531769,1.78410874579652,
13.0096359893986));
#71555=CARTESIAN_POINT('Ctrl Pts',(0.0659926891035543,1.78455345727852,
13.0097698665948));
#71556=CARTESIAN_POINT('Ctrl Pts',(0.0665965042302619,1.78468038128589,
13.0098076092456));
#71557=CARTESIAN_POINT('Ctrl Pts',(0.0675643837474342,1.78488673699047,
13.0098682346868));
#71558=CARTESIAN_POINT('Ctrl Pts',(0.0679286833967781,1.784965067896,13.009891082185));
#71559=CARTESIAN_POINT('Ctrl Pts',(0.0686805442777158,1.78512809614003,
13.0099382957269));
#71560=CARTESIAN_POINT('Ctrl Pts',(0.0690680864777507,1.78521287759694,
13.0099626644334));
#71561=CARTESIAN_POINT('Ctrl Pts',(0.0699702577501759,1.78541198915028,
13.0100194698843));
#71562=CARTESIAN_POINT('Ctrl Pts',(0.0704847636873698,1.7855268666123,13.0100519241444));
#71563=CARTESIAN_POINT('Ctrl Pts',(0.072125463109162,1.78589742617481,13.010155604368));
#71564=CARTESIAN_POINT('Ctrl Pts',(0.0732505555630983,1.78615789739683,
13.0102269840148));
#71565=CARTESIAN_POINT('Ctrl Pts',(0.0991076464729995,1.7922907113338,13.0118740382368));
#71566=CARTESIAN_POINT('Ctrl Pts',(0.123054574328012,1.80106126766966,13.0135494222347));
#71567=CARTESIAN_POINT('Ctrl Pts',(0.16736542379948,1.82352390441864,13.0169037649004));
#71568=CARTESIAN_POINT('Ctrl Pts',(0.187705880118596,1.83690888636158,13.0185658893423));
#71569=CARTESIAN_POINT('Ctrl Pts',(0.207352651939784,1.85328609498175,13.0201806953776));
#71570=CARTESIAN_POINT('Ctrl Pts',(0.208348403318061,1.85412642238815,13.0202625486588));
#71571=CARTESIAN_POINT('Ctrl Pts',(0.209646100760314,1.85523511044956,13.0203692051224));
#71572=CARTESIAN_POINT('Ctrl Pts',(0.209952659244786,1.85549801718406,13.0203943995641));
#71573=CARTESIAN_POINT('Ctrl Pts',(0.210424996806164,1.85590464060243,13.0204332154082));
#71574=CARTESIAN_POINT('Ctrl Pts',(0.210591123280743,1.8560479502928,13.0204468667839));
#71575=CARTESIAN_POINT('Ctrl Pts',(0.210918949080065,1.85633133498288,13.0204738043281));
#71576=CARTESIAN_POINT('Ctrl Pts',(0.211080654183117,1.85647140040165,13.0204870909708));
#71577=CARTESIAN_POINT('Ctrl Pts',(0.211441372608775,1.85678447600533,13.020516728238));
#71578=CARTESIAN_POINT('Ctrl Pts',(0.211640312619265,1.8569575690578,13.020533072531));
#71579=CARTESIAN_POINT('Ctrl Pts',(0.21205436741509,1.85731872234266,13.020567088509));
#71580=CARTESIAN_POINT('Ctrl Pts',(0.212269445140151,1.85750682498965,13.0205847570259));
#71581=CARTESIAN_POINT('Ctrl Pts',(0.212825954481056,1.8579948445828,13.0206304726713));
#71582=CARTESIAN_POINT('Ctrl Pts',(0.213167003837131,1.85829519940583,13.020658487635));
#71583=CARTESIAN_POINT('Ctrl Pts',(0.224561970124997,1.86837337803091,13.0215945121563));
#71584=CARTESIAN_POINT('Ctrl Pts',(0.234933599784499,1.87889979022904,13.0224468577848));
#71585=CARTESIAN_POINT('Ctrl Pts',(0.267120230014987,1.91639977328706,13.0252436839158));
#71586=CARTESIAN_POINT('Ctrl Pts',(0.285300683463496,1.94616323829224,13.0271209049882));
#71587=CARTESIAN_POINT('Ctrl Pts',(0.298568623717848,1.97868154100987,13.0292446308518));
#71588=CARTESIAN_POINT('Ctrl Pts',(0.298743241807744,1.97911217169938,13.0292727608452));
#71589=CARTESIAN_POINT('Ctrl Pts',(0.299526950090914,1.98105696540774,13.029399829494));
#71590=CARTESIAN_POINT('Ctrl Pts',(0.300125455930805,1.9825753439068,13.0294991173425));
#71591=CARTESIAN_POINT('Ctrl Pts',(0.30093764020589,1.98468259193223,13.0296370451498));
#71592=CARTESIAN_POINT('Ctrl Pts',(0.301161180692527,1.98526765438069,13.0296753539547));
#71593=CARTESIAN_POINT('Ctrl Pts',(0.301515630680638,1.98620351378748,13.0297366561829));
#71594=CARTESIAN_POINT('Ctrl Pts',(0.301647637560282,1.98655389574145,13.0297596128241));
#71595=CARTESIAN_POINT('Ctrl Pts',(0.301917922662678,1.98727511259806,13.0298068774825));
#71596=CARTESIAN_POINT('Ctrl Pts',(0.302056128934785,1.987645973657,13.029831187859));
#71597=CARTESIAN_POINT('Ctrl Pts',(0.302374736552156,1.9885057583928,13.0298875624319));
#71598=CARTESIAN_POINT('Ctrl Pts',(0.302554635430714,1.98899486592571,13.0299196433303));
#71599=CARTESIAN_POINT('Ctrl Pts',(0.30311840131328,1.99053917949306,13.030020971847));
#71600=CARTESIAN_POINT('Ctrl Pts',(0.303497937196138,1.99159594792018,13.0300903634638));
#71601=CARTESIAN_POINT('Ctrl Pts',(0.309593301805848,2.00885063632491,13.0312242976386));
#71602=CARTESIAN_POINT('Ctrl Pts',(0.314009727309315,2.02547526623345,13.0323323605864));
#71603=CARTESIAN_POINT('Ctrl Pts',(0.32137831083781,2.06601739940995,13.0350684210968));
#71604=CARTESIAN_POINT('Ctrl Pts',(0.323017197557475,2.09006916548321,13.036722112365));
#71605=CARTESIAN_POINT('Ctrl Pts',(0.321562127936125,2.12334551864251,13.0389284858201));
#71606=CARTESIAN_POINT('Ctrl Pts',(0.320756973030407,2.13259167654339,13.0395317716445));
#71607=CARTESIAN_POINT('Ctrl Pts',(0.319460450137995,2.14250547530872,13.0401592455322));
#71608=CARTESIAN_POINT('Ctrl Pts',(0.31936463298086,2.14321950784399,13.0402043292886));
#71609=CARTESIAN_POINT('Ctrl Pts',(0.319227613661866,2.14421523878377,13.0402670408607));
#71610=CARTESIAN_POINT('Ctrl Pts',(0.319188432290649,2.14449720618567,13.0402847815427));
#71611=CARTESIAN_POINT('Ctrl Pts',(0.319120151431184,2.14498385617715,13.0403153692592));
#71612=CARTESIAN_POINT('Ctrl Pts',(0.319091228593618,2.14518856272546,13.0403282263105));
#71613=CARTESIAN_POINT('Ctrl Pts',(0.319031375842144,2.14560925849995,13.0403546293233));
#71614=CARTESIAN_POINT('Ctrl Pts',(0.319000423606129,2.14582524382913,13.0403681739195));
#71615=CARTESIAN_POINT('Ctrl Pts',(0.318927743830487,2.14632876273526,13.0403997252728));
#71616=CARTESIAN_POINT('Ctrl Pts',(0.318885846626649,2.14661627252607,13.0404177223624));
#71617=CARTESIAN_POINT('Ctrl Pts',(0.318795871370844,2.14722790901982,13.0404559694471));
#71618=CARTESIAN_POINT('Ctrl Pts',(0.318747687638349,2.14755202015559,13.0404762134612));
#71619=CARTESIAN_POINT('Ctrl Pts',(0.318389631266875,2.14993551231312,13.0406249179909));
#71620=CARTESIAN_POINT('Ctrl Pts',(0.318060288284193,2.15199198248878,13.0407522935955));
#71621=CARTESIAN_POINT('Ctrl Pts',(0.31704580974826,2.15795571543072,13.0411193639774));
#71622=CARTESIAN_POINT('Ctrl Pts',(0.316308420675292,2.16185383214356,13.041356397312));
#71623=CARTESIAN_POINT('Ctrl Pts',(0.314191428709977,2.17201407564945,13.0419689429184));
#71624=CARTESIAN_POINT('Ctrl Pts',(0.312696562473269,2.17825055860806,13.0423396617069));
#71625=CARTESIAN_POINT('Ctrl Pts',(0.303351382856004,2.21267207930778,13.0443766578996));
#71626=CARTESIAN_POINT('Ctrl Pts',(0.291877983769051,2.23972980150944,13.0459569635001));
#71627=CARTESIAN_POINT('Ctrl Pts',(0.272205973775907,2.27277051771961,13.0482002207271));
#71628=CARTESIAN_POINT('Ctrl Pts',(0.267165791214756,2.28046650503202,13.0487467697745));
#71629=CARTESIAN_POINT('Ctrl Pts',(0.261140278400599,2.28886033287967,13.0493751543312));
#71630=CARTESIAN_POINT('Ctrl Pts',(0.26047184975478,2.28978115230942,13.049444539783));
#71631=CARTESIAN_POINT('Ctrl Pts',(0.259491861186536,2.29111624279506,13.0495458071596));
#71632=CARTESIAN_POINT('Ctrl Pts',(0.259184150886062,2.29153333967397,13.0495775394843));
#71633=CARTESIAN_POINT('Ctrl Pts',(0.258639137334894,2.29226837926134,13.0496336299236));
#71634=CARTESIAN_POINT('Ctrl Pts',(0.258402250110441,2.29258663027518,13.049657971771));
#71635=CARTESIAN_POINT('Ctrl Pts',(0.257911098678903,2.29324394017619,13.0497083639958));
#71636=CARTESIAN_POINT('Ctrl Pts',(0.25765675223014,2.29358293639695,13.0497344175645));
#71637=CARTESIAN_POINT('Ctrl Pts',(0.257003486732051,2.29445004879544,13.0498012259781));
#71638=CARTESIAN_POINT('Ctrl Pts',(0.256603609579404,2.29497743769308,13.0498420184259));
#71639=CARTESIAN_POINT('Ctrl Pts',(0.254961455413181,2.29712943588291,13.0500091251482));
#71640=CARTESIAN_POINT('Ctrl Pts',(0.253705373227394,2.2987434062393,13.05013598401));
#71641=CARTESIAN_POINT('Ctrl Pts',(0.245297764176558,2.30933695088757,13.050978979991));
#71642=CARTESIAN_POINT('Ctrl Pts',(0.237686995280068,2.31793988026829,13.0517136454886));
#71643=CARTESIAN_POINT('Ctrl Pts',(0.226117038792136,2.32968977083719,13.0527928751491));
#71644=CARTESIAN_POINT('Ctrl Pts',(0.222517015211541,2.33317907383562,13.0531238879797));
#71645=CARTESIAN_POINT('Ctrl Pts',(0.215989808659054,2.33921668581548,13.0537152254305));
#71646=CARTESIAN_POINT('Ctrl Pts',(0.213095163819517,2.34179882160189,13.0539745505745));
#71647=CARTESIAN_POINT('Ctrl Pts',(0.189037202863037,2.36249187536752,13.0561046042451));
#71648=CARTESIAN_POINT('Ctrl Pts',(0.165653580067553,2.37784183739132,13.0580306229208));
#71649=CARTESIAN_POINT('Ctrl Pts',(0.13923296202041,2.3906503423667,13.0598877541481));
#71650=CARTESIAN_POINT('Ctrl Pts',(0.13787452510135,2.39129719320389,13.0599823840816));
#71651=CARTESIAN_POINT('Ctrl Pts',(0.13612472187324,2.39211541914222,13.0601031342494));
#71652=CARTESIAN_POINT('Ctrl Pts',(0.13573750496316,2.39229554864399,13.0601297837855));
#71653=CARTESIAN_POINT('Ctrl Pts',(0.135124028410765,2.39257944994594,13.0601718908743));
#71654=CARTESIAN_POINT('Ctrl Pts',(0.134898006370842,2.39268372941249,13.0601873797864));
#71655=CARTESIAN_POINT('Ctrl Pts',(0.134477180438365,2.39287729424834,13.0602161723535));
#71656=CARTESIAN_POINT('Ctrl Pts',(0.134282409826652,2.39296664649135,13.0602294800811));
#71657=CARTESIAN_POINT('Ctrl Pts',(0.133843739223327,2.39316736002346,13.0602594112364));
#71658=CARTESIAN_POINT('Ctrl Pts',(0.13359978982904,2.39327861100205,13.0602760277555));
#71659=CARTESIAN_POINT('Ctrl Pts',(0.133089981637661,2.39351033645654,13.0603106941993));
#71660=CARTESIAN_POINT('Ctrl Pts',(0.132824097254377,2.39363075453586,13.0603287406434));
#71661=CARTESIAN_POINT('Ctrl Pts',(0.13213041104132,2.39394378751114,13.0603757372296));
#71662=CARTESIAN_POINT('Ctrl Pts',(0.131702349649893,2.39413583059789,13.060404652653));
#71663=CARTESIAN_POINT('Ctrl Pts',(0.119676833351551,2.39949937643015,13.0612146219413));
#71664=CARTESIAN_POINT('Ctrl Pts',(0.107782593827991,2.40398259881624,13.061954587522));
#71665=CARTESIAN_POINT('Ctrl Pts',(0.0810885146029854,2.41227944893016,
13.0635473878274));
#71666=CARTESIAN_POINT('Ctrl Pts',(0.0662202957728761,2.41576685439528,
13.0643915437928));
#71667=CARTESIAN_POINT('Ctrl Pts',(0.0374926798737054,2.42038588545408,
13.0660233794245));
#71668=CARTESIAN_POINT('Ctrl Pts',(0.0236982847111115,2.42170042176613,
13.0668073465145));
#71669=CARTESIAN_POINT('Ctrl Pts',(0.00752525042455238,2.4221956182934,
13.0677531170686));
#71670=CARTESIAN_POINT('Ctrl Pts',(0.00518682861953486,2.42224174507862,
13.0678904882338));
#71671=CARTESIAN_POINT('Ctrl Pts',(-0.00369592262513817,2.42232025073422,
13.0684149756304));
#71672=CARTESIAN_POINT('Ctrl Pts',(-0.0102398503973064,2.4221787393623,
13.0688069065576));
#71673=CARTESIAN_POINT('Ctrl Pts',(-0.0178082853604414,2.42178426312994,
13.0692681569696));
#71674=CARTESIAN_POINT('Ctrl Pts',(-0.0188416918970045,2.42172540719195,
13.0693313078984));
#71675=CARTESIAN_POINT('Ctrl Pts',(-0.0203778996808845,2.42163048816571,
13.0694254450355));
#71676=CARTESIAN_POINT('Ctrl Pts',(-0.0208809358563081,2.42159822173998,
13.0694563120646));
#71677=CARTESIAN_POINT('Ctrl Pts',(-0.0217764564429814,2.42153867008201,
13.0695113372047));
#71678=CARTESIAN_POINT('Ctrl Pts',(-0.022168971350692,2.42151184600321,
13.0695354807913));
#71679=CARTESIAN_POINT('Ctrl Pts',(-0.022994866934573,2.42145388550823,
13.069586335824));
#71680=CARTESIAN_POINT('Ctrl Pts',(-0.0234282354308102,2.42142259129584,
13.0696130521795));
#71681=CARTESIAN_POINT('Ctrl Pts',(-0.024569400215618,2.42133786585075,
13.0696834862749));
#71682=CARTESIAN_POINT('Ctrl Pts',(-0.0252770826653947,2.4212829726822,
13.0697272498628));
#71683=CARTESIAN_POINT('Ctrl Pts',(-0.0284479557340132,2.42102647460799,
13.069923722583));
#71684=CARTESIAN_POINT('Ctrl Pts',(-0.0309089070949299,2.42079888169952,
13.0700772463377));
#71685=CARTESIAN_POINT('Ctrl Pts',(-0.0489494170054523,2.4189209537676,
13.0712105788909));
#71686=CARTESIAN_POINT('Ctrl Pts',(-0.0643904779587972,2.41616507799364,
13.0722254561884));
#71687=CARTESIAN_POINT('Ctrl Pts',(-0.0831988261291664,2.41137303779648,
13.0735151867658));
#71688=CARTESIAN_POINT('Ctrl Pts',(-0.0868130447873905,2.41038477320243,
13.0737654505094));
#71689=CARTESIAN_POINT('Ctrl Pts',(-0.0933253073564207,2.40848143073359,
13.0742204623408));
#71690=CARTESIAN_POINT('Ctrl Pts',(-0.0962292423951886,2.40758793631658,
13.0744248464411));
#71691=CARTESIAN_POINT('Ctrl Pts',(-0.101563104495609,2.40586386414598,
13.0748027669341));
#71692=CARTESIAN_POINT('Ctrl Pts',(-0.103996594101321,2.40504503902707,
13.0749761641162));
#71693=CARTESIAN_POINT('Ctrl Pts',(-0.108521069782248,2.40346220143024,
13.0753002119873));
#71694=CARTESIAN_POINT('Ctrl Pts',(-0.110614439152244,2.40270542791465,
13.0754508116235));
#71695=CARTESIAN_POINT('Ctrl Pts',(-0.119645622755248,2.39933437318651,
13.0761031457002));
#71696=CARTESIAN_POINT('Ctrl Pts',(-0.126500016020583,2.39650276754919,
13.0766050429809));
#71697=CARTESIAN_POINT('Ctrl Pts',(-0.138874699940913,2.39088338651718,
13.0775182043687));
#71698=CARTESIAN_POINT('Ctrl Pts',(-0.144424339008915,2.38816825601422,
13.0779304205303));
#71699=CARTESIAN_POINT('Ctrl Pts',(-0.156874990155226,2.38162674322147,
13.0788565722671));
#71700=CARTESIAN_POINT('Ctrl Pts',(-0.163720938351319,2.37770283371383,
13.0793667975492));
#71701=CARTESIAN_POINT('Ctrl Pts',(-0.171006442555565,2.37316378819657,
13.0799053443627));
#71702=CARTESIAN_POINT('Ctrl Pts',(-0.171595096575207,2.37279439405899,
13.0799488251424));
#71703=CARTESIAN_POINT('Ctrl Pts',(-0.172419496447772,2.37227333956213,
13.0800096680891));
#71704=CARTESIAN_POINT('Ctrl Pts',(-0.172656240965963,2.37212327472782,
13.0800271345362));
#71705=CARTESIAN_POINT('Ctrl Pts',(-0.17306630189056,2.3718625995746,13.0800573771307));
#71706=CARTESIAN_POINT('Ctrl Pts',(-0.173239708269755,2.37175213223945,
13.0800701627741));
#71707=CARTESIAN_POINT('Ctrl Pts',(-0.173597619048664,2.37152364584995,
13.0800965452616));
#71708=CARTESIAN_POINT('Ctrl Pts',(-0.173782108686184,2.37140560476137,
13.0801101405308));
#71709=CARTESIAN_POINT('Ctrl Pts',(-0.174219356500851,2.37112521404171,
13.0801423528991));
#71710=CARTESIAN_POINT('Ctrl Pts',(-0.17447200913164,2.37096269835543,13.0801609588961));
#71711=CARTESIAN_POINT('Ctrl Pts',(-0.175007529889489,2.3706171716893,13.0802003817718));
#71712=CARTESIAN_POINT('Ctrl Pts',(-0.175290339312197,2.3704340697423,13.0802211925941));
#71713=CARTESIAN_POINT('Ctrl Pts',(-0.177512649583516,2.36899030796666,
13.0803846612557));
#71714=CARTESIAN_POINT('Ctrl Pts',(-0.179438878520595,2.36770920071841,
13.0805259768813));
#71715=CARTESIAN_POINT('Ctrl Pts',(-0.18514383016156,2.36382567566688,13.0809439224431));
#71716=CARTESIAN_POINT('Ctrl Pts',(-0.188881096957397,2.36116309242474,
13.0812169308504));
#71717=CARTESIAN_POINT('Ctrl Pts',(-0.199613636422901,2.35316583721478,
13.082002646187));
#71718=CARTESIAN_POINT('Ctrl Pts',(-0.206449191695052,2.34762329498498,
13.0825052961444));
#71719=CARTESIAN_POINT('Ctrl Pts',(-0.235322493852153,2.32218385850991,
13.0846791304478));
#71720=CARTESIAN_POINT('Ctrl Pts',(-0.254775586508409,2.29957882845893,
13.0862954092033));
#71721=CARTESIAN_POINT('Ctrl Pts',(-0.27396503515206,2.26981508646467,13.0883945591642));
#71722=CARTESIAN_POINT('Ctrl Pts',(-0.276940596821328,2.26491786935097,
13.0887385133076));
#71723=CARTESIAN_POINT('Ctrl Pts',(-0.280271316338659,2.25909157531224,
13.0891470875488));
#71724=CARTESIAN_POINT('Ctrl Pts',(-0.280754813661814,2.25823676775569,
13.0892070152782));
#71725=CARTESIAN_POINT('Ctrl Pts',(-0.281478631721524,2.25694331986961,
13.0892976749819));
#71726=CARTESIAN_POINT('Ctrl Pts',(-0.281721853876238,2.25650630278552,
13.0893283027928));
#71727=CARTESIAN_POINT('Ctrl Pts',(-0.282154358259389,2.25572491181958,
13.0893830603583));
#71728=CARTESIAN_POINT('Ctrl Pts',(-0.282344030180213,2.25538075384489,
13.0894071761103));
#71729=CARTESIAN_POINT('Ctrl Pts',(-0.282743132988517,2.25465344173868,
13.0894581367137));
#71730=CARTESIAN_POINT('Ctrl Pts',(-0.282952415417319,2.25427020742936,
13.0894849868021));
#71731=CARTESIAN_POINT('Ctrl Pts',(-0.283504455339804,2.25325441930177,
13.0895561501296));
#71732=CARTESIAN_POINT('Ctrl Pts',(-0.283845873183109,2.2526211436746,13.0896005109494));
#71733=CARTESIAN_POINT('Ctrl Pts',(-0.285395452500939,2.24972373649537,
13.0898034570099));
#71734=CARTESIAN_POINT('Ctrl Pts',(-0.286578636452029,2.2474464177079,13.0899629242538));
#71735=CARTESIAN_POINT('Ctrl Pts',(-0.291608083572247,2.23747678057211,
13.0906610163535));
#71736=CARTESIAN_POINT('Ctrl Pts',(-0.295172457925456,2.22964697139591,
13.0912093481336));
#71737=CARTESIAN_POINT('Ctrl Pts',(-0.3019933835955,2.21291933277661,13.0923817145481));
#71738=CARTESIAN_POINT('Ctrl Pts',(-0.305179352762911,2.20400152927173,
13.0930072734632));
#71739=CARTESIAN_POINT('Ctrl Pts',(-0.313909921185657,2.17568623589384,
13.0949890632125));
#71740=CARTESIAN_POINT('Ctrl Pts',(-0.318029698806027,2.1559010431128,13.0963703576027));
#71741=CARTESIAN_POINT('Ctrl Pts',(-0.321389326753392,2.12589625912996,
13.0983782196975));
#71742=CARTESIAN_POINT('Ctrl Pts',(-0.322039543581381,2.1158837424051,13.099033317208));
#71743=CARTESIAN_POINT('Ctrl Pts',(-0.322239111835978,2.10490298855582,
13.0997243153652));
#71744=CARTESIAN_POINT('Ctrl Pts',(-0.322252206061614,2.10394971345929,
13.0997840758538));
#71745=CARTESIAN_POINT('Ctrl Pts',(-0.322264377247691,2.10264070082897,
13.0998658123331));
#71746=CARTESIAN_POINT('Ctrl Pts',(-0.322267095522565,2.10228501423813,
13.0998879889211));
#71747=CARTESIAN_POINT('Ctrl Pts',(-0.322270480605708,2.10171957818711,
13.0999231899422));
#71748=CARTESIAN_POINT('Ctrl Pts',(-0.322271531515003,2.10150983262813,
13.099936235948));
#71749=CARTESIAN_POINT('Ctrl Pts',(-0.322273226028635,2.1010897872172,13.0999623389437));
#71750=CARTESIAN_POINT('Ctrl Pts',(-0.322273868552071,2.10087948834564,
13.0999753957789));
#71751=CARTESIAN_POINT('Ctrl Pts',(-0.322274750300382,2.10045484734119,
13.1000017368163));
#71752=CARTESIAN_POINT('Ctrl Pts',(-0.322274981537786,2.10024050516953,
13.1000150205756));
#71753=CARTESIAN_POINT('Ctrl Pts',(-0.322274998938081,2.10002616218071,
13.100028292361));
#71754=CARTESIAN_POINT('Origin',(0.115470053837925,2.3,13.44));
#71755=CARTESIAN_POINT('',(0.115470053837925,2.3,13.44));
#71756=CARTESIAN_POINT('',(0.23094010767585,2.1,13.44));
#71757=CARTESIAN_POINT('',(0.144337567297406,2.25,13.44));
#71758=CARTESIAN_POINT('',(0.115470053837925,2.3,13.19));
#71759=CARTESIAN_POINT('',(0.115470053837925,2.3,13.44));
#71760=CARTESIAN_POINT('',(0.23094010767585,2.1,13.19));
#71761=CARTESIAN_POINT('',(0.23094010767585,2.1,13.19));
#71762=CARTESIAN_POINT('',(0.23094010767585,2.1,13.44));
#71763=CARTESIAN_POINT('Origin',(-0.115470053837925,2.3,13.44));
#71764=CARTESIAN_POINT('',(-0.115470053837925,2.3,13.44));
#71765=CARTESIAN_POINT('',(-0.0577350269189626,2.3,13.44));
#71766=CARTESIAN_POINT('',(-0.115470053837925,2.3,13.19));
#71767=CARTESIAN_POINT('',(-0.115470053837925,2.3,13.44));
#71768=CARTESIAN_POINT('',(0.115470053837925,2.3,13.19));
#71769=CARTESIAN_POINT('Origin',(-0.23094010767585,2.1,13.44));
#71770=CARTESIAN_POINT('',(-0.23094010767585,2.1,13.44));
#71771=CARTESIAN_POINT('',(-0.202072594216369,2.15,13.44));
#71772=CARTESIAN_POINT('',(-0.23094010767585,2.1,13.19));
#71773=CARTESIAN_POINT('',(-0.23094010767585,2.1,13.44));
#71774=CARTESIAN_POINT('',(-0.115470053837925,2.3,13.19));
#71775=CARTESIAN_POINT('Origin',(-0.115470053837925,1.9,13.44));
#71776=CARTESIAN_POINT('',(-0.115470053837925,1.9,13.44));
#71777=CARTESIAN_POINT('',(-0.144337567297407,1.95,13.44));
#71778=CARTESIAN_POINT('',(-0.115470053837925,1.9,13.19));
#71779=CARTESIAN_POINT('',(-0.115470053837925,1.9,13.44));
#71780=CARTESIAN_POINT('',(-0.23094010767585,2.1,13.19));
#71781=CARTESIAN_POINT('Origin',(0.115470053837925,1.9,13.44));
#71782=CARTESIAN_POINT('',(0.115470053837925,1.9,13.44));
#71783=CARTESIAN_POINT('',(0.0577350269189626,1.9,13.44));
#71784=CARTESIAN_POINT('',(0.115470053837925,1.9,13.19));
#71785=CARTESIAN_POINT('',(0.115470053837925,1.9,13.44));
#71786=CARTESIAN_POINT('',(-0.115470053837925,1.9,13.19));
#71787=CARTESIAN_POINT('Origin',(0.23094010767585,2.1,13.44));
#71788=CARTESIAN_POINT('',(0.202072594216369,2.05,13.44));
#71789=CARTESIAN_POINT('',(0.115470053837925,1.9,13.19));
#71790=CARTESIAN_POINT('Origin',(0.,2.1,13.19));
#71791=CARTESIAN_POINT('Origin',(5.160062080289E-17,2.1,13.3567));
#71792=CARTESIAN_POINT('Ctrl Pts',(0.384471428898087,2.18286501288884,13.3567));
#71793=CARTESIAN_POINT('Ctrl Pts',(0.382813073402951,2.18828203677418,13.3567));
#71794=CARTESIAN_POINT('Ctrl Pts',(0.381028861582513,2.19365655316686,13.3567));
#71795=CARTESIAN_POINT('Ctrl Pts',(0.379117390972968,2.19898452752087,13.3567));
#71796=CARTESIAN_POINT('Ctrl Pts',(0.374010021273159,2.21322065264946,13.3567));
#71797=CARTESIAN_POINT('Ctrl Pts',(0.367994822053367,2.22712503505139,13.3567));
#71798=CARTESIAN_POINT('Ctrl Pts',(0.361137622816578,2.24064162659447,13.3567));
#71799=CARTESIAN_POINT('Ctrl Pts',(0.356608893745571,2.24956844626943,13.3567));
#71800=CARTESIAN_POINT('Ctrl Pts',(0.351712673173096,2.25832598910903,13.3567));
#71801=CARTESIAN_POINT('Ctrl Pts',(0.346465850873052,2.26689606248918,13.3567));
#71802=CARTESIAN_POINT('Ctrl Pts',(0.343067268222326,2.27244725157844,13.3567));
#71803=CARTESIAN_POINT('Ctrl Pts',(0.33952652091561,2.27791158719777,13.3567));
#71804=CARTESIAN_POINT('Ctrl Pts',(0.335850140310723,2.28328316588372,13.3567));
#71805=CARTESIAN_POINT('Ctrl Pts',(0.326134074360472,2.29747936001562,13.3567));
#71806=CARTESIAN_POINT('Ctrl Pts',(0.315469319048827,2.31103259742725,13.3567));
#71807=CARTESIAN_POINT('Ctrl Pts',(0.30394745231302,2.32385415784788,13.3567));
#71808=CARTESIAN_POINT('Ctrl Pts',(0.298033748520208,2.33043494134658,13.3567));
#71809=CARTESIAN_POINT('Ctrl Pts',(0.291892742763497,2.33682398925588,13.3567));
#71810=CARTESIAN_POINT('Ctrl Pts',(0.285539140538778,2.34300405020489,13.3567));
#71811=CARTESIAN_POINT('Ctrl Pts',(0.280685518257919,2.34772510142249,13.3567));
#71812=CARTESIAN_POINT('Ctrl Pts',(0.275712527829575,2.35231944457806,13.3567));
#71813=CARTESIAN_POINT('Ctrl Pts',(0.270633354418833,2.35677538186565,13.3567));
#71814=CARTESIAN_POINT('Ctrl Pts',(0.2549882277151,2.37050078515682,13.3567));
#71815=CARTESIAN_POINT('Ctrl Pts',(0.238317569233452,2.38293578296153,13.3567));
#71816=CARTESIAN_POINT('Ctrl Pts',(0.220781169382088,2.393915845125,13.3567));
#71817=CARTESIAN_POINT('Ctrl Pts',(0.207902841162496,2.40197934992709,13.3567));
#71818=CARTESIAN_POINT('Ctrl Pts',(0.194556907819471,2.40925744118653,13.3567));
#71819=CARTESIAN_POINT('Ctrl Pts',(0.180802143098436,2.41566748709506,13.3567));
#71820=CARTESIAN_POINT('Ctrl Pts',(0.175631391396159,2.41807717976996,13.3567));
#71821=CARTESIAN_POINT('Ctrl Pts',(0.170402849726401,2.42036403435915,13.3567));
#71822=CARTESIAN_POINT('Ctrl Pts',(0.165119631550228,2.42252302855343,13.3567));
#71823=CARTESIAN_POINT('Ctrl Pts',(0.147547306967044,2.42970398256482,13.3567));
#71824=CARTESIAN_POINT('Ctrl Pts',(0.129505974814032,2.43541821356752,13.3567));
#71825=CARTESIAN_POINT('Ctrl Pts',(0.111120125345788,2.43952544314507,13.3567));
#71826=CARTESIAN_POINT('Ctrl Pts',(0.0910677364743285,2.44400496228916,
13.3567));
#71827=CARTESIAN_POINT('Ctrl Pts',(0.0706030552275727,2.44657367360852,
13.3567));
#71828=CARTESIAN_POINT('Ctrl Pts',(0.0499688774172958,2.44728614117711,
13.3567));
#71829=CARTESIAN_POINT('Ctrl Pts',(0.0444598928125659,2.44747635824817,
13.3567));
#71830=CARTESIAN_POINT('Ctrl Pts',(0.0389389090994037,2.44753396627794,
13.3567));
#71831=CARTESIAN_POINT('Ctrl Pts',(0.0334107967153799,2.44745938354123,
13.3567));
#71832=CARTESIAN_POINT('Ctrl Pts',(0.0262902260270452,2.44736331609326,
13.3567));
#71833=CARTESIAN_POINT('Ctrl Pts',(0.0191710656048495,2.44704789928713,
13.3567));
#71834=CARTESIAN_POINT('Ctrl Pts',(0.0120754035985885,2.44651741695667,
13.3567));
#71835=CARTESIAN_POINT('Ctrl Pts',(-0.00763403837127719,2.44504390952366,
13.3567));
#71836=CARTESIAN_POINT('Ctrl Pts',(-0.0271931972657536,2.44191427020158,
13.3567));
#71837=CARTESIAN_POINT('Ctrl Pts',(-0.0463836350019071,2.43718306921555,
13.3567));
#71838=CARTESIAN_POINT('Ctrl Pts',(-0.061026313137871,2.43357307062211,
13.3567));
#71839=CARTESIAN_POINT('Ctrl Pts',(-0.0754543432951754,2.4290295058022,
13.3567));
#71840=CARTESIAN_POINT('Ctrl Pts',(-0.0895595007323578,2.42355945091979,
13.3567));
#71841=CARTESIAN_POINT('Ctrl Pts',(-0.0955309797991314,2.42124367965883,
13.3567));
#71842=CARTESIAN_POINT('Ctrl Pts',(-0.101447746007056,2.41875987556956,
13.3567));
#71843=CARTESIAN_POINT('Ctrl Pts',(-0.107276888624383,2.41611965041911,
13.3567));
#71844=CARTESIAN_POINT('Ctrl Pts',(-0.124508298041685,2.4083149347846,13.3567));
#71845=CARTESIAN_POINT('Ctrl Pts',(-0.141018981529,2.39913172796346,13.3567));
#71846=CARTESIAN_POINT('Ctrl Pts',(-0.156604780393232,2.38860311667185,
13.3567));
#71847=CARTESIAN_POINT('Ctrl Pts',(-0.172190579257463,2.37807450538024,
13.3567));
#71848=CARTESIAN_POINT('Ctrl Pts',(-0.186852752521262,2.3661999008291,13.3567));
#71849=CARTESIAN_POINT('Ctrl Pts',(-0.200344699681301,2.35297855767097,
13.3567));
#71850=CARTESIAN_POINT('Ctrl Pts',(-0.201303803277869,2.35203869053215,
13.3567));
#71851=CARTESIAN_POINT('Ctrl Pts',(-0.202256970802107,2.35109200583289,
13.3567));
#71852=CARTESIAN_POINT('Ctrl Pts',(-0.20320410290731,2.35013849800987,13.3567));
#71853=CARTESIAN_POINT('',(-0.302891002292155,1.98913319379411,13.3568565029309));
#71854=CARTESIAN_POINT('Ctrl Pts',(-0.304247867982273,1.99372483614107,
13.3567));
#71855=CARTESIAN_POINT('Ctrl Pts',(-0.30372261333055,1.99222112067142,13.3567521676436));
#71856=CARTESIAN_POINT('Ctrl Pts',(-0.30318621052403,1.9907212993043,13.3568043352873));
#71857=CARTESIAN_POINT('Ctrl Pts',(-0.302638718523801,1.9892255368992,13.3568565029309));
#71858=CARTESIAN_POINT('Ctrl Pts',(-0.303133276678321,1.98898792129971,
13.3567));
#71859=CARTESIAN_POINT('Ctrl Pts',(-0.301503883177666,1.98230546808694,
13.3567));
#71860=CARTESIAN_POINT('Ctrl Pts',(-0.299648132848088,1.97568975965612,
13.3567));
#71861=CARTESIAN_POINT('Ctrl Pts',(-0.29756501457467,1.96915218281238,13.3567));
#71862=CARTESIAN_POINT('Ctrl Pts',(-0.293021738473608,1.95489374294745,
13.3567));
#71863=CARTESIAN_POINT('Ctrl Pts',(-0.287398567760631,1.94100671820594,
13.3567));
#71864=CARTESIAN_POINT('Ctrl Pts',(-0.280801429454096,1.92755158897031,
13.3567));
#71865=CARTESIAN_POINT('Ctrl Pts',(-0.27801701987579,1.92187267351028,13.3567));
#71866=CARTESIAN_POINT('Ctrl Pts',(-0.275058824312372,1.9162707242298,13.3567));
#71867=CARTESIAN_POINT('Ctrl Pts',(-0.271933633150864,1.91075051906705,
13.3567));
#71868=CARTESIAN_POINT('Ctrl Pts',(-0.263009465455726,1.89498724762603,
13.3567));
#71869=CARTESIAN_POINT('Ctrl Pts',(-0.252774512366312,1.87997443299183,
13.3567));
#71870=CARTESIAN_POINT('Ctrl Pts',(-0.241405887597271,1.86581594627798,
13.3567));
#71871=CARTESIAN_POINT('Ctrl Pts',(-0.235739092739989,1.85875851925168,
13.3567));
#71872=CARTESIAN_POINT('Ctrl Pts',(-0.229790133931066,1.85191365562157,
13.3567));
#71873=CARTESIAN_POINT('Ctrl Pts',(-0.223576577671086,1.84529462501086,
13.3567));
#71874=CARTESIAN_POINT('Ctrl Pts',(-0.218686560518433,1.84008550291298,
13.3567));
#71875=CARTESIAN_POINT('Ctrl Pts',(-0.213634883170243,1.83501929487925,
13.3567));
#71876=CARTESIAN_POINT('Ctrl Pts',(-0.208445611775876,1.8301160680278,13.3567));
#71877=CARTESIAN_POINT('Ctrl Pts',(-0.193804134551959,1.81628166261453,
13.3567));
#71878=CARTESIAN_POINT('Ctrl Pts',(-0.178042964881533,1.80371236102764,
13.3567));
#71879=CARTESIAN_POINT('Ctrl Pts',(-0.161369656581909,1.79254718173484,
13.3567));
#71880=CARTESIAN_POINT('Ctrl Pts',(-0.146268869163077,1.78243503146664,
13.3567));
#71881=CARTESIAN_POINT('Ctrl Pts',(-0.130418577424126,1.77347412276399,
13.3567));
#71882=CARTESIAN_POINT('Ctrl Pts',(-0.113944951420937,1.76579172141804,
13.3567));
#71883=CARTESIAN_POINT('Ctrl Pts',(-0.109408876626858,1.76367634335272,
13.3567));
#71884=CARTESIAN_POINT('Ctrl Pts',(-0.10482625753255,1.76165867681577,13.3567));
#71885=CARTESIAN_POINT('Ctrl Pts',(-0.100211858969317,1.75974617851619,
13.3567));
#71886=CARTESIAN_POINT('Ctrl Pts',(-0.0858955531262678,1.75381259687905,
13.3567));
#71887=CARTESIAN_POINT('Ctrl Pts',(-0.0712445325602557,1.74887619638116,
13.3567));
#71888=CARTESIAN_POINT('Ctrl Pts',(-0.0563443817491956,1.74500131412034,
13.3567));
#71889=CARTESIAN_POINT('Ctrl Pts',(-0.0413634792994686,1.74110543186455,
13.3567));
#71890=CARTESIAN_POINT('Ctrl Pts',(-0.0261304550998762,1.73828213073426,
13.3567));
#71891=CARTESIAN_POINT('Ctrl Pts',(-0.0107379526015333,1.73648531326028,
13.3567));
#71892=CARTESIAN_POINT('Ctrl Pts',(-0.00172422421978484,1.73543311108174,
13.3567));
#71893=CARTESIAN_POINT('Ctrl Pts',(0.00734332949099493,1.7347332825024,
13.3567));
#71894=CARTESIAN_POINT('Ctrl Pts',(0.0164505169552235,1.7343793481264,13.3567));
#71895=CARTESIAN_POINT('Ctrl Pts',(0.0228954295609135,1.73412887824968,
13.3567));
#71896=CARTESIAN_POINT('Ctrl Pts',(0.0293590259401381,1.73405213749439,
13.3567));
#71897=CARTESIAN_POINT('Ctrl Pts',(0.0358141150482056,1.73414609409592,
13.3567));
#71898=CARTESIAN_POINT('Ctrl Pts',(0.056425935663595,1.73444610802043,13.3567));
#71899=CARTESIAN_POINT('Ctrl Pts',(0.07698675111472,1.73647959996866,13.3567));
#71900=CARTESIAN_POINT('Ctrl Pts',(0.097287927881851,1.74013888126268,13.3567));
#71901=CARTESIAN_POINT('Ctrl Pts',(0.118088935260064,1.74388825688109,13.3567));
#71902=CARTESIAN_POINT('Ctrl Pts',(0.138618827654593,1.74934446475836,13.3567));
#71903=CARTESIAN_POINT('Ctrl Pts',(0.15865913407629,1.75644449140174,13.3567));
#71904=CARTESIAN_POINT('Ctrl Pts',(0.161079921109755,1.75730214557497,13.3567));
#71905=CARTESIAN_POINT('Ctrl Pts',(0.163493555065397,1.75818384755897,13.3567));
#71906=CARTESIAN_POINT('Ctrl Pts',(0.165899639879492,1.75908953676982,13.3567));
#71907=CARTESIAN_POINT('Ctrl Pts',(0.170720645667814,1.76090424126501,13.3567));
#71908=CARTESIAN_POINT('Ctrl Pts',(0.175502848112081,1.76281206603697,13.3567));
#71909=CARTESIAN_POINT('Ctrl Pts',(0.180241540932178,1.76481078791832,13.3567));
#71910=CARTESIAN_POINT('Ctrl Pts',(0.200489840282318,1.77335126954643,13.3567));
#71911=CARTESIAN_POINT('Ctrl Pts',(0.219954281019108,1.78355100246641,13.3567));
#71912=CARTESIAN_POINT('Ctrl Pts',(0.238403113750705,1.79532081160773,13.3567));
#71913=CARTESIAN_POINT('Ctrl Pts',(0.256851946482301,1.80709062074905,13.3567));
#71914=CARTESIAN_POINT('Ctrl Pts',(0.274286879817491,1.82043079606709,13.3567));
#71915=CARTESIAN_POINT('Ctrl Pts',(0.29045854394972,1.83530356379869,13.3567));
#71916=CARTESIAN_POINT('Ctrl Pts',(0.291364097891721,1.83613638430113,13.3567));
#71917=CARTESIAN_POINT('Ctrl Pts',(0.292265682104844,1.83697402310408,13.3567));
#71918=CARTESIAN_POINT('Ctrl Pts',(0.29316324943837,1.83781647805643,13.3567));
#71919=CARTESIAN_POINT('Ctrl Pts',(0.315794730921881,2.16133333943205,4.3153592086915));
#71920=CARTESIAN_POINT('Ctrl Pts',(0.295374973081064,2.26647113223029,4.32198265653243));
#71921=CARTESIAN_POINT('Ctrl Pts',(0.141593364461128,2.45291664246826,4.33522955221429));
#71922=CARTESIAN_POINT('Ctrl Pts',(-0.220800772831429,2.41004672910968,
4.35509989573707));
#71923=CARTESIAN_POINT('Ctrl Pts',(-0.379865078018474,2.08219540995681,
4.37497023925986));
#71924=CARTESIAN_POINT('Ctrl Pts',(-0.190837952383979,1.77095809589613,
4.39484058278266));
#71925=CARTESIAN_POINT('Ctrl Pts',(0.173453834391319,1.76142701812932,4.41471092630544));
#71926=CARTESIAN_POINT('Ctrl Pts',(0.378523374757362,2.06256570849522,4.43458126982823));
#71927=CARTESIAN_POINT('Ctrl Pts',(0.236402166296634,2.39800625800675,4.45445161335102));
#71928=CARTESIAN_POINT('Ctrl Pts',(-0.122613317153847,2.46008688645899,
4.47432195687381));
#71929=CARTESIAN_POINT('Ctrl Pts',(-0.369133512413124,2.19182630426626,
4.4941923003966));
#71930=CARTESIAN_POINT('Ctrl Pts',(-0.277031367561046,1.83933304745027,
4.51406264391939));
#71931=CARTESIAN_POINT('Ctrl Pts',(0.06921318690911,1.72596339903695,4.53393298744218));
#71932=CARTESIAN_POINT('Ctrl Pts',(0.351962069027787,1.95572288286177,4.55380333096497));
#71933=CARTESIAN_POINT('Ctrl Pts',(0.311834704349932,2.31783621621276,4.57367367448776));
#71934=CARTESIAN_POINT('Ctrl Pts',(-0.0143590870975264,2.4801148735102,
4.59354401801055));
#71935=CARTESIAN_POINT('Ctrl Pts',(-0.327380091631696,2.29368967642256,
4.61341436153334));
#71936=CARTESIAN_POINT('Ctrl Pts',(-0.340074575883644,1.92958067658856,
4.63328470505612));
#71937=CARTESIAN_POINT('Ctrl Pts',(-0.0407968584462133,1.72180814998663,
4.65315504857892));
#71938=CARTESIAN_POINT('Ctrl Pts',(0.295906383536178,1.86097518841639,4.67302539210171));
#71939=CARTESIAN_POINT('Ctrl Pts',(0.361155822934746,2.21941493622384,4.6928957356245));
#71940=CARTESIAN_POINT('Ctrl Pts',(0.0950939511799071,2.46830774468873,
4.71276607914728));
#71941=CARTESIAN_POINT('Ctrl Pts',(-0.25820366943978,2.37932833394089,4.73263642267008));
#71942=CARTESIAN_POINT('Ctrl Pts',(-0.37463457744399,2.03410320601478,4.75250676619286));
#71943=CARTESIAN_POINT('Ctrl Pts',(-0.147389261061116,1.7493294144447,4.77237710971565));
#71944=CARTESIAN_POINT('Ctrl Pts',(0.215065636343779,1.78624814619657,4.79224745323845));
#71945=CARTESIAN_POINT('Ctrl Pts',(0.380227091343265,2.11099149006219,4.81211779676122));
#71946=CARTESIAN_POINT('Ctrl Pts',(0.196581953073257,2.42565163830413,4.83198814028403));
#71947=CARTESIAN_POINT('Ctrl Pts',(-0.167400364818031,2.44157074179032,
4.85185848380681));
#71948=CARTESIAN_POINT('Ctrl Pts',(-0.37781563754619,2.14414519038242,4.8717288273296));
#71949=CARTESIAN_POINT('Ctrl Pts',(-0.241636497751353,1.80622243660235,
4.89159917085239));
#71950=CARTESIAN_POINT('Ctrl Pts',(0.11621123287666,1.73780060304687,4.91146951437518));
#71951=CARTESIAN_POINT('Ctrl Pts',(0.367450978078876,2.00164740719483,4.93133985789797));
#71952=CARTESIAN_POINT('Ctrl Pts',(0.281604474823222,2.35571932574806,4.95121020142075));
#71953=CARTESIAN_POINT('Ctrl Pts',(-0.0625757970931978,2.47520357596851,
4.97108054494355));
#71954=CARTESIAN_POINT('Ctrl Pts',(-0.349351294103218,2.25048962459309,
4.99095088846634));
#71955=CARTESIAN_POINT('Ctrl Pts',(-0.315644538657038,1.8877219299655,5.01082123198912));
#71956=CARTESIAN_POINT('Ctrl Pts',(0.00762310988300606,1.7196904655451,
5.03069157551192));
#71957=CARTESIAN_POINT('Ctrl Pts',(0.323897592898241,1.90054122451905,5.0505619190347));
#71958=CARTESIAN_POINT('Ctrl Pts',(0.343040129104818,2.26436825613651,5.0704322625575));
#71959=CARTESIAN_POINT('Ctrl Pts',(0.0474900475543018,2.47740978946618,
5.09030260608028));
#71960=CARTESIAN_POINT('Ctrl Pts',(-0.291625687441136,2.34422922066392,
5.11017294960308));
#71961=CARTESIAN_POINT('Ctrl Pts',(-0.363214555461668,1.98700159070856,
5.13004329312585));
#71962=CARTESIAN_POINT('Ctrl Pts',(-0.101603516042804,1.73343461793378,
5.14991363664866));
#71963=CARTESIAN_POINT('Ctrl Pts',(0.253214917275652,1.81614147983423,5.16978398017144));
#71964=CARTESIAN_POINT('Ctrl Pts',(0.375743136091877,2.15924989013876,5.18965432369423));
#71965=CARTESIAN_POINT('Ctrl Pts',(0.153578180352721,2.44800459238517,5.20952466721702));
#71966=CARTESIAN_POINT('Ctrl Pts',(-0.209473848078761,2.41751245766535,
5.22939501073981));
#71967=CARTESIAN_POINT('Ctrl Pts',(-0.380362138187303,2.09574586845546,
5.24926535426261));
#71968=CARTESIAN_POINT('Ctrl Pts',(-0.202319948138264,1.77788186578998,
5.26913569778539));
#71969=CARTESIAN_POINT('Ctrl Pts',(0.16132325095384,1.75551739883805,5.28900604130818));
#71970=CARTESIAN_POINT('Ctrl Pts',(0.376974329473245,2.04916882138084,5.30887638483097));
#71971=CARTESIAN_POINT('Ctrl Pts',(0.246802781121706,2.38945093026661,5.32874672835376));
#71972=CARTESIAN_POINT('Ctrl Pts',(-0.109776719744329,2.46420121581866,
5.34861707187654));
#71973=CARTESIAN_POINT('Ctrl Pts',(-0.365651024995835,2.20484646737545,
5.36848741539934));
#71974=CARTESIAN_POINT('Ctrl Pts',(-0.286090293705716,1.8493093586729,5.38835775892213));
#71975=CARTESIAN_POINT('Ctrl Pts',(0.0559193343828591,1.72374678493893,
5.40822810244491));
#71976=CARTESIAN_POINT('Ctrl Pts',(0.346630585905113,1.94334531377359,5.4280984459677));
#71977=CARTESIAN_POINT('Ctrl Pts',(0.319355464352517,2.30665319061123,5.4479687894905));
#71978=CARTESIAN_POINT('Ctrl Pts',(-0.000884819422922472,2.48038489835456,
5.46783913301329));
#71979=CARTESIAN_POINT('Ctrl Pts',(-0.320313401835117,2.30516524658536,
5.48770947653607));
#71980=CARTESIAN_POINT('Ctrl Pts',(-0.345898044795595,1.94173441180029,
5.50757982005887));
#71981=CARTESIAN_POINT('Ctrl Pts',(-0.0541683214227408,1.7234907082742,
5.52745016358165));
#71982=CARTESIAN_POINT('Ctrl Pts',(0.287253462504416,1.85064302279496,5.54732050710444));
#71983=CARTESIAN_POINT('Ctrl Pts',(0.365159300611444,2.20654641701426,5.56719085062723));
#71984=CARTESIAN_POINT('Ctrl Pts',(0.108081192357295,2.46470797860787,5.58706119415001));
#71985=CARTESIAN_POINT('Ctrl Pts',(-0.248146695958989,2.38829962033665,
5.60693153767281));
#71986=CARTESIAN_POINT('Ctrl Pts',(-0.376733772855055,2.04741560885575,
5.6268018811956));
#71987=CARTESIAN_POINT('Ctrl Pts',(-0.15971890082854,1.75477061753128,5.64667222471839));
#71988=CARTESIAN_POINT('Ctrl Pts',(0.203816318943259,1.77882658588539,5.66654256824118));
#71989=CARTESIAN_POINT('Ctrl Pts',(0.380377813170898,2.09751543787756,5.68641291176396));
#71990=CARTESIAN_POINT('Ctrl Pts',(0.207994447577465,2.41848353737448,5.70628325528676));
#71991=CARTESIAN_POINT('Ctrl Pts',(-0.155195507781162,2.44728634894876,
5.72615359880955));
#71992=CARTESIAN_POINT('Ctrl Pts',(-0.376014712711115,2.15750121412973,
5.74602394233233));
#71993=CARTESIAN_POINT('Ctrl Pts',(-0.251891608509355,1.8149665434301,5.76589428585512));
#71994=CARTESIAN_POINT('Ctrl Pts',(0.10330775455378,1.7339112653322,5.78576462937792));
#71995=CARTESIAN_POINT('Ctrl Pts',(0.363736316894626,1.98869256281116,5.8056349729007));
#71996=CARTESIAN_POINT('Ctrl Pts',(0.290486326712738,2.34558328077163,5.8255053164235));
#71997=CARTESIAN_POINT('Ctrl Pts',(-0.0492453220856943,2.47718477176881,
5.84537565994628));
#71998=CARTESIAN_POINT('Ctrl Pts',(-0.343801092015725,2.262770583738,5.86524600346907));
#71999=CARTESIAN_POINT('Ctrl Pts',(-0.32296616431361,1.89903654434159,5.88511634699187));
#72000=CARTESIAN_POINT('Ctrl Pts',(-0.00585374872675999,1.71965911680776,
5.90498669051464));
#72001=CARTESIAN_POINT('Ctrl Pts',(0.316628684400964,1.88919267086714,5.92485703403744));
#72002=CARTESIAN_POINT('Ctrl Pts',(0.348647404693823,2.25211325057955,5.94472737756023));
#72003=CARTESIAN_POINT('Ctrl Pts',(0.0608295952382777,2.47549063123434,
5.96459772108302));
#72004=CARTESIAN_POINT('Ctrl Pts',(-0.282791086646785,2.3544064761651,5.9844680646058));
#72005=CARTESIAN_POINT('Ctrl Pts',(-0.366989445063476,1.99993901352867,
6.0043384081286));
#72006=CARTESIAN_POINT('Ctrl Pts',(-0.114524948735923,1.73726388390642,
6.02420875165139));
#72007=CARTESIAN_POINT('Ctrl Pts',(0.243000596892941,1.807349758737,6.04407909517418));
#72008=CARTESIAN_POINT('Ctrl Pts',(0.377606176416558,2.14590238919362,6.06394943869696));
#72009=CARTESIAN_POINT('Ctrl Pts',(0.165809495516936,2.4423458266111,6.08381978221975));
#72010=CARTESIAN_POINT('Ctrl Pts',(-0.19809482459498,2.42473357428868,6.10369012574255));
#72011=CARTESIAN_POINT('Ctrl Pts',(-0.380274111316162,2.10922247604054,
6.12356046926533));
#72012=CARTESIAN_POINT('Ctrl Pts',(-0.213603670550259,1.78525101155195,
6.14343081278812));
#72013=CARTESIAN_POINT('Ctrl Pts',(0.149019058431623,1.75001889475892,6.16330115631092));
#72014=CARTESIAN_POINT('Ctrl Pts',(0.374937088415383,2.03584679639947,6.1831714998337));
#72015=CARTESIAN_POINT('Ctrl Pts',(0.256901382853463,2.38052652867348,6.2030418433565));
#72016=CARTESIAN_POINT('Ctrl Pts',(-0.0968063675113594,2.46786136112791,
6.22291218687928));
#72017=CARTESIAN_POINT('Ctrl Pts',(-0.36170745468139,2.21773347454961,6.24278253040208));
#72018=CARTESIAN_POINT('Ctrl Pts',(-0.294791194204682,1.85960115303731,
6.26265287392485));
#72019=CARTESIAN_POINT('Ctrl Pts',(0.042555854757641,1.72200204626551,6.28252321744766));
#72020=CARTESIAN_POINT('Ctrl Pts',(0.340863700436308,1.9311646022705,6.30239356097044));
#72021=CARTESIAN_POINT('Ctrl Pts',(0.326475505367192,2.29521065082841,6.32226390449323));
#72022=CARTESIAN_POINT('Ctrl Pts',(0.0125904797503218,2.48017750278163,
6.34213424801602));
#72023=CARTESIAN_POINT('Ctrl Pts',(-0.312844596998426,2.31638325242612,
6.36200459153881));
#72024=CARTESIAN_POINT('Ctrl Pts',(-0.351287345947157,1.95408682588945,
6.38187493506159));
#72025=CARTESIAN_POINT('Ctrl Pts',(-0.0674717784430968,1.72564587231427,
6.40174527858439));
#72026=CARTESIAN_POINT('Ctrl Pts',(0.278239960329309,1.84062386717827,6.42161562210717));
#72027=CARTESIAN_POINT('Ctrl Pts',(0.36870441444973,2.19354415303425,6.44148596562998));
#72028=CARTESIAN_POINT('Ctrl Pts',(0.120932762886018,2.46065041336782,6.46135630915275));
#72029=CARTESIAN_POINT('Ctrl Pts',(-0.237778235116594,2.39690901755665,
6.48122665267555));
#72030=CARTESIAN_POINT('Ctrl Pts',(-0.3783600729834,2.06079401865006,6.50109699619833));
#72031=CARTESIAN_POINT('Ctrl Pts',(-0.171848052960638,1.76064517021965,
6.52096733972113));
#72032=CARTESIAN_POINT('Ctrl Pts',(0.19231116065365,1.77180817912437,6.54083768324391));
#72033=CARTESIAN_POINT('Ctrl Pts',(0.38005106516863,2.08404250440059,6.56070802676671));
#72034=CARTESIAN_POINT('Ctrl Pts',(0.219145856671893,2.41091565947239,6.58057837028948));
#72035=CARTESIAN_POINT('Ctrl Pts',(-0.142795841306913,2.45256602432321,
6.60044871381229));
#72036=CARTESIAN_POINT('Ctrl Pts',(-0.373741794785009,2.17078505938753,
6.62031905733506));
#72037=CARTESIAN_POINT('Ctrl Pts',(-0.261830531898757,1.82406843897947,
6.64018940085787));
#72038=CARTESIAN_POINT('Ctrl Pts',(0.0902745989964047,1.73048146111777,
6.66005974438064));
#72039=CARTESIAN_POINT('Ctrl Pts',(0.35956507508926,1.975877437274,6.67993008790345));
#72040=CARTESIAN_POINT('Ctrl Pts',(0.29900354515251,2.33513896697027,6.69980043142622));
#72041=CARTESIAN_POINT('Ctrl Pts',(-0.0358530318046874,2.47869250575107,
6.71967077494902));
#72042=CARTESIAN_POINT('Ctrl Pts',(-0.337819333030621,2.2748472248346,6.73954111847181));
#72043=CARTESIAN_POINT('Ctrl Pts',(-0.329882386150286,1.91060341843263,
6.7594114619946));
#72044=CARTESIAN_POINT('Ctrl Pts',(-0.0193232594086513,1.72010519160241,
6.77928180551739));
#72045=CARTESIAN_POINT('Ctrl Pts',(0.308962327216199,1.87810873346892,6.79915214904017));
#72046=CARTESIAN_POINT('Ctrl Pts',(0.35381704004292,2.23966730460951,6.81902249256296));
#72047=CARTESIAN_POINT('Ctrl Pts',(0.0740927864707377,2.47310013775744,
6.83889283608576));
#72048=CARTESIAN_POINT('Ctrl Pts',(-0.273601511866297,2.36426438751011,
6.85876317960853));
#72049=CARTESIAN_POINT('Ctrl Pts',(-0.370303670548427,2.01300203806998,
6.87863352313134));
#72050=CARTESIAN_POINT('Ctrl Pts',(-0.127302623794927,1.74154847499761,
6.89850386665411));
#72051=CARTESIAN_POINT('Ctrl Pts',(0.232481249603138,1.79892538734629,6.91837421017692));
#72052=CARTESIAN_POINT('Ctrl Pts',(0.378995225954534,2.1324972691974,6.9382445536997));
#72053=CARTESIAN_POINT('Ctrl Pts',(0.177832678033613,2.4362573306636,6.95811489722249));
#72054=CARTESIAN_POINT('Ctrl Pts',(-0.186467142250151,2.43154706854785,
6.97798524074528));
#72055=CARTESIAN_POINT('Ctrl Pts',(-0.379708744728557,2.12268750709709,
6.99785558426807));
#72056=CARTESIAN_POINT('Ctrl Pts',(-0.224619266596289,1.79301524650992,
7.01772592779085));
#72057=CARTESIAN_POINT('Ctrl Pts',(0.136527809486201,1.74495970504953,7.03759627131366));
#72058=CARTESIAN_POINT('Ctrl Pts',(0.372429206948008,2.0226052998346,7.05746661483643));
#72059=CARTESIAN_POINT('Ctrl Pts',(0.26667750869322,2.37124999568441,7.07733695835923));
#72060=CARTESIAN_POINT('Ctrl Pts',(-0.0837144989230929,2.47105974784618,
7.09720730188202));
#72061=CARTESIAN_POINT('Ctrl Pts',(-0.357309850477381,2.23047269658226,
7.1170776454048));
#72062=CARTESIAN_POINT('Ctrl Pts',(-0.303122057562357,1.87019470845784,
7.1369479889276));
#72063=CARTESIAN_POINT('Ctrl Pts',(0.0291389568243188,1.72073179015793,
7.15681833245039));
#72064=CARTESIAN_POINT('Ctrl Pts',(0.334668945235442,1.91919582168376,7.17668867597317));
#72065=CARTESIAN_POINT('Ctrl Pts',(0.333185737455809,2.28352307254851,7.19655901949597));
#72066=CARTESIAN_POINT('Ctrl Pts',(0.0260499747027282,2.47949288876026,
7.21642936301875));
#72067=CARTESIAN_POINT('Ctrl Pts',(-0.304983093456289,2.32732964282612,
7.23629970654154));
#72068=CARTESIAN_POINT('Ctrl Pts',(-0.356235693068131,1.96662239773529,
7.25617005006433));
#72069=CARTESIAN_POINT('Ctrl Pts',(-0.0806905414003209,1.72827094500141,
7.27604039358713));
#72070=CARTESIAN_POINT('Ctrl Pts',(0.268877196977014,1.83093029388762,7.29591073710991));
#72071=CARTESIAN_POINT('Ctrl Pts',(0.371786711452961,2.18042446759916,7.31578108063271));
#72072=CARTESIAN_POINT('Ctrl Pts',(0.133632532361157,2.45614014109106,7.33565142415549));
#72073=CARTESIAN_POINT('Ctrl Pts',(-0.227111302745492,2.40514571923404,
7.35552176767828));
#72074=CARTESIAN_POINT('Ctrl Pts',(-0.37951143599511,2.07422164181826,7.37539211120107));
#72075=CARTESIAN_POINT('Ctrl Pts',(-0.183761492535834,1.76694569862766,
7.39526245472386));
#72076=CARTESIAN_POINT('Ctrl Pts',(0.180564603456863,1.76520173569733,7.41513279824664));
#72077=CARTESIAN_POINT('Ctrl Pts',(0.379247257428947,2.07058960159674,7.43500314176944));
#72078=CARTESIAN_POINT('Ctrl Pts',(0.230022182561926,2.40295750416694,7.45487348529222));
#72079=CARTESIAN_POINT('Ctrl Pts',(-0.130216930113199,2.45740314060387,
7.47474382881502));
#72080=CARTESIAN_POINT('Ctrl Pts',(-0.370999736843724,2.18398005158073,
7.49461417233779));
#72081=CARTESIAN_POINT('Ctrl Pts',(-0.271440792073554,1.83351669808392,
7.51448451586061));
#72082=CARTESIAN_POINT('Ctrl Pts',(0.0771281260971214,1.72751549566946,
7.53435485938337));
#72083=CARTESIAN_POINT('Ctrl Pts',(0.354942488619908,1.96321811679202,7.55422520290618));
#72084=CARTESIAN_POINT('Ctrl Pts',(0.3071454388904,2.32439949458597,7.57409554642895));
#72085=CARTESIAN_POINT('Ctrl Pts',(-0.0224157369453323,2.47972488532992,
7.59396588995176));
#72086=CARTESIAN_POINT('Ctrl Pts',(-0.331413525760743,2.28670438865877,
7.61383623347454));
#72087=CARTESIAN_POINT('Ctrl Pts',(-0.336384522568092,1.92240803290055,
7.63370657699733));
#72088=CARTESIAN_POINT('Ctrl Pts',(-0.0327685145367435,1.72102812999291,
7.65357692052013));
#72089=CARTESIAN_POINT('Ctrl Pts',(0.300908144551645,1.86730332545543,7.67344726404291));
#72090=CARTESIAN_POINT('Ctrl Pts',(0.358542545958669,2.22704604102093,7.69331760756571));
#72091=CARTESIAN_POINT('Ctrl Pts',(0.0872629726086352,2.47024130970641,
7.71318795108848));
#72092=CARTESIAN_POINT('Ctrl Pts',(-0.264068498328838,2.37379058053916,
7.73305829461128));
#72093=CARTESIAN_POINT('Ctrl Pts',(-0.373153071729418,2.02617426694902,
7.75292863813407));
#72094=CARTESIAN_POINT('Ctrl Pts',(-0.139920502021753,1.74628301296715,
7.77279898165686));
#72095=CARTESIAN_POINT('Ctrl Pts',(0.221670079834584,1.79087894036843,7.79266932517965));
#72096=CARTESIAN_POINT('Ctrl Pts',(0.379908541099039,2.11905135694947,7.81253966870244));
#72097=CARTESIAN_POINT('Ctrl Pts',(0.189632635782723,2.42974674713742,7.83241001222523));
#72098=CARTESIAN_POINT('Ctrl Pts',(-0.174605396712056,2.43794438779278,
7.85228035574801));
#72099=CARTESIAN_POINT('Ctrl Pts',(-0.378666748101841,2.13612405962227,
7.87215069927082));
#72100=CARTESIAN_POINT('Ctrl Pts',(-0.235352908930933,1.80116482459495,
7.89202104279359));
#72101=CARTESIAN_POINT('Ctrl Pts',(0.12386518377878,1.74034618026627,7.91189138631639));
#72102=CARTESIAN_POINT('Ctrl Pts',(0.369453833093542,2.00946095309699,7.93176172983917));
#72103=CARTESIAN_POINT('Ctrl Pts',(0.276118887142609,2.36163297568301,7.95163207336197));
#72104=CARTESIAN_POINT('Ctrl Pts',(-0.0705175475695523,2.47379236119321,
7.97150241688475));
#72105=CARTESIAN_POINT('Ctrl Pts',(-0.352463732483867,2.24304814254354,
7.99137276040755));
#72106=CARTESIAN_POINT('Ctrl Pts',(-0.311072426448528,1.88107672735627,
8.01124310393033));
#72107=CARTESIAN_POINT('Ctrl Pts',(0.0156854821665361,1.71993761110731,
8.03111344745313));
#72108=CARTESIAN_POINT('Ctrl Pts',(0.328054096279372,1.90745399584531,8.05098379097592));
#72109=CARTESIAN_POINT('Ctrl Pts',(0.33947773758828,2.27160512662376,8.07085413449869));
#72110=CARTESIAN_POINT('Ctrl Pts',(0.0394767703806659,2.47833191565335,
8.0907244780215));
#72111=CARTESIAN_POINT('Ctrl Pts',(-0.296738759374218,2.3379906773104,8.11059482154428));
#72112=CARTESIAN_POINT('Ctrl Pts',(-0.36073687473749,1.97932539204024,8.13046516506707));
#72113=CARTESIAN_POINT('Ctrl Pts',(-0.0938080174200238,1.73136263120875,
8.15033550858987));
#72114=CARTESIAN_POINT('Ctrl Pts',(0.259176925071939,1.82157447079718,8.17020585211264));
#72115=CARTESIAN_POINT('Ctrl Pts',(0.374402322562648,2.16720382921612,8.19007619563545));
#72116=CARTESIAN_POINT('Ctrl Pts',(0.146164559375766,2.45118282330448,8.20994653915821));
#72117=CARTESIAN_POINT('Ctrl Pts',(-0.216159288530444,2.41299938623523,
8.22981688268102));
#72118=CARTESIAN_POINT('Ctrl Pts',(-0.38018641663983,2.08768162331384,8.24968722620381));
#72119=CARTESIAN_POINT('Ctrl Pts',(-0.195444265189107,1.77366429400645,
8.26955756972659));
#72120=CARTESIAN_POINT('Ctrl Pts',(0.168591392238535,1.75901554835347,8.28942791324939));
#72121=CARTESIAN_POINT('Ctrl Pts',(0.377967398932861,2.05717361624485,8.30929825677218));
#72122=CARTESIAN_POINT('Ctrl Pts',(0.240609772721243,2.3946190609459,8.32916860029496));
#72123=CARTESIAN_POINT('Ctrl Pts',(-0.117474563899405,2.46179162599245,
8.34903894381776));
#72124=CARTESIAN_POINT('Ctrl Pts',(-0.367791980860096,2.19706962767325,
8.36890928734054));
#72125=CARTESIAN_POINT('Ctrl Pts',(-0.280710325738522,1.84329946080036,
8.38877963086334));
#72126=CARTESIAN_POINT('Ctrl Pts',(0.0638848379881091,1.72501709202038,
8.40864997438611));
#72127=CARTESIAN_POINT('Ctrl Pts',(0.349874359995995,1.95073049199851,8.42852031790892));
#72128=CARTESIAN_POINT('Ctrl Pts',(0.314901787800618,2.31337834435947,8.44839066143169));
#72129=CARTESIAN_POINT('Ctrl Pts',(-0.00895030469455451,2.48028061460912,
8.4682610049545));
#72130=CARTESIAN_POINT('Ctrl Pts',(-0.324591711106426,2.29832719148573,
8.48813134847726));
#72131=CARTESIAN_POINT('Ctrl Pts',(-0.342464411749368,1.93443556998325,
8.50800169200008));
#72132=CARTESIAN_POINT('Ctrl Pts',(-0.0461726369319628,1.72242677345929,
8.52787203552285));
#72133=CARTESIAN_POINT('Ctrl Pts',(0.292476246433607,1.8567900103332,8.54774237904566));
#72134=CARTESIAN_POINT('Ctrl Pts',(0.362817990741843,2.21426530267612,8.56761272256843));
#72135=CARTESIAN_POINT('Ctrl Pts',(0.100323621753707,2.46691773562999,8.58748306609123));
#72136=CARTESIAN_POINT('Ctrl Pts',(-0.25420401236565,2.38297309748246,8.60735340961401));
#72137=CARTESIAN_POINT('Ctrl Pts',(-0.375534071890836,2.03943916570338,
8.62722375313683));
#72138=CARTESIAN_POINT('Ctrl Pts',(-0.152362744803578,1.75146155477833,
8.64709409665957));
#72139=CARTESIAN_POINT('Ctrl Pts',(0.210580658326276,1.78322051811948,8.6669644401824));
#72140=CARTESIAN_POINT('Ctrl Pts',(0.380344975409706,2.10558153045376,8.68683478370515));
#72141=CARTESIAN_POINT('Ctrl Pts',(0.201194556847495,2.42282224845347,8.70670512722799));
#72142=CARTESIAN_POINT('Ctrl Pts',(-0.162524477456688,2.44391750177775,
8.72657547075073));
#72143=CARTESIAN_POINT('Ctrl Pts',(-0.377149429404031,2.14951526736098,
8.74644581427356));
#72144=CARTESIAN_POINT('Ctrl Pts',(-0.245791124131638,1.80968951603547,
8.76631615779632));
#72145=CARTESIAN_POINT('Ctrl Pts',(0.111047076091526,1.73618411154385,8.78618650131912));
#72146=CARTESIAN_POINT('Ctrl Pts',(0.366014701695009,1.99643025564998,8.80605684484191));
#72147=CARTESIAN_POINT('Ctrl Pts',(0.285213666895485,2.35168754044976,8.8259271883647));
#72148=CARTESIAN_POINT('Ctrl Pts',(-0.0572320789460712,2.47605577105148,
8.84579753188749));
#72149=CARTESIAN_POINT('Ctrl Pts',(-0.347175183798591,2.2554440270838,8.86566787541028));
#72150=CARTESIAN_POINT('Ctrl Pts',(-0.318632321149308,1.89223355006012,
8.88553821893306));
#72151=CARTESIAN_POINT('Ctrl Pts',(0.00221231828093774,1.71962050600822,
8.90540856245586));
#72152=CARTESIAN_POINT('Ctrl Pts',(0.321027456868357,1.89595386370174,8.92527890597865));
#72153=CARTESIAN_POINT('Ctrl Pts',(0.345343607720877,2.25947177307581,8.94514924950143));
#72154=CARTESIAN_POINT('Ctrl Pts',(0.0528540127763269,2.47669604077433,
8.96501959302423));
#72155=CARTESIAN_POINT('Ctrl Pts',(-0.288121943466405,2.34835297359757,
8.984889936547));
#72156=CARTESIAN_POINT('Ctrl Pts',(-0.364785240839391,1.99217986334937,
9.00476028006981));
#72157=CARTESIAN_POINT('Ctrl Pts',(-0.10680774076842,1.73491705009196,9.02463062359258));
#72158=CARTESIAN_POINT('Ctrl Pts',(0.249151320896677,1.81256814181956,9.04450096711538));
#72159=CARTESIAN_POINT('Ctrl Pts',(0.376547964528556,2.15389883311368,9.06437131063818));
#72160=CARTESIAN_POINT('Ctrl Pts',(0.158513113081901,2.44578468268952,9.08424165416096));
#72161=CARTESIAN_POINT('Ctrl Pts',(-0.204935940005677,2.42046016023151,
9.10411199768375));
#72162=CARTESIAN_POINT('Ctrl Pts',(-0.380384167646973,2.10115706747243,
9.12398234120655));
#72163=CARTESIAN_POINT('Ctrl Pts',(-0.206881706100475,1.7807925228279,9.14385268472931));
#72164=CARTESIAN_POINT('Ctrl Pts',(0.156406556392147,1.75325738231484,9.16372302825214));
#72165=CARTESIAN_POINT('Ctrl Pts',(0.376213096224902,2.04381138878305,9.18359337177489));
#72166=CARTESIAN_POINT('Ctrl Pts',(0.250895337059515,2.38591079665415,9.20346371529772));
#72167=CARTESIAN_POINT('Ctrl Pts',(-0.104584737542124,2.46572597183528,
9.22333405882047));
#72168=CARTESIAN_POINT('Ctrl Pts',(-0.364122553375209,2.2100373569527,9.24320440234329));
#72169=CARTESIAN_POINT('Ctrl Pts',(-0.28962749729597,1.85340444729945,9.26307474586605));
#72170=CARTESIAN_POINT('Ctrl Pts',(0.0505613583289935,1.7229893862959,9.28294508938887));
#72171=CARTESIAN_POINT('Ctrl Pts',(0.344367050994486,1.93843023800544,9.30281543291163));
#72172=CARTESIAN_POINT('Ctrl Pts',(0.322262855713179,2.3020893506081,9.32268577643445));
#72173=CARTESIAN_POINT('Ctrl Pts',(0.00452636244120668,2.4803589960086,
9.34255611995722));
#72174=CARTESIAN_POINT('Ctrl Pts',(-0.317362452161966,2.3097010437727,9.36242646348002));
#72175=CARTESIAN_POINT('Ctrl Pts',(-0.348114421903012,1.94667093209458,
9.38229680700281));
#72176=CARTESIAN_POINT('Ctrl Pts',(-0.0595188010471789,1.72429936635199,
9.40216715052558));
#72177=CARTESIAN_POINT('Ctrl Pts',(0.283677217016357,1.84658198495871,9.4220374940484));
#72178=CARTESIAN_POINT('Ctrl Pts',(0.3666380076332,2.20134113261837,9.44190783757116));
#72179=CARTESIAN_POINT('Ctrl Pts',(0.113258339504188,2.46313358745008,9.46177818109397));
#72180=CARTESIAN_POINT('Ctrl Pts',(-0.244020436389291,2.39180041197023,
9.48164852461675));
#72181=CARTESIAN_POINT('Ctrl Pts',(-0.377443682278235,2.05278008354664,
9.50151886813954));
#72182=CARTESIAN_POINT('Ctrl Pts',(-0.164613733994266,1.75707760005785,
9.52138921166233));
#72183=CARTESIAN_POINT('Ctrl Pts',(0.199226905093178,1.77595973384684,9.54125955518512));
#72184=CARTESIAN_POINT('Ctrl Pts',(0.380303981051631,2.09210469773259,9.56112989870792));
#72185=CARTESIAN_POINT('Ctrl Pts',(0.212503928107109,2.41549252660034,9.58100024223071));
#72186=CARTESIAN_POINT('Ctrl Pts',(-0.150239549078219,2.44945891274139,
9.60087058575347));
#72187=CARTESIAN_POINT('Ctrl Pts',(-0.375158693251968,2.16284432097723,
9.6207409292763));
#72188=CARTESIAN_POINT('Ctrl Pts',(-0.25592080961125,1.81857862019822,9.64061127279905));
#72189=CARTESIAN_POINT('Ctrl Pts',(0.0980895763756364,1.73247872332604,
9.66048161632186));
#72190=CARTESIAN_POINT('Ctrl Pts',(0.362116129727866,1.98352956429838,9.68035195984465));
#72191=CARTESIAN_POINT('Ctrl Pts',(0.293950431714302,2.34142617400894,9.70022230336744));
#72192=CARTESIAN_POINT('Ctrl Pts',(-0.0438747696594335,2.477847136272,9.72009264689022));
#72193=CARTESIAN_POINT('Ctrl Pts',(-0.341450842881172,2.26764479024817,
9.73996299041301));
#72194=CARTESIAN_POINT('Ctrl Pts',(-0.325792252094184,1.90365117194896,
9.75983333393581));
#72195=CARTESIAN_POINT('Ctrl Pts',(-0.0112636226208964,1.71978087290739,
9.77970367745858));
#72196=CARTESIAN_POINT('Ctrl Pts',(0.31359784720331,1.88470986081321,9.7995740209814));
#72197=CARTESIAN_POINT('Ctrl Pts',(0.350775984710272,2.24713824231706,9.81944436450417));
#72198=CARTESIAN_POINT('Ctrl Pts',(0.0661649100837423,2.4745873175579,9.83931470802696));
#72199=CARTESIAN_POINT('Ctrl Pts',(-0.279143462005489,2.35840352439781,
9.85918505154976));
#72200=CARTESIAN_POINT('Ctrl Pts',(-0.368375709655487,2.00516967606597,
9.87905539507253));
#72201=CARTESIAN_POINT('Ctrl Pts',(-0.119673393520951,1.73892973996077,
9.89892573859534));
#72202=CARTESIAN_POINT('Ctrl Pts',(0.238812969107689,1.80392261216435,9.91879608211811));
#72203=CARTESIAN_POINT('Ctrl Pts',(0.37822094403001,2.1405261804105,9.93866642564092));
#72204=CARTESIAN_POINT('Ctrl Pts',(0.170662692936798,2.43995249527129,9.95853676916368));
#72205=CARTESIAN_POINT('Ctrl Pts',(-0.193455345298264,2.42751867607382,
9.9784071126865));
#72206=CARTESIAN_POINT('Ctrl Pts',(-0.380104440789253,2.11463105922013,
9.99827745620927));
#72207=CARTESIAN_POINT('Ctrl Pts',(-0.218059458403045,1.78832143737083,
10.0181477997321));
#72208=CARTESIAN_POINT('Ctrl Pts',(0.144025390953336,1.747934465529,10.0380181432549));
#72209=CARTESIAN_POINT('Ctrl Pts',(0.37398655139648,2.03051969216978,10.0578884867777));
#72210=CARTESIAN_POINT('Ctrl Pts',(0.260865964604863,2.37684364235501,10.0777588303004));
#72211=CARTESIAN_POINT('Ctrl Pts',(-0.0915636310175008,2.46920123953815,
10.0976291738232));
#72212=CARTESIAN_POINT('Ctrl Pts',(-0.359996060444061,2.22286696165515,
10.117499517346));
#72213=CARTESIAN_POINT('Ctrl Pts',(-0.298181113451348,1.86381897327997,
10.1373698608688));
#72214=CARTESIAN_POINT('Ctrl Pts',(0.0371744114399661,1.72143492377703,
10.1572402043916));
#72215=CARTESIAN_POINT('Ctrl Pts',(0.338427474674241,1.92633279472729,10.1771105479144));
#72216=CARTESIAN_POINT('Ctrl Pts',(0.329219402635234,2.29054668386019,10.1969808914372));
#72217=CARTESIAN_POINT('Ctrl Pts',(0.0179973478529294,2.47995993113995,
10.21685123496));
#72218=CARTESIAN_POINT('Ctrl Pts',(-0.309734823466772,2.32081166847254,
10.2367215784828));
#72219=CARTESIAN_POINT('Ctrl Pts',(-0.353327460844313,1.95909876077576,
10.2565919220055));
#72220=CARTESIAN_POINT('Ctrl Pts',(-0.072790254087486,1.72664355809562,
10.2764622655283));
#72221=CARTESIAN_POINT('Ctrl Pts',(0.274522101296335,1.83669206297291,10.2963326090511));
#72222=CARTESIAN_POINT('Ctrl Pts',(0.369997801550122,2.18828975393381,10.3162029525739));
#72223=CARTESIAN_POINT('Ctrl Pts',(0.126050889533918,2.45889361522508,10.3360732960967));
#72224=CARTESIAN_POINT('Ctrl Pts',(-0.233530553350605,2.40026144350112,
10.3559436396195));
#72225=CARTESIAN_POINT('Ctrl Pts',(-0.378879505849965,2.06618027426927,
10.3758139831423));
#72226=CARTESIAN_POINT('Ctrl Pts',(-0.176658091519081,1.76312409925545,
10.3956843266651));
#72227=CARTESIAN_POINT('Ctrl Pts',(0.187623071953084,1.76910570166215,10.4155546701879));
#72228=CARTESIAN_POINT('Ctrl Pts',(0.379785609483059,2.07863777560283,10.4354250137107));
#72229=CARTESIAN_POINT('Ctrl Pts',(0.223546553454306,2.40776678222368,10.4552953572334));
#72230=CARTESIAN_POINT('Ctrl Pts',(-0.137766032253613,2.45456166481829,
10.4751657007562));
#72231=CARTESIAN_POINT('Ctrl Pts',(-0.372697038520552,2.1760944891541,10.495036044279));
#72232=CARTESIAN_POINT('Ctrl Pts',(-0.265729250065068,1.8278209790203,10.5149063878018));
#72233=CARTESIAN_POINT('Ctrl Pts',(0.0850089495543705,1.72923466680759,
10.5347767313246));
#72234=CARTESIAN_POINT('Ctrl Pts',(0.357763010881125,1.97077507265668,10.5546470748474));
#72235=CARTESIAN_POINT('Ctrl Pts',(0.302318214760354,2.330861756958,10.5745174183702));
#72236=CARTESIAN_POINT('Ctrl Pts',(-0.0304623864945468,2.47916420824054,
10.594387761893));
#72237=CARTESIAN_POINT('Ctrl Pts',(-0.335297895220145,2.27963511700822,
10.6142581054158));
#72238=CARTESIAN_POINT('Ctrl Pts',(-0.332543231767824,1.91531526103376,
10.6341284489386));
#72239=CARTESIAN_POINT('Ctrl Pts',(-0.0247254248415304,1.72041851050398,
10.6539987924613));
#72240=CARTESIAN_POINT('Ctrl Pts',(0.305774593314228,1.87373610123324,10.6738691359841));
#72241=CARTESIAN_POINT('Ctrl Pts',(0.355768049556133,2.23462001603269,10.6937394795069));
#72242=CARTESIAN_POINT('Ctrl Pts',(0.0793927537767267,2.47200839298242,
10.7136098230297));
#72243=CARTESIAN_POINT('Ctrl Pts',(-0.269814585245385,2.36812971374034,
10.7334801665525));
#72244=CARTESIAN_POINT('Ctrl Pts',(-0.371503774243771,2.01827852470586,
10.7533505100753));
#72245=CARTESIAN_POINT('Ctrl Pts',(-0.132388826045411,1.74339566387952,
10.7732208535981));
#72246=CARTESIAN_POINT('Ctrl Pts',(0.228174846938419,1.79564873414713,10.7930911971209));
#72247=CARTESIAN_POINT('Ctrl Pts',(0.379419161056678,2.12710265715135,10.8129615406436));
#72248=CARTESIAN_POINT('Ctrl Pts',(0.182598048159953,2.4336935819128,10.8328318841665));
#72249=CARTESIAN_POINT('Ctrl Pts',(-0.181731915443975,2.43416607354829,
10.8527022276892));
#72250=CARTESIAN_POINT('Ctrl Pts',(-0.379347587194283,2.12808668530619,
10.872572571212));
#72251=CARTESIAN_POINT('Ctrl Pts',(-0.228963491204467,1.7962415869526,10.8924429147348));
#72252=CARTESIAN_POINT('Ctrl Pts',(0.131463437400806,1.7430534795962,10.9123132582576));
#72253=CARTESIAN_POINT('Ctrl Pts',(0.371290559321738,2.01731521082953,10.9321836017804));
#72254=CARTESIAN_POINT('Ctrl Pts',(0.270509139710306,2.36742897960917,10.9520539453032));
#72255=CARTESIAN_POINT('Ctrl Pts',(-0.0784275890913711,2.47221306676544,
10.971924288826));
#72256=CARTESIAN_POINT('Ctrl Pts',(-0.355417681853844,2.23554233739778,
10.9917946323488));
#72257=CARTESIAN_POINT('Ctrl Pts',(-0.306360437263606,1.87452996589066,
11.0116649758716));
#72258=CARTESIAN_POINT('Ctrl Pts',(0.0237408013085933,1.72035565570544,
11.0315353193943));
#72259=CARTESIAN_POINT('Ctrl Pts',(0.332063086698409,1.91445334750004,11.0514056629171));
#72260=CARTESIAN_POINT('Ctrl Pts',(0.335762696349584,2.27876483306756,11.0712760064399));
#72261=CARTESIAN_POINT('Ctrl Pts',(0.0314457420635472,2.47908392093003,
11.0911463499627));
#72262=CARTESIAN_POINT('Ctrl Pts',(-0.30171839961458,2.33164511895491,11.1110166934855));
#72263=CARTESIAN_POINT('Ctrl Pts',(-0.358096984897371,1.97170345597395,
11.1308870370083));
#72264=CARTESIAN_POINT('Ctrl Pts',(-0.0859703370391827,1.72945640613959,
11.1507573805311));
#72265=CARTESIAN_POINT('Ctrl Pts',(0.265022391247913,1.827132658717,11.1706277240539));
#72266=CARTESIAN_POINT('Ctrl Pts',(0.372893155105661,2.17512754938744,11.1904980675766));
#72267=CARTESIAN_POINT('Ctrl Pts',(0.138685213973004,2.45420314118719,11.2103684110995));
#72268=CARTESIAN_POINT('Ctrl Pts',(-0.222747530692876,2.40834557135112,
11.2302387546222));
#72269=CARTESIAN_POINT('Ctrl Pts',(-0.379839740286083,2.07962291725939,
11.250109098145));
#72270=CARTESIAN_POINT('Ctrl Pts',(-0.188480698678018,1.76959346249285,
11.2699794416678));
#72271=CARTESIAN_POINT('Ctrl Pts',(0.175783724637021,1.76266702510078,11.2898497851906));
#72272=CARTESIAN_POINT('Ctrl Pts',(0.378790511390766,2.0651976684411,11.3097201287134));
#72273=CARTESIAN_POINT('Ctrl Pts',(0.234308571615089,2.39965471307709,11.3295904722362));
#72274=CARTESIAN_POINT('Ctrl Pts',(-0.125119584385799,2.45921935277034,
11.349460815759));
#72275=CARTESIAN_POINT('Ctrl Pts',(-0.369767555206014,2.18924913959576,
11.3693311592818));
#72276=CARTESIAN_POINT('Ctrl Pts',(-0.275204133431753,1.83740499101526,
11.3892015028045));
#72277=CARTESIAN_POINT('Ctrl Pts',(0.0718216151065006,1.72645601409592,
11.4090718463273));
#72278=CARTESIAN_POINT('Ctrl Pts',(0.35296080941452,1.95818279082192,11.4289421898501));
#72279=CARTESIAN_POINT('Ctrl Pts',(0.310306512359927,2.32000755029915,11.4488125333729));
#72280=CARTESIAN_POINT('Ctrl Pts',(-0.0170117653678856,2.48000533370031,
11.4686828768957));
#72281=CARTESIAN_POINT('Ctrl Pts',(-0.328724064313393,2.29139995648615,
11.4885532204185));
#72282=CARTESIAN_POINT('Ctrl Pts',(-0.33887678599166,1.92721117594711,11.5084235639413));
#72283=CARTESIAN_POINT('Ctrl Pts',(-0.038156190431134,1.72153261840233,
11.5282939074641));
#72284=CARTESIAN_POINT('Ctrl Pts',(0.29756751535369,1.86304635979195,11.5481642509869));
#72285=CARTESIAN_POINT('Ctrl Pts',(0.360313535960682,2.22193280774724,11.5680345945097));
#72286=CARTESIAN_POINT('Ctrl Pts',(0.092520939582283,2.46896250424729,11.5879049380324));
#72287=CARTESIAN_POINT('Ctrl Pts',(-0.260147023274306,2.37751933280969,
11.6077752815552));
#72288=CARTESIAN_POINT('Ctrl Pts',(-0.374165508095917,2.03148995436479,
11.627645625078));
#72289=CARTESIAN_POINT('Ctrl Pts',(-0.144938077273781,1.74830921598968,
11.6475159686008));
#72290=CARTESIAN_POINT('Ctrl Pts',(0.21725030790957,1.78775689356719,11.6673863121236));
#72291=CARTESIAN_POINT('Ctrl Pts',(0.380141111544627,2.1136451132363,11.6872566556464));
#72292=CARTESIAN_POINT('Ctrl Pts',(0.194304196876692,2.42701579912555,11.7071269991692));
#72293=CARTESIAN_POINT('Ctrl Pts',(-0.169780366297813,2.44039400849809,
11.726997342692));
#72294=CARTESIAN_POINT('Ctrl Pts',(-0.378114556903807,2.14150705553338,
11.7468676862148));
#72295=CARTESIAN_POINT('Ctrl Pts',(-0.239580117199271,1.80454302979216,
11.7667380297376));
#72296=CARTESIAN_POINT('Ctrl Pts',(0.118736464147836,1.73862055138222,11.7866083732603));
#72297=CARTESIAN_POINT('Ctrl Pts',(0.368128504149248,2.00421451970967,11.8064787167831));
#72298=CARTESIAN_POINT('Ctrl Pts',(0.279812757764116,2.35767862618784,11.8263490603059));
#72299=CARTESIAN_POINT('Ctrl Pts',(-0.0651931008024049,2.47475767291596,
11.8462194038287));
#72300=CARTESIAN_POINT('Ctrl Pts',(-0.350393164621961,2.24804757339389,
11.8660897473515));
#72301=CARTESIAN_POINT('Ctrl Pts',(-0.314155201622804,1.88552398014009,
11.8859600908743));
#72302=CARTESIAN_POINT('Ctrl Pts',(0.0102773904965317,1.71975293683423,
11.9058304343971));
#72303=CARTESIAN_POINT('Ctrl Pts',(0.325281875975677,1.90280680801975,11.9257007779199));
#72304=CARTESIAN_POINT('Ctrl Pts',(0.341884523375812,2.26675858741819,11.9455711214427));
#72305=CARTESIAN_POINT('Ctrl Pts',(0.0448546639536624,2.47773206499213,
11.9654414649654));
#72306=CARTESIAN_POINT('Ctrl Pts',(-0.293323243234879,2.34218779651293,
11.9853118084882));
#72307=CARTESIAN_POINT('Ctrl Pts',(-0.362417007109122,1.98446919562436,
12.005182152011));
#72308=CARTESIAN_POINT('Ctrl Pts',(-0.0990425055810213,1.73273437965167,
12.0250524955338));
#72309=CARTESIAN_POINT('Ctrl Pts',(0.255190011398074,1.81791577164921,12.0449228390566));
#72310=CARTESIAN_POINT('Ctrl Pts',(0.375320433902403,2.1618710408586,12.0647931825794));
#72311=CARTESIAN_POINT('Ctrl Pts',(0.151145453564486,2.44906805306186,12.0846635261022));
#72312=CARTESIAN_POINT('Ctrl Pts',(-0.211684903823395,2.41604264790515,
12.104533869625));
#72313=CARTESIAN_POINT('Ctrl Pts',(-0.380323180250697,2.0930911386168,12.1244042131477));
#72314=CARTESIAN_POINT('Ctrl Pts',(-0.200066715123608,1.77647756909101,
12.1442745566706));
#72315=CARTESIAN_POINT('Ctrl Pts',(0.163723724505573,1.75665178632234,12.1641449001933));
#72316=CARTESIAN_POINT('Ctrl Pts',(0.377319935873306,2.05180124696446,12.1840152437162));
#72317=CARTESIAN_POINT('Ctrl Pts',(0.244776473548098,2.39116650184899,12.2038855872389));
#72318=CARTESIAN_POINT('Ctrl Pts',(-0.112316079949689,2.46342613002693,
12.2237559307617));
#72319=CARTESIAN_POINT('Ctrl Pts',(-0.3663739205472,2.20229175990513,12.2436262742845));
#72320=CARTESIAN_POINT('Ctrl Pts',(-0.284333566348057,1.84731862583599,
12.2634966178073));
#72321=CARTESIAN_POINT('Ctrl Pts',(0.0585441264557262,1.72414625309949,
12.2833669613301));
#72322=CARTESIAN_POINT('Ctrl Pts',(0.347715553299502,1.94576852527698,12.3032373048529));
#72323=CARTESIAN_POINT('Ctrl Pts',(0.317905297189056,2.30887717879355,12.3231076483757));
#72324=CARTESIAN_POINT('Ctrl Pts',(-0.00353979019419505,2.48036945682717,
12.3429779918984));
#72325=CARTESIAN_POINT('Ctrl Pts',(-0.321737601973187,2.30292454084747,
12.3628483354212));
#72326=CARTESIAN_POINT('Ctrl Pts',(-0.344784964561129,1.93932398432187,
12.382718678944));
#72327=CARTESIAN_POINT('Ctrl Pts',(-0.0515390603986663,1.72312179811664,
12.4025890224668));
#72328=CARTESIAN_POINT('Ctrl Pts',(0.288986915270079,1.85265405480521,12.4224593659896));
#72329=CARTESIAN_POINT('Ctrl Pts',(0.364406738194478,2.20909254310024,12.4423297095124));
#72330=CARTESIAN_POINT('Ctrl Pts',(0.105532988323146,2.46545347470943,12.4622000530352));
#72331=CARTESIAN_POINT('Ctrl Pts',(-0.250152911315643,2.38656059527075,
12.4820703965579));
#72332=CARTESIAN_POINT('Ctrl Pts',(-0.376357570066043,2.04478738137345,
12.5019407400808));
#72333=CARTESIAN_POINT('Ctrl Pts',(-0.157305394737393,1.75366422854673,
12.5218110836035));
#72334=CARTESIAN_POINT('Ctrl Pts',(0.206053065067093,1.78025699667065,12.5416814271264));
#72335=CARTESIAN_POINT('Ctrl Pts',(0.3803858892643,2.10017044126998,12.5615517706491));
#72336=CARTESIAN_POINT('Ctrl Pts',(0.205766444924184,2.41992752920759,12.5814221141719));
#72337=CARTESIAN_POINT('Ctrl Pts',(-0.157615700061881,2.44619466329742,
12.6012924576947));
#72338=CARTESIAN_POINT('Ctrl Pts',(-0.376406897681196,2.15487532395946,
12.6211628012175));
#72339=CARTESIAN_POINT('Ctrl Pts',(-0.249896009849807,1.81321534548945,
12.6410331447403));
#72340=CARTESIAN_POINT('Ctrl Pts',(0.105860446748859,1.73464124532766,12.6609034882631));
#72341=CARTESIAN_POINT('Ctrl Pts',(0.364504355054273,1.99123406347468,12.6807738317859));
#72342=CARTESIAN_POINT('Ctrl Pts',(0.288765140383735,2.34760482123854,12.7006441753087));
#72343=CARTESIAN_POINT('Ctrl Pts',(-0.0518767787635012,2.47683186386853,
12.7205145188314));
#72344=CARTESIAN_POINT('Ctrl Pts',(-0.344928815783521,2.26036697242512,
12.7403848623542));
#72345=CARTESIAN_POINT('Ctrl Pts',(-0.321555622135165,1.89678721577324,
12.760255205877));
#72346=CARTESIAN_POINT('Ctrl Pts',(-0.00319892103246907,1.71962752372756,
12.7801255493998));
#72347=CARTESIAN_POINT('Ctrl Pts',(0.318092354642332,1.89140779562403,12.7999958929226));
#72348=CARTESIAN_POINT('Ctrl Pts',(0.34757719926072,2.25454301777328,12.8198662364454));
#72349=CARTESIAN_POINT('Ctrl Pts',(0.0582072819892302,2.47590606024336,
12.8397365799682));
#72350=CARTESIAN_POINT('Ctrl Pts',(-0.284559892434335,2.35242646743737,
12.859606923491));
#72351=CARTESIAN_POINT('Ctrl Pts',(-0.366282104624736,1.99737995550227,
12.8794772670138));
#72352=CARTESIAN_POINT('Ctrl Pts',(-0.111990351120574,1.73647336396665,
12.8993476105365));
#72353=CARTESIAN_POINT('Ctrl Pts',(0.245037304376393,1.80905297125057,12.9192179540593));
#72354=CARTESIAN_POINT('Ctrl Pts',(0.377276590096335,2.14853686866335,12.9390882975821));
#72355=CARTESIAN_POINT('Ctrl Pts',(0.163415969494412,2.4434947965587,12.9589586411049));
#72356=CARTESIAN_POINT('Ctrl Pts',(-0.200356562826449,2.42334301162293,
12.9788289846277));
#72357=CARTESIAN_POINT('Ctrl Pts',(-0.380329211771941,2.10656803189499,
12.9986993281505));
#72358=CARTESIAN_POINT('Ctrl Pts',(-0.211401611228264,1.78376777860929,
13.0185696716733));
#72359=CARTESIAN_POINT('Ctrl Pts',(0.151458236356993,1.75106753433639,13.0384400151961));
#72360=CARTESIAN_POINT('Ctrl Pts',(0.375375677902762,2.03846533019108,13.0583103587189));
#72361=CARTESIAN_POINT('Ctrl Pts',(0.254937217576202,2.38231279733737,13.0781807022417));
#72362=CARTESIAN_POINT('Ctrl Pts',(-0.0993717796601711,2.46717672766403,
13.0980510457644));
#72363=CARTESIAN_POINT('Ctrl Pts',(-0.36252003019322,2.21520595589093,13.1179213892872));
#72364=CARTESIAN_POINT('Ctrl Pts',(-0.29310679059858,1.85754948255962,13.13779173281));
#72365=CARTESIAN_POINT('Ctrl Pts',(0.0451945013969898,1.7223081999728,13.1576620763328));
#72366=CARTESIAN_POINT('Ctrl Pts',(0.342031224084195,1.93354801925746,13.1775324198556));
#72367=CARTESIAN_POINT('Ctrl Pts',(0.325110043695346,2.29748430527921,13.1974027633784));
#72368=CARTESIAN_POINT('Ctrl Pts',(0.00992697299317924,2.48025671492838,
13.2172731069012));
#72369=CARTESIAN_POINT('Ctrl Pts',(-0.314328680327199,2.31419325886201,
13.237143450424));
#72370=CARTESIAN_POINT('Ctrl Pts',(-0.350296176606381,1.95164068828411,
13.2570137939467));
#72371=CARTESIAN_POINT('Ctrl Pts',(-0.0647881917136264,1.72517979117865,
13.2768841374695));
#72372=CARTESIAN_POINT('Ctrl Pts',(0.279910194519454,1.84258056808262,13.2967544809923));
#72373=CARTESIAN_POINT('Ctrl Pts',(0.368303012953287,2.19609810697459,13.3166248245151));
#72374=CARTESIAN_POINT('Ctrl Pts',(0.117820898012969,2.46158919785312,13.3364996043286));
#72375=CARTESIAN_POINT('Ctrl Pts',(-0.11986884365505,2.41719040905852,13.3497509363012));
#72376=CARTESIAN_POINT('Ctrl Pts',(-0.203005792691873,2.34955307066552,
13.3563788204328));
#72377=CARTESIAN_POINT('Ctrl Pts',(0.339316982523676,2.16590180780864,4.32919355271553));
#72378=CARTESIAN_POINT('Ctrl Pts',(0.317376240845729,2.27887088268001,4.33581700055646));
#72379=CARTESIAN_POINT('Ctrl Pts',(0.152140072236355,2.47920395269148,4.34906389623832));
#72380=CARTESIAN_POINT('Ctrl Pts',(-0.237247314916726,2.43314083568054,
4.3689342397611));
#72381=CARTESIAN_POINT('Ctrl Pts',(-0.408159666448758,2.08086921922066,
4.3888045832839));
#72382=CARTESIAN_POINT('Ctrl Pts',(-0.20505268712016,1.74644911680938,4.40867492680669));
#72383=CARTESIAN_POINT('Ctrl Pts',(0.186373697626367,1.73620810823211,4.42854527032948));
#72384=CARTESIAN_POINT('Ctrl Pts',(0.406718025226084,2.0597773819746,4.44841561385227));
#72385=CARTESIAN_POINT('Ctrl Pts',(0.25401079205995,2.42020351937108,4.46828595737505));
#72386=CARTESIAN_POINT('Ctrl Pts',(-0.131746279212509,2.48690827868763,
4.48815630089785));
#72387=CARTESIAN_POINT('Ctrl Pts',(-0.396628750627812,2.19866606826832,
4.50802664442063));
#72388=CARTESIAN_POINT('Ctrl Pts',(-0.297666295542051,1.81991703748627,
4.52789698794343));
#72389=CARTESIAN_POINT('Ctrl Pts',(0.0743685927383873,1.6981029499077,4.54776733146621));
#72390=CARTESIAN_POINT('Ctrl Pts',(0.378178276998698,1.94497627337976,4.56763767498901));
#72391=CARTESIAN_POINT('Ctrl Pts',(0.335061989847928,2.33406194065974,4.58750801851179));
#72392=CARTESIAN_POINT('Ctrl Pts',(-0.0154286364801445,2.50842806818002,
4.60737836203459));
#72393=CARTESIAN_POINT('Ctrl Pts',(-0.351765289137388,2.30811682436188,
4.62724870555736));
#72394=CARTESIAN_POINT('Ctrl Pts',(-0.365405333347371,1.91688684160467,
4.64711904908017));
#72395=CARTESIAN_POINT('Ctrl Pts',(-0.0438356487582682,1.69363819343353,
4.66698939260294));
#72396=CARTESIAN_POINT('Ctrl Pts',(0.317947233881606,1.84317121258462,4.68685973612574));
#72397=CARTESIAN_POINT('Ctrl Pts',(0.388056835848177,2.22830966403225,4.70673007964853));
#72398=CARTESIAN_POINT('Ctrl Pts',(0.102177108770669,2.4957414748595,4.72660042317132));
#72399=CARTESIAN_POINT('Ctrl Pts',(-0.27743619956892,2.40013435350708,4.74647076669411));
#72400=CARTESIAN_POINT('Ctrl Pts',(-0.40253956738364,2.02919482466415,4.7663411102169));
#72401=CARTESIAN_POINT('Ctrl Pts',(-0.158367681353156,1.7232094037697,4.78621145373968));
#72402=CARTESIAN_POINT('Ctrl Pts',(0.231084991683309,1.7628780601152,4.80608179726248));
#72403=CARTESIAN_POINT('Ctrl Pts',(0.408548644658253,2.11181020098235,4.82595214078526));
#72404=CARTESIAN_POINT('Ctrl Pts',(0.211224534813154,2.44990809042533,4.84582248430806));
#72405=CARTESIAN_POINT('Ctrl Pts',(-0.1798693299841,2.46701294250325,4.86569282783084));
#72406=CARTESIAN_POINT('Ctrl Pts',(-0.405957571578824,2.14743338417888,
4.88556317135363));
#72407=CARTESIAN_POINT('Ctrl Pts',(-0.259635007351826,1.78434015331966,
4.90543351487642));
#72408=CARTESIAN_POINT('Ctrl Pts',(0.124867329989842,1.71082185859386,4.92530385839921));
#72409=CARTESIAN_POINT('Ctrl Pts',(0.39482089122616,1.99432152678229,4.94517420192201));
#72410=CARTESIAN_POINT('Ctrl Pts',(0.302580034768886,2.37476680732616,4.96504454544479));
#72411=CARTESIAN_POINT('Ctrl Pts',(-0.0672368110345127,2.50315094826968,
4.98491488896759));
#72412=CARTESIAN_POINT('Ctrl Pts',(-0.375373036180186,2.26169897822225,
5.00478523249037));
#72413=CARTESIAN_POINT('Ctrl Pts',(-0.339155603054294,1.87191020898354,
5.02465557601317));
#72414=CARTESIAN_POINT('Ctrl Pts',(0.00819092400752989,1.69136277138156,
5.04452591953595));
#72415=CARTESIAN_POINT('Ctrl Pts',(0.34802339338622,1.88568436010163,5.06439626305874));
#72416=CARTESIAN_POINT('Ctrl Pts',(0.368591778439678,2.27661137198876,5.08426660658153));
#72417=CARTESIAN_POINT('Ctrl Pts',(0.0510273860142611,2.50552149354335,
5.10413695010432));
#72418=CARTESIAN_POINT('Ctrl Pts',(-0.313347686327946,2.36242085153815,
5.12400729362711));
#72419=CARTESIAN_POINT('Ctrl Pts',(-0.390268914899715,1.97858480361965,
5.1438776371499));
#72420=CARTESIAN_POINT('Ctrl Pts',(-0.109171544366135,1.70613066919371,
5.16374798067268));
#72421=CARTESIAN_POINT('Ctrl Pts',(0.272075855759673,1.79499802531505,5.18361832419548));
#72422=CARTESIAN_POINT('Ctrl Pts',(0.403730698009074,2.16366317094041,5.20348866771826));
#72423=CARTESIAN_POINT('Ctrl Pts',(0.165017587806566,2.47392602418604,5.22335901124106));
#72424=CARTESIAN_POINT('Ctrl Pts',(-0.225076694092472,2.44116265567246,
5.24322935476384));
#72425=CARTESIAN_POINT('Ctrl Pts',(-0.408693750586667,2.095428995681,5.26309969828664));
#72426=CARTESIAN_POINT('Ctrl Pts',(-0.217389929547608,1.75388860986618,
5.28297004180942));
#72427=CARTESIAN_POINT('Ctrl Pts',(0.173339556884877,1.72985830568816,5.30284038533221));
#72428=CARTESIAN_POINT('Ctrl Pts',(0.405053597925272,2.04538261579978,5.32271072885501));
#72429=CARTESIAN_POINT('Ctrl Pts',(0.265186105937205,2.41101094042966,5.34258107237779));
#72430=CARTESIAN_POINT('Ctrl Pts',(-0.117953536419894,2.49132906753156,
5.36245141590058));
#72431=CARTESIAN_POINT('Ctrl Pts',(-0.392886867035704,2.21265604981513,
5.38232175942337));
#72432=CARTESIAN_POINT('Ctrl Pts',(-0.307399983863389,1.83063644312961,
5.40219210294616));
#72433=CARTESIAN_POINT('Ctrl Pts',(0.0600845357746946,1.69572122933572,
5.42206244646895));
#72434=CARTESIAN_POINT('Ctrl Pts',(0.372449673610413,1.93167675004154,5.44193278999174));
#72435=CARTESIAN_POINT('Ctrl Pts',(0.343142940353064,2.32204593744298,5.46180313351452));
#72436=CARTESIAN_POINT('Ctrl Pts',(-0.000950725985197706,2.50871820606524,
5.48167347703732));
#72437=CARTESIAN_POINT('Ctrl Pts',(-0.344172230661694,2.32044716258195,
5.5015438205601));
#72438=CARTESIAN_POINT('Ctrl Pts',(-0.371662568524335,1.92994585860093,
5.5214141640829));
#72439=CARTESIAN_POINT('Ctrl Pts',(-0.0582030970557029,1.6954460785727,
5.54128450760569));
#72440=CARTESIAN_POINT('Ctrl Pts',(0.308649792325372,1.83206944641086,5.56115485112847));
#72441=CARTESIAN_POINT('Ctrl Pts',(0.392358516122868,2.21448262171589,5.58102519465127));
#72442=CARTESIAN_POINT('Ctrl Pts',(0.116131716166284,2.49187357699819,5.60089553817405));
#72443=CARTESIAN_POINT('Ctrl Pts',(-0.266630123467332,2.4097738741548,5.62076588169685));
#72444=CARTESIAN_POINT('Ctrl Pts',(-0.404795123233261,2.04349881367926,
5.64063622521963));
#72445=CARTESIAN_POINT('Ctrl Pts',(-0.171615705312496,1.72905589971106,
5.66050656874243));
#72446=CARTESIAN_POINT('Ctrl Pts',(0.2189977588639,1.75490369827876,5.68037691226521));
#72447=CARTESIAN_POINT('Ctrl Pts',(0.408710593135368,2.09733037305656,5.70024725578801));
#72448=CARTESIAN_POINT('Ctrl Pts',(0.223487099128054,2.44220606711806,5.72011759931079));
#72449=CARTESIAN_POINT('Ctrl Pts',(-0.166755383308063,2.473154281748,5.73998794283358));
#72450=CARTESIAN_POINT('Ctrl Pts',(-0.40402250325452,2.16178424324237,5.75985828635637));
#72451=CARTESIAN_POINT('Ctrl Pts',(-0.270653979162068,1.79373557272706,
5.77972862987916));
#72452=CARTESIAN_POINT('Ctrl Pts',(0.111002724599506,1.70664282009786,5.79959897340195));
#72453=CARTESIAN_POINT('Ctrl Pts',(0.390829540197415,1.98040172928441,5.81946931692473));
#72454=CARTESIAN_POINT('Ctrl Pts',(0.312123459301574,2.3638757700182,5.83933966044753));
#72455=CARTESIAN_POINT('Ctrl Pts',(-0.052913403731456,2.50527971520252,
5.85921000397032));
#72456=CARTESIAN_POINT('Ctrl Pts',(-0.369409422350321,2.27489469553958,
5.87908034749311));
#72457=CARTESIAN_POINT('Ctrl Pts',(-0.347022586514417,1.88406760248188,
5.8989506910159));
#72458=CARTESIAN_POINT('Ctrl Pts',(-0.00628977041069085,1.69132908760561,
5.91882103453869));
#72459=CARTESIAN_POINT('Ctrl Pts',(0.340213053769923,1.87349049933032,5.93869137806147));
#72460=CARTESIAN_POINT('Ctrl Pts',(0.374616716941616,2.26344354143546,5.95856172158427));
#72461=CARTESIAN_POINT('Ctrl Pts',(0.0653605417801722,2.50345938510249,
5.97843206510705));
#72462=CARTESIAN_POINT('Ctrl Pts',(-0.303855032430304,2.37335616897348,
5.99830240862985));
#72463=CARTESIAN_POINT('Ctrl Pts',(-0.394324980513307,1.9924858818933,6.01817275215263));
#72464=CARTESIAN_POINT('Ctrl Pts',(-0.123055441473957,1.71024516145052,
6.03804309567542));
#72465=CARTESIAN_POINT('Ctrl Pts',(0.261100712632129,1.78555144504693,6.05791343919821));
#72466=CARTESIAN_POINT('Ctrl Pts',(0.405732508550515,2.14932146950758,6.077783782721));
#72467=CARTESIAN_POINT('Ctrl Pts',(0.178159963367115,2.46784576020679,6.09765412624379));
#72468=CARTESIAN_POINT('Ctrl Pts',(-0.212850093916746,2.44892164359453,
6.11752446976659));
#72469=CARTESIAN_POINT('Ctrl Pts',(-0.408599166955684,2.10990942037674,
6.13739481328936));
#72470=CARTESIAN_POINT('Ctrl Pts',(-0.229514130066395,1.76180665300904,
6.15726515681217));
#72471=CARTESIAN_POINT('Ctrl Pts',(0.160118875631453,1.72395024063882,6.17713550033494));
#72472=CARTESIAN_POINT('Ctrl Pts',(0.402864611153995,2.03106828793058,6.19700584385775));
#72473=CARTESIAN_POINT('Ctrl Pts',(0.276036911007084,2.40142179684082,6.21687618738052));
#72474=CARTESIAN_POINT('Ctrl Pts',(-0.104017075956755,2.49526184202183,
6.23674653090332));
#72475=CARTESIAN_POINT('Ctrl Pts',(-0.388649556376463,2.22650295718859,
6.2566168744261));
#72476=CARTESIAN_POINT('Ctrl Pts',(-0.316748978680148,1.84169483095733,
6.2764872179489));
#72477=CARTESIAN_POINT('Ctrl Pts',(0.0457256654755972,1.69384653224932,
6.29635756147168));
#72478=CARTESIAN_POINT('Ctrl Pts',(0.366253236544724,1.91858874740084,6.31622790499448));
#72479=CARTESIAN_POINT('Ctrl Pts',(0.35079332395982,2.30975108990015,6.33609824851726));
#72480=CARTESIAN_POINT('Ctrl Pts',(0.0135282928404845,2.50849536244846,
6.35596859204006));
#72481=CARTESIAN_POINT('Ctrl Pts',(-0.336147105249229,2.33250075157222,
6.37583893556284));
#72482=CARTESIAN_POINT('Ctrl Pts',(-0.377453296568852,1.94321835324761,
6.39570927908563));
#72483=CARTESIAN_POINT('Ctrl Pts',(-0.0724974739127934,1.69776177192447,
6.41557962260842));
#72484=CARTESIAN_POINT('Ctrl Pts',(0.298964911418399,1.82130400507063,6.43544996613121));
#72485=CARTESIAN_POINT('Ctrl Pts',(0.396167690920685,2.20051187253084,6.45532030965401));
#72486=CARTESIAN_POINT('Ctrl Pts',(0.129940547364216,2.48751378039983,6.47519065317679));
#72487=CARTESIAN_POINT('Ctrl Pts',(-0.255489358590775,2.41902454998943,
6.49506099669958));
#72488=CARTESIAN_POINT('Ctrl Pts',(-0.406542559774135,2.05787372623439,
6.51493134022237));
#72489=CARTESIAN_POINT('Ctrl Pts',(-0.184648308136553,1.735368023685,6.53480168374516));
#72490=CARTESIAN_POINT('Ctrl Pts',(0.20663562861907,1.74736251924351,6.55467202726795));
#72491=CARTESIAN_POINT('Ctrl Pts',(0.408359507017333,2.08285389613812,6.57454237079073));
#72492=CARTESIAN_POINT('Ctrl Pts',(0.235469130854051,2.43407448909475,6.59441271431353));
#72493=CARTESIAN_POINT('Ctrl Pts',(-0.153432116640315,2.4788272184418,6.61428305783631));
#72494=CARTESIAN_POINT('Ctrl Pts',(-0.401580285013707,2.17605754753732,
6.63415340135911));
#72495=CARTESIAN_POINT('Ctrl Pts',(-0.281333212106144,1.80351543106745,
6.65402374488189));
#72496=CARTESIAN_POINT('Ctrl Pts',(0.096998782850446,1.70295754386386,6.6738940884047));
#72497=CARTESIAN_POINT('Ctrl Pts',(0.386347599733618,1.96663205771569,6.69376443192747));
#72498=CARTESIAN_POINT('Ctrl Pts',(0.321275090337474,2.35265350220752,6.71363477545027));
#72499=CARTESIAN_POINT('Ctrl Pts',(-0.0385235767892308,2.50689975409239,
6.73350511897305));
#72500=CARTESIAN_POINT('Ctrl Pts',(-0.362982106723224,2.28787087599692,
6.75337546249585));
#72501=CARTESIAN_POINT('Ctrl Pts',(-0.354453969290295,1.89649604548453,
6.77324580601863));
#72502=CARTESIAN_POINT('Ctrl Pts',(-0.0207625695840894,1.69180838867837,
6.79311614954142));
#72503=CARTESIAN_POINT('Ctrl Pts',(0.331975661146908,1.86158096498988,6.81298649306421));
#72504=CARTESIAN_POINT('Ctrl Pts',(0.380171417180859,2.25007054810248,6.832856836587));
#72505=CARTESIAN_POINT('Ctrl Pts',(0.0796116536163171,2.50089083359134,
6.85272718010979));
#72506=CARTESIAN_POINT('Ctrl Pts',(-0.293980963993229,2.38394835561892,
6.87259752363258));
#72507=CARTESIAN_POINT('Ctrl Pts',(-0.397886069033289,2.00652191744416,
6.89246786715536));
#72508=CARTESIAN_POINT('Ctrl Pts',(-0.136784873032339,1.71484889412257,
6.91233821067817));
#72509=CARTESIAN_POINT('Ctrl Pts',(0.249797822396835,1.77649957685518,6.93220855420094));
#72510=CARTESIAN_POINT('Ctrl Pts',(0.407225022679635,2.13491785721739,6.95207889772374));
#72511=CARTESIAN_POINT('Ctrl Pts',(0.191078703334628,2.46130375721966,6.97194924124652));
#72512=CARTESIAN_POINT('Ctrl Pts',(-0.200356313303394,2.45624264703787,
6.99181958476931));
#72513=CARTESIAN_POINT('Ctrl Pts',(-0.407991688534603,2.1243774062559,7.0116899282921));
#72514=CARTESIAN_POINT('Ctrl Pts',(-0.241350232588205,1.77014921391832,
7.03156027181489));
#72515=CARTESIAN_POINT('Ctrl Pts',(0.146697204890655,1.71851421268106,7.05143061533769));
#72516=CARTESIAN_POINT('Ctrl Pts',(0.400169927903416,2.01684048670864,7.07130095886047));
#72517=CARTESIAN_POINT('Ctrl Pts',(0.286541220281133,2.3914542930356,7.09117130238326));
#72518=CARTESIAN_POINT('Ctrl Pts',(-0.0899500478844393,2.4986984634215,
7.11104164590605));
#72519=CARTESIAN_POINT('Ctrl Pts',(-0.383924392709289,2.24019107151272,
7.13091198942884));
#72520=CARTESIAN_POINT('Ctrl Pts',(-0.325700373809799,1.85307745678201,
7.15078233295163));
#72521=CARTESIAN_POINT('Ctrl Pts',(0.0313093979581721,1.69248165998501,
7.17065267647442));
#72522=CARTESIAN_POINT('Ctrl Pts',(0.359597059489159,1.90572846153944,7.19052301999722));
#72523=CARTESIAN_POINT('Ctrl Pts',(0.358003373657915,2.29719295194969,7.21039336352));
#72524=CARTESIAN_POINT('Ctrl Pts',(0.0279903302538735,2.50775975434238,
7.23026370704279));
#72525=CARTESIAN_POINT('Ctrl Pts',(-0.327700030618726,2.34426249360385,
7.25013405056558));
#72526=CARTESIAN_POINT('Ctrl Pts',(-0.382770225729345,1.95668764831954,
7.27000439408837));
#72527=CARTESIAN_POINT('Ctrl Pts',(-0.0867008481940784,1.70058237548712,
7.28987473761115));
#72528=CARTESIAN_POINT('Ctrl Pts',(0.288904754304601,1.8108883973458,7.30974508113395));
#72529=CARTESIAN_POINT('Ctrl Pts',(0.399479575559559,2.18641495564909,7.32961542465673));
#72530=CARTESIAN_POINT('Ctrl Pts',(0.143586270471979,2.48266755647825,7.34948576817953));
#72531=CARTESIAN_POINT('Ctrl Pts',(-0.244027890268046,2.42787476972223,
7.36935611170232));
#72532=CARTESIAN_POINT('Ctrl Pts',(-0.40777968308453,2.07230151786536,7.3892264552251));
#72533=CARTESIAN_POINT('Ctrl Pts',(-0.197449130861913,1.74213785255918,
7.4090967987479));
#72534=CARTESIAN_POINT('Ctrl Pts',(0.194014118654607,1.74026398899783,7.42896714227067));
#72535=CARTESIAN_POINT('Ctrl Pts',(0.407495826942742,2.06839894189536,7.44883748579348));
#72536=CARTESIAN_POINT('Ctrl Pts',(0.247155589558341,2.42552356350831,7.46870782931626));
#72537=CARTESIAN_POINT('Ctrl Pts',(-0.139916254050637,2.48402463163385,
7.48857817283906));
#72538=CARTESIAN_POINT('Ctrl Pts',(-0.398633982446133,2.19023538046806,
7.50844851636183));
#72539=CARTESIAN_POINT('Ctrl Pts',(-0.291659301063552,1.81366745216059,
7.52831885988464));
#72540=CARTESIAN_POINT('Ctrl Pts',(0.0828730832164083,1.69977065583932,
7.54818920340741));
#72541=CARTESIAN_POINT('Ctrl Pts',(0.381380695796822,1.95302979648033,7.56805954693022));
#72542=CARTESIAN_POINT('Ctrl Pts',(0.33002344027702,2.34111409066416,7.587929890453));
#72543=CARTESIAN_POINT('Ctrl Pts',(-0.0240853930625828,2.50800903138302,
7.60780023397579));
#72544=CARTESIAN_POINT('Ctrl Pts',(-0.356099157197443,2.30061123122186,
7.62767057749858));
#72545=CARTESIAN_POINT('Ctrl Pts',(-0.361440423126325,1.90917993716765,
7.64754092102137));
#72546=CARTESIAN_POINT('Ctrl Pts',(-0.0352093065071765,1.69280007295633,
7.66741126454416));
#72547=CARTESIAN_POINT('Ctrl Pts',(0.323321555518063,1.84997070654329,7.68728160806695));
#72548=CARTESIAN_POINT('Ctrl Pts',(0.385248906610621,2.23650917846211,7.70715195158974));
#72549=CARTESIAN_POINT('Ctrl Pts',(0.093762832790653,2.49781906318847,7.72702229511252));
#72550=CARTESIAN_POINT('Ctrl Pts',(-0.283737875457696,2.39418411561442,
7.74689263863532));
#72551=CARTESIAN_POINT('Ctrl Pts',(-0.400947710397322,2.02067529151503,
7.7667629821581));
#72552=CARTESIAN_POINT('Ctrl Pts',(-0.150342605149271,1.71993608836669,
7.7866333256809));
#72553=CARTESIAN_POINT('Ctrl Pts',(0.238181373025728,1.76785378311253,7.80650366920368));
#72554=CARTESIAN_POINT('Ctrl Pts',(0.408206366915563,2.12047041422831,7.82637401272647));
#72555=CARTESIAN_POINT('Ctrl Pts',(0.203757591439083,2.45430822708488,7.84624435624926));
#72556=CARTESIAN_POINT('Ctrl Pts',(-0.187611035091498,2.46311647630062,
7.86611469977205));
#72557=CARTESIAN_POINT('Ctrl Pts',(-0.406872077861732,2.13881479235495,
7.88598504329484));
#72558=CARTESIAN_POINT('Ctrl Pts',(-0.252883379825488,1.77890582058044,
7.90585538681763));
#72559=CARTESIAN_POINT('Ctrl Pts',(0.133091392237208,1.71355704539811,7.92572573034042));
#72560=CARTESIAN_POINT('Ctrl Pts',(0.396972930679207,2.00271707160533,7.9455960738632));
#72561=CARTESIAN_POINT('Ctrl Pts',(0.296685848207505,2.38112094073988,7.965466417386));
#72562=CARTESIAN_POINT('Ctrl Pts',(-0.0757701098635524,2.50163461790581,
7.98533676090879));
#72563=CARTESIAN_POINT('Ctrl Pts',(-0.378717307303803,2.25370321075903,
8.00520710443158));
#72564=CARTESIAN_POINT('Ctrl Pts',(-0.334242932998583,1.8647700325435,8.02507744795437));
#72565=CARTESIAN_POINT('Ctrl Pts',(0.0168538292664106,1.69162832580094,
8.04494779147715));
#72566=CARTESIAN_POINT('Ctrl Pts',(0.352489497621136,1.89311203535275,8.06481813499996));
#72567=CARTESIAN_POINT('Ctrl Pts',(0.364764039020369,2.28438728721533,8.08468847852272));
#72568=CARTESIAN_POINT('Ctrl Pts',(0.0424172327582309,2.5065123051203,8.10455882204554));
#72569=CARTESIAN_POINT('Ctrl Pts',(-0.318841609974788,2.35571762473041,
8.1244291655683));
#72570=CARTESIAN_POINT('Ctrl Pts',(-0.387606681921568,1.97033683646142,
8.14429950909111));
#72571=CARTESIAN_POINT('Ctrl Pts',(-0.100795391090152,1.70390434869331,
8.16416985261388));
#72572=CARTESIAN_POINT('Ctrl Pts',(0.278481949013075,1.80083569744543,8.18404019613669));
#72573=CARTESIAN_POINT('Ctrl Pts',(0.402290012790745,2.17220956624924,8.20391053965947));
#72574=CARTESIAN_POINT('Ctrl Pts',(0.157051756672742,2.47734098846412,8.22378088318227));
#72575=CARTESIAN_POINT('Ctrl Pts',(-0.23226010552649,2.43631342410006,8.24365122670504));
#72576=CARTESIAN_POINT('Ctrl Pts',(-0.408504940263331,2.08676407806253,
8.26352157022785));
#72577=CARTESIAN_POINT('Ctrl Pts',(-0.21000210523437,1.74935688849456,8.28339191375062));
#72578=CARTESIAN_POINT('Ctrl Pts',(0.181149072142079,1.73361701798371,8.30326225727343));
#72579=CARTESIAN_POINT('Ctrl Pts',(0.406120637047456,2.0539836549338,8.32313260079619));
#72580=CARTESIAN_POINT('Ctrl Pts',(0.258531805794025,2.41656402392243,8.34300294431901));
#72581=CARTESIAN_POINT('Ctrl Pts',(-0.126224761348229,2.48873999726252,
8.36287328784177));
#72582=CARTESIAN_POINT('Ctrl Pts',(-0.395187293903045,2.20429994528604,
8.38274363136458));
#72583=CARTESIAN_POINT('Ctrl Pts',(-0.301619284193786,1.82417889266499,
8.40261397488735));
#72584=CARTESIAN_POINT('Ctrl Pts',(0.0686433570055766,1.69708615637076,
8.42248431841017));
#72585=CARTESIAN_POINT('Ctrl Pts',(0.375935063101534,1.93961201983962,8.44235466193292));
#72586=CARTESIAN_POINT('Ctrl Pts',(0.338357527739257,2.32927202025381,8.46222500545575));
#72587=CARTESIAN_POINT('Ctrl Pts',(-0.0096169761058694,2.5086061546522,
8.4820953489785));
#72588=CARTESIAN_POINT('Ctrl Pts',(-0.348769213606931,2.3130997688621,8.50196569250134));
#72589=CARTESIAN_POINT('Ctrl Pts',(-0.367973178264597,1.9221033560549,8.52183603602408));
#72590=CARTESIAN_POINT('Ctrl Pts',(-0.0496118468891722,1.69430289562615,
8.5417063795469));
#72591=CARTESIAN_POINT('Ctrl Pts',(0.314261599964,1.83867429778694,8.56157672306968));
#72592=CARTESIAN_POINT('Ctrl Pts',(0.389842811703776,2.22277645544637,8.58144706659247));
#72593=CARTESIAN_POINT('Ctrl Pts',(0.107796316011759,2.49424792973885,8.60131741011526));
#72594=CARTESIAN_POINT('Ctrl Pts',(-0.273138624477781,2.40405060050503,
8.62118775363805));
#72595=CARTESIAN_POINT('Ctrl Pts',(-0.403506061474943,2.03492823805935,
8.64105809716085));
#72596=CARTESIAN_POINT('Ctrl Pts',(-0.163711619458762,1.72550035847378,
8.66092844068362));
#72597=CARTESIAN_POINT('Ctrl Pts',(0.226265946086376,1.75962491646608,8.68079878420643));
#72598=CARTESIAN_POINT('Ctrl Pts',(0.408675309424305,2.10599727571742,8.7006691277292));
#72599=CARTESIAN_POINT('Ctrl Pts',(0.216180712484905,2.44686795095338,8.72053947125199));
#72600=CARTESIAN_POINT('Ctrl Pts',(-0.174630257812926,2.46953450299704,
8.74040981477478));
#72601=CARTESIAN_POINT('Ctrl Pts',(-0.405241740330249,2.15320345612076,
8.76028015829757));
#72602=CARTESIAN_POINT('Ctrl Pts',(-0.264099094775818,1.78806548125019,
8.78015050182035));
#72603=CARTESIAN_POINT('Ctrl Pts',(0.119318516390275,1.7090849612825,8.80002084534317));
#72604=CARTESIAN_POINT('Ctrl Pts',(0.393277632517502,1.98871577106116,8.81989118886592));
#72605=CARTESIAN_POINT('Ctrl Pts',(0.306458060724967,2.37043471091148,8.83976153238875));
#72606=CARTESIAN_POINT('Ctrl Pts',(-0.061495061285089,2.5040666198619,8.85963187591151));
#72607=CARTESIAN_POINT('Ctrl Pts',(-0.373034836362701,2.26702241379209,
8.87950221943433));
#72608=CARTESIAN_POINT('Ctrl Pts',(-0.34236593318474,1.87675788111643,8.89937256295709));
#72609=CARTESIAN_POINT('Ctrl Pts',(0.00237710477717516,1.69128760084632,
8.9192429064799));
#72610=CARTESIAN_POINT('Ctrl Pts',(0.344939472719621,1.88075530563092,8.93911325000267));
#72611=CARTESIAN_POINT('Ctrl Pts',(0.371066833710637,2.27135017002922,8.95898359352548));
#72612=CARTESIAN_POINT('Ctrl Pts',(0.0567908909599779,2.50475458064494,
8.97885393704825));
#72613=CARTESIAN_POINT('Ctrl Pts',(-0.309582962864796,2.36685176587936,
8.99872428057106));
#72614=CARTESIAN_POINT('Ctrl Pts',(-0.391956594175766,1.98414878450696,
9.01859462409382));
#72615=CARTESIAN_POINT('Ctrl Pts',(-0.114763410402393,1.7077235216306,9.03846496761665));
#72616=CARTESIAN_POINT('Ctrl Pts',(0.267709578787657,1.79115852403795,9.05833531113939));
#72617=CARTESIAN_POINT('Ctrl Pts',(0.404595474808187,2.15791353567016,9.07820565466223));
#72618=CARTESIAN_POINT('Ctrl Pts',(0.170320103392353,2.47154076254093,9.09807599818497));
#72619=CARTESIAN_POINT('Ctrl Pts',(-0.220200775897656,2.44432992048782,
9.1179463417078));
#72620=CARTESIAN_POINT('Ctrl Pts',(-0.408717420930249,2.10124325267291,
9.13781668523057));
#72621=CARTESIAN_POINT('Ctrl Pts',(-0.222291474111769,1.75701606978417,
9.15768702875338));
#72622=CARTESIAN_POINT('Ctrl Pts',(0.168056637952715,1.7274299498227,9.17755737227614));
#72623=CARTESIAN_POINT('Ctrl Pts',(0.4042356635409,2.03962613006664,9.19742771579896));
#72624=CARTESIAN_POINT('Ctrl Pts',(0.26958349954657,2.40720711681421,9.21729805932172));
#72625=CARTESIAN_POINT('Ctrl Pts',(-0.112374824802301,2.49296739635717,
9.23716840284454));
#72626=CARTESIAN_POINT('Ctrl Pts',(-0.391244545846019,2.21823358742262,
9.25703874636729));
#72627=CARTESIAN_POINT('Ctrl Pts',(-0.311200659211308,1.83503655807729,
9.2769090898901));
#72628=CARTESIAN_POINT('Ctrl Pts',(0.0543274661056586,1.69490741518066,
9.29677943341289));
#72629=CARTESIAN_POINT('Ctrl Pts',(0.370017537287338,1.9263955704802,9.31664977693567));
#72630=CARTESIAN_POINT('Ctrl Pts',(0.346266891346911,2.31714215575524,9.33652012045848));
#72631=CARTESIAN_POINT('Ctrl Pts',(0.00486351257623498,2.50869037435998,
9.35639046398124));
#72632=CARTESIAN_POINT('Ctrl Pts',(-0.341001476875684,2.32532081265983,
9.37626080750406));
#72633=CARTESIAN_POINT('Ctrl Pts',(-0.374044034453256,1.93525008000303,
9.39613115102683));
#72634=CARTESIAN_POINT('Ctrl Pts',(-0.0639521119170938,1.69631497026714,
9.41600149454963));
#72635=CARTESIAN_POINT('Ctrl Pts',(0.304807167009143,1.8277059185569,9.43587183807241));
#72636=CARTESIAN_POINT('Ctrl Pts',(0.393947365953243,2.20888961707887,9.45574218159522));
#72637=CARTESIAN_POINT('Ctrl Pts',(0.121694487726267,2.49018191591375,9.47561252511798));
#72638=CARTESIAN_POINT('Ctrl Pts',(-0.262196515781061,2.41353542536905,
9.49548286864081));
#72639=CARTESIAN_POINT('Ctrl Pts',(-0.405557910891673,2.04926286604208,
9.51535321216356));
#72640=CARTESIAN_POINT('Ctrl Pts',(-0.176875134483156,1.73153471988443,
9.53522355568638));
#72641=CARTESIAN_POINT('Ctrl Pts',(0.214066498438447,1.75182330621452,9.55509389920915));
#72642=CARTESIAN_POINT('Ctrl Pts',(0.408631261564984,2.09151660911612,9.57496424273194));
#72643=CARTESIAN_POINT('Ctrl Pts',(0.228332472328555,2.4389922682443,9.59483458625474));
#72644=CARTESIAN_POINT('Ctrl Pts',(-0.161430275610144,2.47548867088836,
9.61470492977751));
#72645=CARTESIAN_POINT('Ctrl Pts',(-0.40310272242407,2.16752533615898,9.63457527330032));
#72646=CARTESIAN_POINT('Ctrl Pts',(-0.274983298894178,1.79761669824813,
9.65444561682311));
#72647=CARTESIAN_POINT('Ctrl Pts',(0.10539586577539,1.70510357392534,9.67431596034588));
#72648=CARTESIAN_POINT('Ctrl Pts',(0.389088671947512,1.97485416023215,9.69418630386868));
#72649=CARTESIAN_POINT('Ctrl Pts',(0.315845591247362,2.35940901745832,9.71405664739145));
#72650=CARTESIAN_POINT('Ctrl Pts',(-0.0471428209277333,2.50599141651525,
9.73392699091427));
#72651=CARTESIAN_POINT('Ctrl Pts',(-0.366884112817172,2.28013196165989,
9.75379733443704));
#72652=CARTESIAN_POINT('Ctrl Pts',(-0.350059177958651,1.88902595473377,
9.77366767795985));
#72653=CARTESIAN_POINT('Ctrl Pts',(-0.0121026035768215,1.69145991281669,
9.79353802148261));
#72654=CARTESIAN_POINT('Ctrl Pts',(0.336956461966044,1.86867378317966,9.81340836500543));
#72655=CARTESIAN_POINT('Ctrl Pts',(0.376903846135107,2.25809796525461,9.83327870852819));
#72656=CARTESIAN_POINT('Ctrl Pts',(0.0710932623005305,2.50248878730288,
9.85314905205098));
#72657=CARTESIAN_POINT('Ctrl Pts',(-0.29993571122108,2.37765094090132,9.87301939557379));
#72658=CARTESIAN_POINT('Ctrl Pts',(-0.395814502257283,1.99810615498519,
9.89288973909658));
#72659=CARTESIAN_POINT('Ctrl Pts',(-0.128587372751106,1.71203510027575,
9.91276008261936));
#72660=CARTESIAN_POINT('Ctrl Pts',(0.25660116566415,1.78186902441152,9.93263042614216));
#72661=CARTESIAN_POINT('Ctrl Pts',(0.406393067676822,2.14354480902822,9.95250076966494));
#72662=CARTESIAN_POINT('Ctrl Pts',(0.183374655516321,2.46527415945199,9.97237111318774));
#72663=CARTESIAN_POINT('Ctrl Pts',(-0.207865038875306,2.45191419616498,
9.99224145671052));
#72664=CARTESIAN_POINT('Ctrl Pts',(-0.408416858368564,2.1157208666883,10.0121118002334));
#72665=CARTESIAN_POINT('Ctrl Pts',(-0.234301811243212,1.76510578222783,
10.0319821437561));
#72666=CARTESIAN_POINT('Ctrl Pts',(0.154753250386496,1.72171055084248,10.0518524872789));
#72667=CARTESIAN_POINT('Ctrl Pts',(0.401843272539226,2.02534438960102,10.0717228308017));
#72668=CARTESIAN_POINT('Ctrl Pts',(0.280296798158863,2.39746458745702,10.0915931743245));
#72669=CARTESIAN_POINT('Ctrl Pts',(-0.0983838295689201,2.496701522468,10.1114635178473));
#72670=CARTESIAN_POINT('Ctrl Pts',(-0.386810687416164,2.23201881665018,
10.1313338613701));
#72671=CARTESIAN_POINT('Ctrl Pts',(-0.320391399079057,1.84622681929478,
10.1512042048929));
#72672=CARTESIAN_POINT('Ctrl Pts',(0.0399433805627204,1.69323716713753,
10.1710745484156));
#72673=CARTESIAN_POINT('Ctrl Pts',(0.363635546338438,1.9133970383723,10.1909448919385));
#72674=CARTESIAN_POINT('Ctrl Pts',(0.353741602858043,2.3047397232012,10.2108152354612));
#72675=CARTESIAN_POINT('Ctrl Pts',(0.019337896326029,2.50826158478941,10.230685578984));
#72676=CARTESIAN_POINT('Ctrl Pts',(-0.332805697468255,2.3372590221293,10.2505559225068));
#72677=CARTESIAN_POINT('Ctrl Pts',(-0.3796453712399,1.94860360656475,10.2704262660296));
#72678=CARTESIAN_POINT('Ctrl Pts',(-0.0782121009491967,1.69883377121922,
10.2902966095524));
#72679=CARTESIAN_POINT('Ctrl Pts',(0.294970124346321,1.81707933692959,10.3101669530752));
#72680=CARTESIAN_POINT('Ctrl Pts',(0.397557417110412,2.19486609483677,10.330037296598));
#72681=CARTESIAN_POINT('Ctrl Pts',(0.135439902230809,2.48562612558382,10.3499076401208));
#72682=CARTESIAN_POINT('Ctrl Pts',(-0.250925284467851,2.42262668436416,
10.3697779836436));
#72683=CARTESIAN_POINT('Ctrl Pts',(-0.407100683060082,2.06366118189736,
10.3896483271663));
#72684=CARTESIAN_POINT('Ctrl Pts',(-0.189816626698134,1.73803159795637,
10.4095186706891));
#72685=CARTESIAN_POINT('Ctrl Pts',(0.20159834345907,1.7444587453422,10.4293890142119));
#72686=CARTESIAN_POINT('Ctrl Pts',(0.408074278628758,2.07704659130546,10.4492593577347));
#72687=CARTESIAN_POINT('Ctrl Pts',(0.240197617453087,2.43069106492155,10.4691297012575));
#72688=CARTESIAN_POINT('Ctrl Pts',(-0.148027657782962,2.48097150599536,
10.4890000447803));
#72689=CARTESIAN_POINT('Ctrl Pts',(-0.400457709149021,2.18176245490564,
10.5088703883031));
#72690=CARTESIAN_POINT('Ctrl Pts',(-0.285522329765078,1.80754748239312,
10.5287407318259));
#72691=CARTESIAN_POINT('Ctrl Pts',(0.0913409168230976,1.70161788096979,
10.5486110753487));
#72692=CARTESIAN_POINT('Ctrl Pts',(0.384411307169034,1.96114963892855,10.5684814188715));
#72693=CARTESIAN_POINT('Ctrl Pts',(0.324836656061238,2.3480577004006,10.5883517623942));
#72694=CARTESIAN_POINT('Ctrl Pts',(-0.0327314044652889,2.50740659176162,
10.608222105917));
#72695=CARTESIAN_POINT('Ctrl Pts',(-0.360272857373261,2.2930153985805,10.6280924494398));
#72696=CARTESIAN_POINT('Ctrl Pts',(-0.357313010361907,1.90155885387553,
10.6479627929626));
#72697=CARTESIAN_POINT('Ctrl Pts',(-0.0265671201173655,1.69214504541719,
10.6678331364854));
#72698=CARTESIAN_POINT('Ctrl Pts',(0.328550486048048,1.85688263335032,10.6877034800082));
#72699=CARTESIAN_POINT('Ctrl Pts',(0.382267749374136,2.24464730774375,10.707573823531));
#72700=CARTESIAN_POINT('Ctrl Pts',(0.0853063937042612,2.49971776923506,
10.7274441670538));
#72701=CARTESIAN_POINT('Ctrl Pts',(-0.289911964772453,2.3881015941137,10.7473145105766));
#72702=CARTESIAN_POINT('Ctrl Pts',(-0.399175563520518,2.01219142788338,
10.7671848540993));
#72703=CARTESIAN_POINT('Ctrl Pts',(-0.14224992558436,1.71683367251242,10.7870551976221));
#72704=CARTESIAN_POINT('Ctrl Pts',(0.245170653496777,1.77297885922612,10.8069255411449));
#72705=CARTESIAN_POINT('Ctrl Pts',(0.407680534965181,2.12912142269167,10.8267958846677));
#72706=CARTESIAN_POINT('Ctrl Pts',(0.196199026296186,2.45854904536132,10.8466662281905));
#72707=CARTESIAN_POINT('Ctrl Pts',(-0.19526837891403,2.45905673095678,10.8665365717133));
#72708=CARTESIAN_POINT('Ctrl Pts',(-0.407603629859947,2.13017874705938,
10.8864069152361));
#72709=CARTESIAN_POINT('Ctrl Pts',(-0.246018040632845,1.77361587120043,
10.9062772587589));
#72710=CARTESIAN_POINT('Ctrl Pts',(0.141255608542999,1.71646600032822,10.9261476022817));
#72711=CARTESIAN_POINT('Ctrl Pts',(0.398946467095265,2.01115636071566,10.9460179458045));
#72712=CARTESIAN_POINT('Ctrl Pts',(0.290658253744821,2.38734866517715,10.9658882893272));
#72713=CARTESIAN_POINT('Ctrl Pts',(-0.0842693378683556,2.49993768832696,
10.98575863285));
#72714=CARTESIAN_POINT('Ctrl Pts',(-0.381891284221727,2.24563832903655,
11.0056289763728));
#72715=CARTESIAN_POINT('Ctrl Pts',(-0.329179967105375,1.85773562972326,
11.0254993198956));
#72716=CARTESIAN_POINT('Ctrl Pts',(0.025509156024298,1.69207750882305,11.0453696634184));
#72717=CARTESIAN_POINT('Ctrl Pts',(0.356797101259684,1.90063273994518,11.0652400069412));
#72718=CARTESIAN_POINT('Ctrl Pts',(0.360772279628483,2.29208029076599,11.085110350464));
#72719=CARTESIAN_POINT('Ctrl Pts',(0.0337880061489971,2.50732032417933,
11.1049806939868));
#72720=CARTESIAN_POINT('Ctrl Pts',(-0.324192163150517,2.34889941181302,
11.1248510375096));
#72721=CARTESIAN_POINT('Ctrl Pts',(-0.384770157537106,1.96214717370342,
11.1447213810323));
#72722=CARTESIAN_POINT('Ctrl Pts',(-0.0923739141103156,1.70185613675329,
11.1645917245551));
#72723=CARTESIAN_POINT('Ctrl Pts',(0.284762819939848,1.80680789193946,11.1844620680779));
#72724=CARTESIAN_POINT('Ctrl Pts',(0.400668433652508,2.18072349176992,11.2043324116007));
#72725=CARTESIAN_POINT('Ctrl Pts',(0.14901530557076,2.48058627741254,11.2242027551235));
#72726=CARTESIAN_POINT('Ctrl Pts',(-0.239339078770172,2.43131296567223,
11.2440730986463));
#72727=CARTESIAN_POINT('Ctrl Pts',(-0.408132441412818,2.07810511211504,
11.2639434421691));
#72728=CARTESIAN_POINT('Ctrl Pts',(-0.202519851273868,1.74498283747248,
11.2838137856919));
#72729=CARTESIAN_POINT('Ctrl Pts',(0.188877131820711,1.73754047822651,11.3036841292147));
#72730=CARTESIAN_POINT('Ctrl Pts',(0.407005059769387,2.0626053857996,11.3235544727375));
#72731=CARTESIAN_POINT('Ctrl Pts',(0.251761254115174,2.42197476108452,11.3434248162603));
#72732=CARTESIAN_POINT('Ctrl Pts',(-0.134439227989904,2.48597612598004,
11.363295159783));
#72733=CARTESIAN_POINT('Ctrl Pts',(-0.397310020662451,2.19589694119357,
11.3831655033058));
#72734=CARTESIAN_POINT('Ctrl Pts',(-0.295702958252331,1.81784536805166,
11.4030358468286));
#72735=CARTESIAN_POINT('Ctrl Pts',(0.0771713120316593,1.69863225783778,
11.4229061903514));
#72736=CARTESIAN_POINT('Ctrl Pts',(0.379251409452053,1.94761940977372,11.4427765338742));
#72737=CARTESIAN_POINT('Ctrl Pts',(0.3334199691174,2.33639500849813,11.462646877397));
#72738=CARTESIAN_POINT('Ctrl Pts',(-0.0182789018524544,2.50831036919989,
11.4825172209198));
#72739=CARTESIAN_POINT('Ctrl Pts',(-0.353209368820466,2.30565655259809,
11.5023875644426));
#72740=CARTESIAN_POINT('Ctrl Pts',(-0.364118325009206,1.91434084659901,
11.5222579079654));
#72741=CARTESIAN_POINT('Ctrl Pts',(-0.0409982882357931,1.69334213863394,
11.5421282514881));
#72742=CARTESIAN_POINT('Ctrl Pts',(0.319732096581014,1.84539665700351,11.5619985950109));
#72743=CARTESIAN_POINT('Ctrl Pts',(0.38715181037918,2.23101508145708,11.5818689385337));
#72744=CARTESIAN_POINT('Ctrl Pts',(0.09941244411412,2.49644500476653,11.6017392820565));
#72745=CARTESIAN_POINT('Ctrl Pts',(-0.27952430584347,2.39819060731654,11.6216096255793));
#72746=CARTESIAN_POINT('Ctrl Pts',(-0.402035558987686,2.02638692263911,
11.6414799691021));
#72747=CARTESIAN_POINT('Ctrl Pts',(-0.155733918959777,1.72211321492475,
11.6613503126249));
#72748=CARTESIAN_POINT('Ctrl Pts',(0.233432390455118,1.76449918787656,11.6812206561477));
#72749=CARTESIAN_POINT('Ctrl Pts',(0.408456260577788,2.11466148164041,11.7010909996705));
#72750=CARTESIAN_POINT('Ctrl Pts',(0.208777117919,2.45137386197968,11.7209613431933));
#72751=CARTESIAN_POINT('Ctrl Pts',(-0.182426607992394,2.46574855918441,
11.740831686716));
#72752=CARTESIAN_POINT('Ctrl Pts',(-0.406278756210843,2.14459874550758,
11.7607020302388));
#72753=CARTESIAN_POINT('Ctrl Pts',(-0.257425455464066,1.78253565439849,
11.7805723737616));
#72754=CARTESIAN_POINT('Ctrl Pts',(0.127580655359801,1.71170288151077,11.8004427172844));
#72755=CARTESIAN_POINT('Ctrl Pts',(0.395548883428907,1.99707985295762,11.8203130608072));
#72756=CARTESIAN_POINT('Ctrl Pts',(0.300654860069938,2.37687204800306,11.84018340433));
#72757=CARTESIAN_POINT('Ctrl Pts',(-0.0700490669399977,2.50267183173139,
11.8600537478528));
#72758=CARTESIAN_POINT('Ctrl Pts',(-0.376492511351822,2.25907502866596,
11.8799240913756));
#72759=CARTESIAN_POINT('Ctrl Pts',(-0.3375553314255,1.86954854290914,11.8997944348984));
#72760=CARTESIAN_POINT('Ctrl Pts',(0.0110429110749629,1.69142989590026,
11.9196647784211));
#72761=CARTESIAN_POINT('Ctrl Pts',(0.34951078602074,1.88811869760584,11.9395351219439));
#72762=CARTESIAN_POINT('Ctrl Pts',(0.367350096389415,2.27917974922343,11.9594054654667));
#72763=CARTESIAN_POINT('Ctrl Pts',(0.048195703520538,2.50586777404869,11.9792758089895));
#72764=CARTESIAN_POINT('Ctrl Pts',(-0.315171686075873,2.36022737009233,
11.9991461525123));
#72765=CARTESIAN_POINT('Ctrl Pts',(-0.389411960448281,1.97586378083369,
12.0190164960351));
#72766=CARTESIAN_POINT('Ctrl Pts',(-0.106419774760711,1.70537827303992,
12.0388868395579));
#72767=CARTESIAN_POINT('Ctrl Pts',(0.274198066525711,1.79690447683503,12.0587571830807));
#72768=CARTESIAN_POINT('Ctrl Pts',(0.403276510470796,2.16647956040453,12.0786275266035));
#72769=CARTESIAN_POINT('Ctrl Pts',(0.162403657198292,2.47506869767777,12.0984978701262));
#72770=CARTESIAN_POINT('Ctrl Pts',(-0.227452442292167,2.43958336582408,
12.118368213649));
#72771=CARTESIAN_POINT('Ctrl Pts',(-0.408651890833478,2.0925765259275,12.1382385571718));
#72772=CARTESIAN_POINT('Ctrl Pts',(-0.214968862466393,1.75237971287771,
12.1581089006946));
#72773=CARTESIAN_POINT('Ctrl Pts',(0.175918831845622,1.73107718903387,12.1779792442174));
#72774=CARTESIAN_POINT('Ctrl Pts',(0.405424947125643,2.04821111994596,12.1978495877402));
#72775=CARTESIAN_POINT('Ctrl Pts',(0.263008867040487,2.41285429788827,12.217719931263));
#72776=CARTESIAN_POINT('Ctrl Pts',(-0.120682043130275,2.49049624878478,
12.2375902747857));
#72777=CARTESIAN_POINT('Ctrl Pts',(-0.393663608105616,2.2099110526851,12.2574606183086));
#72778=CARTESIAN_POINT('Ctrl Pts',(-0.305512405104942,1.82849742878552,
12.2773309618313));
#72779=CARTESIAN_POINT('Ctrl Pts',(0.0629048378212723,1.69615045223776,
12.2972013053541));
#72780=CARTESIAN_POINT('Ctrl Pts',(0.373615455766835,1.93428045661052,12.3170716488769));
#72781=CARTESIAN_POINT('Ctrl Pts',(0.34158475619773,2.3244355813645,12.3369419923997));
#72782=CARTESIAN_POINT('Ctrl Pts',(-0.00380345461739179,2.50870161436193,
12.3568123359225));
#72783=CARTESIAN_POINT('Ctrl Pts',(-0.345702513614639,2.31803955588287,
12.3766826794453));
#72784=CARTESIAN_POINT('Ctrl Pts',(-0.370466579517922,1.92735588828642,
12.3965530229681));
#72785=CARTESIAN_POINT('Ctrl Pts',(-0.0553779931841099,1.69504968981369,
12.4164233664909));
#72786=CARTESIAN_POINT('Ctrl Pts',(0.310512362863123,1.8342302719303,12.4362937100137));
#72787=CARTESIAN_POINT('Ctrl Pts',(0.391549898424466,2.21721839826952,12.4561640535365));
#72788=CARTESIAN_POINT('Ctrl Pts',(0.113393706886654,2.4926746020404,12.4760343970593));
#72789=CARTESIAN_POINT('Ctrl Pts',(-0.268785773560433,2.40790531625907,
12.495904740582));
#72790=CARTESIAN_POINT('Ctrl Pts',(-0.404390898644675,2.04067482033373,
12.5157750841048));
#72791=CARTESIAN_POINT('Ctrl Pts',(-0.169022427072041,1.72786710035828,
12.5356454276276));
#72792=CARTESIAN_POINT('Ctrl Pts',(0.221401111013555,1.75644065448449,12.5555157711504));
#72793=CARTESIAN_POINT('Ctrl Pts',(0.408719270783773,2.10018313673971,12.5753861146732));
#72794=CARTESIAN_POINT('Ctrl Pts',(0.221093141714138,2.44375761596807,12.595256458196));
#72795=CARTESIAN_POINT('Ctrl Pts',(-0.169355845764872,2.47198128091927,
12.6151268017188));
#72796=CARTESIAN_POINT('Ctrl Pts',(-0.404443900471156,2.15896276130563,
12.6349971452416));
#72797=CARTESIAN_POINT('Ctrl Pts',(-0.268509736560207,1.79185393524917,
12.6548674887644));
#72798=CARTESIAN_POINT('Ctrl Pts',(0.113745556344726,1.70742717330299,12.6747378322871));
#72799=CARTESIAN_POINT('Ctrl Pts',(0.391654786362965,1.98313253588689,12.6946081758099));
#72800=CARTESIAN_POINT('Ctrl Pts',(0.310274068876934,2.36604788672604,12.7144785193327));
#72801=CARTESIAN_POINT('Ctrl Pts',(-0.0557408668020039,2.50490052064318,
12.7343488628555));
#72802=CARTESIAN_POINT('Ctrl Pts',(-0.370621145626677,2.27231204909876,
12.7542192063783));
#72803=CARTESIAN_POINT('Ctrl Pts',(-0.345506978846376,1.88165073067313,
12.7740895499011));
#72804=CARTESIAN_POINT('Ctrl Pts',(-0.00343719551269503,1.69129514128672,
12.7939598934239));
#72805=CARTESIAN_POINT('Ctrl Pts',(0.341785746791939,1.87587061962627,12.8138302369467));
#72806=CARTESIAN_POINT('Ctrl Pts',(0.373466796304304,2.2660542920012,12.8337005804694));
#72807=CARTESIAN_POINT('Ctrl Pts',(0.062542903194813,2.50390575771099,12.8535709239923));
#72808=CARTESIAN_POINT('Ctrl Pts',(-0.305755589291243,2.37122867753338,
12.873441267515));
#72809=CARTESIAN_POINT('Ctrl Pts',(-0.393564953192428,1.98973621015215,
12.8933116110378));
#72810=CARTESIAN_POINT('Ctrl Pts',(-0.120332052099343,1.70939575892943,
12.9131819545606));
#72811=CARTESIAN_POINT('Ctrl Pts',(0.263289126085232,1.78738152286049,12.9330522980834));
#72812=CARTESIAN_POINT('Ctrl Pts',(0.405378372699886,2.15215218052539,12.9529226416062));
#72813=CARTESIAN_POINT('Ctrl Pts',(0.175588153428475,2.46908031220357,12.972792985129));
#72814=CARTESIAN_POINT('Ctrl Pts',(-0.215280299733418,2.44742750363098,
12.9926633286518));
#72815=CARTESIAN_POINT('Ctrl Pts',(-0.408658371617952,2.10705725759645,
13.0125336721746));
#72816=CARTESIAN_POINT('Ctrl Pts',(-0.227148048395885,1.76021294014051,
13.0324040156973));
#72817=CARTESIAN_POINT('Ctrl Pts',(0.162739737895554,1.72507698906855,13.0522743592201));
#72818=CARTESIAN_POINT('Ctrl Pts',(0.403335869369702,2.03388186554225,13.0721447027429));
#72819=CARTESIAN_POINT('Ctrl Pts',(0.273926443130965,2.403341117316,13.0920150462657));
#72820=CARTESIAN_POINT('Ctrl Pts',(-0.106773575112783,2.49452621302505,
13.1118853897885));
#72821=CARTESIAN_POINT('Ctrl Pts',(-0.389522657298515,2.22378717405302,
13.1317557333113));
#72822=CARTESIAN_POINT('Ctrl Pts',(-0.314939110772262,1.83949033997804,
13.1516260768341));
#72823=CARTESIAN_POINT('Ctrl Pts',(0.0485608540583714,1.694175490088,13.1714964203569));
#72824=CARTESIAN_POINT('Ctrl Pts',(0.367507724230662,1.92114969532342,13.1913667638797));
#72825=CARTESIAN_POINT('Ctrl Pts',(0.349326154660035,2.31219409952635,13.2112371074025));
#72826=CARTESIAN_POINT('Ctrl Pts',(0.010666392411916,2.50858047478247,13.2311074509252));
#72827=CARTESIAN_POINT('Ctrl Pts',(-0.337741731845634,2.3301476343883,13.250977794448));
#72828=CARTESIAN_POINT('Ctrl Pts',(-0.37638829909755,1.94059001290561,13.2708481379708));
#72829=CARTESIAN_POINT('Ctrl Pts',(-0.0696139978372859,1.69726097432062,
13.2907184814936));
#72830=CARTESIAN_POINT('Ctrl Pts',(0.300759554488769,1.82340645258339,13.3105888250164));
#72831=CARTESIAN_POINT('Ctrl Pts',(0.395736390676516,2.20325606000352,13.3304591685392));
#72832=CARTESIAN_POINT('Ctrl Pts',(0.126596892466422,2.48852249108309,13.3503339483527));
#72833=CARTESIAN_POINT('Ctrl Pts',(-0.128797381162466,2.44081661898851,
13.3635852803252));
#72834=CARTESIAN_POINT('Ctrl Pts',(-0.218126859843275,2.36814125324556,
13.3702131644569));
#72835=CARTESIAN_POINT('Ctrl Pts',(0.36283923412547,2.17047027618521,4.34302789673956));
#72836=CARTESIAN_POINT('Ctrl Pts',(0.339377508610394,2.29127063312973,4.34965134458049));
#72837=CARTESIAN_POINT('Ctrl Pts',(0.162686780011582,2.50549126291471,4.36289824026236));
#72838=CARTESIAN_POINT('Ctrl Pts',(-0.253693857002025,2.4562349422514,4.38276858378514));
#72839=CARTESIAN_POINT('Ctrl Pts',(-0.436454254879043,2.07954302848451,
4.40263892730793));
#72840=CARTESIAN_POINT('Ctrl Pts',(-0.219267421856341,1.72194013772262,
4.42250927083072));
#72841=CARTESIAN_POINT('Ctrl Pts',(0.199293560861417,1.71098919833492,4.44237961435351));
#72842=CARTESIAN_POINT('Ctrl Pts',(0.434912675694804,2.05698905545399,4.4622499578763));
#72843=CARTESIAN_POINT('Ctrl Pts',(0.271619417823269,2.44240078073541,4.48212030139909));
#72844=CARTESIAN_POINT('Ctrl Pts',(-0.140879241271172,2.51372967091627,
4.50199064492187));
#72845=CARTESIAN_POINT('Ctrl Pts',(-0.4241239888425,2.2055058322704,4.52186098844467));
#72846=CARTESIAN_POINT('Ctrl Pts',(-0.318301223523056,1.80050102752227,
4.54173133196746));
#72847=CARTESIAN_POINT('Ctrl Pts',(0.0795239985676654,1.67024250077846,
4.56160167549024));
#72848=CARTESIAN_POINT('Ctrl Pts',(0.404394484969609,1.93422966389774,4.58147201901304));
#72849=CARTESIAN_POINT('Ctrl Pts',(0.358289275345924,2.35028766510673,4.60134236253583));
#72850=CARTESIAN_POINT('Ctrl Pts',(-0.0164981858627633,2.53674126284983,
4.62121270605862));
#72851=CARTESIAN_POINT('Ctrl Pts',(-0.376150486643079,2.32254397230123,
4.6410830495814));
#72852=CARTESIAN_POINT('Ctrl Pts',(-0.390736090811099,1.90419300662078,
4.6609533931042));
#72853=CARTESIAN_POINT('Ctrl Pts',(-0.0468744390703233,1.66546823688044,
4.68082373662698));
#72854=CARTESIAN_POINT('Ctrl Pts',(0.339988084227034,1.82536723675285,4.70069408014978));
#72855=CARTESIAN_POINT('Ctrl Pts',(0.414957848761605,2.23720439184066,4.72056442367256));
#72856=CARTESIAN_POINT('Ctrl Pts',(0.109260266361431,2.52317520503028,4.74043476719535));
#72857=CARTESIAN_POINT('Ctrl Pts',(-0.29666872969806,2.42094037307327,4.76030511071814));
#72858=CARTESIAN_POINT('Ctrl Pts',(-0.43044455732329,2.02428644331352,4.78017545424093));
#72859=CARTESIAN_POINT('Ctrl Pts',(-0.169346101645197,1.6970893930947,4.80004579776372));
#72860=CARTESIAN_POINT('Ctrl Pts',(0.24710434702284,1.73950797403383,4.81991614128651));
#72861=CARTESIAN_POINT('Ctrl Pts',(0.436870197973242,2.1126289119025,4.8397864848093));
#72862=CARTESIAN_POINT('Ctrl Pts',(0.225867116553052,2.47416454254653,4.85965682833209));
#72863=CARTESIAN_POINT('Ctrl Pts',(-0.192338295150169,2.49245514321617,
4.87952717185488));
#72864=CARTESIAN_POINT('Ctrl Pts',(-0.434099505611459,2.15072157797534,
4.89939751537767));
#72865=CARTESIAN_POINT('Ctrl Pts',(-0.277633516952299,1.76245787003698,
4.91926785890046));
#72866=CARTESIAN_POINT('Ctrl Pts',(0.133523427103024,1.68384311414085,4.93913820242324));
#72867=CARTESIAN_POINT('Ctrl Pts',(0.422190804373444,1.98699564636976,4.95900854594604));
#72868=CARTESIAN_POINT('Ctrl Pts',(0.32355559471455,2.39381428890427,4.97887888946882));
#72869=CARTESIAN_POINT('Ctrl Pts',(-0.0718978249758275,2.53109832057086,
4.99874923299162));
#72870=CARTESIAN_POINT('Ctrl Pts',(-0.401394778257155,2.27290833185141,
5.0186195765144));
#72871=CARTESIAN_POINT('Ctrl Pts',(-0.362666667451549,1.8560984880016,5.0384899200372));
#72872=CARTESIAN_POINT('Ctrl Pts',(0.0087587381320539,1.66303507721802,
5.05836026355998));
#72873=CARTESIAN_POINT('Ctrl Pts',(0.372149193874197,1.87082749568422,5.07823060708277));
#72874=CARTESIAN_POINT('Ctrl Pts',(0.394143427774538,2.28885448784099,5.09810095060557));
#72875=CARTESIAN_POINT('Ctrl Pts',(0.0545647244742198,2.53363319762053,
5.11797129412835));
#72876=CARTESIAN_POINT('Ctrl Pts',(-0.335069685214756,2.38061248241239,
5.13784163765114));
#72877=CARTESIAN_POINT('Ctrl Pts',(-0.417323274337762,1.97016801653074,
5.15771198117393));
#72878=CARTESIAN_POINT('Ctrl Pts',(-0.116739572689465,1.67882672045364,
5.17758232469673));
#72879=CARTESIAN_POINT('Ctrl Pts',(0.290936794243693,1.77385457079585,5.19745266821951));
#72880=CARTESIAN_POINT('Ctrl Pts',(0.431718259926271,2.16807645174203,5.2173230117423));
#72881=CARTESIAN_POINT('Ctrl Pts',(0.176456995260411,2.49984745598693,5.23719335526509));
#72882=CARTESIAN_POINT('Ctrl Pts',(-0.240679540106183,2.46481285367957,
5.25706369878788));
#72883=CARTESIAN_POINT('Ctrl Pts',(-0.437025362986032,2.09511212290653,
5.27693404231066));
#72884=CARTESIAN_POINT('Ctrl Pts',(-0.232459910956952,1.72989535394238,
5.29680438583346));
#72885=CARTESIAN_POINT('Ctrl Pts',(0.185355862815914,1.70419921253827,5.31667472935624));
#72886=CARTESIAN_POINT('Ctrl Pts',(0.433132866377297,2.04159641021874,5.33654507287904));
#72887=CARTESIAN_POINT('Ctrl Pts',(0.283569430752704,2.43257095059271,5.35641541640182));
#72888=CARTESIAN_POINT('Ctrl Pts',(-0.126130353095458,2.51845691924446,
5.37628575992461));
#72889=CARTESIAN_POINT('Ctrl Pts',(-0.420122709075573,2.22046563225483,
5.39615610344741));
#72890=CARTESIAN_POINT('Ctrl Pts',(-0.328709674021062,1.81196352758631,
5.41602644697019));
#72891=CARTESIAN_POINT('Ctrl Pts',(0.0642497371665301,1.66769567373251,
5.43589679049298));
#72892=CARTESIAN_POINT('Ctrl Pts',(0.398268761315715,1.92000818630949,5.45576713401577));
#72893=CARTESIAN_POINT('Ctrl Pts',(0.36693041635361,2.33743868427474,5.47563747753856));
#72894=CARTESIAN_POINT('Ctrl Pts',(-0.0010166325474728,2.53705151377592,
5.49550782106136));
#72895=CARTESIAN_POINT('Ctrl Pts',(-0.368031059488272,2.33572907857855,
5.51537816458414));
#72896=CARTESIAN_POINT('Ctrl Pts',(-0.397427092253076,1.91815730540157,
5.53524850810693));
#72897=CARTESIAN_POINT('Ctrl Pts',(-0.0622378726886654,1.66740144887119,
5.55511885162973));
#72898=CARTESIAN_POINT('Ctrl Pts',(0.330046122146328,1.81349587002676,5.57498919515251));
#72899=CARTESIAN_POINT('Ctrl Pts',(0.419557731634292,2.22241882641751,5.5948595386753));
#72900=CARTESIAN_POINT('Ctrl Pts',(0.124182239975273,2.5190391753885,5.61472988219809));
#72901=CARTESIAN_POINT('Ctrl Pts',(-0.285113550975675,2.43124812797297,
5.63460022572088));
#72902=CARTESIAN_POINT('Ctrl Pts',(-0.432856473611466,2.03958201850278,
5.65447056924367));
#72903=CARTESIAN_POINT('Ctrl Pts',(-0.183512509796454,1.70334118189083,
5.67434091276646));
#72904=CARTESIAN_POINT('Ctrl Pts',(0.234179198784542,1.73098081067215,5.69421125628924));
#72905=CARTESIAN_POINT('Ctrl Pts',(0.437043373099837,2.09714530823555,5.71408159981204));
#72906=CARTESIAN_POINT('Ctrl Pts',(0.238979750678643,2.46592859686164,5.73395194333482));
#72907=CARTESIAN_POINT('Ctrl Pts',(-0.178315258834963,2.49902221454723,
5.75382228685762));
#72908=CARTESIAN_POINT('Ctrl Pts',(-0.432030293797926,2.16606727235501,
5.7736926303804));
#72909=CARTESIAN_POINT('Ctrl Pts',(-0.289416349814782,1.77250460202403,
5.7935629739032));
#72910=CARTESIAN_POINT('Ctrl Pts',(0.118697694645232,1.67937437486351,5.81343331742598));
#72911=CARTESIAN_POINT('Ctrl Pts',(0.417922763500204,1.97211089575767,5.83330366094877));
#72912=CARTESIAN_POINT('Ctrl Pts',(0.333760591890408,2.38216825926478,5.85317400447156));
#72913=CARTESIAN_POINT('Ctrl Pts',(-0.0565814853772176,2.53337465863622,
5.87304434799435));
#72914=CARTESIAN_POINT('Ctrl Pts',(-0.395017752684917,2.28701880734116,
5.89291469151714));
#72915=CARTESIAN_POINT('Ctrl Pts',(-0.371079008715224,1.86909866062216,
5.91278503503993));
#72916=CARTESIAN_POINT('Ctrl Pts',(-0.00672579209462177,1.66299905840347,
5.93265537856272));
#72917=CARTESIAN_POINT('Ctrl Pts',(0.363797423138882,1.85778832779351,5.95252572208551));
#72918=CARTESIAN_POINT('Ctrl Pts',(0.400586029189409,2.27477383229139,5.9723960656083));
#72919=CARTESIAN_POINT('Ctrl Pts',(0.069891488322067,2.53142813897064,5.99226640913109));
#72920=CARTESIAN_POINT('Ctrl Pts',(-0.324918978213823,2.39230586178187,
6.01213675265388));
#72921=CARTESIAN_POINT('Ctrl Pts',(-0.421660515963138,1.98503275025794,
6.03200709617666));
#72922=CARTESIAN_POINT('Ctrl Pts',(-0.131585934211991,1.68322643899462,
6.05187743969946));
#72923=CARTESIAN_POINT('Ctrl Pts',(0.279200828371318,1.76375313135685,6.07174778322224));
#72924=CARTESIAN_POINT('Ctrl Pts',(0.433858840684473,2.15274054982154,6.09161812674504));
#72925=CARTESIAN_POINT('Ctrl Pts',(0.190510431217294,2.49334569380248,6.11148847026782));
#72926=CARTESIAN_POINT('Ctrl Pts',(-0.227605363238513,2.4731097129004,6.13135881379061));
#72927=CARTESIAN_POINT('Ctrl Pts',(-0.436924222595204,2.11059636471292,
6.15122915731341));
#72928=CARTESIAN_POINT('Ctrl Pts',(-0.245424589582531,1.73836229446614,
6.17109950083618));
#72929=CARTESIAN_POINT('Ctrl Pts',(0.171218692831284,1.69788158651872,6.19096984435899));
#72930=CARTESIAN_POINT('Ctrl Pts',(0.430792133892607,2.02628977946169,6.21084018788177));
#72931=CARTESIAN_POINT('Ctrl Pts',(0.295172439160706,2.42231706500815,6.23071053140457));
#72932=CARTESIAN_POINT('Ctrl Pts',(-0.111227784402149,2.52266232291576,
6.25058087492735));
#72933=CARTESIAN_POINT('Ctrl Pts',(-0.415591658071537,2.23527243982757,
6.27045121845014));
#72934=CARTESIAN_POINT('Ctrl Pts',(-0.338706763155614,1.82378850887735,
6.29032156197293));
#72935=CARTESIAN_POINT('Ctrl Pts',(0.0488954761935535,1.66569101823315,
6.31019190549572));
#72936=CARTESIAN_POINT('Ctrl Pts',(0.391642772653139,1.90601289253119,6.33006224901851));
#72937=CARTESIAN_POINT('Ctrl Pts',(0.375111142552447,2.3242915289719,6.3499325925413));
#72938=CARTESIAN_POINT('Ctrl Pts',(0.0144661059306473,2.53681322211531,
6.36980293606408));
#72939=CARTESIAN_POINT('Ctrl Pts',(-0.359449613500031,2.34861825071831,
6.38967327958688));
#72940=CARTESIAN_POINT('Ctrl Pts',(-0.403619247190546,1.93234988060579,
6.40954362310967));
#72941=CARTESIAN_POINT('Ctrl Pts',(-0.0775231693824896,1.66987767153466,
6.42941396663246));
#72942=CARTESIAN_POINT('Ctrl Pts',(0.31968986250749,1.80198414296301,6.44928431015524));
#72943=CARTESIAN_POINT('Ctrl Pts',(0.423630967391639,2.20747959202741,6.46915465367804));
#72944=CARTESIAN_POINT('Ctrl Pts',(0.138948331842413,2.51437714743185,6.48902499720083));
#72945=CARTESIAN_POINT('Ctrl Pts',(-0.273200482064957,2.4411400824222,6.50889534072361));
#72946=CARTESIAN_POINT('Ctrl Pts',(-0.43472504656487,2.05495343381872,6.52876568424641));
#72947=CARTESIAN_POINT('Ctrl Pts',(-0.197448563312467,1.71009087715033,
6.54863602776919));
#72948=CARTESIAN_POINT('Ctrl Pts',(0.220960096584491,1.72291685936265,6.56850637129198));
#72949=CARTESIAN_POINT('Ctrl Pts',(0.436667948866037,2.08166528787568,6.58837671481477));
#72950=CARTESIAN_POINT('Ctrl Pts',(0.25179240503621,2.4572333187171,6.60824705833756));
#72951=CARTESIAN_POINT('Ctrl Pts',(-0.164068391973716,2.50508841256041,
6.62811740186035));
#72952=CARTESIAN_POINT('Ctrl Pts',(-0.429418775242406,2.1813300356871,6.64798774538314));
#72953=CARTESIAN_POINT('Ctrl Pts',(-0.300835892313531,1.78296242315543,
6.66785808890593));
#72954=CARTESIAN_POINT('Ctrl Pts',(0.103722966704488,1.67543362660996,6.68772843242871));
#72955=CARTESIAN_POINT('Ctrl Pts',(0.413130124377974,1.95738667815736,6.70759877595151));
#72956=CARTESIAN_POINT('Ctrl Pts',(0.343546635522439,2.37016803744478,6.72746911947429));
#72957=CARTESIAN_POINT('Ctrl Pts',(-0.0411941217737742,2.5351070024337,
6.74733946299709));
#72958=CARTESIAN_POINT('Ctrl Pts',(-0.388144880415828,2.30089452715924,
6.76720980651987));
#72959=CARTESIAN_POINT('Ctrl Pts',(-0.379025552430303,1.88238867253643,
6.78708015004267));
#72960=CARTESIAN_POINT('Ctrl Pts',(-0.0222018797595282,1.66351158575433,
6.80695049356545));
#72961=CARTESIAN_POINT('Ctrl Pts',(0.354988995077618,1.84505319651085,6.82682083708825));
#72962=CARTESIAN_POINT('Ctrl Pts',(0.406525794318799,2.26047379159546,6.84669118061103));
#72963=CARTESIAN_POINT('Ctrl Pts',(0.0851305207618968,2.52868152942523,
6.86656152413383));
#72964=CARTESIAN_POINT('Ctrl Pts',(-0.314360416120161,2.40363232372775,
6.88643186765661));
#72965=CARTESIAN_POINT('Ctrl Pts',(-0.425468467518153,2.00004179681833,
6.9063022111794));
#72966=CARTESIAN_POINT('Ctrl Pts',(-0.146267122269751,1.68814931324754,
6.92617255470219));
#72967=CARTESIAN_POINT('Ctrl Pts',(0.267114395190533,1.75407376636406,6.94604289822498));
#72968=CARTESIAN_POINT('Ctrl Pts',(0.435454819404735,2.13733844523737,6.96591324174778));
#72969=CARTESIAN_POINT('Ctrl Pts',(0.204324728635643,2.4863501837757,6.98578358527055));
#72970=CARTESIAN_POINT('Ctrl Pts',(-0.214245484356636,2.48093822552789,
7.00565392879336));
#72971=CARTESIAN_POINT('Ctrl Pts',(-0.43627463234065,2.12606730541472,7.02552427231613));
#72972=CARTESIAN_POINT('Ctrl Pts',(-0.258081198580122,1.74728318132671,
7.04539461583893));
#72973=CARTESIAN_POINT('Ctrl Pts',(0.156866600295109,1.6920687203126,7.06526495936172));
#72974=CARTESIAN_POINT('Ctrl Pts',(0.427910648858824,2.01107567358268,7.08513530288451));
#72975=CARTESIAN_POINT('Ctrl Pts',(0.306404931869047,2.41165859038679,7.1050056464073));
#72976=CARTESIAN_POINT('Ctrl Pts',(-0.0961855968457871,2.52633717899683,
7.12487598993008));
#72977=CARTESIAN_POINT('Ctrl Pts',(-0.410538934941196,2.24990944644317,
7.14474633345288));
#72978=CARTESIAN_POINT('Ctrl Pts',(-0.348278690057241,1.83596020510619,
7.16461667697566));
#72979=CARTESIAN_POINT('Ctrl Pts',(0.0334798390920258,1.66423152981207,
7.18448702049846));
#72980=CARTESIAN_POINT('Ctrl Pts',(0.384525173742875,1.89226110139513,7.20435736402124));
#72981=CARTESIAN_POINT('Ctrl Pts',(0.382821009860021,2.31086283135087,7.22422770754404));
#72982=CARTESIAN_POINT('Ctrl Pts',(0.0299306858050187,2.53602661992451,
7.24409805106682));
#72983=CARTESIAN_POINT('Ctrl Pts',(-0.350416967781163,2.36119534438158,
7.26396839458962));
#72984=CARTESIAN_POINT('Ctrl Pts',(-0.40930475839056,1.94675289890377,7.2838387381124));
#72985=CARTESIAN_POINT('Ctrl Pts',(-0.092711154987836,1.67289380597283,
7.30370908163519));
#72986=CARTESIAN_POINT('Ctrl Pts',(0.308932311632189,1.79084650080398,7.32357942515799));
#72987=CARTESIAN_POINT('Ctrl Pts',(0.427172439666159,2.19240544369902,7.34344976868076));
#72988=CARTESIAN_POINT('Ctrl Pts',(0.153540008582802,2.50919497186543,7.36332011220357));
#72989=CARTESIAN_POINT('Ctrl Pts',(-0.260944477790598,2.45060382021043,
7.38319045572634));
#72990=CARTESIAN_POINT('Ctrl Pts',(-0.436047930173949,2.07038139391246,
7.40306079924915));
#72991=CARTESIAN_POINT('Ctrl Pts',(-0.211136769187992,1.7173300064907,7.42293114277192));
#72992=CARTESIAN_POINT('Ctrl Pts',(0.207463633852353,1.71532624229832,7.44280148629472));
#72993=CARTESIAN_POINT('Ctrl Pts',(0.435744396456537,2.06620828219398,7.46267182981751));
#72994=CARTESIAN_POINT('Ctrl Pts',(0.264288996554756,2.44808962284968,7.48254217334029));
#72995=CARTESIAN_POINT('Ctrl Pts',(-0.149615577988074,2.51064612266384,
7.5024125168631));
#72996=CARTESIAN_POINT('Ctrl Pts',(-0.426268228048542,2.1964907093554,7.52228286038586));
#72997=CARTESIAN_POINT('Ctrl Pts',(-0.31187781005355,1.79381820623728,7.54215320390868));
#72998=CARTESIAN_POINT('Ctrl Pts',(0.0886180403356958,1.67202581600918,
7.56202354743145));
#72999=CARTESIAN_POINT('Ctrl Pts',(0.407818902973736,1.94284147616865,7.58189389095424));
#73000=CARTESIAN_POINT('Ctrl Pts',(0.352901441663641,2.35782868674233,7.60176423447703));
#73001=CARTESIAN_POINT('Ctrl Pts',(-0.025755049179834,2.53629317743611,
7.62163457799982));
#73002=CARTESIAN_POINT('Ctrl Pts',(-0.380784788634143,2.31451807378494,
7.64150492152262));
#73003=CARTESIAN_POINT('Ctrl Pts',(-0.386496323684559,1.89595184143474,
7.66137526504539));
#73004=CARTESIAN_POINT('Ctrl Pts',(-0.037650098477609,1.66457201591976,
7.68124560856821));
#73005=CARTESIAN_POINT('Ctrl Pts',(0.345734966484481,1.83263808763114,7.70111595209096));
#73006=CARTESIAN_POINT('Ctrl Pts',(0.411955267262573,2.24597231590331,7.72098629561378));
#73007=CARTESIAN_POINT('Ctrl Pts',(0.10026269297267,2.52539681667053,7.74085663913655));
#73008=CARTESIAN_POINT('Ctrl Pts',(-0.303407252586554,2.41457765068967,
7.76072698265935));
#73009=CARTESIAN_POINT('Ctrl Pts',(-0.428742349065226,2.01517631608103,
7.78059732618214));
#73010=CARTESIAN_POINT('Ctrl Pts',(-0.160764708276792,1.69358916376624,
7.80046766970493));
#73011=CARTESIAN_POINT('Ctrl Pts',(0.254692666216871,1.74482862585662,7.82033801322772));
#73012=CARTESIAN_POINT('Ctrl Pts',(0.436504192732088,2.12188947150714,7.8402083567505));
#73013=CARTESIAN_POINT('Ctrl Pts',(0.217882547095443,2.47886970703232,7.8600787002733));
#73014=CARTESIAN_POINT('Ctrl Pts',(-0.200616673470941,2.48828856480845,
7.87994904379608));
#73015=CARTESIAN_POINT('Ctrl Pts',(-0.435077407621625,2.14150552508765,
7.89981938731887));
#73016=CARTESIAN_POINT('Ctrl Pts',(-0.270413850720044,1.75664681656592,
7.91968973084166));
#73017=CARTESIAN_POINT('Ctrl Pts',(0.142317600695636,1.68676791052994,7.93956007436446));
#73018=CARTESIAN_POINT('Ctrl Pts',(0.424492028264872,1.99597319011368,7.95943041788724));
#73019=CARTESIAN_POINT('Ctrl Pts',(0.3172528092724,2.40060890579676,7.97930076141003));
#73020=CARTESIAN_POINT('Ctrl Pts',(-0.0810226721575523,2.52947687461842,
7.99917110493282));
#73021=CARTESIAN_POINT('Ctrl Pts',(-0.404970882123739,2.26435827897454,
8.01904144845561));
#73022=CARTESIAN_POINT('Ctrl Pts',(-0.357413439548636,1.84846333773073,
8.03891179197839));
#73023=CARTESIAN_POINT('Ctrl Pts',(0.0180221763662852,1.66331904049457,
8.05878213550118));
#73024=CARTESIAN_POINT('Ctrl Pts',(0.376924898962899,1.8787700748602,8.07865247902397));
#73025=CARTESIAN_POINT('Ctrl Pts',(0.390050340452458,2.29716944780689,8.09852282254676));
#73026=CARTESIAN_POINT('Ctrl Pts',(0.0453576951357961,2.53469269458724,
8.11839316606954));
#73027=CARTESIAN_POINT('Ctrl Pts',(-0.340944460575358,2.37344457215043,
8.13826350959235));
#73028=CARTESIAN_POINT('Ctrl Pts',(-0.414476489105645,1.9613482808826,8.15813385311513));
#73029=CARTESIAN_POINT('Ctrl Pts',(-0.10778276476028,1.67644606617789,8.17800419663793));
#73030=CARTESIAN_POINT('Ctrl Pts',(0.297786972954211,1.78009692409369,8.19787454016071));
#73031=CARTESIAN_POINT('Ctrl Pts',(0.430177703018842,2.17721530328235,8.21774488368351));
#73032=CARTESIAN_POINT('Ctrl Pts',(0.16793895396972,2.50349915362378,8.23761522720629));
#73033=CARTESIAN_POINT('Ctrl Pts',(-0.248360922522535,2.45962746196489,
8.25748557072909));
#73034=CARTESIAN_POINT('Ctrl Pts',(-0.436823463886832,2.0858465328112,8.27735591425187));
#73035=CARTESIAN_POINT('Ctrl Pts',(-0.224559945279632,1.72504948298268,
8.29722625777467));
#73036=CARTESIAN_POINT('Ctrl Pts',(0.193706752045623,1.70821848761396,8.31709660129744));
#73037=CARTESIAN_POINT('Ctrl Pts',(0.434273875162049,2.05079369362276,8.33696694482025));
#73038=CARTESIAN_POINT('Ctrl Pts',(0.276453838866806,2.43850898689895,8.35683728834301));
#73039=CARTESIAN_POINT('Ctrl Pts',(-0.134974958797051,2.5156883685326,8.37670763186583));
#73040=CARTESIAN_POINT('Ctrl Pts',(-0.422582606945993,2.21153026289883,
8.39657797538859));
#73041=CARTESIAN_POINT('Ctrl Pts',(-0.322528242649051,1.80505832452963,
8.4164483189114));
#73042=CARTESIAN_POINT('Ctrl Pts',(0.0734018760230442,1.66915522072114,
8.43631866243417));
#73043=CARTESIAN_POINT('Ctrl Pts',(0.401995766207075,1.92849354768073,8.45618900595698));
#73044=CARTESIAN_POINT('Ctrl Pts',(0.361813267677896,2.34516569614813,8.47605934947975));
#73045=CARTESIAN_POINT('Ctrl Pts',(-0.0102836475171846,2.53693169469529,
8.49592969300256));
#73046=CARTESIAN_POINT('Ctrl Pts',(-0.372946716107436,2.32787234623849,
8.51580003652532));
#73047=CARTESIAN_POINT('Ctrl Pts',(-0.393481944779828,1.90977114212655,
8.53567038004815));
#73048=CARTESIAN_POINT('Ctrl Pts',(-0.0530510568463816,1.66617901779301,
8.55554072357091));
#73049=CARTESIAN_POINT('Ctrl Pts',(0.336046953494394,1.82055858524068,8.57541106709373));
#73050=CARTESIAN_POINT('Ctrl Pts',(0.416867632665708,2.23128760821661,8.5952814106165));
#73051=CARTESIAN_POINT('Ctrl Pts',(0.115269010269813,2.52157812384773,8.6151517541393));
#73052=CARTESIAN_POINT('Ctrl Pts',(-0.292073236589911,2.4251281035276,8.63502209766208));
#73053=CARTESIAN_POINT('Ctrl Pts',(-0.43147805105905,2.03041731041534,8.65489244118488));
#73054=CARTESIAN_POINT('Ctrl Pts',(-0.175060494113946,1.69953916216922,
8.67476278470766));
#73055=CARTESIAN_POINT('Ctrl Pts',(0.241951233846475,1.73602931481269,8.69463312823044));
#73056=CARTESIAN_POINT('Ctrl Pts',(0.437005643438904,2.10641302098108,8.71450347175325));
#73057=CARTESIAN_POINT('Ctrl Pts',(0.231166868122316,2.47091365345329,8.73437381527603));
#73058=CARTESIAN_POINT('Ctrl Pts',(-0.186736038169164,2.49515150421634,
8.75424415879882));
#73059=CARTESIAN_POINT('Ctrl Pts',(-0.433334051256465,2.15689164488053,
8.77411450232161));
#73060=CARTESIAN_POINT('Ctrl Pts',(-0.282407065419999,1.76644144646492,
8.7939848458444));
#73061=CARTESIAN_POINT('Ctrl Pts',(0.127589956689025,1.68198581102115,8.81385518936719));
#73062=CARTESIAN_POINT('Ctrl Pts',(0.420540563339994,1.98100128647235,8.83372553288998));
#73063=CARTESIAN_POINT('Ctrl Pts',(0.32770245455445,2.3891818813732,8.85359587641274));
#73064=CARTESIAN_POINT('Ctrl Pts',(-0.0657580436241065,2.53207746867233,
8.87346621993558));
#73065=CARTESIAN_POINT('Ctrl Pts',(-0.398894488926811,2.27860080050036,
8.89333656345832));
#73066=CARTESIAN_POINT('Ctrl Pts',(-0.366099545220169,1.86128221217274,
8.91320690698115));
#73067=CARTESIAN_POINT('Ctrl Pts',(0.00254189127341255,1.6629546956844,
8.93307725050391));
#73068=CARTESIAN_POINT('Ctrl Pts',(0.368851488570885,1.86555674756011,8.95294759402671));
#73069=CARTESIAN_POINT('Ctrl Pts',(0.396790059700396,2.28322856698263,8.97281793754949));
#73070=CARTESIAN_POINT('Ctrl Pts',(0.0607277691436284,2.53281312051553,
8.9926882810723));
#73071=CARTESIAN_POINT('Ctrl Pts',(-0.331043982263186,2.38535055816115,
9.01255862459509));
#73072=CARTESIAN_POINT('Ctrl Pts',(-0.419127947512142,1.97611770566457,
9.03242896811786));
#73073=CARTESIAN_POINT('Ctrl Pts',(-0.122719080036365,1.68052999316926,
9.05229931164065));
#73074=CARTESIAN_POINT('Ctrl Pts',(0.286267836678638,1.76974890625633,9.07216965516346));
#73075=CARTESIAN_POINT('Ctrl Pts',(0.432642985087817,2.16192823822663,9.09203999868623));
#73076=CARTESIAN_POINT('Ctrl Pts',(0.182127093702806,2.49729684239233,9.11191034220904));
#73077=CARTESIAN_POINT('Ctrl Pts',(-0.235465611789637,2.46819968074414,
9.13178068573181));
#73078=CARTESIAN_POINT('Ctrl Pts',(-0.437050674213524,2.1013294378734,9.15165102925462));
#73079=CARTESIAN_POINT('Ctrl Pts',(-0.237701242123064,1.73323961674043,
9.17152137277738));
#73080=CARTESIAN_POINT('Ctrl Pts',(0.179706719513284,1.70160251733058,9.1913917163002));
#73081=CARTESIAN_POINT('Ctrl Pts',(0.432258230856898,2.03544087135022,9.21126205982296));
#73082=CARTESIAN_POINT('Ctrl Pts',(0.288271662033624,2.42850343697429,9.23113240334578));
#73083=CARTESIAN_POINT('Ctrl Pts',(-0.120164912062476,2.52020882087906,
9.25100274686855));
#73084=CARTESIAN_POINT('Ctrl Pts',(-0.418366538316829,2.22642981789257,
9.27087309039134));
#73085=CARTESIAN_POINT('Ctrl Pts',(-0.332773821126645,1.81666866885512,
9.29074343391414));
#73086=CARTESIAN_POINT('Ctrl Pts',(0.0580935738823234,1.66682544406541,
9.3106137774369));
#73087=CARTESIAN_POINT('Ctrl Pts',(0.395668023580192,1.91436090295496,9.33048412095972));
#73088=CARTESIAN_POINT('Ctrl Pts',(0.370270926980643,2.33219496090236,9.35035446448248));
#73089=CARTESIAN_POINT('Ctrl Pts',(0.00520066271126297,2.53702175271137,
9.3702248080053));
#73090=CARTESIAN_POINT('Ctrl Pts',(-0.364640501589402,2.34094058154696,
9.39009515152806));
#73091=CARTESIAN_POINT('Ctrl Pts',(-0.399973647003501,1.92382922791146,
9.40996549505088));
#73092=CARTESIAN_POINT('Ctrl Pts',(-0.068385422787009,1.66833057418229,
9.42983583857364));
#73093=CARTESIAN_POINT('Ctrl Pts',(0.32593711700193,1.80882985215509,9.44970618209645));
#73094=CARTESIAN_POINT('Ctrl Pts',(0.421256724273288,2.21643810153937,9.46957652561924));
#73095=CARTESIAN_POINT('Ctrl Pts',(0.130130635948347,2.51723024437741,9.48944686914203));
#73096=CARTESIAN_POINT('Ctrl Pts',(-0.280372595172832,2.43527043876788,
9.50931721266481));
#73097=CARTESIAN_POINT('Ctrl Pts',(-0.433672139505111,2.04574564853753,
9.52918755618761));
#73098=CARTESIAN_POINT('Ctrl Pts',(-0.189136534972047,1.70599183971101,
9.5490578997104));
#73099=CARTESIAN_POINT('Ctrl Pts',(0.228906091783717,1.72768687858221,9.56892824323319));
#73100=CARTESIAN_POINT('Ctrl Pts',(0.436958542078337,2.09092852049966,9.58879858675598));
#73101=CARTESIAN_POINT('Ctrl Pts',(0.244161016550001,2.46249200988825,9.60866893027878));
#73102=CARTESIAN_POINT('Ctrl Pts',(-0.172621002142068,2.50151842903535,
9.62853927380154));
#73103=CARTESIAN_POINT('Ctrl Pts',(-0.431046751596171,2.17220635134072,
9.64840961732437));
#73104=CARTESIAN_POINT('Ctrl Pts',(-0.294045788177107,1.77665477629806,
9.66827996084712));
#73105=CARTESIAN_POINT('Ctrl Pts',(0.112702155175145,1.67772842452465,9.68815030436993));
#73106=CARTESIAN_POINT('Ctrl Pts',(0.416061214167159,1.96617875616592,9.7080206478927));
#73107=CARTESIAN_POINT('Ctrl Pts',(0.337740750780422,2.37739186090769,9.72789099141552));
#73108=CARTESIAN_POINT('Ctrl Pts',(-0.0504108721960329,2.5341356967585,
9.74776133493826));
#73109=CARTESIAN_POINT('Ctrl Pts',(-0.392317382753171,2.2926191330716,9.7676316784611));
#73110=CARTESIAN_POINT('Ctrl Pts',(-0.374326103823116,1.87440073751858,
9.78750202198385));
#73111=CARTESIAN_POINT('Ctrl Pts',(-0.0129415845327464,1.663138952726,9.80737236550666));
#73112=CARTESIAN_POINT('Ctrl Pts',(0.360315076728777,1.85263770554612,9.82724270902943));
#73113=CARTESIAN_POINT('Ctrl Pts',(0.403031707559942,2.26905768819215,9.84711305255224));
#73114=CARTESIAN_POINT('Ctrl Pts',(0.0760216145173189,2.53039025704787,
9.86698339607502));
#73115=CARTESIAN_POINT('Ctrl Pts',(-0.320727960436671,2.39689835740483,
9.88685373959781));
#73116=CARTESIAN_POINT('Ctrl Pts',(-0.423253294859077,1.99104263390441,
9.9067240831206));
#73117=CARTESIAN_POINT('Ctrl Pts',(-0.137501351981262,1.68514046059072,
9.92659442664338));
#73118=CARTESIAN_POINT('Ctrl Pts',(0.27438936222061,1.75981543665868,9.94646477016618));
#73119=CARTESIAN_POINT('Ctrl Pts',(0.434565191323634,2.14656343764594,9.96633511368898));
#73120=CARTESIAN_POINT('Ctrl Pts',(0.196086618095845,2.49059582363268,9.98620545721174));
#73121=CARTESIAN_POINT('Ctrl Pts',(-0.222274732452348,2.47630971625616,
10.0060758007345));
#73122=CARTESIAN_POINT('Ctrl Pts',(-0.436729275947876,2.11681067415645,
10.0259461442573));
#73123=CARTESIAN_POINT('Ctrl Pts',(-0.250544164083381,1.74189012708484,
10.0458164877801));
#73124=CARTESIAN_POINT('Ctrl Pts',(0.165481109819656,1.69548663615597,10.0656868313029));
#73125=CARTESIAN_POINT('Ctrl Pts',(0.429699993681973,2.02016908703226,10.0855571748257));
#73126=CARTESIAN_POINT('Ctrl Pts',(0.299727631712863,2.41808553255901,10.1054275183485));
#73127=CARTESIAN_POINT('Ctrl Pts',(-0.105204028120338,2.52420180539787,
10.1252978618713));
#73128=CARTESIAN_POINT('Ctrl Pts',(-0.413625314388266,2.2411706716452,10.1451682053941));
#73129=CARTESIAN_POINT('Ctrl Pts',(-0.342601684706765,1.82863466530959,
10.1650385489168));
#73130=CARTESIAN_POINT('Ctrl Pts',(0.0427123496854742,1.66503941049802,
10.1849088924397));
#73131=CARTESIAN_POINT('Ctrl Pts',(0.388843618002635,1.90046128201732,10.2047792359624));
#73132=CARTESIAN_POINT('Ctrl Pts',(0.378263803080852,2.3189327625422,10.2246495794852));
#73133=CARTESIAN_POINT('Ctrl Pts',(0.0206784447991286,2.53656323843889,
10.244519923008));
#73134=CARTESIAN_POINT('Ctrl Pts',(-0.355876571469739,2.35370637578606,
10.2643902665308));
#73135=CARTESIAN_POINT('Ctrl Pts',(-0.405963281635488,1.93810845235375,
10.2842606100536));
#73136=CARTESIAN_POINT('Ctrl Pts',(-0.0836339478109073,1.67102398434281,
10.3041309535764));
#73137=CARTESIAN_POINT('Ctrl Pts',(0.315418147396308,1.79746661088628,10.3240012970991));
#73138=CARTESIAN_POINT('Ctrl Pts',(0.425117032670701,2.20144243573974,10.343871640622));
#73139=CARTESIAN_POINT('Ctrl Pts',(0.1448289149277,2.51235863594257,10.3637419841447));
#73140=CARTESIAN_POINT('Ctrl Pts',(-0.268320015585099,2.44499192522719,
10.3836123276675));
#73141=CARTESIAN_POINT('Ctrl Pts',(-0.435321860270199,2.06114208952546,
10.4034826711903));
#73142=CARTESIAN_POINT('Ctrl Pts',(-0.202975161877188,1.71293909665728,
10.4233530147131));
#73143=CARTESIAN_POINT('Ctrl Pts',(0.215573614965055,1.71981178902226,10.4432233582359));
#73144=CARTESIAN_POINT('Ctrl Pts',(0.436362947774456,2.07545540700811,10.4630937017587));
#73145=CARTESIAN_POINT('Ctrl Pts',(0.256848681451869,2.4536153476194,10.4829640452815));
#73146=CARTESIAN_POINT('Ctrl Pts',(-0.15828928331231,2.50738134717243,10.5028343888043));
#73147=CARTESIAN_POINT('Ctrl Pts',(-0.428218379777491,2.18743042065718,
10.5227047323271));
#73148=CARTESIAN_POINT('Ctrl Pts',(-0.305315409465088,1.78727398576594,
10.5425750758498));
#73149=CARTESIAN_POINT('Ctrl Pts',(0.0976728840918246,1.67400109513199,
10.5624454193726));
#73150=CARTESIAN_POINT('Ctrl Pts',(0.411059603456944,1.95152420520041,10.5823157628954));
#73151=CARTESIAN_POINT('Ctrl Pts',(0.347355097362123,2.36525364384322,10.6021861064182));
#73152=CARTESIAN_POINT('Ctrl Pts',(-0.0350004224360313,2.53564897528268,
10.622056449941));
#73153=CARTESIAN_POINT('Ctrl Pts',(-0.385247819526378,2.30639568015277,
10.6419267934638));
#73154=CARTESIAN_POINT('Ctrl Pts',(-0.382082788955989,1.8878024467173,10.6617971369866));
#73155=CARTESIAN_POINT('Ctrl Pts',(-0.0284088153932009,1.66387158033039,
10.6816674805094));
#73156=CARTESIAN_POINT('Ctrl Pts',(0.351326378781868,1.84002916546741,10.7015378240322));
#73157=CARTESIAN_POINT('Ctrl Pts',(0.408767449192139,2.25467459945481,10.7214081675549));
#73158=CARTESIAN_POINT('Ctrl Pts',(0.0912200336317959,2.52742714548771,
10.7412785110778));
#73159=CARTESIAN_POINT('Ctrl Pts',(-0.310009344299521,2.40807347448707,
10.7611488546005));
#73160=CARTESIAN_POINT('Ctrl Pts',(-0.426847352797267,2.00610433106091,
10.7810191981233));
#73161=CARTESIAN_POINT('Ctrl Pts',(-0.152111025123309,1.69027168114532,
10.8008895416461));
#73162=CARTESIAN_POINT('Ctrl Pts',(0.262166460055135,1.75030898430513,10.8207598851689));
#73163=CARTESIAN_POINT('Ctrl Pts',(0.435941908873682,2.131140188232,10.8406302286917));
#73164=CARTESIAN_POINT('Ctrl Pts',(0.209800004432418,2.48340450880984,10.8605005722145));
#73165=CARTESIAN_POINT('Ctrl Pts',(-0.208804842384087,2.48394738836527,
10.8803709157373));
#73166=CARTESIAN_POINT('Ctrl Pts',(-0.435859672525612,2.13227080881258,
10.9002412592601));
#73167=CARTESIAN_POINT('Ctrl Pts',(-0.263072590061224,1.75099015544825,
10.9201116027828));
#73168=CARTESIAN_POINT('Ctrl Pts',(0.151047779685193,1.68987852106024,10.9399819463056));
#73169=CARTESIAN_POINT('Ctrl Pts',(0.426602374868791,2.00499751060179,10.9598522898284));
#73170=CARTESIAN_POINT('Ctrl Pts',(0.310807367779338,2.40726835074513,10.9797226333512));
#73171=CARTESIAN_POINT('Ctrl Pts',(-0.0901110866453405,2.52766230988848,
10.999592976874));
#73172=CARTESIAN_POINT('Ctrl Pts',(-0.408364886589611,2.25573432067532,
11.0194633203968));
#73173=CARTESIAN_POINT('Ctrl Pts',(-0.351999496947143,1.84094129355586,
11.0393336639196));
#73174=CARTESIAN_POINT('Ctrl Pts',(0.0272775107400031,1.66379936194065,
11.0592040074423));
#73175=CARTESIAN_POINT('Ctrl Pts',(0.381531115820961,1.8868121323903,11.0790743509652));
#73176=CARTESIAN_POINT('Ctrl Pts',(0.385781862907382,2.30539574846443,11.0989446944879));
#73177=CARTESIAN_POINT('Ctrl Pts',(0.0361302702344473,2.53555672742862,
11.1188150380107));
#73178=CARTESIAN_POINT('Ctrl Pts',(-0.346665926686456,2.36615370467115,
11.1386853815335));
#73179=CARTESIAN_POINT('Ctrl Pts',(-0.411443330176841,1.9525908914329,11.1585557250563));
#73180=CARTESIAN_POINT('Ctrl Pts',(-0.0987774911814487,1.67425586736697,
11.1784260685791));
#73181=CARTESIAN_POINT('Ctrl Pts',(0.304503248631784,1.7864831251619,11.1982964121019));
#73182=CARTESIAN_POINT('Ctrl Pts',(0.428443712199356,2.18631943415239,11.2181667556247));
#73183=CARTESIAN_POINT('Ctrl Pts',(0.159345397168516,2.50696941363788,11.2380370991475));
#73184=CARTESIAN_POINT('Ctrl Pts',(-0.255930626847466,2.45428035999335,
11.2579074426703));
#73185=CARTESIAN_POINT('Ctrl Pts',(-0.436425142539554,2.07658730697071,
11.2777777861931));
#73186=CARTESIAN_POINT('Ctrl Pts',(-0.216559003869717,1.7203722124521,11.2976481297158));
#73187=CARTESIAN_POINT('Ctrl Pts',(0.2019705390044,1.71241393135224,11.3175184732386));
#73188=CARTESIAN_POINT('Ctrl Pts',(0.435219608148008,2.0600131031581,11.3373888167614));
#73189=CARTESIAN_POINT('Ctrl Pts',(0.26921393661526,2.44429480909196,11.3572591602842));
#73190=CARTESIAN_POINT('Ctrl Pts',(-0.143758871594009,2.51273289918974,
11.377129503807));
#73191=CARTESIAN_POINT('Ctrl Pts',(-0.424852486118888,2.20254474279138,
11.3969998473298));
#73192=CARTESIAN_POINT('Ctrl Pts',(-0.316201783072909,1.79828574508806,
11.4168701908526));
#73193=CARTESIAN_POINT('Ctrl Pts',(0.0825210089568178,1.67080850157966,
11.4367405343754));
#73194=CARTESIAN_POINT('Ctrl Pts',(0.405542009489586,1.93705602872551,11.4566108778982));
#73195=CARTESIAN_POINT('Ctrl Pts',(0.356533425874872,2.35278246669712,11.476481221421));
#73196=CARTESIAN_POINT('Ctrl Pts',(-0.0195460383370229,2.53661540469947,
11.4963515649437));
#73197=CARTESIAN_POINT('Ctrl Pts',(-0.37769467332754,2.31991314871002,11.5162219084665));
#73198=CARTESIAN_POINT('Ctrl Pts',(-0.389359864026752,1.90147051725091,
11.5360922519893));
#73199=CARTESIAN_POINT('Ctrl Pts',(-0.0438403860404519,1.66515165886556,
11.5559625955121));
#73200=CARTESIAN_POINT('Ctrl Pts',(0.341896677808339,1.82774695421506,11.5758329390349));
#73201=CARTESIAN_POINT('Ctrl Pts',(0.41399008479768,2.24009735516691,11.5957032825577));
#73202=CARTESIAN_POINT('Ctrl Pts',(0.106303948645956,2.52392750528579,11.6155736260805));
#73203=CARTESIAN_POINT('Ctrl Pts',(-0.298901588412632,2.4188618818234,11.6354439696033));
#73204=CARTESIAN_POINT('Ctrl Pts',(-0.429905609879455,2.02128389091344,
11.6553143131261));
#73205=CARTESIAN_POINT('Ctrl Pts',(-0.166529760645773,1.69591721385982,
11.6751846566488));
#73206=CARTESIAN_POINT('Ctrl Pts',(0.249614473000665,1.74124148218593,11.6950550001716));
#73207=CARTESIAN_POINT('Ctrl Pts',(0.43677140961095,2.11567785004451,11.7149253436944));
#73208=CARTESIAN_POINT('Ctrl Pts',(0.223250038961308,2.47573192483382,11.7347956872172));
#73209=CARTESIAN_POINT('Ctrl Pts',(-0.195072849686974,2.49110310987073,
11.75466603074));
#73210=CARTESIAN_POINT('Ctrl Pts',(-0.43444295551788,2.14769043548176,11.7745363742628));
#73211=CARTESIAN_POINT('Ctrl Pts',(-0.275270793728863,1.76052827900481,
11.7944067177856));
#73212=CARTESIAN_POINT('Ctrl Pts',(0.136424846571767,1.68478521163929,11.8142770613084));
#73213=CARTESIAN_POINT('Ctrl Pts',(0.422969262708565,1.98994518620559,11.8341474048312));
#73214=CARTESIAN_POINT('Ctrl Pts',(0.321496962375759,2.39606546981827,11.8540177483539));
#73215=CARTESIAN_POINT('Ctrl Pts',(-0.0749050330775907,2.53058599054684,
11.8738880918767));
#73216=CARTESIAN_POINT('Ctrl Pts',(-0.402591858081682,2.27010248393803,
11.8937584353995));
#73217=CARTESIAN_POINT('Ctrl Pts',(-0.360955461228196,1.85357310567818,
11.9136287789223));
#73218=CARTESIAN_POINT('Ctrl Pts',(0.0118084316533941,1.66310685496629,
11.9334991224451));
#73219=CARTESIAN_POINT('Ctrl Pts',(0.373739696065804,1.87343058719194,11.9533694659679));
#73220=CARTESIAN_POINT('Ctrl Pts',(0.392815669403017,2.29160091102866,11.9732398094907));
#73221=CARTESIAN_POINT('Ctrl Pts',(0.0515367430874135,2.53400348310525,
11.9931101530135));
#73222=CARTESIAN_POINT('Ctrl Pts',(-0.337020128916868,2.37826694367174,
12.0129804965363));
#73223=CARTESIAN_POINT('Ctrl Pts',(-0.416406913787441,1.967258366043,12.032850840059));
#73224=CARTESIAN_POINT('Ctrl Pts',(-0.1137970439404,1.67802216642817,12.0527211835818));
#73225=CARTESIAN_POINT('Ctrl Pts',(0.293206121653347,1.77589318202087,12.0725915271046));
#73226=CARTESIAN_POINT('Ctrl Pts',(0.431232587039189,2.17108807995046,12.0924618706274));
#73227=CARTESIAN_POINT('Ctrl Pts',(0.173661860832098,2.50106934229368,12.1123322141502));
#73228=CARTESIAN_POINT('Ctrl Pts',(-0.24321998076094,2.46312408374301,12.132202557673));
#73229=CARTESIAN_POINT('Ctrl Pts',(-0.436980601416259,2.09206191323819,
12.1520729011958));
#73230=CARTESIAN_POINT('Ctrl Pts',(-0.22987100980918,1.72828185666441,12.1719432447186));
#73231=CARTESIAN_POINT('Ctrl Pts',(0.18811393918567,1.70550259174539,12.1918135882414));
#73232=CARTESIAN_POINT('Ctrl Pts',(0.433529958377981,2.04462099292745,12.2116839317642));
#73233=CARTESIAN_POINT('Ctrl Pts',(0.281241260532876,2.43454209392756,12.2315542752869));
#73234=CARTESIAN_POINT('Ctrl Pts',(-0.12904800631086,2.51756636754263,12.2514246188097));
#73235=CARTESIAN_POINT('Ctrl Pts',(-0.420953295664032,2.21753034546508,
12.2712949623325));
#73236=CARTESIAN_POINT('Ctrl Pts',(-0.326691243861827,1.80967623173504,
12.2911653058553));
#73237=CARTESIAN_POINT('Ctrl Pts',(0.0672655491868179,1.66815465137604,
12.3110356493781));
#73238=CARTESIAN_POINT('Ctrl Pts',(0.399515358234169,1.92279238794404,12.3309059929009));
#73239=CARTESIAN_POINT('Ctrl Pts',(0.365264215206402,2.33999398393544,12.3507763364237));
#73240=CARTESIAN_POINT('Ctrl Pts',(-0.00406711904058771,2.53703377189671,
12.3706466799465));
#73241=CARTESIAN_POINT('Ctrl Pts',(-0.369667425256092,2.33315457091827,
12.3905170234693));
#73242=CARTESIAN_POINT('Ctrl Pts',(-0.396148194474713,1.91538779225095,
12.410387366992));
#73243=CARTESIAN_POINT('Ctrl Pts',(-0.0592169259695541,1.66697758151076,
12.4302577105148));
#73244=CARTESIAN_POINT('Ctrl Pts',(0.332037810456167,1.81580648905538,12.4501280540376));
#73245=CARTESIAN_POINT('Ctrl Pts',(0.418693058654454,2.22534425343881,12.4699983975604));
#73246=CARTESIAN_POINT('Ctrl Pts',(0.121254425450163,2.51989572937136,12.4898687410832));
#73247=CARTESIAN_POINT('Ctrl Pts',(-0.287418635805224,2.4292500372474,12.509739084606));
#73248=CARTESIAN_POINT('Ctrl Pts',(-0.432424227223307,2.03656225929401,
12.5296094281288));
#73249=CARTESIAN_POINT('Ctrl Pts',(-0.180739459406689,1.70206997216982,
12.5494797716516));
#73250=CARTESIAN_POINT('Ctrl Pts',(0.236749156960017,1.73262431229833,12.5693501151744));
#73251=CARTESIAN_POINT('Ctrl Pts',(0.437052652303248,2.10019583220945,12.5892204586972));
#73252=CARTESIAN_POINT('Ctrl Pts',(0.236419838504093,2.46758770272854,12.6090908022199));
#73253=CARTESIAN_POINT('Ctrl Pts',(-0.181095991467864,2.49776789854112,
12.6289611457427));
#73254=CARTESIAN_POINT('Ctrl Pts',(-0.432480903261117,2.16305019865179,
12.6488314892655));
#73255=CARTESIAN_POINT('Ctrl Pts',(-0.287123463270608,1.7704925250089,12.6687018327883));
#73256=CARTESIAN_POINT('Ctrl Pts',(0.121630665940594,1.68021310127832,12.6885721763111));
#73257=CARTESIAN_POINT('Ctrl Pts',(0.418805217671658,1.97503100829909,12.7084425198339));
#73258=CARTESIAN_POINT('Ctrl Pts',(0.331782997370132,2.38449095221355,12.7283128633567));
#73259=CARTESIAN_POINT('Ctrl Pts',(-0.0596049548405058,2.53296917741782,
12.7481832068795));
#73260=CARTESIAN_POINT('Ctrl Pts',(-0.396313475469834,2.28425712577239,
12.7680535504023));
#73261=CARTESIAN_POINT('Ctrl Pts',(-0.369458335557585,1.86651424557301,
12.7879238939251));
#73262=CARTESIAN_POINT('Ctrl Pts',(-0.00367546999292127,1.66296275884588,
12.8077942374478));
#73263=CARTESIAN_POINT('Ctrl Pts',(0.365479138941547,1.86033344362852,12.8276645809706));
#73264=CARTESIAN_POINT('Ctrl Pts',(0.39935639334789,2.27756556622912,12.8475349244934));
#73265=CARTESIAN_POINT('Ctrl Pts',(0.0668785244003959,2.53190545517864,
12.8674052680162));
#73266=CARTESIAN_POINT('Ctrl Pts',(-0.326951286148151,2.39003088762939,
12.887275611539));
#73267=CARTESIAN_POINT('Ctrl Pts',(-0.420847801760121,1.98209246480204,
12.9071459550618));
#73268=CARTESIAN_POINT('Ctrl Pts',(-0.12867375307811,1.68231815389222,12.9270162985846));
#73269=CARTESIAN_POINT('Ctrl Pts',(0.281540947794072,1.76571007447041,12.9468866421074));
#73270=CARTESIAN_POINT('Ctrl Pts',(0.433480155303436,2.15576749238745,12.9667569856302));
#73271=CARTESIAN_POINT('Ctrl Pts',(0.187760337362539,2.49466582784844,12.9866273291529));
#73272=CARTESIAN_POINT('Ctrl Pts',(-0.230204036640388,2.47151199563903,
13.0064976726757));
#73273=CARTESIAN_POINT('Ctrl Pts',(-0.436987531463964,2.1075464832979,13.0263680161985));
#73274=CARTESIAN_POINT('Ctrl Pts',(-0.242894485563508,1.73665810167174,
13.0462383597213));
#73275=CARTESIAN_POINT('Ctrl Pts',(0.174021239434115,1.69908644380071,13.0661087032441));
#73276=CARTESIAN_POINT('Ctrl Pts',(0.431296060836643,2.02929840089342,13.0859790467669));
#73277=CARTESIAN_POINT('Ctrl Pts',(0.29291566868573,2.42436943729461,13.1058493902897));
#73278=CARTESIAN_POINT('Ctrl Pts',(-0.114175370565393,2.52187569838607,
13.1257197338125));
#73279=CARTESIAN_POINT('Ctrl Pts',(-0.41652528440381,2.23236839221512,13.1455900773353));
#73280=CARTESIAN_POINT('Ctrl Pts',(-0.336771430945945,1.82143119739647,
13.165460420858));
#73281=CARTESIAN_POINT('Ctrl Pts',(0.0519272067197533,1.66604278020319,
13.1853307643808));
#73282=CARTESIAN_POINT('Ctrl Pts',(0.39298422437713,1.90875137138937,13.2052011079036));
#73283=CARTESIAN_POINT('Ctrl Pts',(0.373542265624722,2.32690389377349,13.2250714514264));
#73284=CARTESIAN_POINT('Ctrl Pts',(0.0114058118306527,2.53690423463656,
13.2449417949492));
#73285=CARTESIAN_POINT('Ctrl Pts',(-0.36115478336407,2.34610200991459,13.264812138472));
#73286=CARTESIAN_POINT('Ctrl Pts',(-0.402480421588718,1.92953933752709,
13.2846824819948));
#73287=CARTESIAN_POINT('Ctrl Pts',(-0.0744398039609454,1.66934215746259,
13.3045528255176));
#73288=CARTESIAN_POINT('Ctrl Pts',(0.321608914458083,1.80423233708416,13.3244231690404));
#73289=CARTESIAN_POINT('Ctrl Pts',(0.423169768399744,2.21041401303246,13.3442935125631));
#73290=CARTESIAN_POINT('Ctrl Pts',(0.135372886919875,2.51545578431306,13.3641682923767));
#73291=CARTESIAN_POINT('Ctrl Pts',(-0.137725918669883,2.46444282891852,
13.3774196243492));
#73292=CARTESIAN_POINT('Ctrl Pts',(-0.233247926994675,2.38672943582559,
13.3840475084809));
#73293=CARTESIAN_POINT('Ctrl Pts',(0.386361485727264,2.1750387445618,4.3568622407636));
#73294=CARTESIAN_POINT('Ctrl Pts',(0.361378776375058,2.30367038357945,4.36348568860453));
#73295=CARTESIAN_POINT('Ctrl Pts',(0.173233487786809,2.53177857313794,4.37673258428639));
#73296=CARTESIAN_POINT('Ctrl Pts',(-0.270140399087323,2.47932904882227,
4.39660292780918));
#73297=CARTESIAN_POINT('Ctrl Pts',(-0.464748843309329,2.07821683774835,
4.41647327133197));
#73298=CARTESIAN_POINT('Ctrl Pts',(-0.233482156592523,1.69743115863587,
4.43634361485476));
#73299=CARTESIAN_POINT('Ctrl Pts',(0.212213424096465,1.68577028843772,4.45621395837754));
#73300=CARTESIAN_POINT('Ctrl Pts',(0.463107326163524,2.05420072893338,4.47608430190034));
#73301=CARTESIAN_POINT('Ctrl Pts',(0.289228043586586,2.46459804209974,4.49595464542312));
#73302=CARTESIAN_POINT('Ctrl Pts',(-0.150012203329834,2.54055106314491,
4.51582498894591));
#73303=CARTESIAN_POINT('Ctrl Pts',(-0.451619227057188,2.21234559627247,
4.5356953324687));
#73304=CARTESIAN_POINT('Ctrl Pts',(-0.338936151504061,1.78108501755827,
4.55556567599149));
#73305=CARTESIAN_POINT('Ctrl Pts',(0.0846794043969424,1.64238205164921,
4.57543601951428));
#73306=CARTESIAN_POINT('Ctrl Pts',(0.43061069294052,1.92348305441572,4.59530636303707));
#73307=CARTESIAN_POINT('Ctrl Pts',(0.38151656084392,2.36651338955372,4.61517670655986));
#73308=CARTESIAN_POINT('Ctrl Pts',(-0.0175677352453814,2.56505445751964,
4.63504705008264));
#73309=CARTESIAN_POINT('Ctrl Pts',(-0.400535684148771,2.33697112024056,
4.65491739360544));
#73310=CARTESIAN_POINT('Ctrl Pts',(-0.416066848274827,1.89149917163689,
4.67478773712822));
#73311=CARTESIAN_POINT('Ctrl Pts',(-0.0499132293823783,1.63729828032735,
4.69465808065102));
#73312=CARTESIAN_POINT('Ctrl Pts',(0.362028934572462,1.80756326092109,4.71452842417379));
#73313=CARTESIAN_POINT('Ctrl Pts',(0.441858861675035,2.24609911964907,4.73439876769659));
#73314=CARTESIAN_POINT('Ctrl Pts',(0.116343423952193,2.55060893520105,4.75426911121937));
#73315=CARTESIAN_POINT('Ctrl Pts',(-0.315901259827201,2.44174639263947,
4.77413945474218));
#73316=CARTESIAN_POINT('Ctrl Pts',(-0.458349547262939,2.0193780619629,4.79400979826496));
#73317=CARTESIAN_POINT('Ctrl Pts',(-0.180324521937238,1.67096938241971,
4.81388014178775));
#73318=CARTESIAN_POINT('Ctrl Pts',(0.263123702362371,1.71613788795246,4.83375048531054));
#73319=CARTESIAN_POINT('Ctrl Pts',(0.46519175128823,2.11344762282265,4.85362082883332));
#73320=CARTESIAN_POINT('Ctrl Pts',(0.240509698292949,2.49842099466773,4.87349117235613));
#73321=CARTESIAN_POINT('Ctrl Pts',(-0.204807260316238,2.5178973439291,4.89336151587891));
#73322=CARTESIAN_POINT('Ctrl Pts',(-0.462241439644094,2.1540097717718,4.9132318594017));
#73323=CARTESIAN_POINT('Ctrl Pts',(-0.295632026552772,1.7405755867543,4.93310220292448));
#73324=CARTESIAN_POINT('Ctrl Pts',(0.142179524216207,1.65686436968784,4.95297254644727));
#73325=CARTESIAN_POINT('Ctrl Pts',(0.449560717520727,1.97966976595722,4.97284288997007));
#73326=CARTESIAN_POINT('Ctrl Pts',(0.344531154660214,2.41286177048237,4.99271323349286));
#73327=CARTESIAN_POINT('Ctrl Pts',(-0.0765588389171428,2.55904569287204,
5.01258357701564));
#73328=CARTESIAN_POINT('Ctrl Pts',(-0.427416520334123,2.28411768548057,
5.03245392053844));
#73329=CARTESIAN_POINT('Ctrl Pts',(-0.386177731848805,1.84028676701965,
5.05232426406122));
#73330=CARTESIAN_POINT('Ctrl Pts',(0.00932655225657797,1.6347073830545,
5.07219460758402));
#73331=CARTESIAN_POINT('Ctrl Pts',(0.396274994362174,1.85597063126681,5.09206495110681));
#73332=CARTESIAN_POINT('Ctrl Pts',(0.419695077109399,2.30109760369322,5.11193529462959));
#73333=CARTESIAN_POINT('Ctrl Pts',(0.0581020629341788,2.5617449016977,5.13180563815239));
#73334=CARTESIAN_POINT('Ctrl Pts',(-0.356791684101566,2.39880411328662,
5.15167598167517));
#73335=CARTESIAN_POINT('Ctrl Pts',(-0.444377633775809,1.96175122944184,
5.17154632519797));
#73336=CARTESIAN_POINT('Ctrl Pts',(-0.124307601012795,1.65152277171357,
5.19141666872075));
#73337=CARTESIAN_POINT('Ctrl Pts',(0.309797732727714,1.75271111627667,5.21128701224355));
#73338=CARTESIAN_POINT('Ctrl Pts',(0.459705821843468,2.17248973254367,5.23115735576633));
#73339=CARTESIAN_POINT('Ctrl Pts',(0.187896402714256,2.52576888778782,5.25102769928912));
#73340=CARTESIAN_POINT('Ctrl Pts',(-0.256282386119894,2.48846305168667,
5.2708980428119));
#73341=CARTESIAN_POINT('Ctrl Pts',(-0.465356975385395,2.09479525013207,
5.2907683863347));
#73342=CARTESIAN_POINT('Ctrl Pts',(-0.247529892366297,1.70590209801857,
5.31063872985749));
#73343=CARTESIAN_POINT('Ctrl Pts',(0.197372168746952,1.67854011938838,5.33050907338028));
#73344=CARTESIAN_POINT('Ctrl Pts',(0.461212134829325,2.03781020463768,5.35037941690307));
#73345=CARTESIAN_POINT('Ctrl Pts',(0.301952755568203,2.45413096075576,5.37024976042586));
#73346=CARTESIAN_POINT('Ctrl Pts',(-0.134307169771021,2.54558477095736,
5.39012010394865));
#73347=CARTESIAN_POINT('Ctrl Pts',(-0.447358551115442,2.22827521469451,
5.40999044747144));
#73348=CARTESIAN_POINT('Ctrl Pts',(-0.350019364178736,1.79329061204303,
5.42986079099422));
#73349=CARTESIAN_POINT('Ctrl Pts',(0.0684149385583651,1.6396701181293,5.44973113451702));
#73350=CARTESIAN_POINT('Ctrl Pts',(0.424087849021016,1.90833962257744,5.46960147803981));
#73351=CARTESIAN_POINT('Ctrl Pts',(0.390717892354156,2.35283143110649,5.4894718215626));
#73352=CARTESIAN_POINT('Ctrl Pts',(-0.00108253910974737,2.5653848214866,
5.50934216508539));
#73353=CARTESIAN_POINT('Ctrl Pts',(-0.391889888314849,2.35101099457515,
5.52921250860817));
#73354=CARTESIAN_POINT('Ctrl Pts',(-0.423191615981816,1.9063687522022,5.54908285213097));
#73355=CARTESIAN_POINT('Ctrl Pts',(-0.0662726483216284,1.63935681916968,
5.56895319565376));
#73356=CARTESIAN_POINT('Ctrl Pts',(0.351442451967285,1.79492229364266,5.58882353917654));
#73357=CARTESIAN_POINT('Ctrl Pts',(0.446756947145716,2.23035503111914,5.60869388269934));
#73358=CARTESIAN_POINT('Ctrl Pts',(0.132232763784262,2.54620477377881,5.62856422622211));
#73359=CARTESIAN_POINT('Ctrl Pts',(-0.303596978484018,2.45272238179113,
5.64843456974492));
#73360=CARTESIAN_POINT('Ctrl Pts',(-0.460917823989673,2.03566522332629,
5.6683049132677));
#73361=CARTESIAN_POINT('Ctrl Pts',(-0.195409314280412,1.67762646407061,
5.68817525679049));
#73362=CARTESIAN_POINT('Ctrl Pts',(0.249360638705182,1.70705792306553,5.70804560031327));
#73363=CARTESIAN_POINT('Ctrl Pts',(0.465376153064306,2.09696024341454,5.72791594383607));
#73364=CARTESIAN_POINT('Ctrl Pts',(0.254472402229233,2.48965112660522,5.74778628735886));
#73365=CARTESIAN_POINT('Ctrl Pts',(-0.189875134361864,2.52489014734646,
5.76765663088165));
#73366=CARTESIAN_POINT('Ctrl Pts',(-0.460038084341331,2.17035030146765,
5.78752697440444));
#73367=CARTESIAN_POINT('Ctrl Pts',(-0.308178720467497,1.75127363132099,
5.80739731792722));
#73368=CARTESIAN_POINT('Ctrl Pts',(0.126392664690959,1.65210592962917,5.82726766145002));
#73369=CARTESIAN_POINT('Ctrl Pts',(0.445015986802993,1.96382006223093,5.8471380049728));
#73370=CARTESIAN_POINT('Ctrl Pts',(0.355397724479243,2.40046074851136,5.86700834849559));
#73371=CARTESIAN_POINT('Ctrl Pts',(-0.060249567022979,2.56146960206993,
5.88687869201838));
#73372=CARTESIAN_POINT('Ctrl Pts',(-0.420626083019512,2.29914291914275,
5.90674903554117));
#73373=CARTESIAN_POINT('Ctrl Pts',(-0.39513543091603,1.85412971876244,5.92661937906395));
#73374=CARTESIAN_POINT('Ctrl Pts',(-0.00716181377855303,1.63466902920133,
5.94648972258676));
#73375=CARTESIAN_POINT('Ctrl Pts',(0.387381792507841,1.8420861562567,5.96636006610954));
#73376=CARTESIAN_POINT('Ctrl Pts',(0.426555341437201,2.2861041231473,5.98623040963234));
#73377=CARTESIAN_POINT('Ctrl Pts',(0.0744224348639616,2.5593968928388,6.00610075315511));
#73378=CARTESIAN_POINT('Ctrl Pts',(-0.345982923997342,2.41125555459024,
6.02597109667792));
#73379=CARTESIAN_POINT('Ctrl Pts',(-0.44899605141297,1.97757961862258,6.0458414402007));
#73380=CARTESIAN_POINT('Ctrl Pts',(-0.140116426950026,1.65620771653871,
6.0657117837235));
#73381=CARTESIAN_POINT('Ctrl Pts',(0.297300944110507,1.74195481766678,6.08558212724628));
#73382=CARTESIAN_POINT('Ctrl Pts',(0.46198517281843,2.15615963013551,6.10545247076906));
#73383=CARTESIAN_POINT('Ctrl Pts',(0.202860899067473,2.51884562739817,6.12532281429185));
#73384=CARTESIAN_POINT('Ctrl Pts',(-0.24236063256028,2.49729778220626,6.14519315781465));
#73385=CARTESIAN_POINT('Ctrl Pts',(-0.465249278234726,2.11128330904911,
6.16506350133744));
#73386=CARTESIAN_POINT('Ctrl Pts',(-0.261335049098668,1.71491793592323,
6.18493384486023));
#73387=CARTESIAN_POINT('Ctrl Pts',(0.182318510031114,1.67181293239863,6.20480418838301));
#73388=CARTESIAN_POINT('Ctrl Pts',(0.458719656631219,2.0215112709928,6.2246745319058));
#73389=CARTESIAN_POINT('Ctrl Pts',(0.314307967314327,2.44321233317549,6.24454487542858));
#73390=CARTESIAN_POINT('Ctrl Pts',(-0.118438492847544,2.55006280380969,
6.26441521895139));
#73391=CARTESIAN_POINT('Ctrl Pts',(-0.442533759766611,2.24404192246654,
6.28428556247417));
#73392=CARTESIAN_POINT('Ctrl Pts',(-0.360664547631079,1.80588218679737,
6.30415590599697));
#73393=CARTESIAN_POINT('Ctrl Pts',(0.0520652869115094,1.63753550421697,
6.32402624951974));
#73394=CARTESIAN_POINT('Ctrl Pts',(0.417032308761556,1.89343703766155,6.34389659304255));
#73395=CARTESIAN_POINT('Ctrl Pts',(0.399428961145075,2.33883196804363,6.36376693656534));
#73396=CARTESIAN_POINT('Ctrl Pts',(0.0154039190208104,2.56513108178215,
6.3836372800881));
#73397=CARTESIAN_POINT('Ctrl Pts',(-0.382752121750834,2.3647357498644,6.40350762361091));
#73398=CARTESIAN_POINT('Ctrl Pts',(-0.429785197812239,1.92148140796398,
6.42337796713368));
#73399=CARTESIAN_POINT('Ctrl Pts',(-0.0825488648521865,1.64199357114485,
6.44324831065649));
#73400=CARTESIAN_POINT('Ctrl Pts',(0.340414813596581,1.78266428085538,6.46311865417927));
#73401=CARTESIAN_POINT('Ctrl Pts',(0.451094243862592,2.21444731152398,6.48298899770206));
#73402=CARTESIAN_POINT('Ctrl Pts',(0.147956116320611,2.54124051446389,6.50285934122486));
#73403=CARTESIAN_POINT('Ctrl Pts',(-0.290911605539139,2.46325561485498,
6.52272968474764));
#73404=CARTESIAN_POINT('Ctrl Pts',(-0.462907533355605,2.05203314140305,
6.54260002827044));
#73405=CARTESIAN_POINT('Ctrl Pts',(-0.210248818488382,1.68481373061568,
6.56247037179321));
#73406=CARTESIAN_POINT('Ctrl Pts',(0.235284564549913,1.69847119948179,6.58234071531602));
#73407=CARTESIAN_POINT('Ctrl Pts',(0.46497639071474,2.08047667961323,6.6022110588388));
#73408=CARTESIAN_POINT('Ctrl Pts',(0.268115679218368,2.48039214833945,6.6220814023616));
#73409=CARTESIAN_POINT('Ctrl Pts',(-0.174704667307117,2.53134960667902,
6.64195174588437));
#73410=CARTESIAN_POINT('Ctrl Pts',(-0.457257265471105,2.18660252383689,
6.66182208940717));
#73411=CARTESIAN_POINT('Ctrl Pts',(-0.320338572520919,1.76240941524342,
6.68169243292995));
#73412=CARTESIAN_POINT('Ctrl Pts',(0.110447150558528,1.64790970935605,6.70156277645275));
#73413=CARTESIAN_POINT('Ctrl Pts',(0.439912649022332,1.94814129859904,6.72143311997555));
#73414=CARTESIAN_POINT('Ctrl Pts',(0.365818180707404,2.38768257268204,6.74130346349833));
#73415=CARTESIAN_POINT('Ctrl Pts',(-0.0438646667583175,2.56331425077502,
6.76117380702112));
#73416=CARTESIAN_POINT('Ctrl Pts',(-0.41330765410843,2.31391817832157,6.78104415054392));
#73417=CARTESIAN_POINT('Ctrl Pts',(-0.403597135570311,1.86828129958834,
6.80091449406668));
#73418=CARTESIAN_POINT('Ctrl Pts',(-0.0236411899349659,1.63521478283029,
6.8207848375895));
#73419=CARTESIAN_POINT('Ctrl Pts',(0.378002329008327,1.82852542803181,6.84065518111227));
#73420=CARTESIAN_POINT('Ctrl Pts',(0.432880171456738,2.27087703508844,6.86052552463507));
#73421=CARTESIAN_POINT('Ctrl Pts',(0.0906493879074764,2.55647222525914,
6.88039586815785));
#73422=CARTESIAN_POINT('Ctrl Pts',(-0.334739868247094,2.42331629183657,
6.90026621168064));
#73423=CARTESIAN_POINT('Ctrl Pts',(-0.453050866003015,1.99356167619252,
6.92013655520344));
#73424=CARTESIAN_POINT('Ctrl Pts',(-0.155749371507164,1.6614497323725,6.94000689872622));
#73425=CARTESIAN_POINT('Ctrl Pts',(0.284430967984231,1.73164795587294,6.959877242249));
#73426=CARTESIAN_POINT('Ctrl Pts',(0.463684616129835,2.13975903325736,6.9797475857718));
#73427=CARTESIAN_POINT('Ctrl Pts',(0.217570753936658,2.51139661033176,6.9996179292946));
#73428=CARTESIAN_POINT('Ctrl Pts',(-0.228134655409879,2.50563380401792,
7.01948827281737));
#73429=CARTESIAN_POINT('Ctrl Pts',(-0.464557576146697,2.12775720457354,
7.03935861634017));
#73430=CARTESIAN_POINT('Ctrl Pts',(-0.274812164572039,1.72441714873511,
7.05922895986296));
#73431=CARTESIAN_POINT('Ctrl Pts',(0.167035995699563,1.66562322794412,7.07909930338575));
#73432=CARTESIAN_POINT('Ctrl Pts',(0.455651369814231,2.00531086045673,7.09896964690853));
#73433=CARTESIAN_POINT('Ctrl Pts',(0.32626864345696,2.43186288773797,7.11883999043134));
#73434=CARTESIAN_POINT('Ctrl Pts',(-0.102421145807134,2.55397589457215,
7.13871033395412));
#73435=CARTESIAN_POINT('Ctrl Pts',(-0.437153477173104,2.25962782137364,
7.15858067747691));
#73436=CARTESIAN_POINT('Ctrl Pts',(-0.370857006304683,1.81884295343036,
7.17845102099969));
#73437=CARTESIAN_POINT('Ctrl Pts',(0.0356502802258794,1.63598139963914,
7.19832136452249));
#73438=CARTESIAN_POINT('Ctrl Pts',(0.409453287996592,1.87879374125082,7.21819170804527));
#73439=CARTESIAN_POINT('Ctrl Pts',(0.407638646062127,2.32453271075205,7.23806205156807));
#73440=CARTESIAN_POINT('Ctrl Pts',(0.0318710413561637,2.56429348550664,
7.25793239509085));
#73441=CARTESIAN_POINT('Ctrl Pts',(-0.373133904943599,2.37812819515931,
7.27780273861364));
#73442=CARTESIAN_POINT('Ctrl Pts',(-0.435839291051773,1.93681814948801,
7.29767308213644));
#73443=CARTESIAN_POINT('Ctrl Pts',(-0.0987214617815934,1.64520523645854,
7.31754342565922));
#73444=CARTESIAN_POINT('Ctrl Pts',(0.328959868959777,1.77080460426215,7.337413769182));
#73445=CARTESIAN_POINT('Ctrl Pts',(0.454865303772759,2.19839593174896,7.35728411270481));
#73446=CARTESIAN_POINT('Ctrl Pts',(0.163493746693623,2.5357223872526,7.37715445622759));
#73447=CARTESIAN_POINT('Ctrl Pts',(-0.277861065313151,2.47333287069862,
7.39702479975038));
#73448=CARTESIAN_POINT('Ctrl Pts',(-0.46431617726337,2.06846126995956,7.41689514327317));
#73449=CARTESIAN_POINT('Ctrl Pts',(-0.224824407514071,1.69252216042222,
7.43676548679595));
#73450=CARTESIAN_POINT('Ctrl Pts',(0.220913149050097,1.69038849559882,7.45663583031875));
#73451=CARTESIAN_POINT('Ctrl Pts',(0.463992965970334,2.06401762249259,7.47650617384153));
#73452=CARTESIAN_POINT('Ctrl Pts',(0.281422403551169,2.47065568219105,7.49637651736432));
#73453=CARTESIAN_POINT('Ctrl Pts',(-0.159314901925512,2.53726761369383,
7.51624686088712));
#73454=CARTESIAN_POINT('Ctrl Pts',(-0.453902473650952,2.20274603824273,
7.5361172044099));
#73455=CARTESIAN_POINT('Ctrl Pts',(-0.332096319043547,1.77396896031397,
7.55598754793269));
#73456=CARTESIAN_POINT('Ctrl Pts',(0.0943629974549827,1.64428097617902,
7.57585789145548));
#73457=CARTESIAN_POINT('Ctrl Pts',(0.43425711015065,1.93265315585696,7.59572823497828));
#73458=CARTESIAN_POINT('Ctrl Pts',(0.375779443050263,2.37454328282052,7.61559857850106));
#73459=CARTESIAN_POINT('Ctrl Pts',(-0.0274247052970846,2.56457732348921,
7.63546892202385));
#73460=CARTESIAN_POINT('Ctrl Pts',(-0.405470420070843,2.32842491634803,
7.65533926554663));
#73461=CARTESIAN_POINT('Ctrl Pts',(-0.411552224242792,1.88272374570183,
7.67520960906944));
#73462=CARTESIAN_POINT('Ctrl Pts',(-0.0400908904480416,1.63634395888319,
7.6950799525922));
#73463=CARTESIAN_POINT('Ctrl Pts',(0.368148377450899,1.81530546871901,7.71495029611502));
#73464=CARTESIAN_POINT('Ctrl Pts',(0.438661627914525,2.2554354533445,7.73482063963779));
#73465=CARTESIAN_POINT('Ctrl Pts',(0.106762553154688,2.55297457015259,7.7546909831606));
#73466=CARTESIAN_POINT('Ctrl Pts',(-0.32307662971541,2.43497118576493,7.77456132668337));
#73467=CARTESIAN_POINT('Ctrl Pts',(-0.456536987733129,2.00967734064704,
7.79443167020617));
#73468=CARTESIAN_POINT('Ctrl Pts',(-0.171186811404311,1.66724223916577,
7.81430201372895));
#73469=CARTESIAN_POINT('Ctrl Pts',(0.271203959408015,1.72180346860072,7.83417235725175));
#73470=CARTESIAN_POINT('Ctrl Pts',(0.464802018548613,2.12330852878598,7.85404270077455));
#73471=CARTESIAN_POINT('Ctrl Pts',(0.232007502751803,2.50343118697977,7.87391304429731));
#73472=CARTESIAN_POINT('Ctrl Pts',(-0.213622311850383,2.51346065331628,
7.89378338782013));
#73473=CARTESIAN_POINT('Ctrl Pts',(-0.463282737381516,2.14419625782033,
7.9136537313429));
#73474=CARTESIAN_POINT('Ctrl Pts',(-0.287944321614599,1.73438781255141,
7.9335240748657));
#73475=CARTESIAN_POINT('Ctrl Pts',(0.151543809154065,1.65997877566178,7.95339441838848));
#73476=CARTESIAN_POINT('Ctrl Pts',(0.452011125850539,1.98922930862201,7.97326476191127));
#73477=CARTESIAN_POINT('Ctrl Pts',(0.337819770337296,2.42009687085364,7.99313510543406));
#73478=CARTESIAN_POINT('Ctrl Pts',(-0.0862752344515524,2.55731913133102,
8.01300544895685));
#73479=CARTESIAN_POINT('Ctrl Pts',(-0.431224456943676,2.27501334719004,
8.03287579247963));
#73480=CARTESIAN_POINT('Ctrl Pts',(-0.380583946098691,1.83215664291795,
8.05274613600243));
#73481=CARTESIAN_POINT('Ctrl Pts',(0.0191905234661595,1.63500975518821,
8.07261647952521));
#73482=CARTESIAN_POINT('Ctrl Pts',(0.401360300304663,1.86442811436765,8.09248682304802));
#73483=CARTESIAN_POINT('Ctrl Pts',(0.415336641884546,2.30995160839845,8.11235716657078));
#73484=CARTESIAN_POINT('Ctrl Pts',(0.0482981575133614,2.5628730840542,8.1322275100936));
#73485=CARTESIAN_POINT('Ctrl Pts',(-0.363047311175928,2.39117151957044,
8.15209785361636));
#73486=CARTESIAN_POINT('Ctrl Pts',(-0.441346296289723,1.95235972530378,
8.17196819713918));
#73487=CARTESIAN_POINT('Ctrl Pts',(-0.114770138430408,1.64898778366247,
8.19183854066195));
#73488=CARTESIAN_POINT('Ctrl Pts',(0.317091996895345,1.75935815074194,8.21170888418476));
#73489=CARTESIAN_POINT('Ctrl Pts',(0.458065393246939,2.18222104031546,8.23157922770753));
#73490=CARTESIAN_POINT('Ctrl Pts',(0.178826151266698,2.52965731878344,8.25144957123033));
#73491=CARTESIAN_POINT('Ctrl Pts',(-0.264461739518581,2.48294149982973,
8.27131991475312));
#73492=CARTESIAN_POINT('Ctrl Pts',(-0.465141987510332,2.08492898755989,
8.29119025827591));
#73493=CARTESIAN_POINT('Ctrl Pts',(-0.239117785324893,1.70074207747079,
8.31106060179869));
#73494=CARTESIAN_POINT('Ctrl Pts',(0.206264431949168,1.68281995724421,8.33093094532149));
#73495=CARTESIAN_POINT('Ctrl Pts',(0.462427113276644,2.04760373231172,8.35080128884428));
#73496=CARTESIAN_POINT('Ctrl Pts',(0.294375871939588,2.46045394987548,8.37067163236707));
#73497=CARTESIAN_POINT('Ctrl Pts',(-0.143725156245875,2.54263673980266,
8.39054197588985));
#73498=CARTESIAN_POINT('Ctrl Pts',(-0.44997791998894,2.21876058051162,8.41041231941266));
#73499=CARTESIAN_POINT('Ctrl Pts',(-0.343437201104315,1.78593775639426,
8.43028266293542));
#73500=CARTESIAN_POINT('Ctrl Pts',(0.0781603950405117,1.64122428507152,
8.45015300645822));
#73501=CARTESIAN_POINT('Ctrl Pts',(0.428056469312614,1.91737507552185,8.470023349981));
#73502=CARTESIAN_POINT('Ctrl Pts',(0.385269007616535,2.36105937204245,8.48989369350379));
#73503=CARTESIAN_POINT('Ctrl Pts',(-0.0109503189284993,2.56525723473837,
8.50976403702659));
#73504=CARTESIAN_POINT('Ctrl Pts',(-0.397124218607941,2.34264492361486,
8.52963438054937));
#73505=CARTESIAN_POINT('Ctrl Pts',(-0.418990711295057,1.89743892819821,
8.54950472407216));
#73506=CARTESIAN_POINT('Ctrl Pts',(-0.0564902668035913,1.63805513995987,
8.56937506759495));
#73507=CARTESIAN_POINT('Ctrl Pts',(0.357832307024788,1.80244287269442,8.58924541111775));
#73508=CARTESIAN_POINT('Ctrl Pts',(0.443892453627643,2.23979876098687,8.60911575464052));
#73509=CARTESIAN_POINT('Ctrl Pts',(0.122741704527867,2.5489083179566,8.62898609816333));
#73510=CARTESIAN_POINT('Ctrl Pts',(-0.311007848702041,2.44620560655015,
8.64885644168609));
#73511=CARTESIAN_POINT('Ctrl Pts',(-0.459450040643157,2.02590638277131,
8.66872678520892));
#73512=CARTESIAN_POINT('Ctrl Pts',(-0.18640936876913,1.67357796586466,8.68859712873168));
#73513=CARTESIAN_POINT('Ctrl Pts',(0.257636521606575,1.71243371315928,8.7084674722545));
#73514=CARTESIAN_POINT('Ctrl Pts',(0.465335977453503,2.10682876624473,8.72833781577727));
#73515=CARTESIAN_POINT('Ctrl Pts',(0.246153023759728,2.49495935595321,8.74820815930007));
#73516=CARTESIAN_POINT('Ctrl Pts',(-0.198841818525403,2.52076850543563,
8.76807850282285));
#73517=CARTESIAN_POINT('Ctrl Pts',(-0.461426362182681,2.16057983364032,
8.78794884634566));
#73518=CARTESIAN_POINT('Ctrl Pts',(-0.30071503606418,1.74481741167964,8.80781918986842));
#73519=CARTESIAN_POINT('Ctrl Pts',(0.135861396987775,1.6548866607598,8.82768953339124));
#73520=CARTESIAN_POINT('Ctrl Pts',(0.447803494162487,1.97328680188354,8.847559876914));
#73521=CARTESIAN_POINT('Ctrl Pts',(0.348946848383933,2.40792905183493,8.86743022043681));
#73522=CARTESIAN_POINT('Ctrl Pts',(-0.0700210259631247,2.56008831748274,
8.88730056395958));
#73523=CARTESIAN_POINT('Ctrl Pts',(-0.424754141490919,2.29017918720865,
8.9071709074824));
#73524=CARTESIAN_POINT('Ctrl Pts',(-0.389833157255602,1.84580654322906,
8.92704125100514));
#73525=CARTESIAN_POINT('Ctrl Pts',(0.00270667776965062,1.6346217905225,
8.94691159452797));
#73526=CARTESIAN_POINT('Ctrl Pts',(0.392763504422148,1.85035818948929,8.96678193805073));
#73527=CARTESIAN_POINT('Ctrl Pts',(0.422513285690156,2.29510696393603,8.98665228157354));
#73528=CARTESIAN_POINT('Ctrl Pts',(0.0646646473272788,2.56087166038613,
9.00652262509631));
#73529=CARTESIAN_POINT('Ctrl Pts',(-0.352505001661575,2.40384935044295,
9.02639296861913));
#73530=CARTESIAN_POINT('Ctrl Pts',(-0.446299300848517,1.96808662682216,
9.04626331214188));
#73531=CARTESIAN_POINT('Ctrl Pts',(-0.130674749670337,1.65333646470792,
9.0661336556647));
#73532=CARTESIAN_POINT('Ctrl Pts',(0.304826094569618,1.74833928847471,9.08600399918746));
#73533=CARTESIAN_POINT('Ctrl Pts',(0.460690495367448,2.16594294078312,9.10587434271029));
#73534=CARTESIAN_POINT('Ctrl Pts',(0.19393408401326,2.52305292224374,9.12574468623304));
#73535=CARTESIAN_POINT('Ctrl Pts',(-0.250730447681617,2.49206944100045,
9.14561502975586));
#73536=CARTESIAN_POINT('Ctrl Pts',(-0.465383927496798,2.10141562307388,
9.16548537327863));
#73537=CARTESIAN_POINT('Ctrl Pts',(-0.253111010134359,1.70946316369669,
9.18535571680145));
#73538=CARTESIAN_POINT('Ctrl Pts',(0.191356801073853,1.67577508483846,9.20522606032421));
#73539=CARTESIAN_POINT('Ctrl Pts',(0.460280798172897,2.0312556126338,9.22509640384702));
#73540=CARTESIAN_POINT('Ctrl Pts',(0.306959824520678,2.44979975713437,9.2449667473698));
#73541=CARTESIAN_POINT('Ctrl Pts',(-0.127954999322651,2.54745024540095,
9.26483709089259));
#73542=CARTESIAN_POINT('Ctrl Pts',(-0.445488530787639,2.2346260483625,9.28470743441539));
#73543=CARTESIAN_POINT('Ctrl Pts',(-0.354346983041982,1.79830077963296,
9.30457777793815));
#73544=CARTESIAN_POINT('Ctrl Pts',(0.0618596816589883,1.63874347295017,
9.32444812146097));
#73545=CARTESIAN_POINT('Ctrl Pts',(0.421318509873045,1.90232623542972,9.34431846498375));
#73546=CARTESIAN_POINT('Ctrl Pts',(0.394274962614376,2.34724776604949,9.36418880850655));
#73547=CARTESIAN_POINT('Ctrl Pts',(0.00553781284629133,2.56535313106277,
9.38405915202932));
#73548=CARTESIAN_POINT('Ctrl Pts',(-0.38827952630312,2.35656035043407,9.4039294955521));
#73549=CARTESIAN_POINT('Ctrl Pts',(-0.425903259553746,1.91240837581992,
9.4237998390749));
#73550=CARTESIAN_POINT('Ctrl Pts',(-0.0728187336569238,1.64034617809743,
9.44367018259769));
#73551=CARTESIAN_POINT('Ctrl Pts',(0.347067066994716,1.78995378575329,9.46354052612046));
#73552=CARTESIAN_POINT('Ctrl Pts',(0.448566082593332,2.22398658599988,9.48341086964328));
#73553=CARTESIAN_POINT('Ctrl Pts',(0.138566784170425,2.54427857284107,9.50328121316604));
#73554=CARTESIAN_POINT('Ctrl Pts',(-0.298548674564602,2.4570054521667,9.52315155668886));
#73555=CARTESIAN_POINT('Ctrl Pts',(-0.461786368118551,2.04222843103298,
9.54302190021163));
#73556=CARTESIAN_POINT('Ctrl Pts',(-0.201397935460937,1.68044895953757,
9.56289224373443));
#73557=CARTESIAN_POINT('Ctrl Pts',(0.243745685128986,1.7035504509499,9.58276258725722));
#73558=CARTESIAN_POINT('Ctrl Pts',(0.465285822591689,2.09034043188319,9.60263293078001));
#73559=CARTESIAN_POINT('Ctrl Pts',(0.259989560771447,2.48599175153221,9.6225032743028));
#73560=CARTESIAN_POINT('Ctrl Pts',(-0.183811728673993,2.52754818718234,
9.64237361782559));
#73561=CARTESIAN_POINT('Ctrl Pts',(-0.458990780768273,2.17688736652246,
9.66224396134838));
#73562=CARTESIAN_POINT('Ctrl Pts',(-0.313108277460035,1.75569285434797,
9.68211430487117));
#73563=CARTESIAN_POINT('Ctrl Pts',(0.120008444574899,1.65035327512396,9.70198464839396));
#73564=CARTESIAN_POINT('Ctrl Pts',(0.443033756386806,1.95750335209969,9.72185499191675));
#73565=CARTESIAN_POINT('Ctrl Pts',(0.359635910313481,2.39537470435707,9.74172533543954));
#73566=CARTESIAN_POINT('Ctrl Pts',(-0.0536789234643323,2.56227997700175,
9.76159567896233));
#73567=CARTESIAN_POINT('Ctrl Pts',(-0.417750652689171,2.30510630448332,
9.78146602248512));
#73568=CARTESIAN_POINT('Ctrl Pts',(-0.398593029687583,1.8597755203034,9.80133636600791));
#73569=CARTESIAN_POINT('Ctrl Pts',(-0.0137805654886717,1.63481799263531,
9.82120670953068));
#73570=CARTESIAN_POINT('Ctrl Pts',(0.383673691491512,1.83660162791257,9.84107705305349));
#73571=CARTESIAN_POINT('Ctrl Pts',(0.429159568984776,2.28001741112968,9.86094739657626));
#73572=CARTESIAN_POINT('Ctrl Pts',(0.0809499667341075,2.55829172679285,
9.88081774009907));
#73573=CARTESIAN_POINT('Ctrl Pts',(-0.341520209652263,2.41614577390835,
9.90068808362184));
#73574=CARTESIAN_POINT('Ctrl Pts',(-0.450692087460871,1.98397911282362,
9.92055842714464));
#73575=CARTESIAN_POINT('Ctrl Pts',(-0.146415331211417,1.6582458209057,9.94042877066742));
#73576=CARTESIAN_POINT('Ctrl Pts',(0.29217755877707,1.73776184890586,9.96029911419022));
#73577=CARTESIAN_POINT('Ctrl Pts',(0.462737314970446,2.14958206626366,9.980169457713));
#73578=CARTESIAN_POINT('Ctrl Pts',(0.20879858067537,2.51591748781337,10.0000398012358));
#73579=CARTESIAN_POINT('Ctrl Pts',(-0.23668442602939,2.50070523634733,10.0199101447586));
#73580=CARTESIAN_POINT('Ctrl Pts',(-0.465041693527188,2.11790048162462,
10.0397804882814));
#73581=CARTESIAN_POINT('Ctrl Pts',(-0.26678651692355,1.71867447194184,10.0596508318042));
#73582=CARTESIAN_POINT('Ctrl Pts',(0.176208969252817,1.66926272146946,10.0795211753269));
#73583=CARTESIAN_POINT('Ctrl Pts',(0.457556714824719,2.0149937844635,10.0993915188498));
#73584=CARTESIAN_POINT('Ctrl Pts',(0.319158465266864,2.43870647766102,10.1192618623725));
#73585=CARTESIAN_POINT('Ctrl Pts',(-0.112024226671758,2.55170208832772,
10.1391322058953));
#73586=CARTESIAN_POINT('Ctrl Pts',(-0.440439941360369,2.25032252664023,
10.1590025494181));
#73587=CARTESIAN_POINT('Ctrl Pts',(-0.364811970334474,1.81104251132439,
10.1788728929409));
#73588=CARTESIAN_POINT('Ctrl Pts',(0.0454813188082286,1.63684165385853,
10.1987432364637));
#73589=CARTESIAN_POINT('Ctrl Pts',(0.414051689666831,1.88752552566232,10.2186135799865));
#73590=CARTESIAN_POINT('Ctrl Pts',(0.402786003303662,2.33312580188322,10.2384839235093));
#73591=CARTESIAN_POINT('Ctrl Pts',(0.0220189932722285,2.56486489208834,
10.2583542670321));
#73592=CARTESIAN_POINT('Ctrl Pts',(-0.378947445471223,2.37015372944282,
10.2782246105549));
#73593=CARTESIAN_POINT('Ctrl Pts',(-0.432281192031075,1.92761329814274,
10.2980949540776));
#73594=CARTESIAN_POINT('Ctrl Pts',(-0.0890557946726181,1.64321419746641,
10.3179652976004));
#73595=CARTESIAN_POINT('Ctrl Pts',(0.335866170446296,1.77785388484296,10.3378356411232));
#73596=CARTESIAN_POINT('Ctrl Pts',(0.452676648230991,2.20801877664271,10.357705984646));
#73597=CARTESIAN_POINT('Ctrl Pts',(0.154217927624591,2.53909114630132,10.3775763281688));
#73598=CARTESIAN_POINT('Ctrl Pts',(-0.285714746702346,2.46735716609023,
10.3974466716916));
#73599=CARTESIAN_POINT('Ctrl Pts',(-0.463543037480315,2.05862299715355,
10.4173170152144));
#73600=CARTESIAN_POINT('Ctrl Pts',(-0.216133697056242,1.68784659535819,
10.4371873587372));
#73601=CARTESIAN_POINT('Ctrl Pts',(0.229548886471042,1.69516483270233,10.45705770226));
#73602=CARTESIAN_POINT('Ctrl Pts',(0.464651616920155,2.07386422271074,10.4769280457828));
#73603=CARTESIAN_POINT('Ctrl Pts',(0.27349974545065,2.47653963031726,10.4967983893055));
#73604=CARTESIAN_POINT('Ctrl Pts',(-0.16855090884166,2.53379118834951,10.5166687328283));
#73605=CARTESIAN_POINT('Ctrl Pts',(-0.455979050405958,2.19309838640872,
10.5365390763511));
#73606=CARTESIAN_POINT('Ctrl Pts',(-0.325108489165098,1.76700048913877,
10.5564094198739));
#73607=CARTESIAN_POINT('Ctrl Pts',(0.104004851360552,1.6463843092942,10.5762797633967));
#73608=CARTESIAN_POINT('Ctrl Pts',(0.437707899744855,1.94189877147228,10.5961501069195));
#73609=CARTESIAN_POINT('Ctrl Pts',(0.369873538663006,2.38244958728584,10.6160204504423));
#73610=CARTESIAN_POINT('Ctrl Pts',(-0.0372694404067732,2.56389135880376,
10.635890793965));
#73611=CARTESIAN_POINT('Ctrl Pts',(-0.410222781679494,2.31977596172505,
10.6557611374879));
#73612=CARTESIAN_POINT('Ctrl Pts',(-0.406852567550072,1.87404603955906,
10.6756314810106));
#73613=CARTESIAN_POINT('Ctrl Pts',(-0.0302505106690354,1.63559811524361,
10.6955018245334));
#73614=CARTESIAN_POINT('Ctrl Pts',(0.374102271515687,1.82317569758449,10.7153721680562));
#73615=CARTESIAN_POINT('Ctrl Pts',(0.435267149010142,2.26470189116587,10.735242511579));
#73616=CARTESIAN_POINT('Ctrl Pts',(0.0971336735593306,2.55513652174034,
10.7551128551018));
#73617=CARTESIAN_POINT('Ctrl Pts',(-0.330106723826589,2.42804535486044,
10.7749831986246));
#73618=CARTESIAN_POINT('Ctrl Pts',(-0.454519142074015,2.00001723423843,
10.7948535421474));
#73619=CARTESIAN_POINT('Ctrl Pts',(-0.161972124662258,1.66370968977821,
10.8147238856702));
#73620=CARTESIAN_POINT('Ctrl Pts',(0.279162266613492,1.72763910938412,10.834594229193));
#73621=CARTESIAN_POINT('Ctrl Pts',(0.464203282782185,2.13315895377233,10.8544645727157));
#73622=CARTESIAN_POINT('Ctrl Pts',(0.223400982568651,2.50825997225836,10.8743349162385));
#73623=CARTESIAN_POINT('Ctrl Pts',(-0.222341305854143,2.50883804577376,
10.8942052597613));
#73624=CARTESIAN_POINT('Ctrl Pts',(-0.464115715191275,2.13436287056577,
10.9140756032841));
#73625=CARTESIAN_POINT('Ctrl Pts',(-0.280127139489603,1.72836443969608,
10.9339459468069));
#73626=CARTESIAN_POINT('Ctrl Pts',(0.160839950827386,1.66329104179227,10.9538162903297));
#73627=CARTESIAN_POINT('Ctrl Pts',(0.454258282642319,1.99883866048791,10.9736866338525));
#73628=CARTESIAN_POINT('Ctrl Pts',(0.330956481813854,2.42718803631311,10.9935569773753));
#73629=CARTESIAN_POINT('Ctrl Pts',(-0.0959528354223248,2.55538693145,11.0134273208981));
#73630=CARTESIAN_POINT('Ctrl Pts',(-0.434838488957494,2.2658303123141,11.0332976644208));
#73631=CARTESIAN_POINT('Ctrl Pts',(-0.374819026788911,1.82414695738845,
11.0531680079437));
#73632=CARTESIAN_POINT('Ctrl Pts',(0.0290458654557084,1.63552121505825,
11.0730383514664));
#73633=CARTESIAN_POINT('Ctrl Pts',(0.406265130382235,1.87299152483544,11.0929086949892));
#73634=CARTESIAN_POINT('Ctrl Pts',(0.410791446186281,2.31871120616287,11.112779038512));
#73635=CARTESIAN_POINT('Ctrl Pts',(0.038472534319897,2.56379313067792,11.1326493820348));
#73636=CARTESIAN_POINT('Ctrl Pts',(-0.369139690222393,2.38340799752927,
11.1525197255576));
#73637=CARTESIAN_POINT('Ctrl Pts',(-0.438116502816576,1.94303460916239,
11.1723900690804));
#73638=CARTESIAN_POINT('Ctrl Pts',(-0.105181068252582,1.64665559798066,
11.1922604126032));
#73639=CARTESIAN_POINT('Ctrl Pts',(0.324243677323718,1.76615835838436,11.212130756126));
#73640=CARTESIAN_POINT('Ctrl Pts',(0.456218990746203,2.19191537653487,11.2320010996487));
#73641=CARTESIAN_POINT('Ctrl Pts',(0.169675488766272,2.53335254986322,11.2518714431715));
#73642=CARTESIAN_POINT('Ctrl Pts',(-0.27252217492476,2.47724775431447,11.2717417866943));
#73643=CARTESIAN_POINT('Ctrl Pts',(-0.46471784366629,2.07506950182638,11.2916121302171));
#73644=CARTESIAN_POINT('Ctrl Pts',(-0.230598156465567,1.69576158743173,
11.3114824737399));
#73645=CARTESIAN_POINT('Ctrl Pts',(0.215063946188089,1.68728738447797,11.3313528172627));
#73646=CARTESIAN_POINT('Ctrl Pts',(0.463434156526629,2.0574208205166,11.3512231607855));
#73647=CARTESIAN_POINT('Ctrl Pts',(0.286666619115345,2.46661485709939,11.3710935043083));
#73648=CARTESIAN_POINT('Ctrl Pts',(-0.153078515198115,2.53948967239944,
11.3909638478311));
#73649=CARTESIAN_POINT('Ctrl Pts',(-0.452394951575326,2.2091925443892,11.4108341913539));
#73650=CARTESIAN_POINT('Ctrl Pts',(-0.336700607893486,1.77872612212446,
11.4307045348766));
#73651=CARTESIAN_POINT('Ctrl Pts',(0.0878707058819758,1.64298474532153,
11.4505748783994));
#73652=CARTESIAN_POINT('Ctrl Pts',(0.431832609527119,1.92649264767732,11.4704452219222));
#73653=CARTESIAN_POINT('Ctrl Pts',(0.379646882632345,2.36916992489611,11.490315565445));
#73654=CARTESIAN_POINT('Ctrl Pts',(-0.0208131748215914,2.56492044019905,
11.5101859089678));
#73655=CARTESIAN_POINT('Ctrl Pts',(-0.402179977834614,2.33416974482196,
11.5300562524906));
#73656=CARTESIAN_POINT('Ctrl Pts',(-0.414601403044297,1.8886001879028,11.5499265960134));
#73657=CARTESIAN_POINT('Ctrl Pts',(-0.0466824838451108,1.63696117909718,
11.5697969395362));
#73658=CARTESIAN_POINT('Ctrl Pts',(0.364061259035663,1.81009725142662,11.589667283059));
#73659=CARTESIAN_POINT('Ctrl Pts',(0.440828359216179,2.24917962887675,11.6095376265817));
#73660=CARTESIAN_POINT('Ctrl Pts',(0.113195453177793,2.55141000580503,11.6294079701045));
#73661=CARTESIAN_POINT('Ctrl Pts',(-0.318278870981795,2.43953315633025,
11.6492783136273));
#73662=CARTESIAN_POINT('Ctrl Pts',(-0.457775660771225,2.01618085918777,
11.6691486571501));
#73663=CARTESIAN_POINT('Ctrl Pts',(-0.17732560233177,1.66972121279488,11.6890190006729));
#73664=CARTESIAN_POINT('Ctrl Pts',(0.265796555546213,1.71798377649529,11.7088893441957));
#73665=CARTESIAN_POINT('Ctrl Pts',(0.46508655864411,2.11669421844861,11.7287596877185));
#73666=CARTESIAN_POINT('Ctrl Pts',(0.237722960003616,2.50008998768796,11.7486300312413));
#73667=CARTESIAN_POINT('Ctrl Pts',(-0.207719091381555,2.51645766055705,
11.7685003747641));
#73668=CARTESIAN_POINT('Ctrl Pts',(-0.462607154824915,2.15078212545596,
11.7883707182868));
#73669=CARTESIAN_POINT('Ctrl Pts',(-0.293116131993658,1.73852090361114,
11.8082410618096));
#73670=CARTESIAN_POINT('Ctrl Pts',(0.145269037783732,1.65786754176783,11.8281114053324));
#73671=CARTESIAN_POINT('Ctrl Pts',(0.450389641988224,1.98281051945354,11.8479817488552));
#73672=CARTESIAN_POINT('Ctrl Pts',(0.342339064681582,2.41525889163349,11.867852092378));
#73673=CARTESIAN_POINT('Ctrl Pts',(-0.0797609992151842,2.55850014936227,
11.8877224359008));
#73674=CARTESIAN_POINT('Ctrl Pts',(-0.428691204811542,2.28112993921011,
11.9075927794236));
#73675=CARTESIAN_POINT('Ctrl Pts',(-0.384355591030892,1.83759766844724,
11.9274631229464));
#73676=CARTESIAN_POINT('Ctrl Pts',(0.0125739522318252,1.63478381403233,
11.9473334664692));
#73677=CARTESIAN_POINT('Ctrl Pts',(0.397968606110868,1.85874247677801,11.967203809992));
#73678=CARTESIAN_POINT('Ctrl Pts',(0.41828124241662,2.3040220728339,11.9870741535147));
#73679=CARTESIAN_POINT('Ctrl Pts',(0.0548777826542892,2.56213919216181,
12.0069444970375));
#73680=CARTESIAN_POINT('Ctrl Pts',(-0.358868571757863,2.39630651725115,
12.0268148405603));
#73681=CARTESIAN_POINT('Ctrl Pts',(-0.443401867126601,1.95865295125233,
12.0466851840831));
#73682=CARTESIAN_POINT('Ctrl Pts',(-0.12117431312009,1.65066605981642,12.0665555276059));
#73683=CARTESIAN_POINT('Ctrl Pts',(0.312214176780983,1.7548818872067,12.0864258711287));
#73684=CARTESIAN_POINT('Ctrl Pts',(0.459188663607583,2.17569659949637,12.1062962146515));
#73685=CARTESIAN_POINT('Ctrl Pts',(0.184920064465904,2.52706998690959,12.1261665581743));
#73686=CARTESIAN_POINT('Ctrl Pts',(-0.258987519229711,2.48666480166194,
12.1460369016971));
#73687=CARTESIAN_POINT('Ctrl Pts',(-0.465309311999041,2.09154730054888,
12.1659072452199));
#73688=CARTESIAN_POINT('Ctrl Pts',(-0.244773157151966,1.70418400045111,
12.1857775887426));
#73689=CARTESIAN_POINT('Ctrl Pts',(0.20030904652572,1.67992799445691,12.2056479322654));
#73690=CARTESIAN_POINT('Ctrl Pts',(0.461634969630317,2.04103086590896,12.2255182757882));
#73691=CARTESIAN_POINT('Ctrl Pts',(0.299473654025266,2.45622988996684,12.245388619311));
#73692=CARTESIAN_POINT('Ctrl Pts',(-0.137413969491446,2.54463648630048,
12.2652589628338));
#73693=CARTESIAN_POINT('Ctrl Pts',(-0.448242983222447,2.22514963824505,
12.2851293063566));
#73694=CARTESIAN_POINT('Ctrl Pts',(-0.347870082618712,1.79085503468456,
12.3049996498794));
#73695=CARTESIAN_POINT('Ctrl Pts',(0.0716262605523633,1.64015885051431,
12.3248699934022));
#73696=CARTESIAN_POINT('Ctrl Pts',(0.425415260701503,1.91130431927756,12.3447403369249));
#73697=CARTESIAN_POINT('Ctrl Pts',(0.388943674215075,2.35555238650639,12.3646106804478));
#73698=CARTESIAN_POINT('Ctrl Pts',(-0.00433078346378373,2.56536592943147,
12.3844810239705));
#73699=CARTESIAN_POINT('Ctrl Pts',(-0.393632336897545,2.34826958595367,
12.4043513674933));
#73700=CARTESIAN_POINT('Ctrl Pts',(-0.421829809431507,1.90341969621549,
12.4242217110161));
#73701=CARTESIAN_POINT('Ctrl Pts',(-0.0630558587549978,1.63890547320782,
12.4440920545389));
#73702=CARTESIAN_POINT('Ctrl Pts',(0.353563258049211,1.79738270618047,12.4639623980617));
#73703=CARTESIAN_POINT('Ctrl Pts',(0.445836218884442,2.23347010860809,12.4838327415845));
#73704=CARTESIAN_POINT('Ctrl Pts',(0.129115144013671,2.54711685670232,12.5037030851073));
#73705=CARTESIAN_POINT('Ctrl Pts',(-0.306051498050013,2.45059475823574,
12.5235734286301));
#73706=CARTESIAN_POINT('Ctrl Pts',(-0.46045755580194,2.03244969825429,12.5434437721529));
#73707=CARTESIAN_POINT('Ctrl Pts',(-0.192456491741336,1.67627284398136,
12.5633141156756));
#73708=CARTESIAN_POINT('Ctrl Pts',(0.25209720290648,1.70880797011217,12.5831844591984));
#73709=CARTESIAN_POINT('Ctrl Pts',(0.465386033822722,2.10020852767918,12.6030548027212));
#73710=CARTESIAN_POINT('Ctrl Pts',(0.251746535294047,2.49141778948901,12.622925146244));
#73711=CARTESIAN_POINT('Ctrl Pts',(-0.192836137170855,2.52355451616297,
12.6427954897668));
#73712=CARTESIAN_POINT('Ctrl Pts',(-0.460517906051078,2.16713763599796,
12.6626658332896));
#73713=CARTESIAN_POINT('Ctrl Pts',(-0.305737189981008,1.74913111476862,
12.6825361768124));
#73714=CARTESIAN_POINT('Ctrl Pts',(0.129515775536461,1.65299902925365,12.7024065203352));
#73715=CARTESIAN_POINT('Ctrl Pts',(0.445955648980351,1.96692948071131,12.722276863858));
#73716=CARTESIAN_POINT('Ctrl Pts',(0.353291925863331,2.40293401770104,12.7421472073807));
#73717=CARTESIAN_POINT('Ctrl Pts',(-0.0634690428790086,2.56103783419247,
12.7620175509035));
#73718=CARTESIAN_POINT('Ctrl Pts',(-0.422005805312989,2.29620220244602,
12.7818878944263));
#73719=CARTESIAN_POINT('Ctrl Pts',(-0.393409692268796,1.8513777604729,12.8017582379491));
#73720=CARTESIAN_POINT('Ctrl Pts',(-0.00391374447314742,1.63463037640504,
12.8216285814719));
#73721=CARTESIAN_POINT('Ctrl Pts',(0.389172531091156,1.84479626763077,12.8414989249947));
#73722=CARTESIAN_POINT('Ctrl Pts',(0.425245990391475,2.28907684045705,12.8613692685175));
#73723=CARTESIAN_POINT('Ctrl Pts',(0.0712141456059791,2.55990515264628,
12.8812396120403));
#73724=CARTESIAN_POINT('Ctrl Pts',(-0.34814698300506,2.40883309772541,12.9011099555631));
#73725=CARTESIAN_POINT('Ctrl Pts',(-0.448130650327812,1.97444871945192,
12.9209802990858));
#73726=CARTESIAN_POINT('Ctrl Pts',(-0.137015454056879,1.65524054885501,
12.9408506426087));
#73727=CARTESIAN_POINT('Ctrl Pts',(0.299792769502911,1.74403862608033,12.9607209861314));
#73728=CARTESIAN_POINT('Ctrl Pts',(0.461581937906987,2.15938280424948,12.9805913296542));
#73729=CARTESIAN_POINT('Ctrl Pts',(0.199932521296602,2.5202513434933,13.000461673177));
#73730=CARTESIAN_POINT('Ctrl Pts',(-0.245127773547357,2.49559648764708,
13.0203320166998));
#73731=CARTESIAN_POINT('Ctrl Pts',(-0.465316691309975,2.10803570899936,
13.0402023602226));
#73732=CARTESIAN_POINT('Ctrl Pts',(-0.258640922731129,1.71310326320296,
13.0600727037454));
#73733=CARTESIAN_POINT('Ctrl Pts',(0.185302740972675,1.67309589853287,13.0799430472682));
#73734=CARTESIAN_POINT('Ctrl Pts',(0.459256252303584,2.02471493624459,13.099813390791));
#73735=CARTESIAN_POINT('Ctrl Pts',(0.311904894240494,2.44539775727322,13.1196837343137));
#73736=CARTESIAN_POINT('Ctrl Pts',(-0.121577166018006,2.54922518374711,
13.1395540778365));
#73737=CARTESIAN_POINT('Ctrl Pts',(-0.443527911509105,2.24094961037721,
13.1594244213593));
#73738=CARTESIAN_POINT('Ctrl Pts',(-0.358603751119627,1.80337205481489,
13.1792947648821));
#73739=CARTESIAN_POINT('Ctrl Pts',(0.0552935593811353,1.63791007031839,
13.1991651084049));
#73740=CARTESIAN_POINT('Ctrl Pts',(0.418460724523598,1.89635304745533,13.2190354519277));
#73741=CARTESIAN_POINT('Ctrl Pts',(0.397758376589411,2.34161368802065,13.2389057954505));
#73742=CARTESIAN_POINT('Ctrl Pts',(0.0121452312493891,2.56522799449065,
13.2587761389733));
#73743=CARTESIAN_POINT('Ctrl Pts',(-0.384567834882505,2.36205638544088,
13.2786464824961));
#73744=CARTESIAN_POINT('Ctrl Pts',(-0.428572544079887,1.91848866214859,
13.2985168260188));
#73745=CARTESIAN_POINT('Ctrl Pts',(-0.0792656100846051,1.64142334060457,
13.3183871695417));
#73746=CARTESIAN_POINT('Ctrl Pts',(0.342458274427398,1.78505822158492,13.3382575130644));
#73747=CARTESIAN_POINT('Ctrl Pts',(0.450603146122972,2.21757196606139,13.3581278565872));
#73748=CARTESIAN_POINT('Ctrl Pts',(0.144148881373328,2.54238907754302,13.3780026364007));
#73749=CARTESIAN_POINT('Ctrl Pts',(-0.146654456177299,2.48806903884852,
13.3912539683733));
#73750=CARTESIAN_POINT('Ctrl Pts',(-0.248368994146077,2.40531761840563,
13.3978818525049));
#73751=CARTESIAN_POINT('Ctrl Pts',(-0.203466370082455,2.35062899684047,
4.3567));
#73752=CARTESIAN_POINT('Ctrl Pts',(-0.198643714809141,2.35553329018579,
4.3567));
#73753=CARTESIAN_POINT('Ctrl Pts',(-0.193660853029549,2.36026430325056,
4.3567));
#73754=CARTESIAN_POINT('Ctrl Pts',(-0.188522749684309,2.36481173887452,
4.3567));
#73755=CARTESIAN_POINT('Ctrl Pts',(-0.174734518930225,2.37701489780488,
4.3567));
#73756=CARTESIAN_POINT('Ctrl Pts',(-0.159831435216182,2.38789858237333,
4.3567));
#73757=CARTESIAN_POINT('Ctrl Pts',(-0.144036878378854,2.3974639952058,4.3567));
#73758=CARTESIAN_POINT('Ctrl Pts',(-0.141576690706492,2.39895392056261,
4.3567));
#73759=CARTESIAN_POINT('Ctrl Pts',(-0.139094796118624,2.40041179592735,
4.3567));
#73760=CARTESIAN_POINT('Ctrl Pts',(-0.136591958438483,2.40183754983713,
4.3567));
#73761=CARTESIAN_POINT('Ctrl Pts',(-0.131420216294938,2.4047836584242,4.3567));
#73762=CARTESIAN_POINT('Ctrl Pts',(-0.12616810244625,2.40758749052332,4.3567));
#73763=CARTESIAN_POINT('Ctrl Pts',(-0.120843445135949,2.41024936098874,
4.3567));
#73764=CARTESIAN_POINT('Ctrl Pts',(-0.105969803272818,2.41768490203512,
4.3567));
#73765=CARTESIAN_POINT('Ctrl Pts',(-0.0905311339839462,2.42401457076917,
4.3567));
#73766=CARTESIAN_POINT('Ctrl Pts',(-0.0746791492274175,2.42923308272867,
4.3567));
#73767=CARTESIAN_POINT('Ctrl Pts',(-0.0679382765650449,2.43145219441382,
4.3567));
#73768=CARTESIAN_POINT('Ctrl Pts',(-0.0611197830975242,2.43347078159887,
4.3567));
#73769=CARTESIAN_POINT('Ctrl Pts',(-0.0542434236638015,2.4352848700941,
4.3567));
#73770=CARTESIAN_POINT('Ctrl Pts',(-0.0458797197062097,2.43749134275936,
4.3567));
#73771=CARTESIAN_POINT('Ctrl Pts',(-0.0374438472594873,2.43939194329253,
4.3567));
#73772=CARTESIAN_POINT('Ctrl Pts',(-0.0289612584600339,2.44098632127078,
4.3567));
#73773=CARTESIAN_POINT('Ctrl Pts',(-0.0091843508866179,2.44470356687333,
4.3567));
#73774=CARTESIAN_POINT('Ctrl Pts',(0.0108541911413975,2.44676182489034,
4.3567));
#73775=CARTESIAN_POINT('Ctrl Pts',(0.0309100698820238,2.44713877334642,
4.3567));
#73776=CARTESIAN_POINT('Ctrl Pts',(0.0450748590705997,2.44740499929864,
4.3567));
#73777=CARTESIAN_POINT('Ctrl Pts',(0.0592490886611076,2.44683168334103,
4.35670000000001));
#73778=CARTESIAN_POINT('Ctrl Pts',(0.073350647231715,2.44539578335235,4.3567));
#73779=CARTESIAN_POINT('Ctrl Pts',(0.0795644863214801,2.44476305531496,
4.3567));
#73780=CARTESIAN_POINT('Ctrl Pts',(0.0857603507931046,2.44396272953801,
4.3567));
#73781=CARTESIAN_POINT('Ctrl Pts',(0.0919138197553597,2.44299632212969,
4.3567));
#73782=CARTESIAN_POINT('Ctrl Pts',(0.105989893738086,2.44078566302662,4.3567));
#73783=CARTESIAN_POINT('Ctrl Pts',(0.119869569405396,2.43770438812349,4.3567));
#73784=CARTESIAN_POINT('Ctrl Pts',(0.133470056976512,2.43374310478803,4.3567));
#73785=CARTESIAN_POINT('Ctrl Pts',(0.150216753309979,2.42886545545649,4.35670000000001));
#73786=CARTESIAN_POINT('Ctrl Pts',(0.16654080005684,2.42265470234242,4.35670000000001));
#73787=CARTESIAN_POINT('Ctrl Pts',(0.182361818588615,2.41523366612292,4.3567));
#73788=CARTESIAN_POINT('Ctrl Pts',(0.189998595912251,2.41165154522438,4.3567));
#73789=CARTESIAN_POINT('Ctrl Pts',(0.197518709781143,2.40778664511544,4.3567));
#73790=CARTESIAN_POINT('Ctrl Pts',(0.204911457815444,2.40365083222556,4.3567));
#73791=CARTESIAN_POINT('Ctrl Pts',(0.210963294651808,2.40026518122282,4.3567));
#73792=CARTESIAN_POINT('Ctrl Pts',(0.21692334188249,2.39670120955451,4.3567));
#73793=CARTESIAN_POINT('Ctrl Pts',(0.222772819046754,2.39297545721447,4.3567));
#73794=CARTESIAN_POINT('Ctrl Pts',(0.240435976311113,2.38172512702901,4.3567));
#73795=CARTESIAN_POINT('Ctrl Pts',(0.25712640745556,2.36898505359157,4.3567));
#73796=CARTESIAN_POINT('Ctrl Pts',(0.272712722894781,2.35495932065901,4.3567));
#73797=CARTESIAN_POINT('Ctrl Pts',(0.284847641215269,2.34403941311669,4.3567));
#73798=CARTESIAN_POINT('Ctrl Pts',(0.296313349003292,2.33233885512433,4.3567));
#73799=CARTESIAN_POINT('Ctrl Pts',(0.30703861953246,2.31993423667894,4.3567));
#73800=CARTESIAN_POINT('Ctrl Pts',(0.310476070462662,2.3159585544714,4.3567));
#73801=CARTESIAN_POINT('Ctrl Pts',(0.313837377253384,2.31191043772024,4.3567));
#73802=CARTESIAN_POINT('Ctrl Pts',(0.317119922049988,2.30779211050345,4.3567));
#73803=CARTESIAN_POINT('Ctrl Pts',(0.326850704545219,2.29558373289585,4.3567));
#73804=CARTESIAN_POINT('Ctrl Pts',(0.33583295276189,2.28283021741324,4.3567));
#73805=CARTESIAN_POINT('Ctrl Pts',(0.344012277935068,2.2696119465451,4.3567));
#73806=CARTESIAN_POINT('Ctrl Pts',(0.355355398230413,2.25128079655666,4.3567));
#73807=CARTESIAN_POINT('Ctrl Pts',(0.365158565020612,2.23205391983181,4.3567));
#73808=CARTESIAN_POINT('Ctrl Pts',(0.373259765356344,2.2120995657669,4.3567));
#73809=CARTESIAN_POINT('Ctrl Pts',(0.377716509485494,2.20112200112904,4.3567));
#73810=CARTESIAN_POINT('Ctrl Pts',(0.381657543398439,2.18992363295171,4.3567));
#73811=CARTESIAN_POINT('Ctrl Pts',(0.385050100177468,2.17852889782573,4.3567));
#73812=CARTESIAN_POINT('Ctrl Pts',(0.385401167965355,2.1773497504408,4.3567));
#73813=CARTESIAN_POINT('Ctrl Pts',(0.385746358064522,2.17616849861351,4.3567));
#73814=CARTESIAN_POINT('Ctrl Pts',(0.386085631082114,2.17498516834631,4.3567));
#73815=CARTESIAN_POINT('Origin',(-5.160062080289E-17,2.1,4.3567));
#73816=CARTESIAN_POINT('Ctrl Pts',(0.287740166859834,1.83187598694732,4.3567));
#73817=CARTESIAN_POINT('Ctrl Pts',(0.283540929289304,1.82807333637404,4.3567));
#73818=CARTESIAN_POINT('Ctrl Pts',(0.279255381327226,1.82437166421582,4.3567));
#73819=CARTESIAN_POINT('Ctrl Pts',(0.274884385304385,1.82077515375635,4.3567));
#73820=CARTESIAN_POINT('Ctrl Pts',(0.25810235391389,1.80696668742242,4.3567));
#73821=CARTESIAN_POINT('Ctrl Pts',(0.240062114400838,1.79470455623045,4.3567));
#73822=CARTESIAN_POINT('Ctrl Pts',(0.221014146357085,1.78403910870001,4.3567));
#73823=CARTESIAN_POINT('Ctrl Pts',(0.218046748141756,1.78237758606963,4.3567));
#73824=CARTESIAN_POINT('Ctrl Pts',(0.215054865633032,1.78075491256672,4.3567));
#73825=CARTESIAN_POINT('Ctrl Pts',(0.212039424147889,1.77917138918029,4.3567));
#73826=CARTESIAN_POINT('Ctrl Pts',(0.206236204436223,1.77612389707164,4.3567));
#73827=CARTESIAN_POINT('Ctrl Pts',(0.200354322111735,1.77322592154459,4.3567));
#73828=CARTESIAN_POINT('Ctrl Pts',(0.194402554160535,1.77047920260614,4.3567));
#73829=CARTESIAN_POINT('Ctrl Pts',(0.178891787748209,1.76332104116505,4.3567));
#73830=CARTESIAN_POINT('Ctrl Pts',(0.16290270656968,1.757186694163,4.3567));
#73831=CARTESIAN_POINT('Ctrl Pts',(0.14655689918141,1.75210485469583,4.3567));
#73832=CARTESIAN_POINT('Ctrl Pts',(0.139384822531743,1.74987508767887,4.3567));
#73833=CARTESIAN_POINT('Ctrl Pts',(0.132143750868839,1.74784812676099,4.3567));
#73834=CARTESIAN_POINT('Ctrl Pts',(0.124844069854122,1.7460277175469,4.3567));
#73835=CARTESIAN_POINT('Ctrl Pts',(0.11859715027019,1.74446984810748,4.3567));
#73836=CARTESIAN_POINT('Ctrl Pts',(0.112309084212408,1.74306396104996,4.3567));
#73837=CARTESIAN_POINT('Ctrl Pts',(0.106001682669741,1.74181480813219,4.3567));
#73838=CARTESIAN_POINT('Ctrl Pts',(0.0854450059383791,1.73774364942367,
4.3567));
#73839=CARTESIAN_POINT('Ctrl Pts',(0.0646473420272781,1.73532368510841,
4.3567));
#73840=CARTESIAN_POINT('Ctrl Pts',(0.0438340188223849,1.73461140981212,
4.3567));
#73841=CARTESIAN_POINT('Ctrl Pts',(0.0315896664796848,1.73419238255698,
4.3567));
#73842=CARTESIAN_POINT('Ctrl Pts',(0.0193398602704868,1.73436532131983,
4.3567));
#73843=CARTESIAN_POINT('Ctrl Pts',(0.00713247518961179,1.73515005238391,
4.3567));
#73844=CARTESIAN_POINT('Ctrl Pts',(-0.000437632244075232,1.73563668391247,
4.3567));
#73845=CARTESIAN_POINT('Ctrl Pts',(-0.00799138412230426,1.73635870589722,
4.3567));
#73846=CARTESIAN_POINT('Ctrl Pts',(-0.0155167357365803,1.73732206252591,
4.3567));
#73847=CARTESIAN_POINT('Ctrl Pts',(-0.0218591581541978,1.73813398667128,
4.3567));
#73848=CARTESIAN_POINT('Ctrl Pts',(-0.028183730479901,1.73911809273902,
4.3567));
#73849=CARTESIAN_POINT('Ctrl Pts',(-0.0344595927017996,1.74027323764255,
4.3567));
#73850=CARTESIAN_POINT('Ctrl Pts',(-0.0494189029188666,1.74302667140936,
4.3567));
#73851=CARTESIAN_POINT('Ctrl Pts',(-0.0641299531612682,1.74675330792951,
4.3567));
#73852=CARTESIAN_POINT('Ctrl Pts',(-0.0785012988446161,1.75148487175215,
4.3567));
#73853=CARTESIAN_POINT('Ctrl Pts',(-0.0986706061389512,1.75812533304398,
4.3567));
#73854=CARTESIAN_POINT('Ctrl Pts',(-0.118172845707065,1.76674387676704,
4.3567));
#73855=CARTESIAN_POINT('Ctrl Pts',(-0.136807949554667,1.77715217457513,
4.3567));
#73856=CARTESIAN_POINT('Ctrl Pts',(-0.142094148121254,1.78010468449424,
4.3567));
#73857=CARTESIAN_POINT('Ctrl Pts',(-0.147312413818575,1.78320284198279,
4.3567));
#73858=CARTESIAN_POINT('Ctrl Pts',(-0.152450181179759,1.78643826777209,
4.3567));
#73859=CARTESIAN_POINT('Ctrl Pts',(-0.158904634512563,1.79050285522823,
4.3567));
#73860=CARTESIAN_POINT('Ctrl Pts',(-0.165222236643709,1.79477770660458,
4.3567));
#73861=CARTESIAN_POINT('Ctrl Pts',(-0.171390503137907,1.79924948335615,
4.3567));
#73862=CARTESIAN_POINT('Ctrl Pts',(-0.187020189413487,1.81058045742919,
4.3567));
#73863=CARTESIAN_POINT('Ctrl Pts',(-0.201704919669262,1.82318105360677,
4.3567));
#73864=CARTESIAN_POINT('Ctrl Pts',(-0.215292904901525,1.83690543855032,
4.3567));
#73865=CARTESIAN_POINT('Ctrl Pts',(-0.222370765829106,1.8440543488771,4.3567));
#73866=CARTESIAN_POINT('Ctrl Pts',(-0.229150448230971,1.85150865969543,
4.3567));
#73867=CARTESIAN_POINT('Ctrl Pts',(-0.235605904128297,1.85925002016915,
4.3567));
#73868=CARTESIAN_POINT('Ctrl Pts',(-0.239875651825072,1.8643702868983,4.3567));
#73869=CARTESIAN_POINT('Ctrl Pts',(-0.244004693787793,1.86961778453864,
4.3567));
#73870=CARTESIAN_POINT('Ctrl Pts',(-0.247980890826324,1.874982371717,4.3567));
#73871=CARTESIAN_POINT('Ctrl Pts',(-0.251720955269355,1.88002837460943,
4.3567));
#73872=CARTESIAN_POINT('Ctrl Pts',(-0.255320614079644,1.88517104298149,
4.3567));
#73873=CARTESIAN_POINT('Ctrl Pts',(-0.258770422630349,1.89039903119355,
4.3567));
#73874=CARTESIAN_POINT('Ctrl Pts',(-0.269038181960046,1.90595923517325,
4.3567));
#73875=CARTESIAN_POINT('Ctrl Pts',(-0.277995587721695,1.92229271891481,
4.3567));
#73876=CARTESIAN_POINT('Ctrl Pts',(-0.285483839243767,1.93927368372052,
4.3567));
#73877=CARTESIAN_POINT('Ctrl Pts',(-0.292051816918351,1.95416776111737,
4.3567));
#73878=CARTESIAN_POINT('Ctrl Pts',(-0.297489248769509,1.96956071430832,
4.3567));
#73879=CARTESIAN_POINT('Ctrl Pts',(-0.301655992406196,1.98537103162613,
4.3567));
#73880=CARTESIAN_POINT('Ctrl Pts',(-0.301998194302805,1.98666948457738,
4.3567));
#73881=CARTESIAN_POINT('Ctrl Pts',(-0.302331806399809,1.98797075138032,
4.3567));
#73882=CARTESIAN_POINT('Ctrl Pts',(-0.302656740537857,1.98927478592477,
4.3567));
#73883=CARTESIAN_POINT('Ctrl Pts',(-0.369736275429134,1.96501449663477,
4.3155034837597));
#73884=CARTESIAN_POINT('Ctrl Pts',(-0.324771331358241,1.84183163773061,
4.32213136767731));
#73885=CARTESIAN_POINT('Ctrl Pts',(-0.102837691495962,1.64619446151566,
4.33538269943585));
#73886=CARTESIAN_POINT('Ctrl Pts',(0.326776737212504,1.76816965157351,4.35525747903531));
#73887=CARTESIAN_POINT('Ctrl Pts',(0.45547744888119,2.19504797546089,4.37512782255811));
#73888=CARTESIAN_POINT('Ctrl Pts',(0.166857071268261,2.53446779707742,4.3949981660809));
#73889=CARTESIAN_POINT('Ctrl Pts',(-0.275097988964059,2.4754595193049,4.41486850960369));
#73890=CARTESIAN_POINT('Ctrl Pts',(-0.464550239979861,2.07194719672028,
4.43473885312647));
#73891=CARTESIAN_POINT('Ctrl Pts',(-0.227912439379459,1.69420638760595,
4.45460919664927));
#73892=CARTESIAN_POINT('Ctrl Pts',(0.217841145994397,1.68870682220133,4.47447954017205));
#73893=CARTESIAN_POINT('Ctrl Pts',(0.46373584719812,2.06052269932018,4.49434988369485));
#73894=CARTESIAN_POINT('Ctrl Pts',(0.284226056250109,2.46854846190176,4.51422022721762));
#73895=CARTESIAN_POINT('Ctrl Pts',(-0.156027648019584,2.53848386517764,
4.53409057074043));
#73896=CARTESIAN_POINT('Ctrl Pts',(-0.453144526100725,2.20616862417218,
4.5539609142632));
#73897=CARTESIAN_POINT('Ctrl Pts',(-0.334564393695026,1.7764588469168,4.57383125778601));
#73898=CARTESIAN_POINT('Ctrl Pts',(0.0909337511562546,1.6435536561162,4.59370160130879));
#73899=CARTESIAN_POINT('Ctrl Pts',(0.433012180793506,1.92937604116777,4.61357194483159));
#73900=CARTESIAN_POINT('Ctrl Pts',(0.377861080133257,2.37172257889418,4.63344228835436));
#73901=CARTESIAN_POINT('Ctrl Pts',(-0.0239262223333663,2.56480069472104,
4.65331263187717));
#73902=CARTESIAN_POINT('Ctrl Pts',(-0.403764420146204,2.33148742275733,
4.67318297539994));
#73903=CARTESIAN_POINT('Ctrl Pts',(-0.413203757517612,1.88581596874811,
4.69305331892275));
#73904=CARTESIAN_POINT('Ctrl Pts',(-0.0435848857095753,1.63662919753327,
4.71292366244552));
#73905=CARTESIAN_POINT('Ctrl Pts',(0.366017177781486,1.81252205916294,4.73279400596832));
#73906=CARTESIAN_POINT('Ctrl Pts',(0.439848313244426,2.25213679293958,4.7526643494911));
#73907=CARTESIAN_POINT('Ctrl Pts',(0.110178499248734,2.55218673177814,4.7725346930139));
#73908=CARTESIAN_POINT('Ctrl Pts',(-0.320565087322196,2.43741690334024,
4.79240503653668));
#73909=CARTESIAN_POINT('Ctrl Pts',(-0.45723384780948,2.01311300152881,4.81227538005947));
#73910=CARTESIAN_POINT('Ctrl Pts',(-0.174452799419451,1.66851609207379,
4.83214572358226));
#73911=CARTESIAN_POINT('Ctrl Pts',(0.268364942688647,1.71974692698616,4.85201606710506));
#73912=CARTESIAN_POINT('Ctrl Pts',(0.46499438454321,2.11980818956847,4.87188641062784));
#73913=CARTESIAN_POINT('Ctrl Pts',(0.235054781809442,2.50169813488339,4.89175675415064));
#73914=CARTESIAN_POINT('Ctrl Pts',(-0.210515583395179,2.51508472769526,
4.91162709767341));
#73915=CARTESIAN_POINT('Ctrl Pts',(-0.462966559954061,2.14768759153516,
4.93149744119622));
#73916=CARTESIAN_POINT('Ctrl Pts',(-0.290708744955435,1.73654358221807,
4.951367784719));
#73917=CARTESIAN_POINT('Ctrl Pts',(0.148234767115052,1.65882135609411,4.97123812824179));
#73918=CARTESIAN_POINT('Ctrl Pts',(0.45119306070023,1.98582047470415,4.99110847176458));
#73919=CARTESIAN_POINT('Ctrl Pts',(0.340243145480813,2.41756376363479,5.01097881528736));
#73920=CARTESIAN_POINT('Ctrl Pts',(-0.0828335357952513,2.55798553183285,
5.03084915881016));
#73921=CARTESIAN_POINT('Ctrl Pts',(-0.429921724746993,2.27826792367447,
5.05071950233295));
#73922=CARTESIAN_POINT('Ctrl Pts',(-0.382615259800999,1.83501376453104,
5.07058984585574));
#73923=CARTESIAN_POINT('Ctrl Pts',(0.0156886176482768,1.63484840181196,
5.09046018937852));
#73924=CARTESIAN_POINT('Ctrl Pts',(0.399600324217718,1.86139630575847,5.11033053290132));
#73925=CARTESIAN_POINT('Ctrl Pts',(0.416933133989187,2.30683061621182,5.13020087642411));
#73926=CARTESIAN_POINT('Ctrl Pts',(0.0517865536463587,2.56252599373661,
5.1500712199469));
#73927=CARTESIAN_POINT('Ctrl Pts',(-0.360867139564347,2.39391673923622,
5.16994156346968));
#73928=CARTESIAN_POINT('Ctrl Pts',(-0.442474359849625,1.95567888963748,
5.18981190699248));
#73929=CARTESIAN_POINT('Ctrl Pts',(-0.118171592417568,1.64983601125134,
5.20968225051526));
#73930=CARTESIAN_POINT('Ctrl Pts',(0.314537523448001,1.75695730824896,5.22955259403806));
#73931=CARTESIAN_POINT('Ctrl Pts',(0.458701281967192,2.17877357388274,5.24942293756084));
#73932=CARTESIAN_POINT('Ctrl Pts',(0.182069060822143,2.52832580953282,5.26929328108364));
#73933=CARTESIAN_POINT('Ctrl Pts',(-0.261586737162791,2.48494742623004,
5.28916362460641));
#73934=CARTESIAN_POINT('Ctrl Pts',(-0.465272315619407,2.08843218522106,
5.30903396812922));
#73935=CARTESIAN_POINT('Ctrl Pts',(-0.242133885601332,1.70252883945599,
5.328904311652));
#73936=CARTESIAN_POINT('Ctrl Pts',(0.203129420904025,1.68125117267771,5.34877465517479));
#73937=CARTESIAN_POINT('Ctrl Pts',(0.462049137303498,2.04411854746253,5.36864499869758));
#73938=CARTESIAN_POINT('Ctrl Pts',(0.297101672537019,2.45824954737767,5.38851534222037));
#73939=CARTESIAN_POINT('Ctrl Pts',(-0.140396130041771,2.54373535884567,
5.40838568574316));
#73940=CARTESIAN_POINT('Ctrl Pts',(-0.449099596514432,2.22215438768698,
5.42825602926594));
#73941=CARTESIAN_POINT('Ctrl Pts',(-0.345815322574325,1.78851339564369,
5.44812637278874));
#73942=CARTESIAN_POINT('Ctrl Pts',(0.0747074313227155,1.64061895802529,
5.46799671631152));
#73943=CARTESIAN_POINT('Ctrl Pts',(0.426696287479547,1.91414408733705,5.48786705983432));
#73944=CARTESIAN_POINT('Ctrl Pts',(0.387249389327999,2.35816671451931,5.5077374033571));
#73945=CARTESIAN_POINT('Ctrl Pts',(-0.00744610428814212,2.5653565273546,
5.5276077468799));
#73946=CARTESIAN_POINT('Ctrl Pts',(-0.395310810915475,2.34564507891255,
5.54747809040268));
#73947=CARTESIAN_POINT('Ctrl Pts',(-0.420531665235156,1.90058771212598,
5.56734843392548));
#73948=CARTESIAN_POINT('Ctrl Pts',(-0.0599719669181471,1.63846397193223,
5.58721877744826));
#73949=CARTESIAN_POINT('Ctrl Pts',(0.355603846600209,1.79973670503416,5.60708912097106));
#73950=CARTESIAN_POINT('Ctrl Pts',(0.4449615419551,2.23646013411083,5.62695946449384));
#73951=CARTESIAN_POINT('Ctrl Pts',(0.126127598610152,2.54799996751054,5.64682980801663));
#73952=CARTESIAN_POINT('Ctrl Pts',(-0.30841124573757,2.44856082040759,5.66670015153942));
#73953=CARTESIAN_POINT('Ctrl Pts',(-0.460024758520828,2.02936457285146,
5.68657049506221));
#73954=CARTESIAN_POINT('Ctrl Pts',(-0.189628182076955,1.67496671355905,
5.706440838585));
#73955=CARTESIAN_POINT('Ctrl Pts',(0.254726435876664,1.71047903151925,5.72631118210778));
#73956=CARTESIAN_POINT('Ctrl Pts',(0.465404226786298,2.10332380956912,5.74618152563059));
#73957=CARTESIAN_POINT('Ctrl Pts',(0.249136998683705,2.49311944483512,5.76605186915336));
#73958=CARTESIAN_POINT('Ctrl Pts',(-0.195679508771493,2.52228150784466,
5.78592221267616));
#73959=CARTESIAN_POINT('Ctrl Pts',(-0.46098670628845,2.16405777584283,5.80579255619895));
#73960=CARTESIAN_POINT('Ctrl Pts',(-0.303401358458842,1.74706975518393,
5.82566289972174));
#73961=CARTESIAN_POINT('Ctrl Pts',(0.132513431391554,1.65384718702956,5.84553324324452));
#73962=CARTESIAN_POINT('Ctrl Pts',(0.446865188014881,1.96990908655471,5.86540358676732));
#73963=CARTESIAN_POINT('Ctrl Pts',(0.351278969836519,2.40531168888727,5.8852739302901));
#73964=CARTESIAN_POINT('Ctrl Pts',(-0.066557880853422,2.56063238109896,
5.9051442738129));
#73965=CARTESIAN_POINT('Ctrl Pts',(-0.423336936897625,2.29338557308844,
5.92501461733567));
#73966=CARTESIAN_POINT('Ctrl Pts',(-0.391761985458073,1.84873382883771,
5.94488496085848));
#73967=CARTESIAN_POINT('Ctrl Pts',(-0.000798745939078063,1.63458458982805,
5.96475530438125));
#73968=CARTESIAN_POINT('Ctrl Pts',(0.390897234239583,1.84739062906445,5.98462564790406));
#73969=CARTESIAN_POINT('Ctrl Pts',(0.423998217856513,2.29193137647374,6.00449599142684));
#73970=CARTESIAN_POINT('Ctrl Pts',(0.068138558735181,2.56040121506583,6.02436633494963));
#73971=CARTESIAN_POINT('Ctrl Pts',(-0.350228951798542,2.40651561680067,
6.04423667847242));
#73972=CARTESIAN_POINT('Ctrl Pts',(-0.44730907842348,1.97144366845409,6.06410702199521));
#73973=CARTESIAN_POINT('Ctrl Pts',(-0.134044021227067,1.65430465293669,
6.083977365518));
#73974=CARTESIAN_POINT('Ctrl Pts',(0.302188176999508,1.74603044240738,6.10384770904079));
#73975=CARTESIAN_POINT('Ctrl Pts',(0.461203862034495,2.16247511236542,6.12371805256357));
#73976=CARTESIAN_POINT('Ctrl Pts',(0.197127790889,2.52160737194673,6.14358839608637));
#73977=CARTESIAN_POINT('Ctrl Pts',(-0.24778619187174,2.49397226442772,6.16345873960915));
#73978=CARTESIAN_POINT('Ctrl Pts',(-0.465390076634112,2.10492123877693,
6.18332908313195));
#73979=CARTESIAN_POINT('Ctrl Pts',(-0.256061923222516,1.71135564651446,
6.20319942665474));
#73980=CARTESIAN_POINT('Ctrl Pts',(0.188168185062698,1.67431833942391,6.22306977017752));
#73981=CARTESIAN_POINT('Ctrl Pts',(0.459779600338103,2.0277860045868,6.24294011370032));
#73982=CARTESIAN_POINT('Ctrl Pts',(0.309605825643754,2.44750017949355,6.2628104572231));
#73983=CARTESIAN_POINT('Ctrl Pts',(-0.124589145051608,2.54843024759255,
6.2826808007459));
#73984=CARTESIAN_POINT('Ctrl Pts',(-0.444490536442624,2.23798661179097,
6.30255114426868));
#73985=CARTESIAN_POINT('Ctrl Pts',(-0.356632372569888,1.80095904485208,
6.32242148779147));
#73986=CARTESIAN_POINT('Ctrl Pts',(0.0583874420223328,1.63826084351152,
6.34229183131426));
#73987=CARTESIAN_POINT('Ctrl Pts',(0.419844727291524,1.89914545813921,6.36216217483705));
#73988=CARTESIAN_POINT('Ctrl Pts',(0.396151631969156,2.34428677104743,6.38203251835984));
#73989=CARTESIAN_POINT('Ctrl Pts',(0.00904334548983111,2.56532822816046,
6.40190286188263));
#73990=CARTESIAN_POINT('Ctrl Pts',(-0.386360979336095,2.35949438465419,
6.42177320540542));
#73991=CARTESIAN_POINT('Ctrl Pts',(-0.427331703918903,1.91560977019817,
6.44164354892821));
#73992=CARTESIAN_POINT('Ctrl Pts',(-0.0762837661143578,1.64087808912227,
6.46151389245099));
#73993=CARTESIAN_POINT('Ctrl Pts',(0.344744142003126,1.78732825747258,6.48138423597379));
#73994=CARTESIAN_POINT('Ctrl Pts',(0.449516232509681,2.22061218317777,6.50125457949658));
#73995=CARTESIAN_POINT('Ctrl Pts',(0.141918375797697,2.54325085068338,6.52112492301936));
#73996=CARTESIAN_POINT('Ctrl Pts',(-0.295870270266432,2.45926720584139,
6.54099526654216));
#73997=CARTESIAN_POINT('Ctrl Pts',(-0.46223822246123,2.04570480945345,6.56086561006495));
#73998=CARTESIAN_POINT('Ctrl Pts',(-0.204565533599482,1.68195085876925,
6.58073595358773));
#73999=CARTESIAN_POINT('Ctrl Pts',(0.240768183257146,1.70170008291281,6.60060629711053));
#74000=CARTESIAN_POINT('Ctrl Pts',(0.465229869603695,2.08683525734651,6.62047664063331));
#74001=CARTESIAN_POINT('Ctrl Pts',(0.262906485916467,2.4840472909469,6.6403469841561));
#74002=CARTESIAN_POINT('Ctrl Pts',(-0.180597807113009,2.52894821842103,
6.66021732767889));
#74003=CARTESIAN_POINT('Ctrl Pts',(-0.458428198287625,2.18034755152067,
6.68008767120168));
#74004=CARTESIAN_POINT('Ctrl Pts',(-0.315713126897015,1.75803894443152,
6.69995801472447));
#74005=CARTESIAN_POINT('Ctrl Pts',(0.116625757960482,1.6494330520325,6.71982835824726));
#74006=CARTESIAN_POINT('Ctrl Pts',(0.441976387052489,1.95416099524259,6.73969870177005));
#74007=CARTESIAN_POINT('Ctrl Pts',(0.361873850675656,2.39267637112992,6.75956904529284));
#74008=CARTESIAN_POINT('Ctrl Pts',(-0.050198679019885,2.56270102079557,
6.77943938881563));
#74009=CARTESIAN_POINT('Ctrl Pts',(-0.416220754647733,2.30826047493722,
6.79930973233842));
#74010=CARTESIAN_POINT('Ctrl Pts',(-0.40041695122537,1.86276929542746,6.8191800758612));
#74011=CARTESIAN_POINT('Ctrl Pts',(-0.017285106899255,1.63490499131889,
6.839050419384));
#74012=CARTESIAN_POINT('Ctrl Pts',(0.381703469852107,1.83370204070729,6.85892076290678));
#74013=CARTESIAN_POINT('Ctrl Pts',(0.430531077249251,2.27679121455323,6.87879110642958));
#74014=CARTESIAN_POINT('Ctrl Pts',(0.0844050327837897,2.55769851699713,
6.89866144995237));
#74015=CARTESIAN_POINT('Ctrl Pts',(-0.339151138553184,2.4187297401227,6.91853179347515));
#74016=CARTESIAN_POINT('Ctrl Pts',(-0.451582311525894,1.98736981782162,
6.93840213699795));
#74017=CARTESIAN_POINT('Ctrl Pts',(-0.149748191053947,1.65933275445448,
6.95827248052074));
#74018=CARTESIAN_POINT('Ctrl Pts',(0.28945950833466,1.73554789744705,6.97814282404352));
#74019=CARTESIAN_POINT('Ctrl Pts',(0.463127515179909,2.14609822885846,6.99801316756631));
#74020=CARTESIAN_POINT('Ctrl Pts',(0.211939075965495,2.51435971099939,7.0178835110891));
#74021=CARTESIAN_POINT('Ctrl Pts',(-0.233674612547471,2.50250256827925,
7.0377538546119));
#74022=CARTESIAN_POINT('Ctrl Pts',(-0.46492365597403,2.12140411493955,7.05762419813467));
#74023=CARTESIAN_POINT('Ctrl Pts',(-0.269668538684808,1.72067030004994,
7.07749454165748));
#74024=CARTESIAN_POINT('Ctrl Pts',(0.172970750791257,1.66791984378901,7.09736488518025));
#74025=CARTESIAN_POINT('Ctrl Pts',(0.45693292425771,2.01154410845002,7.11723522870305));
#74026=CARTESIAN_POINT('Ctrl Pts',(0.321721345518213,2.4363146114259,7.13710557222584));
#74027=CARTESIAN_POINT('Ctrl Pts',(-0.108625769328017,2.5525622435185,7.15697591574863));
#74028=CARTESIAN_POINT('Ctrl Pts',(-0.439323528878937,2.25364562796892,
7.17684625927142));
#74029=CARTESIAN_POINT('Ctrl Pts',(-0.367001759181217,1.81378006572131,
7.19671660279421));
#74030=CARTESIAN_POINT('Ctrl Pts',(0.0419941617873573,1.63648232784889,
7.21658694631699));
#74031=CARTESIAN_POINT('Ctrl Pts',(0.412466156304921,1.88439895194213,7.2364572898398));
#74032=CARTESIAN_POINT('Ctrl Pts',(0.404556604609395,2.33010018619619,7.25632763336257));
#74033=CARTESIAN_POINT('Ctrl Pts',(0.0255214435931988,2.56471582492693,
7.27619797688537));
#74034=CARTESIAN_POINT('Ctrl Pts',(-0.376926167488953,2.37301795963397,
7.29606832040816));
#74035=CARTESIAN_POINT('Ctrl Pts',(-0.433595333764087,1.93086328441579,
7.31593866393094));
#74036=CARTESIAN_POINT('Ctrl Pts',(-0.0924998099851176,1.64386851986152,
7.33580900745374));
#74037=CARTESIAN_POINT('Ctrl Pts',(0.333451696743183,1.77531229164058,7.35567935097652));
#74038=CARTESIAN_POINT('Ctrl Pts',(0.453506667058955,2.20461283359934,7.37554969449932));
#74039=CARTESIAN_POINT('Ctrl Pts',(0.157531009705832,2.53794534248199,7.3954200380221));
#74040=CARTESIAN_POINT('Ctrl Pts',(-0.282957903141967,2.46952262051206,
7.41529038154489));
#74041=CARTESIAN_POINT('Ctrl Pts',(-0.463871461097088,2.06211320018452,
7.43516072506768));
#74042=CARTESIAN_POINT('Ctrl Pts',(-0.219246103892619,1.68945976086563,
7.45503106859047));
#74043=CARTESIAN_POINT('Ctrl Pts',(0.226507705971502,1.69342110094579,7.47490141211325));
#74044=CARTESIAN_POINT('Ctrl Pts',(0.464471531846451,2.07036323018922,7.49477175563605));
#74045=CARTESIAN_POINT('Ctrl Pts',(0.276345959341524,2.47449306105215,7.51464209915884));
#74046=CARTESIAN_POINT('Ctrl Pts',(-0.165289409754046,2.53507649102631,
7.53451244268163));
#74047=CARTESIAN_POINT('Ctrl Pts',(-0.455294247521488,2.19653647079961,
7.55438278620442));
#74048=CARTESIAN_POINT('Ctrl Pts',(-0.327628595902773,1.76943738086804,
7.5742531297272));
#74049=CARTESIAN_POINT('Ctrl Pts',(0.10059168985099,1.64558449195309,7.59412347325));
#74050=CARTESIAN_POINT('Ctrl Pts',(0.436532794488454,1.93859596858596,7.61399381677278));
#74051=CARTESIAN_POINT('Ctrl Pts',(0.372014488756375,2.37967367086649,7.63386416029558));
#74052=CARTESIAN_POINT('Ctrl Pts',(-0.0337764652102615,2.56418885425923,
7.65373450381837));
#74053=CARTESIAN_POINT('Ctrl Pts',(-0.408582110597001,2.32287395747531,
7.67360484734115));
#74054=CARTESIAN_POINT('Ctrl Pts',(-0.408569292942596,1.87710254625726,
7.69347519086395));
#74055=CARTESIAN_POINT('Ctrl Pts',(-0.0337497706999876,1.63580920409997,
7.71334553438673));
#74056=CARTESIAN_POINT('Ctrl Pts',(0.372030571543465,1.82034772331045,7.73321587790953));
#74057=CARTESIAN_POINT('Ctrl Pts',(0.436523511784681,2.26142913516393,7.75308622143231));
#74058=CARTESIAN_POINT('Ctrl Pts',(0.100565557273339,2.55442129209678,7.77295656495511));
#74059=CARTESIAN_POINT('Ctrl Pts',(-0.327647605271937,2.43054377740349,
7.79282690847788));
#74060=CARTESIAN_POINT('Ctrl Pts',(-0.455288695173849,2.00343734641438,
7.81269725200069));
#74061=CARTESIAN_POINT('Ctrl Pts',(-0.165264389212678,1.66491400427184,
7.83256759552346));
#74062=CARTESIAN_POINT('Ctrl Pts',(0.276367495136158,1.72552283160015,7.85243793904627));
#74063=CARTESIAN_POINT('Ctrl Pts',(0.464469826734602,2.12966348047235,7.87230828256904));
#74064=CARTESIAN_POINT('Ctrl Pts',(0.226484324161168,2.50659192432938,7.89217862609184));
#74065=CARTESIAN_POINT('Ctrl Pts',(-0.219269712773607,2.51052763010641,
7.91204896961463));
#74066=CARTESIAN_POINT('Ctrl Pts',(-0.463873639114477,2.13786012355098,
7.93191931313741));
#74067=CARTESIAN_POINT('Ctrl Pts',(-0.282936652261319,1.73046110782793,
7.95178965666021));
#74068=CARTESIAN_POINT('Ctrl Pts',(0.157556194694575,1.66206371749538,7.97166000018299));
#74069=CARTESIAN_POINT('Ctrl Pts',(0.453512682357245,1.99541324671956,7.9915303437058));
#74070=CARTESIAN_POINT('Ctrl Pts',(0.333433024133746,2.4247068838778,8.01140068722857));
#74071=CARTESIAN_POINT('Ctrl Pts',(-0.0925260409251638,2.55612615992871,
8.03127103075137));
#74072=CARTESIAN_POINT('Ctrl Pts',(-0.433605059718277,2.2691117802145,8.05114137427415));
#74073=CARTESIAN_POINT('Ctrl Pts',(-0.376910466218381,1.82696036464343,
8.07101171779694));
#74074=CARTESIAN_POINT('Ctrl Pts',(0.0255481683103127,1.63528564352218,
8.09088206131974));
#74075=CARTESIAN_POINT('Ctrl Pts',(0.404569836483345,1.8699230793225,8.11075240484252));
#74076=CARTESIAN_POINT('Ctrl Pts',(0.41245375689271,2.31562476770003,8.13062274836531));
#74077=CARTESIAN_POINT('Ctrl Pts',(0.0419675058616662,2.56352008637421,
8.1504930918881));
#74078=CARTESIAN_POINT('Ctrl Pts',(-0.367018218437449,2.3861988283617,8.17036343541089));
#74079=CARTESIAN_POINT('Ctrl Pts',(-0.439314692338837,1.94632910777952,
8.19023377893367));
#74080=CARTESIAN_POINT('Ctrl Pts',(-0.108599743314144,1.64743151040677,
8.21010412245648));
#74081=CARTESIAN_POINT('Ctrl Pts',(0.321740685681253,1.76370389059942,8.22997446597924));
#74082=CARTESIAN_POINT('Ctrl Pts',(0.456927836603256,2.18848216858596,8.24984480950206));
#74083=CARTESIAN_POINT('Ctrl Pts',(0.172945902549646,2.5320901026544,8.26971515302483));
#74084=CARTESIAN_POINT('Ctrl Pts',(-0.269690352634677,2.47931419129317,
8.28958549654763));
#74085=CARTESIAN_POINT('Ctrl Pts',(-0.464922424302857,2.07856914838463,
8.30945584007041));
#74086=CARTESIAN_POINT('Ctrl Pts',(-0.233651465145874,1.6974839942862,8.32932618359321));
#74087=CARTESIAN_POINT('Ctrl Pts',(0.211962904507778,1.6856524778242,8.349196527116));
#74088=CARTESIAN_POINT('Ctrl Pts',(0.463130165419301,2.05392840463697,8.36906687063877));
#74089=CARTESIAN_POINT('Ctrl Pts',(0.289438549037316,2.46446874811399,8.38893721416159));
#74090=CARTESIAN_POINT('Ctrl Pts',(-0.149773532586065,2.54065863313601,
8.40880755768436));
#74091=CARTESIAN_POINT('Ctrl Pts',(-0.451588787887004,2.21260421251156,
8.42867790120716));
#74092=CARTESIAN_POINT('Ctrl Pts',(-0.339132808563647,1.78125075658703,
8.44854824472993));
#74093=CARTESIAN_POINT('Ctrl Pts',(0.0844313538539795,1.64230633770284,
8.46841858825274));
#74094=CARTESIAN_POINT('Ctrl Pts',(0.430541243401479,1.92323354461066,8.48828893177552));
#74095=CARTESIAN_POINT('Ctrl Pts',(0.38168815502571,2.36631990975832,8.50815927529831));
#74096=CARTESIAN_POINT('Ctrl Pts',(-0.0173118534359932,2.56509401388452,
8.52802961882109));
#74097=CARTESIAN_POINT('Ctrl Pts',(-0.400430593166196,2.3372076771042,8.5478999623439));
#74098=CARTESIAN_POINT('Ctrl Pts',(-0.416208777369125,1.89171558948999,
8.56777030586666));
#74099=CARTESIAN_POINT('Ctrl Pts',(-0.0501720700444095,1.63729609315669,
8.58764064938948));
#74100=CARTESIAN_POINT('Ctrl Pts',(0.361890681235488,1.8073444399033,8.60751099291225));
#74101=CARTESIAN_POINT('Ctrl Pts',(0.441967999449303,2.24586442158177,8.62738133643504));
#74102=CARTESIAN_POINT('Ctrl Pts',(0.116599846678335,2.55057365410685,8.64725167995784));
#74103=CARTESIAN_POINT('Ctrl Pts',(-0.315732791784264,2.44194289905293,
8.66712202348063));
#74104=CARTESIAN_POINT('Ctrl Pts',(-0.458423576923048,2.01962608544011,
8.68699236700342));
#74105=CARTESIAN_POINT('Ctrl Pts',(-0.180573138969472,1.67104139651556,
8.7068627105262));
#74106=CARTESIAN_POINT('Ctrl Pts',(0.262928571175537,1.71596782884738,8.726733054049));
#74107=CARTESIAN_POINT('Ctrl Pts',(0.465229111759736,2.11319149695258,8.74660339757178));
#74108=CARTESIAN_POINT('Ctrl Pts',(0.240745277528821,2.49831376246394,8.76647374109457));
#74109=CARTESIAN_POINT('Ctrl Pts',(-0.20458957432477,2.51803737643686,8.78634408461736));
#74110=CARTESIAN_POINT('Ctrl Pts',(-0.462241344090878,2.15426860817877,
8.80621442814016));
#74111=CARTESIAN_POINT('Ctrl Pts',(-0.29584960913021,1.74071577992054,8.82608477166294));
#74112=CARTESIAN_POINT('Ctrl Pts',(0.141943865920065,1.65675731145537,8.84595511518573));
#74113=CARTESIAN_POINT('Ctrl Pts',(0.449523167901091,1.9794136676867,8.86582545870853));
#74114=CARTESIAN_POINT('Ctrl Pts',(0.34472616038612,2.41269156746872,8.8856958022313));
#74115=CARTESIAN_POINT('Ctrl Pts',(-0.076310169054144,2.55911752321113,
8.9055661457541));
#74116=CARTESIAN_POINT('Ctrl Pts',(-0.427342307078658,2.28436565461413,
8.92543648927688));
#74117=CARTESIAN_POINT('Ctrl Pts',(-0.386346055760231,1.84048339702609,
8.94530683279968));
#74118=CARTESIAN_POINT('Ctrl Pts',(0.00907010545211835,1.6346722926714,
8.96517717632246));
#74119=CARTESIAN_POINT('Ctrl Pts',(0.396165679695509,1.85573601114368,8.98504751984527));
#74120=CARTESIAN_POINT('Ctrl Pts',(0.41983317590544,2.30087868585233,9.00491786336803));
#74121=CARTESIAN_POINT('Ctrl Pts',(0.0583608883479577,2.56174251345511,
9.02478820689085));
#74122=CARTESIAN_POINT('Ctrl Pts',(-0.356649569151262,2.39902044552977,
9.04465855041361));
#74123=CARTESIAN_POINT('Ctrl Pts',(-0.444482600408699,1.96198782678863,
9.06452889393643));
#74124=CARTESIAN_POINT('Ctrl Pts',(-0.124563356633115,1.65156258830814,
9.08439923745919));
#74125=CARTESIAN_POINT('Ctrl Pts',(0.309625809083618,1.75251762581403,9.10426958098201));
#74126=CARTESIAN_POINT('Ctrl Pts',(0.459775446713771,2.17224043618195,9.12413992450477));
#74127=CARTESIAN_POINT('Ctrl Pts',(0.18814370475902,2.52569248100026,9.14401026802759));
#74128=CARTESIAN_POINT('Ctrl Pts',(-0.256084272859606,2.48862962729902,
9.16388061155035));
#74129=CARTESIAN_POINT('Ctrl Pts',(-0.465389792855207,2.0950519976972,9.18375095507316));
#74130=CARTESIAN_POINT('Ctrl Pts',(-0.247763535005359,1.70601348659852,
9.20362129859593));
#74131=CARTESIAN_POINT('Ctrl Pts',(0.197152036252414,1.67840396512523,9.22349164211874));
#74132=CARTESIAN_POINT('Ctrl Pts',(0.461207454074709,2.03755141053213,9.24336198564151));
#74133=CARTESIAN_POINT('Ctrl Pts',(0.302167820508651,2.45398693516803,9.26323232916431));
#74134=CARTESIAN_POINT('Ctrl Pts',(-0.134069651939929,2.54568763775688,
9.28310267268709));
#74135=CARTESIAN_POINT('Ctrl Pts',(-0.447316470668593,2.22853060759678,
9.30297301620988));
#74136=CARTESIAN_POINT('Ctrl Pts',(-0.350211324197387,1.79346424282881,
9.32284335973268));
#74137=CARTESIAN_POINT('Ctrl Pts',(0.0681650352583336,1.63960270419035,
9.34271370325547));
#74138=CARTESIAN_POINT('Ctrl Pts',(0.424009254696116,1.90809300702516,9.36258404677826));
#74139=CARTESIAN_POINT('Ctrl Pts',(0.390882706597841,2.35263185013642,9.38245439030104));
#74140=CARTESIAN_POINT('Ctrl Pts',(-0.00082551092863093,2.56541536346828,
9.40232473382384));
#74141=CARTESIAN_POINT('Ctrl Pts',(-0.391776434561243,2.35124364139831,
9.42219507734661));
#74142=CARTESIAN_POINT('Ctrl Pts',(-0.423325815029323,1.90659008207859,
9.44206542086942));
#74143=CARTESIAN_POINT('Ctrl Pts',(-0.0665313908137084,1.63936379206905,
9.4619357643922));
#74144=CARTESIAN_POINT('Ctrl Pts',(0.351296527042499,1.79470851287912,9.481806107915));
#74145=CARTESIAN_POINT('Ctrl Pts',(0.446857706040839,2.2301166114396,9.50167645143777));
#74146=CARTESIAN_POINT('Ctrl Pts',(0.132487773930098,2.54616043278137,9.52154679496058));
#74147=CARTESIAN_POINT('Ctrl Pts',(-0.303421654179774,2.45291279630443,
9.54141713848336));
#74148=CARTESIAN_POINT('Ctrl Pts',(-0.46098302170792,2.035915713957,9.56128748200614));
#74149=CARTESIAN_POINT('Ctrl Pts',(-0.195655223990523,1.67770723976627,
9.58115782552895));
#74150=CARTESIAN_POINT('Ctrl Pts',(0.249159605684645,1.706894883122,9.60102816905172));
#74151=CARTESIAN_POINT('Ctrl Pts',(0.465404417161516,2.09670295478412,9.62089851257453));
#74152=CARTESIAN_POINT('Ctrl Pts',(0.254704034982808,2.48953561657965,9.6407688560973));
#74153=CARTESIAN_POINT('Ctrl Pts',(-0.189652624469372,2.52502238064893,
9.6606391996201));
#74154=CARTESIAN_POINT('Ctrl Pts',(-0.460028819844302,2.1706089720451,9.68050954314289));
#74155=CARTESIAN_POINT('Ctrl Pts',(-0.308391200280706,1.75142144413341,
9.70037988666567));
#74156=CARTESIAN_POINT('Ctrl Pts',(0.126153361869621,1.65200728654409,9.72025023018848));
#74157=CARTESIAN_POINT('Ctrl Pts',(0.444969388733965,1.96356545484986,9.74012057371125));
#74158=CARTESIAN_POINT('Ctrl Pts',(0.355586578547096,2.40028374444477,9.75999091723406));
#74159=CARTESIAN_POINT('Ctrl Pts',(-0.0599985087153332,2.56153257845199,
9.77986126075682));
#74160=CARTESIAN_POINT('Ctrl Pts',(-0.420543132290841,2.29938810371638,
9.79973160427964));
#74161=CARTESIAN_POINT('Ctrl Pts',(-0.395296683767164,1.85433218806021,
9.8196019478024));
#74162=CARTESIAN_POINT('Ctrl Pts',(-0.00741934267117735,1.63464304520623,
9.83947229132522));
#74163=CARTESIAN_POINT('Ctrl Pts',(0.387264235273323,1.84185555574684,9.85934263484798));
#74164=CARTESIAN_POINT('Ctrl Pts',(0.426685598619483,2.28588045069704,9.87921297837078));
#74165=CARTESIAN_POINT('Ctrl Pts',(0.0746810132312207,2.55938533747102,
9.89908332189357));
#74166=CARTESIAN_POINT('Ctrl Pts',(-0.345833234894805,2.41146671678174,
9.91895366541636));
#74167=CARTESIAN_POINT('Ctrl Pts',(-0.449092570948396,1.9778197858098,9.93882400893915));
#74168=CARTESIAN_POINT('Ctrl Pts',(-0.140370611589618,1.65625656802318,
9.95869435246194));
#74169=CARTESIAN_POINT('Ctrl Pts',(0.297122274169468,1.74176753886202,9.97856469598473));
#74170=CARTESIAN_POINT('Ctrl Pts',(0.462045922923124,2.15590802384918,9.99843503950751));
#74171=CARTESIAN_POINT('Ctrl Pts',(0.203105339267231,2.51876050814486,10.0183053830303));
#74172=CARTESIAN_POINT('Ctrl Pts',(-0.242156742871212,2.49745723531295,
10.0381757265531));
#74173=CARTESIAN_POINT('Ctrl Pts',(-0.465272980088995,2.11154105799798,
10.0580460700759));
#74174=CARTESIAN_POINT('Ctrl Pts',(-0.261564599271689,1.71503753114305,
10.0779164135986));
#74175=CARTESIAN_POINT('Ctrl Pts',(0.182093692572646,1.67168466155662,10.0977867571214));
#74176=CARTESIAN_POINT('Ctrl Pts',(0.458705811299323,2.02125280512402,10.1176571006442));
#74177=CARTESIAN_POINT('Ctrl Pts',(0.314517795316142,2.44306077952759,10.137527444167));
#74178=CARTESIAN_POINT('Ctrl Pts',(-0.118197480138174,2.55015719222244,
10.1573977876898));
#74179=CARTESIAN_POINT('Ctrl Pts',(-0.442482658699621,2.24429566442108,
10.1772681312126));
#74180=CARTESIAN_POINT('Ctrl Pts',(-0.360850236478646,1.80606250859424,
10.1971384747354));
#74181=CARTESIAN_POINT('Ctrl Pts',(0.0518131523877713,1.63747698515616,
10.2170088182582));
#74182=CARTESIAN_POINT('Ctrl Pts',(0.41694502766216,1.89319336101468,10.236879161781));
#74183=CARTESIAN_POINT('Ctrl Pts',(0.39958660199647,2.33862667396065,10.2567495053038));
#74184=CARTESIAN_POINT('Ctrl Pts',(0.0156618678027072,2.56515249963591,
10.2766198488265));
#74185=CARTESIAN_POINT('Ctrl Pts',(-0.382630497929272,2.36496423168987,
10.2964901923493));
#74186=CARTESIAN_POINT('Ctrl Pts',(-0.429911472249707,1.92170735279128,
10.3163605358721));
#74187=CARTESIAN_POINT('Ctrl Pts',(-0.0828071979430214,1.64200970535455,
10.3362308793949));
#74188=CARTESIAN_POINT('Ctrl Pts',(0.340261407294346,1.78245580350654,10.3561012229177));
#74189=CARTESIAN_POINT('Ctrl Pts',(0.451186493746875,2.21420547220255,10.3759715664405));
#74190=CARTESIAN_POINT('Ctrl Pts',(0.148209395681264,2.54118716782383,10.3958419099633));
#74191=CARTESIAN_POINT('Ctrl Pts',(-0.290729646034643,2.46343969917604,
10.4157122534861));
#74192=CARTESIAN_POINT('Ctrl Pts',(-0.462963816781086,2.05228578438148,
10.4355825970089));
#74193=CARTESIAN_POINT('Ctrl Pts',(-0.210491712463267,1.68490316671301,
10.4554529405316));
#74194=CARTESIAN_POINT('Ctrl Pts',(0.235077882180559,1.69831538325434,10.4753232840544));
#74195=CARTESIAN_POINT('Ctrl Pts',(0.464995522887528,2.0802185512372,10.4951936275772));
#74196=CARTESIAN_POINT('Ctrl Pts',(0.268343074769386,2.48026850545887,10.5150639711));
#74197=CARTESIAN_POINT('Ctrl Pts',(-0.174477612838825,2.53147387480434,
10.5349343146228));
#74198=CARTESIAN_POINT('Ctrl Pts',(-0.457238843649517,2.18686070388073,
10.5548046581456));
#74199=CARTESIAN_POINT('Ctrl Pts',(-0.320545682859447,1.76256466216359,
10.5746750016684));
#74200=CARTESIAN_POINT('Ctrl Pts',(0.110204503599964,1.64781960523825,10.5945453451912));
#74201=CARTESIAN_POINT('Ctrl Pts',(0.439857060994807,1.94788850170479,10.614415688714));
#74202=CARTESIAN_POINT('Ctrl Pts',(0.366000646058553,2.38749898974663,10.6342860322368));
#74203=CARTESIAN_POINT('Ctrl Pts',(-0.0436115351477654,2.56336829414912,
10.6541563757595));
#74204=CARTESIAN_POINT('Ctrl Pts',(-0.413216070030391,2.31416027056679,
10.6740267192823));
#74205=CARTESIAN_POINT('Ctrl Pts',(-0.40375111494835,1.86848935402757,10.6938970628051));
#74206=CARTESIAN_POINT('Ctrl Pts',(-0.0238994776521259,1.63519793783959,
10.7137674063279));
#74207=CARTESIAN_POINT('Ctrl Pts',(0.377876676769845,1.82829913659691,10.7336377498507));
#74208=CARTESIAN_POINT('Ctrl Pts',(0.433002423519727,2.27064888879407,10.7535080933735));
#74209=CARTESIAN_POINT('Ctrl Pts',(0.0909073946472628,2.55645151727105,
10.7733784368963));
#74210=CARTESIAN_POINT('Ctrl Pts',(-0.334582792889821,2.42352201891472,
10.7932487804191));
#74211=CARTESIAN_POINT('Ctrl Pts',(-0.453138817284674,1.9938051117499,10.8131191239419));
#74212=CARTESIAN_POINT('Ctrl Pts',(-0.156001666100313,1.66150755742598,
10.8329894674646));
#74213=CARTESIAN_POINT('Ctrl Pts',(0.284245776021994,1.73146712380812,10.8528598109874));
#74214=CARTESIAN_POINT('Ctrl Pts',(0.463736415212255,2.13950543287564,10.8727301545102));
#74215=CARTESIAN_POINT('Ctrl Pts',(0.217812025457425,2.5113028854588,10.892600498033));
#74216=CARTESIAN_POINT('Ctrl Pts',(-0.227925245224916,2.50578593446517,
10.9124708415558));
#74217=CARTESIAN_POINT('Ctrl Pts',(-0.464572132633622,2.12801563136634,
10.9323411850786));
#74218=CARTESIAN_POINT('Ctrl Pts',(-0.275037334135784,1.7245448004727,10.9522115286014));
#74219=CARTESIAN_POINT('Ctrl Pts',(0.166806775479661,1.66550300153548,10.9720818721242));
#74220=CARTESIAN_POINT('Ctrl Pts',(0.455628377284424,2.00505304726444,10.9919522156469));
#74221=CARTESIAN_POINT('Ctrl Pts',(0.326472971133189,2.43170399626786,11.0118225591698));
#74222=CARTESIAN_POINT('Ctrl Pts',(-0.1021769407511,2.55406168611693,11.0316929026925));
#74223=CARTESIAN_POINT('Ctrl Pts',(-0.437093419630667,2.25987959387044,
11.0515632462153));
#74224=CARTESIAN_POINT('Ctrl Pts',(-0.371036190894924,1.81902973988909,
11.0714335897381));
#74225=CARTESIAN_POINT('Ctrl Pts',(0.0353962309707253,1.6359318489126,11.0913039332609));
#74226=CARTESIAN_POINT('Ctrl Pts',(0.409357429682445,1.87855330938489,11.1111742767837));
#74227=CARTESIAN_POINT('Ctrl Pts',(0.40778891564229,2.32432196125189,11.1310446203065));
#74228=CARTESIAN_POINT('Ctrl Pts',(0.0321295869481889,2.56430575234768,
11.1509149638293));
#74229=CARTESIAN_POINT('Ctrl Pts',(-0.373004263722582,2.37835222518488,
11.1707853073521));
#74230=CARTESIAN_POINT('Ctrl Pts',(-0.435957482373001,1.9370484256486,11.1906556508749));
#74231=CARTESIAN_POINT('Ctrl Pts',(-0.0989790611981271,1.64523051172605,
11.2105259943976));
#74232=CARTESIAN_POINT('Ctrl Pts',(0.328799173843605,1.77060169201958,11.2303963379204));
#74233=CARTESIAN_POINT('Ctrl Pts',(0.45494892884938,2.19815097635484,11.2502666814432));
#74234=CARTESIAN_POINT('Ctrl Pts',(0.163744977339756,2.53566010193339,11.270137024966));
#74235=CARTESIAN_POINT('Ctrl Pts',(-0.277672699013363,2.4735103937553,11.2900073684888));
#74236=CARTESIAN_POINT('Ctrl Pts',(-0.464363475746229,2.06871574815522,
11.3098777120116));
#74237=CARTESIAN_POINT('Ctrl Pts',(-0.225063980860663,1.69262014465643,
11.3297480555344));
#74238=CARTESIAN_POINT('Ctrl Pts',(0.220701076770306,1.69024009867603,11.3496183990572));
#74239=CARTESIAN_POINT('Ctrl Pts',(0.464002942203016,2.06375897838704,11.36948874258));
#74240=CARTESIAN_POINT('Ctrl Pts',(0.281645276460985,2.47052406165838,11.3893590861028));
#74241=CARTESIAN_POINT('Ctrl Pts',(-0.15908358789192,2.53738376065424,11.4092294296255));
#74242=CARTESIAN_POINT('Ctrl Pts',(-0.453874917628838,2.20300340367202,
11.4290997731483));
#74243=CARTESIAN_POINT('Ctrl Pts',(-0.332297799931782,1.77413144646791,
11.4489701166711));
#74244=CARTESIAN_POINT('Ctrl Pts',(0.0941173109422024,1.64419952413187,
11.4688404601939));
#74245=CARTESIAN_POINT('Ctrl Pts',(0.434192601941608,1.93240248677327,11.4887108037167));
#74246=CARTESIAN_POINT('Ctrl Pts',(0.375955290644748,2.37435335145907,11.5085811472395));
#74247=CARTESIAN_POINT('Ctrl Pts',(-0.0271698181275119,2.56462236601731,
11.5284514907623));
#74248=CARTESIAN_POINT('Ctrl Pts',(-0.40537031760452,2.32866361237813,11.548321834285));
#74249=CARTESIAN_POINT('Ctrl Pts',(-0.411698736864844,1.88293712412185,
11.5681921778079));
#74250=CARTESIAN_POINT('Ctrl Pts',(-0.0403496127736347,1.63633627404161,
11.5880625213306));
#74251=CARTESIAN_POINT('Ctrl Pts',(0.368014787933636,1.81508377041178,11.6079328648534));
#74252=CARTESIAN_POINT('Ctrl Pts',(0.43877572140111,2.255203119587,11.6278032083762));
#74253=CARTESIAN_POINT('Ctrl Pts',(0.10701966440361,2.55294473553796,11.647673551899));
#74254=CARTESIAN_POINT('Ctrl Pts',(-0.322912365272506,2.43517121949046,
11.6675438954218));
#74255=CARTESIAN_POINT('Ctrl Pts',(-0.456616260360021,2.00992373900169,
11.6874142389446));
#74256=CARTESIAN_POINT('Ctrl Pts',(-0.171436899257811,1.66730896520326,
11.7072845824674));
#74257=CARTESIAN_POINT('Ctrl Pts',(0.271012477887101,1.72162931026559,11.7271549259902));
#74258=CARTESIAN_POINT('Ctrl Pts',(0.464844801587871,2.12305325264119,11.747025269513));
#74259=CARTESIAN_POINT('Ctrl Pts',(0.232245302737102,2.50332897413545,11.7668956130357));
#74260=CARTESIAN_POINT('Ctrl Pts',(-0.213407644032012,2.51360527014209,
11.7867659565585));
#74261=CARTESIAN_POINT('Ctrl Pts',(-0.463288130229042,2.14445503806638,
11.8066363000813));
#74262=CARTESIAN_POINT('Ctrl Pts',(-0.28816482792459,1.73452336057171,11.8265066436041));
#74263=CARTESIAN_POINT('Ctrl Pts',(0.151310473901801,1.6598667446009,11.8463769871269));
#74264=CARTESIAN_POINT('Ctrl Pts',(0.451979014984232,1.98897247172665,11.8662473306497));
#74265=CARTESIAN_POINT('Ctrl Pts',(0.338018341205278,2.41993084101011,11.8861176741725));
#74266=CARTESIAN_POINT('Ctrl Pts',(-0.0860281435876672,2.55739621831784,
11.9059880176953));
#74267=CARTESIAN_POINT('Ctrl Pts',(-0.431155518313124,2.27526283419125,
11.9258583612181));
#74268=CARTESIAN_POINT('Ctrl Pts',(-0.380756401509851,1.83234965957452,
11.9457287047409));
#74269=CARTESIAN_POINT('Ctrl Pts',(0.0189348783753338,1.63496923499459,
11.9655990482636));
#74270=CARTESIAN_POINT('Ctrl Pts',(0.401255985102072,1.86419122908516,11.9854693917864));
#74271=CARTESIAN_POINT('Ctrl Pts',(0.415479351567335,2.30973566802477,12.0053397353092));
#74272=CARTESIAN_POINT('Ctrl Pts',(0.0485569753757318,2.56287618448453,
12.025210078832));
#74273=CARTESIAN_POINT('Ctrl Pts',(-0.362909815287825,2.39139081658207,
12.0450804223548));
#74274=CARTESIAN_POINT('Ctrl Pts',(-0.441456256134848,1.95259404374312,
12.0649507658776));
#74275=CARTESIAN_POINT('Ctrl Pts',(-0.115026680820544,1.649022168261,12.0848211094004));
#74276=CARTESIAN_POINT('Ctrl Pts',(0.31692421467806,1.75916105831155,12.1046914529232));
#74277=CARTESIAN_POINT('Ctrl Pts',(0.458140288545373,2.18197327632933,12.124561796446));
#74278=CARTESIAN_POINT('Ctrl Pts',(0.179075017840616,2.52958617296881,12.1444321399687));
#74279=CARTESIAN_POINT('Ctrl Pts',(-0.264267202870627,2.4831122387859,12.1643024834915));
#74280=CARTESIAN_POINT('Ctrl Pts',(-0.465180241679061,2.08518498153858,
12.1841728270143));
#74281=CARTESIAN_POINT('Ctrl Pts',(-0.239353737318343,1.70084848684698,
12.2040431705371));
#74282=CARTESIAN_POINT('Ctrl Pts',(0.206047235963034,1.68267916590158,12.2239135140599));
#74283=CARTESIAN_POINT('Ctrl Pts',(0.462427921046529,2.0473448971401,12.2437838575827));
#74284=CARTESIAN_POINT('Ctrl Pts',(0.294593942446601,2.46031451690763,12.2636542011055));
#74285=CARTESIAN_POINT('Ctrl Pts',(-0.14348987300431,2.54274461980447,12.2835245446283));
#74286=CARTESIAN_POINT('Ctrl Pts',(-0.449941264356029,2.21901680826798,
12.3033948881511));
#74287=CARTESIAN_POINT('Ctrl Pts',(-0.34363279963305,1.78610727782098,12.3232652316739));
#74288=CARTESIAN_POINT('Ctrl Pts',(0.0779119773719135,1.64115158733782,
12.3431355751966));
#74289=CARTESIAN_POINT('Ctrl Pts',(0.427983121896085,1.91712684890152,12.3630059187194));
#74290=CARTESIAN_POINT('Ctrl Pts',(0.385438016721381,2.36086333066664,12.3828762622422));
#74291=CARTESIAN_POINT('Ctrl Pts',(-0.0106939961474559,2.56529321988075,
12.402746605765));
#74292=CARTESIAN_POINT('Ctrl Pts',(-0.397015723407115,2.34287992380626,
12.4226169492878));
#74293=CARTESIAN_POINT('Ctrl Pts',(-0.419129573250919,1.89765736275538,
12.4424872928106));
#74294=CARTESIAN_POINT('Ctrl Pts',(-0.0567490989759844,1.63805662491381,
12.4623576363334));
#74295=CARTESIAN_POINT('Ctrl Pts',(0.357690947917213,1.80222604580204,12.4822279798562));
#74296=CARTESIAN_POINT('Ctrl Pts',(0.443998245321784,2.23956253140361,12.502098323379));
#74297=CARTESIAN_POINT('Ctrl Pts',(0.122997597546583,2.54886939416535,12.5219686669018));
#74298=CARTESIAN_POINT('Ctrl Pts',(-0.310836601366722,2.4463996958304,12.5418390104245));
#74299=CARTESIAN_POINT('Ctrl Pts',(-0.45952053510819,2.0261554346313,12.5617093539473));
#74300=CARTESIAN_POINT('Ctrl Pts',(-0.18665693595978,1.6736535091282,12.5815796974701));
#74301=CARTESIAN_POINT('Ctrl Pts',(0.257438990884462,1.71226644716637,12.6014500409929));
#74302=CARTESIAN_POINT('Ctrl Pts',(0.46536969074615,2.10657213477266,12.6213203845157));
#74303=CARTESIAN_POINT('Ctrl Pts',(0.246387053710664,2.49484878344037,12.6411907280385));
#74304=CARTESIAN_POINT('Ctrl Pts',(-0.198622162535629,2.52090542710951,
12.6610610715613));
#74305=CARTESIAN_POINT('Ctrl Pts',(-0.461422584621671,2.16083864250527,
12.6809314150841));
#74306=CARTESIAN_POINT('Ctrl Pts',(-0.300930602329029,1.7449606858358,12.7008017586068));
#74307=CARTESIAN_POINT('Ctrl Pts',(0.13562423959672,1.65478296567376,12.7206721021296));
#74308=CARTESIAN_POINT('Ctrl Pts',(0.447762305268633,1.97303126368024,12.7405424456524));
#74309=CARTESIAN_POINT('Ctrl Pts',(0.349139413183901,2.4077560920269,12.7604127891752));
#74310=CARTESIAN_POINT('Ctrl Pts',(-0.0697713594461587,2.56015660314866,
12.780283132698));
#74311=CARTESIAN_POINT('Ctrl Pts',(-0.424676408320006,2.29042607554407,
12.8001534762208));
#74312=CARTESIAN_POINT('Ctrl Pts',(-0.389998666988802,1.84600554780131,
12.8200238197436));
#74313=CARTESIAN_POINT('Ctrl Pts',(0.00244975769600178,1.63459035172035,
12.8398941632664));
#74314=CARTESIAN_POINT('Ctrl Pts',(0.392650863361715,1.85012514814954,12.8597645067892));
#74315=CARTESIAN_POINT('Ctrl Pts',(0.422648256168044,2.29488610373169,12.879634850312));
#74316=CARTESIAN_POINT('Ctrl Pts',(0.0649234129076833,2.56086559054602,
12.8995051938347));
#74317=CARTESIAN_POINT('Ctrl Pts',(-0.352359824332398,2.40406363910594,
12.9193755373576));
#74318=CARTESIAN_POINT('Ctrl Pts',(-0.446400889969114,1.96832469353053,
12.9392458808803));
#74319=CARTESIAN_POINT('Ctrl Pts',(-0.130929915360603,1.65337991524715,
12.9591162244031));
#74320=CARTESIAN_POINT('Ctrl Pts',(0.304651440389382,1.74814826369811,12.9789865679259));
#74321=CARTESIAN_POINT('Ctrl Pts',(0.460756558152438,2.16569267836185,12.9988569114487));
#74322=CARTESIAN_POINT('Ctrl Pts',(0.19418029092386,2.52297300687519,13.0187272549715));
#74323=CARTESIAN_POINT('Ctrl Pts',(-0.25053001723091,2.49223317838584,13.0385975984943));
#74324=CARTESIAN_POINT('Ctrl Pts',(-0.465413027024947,2.10167281756508,
13.0584679420171));
#74325=CARTESIAN_POINT('Ctrl Pts',(-0.253343164592808,1.70957785296128,
13.0783382855398));
#74326=CARTESIAN_POINT('Ctrl Pts',(0.191134985117061,1.6756420983047,13.0982086290627));
#74327=CARTESIAN_POINT('Ctrl Pts',(0.460271991395613,2.03099686796687,13.1180789725854));
#74328=CARTESIAN_POINT('Ctrl Pts',(0.307173676042658,2.44965277020794,13.1379493161082));
#74329=CARTESIAN_POINT('Ctrl Pts',(-0.127717692980967,2.54754956230708,
13.157819659631));
#74330=CARTESIAN_POINT('Ctrl Pts',(-0.445439642377961,2.2348811263436,13.1776900031538));
#74331=CARTESIAN_POINT('Ctrl Pts',(-0.354542576399878,1.79847652742844,
13.1975603466766));
#74332=CARTESIAN_POINT('Ctrl Pts',(0.0616206363204805,1.63868076881278,
13.2174306901994));
#74333=CARTESIAN_POINT('Ctrl Pts',(0.421213705444151,1.9020785519879,13.2373010337222));
#74334=CARTESIAN_POINT('Ctrl Pts',(0.394480663010893,2.34705011774784,13.257171377245));
#74335=CARTESIAN_POINT('Ctrl Pts',(0.00571095611368224,2.56537182328736,
13.2770417207678));
#74336=CARTESIAN_POINT('Ctrl Pts',(-0.387999947893056,2.35680705697765,
13.2969120642905));
#74337=CARTESIAN_POINT('Ctrl Pts',(-0.426352479043764,1.912602081833,13.3167824078133));
#74338=CARTESIAN_POINT('Ctrl Pts',(-0.0724212997312765,1.64040692913555,
13.3366527513361));
#74339=CARTESIAN_POINT('Ctrl Pts',(0.206034670117974,1.73993310315546,13.349899647018));
#74340=CARTESIAN_POINT('Ctrl Pts',(0.293391644475074,1.83761221843237,13.3565230948589));
#74341=CARTESIAN_POINT('Ctrl Pts',(-0.347219699208383,1.97323498128075,
4.32934271053038));
#74342=CARTESIAN_POINT('Ctrl Pts',(-0.304993076091424,1.85755383756099,
4.33597059444799));
#74343=CARTESIAN_POINT('Ctrl Pts',(-0.0965749770348568,1.67383077332961,
4.34922192620653));
#74344=CARTESIAN_POINT('Ctrl Pts',(0.306876354697739,1.78837779405028,4.36909670580601));
#74345=CARTESIAN_POINT('Ctrl Pts',(0.427739319365321,2.18925964705946,4.38896704932879));
#74346=CARTESIAN_POINT('Ctrl Pts',(0.156695639423864,2.5080091347322,4.40883739285158));
#74347=CARTESIAN_POINT('Ctrl Pts',(-0.258344791487002,2.45259440315036,
4.42870773637437));
#74348=CARTESIAN_POINT('Ctrl Pts',(-0.436259586392415,2.07365558490192,
4.44857807989716));
#74349=CARTESIAN_POINT('Ctrl Pts',(-0.214032795552298,1.71891882025207,
4.46844842341995));
#74350=CARTESIAN_POINT('Ctrl Pts',(0.204574834047816,1.71375417298191,4.48831876694274));
#74351=CARTESIAN_POINT('Ctrl Pts',(0.435494789331625,2.06292682817853,4.50818911046552));
#74352=CARTESIAN_POINT('Ctrl Pts',(0.266916968435977,2.44610422235877,4.52805945398832));
#74353=CARTESIAN_POINT('Ctrl Pts',(-0.146525717420236,2.51178062822751,
4.54792979751111));
#74354=CARTESIAN_POINT('Ctrl Pts',(-0.425548469292051,2.19970305918092,
4.56780014103389));
#74355=CARTESIAN_POINT('Ctrl Pts',(-0.314189750545297,1.7961621855343,4.58767048455669));
#74356=CARTESIAN_POINT('Ctrl Pts',(0.0853959749762369,1.67135079038661,
4.60754082807948));
#74357=CARTESIAN_POINT('Ctrl Pts',(0.406642164051052,1.93976687276704,4.62741117160227));
#74358=CARTESIAN_POINT('Ctrl Pts',(0.354849711281776,2.3551749405769,4.64728151512505));
#74359=CARTESIAN_POINT('Ctrl Pts',(-0.0224691388804926,2.53649478868572,
4.66715185864785));
#74360=CARTESIAN_POINT('Ctrl Pts',(-0.379175563316004,2.31739006595186,
4.68702220217063));
#74361=CARTESIAN_POINT('Ctrl Pts',(-0.388040054307679,1.89885956599689,
4.70689254569342));
#74362=CARTESIAN_POINT('Ctrl Pts',(-0.0409306089551436,1.66484802453397,
4.72676288921621));
#74363=CARTESIAN_POINT('Ctrl Pts',(0.343727090956584,1.83002918355619,4.746633232739));
#74364=CARTESIAN_POINT('Ctrl Pts',(0.413061982746445,2.24287181159513,4.76650357626179));
#74365=CARTESIAN_POINT('Ctrl Pts',(0.103468736801614,2.5246490037035,4.78637391978458));
#74366=CARTESIAN_POINT('Ctrl Pts',(-0.301042988188063,2.4168685451533,4.80624426330737));
#74367=CARTESIAN_POINT('Ctrl Pts',(-0.429388755323053,2.01840433444282,
4.82611460683016));
#74368=CARTESIAN_POINT('Ctrl Pts',(-0.163828795187018,1.69479303849886,
4.84598495035295));
#74369=CARTESIAN_POINT('Ctrl Pts',(0.252021781120245,1.74290396585595,4.86585529387574));
#74370=CARTESIAN_POINT('Ctrl Pts',(0.436676682987851,2.11860189026849,4.88572563739853));
#74371=CARTESIAN_POINT('Ctrl Pts',(0.220740176339599,2.47723511279732,4.90559598092132));
#74372=CARTESIAN_POINT('Ctrl Pts',(-0.197695391019725,2.48980647524797,
4.9254663244441));
#74373=CARTESIAN_POINT('Ctrl Pts',(-0.434772350925555,2.14478346402337,
4.9453366679669));
#74374=CARTESIAN_POINT('Ctrl Pts',(-0.273004867762902,1.75867772127277,
4.96520701148968));
#74375=CARTESIAN_POINT('Ctrl Pts',(0.139207415312882,1.68568870242346,4.98507735501248));
#74376=CARTESIAN_POINT('Ctrl Pts',(0.423715846218783,1.99277389570991,5.00494769853526));
#74377=CARTESIAN_POINT('Ctrl Pts',(0.319522671921894,2.39822444216695,5.02481804205805));
#74378=CARTESIAN_POINT('Ctrl Pts',(-0.0777890547791136,2.5300946625273,
5.04468838558084));
#74379=CARTESIAN_POINT('Ctrl Pts',(-0.403739913744015,2.26741158212004,
5.06455872910363));
#74380=CARTESIAN_POINT('Ctrl Pts',(-0.359314366074708,1.85115116614648,
5.08442907262642));
#74381=CARTESIAN_POINT('Ctrl Pts',(0.0147331962342516,1.66317567752396,
5.10429941614921));
#74382=CARTESIAN_POINT('Ctrl Pts',(0.375265056741863,1.87592703651163,5.124169759672));
#74383=CARTESIAN_POINT('Ctrl Pts',(0.39154231541309,2.29423483472046,5.14404010319479));
#74384=CARTESIAN_POINT('Ctrl Pts',(0.0486328033657723,2.53435861475826,
5.16391044671758));
#74385=CARTESIAN_POINT('Ctrl Pts',(-0.338890685011317,2.37601749834112,
5.18378079024037));
#74386=CARTESIAN_POINT('Ctrl Pts',(-0.415528105691254,1.96446790358528,
5.20365113376316));
#74387=CARTESIAN_POINT('Ctrl Pts',(-0.110975058442913,1.67725055626113,
5.22352147728595));
#74388=CARTESIAN_POINT('Ctrl Pts',(0.295382497036827,1.77784827142755,5.24339182080874));
#74389=CARTESIAN_POINT('Ctrl Pts',(0.430766824181072,2.1739763405616,5.26326216433152));
#74390=CARTESIAN_POINT('Ctrl Pts',(0.170981233746816,2.50224118819976,5.28313250785433));
#74391=CARTESIAN_POINT('Ctrl Pts',(-0.245656361657064,2.46150450585759,
5.30300285137709));
#74392=CARTESIAN_POINT('Ctrl Pts',(-0.436937688334339,2.08913665378555,
5.32287319489991));
#74393=CARTESIAN_POINT('Ctrl Pts',(-0.22738816965979,1.72673444295421,5.34274353842268));
#74394=CARTESIAN_POINT('Ctrl Pts',(0.190759038573631,1.70675256519541,5.36261388194548));
#74395=CARTESIAN_POINT('Ctrl Pts',(0.433910798413821,2.04752167306581,5.38248422546826));
#74396=CARTESIAN_POINT('Ctrl Pts',(0.279008472330408,2.43643250161924,5.40235456899106));
#74397=CARTESIAN_POINT('Ctrl Pts',(-0.131846143542539,2.51671231108631,
5.42222491251384));
#74398=CARTESIAN_POINT('Ctrl Pts',(-0.421749871946843,2.21471530539013,
5.44209525603663));
#74399=CARTESIAN_POINT('Ctrl Pts',(-0.324755508900358,1.80748262407713,
5.46196559955943));
#74400=CARTESIAN_POINT('Ctrl Pts',(0.0701578220919378,1.66859481252858,
5.48183594308221));
#74401=CARTESIAN_POINT('Ctrl Pts',(0.400710902439894,1.92546252997211,5.50170628660501));
#74402=CARTESIAN_POINT('Ctrl Pts',(0.363666281662623,2.3424446150353,5.52157663012779));
#74403=CARTESIAN_POINT('Ctrl Pts',(-0.00699264384645848,2.53701677165752,
5.54144697365058));
#74404=CARTESIAN_POINT('Ctrl Pts',(-0.371236770588911,2.33068553474513,
5.56131731717337));
#74405=CARTESIAN_POINT('Ctrl Pts',(-0.39492169963869,1.91273172470378,5.58118766069616));
#74406=CARTESIAN_POINT('Ctrl Pts',(-0.0563197330045467,1.66657106297314,
5.60105800421896));
#74407=CARTESIAN_POINT('Ctrl Pts',(0.333947921421964,1.81802244494308,5.62092834774173));
#74408=CARTESIAN_POINT('Ctrl Pts',(0.417863820848056,2.2281498459,5.64079869126453));
#74409=CARTESIAN_POINT('Ctrl Pts',(0.118446551668408,2.52071720926984,5.66066903478731));
#74410=CARTESIAN_POINT('Ctrl Pts',(-0.289629303625079,2.4273338086107,5.68053937831011));
#74411=CARTESIAN_POINT('Ctrl Pts',(-0.432009702311787,2.03366620102533,
5.7004097218329));
#74412=CARTESIAN_POINT('Ctrl Pts',(-0.178080011937646,1.70085082346795,
5.72028006535568));
#74413=CARTESIAN_POINT('Ctrl Pts',(0.239213845984823,1.73420047612512,5.74015040887847));
#74414=CARTESIAN_POINT('Ctrl Pts',(0.437061566240658,2.10312139282916,5.76002075240126));
#74415=CARTESIAN_POINT('Ctrl Pts',(0.233964800030075,2.46917885655169,5.77989109592406));
#74416=CARTESIAN_POINT('Ctrl Pts',(-0.183762818776739,2.49656497855101,
5.79976143944684));
#74417=CARTESIAN_POINT('Ctrl Pts',(-0.432913068404649,2.16015672017656,
5.81963178296963));
#74418=CARTESIAN_POINT('Ctrl Pts',(-0.284924513563698,1.76856286063808,
5.83950212649242));
#74419=CARTESIAN_POINT('Ctrl Pts',(0.124443493502042,1.68101745537201,5.85937247001521));
#74420=CARTESIAN_POINT('Ctrl Pts',(0.4196515367315,1.97783149547931,5.879242813538));
#74421=CARTESIAN_POINT('Ctrl Pts',(0.329886425407692,2.38671850674427,5.89911315706079));
#74422=CARTESIAN_POINT('Ctrl Pts',(-0.06250457124619,2.5325803212714,5.91898350058358));
#74423=CARTESIAN_POINT('Ctrl Pts',(-0.397556133010694,2.28160858152498,
5.93885384410637));
#74424=CARTESIAN_POINT('Ctrl Pts',(-0.36790406511818,1.86403569200524,5.95872418762916));
#74425=CARTESIAN_POINT('Ctrl Pts',(-0.000750103095509274,1.66292793143089,
5.97859453115195));
#74426=CARTESIAN_POINT('Ctrl Pts',(0.367091976399978,1.86277429177955,5.99846487467474));
#74427=CARTESIAN_POINT('Ctrl Pts',(0.398177142608358,2.28024294405656,6.01833521819753));
#74428=CARTESIAN_POINT('Ctrl Pts',(0.063988987396686,2.53236323302274,6.03820556172031));
#74429=CARTESIAN_POINT('Ctrl Pts',(-0.328900352437435,2.38784911662964,
6.05807590524311));
#74430=CARTESIAN_POINT('Ctrl Pts',(-0.420068394649978,1.9792726228475,6.07794624876589));
#74431=CARTESIAN_POINT('Ctrl Pts',(-0.125880871919137,1.6814470620545,6.09781659228868));
#74432=CARTESIAN_POINT('Ctrl Pts',(0.283785213664268,1.76758684098932,6.11768693581147));
#74433=CARTESIAN_POINT('Ctrl Pts',(0.43311699957894,2.15867043935124,6.13755727933426));
#74434=CARTESIAN_POINT('Ctrl Pts',(0.185122901935055,2.49593189686748,6.15742762285705));
#74435=CARTESIAN_POINT('Ctrl Pts',(-0.232696256026886,2.4699797402683,6.17729796637985));
#74436=CARTESIAN_POINT('Ctrl Pts',(-0.437048277818848,2.10462154016639,
6.19716830990262));
#74437=CARTESIAN_POINT('Ctrl Pts',(-0.24046800346235,1.7350237061277,6.21703865342543));
#74438=CARTESIAN_POINT('Ctrl Pts',(0.176708927308292,1.70024193468113,6.2369089969482));
#74439=CARTESIAN_POINT('Ctrl Pts',(0.431779474021718,2.03218376601832,6.256779340471));
#74440=CARTESIAN_POINT('Ctrl Pts',(0.290751134787684,2.42633775968712,6.27664968399379));
#74441=CARTESIAN_POINT('Ctrl Pts',(-0.117001788421295,2.52112128571726,
6.29652002751657));
#74442=CARTESIAN_POINT('Ctrl Pts',(-0.417421499108909,2.22958336258796,
6.31639037103937));
#74443=CARTESIAN_POINT('Ctrl Pts',(-0.334913811169784,1.81917034546604,
6.33626071456215));
#74444=CARTESIAN_POINT('Ctrl Pts',(0.0548317041193742,1.66638030487385,
6.35613105808495));
#74445=CARTESIAN_POINT('Ctrl Pts',(0.394276595541465,1.91137730256896,6.37600140160773));
#74446=CARTESIAN_POINT('Ctrl Pts',(0.372026386465847,2.32940994649555,6.39587174513052));
#74447=CARTESIAN_POINT('Ctrl Pts',(0.00849261462696172,2.53699019585654,
6.41574208865331));
#74448=CARTESIAN_POINT('Ctrl Pts',(-0.362831974967082,2.34369143136232,
6.43561243217611));
#74449=CARTESIAN_POINT('Ctrl Pts',(-0.401307622641875,1.92683895418584,
6.45548277569889));
#74450=CARTESIAN_POINT('Ctrl Pts',(-0.0716381596422418,1.66883816279614,
6.47535311922169));
#74451=CARTESIAN_POINT('Ctrl Pts',(0.323749562174376,1.8063696596572,6.49522346274447));
#74452=CARTESIAN_POINT('Ctrl Pts',(0.422141135218989,2.21326701962157,6.51509380626727));
#74453=CARTESIAN_POINT('Ctrl Pts',(0.133275686026303,2.51625730899547,6.53496414979004));
#74454=CARTESIAN_POINT('Ctrl Pts',(-0.277852061249243,2.43738818568153,
6.55483449331285));
#74455=CARTESIAN_POINT('Ctrl Pts',(-0.434088368471071,2.04901133325871,
6.57470483683562));
#74456=CARTESIAN_POINT('Ctrl Pts',(-0.192107693415753,1.70740964109086,
6.59457518035843));
#74457=CARTESIAN_POINT('Ctrl Pts',(0.226105637247668,1.72595615687094,6.6144455238812));
#74458=CARTESIAN_POINT('Ctrl Pts',(0.436897827239315,2.08763697725087,6.634315867404));
#74459=CARTESIAN_POINT('Ctrl Pts',(0.246895739007226,2.46065918792955,6.65418621092679));
#74460=CARTESIAN_POINT('Ctrl Pts',(-0.169599577944252,2.50282569299769,
6.67405655444958));
#74461=CARTESIAN_POINT('Ctrl Pts',(-0.430510371029507,2.17545446450653,
6.69392689797236));
#74462=CARTESIAN_POINT('Ctrl Pts',(-0.296486507389875,1.77886403702843,
6.71379724149516));
#74463=CARTESIAN_POINT('Ctrl Pts',(0.109523363786731,1.67687213686313,6.73366758501794));
#74464=CARTESIAN_POINT('Ctrl Pts',(0.41506045894861,1.96304244746893,6.75353792854074));
#74465=CARTESIAN_POINT('Ctrl Pts',(0.339836088404225,2.37485266743484,6.77340827206352));
#74466=CARTESIAN_POINT('Ctrl Pts',(-0.0471416287452485,2.53452298284116,
6.79327861558631));
#74467=CARTESIAN_POINT('Ctrl Pts',(-0.390873319274194,2.29557761645317,
6.8131489591091));
#74468=CARTESIAN_POINT('Ctrl Pts',(-0.376031951966423,1.87721641245762,
6.8330193026319));
#74469=CARTESIAN_POINT('Ctrl Pts',(-0.0162324608571044,1.66322882078547,
6.85288964615468));
#74470=CARTESIAN_POINT('Ctrl Pts',(0.358458103238608,1.84991932501589,6.87275998967748));
#74471=CARTESIAN_POINT('Ctrl Pts',(0.404312157277081,2.26602480313461,6.89263033320026));
#74472=CARTESIAN_POINT('Ctrl Pts',(0.0792648491437742,2.52982512661331,
6.91250067672305));
#74473=CARTESIAN_POINT('Ctrl Pts',(-0.318497167144145,2.39931941183139,
6.93237102024584));
#74474=CARTESIAN_POINT('Ctrl Pts',(-0.424081392051288,1.99422888535251,
6.95224136376863));
#74475=CARTESIAN_POINT('Ctrl Pts',(-0.140628673219612,1.68616895712571,
6.97211170729142));
#74476=CARTESIAN_POINT('Ctrl Pts',(0.271831708425969,1.75774267272686,6.99198205081421));
#74477=CARTESIAN_POINT('Ctrl Pts',(0.434923504136159,2.14329089197343,7.01185239433699));
#74478=CARTESIAN_POINT('Ctrl Pts',(0.199032194289939,2.48912561135713,7.03172273785979));
#74479=CARTESIAN_POINT('Ctrl Pts',(-0.219444058030784,2.47799055698908,
7.05159308138258));
#74480=CARTESIAN_POINT('Ctrl Pts',(-0.436610261719101,2.12010062535118,
7.07146342490537));
#74481=CARTESIAN_POINT('Ctrl Pts',(-0.253245989399967,1.74377110640662,
7.09133376842815));
#74482=CARTESIAN_POINT('Ctrl Pts',(0.162437001865369,1.69423310114929,7.11120411195095));
#74483=CARTESIAN_POINT('Ctrl Pts',(0.42910615772017,2.01693098541236,7.13107445547373));
#74484=CARTESIAN_POINT('Ctrl Pts',(0.30212883139503,2.41583338173442,7.15094479899653));
#74485=CARTESIAN_POINT('Ctrl Pts',(-0.102010566608769,2.5250016471475,7.17081514251931));
#74486=CARTESIAN_POINT('Ctrl Pts',(-0.412569157233639,2.24428876005239,
7.19068548604211));
#74487=CARTESIAN_POINT('Ctrl Pts',(-0.344651712315627,1.83121057875013,
7.21055582956488));
#74488=CARTESIAN_POINT('Ctrl Pts',(0.0394367585581893,1.66471009906919,
7.23042617308769));
#74489=CARTESIAN_POINT('Ctrl Pts',(0.387347372284745,1.89752884412333,7.25029651661046));
#74490=CARTESIAN_POINT('Ctrl Pts',(0.379919504523068,2.31608731073545,7.27016686013327));
#74491=CARTESIAN_POINT('Ctrl Pts',(0.0239672127316146,2.53641508737876,
7.29003720365604));
#74492=CARTESIAN_POINT('Ctrl Pts',(-0.353971733899714,2.3563914339013,7.30990754717885));
#74493=CARTESIAN_POINT('Ctrl Pts',(-0.407189803578201,1.94116354436126,
7.32977789070163));
#74494=CARTESIAN_POINT('Ctrl Pts',(-0.0868666623598067,1.67164647923894,
7.34964823422442));
#74495=CARTESIAN_POINT('Ctrl Pts',(0.313144815745497,1.79508545434884,7.36951857774721));
#74496=CARTESIAN_POINT('Ctrl Pts',(0.425888556221436,2.19824201472666,7.38938892126999));
#74497=CARTESIAN_POINT('Ctrl Pts',(0.147937525855628,2.51127490103536,7.40925926479279));
#74498=CARTESIAN_POINT('Ctrl Pts',(-0.265726044607188,2.44701905566604,
7.42912960831557));
#74499=CARTESIAN_POINT('Ctrl Pts',(-0.435622144477278,2.0644204691016,7.44899995183837));
#74500=CARTESIAN_POINT('Ctrl Pts',(-0.20589423138927,1.7144612584207,7.46887029536115));
#74501=CARTESIAN_POINT('Ctrl Pts',(0.212713609029873,1.71818135677861,7.48874063888394));
#74502=CARTESIAN_POINT('Ctrl Pts',(0.436185671507062,2.07216808037763,7.50861098240673));
#74503=CARTESIAN_POINT('Ctrl Pts',(0.259516761693601,2.45168680125645,7.52848132592952));
#74504=CARTESIAN_POINT('Ctrl Pts',(-0.155223446956909,2.50858075981714,
7.54835166945232));
#74505=CARTESIAN_POINT('Ctrl Pts',(-0.427567274788573,2.1906574944933,7.56822201297509));
#74506=CARTESIAN_POINT('Ctrl Pts',(-0.307676336030043,1.78956831987527,
7.5880923564979));
#74507=CARTESIAN_POINT('Ctrl Pts',(0.0944657546852107,1.67325795031462,
7.60796270002068));
#74508=CARTESIAN_POINT('Ctrl Pts',(0.409948375828002,1.94842531565623,7.62783304354347));
#74509=CARTESIAN_POINT('Ctrl Pts',(0.349359171580419,2.36264181885332,7.64770338706626));
#74510=CARTESIAN_POINT('Ctrl Pts',(-0.031719511635709,2.53592020870742,
7.66757373058905));
#74511=CARTESIAN_POINT('Ctrl Pts',(-0.38369986114765,2.30930115225006,7.68744407411183));
#74512=CARTESIAN_POINT('Ctrl Pts',(-0.383687824075844,1.89067678238218,
7.70731441763464));
#74513=CARTESIAN_POINT('Ctrl Pts',(-0.0316944427949657,1.6640779678958,
7.72718476115741));
#74514=CARTESIAN_POINT('Ctrl Pts',(0.349374274941528,1.83737827243922,7.74705510468021));
#74515=CARTESIAN_POINT('Ctrl Pts',(0.409939658431796,2.25159825929987,7.76692544820299));
#74516=CARTESIAN_POINT('Ctrl Pts',(0.0944412135559431,2.5267474814923,7.78679579172579));
#74517=CARTESIAN_POINT('Ctrl Pts',(-0.307694187747241,2.41041398583906,
7.80666613524857));
#74518=CARTESIAN_POINT('Ctrl Pts',(-0.427562060573467,2.00931791722671,
7.82653647877136));
#74519=CARTESIAN_POINT('Ctrl Pts',(-0.155199950142004,1.69141031430805,
7.84640682229416));
#74520=CARTESIAN_POINT('Ctrl Pts',(0.259536985979435,1.7483281235489,7.86627716581694));
#74521=CARTESIAN_POINT('Ctrl Pts',(0.436184070234853,2.1278570036308,7.88614750933974));
#74522=CARTESIAN_POINT('Ctrl Pts',(0.212691651148888,2.48183087527004,7.90601785286252));
#74523=CARTESIAN_POINT('Ctrl Pts',(-0.205916402512528,2.48552690042879,
7.92588819638531));
#74524=CARTESIAN_POINT('Ctrl Pts',(-0.435624189855542,2.13555447919227,
7.9457585399081));
#74525=CARTESIAN_POINT('Ctrl Pts',(-0.265706087884356,1.75296566360212,
7.96562888343089));
#74526=CARTESIAN_POINT('Ctrl Pts',(0.147961177103221,1.68873360719825,7.98549922695368));
#74527=CARTESIAN_POINT('Ctrl Pts',(0.425894205193953,2.00178247732637,8.00536957047647));
#74528=CARTESIAN_POINT('Ctrl Pts',(0.313127280279686,2.40493255339923,8.02523991399926));
#74529=CARTESIAN_POINT('Ctrl Pts',(-0.0868912958612956,2.52834852454686,
8.04511025752205));
#74530=CARTESIAN_POINT('Ctrl Pts',(-0.407198937231307,2.25881303880861,
8.06498060104484));
#74531=CARTESIAN_POINT('Ctrl Pts',(-0.353956988821141,1.84358821040638,
8.08485094456762));
#74532=CARTESIAN_POINT('Ctrl Pts',(0.0239923099396314,1.66358629164325,
8.10472128809042));
#74533=CARTESIAN_POINT('Ctrl Pts',(0.379931930588853,1.88393453793593,8.1245916316132));
#74534=CARTESIAN_POINT('Ctrl Pts',(0.387335727984592,2.30249343101586,8.144461975136));
#74535=CARTESIAN_POINT('Ctrl Pts',(0.0394117259522656,2.53529216813009,
8.16433231865878));
#74536=CARTESIAN_POINT('Ctrl Pts',(-0.344667169219275,2.36876960066255,
8.18420266218158));
#74537=CARTESIAN_POINT('Ctrl Pts',(-0.412560858830175,1.95568751426422,
8.20407300570436));
#74538=CARTESIAN_POINT('Ctrl Pts',(-0.10198612555365,1.67499248715759,8.22394334922715));
#74539=CARTESIAN_POINT('Ctrl Pts',(0.302146993761083,1.78418399353568,8.24381369274995));
#74540=CARTESIAN_POINT('Ctrl Pts',(0.42910137989889,2.18309369137787,8.26368403627273));
#74541=CARTESIAN_POINT('Ctrl Pts',(0.162413666857334,2.50577623956545,8.28355437979553));
#74542=CARTESIAN_POINT('Ctrl Pts',(-0.253266474901655,2.4562143293985,8.30342472331831));
#74543=CARTESIAN_POINT('Ctrl Pts',(-0.436609105055496,2.07987426621036,
8.3232950668411));
#74544=CARTESIAN_POINT('Ctrl Pts',(-0.219422320283272,1.72199682390298,
8.34316541036389));
#74545=CARTESIAN_POINT('Ctrl Pts',(0.199054571697336,1.71088583517903,8.36303575388668));
#74546=CARTESIAN_POINT('Ctrl Pts',(0.434925992978568,2.05673411956821,8.38290609740947));
#74547=CARTESIAN_POINT('Ctrl Pts',(0.271812025529305,2.44227295913581,8.40277644093226));
#74548=CARTESIAN_POINT('Ctrl Pts',(-0.140652471477245,2.51382295495208,
8.42264678445504));
#74549=CARTESIAN_POINT('Ctrl Pts',(-0.42408747400835,2.20574672650795,8.44251712797784));
#74550=CARTESIAN_POINT('Ctrl Pts',(-0.318479953433018,1.80066227260963,
8.46238747150062));
#74551=CARTESIAN_POINT('Ctrl Pts',(0.0792895672865693,1.67017943244019,
8.48225781502342));
#74552=CARTESIAN_POINT('Ctrl Pts',(0.404321704320595,1.93399844822044,8.5021281585462));
#74553=CARTESIAN_POINT('Ctrl Pts',(0.358443721070139,2.35010128868785,8.521998502069));
#74554=CARTESIAN_POINT('Ctrl Pts',(-0.0162575785559514,2.53677024500007,
8.54186884559178));
#74555=CARTESIAN_POINT('Ctrl Pts',(-0.376044763126415,2.32276196242431,
8.56173918911457));
#74556=CARTESIAN_POINT('Ctrl Pts',(-0.390862071400124,1.90439990562698,
8.58160953263737));
#74557=CARTESIAN_POINT('Ctrl Pts',(-0.0471166402303176,1.66547430686859,
8.60147987616015));
#74558=CARTESIAN_POINT('Ctrl Pts',(0.339851893999448,1.82516687622683,8.62135021968295));
#74559=CARTESIAN_POINT('Ctrl Pts',(0.415052582142242,2.23698142149572,8.64122056320573));
#74560=CARTESIAN_POINT('Ctrl Pts',(0.109499030476289,2.5231341608789,8.66109090672852));
#74561=CARTESIAN_POINT('Ctrl Pts',(-0.296504974704751,2.42111891217004,
8.68096125025131));
#74562=CARTESIAN_POINT('Ctrl Pts',(-0.430506031101505,2.0245207779375,8.7008315937741));
#74563=CARTESIAN_POINT('Ctrl Pts',(-0.169576412066495,1.6971645543791,8.72070193729689));
#74564=CARTESIAN_POINT('Ctrl Pts',(0.246916479295651,1.73935501108407,8.74057228081968));
#74565=CARTESIAN_POINT('Ctrl Pts',(0.436897115547312,2.11238814773762,8.76044262434247));
#74566=CARTESIAN_POINT('Ctrl Pts',(0.226084126455762,2.47405684533593,8.78031296786525));
#74567=CARTESIAN_POINT('Ctrl Pts',(-0.192130270084417,2.49257931057968,
8.80018331138805));
#74568=CARTESIAN_POINT('Ctrl Pts',(-0.43409129999653,2.15096370321368,8.82005365491084));
#74569=CARTESIAN_POINT('Ctrl Pts',(-0.277832658355979,1.76259583623082,
8.83992399843362));
#74570=CARTESIAN_POINT('Ctrl Pts',(0.133299623825185,1.68375035607703,8.85979434195643));
#74571=CARTESIAN_POINT('Ctrl Pts',(0.422147648251856,1.98675725695057,8.87966468547919));
#74572=CARTESIAN_POINT('Ctrl Pts',(0.323732675620234,2.39364895796461,8.89953502900202));
#74573=CARTESIAN_POINT('Ctrl Pts',(-0.0716629546688544,2.53115771674186,
8.91940537252477));
#74574=CARTESIAN_POINT('Ctrl Pts',(-0.401317580079588,2.27313796723133,
8.93927571604757));
#74575=CARTESIAN_POINT('Ctrl Pts',(-0.362817960222371,1.85628770339187,
8.95914605957037));
#74576=CARTESIAN_POINT('Ctrl Pts',(0.00851774493375449,1.66301029325719,
8.97901640309315));
#74577=CARTESIAN_POINT('Ctrl Pts',(0.372039578699426,1.87061144828242,8.99888674661594));
#74578=CARTESIAN_POINT('Ctrl Pts',(0.394265747623478,2.28864537107714,9.01875709013873));
#74579=CARTESIAN_POINT('Ctrl Pts',(0.0548067675377615,2.5336228476568,9.03862743366152));
#74580=CARTESIAN_POINT('Ctrl Pts',(-0.334929960496195,2.38081039393147,
9.05849777718431));
#74581=CARTESIAN_POINT('Ctrl Pts',(-0.417414046371677,1.97039263265711,
9.0783681207071));
#74582=CARTESIAN_POINT('Ctrl Pts',(-0.116977570492231,1.67887198647007,
9.09823846422989));
#74583=CARTESIAN_POINT('Ctrl Pts',(0.290769901255634,1.77367896129468,9.11810880775268));
#74584=CARTESIAN_POINT('Ctrl Pts',(0.43177557334904,2.16784106453351,9.13797915127547));
#74585=CARTESIAN_POINT('Ctrl Pts',(0.176685937831131,2.49976822678981,9.15784949479826));
#74586=CARTESIAN_POINT('Ctrl Pts',(-0.240488992028429,2.46496246449612,
9.17771983832104));
#74587=CARTESIAN_POINT('Ctrl Pts',(-0.437048011321802,2.09535332618026,
9.19759018184385));
#74588=CARTESIAN_POINT('Ctrl Pts',(-0.232674978941475,1.73000687850648,
9.21746052536661));
#74589=CARTESIAN_POINT('Ctrl Pts',(0.185145670779582,1.7040787497879,9.23733086888943));
#74590=CARTESIAN_POINT('Ctrl Pts',(0.433120372867424,2.04135446832782,9.2572012124122));
#74591=CARTESIAN_POINT('Ctrl Pts',(0.283766096863767,2.43242947830877,9.277071555935));
#74592=CARTESIAN_POINT('Ctrl Pts',(-0.125904941746689,2.51854569812828,
9.29694189945778));
#74593=CARTESIAN_POINT('Ctrl Pts',(-0.420075336714605,2.22070321976667,
9.31681224298058));
#74594=CARTESIAN_POINT('Ctrl Pts',(-0.328883798339925,1.81213196952868,
9.33668258650336));
#74595=CARTESIAN_POINT('Ctrl Pts',(0.0640138515255109,1.66764044755458,
9.35655293002616));
#74596=CARTESIAN_POINT('Ctrl Pts',(0.398187507315239,1.91977995451115,9.37642327354892));
#74597=CARTESIAN_POINT('Ctrl Pts',(0.367078333477388,2.33724681846001,9.39629361707175));
#74598=CARTESIAN_POINT('Ctrl Pts',(-0.000775238123413455,2.53707202470964,
9.4161639605945));
#74599=CARTESIAN_POINT('Ctrl Pts',(-0.367917634285118,2.33594315027136,
9.43603430411731));
#74600=CARTESIAN_POINT('Ctrl Pts',(-0.397545688453278,1.91836855621853,
9.45590464764009));
#74601=CARTESIAN_POINT('Ctrl Pts',(-0.0624796944239493,1.66741608494695,
9.47577499116289));
#74602=CARTESIAN_POINT('Ctrl Pts',(0.329902913397025,1.81330046475433,9.49564533468568));
#74603=CARTESIAN_POINT('Ctrl Pts',(0.419644510402349,2.22219263753232,9.51551567820846));
#74604=CARTESIAN_POINT('Ctrl Pts',(0.124419398554859,2.51898970039988,9.53538602173126));
#74605=CARTESIAN_POINT('Ctrl Pts',(-0.284943573295104,2.43142075344756,
9.55525636525406));
#74606=CARTESIAN_POINT('Ctrl Pts',(-0.432909608211464,2.03981838406849,
9.57512670877682));
#74607=CARTESIAN_POINT('Ctrl Pts',(-0.183740012915144,1.70342445431939,
9.59499705229965));
#74608=CARTESIAN_POINT('Ctrl Pts',(0.233986030286801,1.73083459884687,9.61486739582239));
#74609=CARTESIAN_POINT('Ctrl Pts',(0.437061745022211,2.09690374160118,9.63473773934522));
#74610=CARTESIAN_POINT('Ctrl Pts',(0.239192809283464,2.46581327991889,9.65460808286798));
#74611=CARTESIAN_POINT('Ctrl Pts',(-0.178102965812306,2.49913893489208,
9.67447842639079));
#74612=CARTESIAN_POINT('Ctrl Pts',(-0.432013516304637,2.16630895496111,
9.69434876991358));
#74613=CARTESIAN_POINT('Ctrl Pts',(-0.289610478916907,1.77264953600239,
9.71421911343635));
#74614=CARTESIAN_POINT('Ctrl Pts',(0.118470745970611,1.67928960301997,9.73408945695917));
#74615=CARTESIAN_POINT('Ctrl Pts',(0.417871189765774,1.97187418471803,9.75395980048193));
#74616=CARTESIAN_POINT('Ctrl Pts',(0.333931704976374,2.38199675918263,9.77383014400474));
#74617=CARTESIAN_POINT('Ctrl Pts',(-0.0563446584322808,2.53342569748929,
9.79370048752751));
#74618=CARTESIAN_POINT('Ctrl Pts',(-0.394932468361915,2.28724556393009,
9.81357083105031));
#74619=CARTESIAN_POINT('Ctrl Pts',(-0.371223503770095,1.86929311664672,
9.8334411745731));
#74620=CARTESIAN_POINT('Ctrl Pts',(-0.0069675119857552,1.66298282693393,
9.85331151809589));
#74621=CARTESIAN_POINT('Ctrl Pts',(0.363680223504416,1.85757629899345,9.87318186161868));
#74622=CARTESIAN_POINT('Ctrl Pts',(0.40070086452094,2.27456051371974,9.89305220514146));
#74623=CARTESIAN_POINT('Ctrl Pts',(0.0701330128363399,2.53140922137621,
9.91292254866427));
#74624=CARTESIAN_POINT('Ctrl Pts',(-0.324772330378065,2.39249869948212,
9.93279289218704));
#74625=CARTESIAN_POINT('Ctrl Pts',(-0.421743274230899,1.9852604409154,9.95266323570984));
#74626=CARTESIAN_POINT('Ctrl Pts',(-0.131822179139127,1.68328010742834,
9.97253357923261));
#74627=CARTESIAN_POINT('Ctrl Pts',(0.279027819343617,1.76358354408519,9.99240392275542));
#74628=CARTESIAN_POINT('Ctrl Pts',(0.433907779786064,2.15250328007904,10.0122742662782));
#74629=CARTESIAN_POINT('Ctrl Pts',(0.190736423484932,2.49325840427651,10.0321446098011));
#74630=CARTESIAN_POINT('Ctrl Pts',(-0.227409634944321,2.47325247984765,
10.0520149533238));
#74631=CARTESIAN_POINT('Ctrl Pts',(-0.43693831233838,2.11083821889525,10.0718852968466));
#74632=CARTESIAN_POINT('Ctrl Pts',(-0.245635571941848,1.73848136759673,
10.0917556403694));
#74633=CARTESIAN_POINT('Ctrl Pts',(0.171004365447838,1.69776864521061,10.1116259838922));
#74634=CARTESIAN_POINT('Ctrl Pts',(0.430771077681311,2.02604843198948,10.131496327415));
#74635=CARTESIAN_POINT('Ctrl Pts',(0.295363970328877,2.42216871482112,10.1513666709378));
#74636=CARTESIAN_POINT('Ctrl Pts',(-0.11099936962669,2.52274306111444,10.1712370144606));
#74637=CARTESIAN_POINT('Ctrl Pts',(-0.415535899149414,2.23550820010619,
10.1911073579834));
#74638=CARTESIAN_POINT('Ctrl Pts',(-0.338874811306978,1.82396301327614,
10.2109777015061));
#74639=CARTESIAN_POINT('Ctrl Pts',(0.0486577822698844,1.66564418272284,
10.2308480450289));
#74640=CARTESIAN_POINT('Ctrl Pts',(0.391553484773028,1.90578768231641,10.2507183885517));
#74641=CARTESIAN_POINT('Ctrl Pts',(0.375252170190449,2.3240945437651,10.2705887320745));
#74642=CARTESIAN_POINT('Ctrl Pts',(0.0147080754280776,2.53682516902661,
10.2904590755973));
#74643=CARTESIAN_POINT('Ctrl Pts',(-0.359328676215894,2.34882817008302,
10.3103294191201));
#74644=CARTESIAN_POINT('Ctrl Pts',(-0.403730285613773,1.93256519998473,
10.3301997626429));
#74645=CARTESIAN_POINT('Ctrl Pts',(-0.0777643208762883,1.66990086471073,
10.3500701061657));
#74646=CARTESIAN_POINT('Ctrl Pts',(0.319539821608869,1.80179393335463,10.3699404496885));
#74647=CARTESIAN_POINT('Ctrl Pts',(0.423709679186456,2.20725047105558,10.3898107932113));
#74648=CARTESIAN_POINT('Ctrl Pts',(0.139183588974562,2.51431930239623,10.409681136734));
#74649=CARTESIAN_POINT('Ctrl Pts',(-0.273024495986857,2.44130657826807,
10.4295514802568));
#74650=CARTESIAN_POINT('Ctrl Pts',(-0.434769774809129,2.05519153327387,
10.4494218237796));
#74651=CARTESIAN_POINT('Ctrl Pts',(-0.197672973804186,1.71018215637898,
10.4692921673024));
#74652=CARTESIAN_POINT('Ctrl Pts',(0.22076186992074,1.72277758209906,10.4891625108252));
#74653=CARTESIAN_POINT('Ctrl Pts',(0.436677752008117,2.0814232220483,10.509032854348));
#74654=CARTESIAN_POINT('Ctrl Pts',(0.252001244935848,2.45711052676827,10.5289031978708));
#74655=CARTESIAN_POINT('Ctrl Pts',(-0.163852097493456,2.50519753938657,
10.5487735413936));
#74656=CARTESIAN_POINT('Ctrl Pts',(-0.429393446921325,2.18157097228152,
10.5686438849163));
#74657=CARTESIAN_POINT('Ctrl Pts',(-0.301024765438089,1.78311414299329,
10.5885142284392));
#74658=CARTESIAN_POINT('Ctrl Pts',(0.103493157513323,1.67535694739481,10.6083845719619));
#74659=CARTESIAN_POINT('Ctrl Pts',(0.413070197767395,1.95715194263017,10.6282549154847));
#74660=CARTESIAN_POINT('Ctrl Pts',(0.343711565999386,2.3699905834954,10.6481252590075));
#74661=CARTESIAN_POINT('Ctrl Pts',(-0.0409556354686489,2.5351496199025,
10.6679956025303));
#74662=CARTESIAN_POINT('Ctrl Pts',(-0.388051617000489,2.30111812032046,
10.6878659460531));
#74663=CARTESIAN_POINT('Ctrl Pts',(-0.379163068391668,1.88258812510411,
10.7077362895759));
#74664=CARTESIAN_POINT('Ctrl Pts',(-0.0224440229241447,1.66350392715064,
10.7276066330987));
#74665=CARTESIAN_POINT('Ctrl Pts',(0.354864358098471,1.84484545246206,10.7474769766215));
#74666=CARTESIAN_POINT('Ctrl Pts',(0.40663300098569,2.26025653898454,10.7673473201443));
#74667=CARTESIAN_POINT('Ctrl Pts',(0.0853712235528269,2.52865406794643,
10.787217663667));
#74668=CARTESIAN_POINT('Ctrl Pts',(-0.314207029247148,2.40381984554933,
10.8070880071898));
#74669=CARTESIAN_POINT('Ctrl Pts',(-0.425543108137308,2.00027227619777,
10.8269583507126));
#74670=CARTESIAN_POINT('Ctrl Pts',(-0.146501317774399,1.68821131673115,
10.8468286942354));
#74671=CARTESIAN_POINT('Ctrl Pts',(0.266935487293065,1.75391041419663,10.8666990377582));
#74672=CARTESIAN_POINT('Ctrl Pts',(0.435495322754263,2.13709959079413,10.886569381281));
#74673=CARTESIAN_POINT('Ctrl Pts',(0.204547486923011,2.48625494349122,10.9064397248038));
#74674=CARTESIAN_POINT('Ctrl Pts',(-0.214044821534287,2.4810739693974,10.9263100683266));
#74675=CARTESIAN_POINT('Ctrl Pts',(-0.436280145805049,2.12630950691779,
10.9461804118494));
#74676=CARTESIAN_POINT('Ctrl Pts',(-0.258287830478275,1.74740965355706,
10.9660507553721));
#74677=CARTESIAN_POINT('Ctrl Pts',(0.156648406599361,1.6919634422165,10.9859210988949));
#74678=CARTESIAN_POINT('Ctrl Pts',(0.427881056376946,2.01083522348101,11.0057914424177));
#74679=CARTESIAN_POINT('Ctrl Pts',(0.306591087674502,2.41150354851348,11.0256617859405));
#74680=CARTESIAN_POINT('Ctrl Pts',(-0.0959544653616712,2.52640977516363,
11.0455321294633));
#74681=CARTESIAN_POINT('Ctrl Pts',(-0.410474859449393,2.2501430835501,11.0654024729861));
#74682=CARTESIAN_POINT('Ctrl Pts',(-0.348440451098382,1.83614055291446,
11.0852728165089));
#74683=CARTESIAN_POINT('Ctrl Pts',(0.0332406352514093,1.66419314375975,
11.1051431600317));
#74684=CARTESIAN_POINT('Ctrl Pts',(0.384427964061884,1.89203919545942,11.1250135035545));
#74685=CARTESIAN_POINT('Ctrl Pts',(0.382954970987067,2.31066097401803,11.1448838470773));
#74686=CARTESIAN_POINT('Ctrl Pts',(0.0301729266431917,2.53602998781703,
11.1647541906));
#74687=CARTESIAN_POINT('Ctrl Pts',(-0.350288670222764,2.36140084791656,
11.1846245341228));
#74688=CARTESIAN_POINT('Ctrl Pts',(-0.409408099655643,1.94697201656466,
11.2044948776456));
#74689=CARTESIAN_POINT('Ctrl Pts',(-0.0929513335343224,1.67292552713593,
11.2243652211684));
#74690=CARTESIAN_POINT('Ctrl Pts',(0.308775626923337,1.7906617256206,11.2442355646912));
#74691=CARTESIAN_POINT('Ctrl Pts',(0.427242985684624,2.19217367824504,11.264105908214));
#74692=CARTESIAN_POINT('Ctrl Pts',(0.153773068960608,2.50912882939285,11.2839762517368));
#74693=CARTESIAN_POINT('Ctrl Pts',(-0.260762704221777,2.45076397743336,
11.3038465952596));
#74694=CARTESIAN_POINT('Ctrl Pts',(-0.436084195917273,2.07062092838231,
11.3237169387824));
#74695=CARTESIAN_POINT('Ctrl Pts',(-0.211357805361098,1.71742917794104,
11.3435872823051));
#74696=CARTESIAN_POINT('Ctrl Pts',(0.207260597846932,1.71519407442444,11.3634576258279));
#74697=CARTESIAN_POINT('Ctrl Pts',(0.435745618512919,2.06596602102712,11.3833279693507));
#74698=CARTESIAN_POINT('Ctrl Pts',(0.26449335560258,2.44795951002957,11.4031983128735));
#74699=CARTESIAN_POINT('Ctrl Pts',(-0.14939555355422,2.51074751898966,11.4230686563963));
#74700=CARTESIAN_POINT('Ctrl Pts',(-0.426234380693095,2.19673059750206,
11.4429389999191));
#74701=CARTESIAN_POINT('Ctrl Pts',(-0.312061190117224,1.79397652148806,
11.4628093434419));
#74702=CARTESIAN_POINT('Ctrl Pts',(0.0883856590963718,1.67195732567414,
11.4826796869647));
#74703=CARTESIAN_POINT('Ctrl Pts',(0.407750698710001,1.94260901080609,11.5025500304875));
#74704=CARTESIAN_POINT('Ctrl Pts',(0.353059982502292,2.35764550167509,11.5224203740102));
#74705=CARTESIAN_POINT('Ctrl Pts',(-0.0255152028748612,2.53632732002498,
11.5422907175331));
#74706=CARTESIAN_POINT('Ctrl Pts',(-0.380683663195544,2.31473822285275,
11.5621610610558));
#74707=CARTESIAN_POINT('Ctrl Pts',(-0.386626687935257,1.89615604018234,
11.5820314045786));
#74708=CARTESIAN_POINT('Ctrl Pts',(-0.0378923609650846,1.6645729397954,
11.6019017481014));
#74709=CARTESIAN_POINT('Ctrl Pts',(0.34560304861143,1.83243488910469,11.6217720916242));
#74710=CARTESIAN_POINT('Ctrl Pts',(0.412054710693474,2.2457514019598,11.641642435147));
#74711=CARTESIAN_POINT('Ctrl Pts',(0.100502271897677,2.52536084577843,11.6615127786698));
#74712=CARTESIAN_POINT('Ctrl Pts',(-0.303247319215413,2.41475962124548,
11.6813831221926));
#74713=CARTESIAN_POINT('Ctrl Pts',(-0.428808778343008,2.01540929487284,
11.7012534657153));
#74714=CARTESIAN_POINT('Ctrl Pts',(-0.160996560384653,1.69365942446977,
11.7211238092381));
#74715=CARTESIAN_POINT('Ctrl Pts',(0.254508084024075,1.74467171384151,11.7409941527609));
#74716=CARTESIAN_POINT('Ctrl Pts',(0.436536209487655,2.12164933218561,11.7608644962837));
#74717=CARTESIAN_POINT('Ctrl Pts',(0.21810179178483,2.47876663553985,11.7807348398065));
#74718=CARTESIAN_POINT('Ctrl Pts',(-0.200411328002777,2.48841711520747,
11.8006051833293));
#74719=CARTESIAN_POINT('Ctrl Pts',(-0.435074337886463,2.14174776988761,
11.8204755268521));
#74720=CARTESIAN_POINT('Ctrl Pts',(-0.27061587278199,1.75678052914153,11.8403458703749));
#74721=CARTESIAN_POINT('Ctrl Pts',(0.142095814575594,1.68667042779638,11.8602162138977));
#74722=CARTESIAN_POINT('Ctrl Pts',(0.424453936658425,1.99573393920792,11.8800865574205));
#74723=CARTESIAN_POINT('Ctrl Pts',(0.317433356042753,2.40044736685377,11.8999569009432));
#74724=CARTESIAN_POINT('Ctrl Pts',(-0.0807891140929695,2.52954123762685,
11.919827244466));
#74725=CARTESIAN_POINT('Ctrl Pts',(-0.404898570493126,2.26458949963638,
11.9396975879888));
#74726=CARTESIAN_POINT('Ctrl Pts',(-0.357568710428738,1.84864930256659,
11.9595679315116));
#74727=CARTESIAN_POINT('Ctrl Pts',(0.0177817628697346,1.66328915208438,
11.9794382750344));
#74728=CARTESIAN_POINT('Ctrl Pts',(0.376819889503645,1.87855175175136,11.9993086185572));
#74729=CARTESIAN_POINT('Ctrl Pts',(0.39017706691362,2.29696297172976,12.01917896208));
#74730=CARTESIAN_POINT('Ctrl Pts',(0.0455999032414989,2.53468747923341,
12.0390493056028));
#74731=CARTESIAN_POINT('Ctrl Pts',(-0.340808963788434,2.37364540189703,
12.0589196491256));
#74732=CARTESIAN_POINT('Ctrl Pts',(-0.414572003493282,1.96157092177763,
12.0787899926484));
#74733=CARTESIAN_POINT('Ctrl Pts',(-0.108021668874934,1.67648627550999,
12.0986603361712));
#74734=CARTESIAN_POINT('Ctrl Pts',(0.297623841113879,1.77991781527464,12.1185306796939));
#74735=CARTESIAN_POINT('Ctrl Pts',(0.430239994707939,2.17698118427019,12.1384010232167));
#74736=CARTESIAN_POINT('Ctrl Pts',(0.168169525043752,2.50342479673972,12.1582713667395));
#74737=CARTESIAN_POINT('Ctrl Pts',(-0.248173589634581,2.45978107952729,
12.1781417102623));
#74738=CARTESIAN_POINT('Ctrl Pts',(-0.436851221606576,2.08608720161969,
12.1980120537851));
#74739=CARTESIAN_POINT('Ctrl Pts',(-0.224777329678093,1.72515642216957,
12.2178823973079));
#74740=CARTESIAN_POINT('Ctrl Pts',(0.19349916155983,1.70809359503374,12.2377527408307));
#74741=CARTESIAN_POINT('Ctrl Pts',(0.434266514598737,2.05055154121518,12.2576230843535));
#74742=CARTESIAN_POINT('Ctrl Pts',(0.276653460540773,2.4383717165319,12.2774934278763));
#74743=CARTESIAN_POINT('Ctrl Pts',(-0.134751480595642,2.51578190708016,
12.297363771399));
#74744=CARTESIAN_POINT('Ctrl Pts',(-0.422540283043114,2.21176880147776,
12.3172341149218));
#74745=CARTESIAN_POINT('Ctrl Pts',(-0.322705899463725,1.80522303646784,
12.3371044584446));
#74746=CARTESIAN_POINT('Ctrl Pts',(0.0731672144324927,1.66909500523883,
12.3569748019674));
#74747=CARTESIAN_POINT('Ctrl Pts',(0.401919369903692,1.92826364428534,12.3768451454902));
#74748=CARTESIAN_POINT('Ctrl Pts',(0.361965219869607,2.3449770099064,12.396715489013));
#74749=CARTESIAN_POINT('Ctrl Pts',(-0.0100427422798438,2.53695731954669,
12.4165858325358));
#74750=CARTESIAN_POINT('Ctrl Pts',(-0.372837855583444,2.32808877487038,
12.4364561760586));
#74751=CARTESIAN_POINT('Ctrl Pts',(-0.393604993679923,1.90997983073326,
12.4563265195813));
#74752=CARTESIAN_POINT('Ctrl Pts',(-0.0532931345563228,1.66618852298828,
12.4761968631042));
#74753=CARTESIAN_POINT('Ctrl Pts',(0.335907920317574,1.82036018730185,12.4960672066269));
#74754=CARTESIAN_POINT('Ctrl Pts',(0.416959188034086,2.23106331024313,12.5159375501497));
#74755=CARTESIAN_POINT('Ctrl Pts',(0.115507164597036,2.52153368869485,12.5358078936725));
#74756=CARTESIAN_POINT('Ctrl Pts',(-0.291906957477275,2.42530429439879,
12.5556782371953));
#74757=CARTESIAN_POINT('Ctrl Pts',(-0.431536185610004,2.0306524961725,12.5755485807181));
#74758=CARTESIAN_POINT('Ctrl Pts',(-0.175289711792273,1.69961759189781,
12.5954189242409));
#74759=CARTESIAN_POINT('Ctrl Pts',(0.241761209055436,1.73587903991396,12.6152892677637));
#74760=CARTESIAN_POINT('Ctrl Pts',(0.437029133411453,2.10617189821653,12.6351596112864));
#74761=CARTESIAN_POINT('Ctrl Pts',(0.231382324006401,2.47080288013349,12.6550299548093));
#74762=CARTESIAN_POINT('Ctrl Pts',(-0.186526267815305,2.4952726997818,12.674900298332));
#74763=CARTESIAN_POINT('Ctrl Pts',(-0.43332240217526,2.15713362889919,12.6947706418548));
#74764=CARTESIAN_POINT('Ctrl Pts',(-0.282604224056764,1.76658223154287,
12.7146409853776));
#74765=CARTESIAN_POINT('Ctrl Pts',(0.127364856541248,1.6818962460154,12.7345113289004));
#74766=CARTESIAN_POINT('Ctrl Pts',(0.420494020425157,1.98076353508279,12.7543816724232));
#74767=CARTESIAN_POINT('Ctrl Pts',(0.327877165654917,2.38901404813226,12.774252015946));
#74768=CARTESIAN_POINT('Ctrl Pts',(-0.0655223521471513,2.53213351773121,
12.7941223594688));
#74769=CARTESIAN_POINT('Ctrl Pts',(-0.398814031938348,2.27882931447587,
12.8139927029916));
#74770=CARTESIAN_POINT('Ctrl Pts',(-0.366248131012719,1.86147356060571,
12.8338630465143));
#74771=CARTESIAN_POINT('Ctrl Pts',(0.00230056985709836,1.66293334242961,
12.8537333900371));
#74772=CARTESIAN_POINT('Ctrl Pts',(0.368738811230028,1.8653422813367,12.8736037335599));
#74773=CARTESIAN_POINT('Ctrl Pts',(0.396909392261523,2.28301773132501,12.8934740770827));
#74774=CARTESIAN_POINT('Ctrl Pts',(0.0609696407939242,2.53279932849204,
12.9133444206055));
#74775=CARTESIAN_POINT('Ctrl Pts',(-0.330901456925757,2.38554646196952,
12.9332147641282));
#74776=CARTESIAN_POINT('Ctrl Pts',(-0.419215513980957,1.97634359043503,
12.9530851076511));
#74777=CARTESIAN_POINT('Ctrl Pts',(-0.122956412042968,1.68057863998248,
12.9729554511739));
#74778=CARTESIAN_POINT('Ctrl Pts',(0.286098466731769,1.76957568904242,12.9928257946967));
#74779=CARTESIAN_POINT('Ctrl Pts',(0.432696936064204,2.16169205873702,13.0126961382195));
#74780=CARTESIAN_POINT('Ctrl Pts',(0.182354901824367,2.49721436596937,13.0325664817423));
#74781=CARTESIAN_POINT('Ctrl Pts',(-0.235272985115168,2.46834656285919,
13.052436825265));
#74782=CARTESIAN_POINT('Ctrl Pts',(-0.437069830553411,2.10157094461754,
13.0723071687878));
#74783=CARTESIAN_POINT('Ctrl Pts',(-0.237914814564311,1.73335417845672,
13.0921775123106));
#74784=CARTESIAN_POINT('Ctrl Pts',(0.179495052151714,1.70148507794555,13.1120478558334));
#74785=CARTESIAN_POINT('Ctrl Pts',(0.432241878947184,2.03519909097049,13.1319181993562));
#74786=CARTESIAN_POINT('Ctrl Pts',(0.288467100709767,2.42835925974009,13.151788542879));
#74787=CARTESIAN_POINT('Ctrl Pts',(-0.119939810852905,2.52029423330114,
13.1716588864018));
#74788=CARTESIAN_POINT('Ctrl Pts',(-0.418312805424477,2.22666699815582,
13.1915292299246));
#74789=CARTESIAN_POINT('Ctrl Pts',(-0.332951281535073,1.81683901091653,
13.2113995734473));
#74790=CARTESIAN_POINT('Ctrl Pts',(0.0578680000586412,1.66677465713648,
13.2312699169702));
#74791=CARTESIAN_POINT('Ctrl Pts',(0.395562204268459,1.91413177388155,13.2511402604929));
#74792=CARTESIAN_POINT('Ctrl Pts',(0.370457177876832,2.33200500809455,13.2710106040157));
#74793=CARTESIAN_POINT('Ctrl Pts',(0.00536316449256819,2.537031136083,13.2908809475385));
#74794=CARTESIAN_POINT('Ctrl Pts',(-0.364371131947823,2.34116775930325,
13.3107512910613));
#74795=CARTESIAN_POINT('Ctrl Pts',(-0.400388031600374,1.92401443108959,
13.3306216345841));
#74796=CARTESIAN_POINT('Ctrl Pts',(-0.0680109136702867,1.66839569599009,
13.3504919781069));
#74797=CARTESIAN_POINT('Ctrl Pts',(0.193487360962402,1.76186082371239,13.3637388737887));
#74798=CARTESIAN_POINT('Ctrl Pts',(0.275524381335433,1.85359137675596,13.3703623216297));
#74799=CARTESIAN_POINT('Ctrl Pts',(-0.324703122987632,1.98145546592675,
4.34318193730108));
#74800=CARTESIAN_POINT('Ctrl Pts',(-0.285214820824608,1.87327603739136,
4.34980982121868));
#74801=CARTESIAN_POINT('Ctrl Pts',(-0.0903122625737519,1.70146708514356,
4.36306115297722));
#74802=CARTESIAN_POINT('Ctrl Pts',(0.286975972182973,1.80858593652704,4.38293593257671));
#74803=CARTESIAN_POINT('Ctrl Pts',(0.400001189849452,2.18347131865804,4.40280627609948));
#74804=CARTESIAN_POINT('Ctrl Pts',(0.146534207579467,2.48155047238696,4.42267661962228));
#74805=CARTESIAN_POINT('Ctrl Pts',(-0.241591594009944,2.42972928699582,
4.44254696314506));
#74806=CARTESIAN_POINT('Ctrl Pts',(-0.407968932804969,2.07536397308355,
4.46241730666785));
#74807=CARTESIAN_POINT('Ctrl Pts',(-0.200153151725138,1.74363125289821,
4.48228765019064));
#74808=CARTESIAN_POINT('Ctrl Pts',(0.191308522101233,1.73880152376249,4.50215799371343));
#74809=CARTESIAN_POINT('Ctrl Pts',(0.407253731465132,2.06533095703686,4.52202833723622));
#74810=CARTESIAN_POINT('Ctrl Pts',(0.249607880621845,2.42365998281579,4.54189868075901));
#74811=CARTESIAN_POINT('Ctrl Pts',(-0.137023786820888,2.48507739127738,
4.56176902428181));
#74812=CARTESIAN_POINT('Ctrl Pts',(-0.397952412483378,2.19323749418965,
4.58163936780458));
#74813=CARTESIAN_POINT('Ctrl Pts',(-0.293815107395566,1.81586552415182,
4.60150971132738));
#74814=CARTESIAN_POINT('Ctrl Pts',(0.0798581987962179,1.69914792465702,
4.62138005485017));
#74815=CARTESIAN_POINT('Ctrl Pts',(0.380272147308599,1.9501577043663,4.64125039837296));
#74816=CARTESIAN_POINT('Ctrl Pts',(0.331838342430293,2.33862730225961,4.66112074189575));
#74817=CARTESIAN_POINT('Ctrl Pts',(-0.0210120554276185,2.5081888826504,
4.68099108541854));
#74818=CARTESIAN_POINT('Ctrl Pts',(-0.354586706485803,2.30329270914637,
4.70086142894133));
#74819=CARTESIAN_POINT('Ctrl Pts',(-0.362876351097746,1.91190316324567,
4.72073177246412));
#74820=CARTESIAN_POINT('Ctrl Pts',(-0.0382763322007111,1.69306685153467,
4.7406021159869));
#74821=CARTESIAN_POINT('Ctrl Pts',(0.321437004131683,1.84753630794944,4.76047245950971));
#74822=CARTESIAN_POINT('Ctrl Pts',(0.386275652248465,2.23360683025069,4.78034280303248));
#74823=CARTESIAN_POINT('Ctrl Pts',(0.0967589743544941,2.49711127562884,
4.80021314655528));
#74824=CARTESIAN_POINT('Ctrl Pts',(-0.28152088905393,2.39632018696635,4.82008349007806));
#74825=CARTESIAN_POINT('Ctrl Pts',(-0.401543662836625,2.02369566735683,
4.83995383360086));
#74826=CARTESIAN_POINT('Ctrl Pts',(-0.153204790954587,1.72106998492393,
4.85982417712364));
#74827=CARTESIAN_POINT('Ctrl Pts',(0.235678619551842,1.76606100472576,4.87969452064644));
#74828=CARTESIAN_POINT('Ctrl Pts',(0.408358981432492,2.11739559096851,4.89956486416922));
#74829=CARTESIAN_POINT('Ctrl Pts',(0.206425570869757,2.45277209071125,4.91943520769201));
#74830=CARTESIAN_POINT('Ctrl Pts',(-0.184875198644271,2.46452822280067,
4.9393055512148));
#74831=CARTESIAN_POINT('Ctrl Pts',(-0.406578141897051,2.14187933651161,
4.95917589473759));
#74832=CARTESIAN_POINT('Ctrl Pts',(-0.255300990570369,1.78081186032747,
4.97904623826038));
#74833=CARTESIAN_POINT('Ctrl Pts',(0.130180063510712,1.7125560487528,4.99891658178317));
#74834=CARTESIAN_POINT('Ctrl Pts',(0.396238631737338,1.99972731671569,5.01878692530596));
#74835=CARTESIAN_POINT('Ctrl Pts',(0.298802198362976,2.37888512069913,5.03865726882875));
#74836=CARTESIAN_POINT('Ctrl Pts',(-0.0727445737629762,2.50220379322174,
5.05852761235154));
#74837=CARTESIAN_POINT('Ctrl Pts',(-0.377558102741037,2.25655524056561,
5.07839795587433));
#74838=CARTESIAN_POINT('Ctrl Pts',(-0.336013472348416,1.86728856776192,
5.09826829939711));
#74839=CARTESIAN_POINT('Ctrl Pts',(0.013777774820227,1.69150295323597,5.11813864291991));
#74840=CARTESIAN_POINT('Ctrl Pts',(0.350929789266008,1.89045776726478,5.13800898644269));
#74841=CARTESIAN_POINT('Ctrl Pts',(0.366151496836993,2.28163905322912,5.15787932996549));
#74842=CARTESIAN_POINT('Ctrl Pts',(0.045479053085185,2.50619123577992,5.17774967348827));
#74843=CARTESIAN_POINT('Ctrl Pts',(-0.316914230458285,2.35811825744603,
5.19762001701106));
#74844=CARTESIAN_POINT('Ctrl Pts',(-0.388581851532883,1.97325691753307,
5.21749036053385));
#74845=CARTESIAN_POINT('Ctrl Pts',(-0.103778524468258,1.70466510127092,
5.23736070405664));
#74846=CARTESIAN_POINT('Ctrl Pts',(0.276227470625653,1.79873923460613,5.25723104757944));
#74847=CARTESIAN_POINT('Ctrl Pts',(0.40283236639495,2.16917910724046,5.27710139110222));
#74848=CARTESIAN_POINT('Ctrl Pts',(0.159893406671488,2.47615656686668,5.29697173462502));
#74849=CARTESIAN_POINT('Ctrl Pts',(-0.229725986151337,2.43806158548516,
5.31684207814779));
#74850=CARTESIAN_POINT('Ctrl Pts',(-0.408603061049272,2.08984112235003,
5.33671242167059));
#74851=CARTESIAN_POINT('Ctrl Pts',(-0.212642453718247,1.75094004645244,
5.35658276519338));
#74852=CARTESIAN_POINT('Ctrl Pts',(0.178388656243237,1.73225395771311,5.37645310871617));
#74853=CARTESIAN_POINT('Ctrl Pts',(0.405772459524144,2.05092479866909,5.39632345223896));
#74854=CARTESIAN_POINT('Ctrl Pts',(0.260915272123794,2.41461545586081,5.41619379576174));
#74855=CARTESIAN_POINT('Ctrl Pts',(-0.123296157043305,2.48968926332694,
5.43606413928454));
#74856=CARTESIAN_POINT('Ctrl Pts',(-0.394400147379255,2.2072762230933,5.45593448280733));
#74857=CARTESIAN_POINT('Ctrl Pts',(-0.303695695226391,1.82645185251057,
5.4758048263301));
#74858=CARTESIAN_POINT('Ctrl Pts',(0.0656082128611597,1.69657066703188,
5.49567516985291));
#74859=CARTESIAN_POINT('Ctrl Pts',(0.374725517400243,1.93678097260717,5.51554551337569));
#74860=CARTESIAN_POINT('Ctrl Pts',(0.340083173997246,2.32672251555128,5.53541585689848));
#74861=CARTESIAN_POINT('Ctrl Pts',(-0.00653918340477464,2.50867701596045,
5.55528620042128));
#74862=CARTESIAN_POINT('Ctrl Pts',(-0.347162730262346,2.31572599057771,
5.57515654394406));
#74863=CARTESIAN_POINT('Ctrl Pts',(-0.369311734042224,1.92487573728159,
5.59502688746686));
#74864=CARTESIAN_POINT('Ctrl Pts',(-0.0526674990909465,1.69467815401406,
5.61489723098964));
#74865=CARTESIAN_POINT('Ctrl Pts',(0.31229199624372,1.83630818485199,5.63476757451243));
#74866=CARTESIAN_POINT('Ctrl Pts',(0.390766099741013,2.21983955768918,5.65463791803522));
#74867=CARTESIAN_POINT('Ctrl Pts',(0.110765504726666,2.49343445102912,5.67450826155801));
#74868=CARTESIAN_POINT('Ctrl Pts',(-0.270847361512589,2.40610679681381,
5.6943786050808));
#74869=CARTESIAN_POINT('Ctrl Pts',(-0.403994646102744,2.03796782919919,
5.71424894860358));
#74870=CARTESIAN_POINT('Ctrl Pts',(-0.166531841798338,1.72673493337684,
5.73411929212638));
#74871=CARTESIAN_POINT('Ctrl Pts',(0.223701256092982,1.75792192073101,5.75398963564917));
#74872=CARTESIAN_POINT('Ctrl Pts',(0.408718905695017,2.1029189760892,5.77385997917195));
#74873=CARTESIAN_POINT('Ctrl Pts',(0.218792601376446,2.44523826826826,5.79373032269475));
#74874=CARTESIAN_POINT('Ctrl Pts',(-0.171846128781984,2.47084844925736,
5.81360066621753));
#74875=CARTESIAN_POINT('Ctrl Pts',(-0.404839430520849,2.1562556645103,5.83347100974033));
#74876=CARTESIAN_POINT('Ctrl Pts',(-0.266447668668554,1.79005596609221,
5.85334135326312));
#74877=CARTESIAN_POINT('Ctrl Pts',(0.116373555612529,1.70818772371448,5.8732116967859));
#74878=CARTESIAN_POINT('Ctrl Pts',(0.392437885448118,1.98575390440391,5.8930820403087));
#74879=CARTESIAN_POINT('Ctrl Pts',(0.308493880978865,2.36812532460127,5.91295238383148));
#74880=CARTESIAN_POINT('Ctrl Pts',(-0.0584512616389577,2.50452826144382,
5.93282272735428));
#74881=CARTESIAN_POINT('Ctrl Pts',(-0.371775329123761,2.26983158996152,
5.95269307087706));
#74882=CARTESIAN_POINT('Ctrl Pts',(-0.344046144778287,1.87933755517274,
5.97256341439985));
#74883=CARTESIAN_POINT('Ctrl Pts',(-0.00070146025194062,1.69127127303375,
5.99243375792264));
#74884=CARTESIAN_POINT('Ctrl Pts',(0.343286718560372,1.87815795449466,6.01230410144543));
#74885=CARTESIAN_POINT('Ctrl Pts',(0.372356067360204,2.26855451163937,6.0321744449682));
#74886=CARTESIAN_POINT('Ctrl Pts',(0.059839416058191,2.50432525097965,6.05204478849101));
#74887=CARTESIAN_POINT('Ctrl Pts',(-0.307571753076327,2.3691826164586,6.0719151320138));
#74888=CARTESIAN_POINT('Ctrl Pts',(-0.392827710876478,1.98710157724091,
6.09178547553659));
#74889=CARTESIAN_POINT('Ctrl Pts',(-0.117717722611208,1.70858947117231,
6.11165581905938));
#74890=CARTESIAN_POINT('Ctrl Pts',(0.265382250329029,1.78914323957127,6.13152616258216));
#74891=CARTESIAN_POINT('Ctrl Pts',(0.405030137123385,2.15486576633707,6.15139650610496));
#74892=CARTESIAN_POINT('Ctrl Pts',(0.173118012981109,2.47025642178822,6.17126684962775));
#74893=CARTESIAN_POINT('Ctrl Pts',(-0.217606320182031,2.44598721610888,
6.19113719315053));
#74894=CARTESIAN_POINT('Ctrl Pts',(-0.408706479003584,2.10432184155586,
6.21100753667333));
#74895=CARTESIAN_POINT('Ctrl Pts',(-0.224874083702182,1.75869176574093,
6.23087788019611));
#74896=CARTESIAN_POINT('Ctrl Pts',(0.165249669553886,1.72616552993835,6.25074822371891));
#74897=CARTESIAN_POINT('Ctrl Pts',(0.403779347705335,2.03658152744984,6.27061856724169));
#74898=CARTESIAN_POINT('Ctrl Pts',(0.271896443931615,2.40517533988068,6.29048891076448));
#74899=CARTESIAN_POINT('Ctrl Pts',(-0.109414431790982,2.49381232384195,
6.31035925428728));
#74900=CARTESIAN_POINT('Ctrl Pts',(-0.390352461775193,2.22118011338494,
6.33022959781006));
#74901=CARTESIAN_POINT('Ctrl Pts',(-0.313195249769681,1.83738164608,6.35009994133285));
#74902=CARTESIAN_POINT('Ctrl Pts',(0.0512759662164159,1.69449976623618,
6.36997028485564));
#74903=CARTESIAN_POINT('Ctrl Pts',(0.368708463791405,1.92360914699871,6.38984062837843));
#74904=CARTESIAN_POINT('Ctrl Pts',(0.347901140962541,2.31453312194368,6.40971097190122));
#74905=CARTESIAN_POINT('Ctrl Pts',(0.00794188376409148,2.5086521635526,
6.42958131542401));
#74906=CARTESIAN_POINT('Ctrl Pts',(-0.339302970598069,2.32788847807045,
6.4494516589468));
#74907=CARTESIAN_POINT('Ctrl Pts',(-0.375283541364848,1.9380681381735,6.46932200246958));
#74908=CARTESIAN_POINT('Ctrl Pts',(-0.0669925531701256,1.69679823647001,
6.48919234599238));
#74909=CARTESIAN_POINT('Ctrl Pts',(0.302754982345627,1.82541106184181,6.50906268951516));
#74910=CARTESIAN_POINT('Ctrl Pts',(0.394766037928299,2.20592185606538,6.52893303303795));
#74911=CARTESIAN_POINT('Ctrl Pts',(0.124632996254909,2.48926376730755,6.54880337656074));
#74912=CARTESIAN_POINT('Ctrl Pts',(-0.259833852232052,2.41550916552169,
6.56867372008354));
#74913=CARTESIAN_POINT('Ctrl Pts',(-0.405938514480912,2.05231785706397,
6.58854406360632));
#74914=CARTESIAN_POINT('Ctrl Pts',(-0.179649853232024,1.73286842341246,
6.60841440712912));
#74915=CARTESIAN_POINT('Ctrl Pts',(0.21144309123819,1.75021223082906,6.6282847506519));
#74916=CARTESIAN_POINT('Ctrl Pts',(0.408565784874935,2.08843869715522,6.64815509417468));
#74917=CARTESIAN_POINT('Ctrl Pts',(0.230884992097985,2.4372710849122,6.66802543769748));
#74918=CARTESIAN_POINT('Ctrl Pts',(-0.158601348775496,2.47670316757433,
6.68789578122028));
#74919=CARTESIAN_POINT('Ctrl Pts',(-0.402592543771387,2.17056137749241,
6.70776612474306));
#74920=CARTESIAN_POINT('Ctrl Pts',(-0.277259887882735,1.79968912962533,
6.72763646826585));
#74921=CARTESIAN_POINT('Ctrl Pts',(0.102420969612983,1.70431122169376,6.74750681178864));
#74922=CARTESIAN_POINT('Ctrl Pts',(0.388144530844729,1.97192389969527,6.76737715531141));
#74923=CARTESIAN_POINT('Ctrl Pts',(0.317798326132794,2.35702896373975,6.78724749883422));
#74924=CARTESIAN_POINT('Ctrl Pts',(-0.0440845784706122,2.50634494488675,
6.807117842357));
#74925=CARTESIAN_POINT('Ctrl Pts',(-0.365525883900656,2.28289475796913,
6.8269881858798));
#74926=CARTESIAN_POINT('Ctrl Pts',(-0.351646952707478,1.89166352948779,
6.84685852940258));
#74927=CARTESIAN_POINT('Ctrl Pts',(-0.0151798148149533,1.69155265025205,
6.86672887292538));
#74928=CARTESIAN_POINT('Ctrl Pts',(0.335212736625109,1.86613660932448,6.88659921644816));
#74929=CARTESIAN_POINT('Ctrl Pts',(0.378093237304912,2.25525839171599,6.90646955997095));
#74930=CARTESIAN_POINT('Ctrl Pts',(0.0741246655037585,2.50195173622948,
6.92633990349375));
#74931=CARTESIAN_POINT('Ctrl Pts',(-0.297843195735107,2.37990908354007,
6.94621024701653));
#74932=CARTESIAN_POINT('Ctrl Pts',(-0.396580472576683,2.00108795288341,
6.96608059053932));
#74933=CARTESIAN_POINT('Ctrl Pts',(-0.131509155385276,1.71300515979694,
6.98595093406212));
#74934=CARTESIAN_POINT('Ctrl Pts',(0.254203908517277,1.77993744800668,7.0058212775849));
#74935=CARTESIAN_POINT('Ctrl Pts',(0.406719493092408,2.1404835550884,7.0256916211077));
#74936=CARTESIAN_POINT('Ctrl Pts',(0.186125312614382,2.46389151171488,7.04556196463048));
#74937=CARTESIAN_POINT('Ctrl Pts',(-0.205213503514097,2.4534785456989,7.06543230815328));
#74938=CARTESIAN_POINT('Ctrl Pts',(-0.408296867464171,2.11879713576282,
7.08530265167605));
#74939=CARTESIAN_POINT('Ctrl Pts',(-0.236823440115126,1.76687191276331,
7.10517299519885));
#74940=CARTESIAN_POINT('Ctrl Pts',(0.151903252939481,1.72054635850957,7.12504333872164));
#74941=CARTESIAN_POINT('Ctrl Pts',(0.401279391182633,2.0223178623747,7.14491368224442));
#74942=CARTESIAN_POINT('Ctrl Pts',(0.282536317271847,2.39535215204295,7.16478402576722));
#74943=CARTESIAN_POINT('Ctrl Pts',(-0.0953953638895205,2.49744105077651,
7.18465436928999));
#74944=CARTESIAN_POINT('Ctrl Pts',(-0.38581478558834,2.23493189213586,7.20452471281281));
#74945=CARTESIAN_POINT('Ctrl Pts',(-0.322301665450036,1.84864109177896,
7.22439505633558));
#74946=CARTESIAN_POINT('Ctrl Pts',(0.0368793553290216,1.69293787028949,
7.24426539985838));
#74947=CARTESIAN_POINT('Ctrl Pts',(0.36222858826457,1.91065873630452,7.26413574338117));
#74948=CARTESIAN_POINT('Ctrl Pts',(0.355282404436738,2.3020744352747,7.28400608690396));
#74949=CARTESIAN_POINT('Ctrl Pts',(0.0224129818700309,2.50811434983058,
7.30387643042674));
#74950=CARTESIAN_POINT('Ctrl Pts',(-0.331017300310477,2.33976490816863,
7.32374677394954));
#74951=CARTESIAN_POINT('Ctrl Pts',(-0.380784273392315,1.95146380430673,
7.34361711747232));
#74952=CARTESIAN_POINT('Ctrl Pts',(-0.0812335147344956,1.69942443861635,
7.36348746099511));
#74953=CARTESIAN_POINT('Ctrl Pts',(0.29283793474781,1.81485861705711,7.38335780451791));
#74954=CARTESIAN_POINT('Ctrl Pts',(0.398270445383918,2.19187119585397,7.40322814804069));
#74955=CARTESIAN_POINT('Ctrl Pts',(0.138344042005423,2.48460445958874,7.42309849156349));
#74956=CARTESIAN_POINT('Ctrl Pts',(-0.248494186072408,2.42451549082001,
7.44296883508627));
#74957=CARTESIAN_POINT('Ctrl Pts',(-0.407372827857467,2.06672773801869,
7.46283917860906));
#74958=CARTESIAN_POINT('Ctrl Pts',(-0.19254235888592,1.73946275597577,7.48270952213185));
#74959=CARTESIAN_POINT('Ctrl Pts',(0.198919512088243,1.74294161261145,7.50257986565464));
#74960=CARTESIAN_POINT('Ctrl Pts',(0.407899811167672,2.07397293056604,7.52245020917743));
#74961=CARTESIAN_POINT('Ctrl Pts',(0.242687564045679,2.42888054146076,7.54232055270022));
#74962=CARTESIAN_POINT('Ctrl Pts',(-0.145157484159772,2.48208502860796,
7.56219089622301));
#74963=CARTESIAN_POINT('Ctrl Pts',(-0.399840302055658,2.184778518187,7.58206123974579));
#74964=CARTESIAN_POINT('Ctrl Pts',(-0.287724076157312,1.80969925888251,
7.60193158326859));
#74965=CARTESIAN_POINT('Ctrl Pts',(0.0883398195194317,1.70093140867613,
7.62180192679138));
#74966=CARTESIAN_POINT('Ctrl Pts',(0.38336395716755,1.9582546627265,7.64167227031415));
#74967=CARTESIAN_POINT('Ctrl Pts',(0.326703854404464,2.34560996684013,7.66154261383696));
#74968=CARTESIAN_POINT('Ctrl Pts',(-0.0296625580611567,2.5076515631556,
7.68141295735974));
#74969=CARTESIAN_POINT('Ctrl Pts',(-0.358817611698299,2.29572834702483,
7.70128330088253));
#74970=CARTESIAN_POINT('Ctrl Pts',(-0.358806355209093,1.9042510185071,7.72115364440532));
#74971=CARTESIAN_POINT('Ctrl Pts',(-0.0296391148899432,1.69234673169165,
7.74102398792811));
#74972=CARTESIAN_POINT('Ctrl Pts',(0.32671797833959,1.85440882156797,7.76089433145089));
#74973=CARTESIAN_POINT('Ctrl Pts',(0.383355805078912,2.24176738343583,7.78076467497369));
#74974=CARTESIAN_POINT('Ctrl Pts',(0.0883168698385477,2.4990736708878,7.80063501849648));
#74975=CARTESIAN_POINT('Ctrl Pts',(-0.287740770222548,2.39028419427463,
7.82050536201926));
#74976=CARTESIAN_POINT('Ctrl Pts',(-0.399835425973084,2.01519848803905,
7.84037570554206));
#74977=CARTESIAN_POINT('Ctrl Pts',(-0.14513551107133,1.71790662434425,7.86024604906485));
#74978=CARTESIAN_POINT('Ctrl Pts',(0.242706476822712,1.77113341549764,7.88011639258762));
#74979=CARTESIAN_POINT('Ctrl Pts',(0.407898313735106,2.12605052678927,7.89998673611043));
#74980=CARTESIAN_POINT('Ctrl Pts',(0.198898978136607,2.45706982621072,7.91985707963321));
#74981=CARTESIAN_POINT('Ctrl Pts',(-0.19256309225145,2.46052617075117,7.93972742315602));
#74982=CARTESIAN_POINT('Ctrl Pts',(-0.407374740596605,2.13324883483357,
7.95959776667879));
#74983=CARTESIAN_POINT('Ctrl Pts',(-0.248475523507394,1.7754702193763,7.97946811020159));
#74984=CARTESIAN_POINT('Ctrl Pts',(0.138366159511869,1.71540349690113,7.99933845372437));
#74985=CARTESIAN_POINT('Ctrl Pts',(0.398275728030659,2.00815170793318,8.01920879724717));
#74986=CARTESIAN_POINT('Ctrl Pts',(0.292821536425625,2.38515822292067,8.03907914076994));
#74987=CARTESIAN_POINT('Ctrl Pts',(-0.0812565507974271,2.500570889165,8.05894948429274));
#74988=CARTESIAN_POINT('Ctrl Pts',(-0.380792814744337,2.24851429740273,
8.07881982781553));
#74989=CARTESIAN_POINT('Ctrl Pts',(-0.331003511423903,1.86021605616934,
8.09869017133833));
#74990=CARTESIAN_POINT('Ctrl Pts',(0.0224364515689504,1.69188693976432,
8.11856051486111));
#74991=CARTESIAN_POINT('Ctrl Pts',(0.35529402469436,1.89794599654937,8.13843085838391));
#74992=CARTESIAN_POINT('Ctrl Pts',(0.362217699076477,2.28936209433169,8.15830120190667));
#74993=CARTESIAN_POINT('Ctrl Pts',(0.0368559460428643,2.50706424988597,
8.17817154542949));
#74994=CARTESIAN_POINT('Ctrl Pts',(-0.3223161200011,2.3513403729634,8.19804188895226));
#74995=CARTESIAN_POINT('Ctrl Pts',(-0.385807025321515,1.96504592074892,
8.21791223247506));
#74996=CARTESIAN_POINT('Ctrl Pts',(-0.0953725077931551,1.70255346390843,
8.23778257599785));
#74997=CARTESIAN_POINT('Ctrl Pts',(0.282553301840913,1.80466409647193,8.25765291952063));
#74998=CARTESIAN_POINT('Ctrl Pts',(0.401274923194525,2.17770521416978,8.27752326304343));
#74999=CARTESIAN_POINT('Ctrl Pts',(0.151881431165022,2.47946237647651,8.29739360656621));
#75000=CARTESIAN_POINT('Ctrl Pts',(-0.236842597168632,2.43311446750383,
8.317263950089));
#75001=CARTESIAN_POINT('Ctrl Pts',(-0.408295785808135,2.08117938403611,
8.3371342936118));
#75002=CARTESIAN_POINT('Ctrl Pts',(-0.205193175420671,1.74650965351976,
8.35700463713457));
#75003=CARTESIAN_POINT('Ctrl Pts',(0.186146238886892,1.73611919253387,8.37687498065739));
#75004=CARTESIAN_POINT('Ctrl Pts',(0.406721820537833,2.05953983449946,8.39674532418016));
#75005=CARTESIAN_POINT('Ctrl Pts',(0.254185502021292,2.42007717015764,8.41661566770295));
#75006=CARTESIAN_POINT('Ctrl Pts',(-0.131531410368423,2.48698727676816,
8.43648601122574));
#75007=CARTESIAN_POINT('Ctrl Pts',(-0.396586160129697,2.19888924050433,
8.45635635474853));
#75008=CARTESIAN_POINT('Ctrl Pts',(-0.297827098302388,1.82007378863221,
8.47622669827132));
#75009=CARTESIAN_POINT('Ctrl Pts',(0.0741477807191584,1.69805252717754,
8.49609704179411));
#75010=CARTESIAN_POINT('Ctrl Pts',(0.378102165239712,1.94476335183023,8.5159673853169));
#75011=CARTESIAN_POINT('Ctrl Pts',(0.335199287114567,2.3338826676174,8.53583772883967));
#75012=CARTESIAN_POINT('Ctrl Pts',(-0.0152033036759094,2.50844647611563,
8.55570807236248));
#75013=CARTESIAN_POINT('Ctrl Pts',(-0.351658933086634,2.30831624774441,
8.57557841588528));
#75014=CARTESIAN_POINT('Ctrl Pts',(-0.36551536543112,1.91708422176396,8.59544875940805));
#75015=CARTESIAN_POINT('Ctrl Pts',(-0.0440612104162264,1.69365252058048,
8.61531910293085));
#75016=CARTESIAN_POINT('Ctrl Pts',(0.317813106763408,1.84298931255037,8.63518944645363));
#75017=CARTESIAN_POINT('Ctrl Pts',(0.38813716483518,2.22809842140966,8.65505978997641));
#75018=CARTESIAN_POINT('Ctrl Pts',(0.102398214274245,2.49569466765094,8.67493013349922));
#75019=CARTESIAN_POINT('Ctrl Pts',(-0.277277157625239,2.40029492528715,
8.69480047702201));
#75020=CARTESIAN_POINT('Ctrl Pts',(-0.402588485279962,2.0294154704349,8.71467082054478));
#75021=CARTESIAN_POINT('Ctrl Pts',(-0.15857968516352,1.72328771224265,8.73454116406759));
#75022=CARTESIAN_POINT('Ctrl Pts',(0.230904387415763,1.76274219332076,8.75441150759036));
#75023=CARTESIAN_POINT('Ctrl Pts',(0.408565119334887,2.11158479852265,8.77428185111318));
#75024=CARTESIAN_POINT('Ctrl Pts',(0.211422975382705,2.44979992820792,8.79415219463594));
#75025=CARTESIAN_POINT('Ctrl Pts',(-0.179670965844065,2.4671212447225,8.81402253815874));
#75026=CARTESIAN_POINT('Ctrl Pts',(-0.405941255902183,2.14765879824859,
8.83389288168152));
#75027=CARTESIAN_POINT('Ctrl Pts',(-0.259815707581749,1.7844758925411,8.85376322520432));
#75028=CARTESIAN_POINT('Ctrl Pts',(0.124655381730304,1.7107434006987,8.87363356872711));
#75029=CARTESIAN_POINT('Ctrl Pts',(0.394772128602621,1.99410084621444,8.8935039122499));
#75030=CARTESIAN_POINT('Ctrl Pts',(0.302739190854349,2.37460634846047,8.91337425577268));
#75031=CARTESIAN_POINT('Ctrl Pts',(-0.0670157402835653,2.5031979102726,
8.93324459929548));
#75032=CARTESIAN_POINT('Ctrl Pts',(-0.375292853080517,2.26191027984853,
8.95311494281827));
#75033=CARTESIAN_POINT('Ctrl Pts',(-0.339289864684512,1.87209200975764,
8.97298528634106));
#75034=CARTESIAN_POINT('Ctrl Pts',(0.00796538441539088,1.69134829384296,
8.99285562986384));
#75035=CARTESIAN_POINT('Ctrl Pts',(0.347913477703343,1.88548688542118,9.01272597338664));
#75036=CARTESIAN_POINT('Ctrl Pts',(0.368698319341517,2.27641205630196,9.03259631690941));
#75037=CARTESIAN_POINT('Ctrl Pts',(0.0512526467275652,2.50550318185849,
9.05246666043221));
#75038=CARTESIAN_POINT('Ctrl Pts',(-0.313210351841129,2.36260034233317,
9.07233700395502));
#75039=CARTESIAN_POINT('Ctrl Pts',(-0.390345492334655,1.97879743852559,
9.09220734747776));
#75040=CARTESIAN_POINT('Ctrl Pts',(-0.109391784351346,1.70618138463199,
9.1120776910006));
#75041=CARTESIAN_POINT('Ctrl Pts',(0.271913993427649,1.79484029677533,9.13194803452336));
#75042=CARTESIAN_POINT('Ctrl Pts',(0.403775699984309,2.16344169288507,9.15181837804616));
#75043=CARTESIAN_POINT('Ctrl Pts',(0.165228170903243,2.47384397257935,9.17168872156895));
#75044=CARTESIAN_POINT('Ctrl Pts',(-0.224893711197254,2.44129530169322,
9.19155906509174));
#75045=CARTESIAN_POINT('Ctrl Pts',(-0.408706229788395,2.0956546546633,9.21142940861454));
#75046=CARTESIAN_POINT('Ctrl Pts',(-0.217586422877593,1.75400027041444,
9.23129975213731));
#75047=CARTESIAN_POINT('Ctrl Pts',(0.173139305306751,1.72975353445058,9.25117009566012));
#75048=CARTESIAN_POINT('Ctrl Pts',(0.405033291660138,2.0451575261235,9.27104043918287));
#75049=CARTESIAN_POINT('Ctrl Pts',(0.265364373218883,2.41087202144949,9.2909107827057));
#75050=CARTESIAN_POINT('Ctrl Pts',(-0.11774023155345,2.49140375849969,9.31078112622846));
#75051=CARTESIAN_POINT('Ctrl Pts',(-0.392834202760616,2.21287583193656,
9.33065146975127));
#75052=CARTESIAN_POINT('Ctrl Pts',(-0.307556272482463,1.83079969622856,
9.35052181327406));
#75053=CARTESIAN_POINT('Ctrl Pts',(0.0598626677926879,1.69567819091881,
9.37039215679684));
#75054=CARTESIAN_POINT('Ctrl Pts',(0.372365759934363,1.93146690199714,9.39026250031962));
#75055=CARTESIAN_POINT('Ctrl Pts',(0.343273960356936,2.32186178678359,9.41013284384242));
#75056=CARTESIAN_POINT('Ctrl Pts',(-0.000724965318195603,2.508728685951,
9.43000318736521));
#75057=CARTESIAN_POINT('Ctrl Pts',(-0.344058834008994,2.3206426591444,9.44987353088801));
#75058=CARTESIAN_POINT('Ctrl Pts',(-0.371765561877234,1.93014703035847,
9.46974387441079));
#75059=CARTESIAN_POINT('Ctrl Pts',(-0.05842799803419,1.69546837782485,9.48961421793357));
#75060=CARTESIAN_POINT('Ctrl Pts',(0.308509299751549,1.83189241662954,9.50948456145638));
#75061=CARTESIAN_POINT('Ctrl Pts',(0.392431314763861,2.21426866362503,9.52935490497914));
#75062=CARTESIAN_POINT('Ctrl Pts',(0.116351023179618,2.49181896801839,9.54922524850196));
#75063=CARTESIAN_POINT('Ctrl Pts',(-0.266465492410433,2.40992871059069,
9.56909559202474));
#75064=CARTESIAN_POINT('Ctrl Pts',(-0.40483619471501,2.04372105417998,9.58896593554751));
#75065=CARTESIAN_POINT('Ctrl Pts',(-0.171824801839765,1.72914166887251,
9.60883627907033));
#75066=CARTESIAN_POINT('Ctrl Pts',(0.218812454888957,1.75477431457174,9.62870662259308));
#75067=CARTESIAN_POINT('Ctrl Pts',(0.408719072882905,2.09710452841824,9.64857696611591));
#75068=CARTESIAN_POINT('Ctrl Pts',(0.223681583584119,2.44209094325814,9.66844730963867));
#75069=CARTESIAN_POINT('Ctrl Pts',(-0.166553307155238,2.47325548913525,
9.68831765316147));
#75070=CARTESIAN_POINT('Ctrl Pts',(-0.403998212764973,2.16200893787714,
9.70818799668428));
#75071=CARTESIAN_POINT('Ctrl Pts',(-0.270829757553105,1.79387762787135,
9.72805834020705));
#75072=CARTESIAN_POINT('Ctrl Pts',(0.1107881300716,1.70657191949585,9.74792868372986));
#75073=CARTESIAN_POINT('Ctrl Pts',(0.390772990797583,1.98018291458621,9.76779902725263));
#75074=CARTESIAN_POINT('Ctrl Pts',(0.31227683140565,2.36370977392047,9.78766937077542));
#75075=CARTESIAN_POINT('Ctrl Pts',(-0.0526908081492277,2.5053188165266,
9.80753971429822));
#75076=CARTESIAN_POINT('Ctrl Pts',(-0.369321804432989,2.2751030241438,9.82741005782098));
#75077=CARTESIAN_POINT('Ctrl Pts',(-0.347150323773027,1.88425404523324,
9.84728040134381));
#75078=CARTESIAN_POINT('Ctrl Pts',(-0.00651568130033314,1.69132260866163,
9.86715074486657));
#75079=CARTESIAN_POINT('Ctrl Pts',(0.34009621173551,1.87329704224007,9.88702108838937));
#75080=CARTESIAN_POINT('Ctrl Pts',(0.374716130422396,2.26324057674245,9.90689143191215));
#75081=CARTESIAN_POINT('Ctrl Pts',(0.0655850124414589,2.50343310528141,
9.92676177543496));
#75082=CARTESIAN_POINT('Ctrl Pts',(-0.303711425861324,2.3735306821825,9.94663211895772));
#75083=CARTESIAN_POINT('Ctrl Pts',(-0.394393977513401,1.99270109602099,
9.96650246248053));
#75084=CARTESIAN_POINT('Ctrl Pts',(-0.123273746688637,1.71030364683348,
9.98637280600333));
#75085=CARTESIAN_POINT('Ctrl Pts',(0.260933364517766,1.78539954930836,10.0062431495261));
#75086=CARTESIAN_POINT('Ctrl Pts',(0.405769636649003,2.14909853630889,10.0261134930489));
#75087=CARTESIAN_POINT('Ctrl Pts',(0.178367507702632,2.46775630040815,10.0459838365717));
#75088=CARTESIAN_POINT('Ctrl Pts',(-0.212662527017431,2.44904772438236,
10.0658541800945));
#75089=CARTESIAN_POINT('Ctrl Pts',(-0.408603644587765,2.11013537979253,
10.0857245236173));
#75090=CARTESIAN_POINT('Ctrl Pts',(-0.229706544612006,1.76192520405042,
10.1055948671401));
#75091=CARTESIAN_POINT('Ctrl Pts',(0.159915038323031,1.72385262886458,10.1254652106629));
#75092=CARTESIAN_POINT('Ctrl Pts',(0.402836344063299,2.03084405885495,10.1453355541856));
#75093=CARTESIAN_POINT('Ctrl Pts',(0.27621014534161,2.40127665011465,10.1652058977085));
#75094=CARTESIAN_POINT('Ctrl Pts',(-0.103801259115205,2.49532893000645,
10.1850762412312));
#75095=CARTESIAN_POINT('Ctrl Pts',(-0.388589139599207,2.22672073579131,
10.204946584754));
#75096=CARTESIAN_POINT('Ctrl Pts',(-0.316899386135312,1.84186351795803,
10.2248169282768));
#75097=CARTESIAN_POINT('Ctrl Pts',(0.0455024121519973,1.69381138028954,
10.2446872717996));
#75098=CARTESIAN_POINT('Ctrl Pts',(0.366161941883896,1.91838200361815,10.2645576153224));
#75099=CARTESIAN_POINT('Ctrl Pts',(0.350917738384428,2.30956241356956,10.2844279588452));
#75100=CARTESIAN_POINT('Ctrl Pts',(0.0137542830534484,2.50849783841733,
10.304298302368));
#75101=CARTESIAN_POINT('Ctrl Pts',(-0.336026854502516,2.33269210847617,
10.3241686458908));
#75102=CARTESIAN_POINT('Ctrl Pts',(-0.377549098977838,1.94342304717818,
10.3440389894135));
#75103=CARTESIAN_POINT('Ctrl Pts',(-0.0727214438095559,1.69779202406691,
10.3639093329363));
#75104=CARTESIAN_POINT('Ctrl Pts',(0.298818235923393,1.82113206320271,10.3837796764591));
#75105=CARTESIAN_POINT('Ctrl Pts',(0.396232864626036,2.2002954699086,10.4036500199819));
#75106=CARTESIAN_POINT('Ctrl Pts',(0.130157782267859,2.48745143696863,10.4235203635047));
#75107=CARTESIAN_POINT('Ctrl Pts',(-0.255319345939072,2.41917345736008,
10.4433907070275));
#75108=CARTESIAN_POINT('Ctrl Pts',(-0.406575732837171,2.05809728216624,
10.4632610505503));
#75109=CARTESIAN_POINT('Ctrl Pts',(-0.184854235145107,1.73546114604495,
10.4831313940731));
#75110=CARTESIAN_POINT('Ctrl Pts',(0.206445857660923,1.74723978094379,10.5030017375959));
#75111=CARTESIAN_POINT('Ctrl Pts',(0.408359981128703,2.08262789285941,10.5228720811187));
#75112=CARTESIAN_POINT('Ctrl Pts',(0.23565941510231,2.43395254807768,10.5427424246414));
#75113=CARTESIAN_POINT('Ctrl Pts',(-0.153226582148086,2.47892120396879,
10.5626127681642));
#75114=CARTESIAN_POINT('Ctrl Pts',(-0.401548050193132,2.17628124068232,
10.582483111687));
#75115=CARTESIAN_POINT('Ctrl Pts',(-0.281503848016732,1.803663623823,10.6023534552098));
#75116=CARTESIAN_POINT('Ctrl Pts',(0.096781811426683,1.70289428955137,10.6222237987326));
#75117=CARTESIAN_POINT('Ctrl Pts',(0.386283334539984,1.96641538355556,10.6420941422554));
#75118=CARTESIAN_POINT('Ctrl Pts',(0.321422485940219,2.35248217724416,10.6619644857782));
#75119=CARTESIAN_POINT('Ctrl Pts',(-0.0382997357895325,2.50693094565589,
10.681834829301));
#75120=CARTESIAN_POINT('Ctrl Pts',(-0.362887163970587,2.28807597007412,
10.7017051728238));
#75121=CARTESIAN_POINT('Ctrl Pts',(-0.354575021834985,1.89668689618064,
10.7215755163465));
#75122=CARTESIAN_POINT('Ctrl Pts',(-0.0209885681961636,1.69180991646168,
10.7414458598693));
#75123=CARTESIAN_POINT('Ctrl Pts',(0.331852039427098,1.86139176832721,10.7613162033921));
#75124=CARTESIAN_POINT('Ctrl Pts',(0.380263578451655,2.24986418917502,10.7811865469149));
#75125=CARTESIAN_POINT('Ctrl Pts',(0.0798350524583911,2.50085661862181,
10.8010568904377));
#75126=CARTESIAN_POINT('Ctrl Pts',(-0.293831265604475,2.38411767218393,
10.8209272339605));
#75127=CARTESIAN_POINT('Ctrl Pts',(-0.397947398989942,2.00673944064567,
10.8407975774833));
#75128=CARTESIAN_POINT('Ctrl Pts',(-0.137000969448484,1.71491507603632,
10.8606679210061));
#75129=CARTESIAN_POINT('Ctrl Pts',(0.249625198564137,1.77635370458515,10.8805382645289));
#75130=CARTESIAN_POINT('Ctrl Pts',(0.407254230296271,2.13469374871262,10.9004086080516));
#75131=CARTESIAN_POINT('Ctrl Pts',(0.191282948388597,2.46120700152365,10.9202789515745));
#75132=CARTESIAN_POINT('Ctrl Pts',(-0.200164397843656,2.45636200432963,
10.9401492950972));
#75133=CARTESIAN_POINT('Ctrl Pts',(-0.407988158976476,2.12460338246925,
10.96001963862));
#75134=CARTESIAN_POINT('Ctrl Pts',(-0.241538326820766,1.77027450664141,
10.9798899821428));
#75135=CARTESIAN_POINT('Ctrl Pts',(0.146490037719062,1.71842388289751,10.9997603256656));
#75136=CARTESIAN_POINT('Ctrl Pts',(0.400133735469466,2.01661739969757,11.0196306691884));
#75137=CARTESIAN_POINT('Ctrl Pts',(0.286709204215817,2.39130310075911,11.0395010127112));
#75138=CARTESIAN_POINT('Ctrl Pts',(-0.0897319899722423,2.4987578642103,
11.059371356234));
#75139=CARTESIAN_POINT('Ctrl Pts',(-0.38385629926812,2.24040657322977,11.0792416997568));
#75140=CARTESIAN_POINT('Ctrl Pts',(-0.325844711301839,1.85325136593982,
11.0991120432796));
#75141=CARTESIAN_POINT('Ctrl Pts',(0.0310850395320932,1.69245443860689,
11.1189823868023));
#75142=CARTESIAN_POINT('Ctrl Pts',(0.359498498441325,1.90552508153396,11.1388527303251));
#75143=CARTESIAN_POINT('Ctrl Pts',(0.358121026331844,2.29699998678418,11.1587230738479));
#75144=CARTESIAN_POINT('Ctrl Pts',(0.0282162663381952,2.50775422328637,
11.1785934173707));
#75145=CARTESIAN_POINT('Ctrl Pts',(-0.327573076722947,2.34444947064824,
11.1984637608935));
#75146=CARTESIAN_POINT('Ctrl Pts',(-0.382858716938286,1.95689560748072,
11.2183341044163));
#75147=CARTESIAN_POINT('Ctrl Pts',(-0.0869236058705181,1.70062054254581,
11.2382044479391));
#75148=CARTESIAN_POINT('Ctrl Pts',(0.28875208000307,1.81072175922161,11.2580747914619));
#75149=CARTESIAN_POINT('Ctrl Pts',(0.399537042519869,2.18619638013524,11.2779451349846));
#75150=CARTESIAN_POINT('Ctrl Pts',(0.143801160581459,2.48259755685232,11.2978154785074));
#75151=CARTESIAN_POINT('Ctrl Pts',(-0.243852709430189,2.42801756111144,
11.3176858220302));
#75152=CARTESIAN_POINT('Ctrl Pts',(-0.407804916088317,2.07252610860939,
11.337556165553));
#75153=CARTESIAN_POINT('Ctrl Pts',(-0.197651629861533,1.74223821122565,
11.3574265090758));
#75154=CARTESIAN_POINT('Ctrl Pts',(0.193820118923557,1.74014805017286,11.3772968525986));
#75155=CARTESIAN_POINT('Ctrl Pts',(0.407488294822822,2.0681730636672,11.3971671961214));
#75156=CARTESIAN_POINT('Ctrl Pts',(0.247341434744175,2.42539495840076,11.4170375396442));
#75157=CARTESIAN_POINT('Ctrl Pts',(-0.13970751921652,2.48411127732509,11.436907883167));
#75158=CARTESIAN_POINT('Ctrl Pts',(-0.398593843757351,2.19045779133211,
11.4567782266897));
#75159=CARTESIAN_POINT('Ctrl Pts',(-0.291824580302666,1.81382159650821,
11.4766485702126));
#75160=CARTESIAN_POINT('Ctrl Pts',(0.0826540072505418,1.69971512721642,
11.4965189137353));
#75161=CARTESIAN_POINT('Ctrl Pts',(0.381308795478392,1.9528155348389,11.5163892572581));
#75162=CARTESIAN_POINT('Ctrl Pts',(0.330164674359836,2.34093765189111,11.5362596007809));
#75163=CARTESIAN_POINT('Ctrl Pts',(-0.0238605876222108,2.50803227403266,
11.5561299443037));
#75164=CARTESIAN_POINT('Ctrl Pts',(-0.355997008786566,2.30081283332735,
11.5760002878265));
#75165=CARTESIAN_POINT('Ctrl Pts',(-0.361554639005669,1.90937495624284,
11.5958706313493));
#75166=CARTESIAN_POINT('Ctrl Pts',(-0.0354351091565347,1.69280960554918,
11.6157409748721));
#75167=CARTESIAN_POINT('Ctrl Pts',(0.323191309289222,1.84978600779761,11.6356113183949));
#75168=CARTESIAN_POINT('Ctrl Pts',(0.385333699985837,2.23629968433259,11.6554816619177));
#75169=CARTESIAN_POINT('Ctrl Pts',(0.0939848793917442,2.4977769560189,11.6753520054404));
#75170=CARTESIAN_POINT('Ctrl Pts',(-0.283582273158319,2.3943480230005,11.6952223489632));
#75171=CARTESIAN_POINT('Ctrl Pts',(-0.401001296325997,2.020894850744,11.715092692486));
#75172=CARTESIAN_POINT('Ctrl Pts',(-0.150556221511496,1.72000988373627,
11.7349630360088));
#75173=CARTESIAN_POINT('Ctrl Pts',(0.238003690161047,1.76771411741745,11.7548333795316));
#75174=CARTESIAN_POINT('Ctrl Pts',(0.408227617387438,2.12024541173004,11.7747037230544));
#75175=CARTESIAN_POINT('Ctrl Pts',(0.203958280832558,2.45420429694426,11.7945740665772));
#75176=CARTESIAN_POINT('Ctrl Pts',(-0.187415011973541,2.46322896027285,
11.8144444101));
#75177=CARTESIAN_POINT('Ctrl Pts',(-0.406860545543882,2.13904050170884,
11.8343147536228));
#75178=CARTESIAN_POINT('Ctrl Pts',(-0.253066917639391,1.77903769771133,
11.8541850971455));
#75179=CARTESIAN_POINT('Ctrl Pts',(0.132881155249389,1.71347411099187,11.8740554406683));
#75180=CARTESIAN_POINT('Ctrl Pts',(0.396928858332618,2.00249540668918,11.8939257841911));
#75181=CARTESIAN_POINT('Ctrl Pts',(0.296848370880228,2.38096389269744,11.9137961277139));
#75182=CARTESIAN_POINT('Ctrl Pts',(-0.0755500845982718,2.50168625693585,
11.9336664712367));
#75183=CARTESIAN_POINT('Ctrl Pts',(-0.378641622673128,2.25391616508152,
11.9535368147595));
#75184=CARTESIAN_POINT('Ctrl Pts',(-0.334381019347623,1.86494894555866,
11.9734071582823));
#75185=CARTESIAN_POINT('Ctrl Pts',(0.0166286473641349,1.69160906917418,
11.9932775018051));
#75186=CARTESIAN_POINT('Ctrl Pts',(0.352383793905219,1.89291227441756,12.0131478453279));
#75187=CARTESIAN_POINT('Ctrl Pts',(0.364874782259903,2.28419027543476,12.0330181888507));
#75188=CARTESIAN_POINT('Ctrl Pts',(0.0426428311072668,2.50649877398228,
12.0528885323734));
#75189=CARTESIAN_POINT('Ctrl Pts',(-0.318708112289043,2.35589998721199,
12.0727588758962));
#75190=CARTESIAN_POINT('Ctrl Pts',(-0.387687750851717,1.97054779981215,
12.092629219419));
#75191=CARTESIAN_POINT('Ctrl Pts',(-0.101016656929325,1.70395038275897,
12.1124995629418));
#75192=CARTESIAN_POINT('Ctrl Pts',(0.278323467549698,1.80067457223775,12.1323699064646));
#75193=CARTESIAN_POINT('Ctrl Pts',(0.402339700870507,2.17198909221105,12.1522402499874));
#75194=CARTESIAN_POINT('Ctrl Pts',(0.157264032246886,2.47726342051065,12.1721105935102));
#75195=CARTESIAN_POINT('Ctrl Pts',(-0.232079976398536,2.43644992026867,
12.191980937033));
#75196=CARTESIAN_POINT('Ctrl Pts',(-0.40852220153409,2.08698942170082,12.2118512805557));
#75197=CARTESIAN_POINT('Ctrl Pts',(-0.210200922037842,1.74946435749216,
12.2317216240786));
#75198=CARTESIAN_POINT('Ctrl Pts',(0.180951087156625,1.73350802416591,12.2515919676013));
#75199=CARTESIAN_POINT('Ctrl Pts',(0.406105108150944,2.05375818529026,12.2714623111241));
#75200=CARTESIAN_POINT('Ctrl Pts',(0.258712978634946,2.41642891615619,12.2913326546469));
#75201=CARTESIAN_POINT('Ctrl Pts',(-0.126013088186973,2.48881919435584,
12.3112029981697));
#75202=CARTESIAN_POINT('Ctrl Pts',(-0.395139301730199,2.20452079468752,
12.3310733416925));
#75203=CARTESIAN_POINT('Ctrl Pts',(-0.301778999294402,1.82433879511471,
12.3509436852153));
#75204=CARTESIAN_POINT('Ctrl Pts',(0.068422451493072,1.69703842313985,12.3708140287381));
#75205=CARTESIAN_POINT('Ctrl Pts',(0.375855617911298,1.93940043966916,12.3906843722609));
#75206=CARTESIAN_POINT('Ctrl Pts',(0.338492423017834,2.32909068914615,12.4105547157836));
#75207=CARTESIAN_POINT('Ctrl Pts',(-0.00939148841223189,2.50862141921263,
12.4304250593064));
#75208=CARTESIAN_POINT('Ctrl Pts',(-0.348659987759772,2.31329762593451,
12.4502954028292));
#75209=CARTESIAN_POINT('Ctrl Pts',(-0.368080414108929,1.92230229871115,
12.470165746352));
#75210=CARTESIAN_POINT('Ctrl Pts',(-0.0498371701366613,1.69432042106275,
12.4900360898748));
#75211=CARTESIAN_POINT('Ctrl Pts',(0.314124892717934,1.83849432880167,12.5099064333976));
#75212=CARTESIAN_POINT('Ctrl Pts',(0.389920130746389,2.22256408908266,12.5297767769204));
#75213=CARTESIAN_POINT('Ctrl Pts',(0.108016731647488,2.49419798322434,12.5496471204432));
#75214=CARTESIAN_POINT('Ctrl Pts',(-0.272977313587828,2.40420889296717,
12.569517463966));
#75215=CARTESIAN_POINT('Ctrl Pts',(-0.403551836111819,2.03514955771372,
12.5893878074887));
#75216=CARTESIAN_POINT('Ctrl Pts',(-0.163922487624767,1.72558167466743,
12.6092581510116));
#75217=CARTESIAN_POINT('Ctrl Pts',(0.226083427226409,1.75949163266156,12.6291284945343));
#75218=CARTESIAN_POINT('Ctrl Pts',(0.408688576076754,2.10577166166041,12.6489988380571));
#75219=CARTESIAN_POINT('Ctrl Pts',(0.216377594302136,2.44675697682662,12.6688691815799));
#75220=CARTESIAN_POINT('Ctrl Pts',(-0.174430373094981,2.46963997245408,
12.6887395251027));
#75221=CARTESIAN_POINT('Ctrl Pts',(-0.405222219728848,2.15342861529311,
12.7086098686255));
#75222=CARTESIAN_POINT('Ctrl Pts',(-0.264277845784499,1.78820377724994,
12.7284802121483));
#75223=CARTESIAN_POINT('Ctrl Pts',(0.119105473485777,1.70900952635704,12.7483505556711));
#75224=CARTESIAN_POINT('Ctrl Pts',(0.393225735581682,1.98849580648535,12.7682208991939));
#75225=CARTESIAN_POINT('Ctrl Pts',(0.30661491812593,2.37027200423761,12.7880912427167));
#75226=CARTESIAN_POINT('Ctrl Pts',(-0.0612733448481435,2.50411043231376,
12.8079615862394));
#75227=CARTESIAN_POINT('Ctrl Pts',(-0.37295165555669,2.26723255340767,12.8278319297622));
#75228=CARTESIAN_POINT('Ctrl Pts',(-0.342497595036638,1.87694157341012,
12.847702273285));
#75229=CARTESIAN_POINT('Ctrl Pts',(0.00215138201819559,1.69127633313888,
12.8675726168078));
#75230=CARTESIAN_POINT('Ctrl Pts',(0.34482675909834,1.88055941452387,12.8874429603306));
#75231=CARTESIAN_POINT('Ctrl Pts',(0.371170528355002,2.27114935891834,12.9073133038534));
#75232=CARTESIAN_POINT('Ctrl Pts',(0.0570158686801648,2.50473306643805,
12.9271836473762));
#75233=CARTESIAN_POINT('Ctrl Pts',(-0.309443089519117,2.3670292848331,12.947053990899));
#75234=CARTESIAN_POINT('Ctrl Pts',(-0.392030137992801,1.98436248733954,
12.9669243344217));
#75235=CARTESIAN_POINT('Ctrl Pts',(-0.114982908725333,1.70777736471782,
12.9867946779446));
#75236=CARTESIAN_POINT('Ctrl Pts',(0.267545493074158,1.79100311438672,13.0066650214673));
#75237=CARTESIAN_POINT('Ctrl Pts',(0.404637313975969,2.15769143911221,13.0265353649901));
#75238=CARTESIAN_POINT('Ctrl Pts',(0.170529512724876,2.47145572506355,13.0464057085129));
#75239=CARTESIAN_POINT('Ctrl Pts',(-0.220015952999425,2.44445994733255,
13.0662760520357));
#75240=CARTESIAN_POINT('Ctrl Pts',(-0.408726634081876,2.10146907166997,
13.0861463955585));
#75241=CARTESIAN_POINT('Ctrl Pts',(-0.222486464535814,1.75713050395217,
13.1060167390813));
#75242=CARTESIAN_POINT('Ctrl Pts',(0.167855119186367,1.72732805758641,13.1258870826041));
#75243=CARTESIAN_POINT('Ctrl Pts',(0.404211766498755,2.03940131397413,13.1457574261269));
#75244=CARTESIAN_POINT('Ctrl Pts',(0.269760525376877,2.40706574927223,13.1656277696497));
#75245=CARTESIAN_POINT('Ctrl Pts',(-0.112161928724845,2.4930389042952,13.1854981131724));
#75246=CARTESIAN_POINT('Ctrl Pts',(-0.391185968470993,2.21845286996803,
13.2053684566952));
#75247=CARTESIAN_POINT('Ctrl Pts',(-0.311359986670267,1.83520149440462,
13.225238800218));
#75248=CARTESIAN_POINT('Ctrl Pts',(0.0541153637968024,1.69486854546018,
13.2451091437408));
#75249=CARTESIAN_POINT('Ctrl Pts',(0.369910703092766,1.92618499577519,13.2649794872636));
#75250=CARTESIAN_POINT('Ctrl Pts',(0.346433692742772,2.31695989844127,13.2848498307864));
#75251=CARTESIAN_POINT('Ctrl Pts',(0.00501537287145404,2.50869044887863,
13.3047201743092));
#75252=CARTESIAN_POINT('Ctrl Pts',(-0.34074231600259,2.32552846162887,13.324590517832));
#75253=CARTESIAN_POINT('Ctrl Pts',(-0.374423584156985,1.93542678034618,
13.3444608613547));
#75254=CARTESIAN_POINT('Ctrl Pts',(-0.0636005276092969,1.69638446284464,
13.3643312048776));
#75255=CARTESIAN_POINT('Ctrl Pts',(0.18094005180683,1.78378854426931,13.3775781005594));
#75256=CARTESIAN_POINT('Ctrl Pts',(0.257657118195791,1.86957053507955,13.3842015484003));
#75257=CARTESIAN_POINT('Ctrl Pts',(-0.30218654676688,1.98967595057273,4.35702116407176));
#75258=CARTESIAN_POINT('Ctrl Pts',(-0.265436565557791,1.88899823722173,
4.36364904798937));
#75259=CARTESIAN_POINT('Ctrl Pts',(-0.0840495481126467,1.72910339695751,
4.37690037974791));
#75260=CARTESIAN_POINT('Ctrl Pts',(0.267075589668208,1.8287940790038,4.39677515934738));
#75261=CARTESIAN_POINT('Ctrl Pts',(0.372263060333583,2.17768299025661,4.41664550287017));
#75262=CARTESIAN_POINT('Ctrl Pts',(0.13637277573507,2.45509181004173,4.43651584639296));
#75263=CARTESIAN_POINT('Ctrl Pts',(-0.224838396532887,2.4068641708413,4.45638618991575));
#75264=CARTESIAN_POINT('Ctrl Pts',(-0.379678279217523,2.07707236126518,
4.47625653343854));
#75265=CARTESIAN_POINT('Ctrl Pts',(-0.186273507897977,1.76834368554434,
4.49612687696133));
#75266=CARTESIAN_POINT('Ctrl Pts',(0.178042210154651,1.76384887454306,4.51599722048411));
#75267=CARTESIAN_POINT('Ctrl Pts',(0.379012673598637,2.06773508589522,4.53586756400691));
#75268=CARTESIAN_POINT('Ctrl Pts',(0.232298792807713,2.40121574327281,4.55573790752969));
#75269=CARTESIAN_POINT('Ctrl Pts',(-0.127521856221539,2.45837415432726,
4.5756082510525));
#75270=CARTESIAN_POINT('Ctrl Pts',(-0.370356355674705,2.18677192919838,
4.59547859457527));
#75271=CARTESIAN_POINT('Ctrl Pts',(-0.273440464245838,1.83556886276934,
4.61534893809807));
#75272=CARTESIAN_POINT('Ctrl Pts',(0.0743204226161996,1.72694505892743,
4.63521928162085));
#75273=CARTESIAN_POINT('Ctrl Pts',(0.353902130566146,1.96054853596556,4.65508962514364));
#75274=CARTESIAN_POINT('Ctrl Pts',(0.308826973578812,2.32207966394233,4.67495996866644));
#75275=CARTESIAN_POINT('Ctrl Pts',(-0.0195549719747447,2.47988297661507,
4.69483031218921));
#75276=CARTESIAN_POINT('Ctrl Pts',(-0.329997849655603,2.2891953523409,4.71470065571202));
#75277=CARTESIAN_POINT('Ctrl Pts',(-0.337712647887813,1.92494676049446,
4.7345709992348));
#75278=CARTESIAN_POINT('Ctrl Pts',(-0.0356220554462792,1.72128567853538,
4.7544413427576));
#75279=CARTESIAN_POINT('Ctrl Pts',(0.299146917306782,1.86504343234269,4.77431168628037));
#75280=CARTESIAN_POINT('Ctrl Pts',(0.359489321750484,2.22434184890623,4.79418202980318));
#75281=CARTESIAN_POINT('Ctrl Pts',(0.0900492119073741,2.46957354755419,
4.81405237332595));
#75282=CARTESIAN_POINT('Ctrl Pts',(-0.261998789919797,2.3757718287794,4.83392271684875));
#75283=CARTESIAN_POINT('Ctrl Pts',(-0.373698570350197,2.02898700027084,
4.85379306037154));
#75284=CARTESIAN_POINT('Ctrl Pts',(-0.142580786722154,1.747346931349,4.87366340389433));
#75285=CARTESIAN_POINT('Ctrl Pts',(0.21933545798344,1.78921804359556,4.89353374741711));
#75286=CARTESIAN_POINT('Ctrl Pts',(0.380041279877134,2.11618929166855,4.91340409093991));
#75287=CARTESIAN_POINT('Ctrl Pts',(0.192110965399915,2.42830906862518,4.9332744344627));
#75288=CARTESIAN_POINT('Ctrl Pts',(-0.172055006268819,2.43924997035339,
4.95314477798548));
#75289=CARTESIAN_POINT('Ctrl Pts',(-0.378383932868546,2.13897520899983,
4.97301512150828));
#75290=CARTESIAN_POINT('Ctrl Pts',(-0.237597113377836,1.80294599938219,
4.99288546503106));
#75291=CARTESIAN_POINT('Ctrl Pts',(0.121152711708541,1.73942339508214,5.01275580855386));
#75292=CARTESIAN_POINT('Ctrl Pts',(0.368761417255891,2.00668073772146,5.03262615207664));
#75293=CARTESIAN_POINT('Ctrl Pts',(0.278081724804058,2.35954579923129,5.05249649559943));
#75294=CARTESIAN_POINT('Ctrl Pts',(-0.0677000927468386,2.47431292391617,
5.07236683912222));
#75295=CARTESIAN_POINT('Ctrl Pts',(-0.35137629173806,2.24569889901118,5.09223718264501));
#75296=CARTESIAN_POINT('Ctrl Pts',(-0.312712578622125,1.88342596937737,
5.1121075261678));
#75297=CARTESIAN_POINT('Ctrl Pts',(0.0128223534062021,1.71983022894796,
5.13197786969059));
#75298=CARTESIAN_POINT('Ctrl Pts',(0.326594521790154,1.90498849801793,5.15184821321338));
#75299=CARTESIAN_POINT('Ctrl Pts',(0.340760678260896,2.26904327173777,5.17171855673617));
#75300=CARTESIAN_POINT('Ctrl Pts',(0.042325302804598,2.47802385680157,5.19158890025895));
#75301=CARTESIAN_POINT('Ctrl Pts',(-0.294937775905254,2.34021901655094,
5.21145924378176));
#75302=CARTESIAN_POINT('Ctrl Pts',(-0.361635597374513,1.98204593148086,
5.23132958730454));
#75303=CARTESIAN_POINT('Ctrl Pts',(-0.096581990493603,1.73207964628071,
5.25119993082733));
#75304=CARTESIAN_POINT('Ctrl Pts',(0.25707244421448,1.81963019778472,5.27107027435011));
#75305=CARTESIAN_POINT('Ctrl Pts',(0.374897908608829,2.16438187391932,5.29094061787291));
#75306=CARTESIAN_POINT('Ctrl Pts',(0.148805579596161,2.45007194553361,5.31081096139569));
#75307=CARTESIAN_POINT('Ctrl Pts',(-0.21379561064561,2.41461866511271,5.33068130491849));
#75308=CARTESIAN_POINT('Ctrl Pts',(-0.380268433764204,2.09054559091451,
5.35055164844128));
#75309=CARTESIAN_POINT('Ctrl Pts',(-0.197896737776705,1.77514564995066,
5.37042199196406));
#75310=CARTESIAN_POINT('Ctrl Pts',(0.166018273912844,1.75775535023081,5.39029233548685));
#75311=CARTESIAN_POINT('Ctrl Pts',(0.377634120634467,2.05432792427237,5.41016267900964));
#75312=CARTESIAN_POINT('Ctrl Pts',(0.242822071917181,2.39279841010239,5.43003302253243));
#75313=CARTESIAN_POINT('Ctrl Pts',(-0.114746170544072,2.46266621556758,
5.44990336605522));
#75314=CARTESIAN_POINT('Ctrl Pts',(-0.367050422811667,2.19983714079646,
5.46977370957801));
#75315=CARTESIAN_POINT('Ctrl Pts',(-0.282635881552423,1.845421080944,5.4896440531008));
#75316=CARTESIAN_POINT('Ctrl Pts',(0.0610586036303811,1.72454652153516,
5.50951439662359));
#75317=CARTESIAN_POINT('Ctrl Pts',(0.34874013236059,1.94809941524223,5.52938474014638));
#75318=CARTESIAN_POINT('Ctrl Pts',(0.31650006633187,2.31100041606727,5.54925508366917));
#75319=CARTESIAN_POINT('Ctrl Pts',(-0.00608572296309057,2.48033726026337,
5.56912542719196));
#75320=CARTESIAN_POINT('Ctrl Pts',(-0.323088689935783,2.30076644641029,
5.58899577071475));
#75321=CARTESIAN_POINT('Ctrl Pts',(-0.343701768445756,1.93701974985939,
5.60886611423753));
#75322=CARTESIAN_POINT('Ctrl Pts',(-0.0490152651773467,1.72278524505498,
5.62873645776033));
#75323=CARTESIAN_POINT('Ctrl Pts',(0.290636071065476,1.8545939247609,5.64860680128312));
#75324=CARTESIAN_POINT('Ctrl Pts',(0.363668378633969,2.21152926947835,5.6684771448059));
#75325=CARTESIAN_POINT('Ctrl Pts',(0.103084457784923,2.46615169278842,5.6883474883287));
#75326=CARTESIAN_POINT('Ctrl Pts',(-0.252065419400099,2.38487978501692,
5.70821783185148));
#75327=CARTESIAN_POINT('Ctrl Pts',(-0.3759795898937,2.04226945737306,5.72808817537427));
#75328=CARTESIAN_POINT('Ctrl Pts',(-0.154983671659029,1.75261904328573,
5.74795851889706));
#75329=CARTESIAN_POINT('Ctrl Pts',(0.208188666201143,1.78164336533688,5.76782886241985));
#75330=CARTESIAN_POINT('Ctrl Pts',(0.380376245149376,2.10271655934924,5.78769920594264));
#75331=CARTESIAN_POINT('Ctrl Pts',(0.203620402722817,2.42129767998483,5.80756954946543));
#75332=CARTESIAN_POINT('Ctrl Pts',(-0.15992943878723,2.44513191996371,5.82743989298822));
#75333=CARTESIAN_POINT('Ctrl Pts',(-0.376765792637049,2.15235460884403,
5.84731023651101));
#75334=CARTESIAN_POINT('Ctrl Pts',(-0.24797082377341,1.81154907154635,5.8671805800338));
#75335=CARTESIAN_POINT('Ctrl Pts',(0.108303617723016,1.73535799205694,5.88705092355659));
#75336=CARTESIAN_POINT('Ctrl Pts',(0.365224234164739,1.99367631332851,5.90692126707937));
#75337=CARTESIAN_POINT('Ctrl Pts',(0.287101336550038,2.34953214245828,5.92679161060217));
#75338=CARTESIAN_POINT('Ctrl Pts',(-0.0543979520317252,2.47647620161624,
5.94666195412495));
#75339=CARTESIAN_POINT('Ctrl Pts',(-0.345994525236831,2.25805459839808,
5.96653229764775));
#75340=CARTESIAN_POINT('Ctrl Pts',(-0.320188224438393,1.89463941834026,
5.98640264117053));
#75341=CARTESIAN_POINT('Ctrl Pts',(-0.000652817408372478,1.7196146146366,
6.00627298469333));
#75342=CARTESIAN_POINT('Ctrl Pts',(0.319481460720768,1.89354161720976,6.02614332821611));
#75343=CARTESIAN_POINT('Ctrl Pts',(0.346534992112049,2.25686607922219,6.0460136717389));
#75344=CARTESIAN_POINT('Ctrl Pts',(0.0556898447196964,2.47628726893655,
6.06588401526169));
#75345=CARTESIAN_POINT('Ctrl Pts',(-0.28624315371522,2.35051611628756,6.08575435878448));
#75346=CARTESIAN_POINT('Ctrl Pts',(-0.365587027102976,1.99493053163432,
6.10562470230728));
#75347=CARTESIAN_POINT('Ctrl Pts',(-0.109554573303277,1.73573188029013,
6.12549504583006));
#75348=CARTESIAN_POINT('Ctrl Pts',(0.24697928699379,1.81069963815322,6.14536538935285));
#75349=CARTESIAN_POINT('Ctrl Pts',(0.376943274667832,2.15106109332289,6.16523573287564));
#75350=CARTESIAN_POINT('Ctrl Pts',(0.161113124027163,2.44458094670896,6.18510607639843));
#75351=CARTESIAN_POINT('Ctrl Pts',(-0.202516384337175,2.42199469194947,
6.20497641992122));
#75352=CARTESIAN_POINT('Ctrl Pts',(-0.380364680188321,2.10402214294532,
6.22484676344401));
#75353=CARTESIAN_POINT('Ctrl Pts',(-0.209280163942015,1.78235982535416,
6.2447171069668));
#75354=CARTESIAN_POINT('Ctrl Pts',(0.15379041179948,1.75208912519557,6.26458745048959));
#75355=CARTESIAN_POINT('Ctrl Pts',(0.37577922138895,2.04097928888135,6.28445779401238));
#75356=CARTESIAN_POINT('Ctrl Pts',(0.253041753075546,2.38401292007423,6.30432813753516));
#75357=CARTESIAN_POINT('Ctrl Pts',(-0.101827075160669,2.46650336196665,
6.32419848105796));
#75358=CARTESIAN_POINT('Ctrl Pts',(-0.363283424441477,2.21277686418193,
6.34406882458075));
#75359=CARTESIAN_POINT('Ctrl Pts',(-0.291476688369577,1.85559294669396,
6.36393916810353));
#75360=CARTESIAN_POINT('Ctrl Pts',(0.0477202283134581,1.72261922759851,
6.38380951162632));
#75361=CARTESIAN_POINT('Ctrl Pts',(0.343140332041345,1.93584099142845,6.40367985514912));
#75362=CARTESIAN_POINT('Ctrl Pts',(0.323775895459235,2.29965629739181,6.4235501986719));
#75363=CARTESIAN_POINT('Ctrl Pts',(0.00739115290122109,2.48031413124866,
6.44342054219469));
#75364=CARTESIAN_POINT('Ctrl Pts',(-0.315773966229056,2.31208552477859,
6.46329088571748));
#75365=CARTESIAN_POINT('Ctrl Pts',(-0.349259460087822,1.94929732216115,
6.48316122924027));
#75366=CARTESIAN_POINT('Ctrl Pts',(-0.0623469466980092,1.72475831014389,
6.50303157276306));
#75367=CARTESIAN_POINT('Ctrl Pts',(0.281760402516878,1.84445246402643,6.52290191628586));
#75368=CARTESIAN_POINT('Ctrl Pts',(0.367390940637607,2.19857669250918,6.54277225980863));
#75369=CARTESIAN_POINT('Ctrl Pts',(0.115990306483514,2.46227022561963,6.56264260333144));
#75370=CARTESIAN_POINT('Ctrl Pts',(-0.241815643214863,2.39363014536184,
6.58251294685422));
#75371=CARTESIAN_POINT('Ctrl Pts',(-0.377788660490751,2.05562438086923,
6.60238329037701));
#75372=CARTESIAN_POINT('Ctrl Pts',(-0.167192013048295,1.75832720573406,
6.62225363389979));
#75373=CARTESIAN_POINT('Ctrl Pts',(0.196780545228712,1.77446830478718,6.64212397742259));
#75374=CARTESIAN_POINT('Ctrl Pts',(0.380233742510557,2.08924041705957,6.66199432094537));
#75375=CARTESIAN_POINT('Ctrl Pts',(0.214874245188744,2.41388298189485,6.68186466446817));
#75376=CARTESIAN_POINT('Ctrl Pts',(-0.147603119606738,2.45058064215098,
6.70173500799095));
#75377=CARTESIAN_POINT('Ctrl Pts',(-0.374674716513269,2.16566829047828,
6.72160535151375));
#75378=CARTESIAN_POINT('Ctrl Pts',(-0.258033268375595,1.82051422222223,
6.74147569503654));
#75379=CARTESIAN_POINT('Ctrl Pts',(0.0953185754392329,1.7317503065244,6.76134603855932));
#75380=CARTESIAN_POINT('Ctrl Pts',(0.361228602740849,1.98080535192161,6.78121638208212));
#75381=CARTESIAN_POINT('Ctrl Pts',(0.295760563861364,2.33920526004468,6.8010867256049));
#75382=CARTESIAN_POINT('Ctrl Pts',(-0.0410275281959761,2.47816690693233,
6.82095706912769));
#75383=CARTESIAN_POINT('Ctrl Pts',(-0.340178448527117,2.27021189948509,
6.84082741265049));
#75384=CARTESIAN_POINT('Ctrl Pts',(-0.327261953448532,1.90611064651795,
6.86069775617327));
#75385=CARTESIAN_POINT('Ctrl Pts',(-0.0141271687728025,1.71987647971863,
6.88056809969606));
#75386=CARTESIAN_POINT('Ctrl Pts',(0.31196737001161,1.88235389363309,6.90043844321885));
#75387=CARTESIAN_POINT('Ctrl Pts',(0.351874317332742,2.24449198029737,6.92030878674164));
#75388=CARTESIAN_POINT('Ctrl Pts',(0.0689844818637428,2.47407834584566,
6.94017913026443));
#75389=CARTESIAN_POINT('Ctrl Pts',(-0.277189224326068,2.36049875524875,
6.96004947378722));
#75390=CARTESIAN_POINT('Ctrl Pts',(-0.369079553102077,2.00794702041429,
6.97991981731001));
#75391=CARTESIAN_POINT('Ctrl Pts',(-0.122389637550941,1.73984136246816,
6.99979016083279));
#75392=CARTESIAN_POINT('Ctrl Pts',(0.236576108608585,1.80213222328648,7.01966050435559));
#75393=CARTESIAN_POINT('Ctrl Pts',(0.378515482048657,2.13767621820337,7.03953084787837));
#75394=CARTESIAN_POINT('Ctrl Pts',(0.173218430938826,2.43865741207262,7.05940119140117));
#75395=CARTESIAN_POINT('Ctrl Pts',(-0.19098294899741,2.42896653440873,7.07927153492395));
#75396=CARTESIAN_POINT('Ctrl Pts',(-0.379983473209242,2.11749364617445,
7.09914187844675));
#75397=CARTESIAN_POINT('Ctrl Pts',(-0.220400890830285,1.78997271911999,
7.11901222196954));
#75398=CARTESIAN_POINT('Ctrl Pts',(0.141369504013592,1.74685961586985,7.13888256549232));
#75399=CARTESIAN_POINT('Ctrl Pts',(0.373452624645094,2.02770473933704,7.15875290901512));
#75400=CARTESIAN_POINT('Ctrl Pts',(0.262943803148664,2.37487092235148,7.1786232525379));
#75401=CARTESIAN_POINT('Ctrl Pts',(-0.0887801611702712,2.4698804544055,
7.19849359606069));
#75402=CARTESIAN_POINT('Ctrl Pts',(-0.359060413943042,2.22557502421934,
7.21836393958349));
#75403=CARTESIAN_POINT('Ctrl Pts',(-0.299951618584444,1.86607160480778,
7.23823428310627));
#75404=CARTESIAN_POINT('Ctrl Pts',(0.0343219520998536,1.72116564150979,
7.25810462662907));
#75405=CARTESIAN_POINT('Ctrl Pts',(0.337109804244394,1.92378862848572,7.27797497015184));
#75406=CARTESIAN_POINT('Ctrl Pts',(0.33064530435041,2.28806155981396,7.29784531367464));
#75407=CARTESIAN_POINT('Ctrl Pts',(0.0208587510084466,2.47981361228239,
7.31771565719742));
#75408=CARTESIAN_POINT('Ctrl Pts',(-0.308062866721238,2.32313838243594,
7.33758600072022));
#75409=CARTESIAN_POINT('Ctrl Pts',(-0.354378743206429,1.9617640642522,7.35745634424301));
#75410=CARTESIAN_POINT('Ctrl Pts',(-0.0756003671091846,1.72720239799378,
7.37732668776579));
#75411=CARTESIAN_POINT('Ctrl Pts',(0.272531053750123,1.83463177976539,7.39719703128859));
#75412=CARTESIAN_POINT('Ctrl Pts',(0.370652334546399,2.18550037698128,7.41706737481138));
#75413=CARTESIAN_POINT('Ctrl Pts',(0.128750558155218,2.45793401814211,7.43693771833416));
#75414=CARTESIAN_POINT('Ctrl Pts',(-0.231262327537628,2.40201192597398,
7.45680806185696));
#75415=CARTESIAN_POINT('Ctrl Pts',(-0.379123511237657,2.06903500693578,
7.47667840537974));
#75416=CARTESIAN_POINT('Ctrl Pts',(-0.17919048638257,1.76446425353084,7.49654874890254));
#75417=CARTESIAN_POINT('Ctrl Pts',(0.185125415146614,1.76770186844427,7.51641909242532));
#75418=CARTESIAN_POINT('Ctrl Pts',(0.379613950828283,2.07577778075445,7.53628943594811));
#75419=CARTESIAN_POINT('Ctrl Pts',(0.225858366397756,2.40607428166505,7.55615977947091));
#75420=CARTESIAN_POINT('Ctrl Pts',(-0.135091521362634,2.45558929739879,
7.57603012299369));
#75421=CARTESIAN_POINT('Ctrl Pts',(-0.372113329322741,2.17889954188068,
7.59590046651648));
#75422=CARTESIAN_POINT('Ctrl Pts',(-0.267771816284581,1.82983019788974,
7.61577081003927));
#75423=CARTESIAN_POINT('Ctrl Pts',(0.0822138843536524,1.72860486703765,
7.63564115356206));
#75424=CARTESIAN_POINT('Ctrl Pts',(0.356779538507097,1.96808400979676,7.65551149708485));
#75425=CARTESIAN_POINT('Ctrl Pts',(0.30404853722851,2.32857811482695,7.67538184060764));
#75426=CARTESIAN_POINT('Ctrl Pts',(-0.0276056044866047,2.47938291760379,
7.69525218413042));
#75427=CARTESIAN_POINT('Ctrl Pts',(-0.333935362248948,2.28215554179958,
7.71512252765322));
#75428=CARTESIAN_POINT('Ctrl Pts',(-0.333924886342341,1.91782525463201,
7.734992871176));
#75429=CARTESIAN_POINT('Ctrl Pts',(-0.0275837869849208,1.72061549548748,
7.7548632146988));
#75430=CARTESIAN_POINT('Ctrl Pts',(0.304061681737653,1.87143937069673,7.77473355822158));
#75431=CARTESIAN_POINT('Ctrl Pts',(0.356771951726028,2.23193650757178,7.79460390174438));
#75432=CARTESIAN_POINT('Ctrl Pts',(0.0821925261211519,2.47139986028331,
7.81447424526716));
#75433=CARTESIAN_POINT('Ctrl Pts',(-0.267787352697854,2.37015440271021,
7.83434458878996));
#75434=CARTESIAN_POINT('Ctrl Pts',(-0.372108791372701,2.02107905885139,
7.85421493231274));
#75435=CARTESIAN_POINT('Ctrl Pts',(-0.135071072000656,1.74440293438045,
7.87408527583553));
#75436=CARTESIAN_POINT('Ctrl Pts',(0.225875967665989,1.79393870744639,7.89395561935832));
#75437=CARTESIAN_POINT('Ctrl Pts',(0.379612557235358,2.12424404994773,7.91382596288111));
#75438=CARTESIAN_POINT('Ctrl Pts',(0.185106305124325,2.43230877715139,7.9336963064039));
#75439=CARTESIAN_POINT('Ctrl Pts',(-0.179209781990372,2.43552544107355,
7.95356664992669));
#75440=CARTESIAN_POINT('Ctrl Pts',(-0.379125291337669,2.13094319047487,
7.97343699344948));
#75441=CARTESIAN_POINT('Ctrl Pts',(-0.231244959130432,1.79797477515049,
7.99330733697226));
#75442=CARTESIAN_POINT('Ctrl Pts',(0.128771141920517,1.74207338660401,8.01317768049507));
#75443=CARTESIAN_POINT('Ctrl Pts',(0.370657250867365,2.01452093853999,8.03304802401784));
#75444=CARTESIAN_POINT('Ctrl Pts',(0.272515792571565,2.36538389244211,8.05291836754064));
#75445=CARTESIAN_POINT('Ctrl Pts',(-0.0756218057335592,2.47279325378316,
8.07278871106342));
#75446=CARTESIAN_POINT('Ctrl Pts',(-0.354386692257366,2.23821555599685,
8.09265905458622));
#75447=CARTESIAN_POINT('Ctrl Pts',(-0.308050034026664,1.87684390193229,
8.11252939810901));
#75448=CARTESIAN_POINT('Ctrl Pts',(0.0208805931982691,1.72018758788538,
8.13239974163179));
#75449=CARTESIAN_POINT('Ctrl Pts',(0.330656118799868,1.91195745516282,8.15227008515458));
#75450=CARTESIAN_POINT('Ctrl Pts',(0.337099670168359,2.27623075764752,8.17214042867737));
#75451=CARTESIAN_POINT('Ctrl Pts',(0.0343001661334638,2.47883633164185,
8.19201077220018));
#75452=CARTESIAN_POINT('Ctrl Pts',(-0.299965070782925,2.33391114526424,
8.21188111572295));
#75453=CARTESIAN_POINT('Ctrl Pts',(-0.359053191812853,1.97440432723363,
8.23175145924575));
#75454=CARTESIAN_POINT('Ctrl Pts',(-0.088758890032661,1.73011444065926,
8.25162180276853));
#75455=CARTESIAN_POINT('Ctrl Pts',(0.262959609920743,1.82514419940819,8.27149214629133));
#75456=CARTESIAN_POINT('Ctrl Pts',(0.373448466490159,2.17231673696168,8.29136248981411));
#75457=CARTESIAN_POINT('Ctrl Pts',(0.141349195472712,2.45314851338758,8.3112328333369));
#75458=CARTESIAN_POINT('Ctrl Pts',(-0.220418719435609,2.41001460560915,
8.33110317685969));
#75459=CARTESIAN_POINT('Ctrl Pts',(-0.379982466560774,2.08248450186184,
8.35097352038248));
#75460=CARTESIAN_POINT('Ctrl Pts',(-0.190964030558069,1.77102248313653,
8.37084386390527));
#75461=CARTESIAN_POINT('Ctrl Pts',(0.173237906076449,1.7613525498887,8.39071420742806));
#75462=CARTESIAN_POINT('Ctrl Pts',(0.3785176480971,2.06234554943069,8.41058455095085));
#75463=CARTESIAN_POINT('Ctrl Pts',(0.23655897851328,2.39788138117948,8.43045489447364));
#75464=CARTESIAN_POINT('Ctrl Pts',(-0.122410349259601,2.46015159858423,
8.45032523799642));
#75465=CARTESIAN_POINT('Ctrl Pts',(-0.369084846251043,2.19203175450071,
8.47019558151923));
#75466=CARTESIAN_POINT('Ctrl Pts',(-0.27717424317176,1.8394853046548,8.490065925042));
#75467=CARTESIAN_POINT('Ctrl Pts',(0.069005994151748,1.72592562191488,8.5099362685648));
#75468=CARTESIAN_POINT('Ctrl Pts',(0.351882626158829,1.95552825544003,8.52980661208759));
#75469=CARTESIAN_POINT('Ctrl Pts',(0.311954853158996,2.31766404654693,8.54967695561037));
#75470=CARTESIAN_POINT('Ctrl Pts',(-0.0141490287958676,2.48012270723119,
8.56954729913317));
#75471=CARTESIAN_POINT('Ctrl Pts',(-0.327273103046854,2.29387053306451,
8.58941764265595));
#75472=CARTESIAN_POINT('Ctrl Pts',(-0.340168659462118,1.92976853790095,
8.60928798617873));
#75473=CARTESIAN_POINT('Ctrl Pts',(-0.0410057806021346,1.72183073429237,
8.62915832970154));
#75474=CARTESIAN_POINT('Ctrl Pts',(0.295774319527368,1.86081174887391,8.64902867322432));
#75475=CARTESIAN_POINT('Ctrl Pts',(0.36122174752812,2.21921542132362,8.6688990167471));
#75476=CARTESIAN_POINT('Ctrl Pts',(0.0952973980721992,2.46825517442299,
8.68876936026991));
#75477=CARTESIAN_POINT('Ctrl Pts',(-0.258049340545726,2.37947093840426,
8.70863970379268));
#75478=CARTESIAN_POINT('Ctrl Pts',(-0.374670939458421,2.0343101629323,8.72851004731549));
#75479=CARTESIAN_POINT('Ctrl Pts',(-0.147582958260542,1.74941087010618,
8.74838039083826));
#75480=CARTESIAN_POINT('Ctrl Pts',(0.214892295535876,1.78612937555744,8.76825073436106));
#75481=CARTESIAN_POINT('Ctrl Pts',(0.380233123122462,2.11078144930768,8.78812107788384));
#75482=CARTESIAN_POINT('Ctrl Pts',(0.196761824309647,2.42554301107991,8.80799142140664));
#75483=CARTESIAN_POINT('Ctrl Pts',(-0.167211661603712,2.44166317886533,
8.82786176492941));
#75484=CARTESIAN_POINT('Ctrl Pts',(-0.377791211807834,2.1443538932835,8.84773210845223));
#75485=CARTESIAN_POINT('Ctrl Pts',(-0.241798756807518,1.80635594885137,
8.86760245197499));
#75486=CARTESIAN_POINT('Ctrl Pts',(0.116011139635423,1.73773644532036,8.88747279549781));
#75487=CARTESIAN_POINT('Ctrl Pts',(0.367396608953386,2.00144443547831,8.90734313902058));
#75488=CARTESIAN_POINT('Ctrl Pts',(0.281745706088464,2.35556373895635,8.92721348254337));
#75489=CARTESIAN_POINT('Ctrl Pts',(-0.0623685258982764,2.47523810380333,
8.94708382606617));
#75490=CARTESIAN_POINT('Ctrl Pts',(-0.349268126081446,2.25068259246573,
8.96695416958895));
#75491=CARTESIAN_POINT('Ctrl Pts',(-0.315761769146652,1.88789631612342,
8.98682451311175));
#75492=CARTESIAN_POINT('Ctrl Pts',(0.00741302389702733,1.71968629442874,
9.00669485663451));
#75493=CARTESIAN_POINT('Ctrl Pts',(0.32378737670726,1.90036232255992,9.02656520015734));
#75494=CARTESIAN_POINT('Ctrl Pts',(0.343130891059556,2.26417874152677,9.0464355436801));
#75495=CARTESIAN_POINT('Ctrl Pts',(0.047698525917369,2.47738351606018,9.0663058872029));
#75496=CARTESIAN_POINT('Ctrl Pts',(-0.291490743186063,2.34439029073487,
9.08617623072569));
#75497=CARTESIAN_POINT('Ctrl Pts',(-0.363276938297633,1.98720224439407,
9.10604657424848));
#75498=CARTESIAN_POINT('Ctrl Pts',(-0.101805998210462,1.73349078279393,
9.12591691777126));
#75499=CARTESIAN_POINT('Ctrl Pts',(0.253058085599665,1.81600163225598,9.14578726129406));
#75500=CARTESIAN_POINT('Ctrl Pts',(0.375775826619579,2.15904232123663,9.16565760481684));
#75501=CARTESIAN_POINT('Ctrl Pts',(0.153770403975355,2.4479197183689,9.18552794833964));
#75502=CARTESIAN_POINT('Ctrl Pts',(-0.209298430366079,2.41762813889032,
9.20539829186242));
#75503=CARTESIAN_POINT('Ctrl Pts',(-0.380364448254989,2.09595598314635,
9.22526863538522));
#75504=CARTESIAN_POINT('Ctrl Pts',(-0.202497866813709,1.77799366232241,
9.245138978908));
#75505=CARTESIAN_POINT('Ctrl Pts',(0.161132939833921,1.75542831911326,9.2650093224308));
#75506=CARTESIAN_POINT('Ctrl Pts',(0.376946210452853,2.04896058391921,9.28487966595358));
#75507=CARTESIAN_POINT('Ctrl Pts',(0.246962649573998,2.38931456459021,9.30475000947638));
#75508=CARTESIAN_POINT('Ctrl Pts',(-0.10957552136021,2.4642618188711,9.32462035299915));
#75509=CARTESIAN_POINT('Ctrl Pts',(-0.365593068806628,2.20504844410645,
9.34449069652196));
#75510=CARTESIAN_POINT('Ctrl Pts',(-0.286228746625001,1.84946742292844,
9.36436104004474));
#75511=CARTESIAN_POINT('Ctrl Pts',(0.0557114840598653,1.72371593428303,
9.38423138356752));
#75512=CARTESIAN_POINT('Ctrl Pts',(0.346544012553486,1.94315384948313,9.40410172709032));
#75513=CARTESIAN_POINT('Ctrl Pts',(0.319469587236485,2.30647675510717,9.42397207061312));
#75514=CARTESIAN_POINT('Ctrl Pts',(-0.000674692512978063,2.48038534719236,
9.44384241413588));
#75515=CARTESIAN_POINT('Ctrl Pts',(-0.32020003373287,2.30534216801744,9.46371275765871));
#75516=CARTESIAN_POINT('Ctrl Pts',(-0.345985435301189,1.94192550449841,
9.48358310118145));
#75517=CARTESIAN_POINT('Ctrl Pts',(-0.0543763016444307,1.72352067070274,
9.50345344470429));
#75518=CARTESIAN_POINT('Ctrl Pts',(0.287115686106074,1.85048436850475,9.52332378822703));
#75519=CARTESIAN_POINT('Ctrl Pts',(0.365218119125371,2.20634468971775,9.54319413174986));
#75520=CARTESIAN_POINT('Ctrl Pts',(0.108282647804378,2.46464823563691,9.56306447527262));
#75521=CARTESIAN_POINT('Ctrl Pts',(-0.247987411525762,2.38843666773381,
9.58293481879543));
#75522=CARTESIAN_POINT('Ctrl Pts',(-0.376762781218556,2.04762372429146,
9.60280516231822));
#75523=CARTESIAN_POINT('Ctrl Pts',(-0.159909590764387,1.75485888342563,
9.62267550584101));
#75524=CARTESIAN_POINT('Ctrl Pts',(0.203638879491112,1.77871403029663,9.64254584936379));
#75525=CARTESIAN_POINT('Ctrl Pts',(0.3803764007436,2.0973053152353,9.66241619288658));
#75526=CARTESIAN_POINT('Ctrl Pts',(0.208170357884774,2.41836860659739,9.68228653640938));
#75527=CARTESIAN_POINT('Ctrl Pts',(-0.155003648498172,2.44737204337841,
9.70215687993214));
#75528=CARTESIAN_POINT('Ctrl Pts',(-0.375982909225308,2.15770892079316,
9.72202722345497));
#75529=CARTESIAN_POINT('Ctrl Pts',(-0.252049036189305,1.81510571974032,
9.74189756697772));
#75530=CARTESIAN_POINT('Ctrl Pts',(0.103105514172589,1.73385423597173,9.76176791050055));
#75531=CARTESIAN_POINT('Ctrl Pts',(0.363674791829392,1.98849164445439,9.7816382540233));
#75532=CARTESIAN_POINT('Ctrl Pts',(0.290621957834928,2.34542278865832,9.80150859754612));
#75533=CARTESIAN_POINT('Ctrl Pts',(-0.0490369578661753,2.47721193556391,
9.82137894106889));
#75534=CARTESIAN_POINT('Ctrl Pts',(-0.343711140504061,2.26296048435751,
9.84124928459169));
#75535=CARTESIAN_POINT('Ctrl Pts',(-0.323077143775959,1.89921497381975,
9.86111962811447));
#75536=CARTESIAN_POINT('Ctrl Pts',(-0.00606385061491112,1.71966239038934,
9.88098997163728));
#75537=CARTESIAN_POINT('Ctrl Pts',(0.316512199966604,1.88901778548669,9.90086031516005));
#75538=CARTESIAN_POINT('Ctrl Pts',(0.348731396323853,2.25192063976514,9.92073065868285));
#75539=CARTESIAN_POINT('Ctrl Pts',(0.0610370120465778,2.47545698918659,
9.94060100220563));
#75540=CARTESIAN_POINT('Ctrl Pts',(-0.282650521344584,2.35456266488288,
9.96047134572842));
#75541=CARTESIAN_POINT('Ctrl Pts',(-0.367044680795904,2.00014175112657,
9.98034168925121));
#75542=CARTESIAN_POINT('Ctrl Pts',(-0.114725314238147,1.73732718623863,
10.000212032774));
#75543=CARTESIAN_POINT('Ctrl Pts',(0.242838909691915,1.80721555453153,10.0200823762968));
#75544=CARTESIAN_POINT('Ctrl Pts',(0.377631493511943,2.14569379253875,10.0399527198196));
#75545=CARTESIAN_POINT('Ctrl Pts',(0.165998591920333,2.44225419653979,10.0598230633424));
#75546=CARTESIAN_POINT('Ctrl Pts',(-0.197915419090541,2.42484296891706,
10.0796934068652));
#75547=CARTESIAN_POINT('Ctrl Pts',(-0.380268976837149,2.10943254068979,
10.099563750388));
#75548=CARTESIAN_POINT('Ctrl Pts',(-0.213777517282165,1.7853690405041,10.1194340939107));
#75549=CARTESIAN_POINT('Ctrl Pts',(0.148825711198222,1.74993661251857,10.1393044374335));
#75550=CARTESIAN_POINT('Ctrl Pts',(0.374901610445288,2.03563968572042,10.1591747809563));
#75551=CARTESIAN_POINT('Ctrl Pts',(0.257056320354344,2.38038458540818,10.1790451244791));
#75552=CARTESIAN_POINT('Ctrl Pts',(-0.0966031486037206,2.46791479889845,
10.1989154680019));
#75553=CARTESIAN_POINT('Ctrl Pts',(-0.361642380049,2.21793327147642,10.2187858115247));
#75554=CARTESIAN_POINT('Ctrl Pts',(-0.294923960963645,1.85976402263992,
10.2386561550475));
#75555=CARTESIAN_POINT('Ctrl Pts',(0.0423470420341099,1.72197857785623,
10.2585264985703));
#75556=CARTESIAN_POINT('Ctrl Pts',(0.340770398994764,1.93097632491989,10.2783968420931));
#75557=CARTESIAN_POINT('Ctrl Pts',(0.326583306578408,2.29503028337402,10.2982671856158));
#75558=CARTESIAN_POINT('Ctrl Pts',(0.0128004906788188,2.48017050780803,
10.3181375291386));
#75559=CARTESIAN_POINT('Ctrl Pts',(-0.312725032789138,2.31655604686932,
10.3380078726614));
#75560=CARTESIAN_POINT('Ctrl Pts',(-0.351367912341904,1.95428089437164,
10.3578782161842));
#75561=CARTESIAN_POINT('Ctrl Pts',(-0.0676785667428226,1.72568318342309,
10.377748559707));
#75562=CARTESIAN_POINT('Ctrl Pts',(0.278096650237917,1.84047019305081,10.3976189032298));
#75563=CARTESIAN_POINT('Ctrl Pts',(0.368756050065618,2.19334046876163,10.4174892467526));
#75564=CARTESIAN_POINT('Ctrl Pts',(0.121131975561155,2.46058357154103,10.4373595902754));
#75565=CARTESIAN_POINT('Ctrl Pts',(-0.237614195891286,2.39704033645209,
10.4572299337982));
#75566=CARTESIAN_POINT('Ctrl Pts',(-0.378381690865214,2.06100303105861,
10.4771002773209));
#75567=CARTESIAN_POINT('Ctrl Pts',(-0.172035496486027,1.76074013571092,
10.4969706208437));
#75568=CARTESIAN_POINT('Ctrl Pts',(0.192129845401105,1.77170197978851,10.5168409643665));
#75569=CARTESIAN_POINT('Ctrl Pts',(0.380042210249291,2.0838325636705,10.5367113078893));
#75570=CARTESIAN_POINT('Ctrl Pts',(0.219317585268772,2.4107945693871,10.5565816514121));
#75571=CARTESIAN_POINT('Ctrl Pts',(-0.142601066802718,2.45264486855102,
10.5764519949349));
#75572=CARTESIAN_POINT('Ctrl Pts',(-0.373702653464939,2.17099150908312,
10.5963223384577));
#75573=CARTESIAN_POINT('Ctrl Pts',(-0.261982930595375,1.82421310465271,
10.6161926819805));
#75574=CARTESIAN_POINT('Ctrl Pts',(0.0900704653400429,1.73043163170793,
10.6360630255033));
#75575=CARTESIAN_POINT('Ctrl Pts',(0.359496471312573,1.97567882448093,10.655933369026));
#75576=CARTESIAN_POINT('Ctrl Pts',(0.299133405881053,2.33497377099293,10.6758037125489));
#75577=CARTESIAN_POINT('Ctrl Pts',(-0.0356438361104161,2.47871227140928,
10.6956740560716));
#75578=CARTESIAN_POINT('Ctrl Pts',(-0.337722710940686,2.27503381982779,
10.7155443995944));
#75579=CARTESIAN_POINT('Ctrl Pts',(-0.329986975278303,1.91078566725718,
10.7354147431172));
#75580=CARTESIAN_POINT('Ctrl Pts',(-0.0195331134681825,1.72011590577272,
10.75528508664));
#75581=CARTESIAN_POINT('Ctrl Pts',(0.308839720755723,1.87793808419235,10.7751554301628));
#75582=CARTESIAN_POINT('Ctrl Pts',(0.353894155917617,2.23947183936549,10.7950257736856));
#75583=CARTESIAN_POINT('Ctrl Pts',(0.0742988813639559,2.47305916929718,
10.8148961172084));
#75584=CARTESIAN_POINT('Ctrl Pts',(-0.273455501961803,2.36441549881854,
10.8347664607312));
#75585=CARTESIAN_POINT('Ctrl Pts',(-0.370351689842575,2.01320660509356,
10.8546368042539));
#75586=CARTESIAN_POINT('Ctrl Pts',(-0.12750062112257,1.74161883534148,10.8745071477767));
#75587=CARTESIAN_POINT('Ctrl Pts',(0.232314909835208,1.79879699497366,10.8943774912995));
#75588=CARTESIAN_POINT('Ctrl Pts',(0.379013137838279,2.13228790663111,10.9142478348223));
#75589=CARTESIAN_POINT('Ctrl Pts',(0.178018409854183,2.43615905955607,10.9341181783451));
#75590=CARTESIAN_POINT('Ctrl Pts',(-0.186283974153027,2.43165003926185,
10.9539885218679));
#75591=CARTESIAN_POINT('Ctrl Pts',(-0.379696172147903,2.12289725802071,
10.9738588653907));
#75592=CARTESIAN_POINT('Ctrl Pts',(-0.224788823163257,1.79313935972577,
10.9937292089135));
#75593=CARTESIAN_POINT('Ctrl Pts',(0.136331668838762,1.74488432357853,11.0135995524363));
#75594=CARTESIAN_POINT('Ctrl Pts',(0.372386414561987,2.02239957591415,11.033469895959));
#75595=CARTESIAN_POINT('Ctrl Pts',(0.266827320757131,2.37110265300474,11.0533402394819));
#75596=CARTESIAN_POINT('Ctrl Pts',(-0.0835095145828133,2.47110595325699,
11.0732105830046));
#75597=CARTESIAN_POINT('Ctrl Pts',(-0.357237739086846,2.23067006290943,
11.0930809265274));
#75598=CARTESIAN_POINT('Ctrl Pts',(-0.303248971505297,1.87036217896519,
11.1129512700502));
#75599=CARTESIAN_POINT('Ctrl Pts',(0.028929443812777,1.72071573345402,11.132821613573));
#75600=CARTESIAN_POINT('Ctrl Pts',(0.334569032820766,1.9190109676085,11.1526919570958));
#75601=CARTESIAN_POINT('Ctrl Pts',(0.333287081676621,2.28333899955034,11.1725623006186));
#75602=CARTESIAN_POINT('Ctrl Pts',(0.026259606033199,2.47947845875572,11.1924326441414));
#75603=CARTESIAN_POINT('Ctrl Pts',(-0.304857483223131,2.3274980933799,11.2123029876641));
#75604=CARTESIAN_POINT('Ctrl Pts',(-0.356309334220927,1.96681919839678,
11.232173331187));
#75605=CARTESIAN_POINT('Ctrl Pts',(-0.0808958782067142,1.72831555795567,
11.2520436747097));
#75606=CARTESIAN_POINT('Ctrl Pts',(0.268728533082803,1.83078179282263,11.2719140182325));
#75607=CARTESIAN_POINT('Ctrl Pts',(0.371831099355113,2.18021908202544,11.2917843617553));
#75608=CARTESIAN_POINT('Ctrl Pts',(0.13382925220231,2.4560662843118,11.3116547052781));
#75609=CARTESIAN_POINT('Ctrl Pts',(-0.226942714638603,2.4052711447895,11.3315250488009));
#75610=CARTESIAN_POINT('Ctrl Pts',(-0.379525636259362,2.07443128883647,
11.3513953923237));
#75611=CARTESIAN_POINT('Ctrl Pts',(-0.183945454361969,1.76704724451027,
11.3712657358465));
#75612=CARTESIAN_POINT('Ctrl Pts',(0.180379640000184,1.76510202592127,11.3911360793693));
#75613=CARTESIAN_POINT('Ctrl Pts',(0.379230971132724,2.07038010630728,11.4110064228921));
#75614=CARTESIAN_POINT('Ctrl Pts',(0.23018951388577,2.40283040677195,11.4308767664148));
#75615=CARTESIAN_POINT('Ctrl Pts',(-0.130019484878821,2.45747503566052,
11.4507471099376));
#75616=CARTESIAN_POINT('Ctrl Pts',(-0.370953306821607,2.18418498516215,
11.4706174534604));
#75617=CARTESIAN_POINT('Ctrl Pts',(-0.27158797048811,1.83366667152836,11.4904877969832));
#75618=CARTESIAN_POINT('Ctrl Pts',(0.0769223554047115,1.72747292875869,
11.510358140506));
#75619=CARTESIAN_POINT('Ctrl Pts',(0.354866892246784,1.9630220588717,11.5302284840288));
#75620=CARTESIAN_POINT('Ctrl Pts',(0.30726936621738,2.32422980210713,11.5500988275516));
#75621=CARTESIAN_POINT('Ctrl Pts',(-0.0222059723695601,2.47973722804034,
11.5699691710744));
#75622=CARTESIAN_POINT('Ctrl Pts',(-0.33131035437759,2.28688744380196,11.5898395145972));
#75623=CARTESIAN_POINT('Ctrl Pts',(-0.336482590076081,1.92259387230333,
11.6097098581199));
#75624=CARTESIAN_POINT('Ctrl Pts',(-0.0329778573479846,1.72104627130298,
11.6295802016427));
#75625=CARTESIAN_POINT('Ctrl Pts',(0.300779569967016,1.86713712649052,11.6494505451655));
#75626=CARTESIAN_POINT('Ctrl Pts',(0.358612689278201,2.22684796670539,11.6693208886883));
#75627=CARTESIAN_POINT('Ctrl Pts',(0.0874674868858114,2.47019306625937,
11.6891912322111));
#75628=CARTESIAN_POINT('Ctrl Pts',(-0.263917227101225,2.37393642475552,
11.7090615757339));
#75629=CARTESIAN_POINT('Ctrl Pts',(-0.373193814308984,2.02638040661516,
11.7289319192567));
#75630=CARTESIAN_POINT('Ctrl Pts',(-0.140115882638339,1.74636034300277,
11.7488022627795));
#75631=CARTESIAN_POINT('Ctrl Pts',(0.221499296298022,1.79075652099338,11.7686726063023));
#75632=CARTESIAN_POINT('Ctrl Pts',(0.37991902528722,2.11884149127447,11.7885429498251));
#75633=CARTESIAN_POINT('Ctrl Pts',(0.189814769880288,2.42964195834864,11.8084132933478));
#75634=CARTESIAN_POINT('Ctrl Pts',(-0.174418695944306,2.43804080533824,
11.8282836368706));
#75635=CARTESIAN_POINT('Ctrl Pts',(-0.378646753201302,2.13633323353006,
11.8481539803934));
#75636=CARTESIAN_POINT('Ctrl Pts',(-0.235517962496791,1.80129486628114,
11.8680243239162));
#75637=CARTESIAN_POINT('Ctrl Pts',(0.123666495923183,1.74027779418735,11.887894667439));
#75638=CARTESIAN_POINT('Ctrl Pts',(0.369403780006811,2.00925687417045,11.9077650109618));
#75639=CARTESIAN_POINT('Ctrl Pts',(0.276263385717702,2.3614804185411,11.9276353544846));
#75640=CARTESIAN_POINT('Ctrl Pts',(-0.0703110551035733,2.47383127624485,
11.9475056980074));
#75641=CARTESIAN_POINT('Ctrl Pts',(-0.352384674853132,2.24324283052666,
11.9673760415301));
#75642=CARTESIAN_POINT('Ctrl Pts',(-0.311193328266508,1.88124858855073,
11.987246385053));
#75643=CARTESIAN_POINT('Ctrl Pts',(0.0154755318585352,1.71992898626397,
12.0071167285757));
#75644=CARTESIAN_POINT('Ctrl Pts',(0.327947698306792,1.90727279708377,12.0269870720985));
#75645=CARTESIAN_POINT('Ctrl Pts',(0.339572497606187,2.27141757913975,12.0468574156213));
#75646=CARTESIAN_POINT('Ctrl Pts',(0.0396857589730344,2.47831006873116,
12.0667277591441));
#75647=CARTESIAN_POINT('Ctrl Pts',(-0.296607260789652,2.33815457252695,
12.0865981026669));
#75648=CARTESIAN_POINT('Ctrl Pts',(-0.360803498210152,1.97952467784666,
12.1064684461897));
#75649=CARTESIAN_POINT('Ctrl Pts',(-0.0940116449837155,1.73141449000796,
12.1263387897125));
#75650=CARTESIAN_POINT('Ctrl Pts',(0.259023093985518,1.82143132920085,12.1462091332353));
#75651=CARTESIAN_POINT('Ctrl Pts',(0.374439407033073,2.16699700015191,12.166079476758));
#75652=CARTESIAN_POINT('Ctrl Pts',(0.146358539450022,2.45110204428156,12.1859498202809));
#75653=CARTESIAN_POINT('Ctrl Pts',(-0.21598636316249,2.41311876101007,12.2058201638036));
#75654=CARTESIAN_POINT('Ctrl Pts',(-0.380193181461606,2.08789164178193,
12.2256905073264));
#75655=CARTESIAN_POINT('Ctrl Pts',(-0.195624514397592,1.77377229281475,
12.2455608508492));
#75656=CARTESIAN_POINT('Ctrl Pts',(0.168403012753421,1.75892245329807,12.265431194372));
#75657=CARTESIAN_POINT('Ctrl Pts',(0.377943701703151,2.05696482936533,12.2853015378948));
#75658=CARTESIAN_POINT('Ctrl Pts',(0.240772496729117,2.39448611578046,12.3051718814176));
#75659=CARTESIAN_POINT('Ctrl Pts',(-0.117274695778305,2.46185648163152,
12.3250422249404));
#75660=CARTESIAN_POINT('Ctrl Pts',(-0.367738320417285,2.19727278789728,
12.3449125684632));
#75661=CARTESIAN_POINT('Ctrl Pts',(-0.280852099125076,1.84345455376157,
12.3647829119859));
#75662=CARTESIAN_POINT('Ctrl Pts',(0.063677688553651,1.72498184104086,12.3846532555087));
#75663=CARTESIAN_POINT('Ctrl Pts',(0.349791865918904,1.95053723505297,12.4045235990315));
#75664=CARTESIAN_POINT('Ctrl Pts',(0.31501962616606,2.31320436838591,12.4243939425543));
#75665=CARTESIAN_POINT('Ctrl Pts',(-0.00874023454461976,2.48028551887856,
12.4442642860771));
#75666=CARTESIAN_POINT('Ctrl Pts',(-0.324482119936101,2.29850647699864,
12.4641346295999));
#75667=CARTESIAN_POINT('Ctrl Pts',(-0.342555834537934,1.93462476668903,
12.4840049731227));
#75668=CARTESIAN_POINT('Ctrl Pts',(-0.0463812057169993,1.72245231913721,
12.5038753166455));
#75669=CARTESIAN_POINT('Ctrl Pts',(0.292341865118294,1.85662847030148,12.5237456601683));
#75670=CARTESIAN_POINT('Ctrl Pts',(0.362881073458691,2.21406486792219,12.543616003691));
#75671=CARTESIAN_POINT('Ctrl Pts',(0.10052629869794,2.46686227775383,12.5634863472138));
#75672=CARTESIAN_POINT('Ctrl Pts',(-0.254047669698381,2.38311349153557,
12.5833566907366));
#75673=CARTESIAN_POINT('Ctrl Pts',(-0.375567486613633,2.03964661925494,
12.6032270342594));
#75674=CARTESIAN_POINT('Ctrl Pts',(-0.15255526345726,1.75154575743705,12.6230973777822));
#75675=CARTESIAN_POINT('Ctrl Pts',(0.210405645397383,1.78310422540914,12.642967721305));
#75676=CARTESIAN_POINT('Ctrl Pts',(0.380348018742057,2.10537142510428,12.6628380648278));
#75677=CARTESIAN_POINT('Ctrl Pts',(0.201372864597873,2.42271107351973,12.6827084083506));
#75678=CARTESIAN_POINT('Ctrl Pts',(-0.162334478374657,2.44400724512638,
12.7025787518734));
#75679=CARTESIAN_POINT('Ctrl Pts',(-0.377122037282437,2.14972360168702,
12.7224490953962));
#75680=CARTESIAN_POINT('Ctrl Pts',(-0.245951467512236,1.80982532295701,
12.7423194389189));
#75681=CARTESIAN_POINT('Ctrl Pts',(0.110846090430305,1.73612280669869,12.7621897824417));
#75682=CARTESIAN_POINT('Ctrl Pts',(0.365957450738205,1.9962280778879,12.7820601259645));
#75683=CARTESIAN_POINT('Ctrl Pts',(0.285352670596945,2.35152996034297,12.8019304694873));
#75684=CARTESIAN_POINT('Ctrl Pts',(-0.0570243375491358,2.4760873468963,
12.8218008130101));
#75685=CARTESIAN_POINT('Ctrl Pts',(-0.347089279175034,2.25563579233946,
12.8416711565329));
#75686=CARTESIAN_POINT('Ctrl Pts',(-0.318747059060556,1.89240958621453,
12.8615415000557));
#75687=CARTESIAN_POINT('Ctrl Pts',(0.00200219417929206,1.71961932384814,
12.8814118435785));
#75688=CARTESIAN_POINT('Ctrl Pts',(0.320914706966654,1.89577654771104,12.9012821871013));
#75689=CARTESIAN_POINT('Ctrl Pts',(0.34543166444848,2.25928098651166,12.9211525306241));
#75690=CARTESIAN_POINT('Ctrl Pts',(0.053062096566406,2.47666680438407,12.9410228741468));
#75691=CARTESIAN_POINT('Ctrl Pts',(-0.287984722112476,2.34851210769668,
12.9608932176696));
#75692=CARTESIAN_POINT('Ctrl Pts',(-0.364844762004644,1.99238138424405,
12.9807635611924));
#75693=CARTESIAN_POINT('Ctrl Pts',(-0.107009405407698,1.73497608945314,
13.0006339047152));
#75694=CARTESIAN_POINT('Ctrl Pts',(0.248992519416547,1.81243053973104,13.020504248238));
#75695=CARTESIAN_POINT('Ctrl Pts',(0.376577691887735,2.15369081948738,13.0403745917608));
#75696=CARTESIAN_POINT('Ctrl Pts',(0.158704123625383,2.44569708415774,13.0602449352836));
#75697=CARTESIAN_POINT('Ctrl Pts',(-0.204758920883683,2.4205733318059,13.0801152788064));
#75698=CARTESIAN_POINT('Ctrl Pts',(-0.380383437610339,2.10136719872242,
13.0999856223292));
#75699=CARTESIAN_POINT('Ctrl Pts',(-0.207058114507318,1.78090682944761,
13.1198559658519));
#75700=CARTESIAN_POINT('Ctrl Pts',(0.15621518622102,1.75317103722726,13.1397263093748));
#75701=CARTESIAN_POINT('Ctrl Pts',(0.376181654050325,2.04360353697775,13.1595966528975));
#75702=CARTESIAN_POINT('Ctrl Pts',(0.251053950043987,2.38577223880439,13.1794669964203));
#75703=CARTESIAN_POINT('Ctrl Pts',(-0.104384046596784,2.46578357528926,
13.1993373399431));
#75704=CARTESIAN_POINT('Ctrl Pts',(-0.364059131517509,2.21023874178026,
13.2192076834659));
#75705=CARTESIAN_POINT('Ctrl Pts',(-0.289768691805461,1.8535639778927,13.2390780269887));
#75706=CARTESIAN_POINT('Ctrl Pts',(0.0503627275349631,1.72296243378388,
13.2589483705115));
#75707=CARTESIAN_POINT('Ctrl Pts',(0.344259201917073,1.93823821766884,13.2788187140342));
#75708=CARTESIAN_POINT('Ctrl Pts',(0.322410207608711,2.301914788788,13.2986890575571));
#75709=CARTESIAN_POINT('Ctrl Pts',(0.00466758125033996,2.48034976167427,
13.3185594010798));
#75710=CARTESIAN_POINT('Ctrl Pts',(-0.317113500057357,2.30988916395447,
13.3384297446026));
#75711=CARTESIAN_POINT('Ctrl Pts',(-0.348459136713594,1.94683912960278,
13.3583000881254));
#75712=CARTESIAN_POINT('Ctrl Pts',(-0.0591901415483071,1.72437322969919,
13.3781704316482));
#75713=CARTESIAN_POINT('Ctrl Pts',(0.168392742651259,1.80571626482623,13.3914173273301));
#75714=CARTESIAN_POINT('Ctrl Pts',(0.239789855056149,1.88554969340314,13.398040775171));
#75715=CARTESIAN_POINT('Origin',(0.35,2.1,3.1));
#75716=CARTESIAN_POINT('',(-0.35,2.1,3.1));
#75717=CARTESIAN_POINT('Origin',(0.,2.1,3.1));
#75718=CARTESIAN_POINT('Origin',(0.,2.1,3.125));
#75719=CARTESIAN_POINT('',(-0.375,2.1,3.125));
#75720=CARTESIAN_POINT('Origin',(0.,2.1,13.42));
#75721=CARTESIAN_POINT('',(-0.36,2.1,13.44));
#75722=CARTESIAN_POINT('',(-0.38,2.1,13.42));
#75723=CARTESIAN_POINT('Origin',(0.,2.1,13.44));
#75724=CARTESIAN_POINT('Origin',(0.,2.1,13.44));
#75725=CARTESIAN_POINT('',(0.,0.,0.));
#75726=CARTESIAN_POINT('Origin',(-0.75,1.45,6.));
#75727=CARTESIAN_POINT('',(-0.755074409108712,1.3000858566639,9.2));
#75728=CARTESIAN_POINT('',(-0.9,1.45,9.2));
#75729=CARTESIAN_POINT('Origin',(-0.75,1.45,9.2));
#75730=CARTESIAN_POINT('',(-0.9,1.45,6.));
#75731=CARTESIAN_POINT('',(-0.9,1.45,6.));
#75732=CARTESIAN_POINT('',(-0.75,1.3,6.));
#75733=CARTESIAN_POINT('Origin',(-0.75,1.45,6.));
#75734=CARTESIAN_POINT('',(-0.75,1.3,9.2));
#75735=CARTESIAN_POINT('',(-0.75,1.3,6.));
#75736=CARTESIAN_POINT('Origin',(-0.75,1.45,9.2));
#75737=CARTESIAN_POINT('Origin',(0.,2.1,9.2));
#75738=CARTESIAN_POINT('',(-0.9,1.46754446796632,9.2));
#75739=CARTESIAN_POINT('Origin',(0.,2.1,9.2));
#75740=CARTESIAN_POINT('',(-0.9,2.9,9.2));
#75741=CARTESIAN_POINT('Origin',(0.75,1.45,6.));
#75742=CARTESIAN_POINT('',(0.9,1.45,9.2));
#75743=CARTESIAN_POINT('',(0.755074409108712,1.3000858566639,9.2));
#75744=CARTESIAN_POINT('Origin',(0.75,1.45,9.2));
#75745=CARTESIAN_POINT('',(0.75,1.3,9.2));
#75746=CARTESIAN_POINT('Origin',(0.75,1.45,9.2));
#75747=CARTESIAN_POINT('',(0.75,1.3,6.));
#75748=CARTESIAN_POINT('',(0.75,1.3,6.));
#75749=CARTESIAN_POINT('',(0.9,1.45,6.));
#75750=CARTESIAN_POINT('Origin',(0.75,1.45,6.));
#75751=CARTESIAN_POINT('',(0.9,1.45,6.));
#75752=CARTESIAN_POINT('Origin',(-0.9,1.3,6.));
#75753=CARTESIAN_POINT('',(-0.9,1.3,6.));
#75754=CARTESIAN_POINT('',(-0.9,1.3,9.2));
#75755=CARTESIAN_POINT('Origin',(0.75,2.75,6.));
#75756=CARTESIAN_POINT('',(0.755074409108712,2.8999141433361,9.2));
#75757=CARTESIAN_POINT('',(0.9,2.75,9.2));
#75758=CARTESIAN_POINT('Origin',(0.75,2.75,9.2));
#75759=CARTESIAN_POINT('',(0.9,2.75,6.));
#75760=CARTESIAN_POINT('',(0.9,2.75,6.));
#75761=CARTESIAN_POINT('',(0.75,2.9,6.));
#75762=CARTESIAN_POINT('Origin',(0.75,2.75,6.));
#75763=CARTESIAN_POINT('',(0.75,2.9,9.2));
#75764=CARTESIAN_POINT('',(0.75,2.9,6.));
#75765=CARTESIAN_POINT('Origin',(0.75,2.75,9.2));
#75766=CARTESIAN_POINT('Origin',(0.,2.1,9.2));
#75767=CARTESIAN_POINT('',(0.9,2.73245553203368,9.2));
#75768=CARTESIAN_POINT('Origin',(0.,2.1,9.2));
#75769=CARTESIAN_POINT('',(0.9,1.3,9.2));
#75770=CARTESIAN_POINT('Origin',(-0.75,2.75,6.));
#75771=CARTESIAN_POINT('',(-0.9,2.75,9.2));
#75772=CARTESIAN_POINT('',(-0.755074409108712,2.8999141433361,9.2));
#75773=CARTESIAN_POINT('Origin',(-0.75,2.75,9.2));
#75774=CARTESIAN_POINT('',(-0.75,2.9,9.2));
#75775=CARTESIAN_POINT('Origin',(-0.75,2.75,9.2));
#75776=CARTESIAN_POINT('',(-0.75,2.9,6.));
#75777=CARTESIAN_POINT('',(-0.75,2.9,6.));
#75778=CARTESIAN_POINT('',(-0.9,2.75,6.));
#75779=CARTESIAN_POINT('Origin',(-0.75,2.75,6.));
#75780=CARTESIAN_POINT('',(-0.9,2.75,6.));
#75781=CARTESIAN_POINT('Origin',(0.9,2.9,6.));
#75782=CARTESIAN_POINT('',(0.9,2.9,6.));
#75783=CARTESIAN_POINT('',(0.9,2.9,9.2));
#75784=CARTESIAN_POINT('',(0.5,2.9,6.3));
#75785=CARTESIAN_POINT('',(0.5,2.9,6.9));
#75786=CARTESIAN_POINT('',(0.5,2.9,6.15));
#75787=CARTESIAN_POINT('',(-0.5,2.9,6.9));
#75788=CARTESIAN_POINT('',(0.7,2.9,6.9));
#75789=CARTESIAN_POINT('',(-0.5,2.9,6.3));
#75790=CARTESIAN_POINT('',(-0.5,2.9,6.45));
#75791=CARTESIAN_POINT('',(0.2,2.9,6.3));
#75792=CARTESIAN_POINT('Origin',(0.5,2.9,6.3));
#75793=CARTESIAN_POINT('',(0.5,2.6,6.3));
#75794=CARTESIAN_POINT('',(0.5,2.9,6.3));
#75795=CARTESIAN_POINT('',(0.5,2.6,6.9));
#75796=CARTESIAN_POINT('',(0.5,2.6,6.3));
#75797=CARTESIAN_POINT('',(0.5,2.9,6.9));
#75798=CARTESIAN_POINT('Origin',(-0.5,2.9,6.3));
#75799=CARTESIAN_POINT('',(-0.5,2.6,6.3));
#75800=CARTESIAN_POINT('',(-0.5,2.9,6.3));
#75801=CARTESIAN_POINT('',(-0.5,2.6,6.3));
#75802=CARTESIAN_POINT('Origin',(-0.5,2.9,6.9));
#75803=CARTESIAN_POINT('',(-0.5,2.6,6.9));
#75804=CARTESIAN_POINT('',(-0.5,2.9,6.9));
#75805=CARTESIAN_POINT('',(-0.5,2.6,6.9));
#75806=CARTESIAN_POINT('Origin',(0.5,2.9,6.9));
#75807=CARTESIAN_POINT('',(0.5,2.6,6.9));
#75808=CARTESIAN_POINT('Origin',(0.,2.6,6.6));
#75809=CARTESIAN_POINT('Origin',(-0.9,2.1,7.4));
#75810=CARTESIAN_POINT('',(-0.9,2.1,7.7));
#75811=CARTESIAN_POINT('Origin',(-0.9,2.1,7.4));
#75812=CARTESIAN_POINT('',(-0.4025,2.1,7.7));
#75813=CARTESIAN_POINT('',(-0.9,2.1,7.7));
#75814=CARTESIAN_POINT('',(-0.26833980323463,1.8,7.4));
#75815=CARTESIAN_POINT('Ctrl Pts',(-0.26833980323463,1.8,7.4));
#75816=CARTESIAN_POINT('Ctrl Pts',(-0.26833980323463,1.8,7.4201160976737));
#75817=CARTESIAN_POINT('Ctrl Pts',(-0.270671600644359,1.8020440352048,7.44032404072543));
#75818=CARTESIAN_POINT('Ctrl Pts',(-0.279265580045418,1.81008344690125,
7.47970055135893));
#75819=CARTESIAN_POINT('Ctrl Pts',(-0.285490508258182,1.81607405099208,
7.49887821451971));
#75820=CARTESIAN_POINT('Ctrl Pts',(-0.307328099584212,1.83922089052474,
7.55348515936485));
#75821=CARTESIAN_POINT('Ctrl Pts',(-0.325904486897266,1.86181444421644,
7.58607851292837));
#75822=CARTESIAN_POINT('Ctrl Pts',(-0.357891266971383,1.91339295489154,
7.63765702360347));
#75823=CARTESIAN_POINT('Ctrl Pts',(-0.373877283104246,1.94605224242681,
7.66056900592672));
#75824=CARTESIAN_POINT('Ctrl Pts',(-0.396259291153439,2.01960899212744,
7.69177630545863));
#75825=CARTESIAN_POINT('Ctrl Pts',(-0.4025,2.06058397109581,7.7));
#75826=CARTESIAN_POINT('Ctrl Pts',(-0.4025,2.1,7.7));
#75827=CARTESIAN_POINT('',(-0.4025,2.1,7.1));
#75828=CARTESIAN_POINT('Ctrl Pts',(-0.4025,2.1,7.1));
#75829=CARTESIAN_POINT('Ctrl Pts',(-0.4025,2.0605839710958,7.1));
#75830=CARTESIAN_POINT('Ctrl Pts',(-0.396259291153439,2.01960899212744,
7.10822369454137));
#75831=CARTESIAN_POINT('Ctrl Pts',(-0.373877283104246,1.94605224242681,
7.13943099407328));
#75832=CARTESIAN_POINT('Ctrl Pts',(-0.357891266971382,1.91339295489154,
7.16234297639653));
#75833=CARTESIAN_POINT('Ctrl Pts',(-0.325904486897266,1.86181444421644,
7.21392148707163));
#75834=CARTESIAN_POINT('Ctrl Pts',(-0.307328099584211,1.83922089052474,
7.24651484063515));
#75835=CARTESIAN_POINT('Ctrl Pts',(-0.285490508258181,1.81607405099208,
7.3011217854803));
#75836=CARTESIAN_POINT('Ctrl Pts',(-0.279265580045417,1.81008344690125,
7.32029944864107));
#75837=CARTESIAN_POINT('Ctrl Pts',(-0.270671600644359,1.8020440352048,7.35967595927457));
#75838=CARTESIAN_POINT('Ctrl Pts',(-0.26833980323463,1.8,7.3798839023263));
#75839=CARTESIAN_POINT('Ctrl Pts',(-0.26833980323463,1.8,7.4));
#75840=CARTESIAN_POINT('Ctrl Pts',(-0.4025,2.1,7.7));
#75841=CARTESIAN_POINT('Ctrl Pts',(-0.4025,2.1394160289042,7.7));
#75842=CARTESIAN_POINT('Ctrl Pts',(-0.396259291153439,2.18039100787256,
7.69177630545863));
#75843=CARTESIAN_POINT('Ctrl Pts',(-0.373877283104246,2.25394775757319,
7.66056900592672));
#75844=CARTESIAN_POINT('Ctrl Pts',(-0.357891266971382,2.28660704510846,
7.63765702360347));
#75845=CARTESIAN_POINT('Ctrl Pts',(-0.325904486897266,2.33818555578356,
7.58607851292837));
#75846=CARTESIAN_POINT('Ctrl Pts',(-0.307328099584212,2.36077910947526,
7.55348515936485));
#75847=CARTESIAN_POINT('Ctrl Pts',(-0.285490508258182,2.38392594900792,
7.49887821451971));
#75848=CARTESIAN_POINT('Ctrl Pts',(-0.279265580045418,2.38991655309875,
7.47970055135893));
#75849=CARTESIAN_POINT('Ctrl Pts',(-0.270671600644359,2.3979559647952,7.44032404072543));
#75850=CARTESIAN_POINT('Ctrl Pts',(-0.26833980323463,2.4,7.4201160976737));
#75851=CARTESIAN_POINT('Ctrl Pts',(-0.26833980323463,2.4,7.3798839023263));
#75852=CARTESIAN_POINT('Ctrl Pts',(-0.27067160064436,2.3979559647952,7.35967595927457));
#75853=CARTESIAN_POINT('Ctrl Pts',(-0.279265580045418,2.38991655309875,
7.32029944864107));
#75854=CARTESIAN_POINT('Ctrl Pts',(-0.285490508258181,2.38392594900792,
7.3011217854803));
#75855=CARTESIAN_POINT('Ctrl Pts',(-0.307328099584212,2.36077910947526,
7.24651484063515));
#75856=CARTESIAN_POINT('Ctrl Pts',(-0.325904486897266,2.33818555578356,
7.21392148707163));
#75857=CARTESIAN_POINT('Ctrl Pts',(-0.357891266971382,2.28660704510846,
7.16234297639653));
#75858=CARTESIAN_POINT('Ctrl Pts',(-0.373877283104246,2.25394775757319,
7.13943099407329));
#75859=CARTESIAN_POINT('Ctrl Pts',(-0.396259291153439,2.18039100787256,
7.10822369454138));
#75860=CARTESIAN_POINT('Ctrl Pts',(-0.4025,2.1394160289042,7.1));
#75861=CARTESIAN_POINT('Ctrl Pts',(-0.4025,2.1,7.1));
#75862=CARTESIAN_POINT('Origin',(-0.9,2.1,7.4));
#75863=CARTESIAN_POINT('',(0.26833980323463,1.8,7.4));
#75864=CARTESIAN_POINT('',(0.4025,2.1,7.7));
#75865=CARTESIAN_POINT('Ctrl Pts',(0.26833980323463,1.8,7.4));
#75866=CARTESIAN_POINT('Ctrl Pts',(0.26833980323463,1.8,7.3798839023263));
#75867=CARTESIAN_POINT('Ctrl Pts',(0.27067160064436,1.8020440352048,7.35967595927457));
#75868=CARTESIAN_POINT('Ctrl Pts',(0.279265580045418,1.81008344690125,7.32029944864107));
#75869=CARTESIAN_POINT('Ctrl Pts',(0.285490508258181,1.81607405099208,7.3011217854803));
#75870=CARTESIAN_POINT('Ctrl Pts',(0.307328099584211,1.83922089052474,7.24651484063515));
#75871=CARTESIAN_POINT('Ctrl Pts',(0.325904486897266,1.86181444421644,7.21392148707163));
#75872=CARTESIAN_POINT('Ctrl Pts',(0.357891266971382,1.91339295489154,7.16234297639653));
#75873=CARTESIAN_POINT('Ctrl Pts',(0.373877283104246,1.94605224242681,7.13943099407328));
#75874=CARTESIAN_POINT('Ctrl Pts',(0.396259291153439,2.01960899212744,7.10822369454137));
#75875=CARTESIAN_POINT('Ctrl Pts',(0.4025,2.0605839710958,7.1));
#75876=CARTESIAN_POINT('Ctrl Pts',(0.4025,2.1394160289042,7.1));
#75877=CARTESIAN_POINT('Ctrl Pts',(0.396259291153439,2.18039100787256,7.10822369454137));
#75878=CARTESIAN_POINT('Ctrl Pts',(0.373877283104246,2.25394775757319,7.13943099407328));
#75879=CARTESIAN_POINT('Ctrl Pts',(0.357891266971382,2.28660704510846,7.16234297639653));
#75880=CARTESIAN_POINT('Ctrl Pts',(0.325904486897266,2.33818555578356,7.21392148707163));
#75881=CARTESIAN_POINT('Ctrl Pts',(0.307328099584211,2.36077910947526,7.24651484063515));
#75882=CARTESIAN_POINT('Ctrl Pts',(0.285490508258181,2.38392594900792,7.3011217854803));
#75883=CARTESIAN_POINT('Ctrl Pts',(0.279265580045418,2.38991655309875,7.32029944864107));
#75884=CARTESIAN_POINT('Ctrl Pts',(0.27067160064436,2.3979559647952,7.35967595927456));
#75885=CARTESIAN_POINT('Ctrl Pts',(0.26833980323463,2.4,7.3798839023263));
#75886=CARTESIAN_POINT('Ctrl Pts',(0.26833980323463,2.4,7.4201160976737));
#75887=CARTESIAN_POINT('Ctrl Pts',(0.270671600644359,2.3979559647952,7.44032404072543));
#75888=CARTESIAN_POINT('Ctrl Pts',(0.279265580045417,2.38991655309875,7.47970055135893));
#75889=CARTESIAN_POINT('Ctrl Pts',(0.285490508258181,2.38392594900792,7.4988782145197));
#75890=CARTESIAN_POINT('Ctrl Pts',(0.307328099584211,2.36077910947526,7.55348515936485));
#75891=CARTESIAN_POINT('Ctrl Pts',(0.325904486897266,2.33818555578356,7.58607851292837));
#75892=CARTESIAN_POINT('Ctrl Pts',(0.357891266971382,2.28660704510846,7.63765702360347));
#75893=CARTESIAN_POINT('Ctrl Pts',(0.373877283104246,2.25394775757319,7.66056900592671));
#75894=CARTESIAN_POINT('Ctrl Pts',(0.396259291153439,2.18039100787256,7.69177630545863));
#75895=CARTESIAN_POINT('Ctrl Pts',(0.4025,2.1394160289042,7.7));
#75896=CARTESIAN_POINT('Ctrl Pts',(0.4025,2.1,7.7));
#75897=CARTESIAN_POINT('Ctrl Pts',(0.4025,2.1,7.7));
#75898=CARTESIAN_POINT('Ctrl Pts',(0.4025,2.06058397109581,7.7));
#75899=CARTESIAN_POINT('Ctrl Pts',(0.396259291153439,2.01960899212744,7.69177630545863));
#75900=CARTESIAN_POINT('Ctrl Pts',(0.373877283104246,1.94605224242681,7.66056900592672));
#75901=CARTESIAN_POINT('Ctrl Pts',(0.357891266971382,1.91339295489154,7.63765702360347));
#75902=CARTESIAN_POINT('Ctrl Pts',(0.325904486897266,1.86181444421644,7.58607851292837));
#75903=CARTESIAN_POINT('Ctrl Pts',(0.307328099584212,1.83922089052474,7.55348515936485));
#75904=CARTESIAN_POINT('Ctrl Pts',(0.285490508258182,1.81607405099208,7.49887821451971));
#75905=CARTESIAN_POINT('Ctrl Pts',(0.279265580045418,1.81008344690125,7.47970055135894));
#75906=CARTESIAN_POINT('Ctrl Pts',(0.27067160064436,1.8020440352048,7.44032404072544));
#75907=CARTESIAN_POINT('Ctrl Pts',(0.26833980323463,1.8,7.4201160976737));
#75908=CARTESIAN_POINT('Ctrl Pts',(0.26833980323463,1.8,7.4));
#75909=CARTESIAN_POINT('',(0.9,2.1,7.7));
#75910=CARTESIAN_POINT('',(-0.9,2.1,7.7));
#75911=CARTESIAN_POINT('Origin',(0.9,2.1,7.4));
#75912=CARTESIAN_POINT('Origin',(-0.9,2.1,8.8));
#75913=CARTESIAN_POINT('',(-0.9,2.1,9.));
#75914=CARTESIAN_POINT('Origin',(-0.9,2.1,8.8));
#75915=CARTESIAN_POINT('',(-0.4025,2.1,9.));
#75916=CARTESIAN_POINT('',(-0.9,2.1,9.));
#75917=CARTESIAN_POINT('',(-0.349293930665851,1.9,8.8));
#75918=CARTESIAN_POINT('Ctrl Pts',(-0.349293930665851,1.9,8.8));
#75919=CARTESIAN_POINT('Ctrl Pts',(-0.349293930665851,1.9,8.82565270096287));
#75920=CARTESIAN_POINT('Ctrl Pts',(-0.352420767781585,1.90521995494474,
8.85261753143099));
#75921=CARTESIAN_POINT('Ctrl Pts',(-0.36301047494859,1.92575005043977,8.9017095986343));
#75922=CARTESIAN_POINT('Ctrl Pts',(-0.370257522731817,1.94104625437123,
8.92388896684585));
#75923=CARTESIAN_POINT('Ctrl Pts',(-0.383399376780438,1.97606457955938,
8.958907292034));
#75924=CARTESIAN_POINT('Ctrl Pts',(-0.390233771050516,1.99825967753044,
8.97423762194434));
#75925=CARTESIAN_POINT('Ctrl Pts',(-0.399836030760712,2.04742017386295,
8.99479529221648));
#75926=CARTESIAN_POINT('Ctrl Pts',(-0.4025,2.07441526810562,9.));
#75927=CARTESIAN_POINT('Ctrl Pts',(-0.4025,2.1,9.));
#75928=CARTESIAN_POINT('',(-0.4025,2.1,8.6));
#75929=CARTESIAN_POINT('Ctrl Pts',(-0.4025,2.1,8.6));
#75930=CARTESIAN_POINT('Ctrl Pts',(-0.4025,2.07441526810562,8.6));
#75931=CARTESIAN_POINT('Ctrl Pts',(-0.399836030760712,2.04742017386295,
8.60520470778352));
#75932=CARTESIAN_POINT('Ctrl Pts',(-0.390233771050516,1.99825967753044,
8.62576237805566));
#75933=CARTESIAN_POINT('Ctrl Pts',(-0.383399376780438,1.97606457955938,
8.641092707966));
#75934=CARTESIAN_POINT('Ctrl Pts',(-0.370257522731817,1.94104625437123,
8.67611103315415));
#75935=CARTESIAN_POINT('Ctrl Pts',(-0.36301047494859,1.92575005043977,8.6982904013657));
#75936=CARTESIAN_POINT('Ctrl Pts',(-0.352420767781585,1.90521995494474,
8.74738246856901));
#75937=CARTESIAN_POINT('Ctrl Pts',(-0.349293930665851,1.9,8.77434729903714));
#75938=CARTESIAN_POINT('Ctrl Pts',(-0.349293930665851,1.9,8.8));
#75939=CARTESIAN_POINT('Ctrl Pts',(-0.4025,2.1,9.));
#75940=CARTESIAN_POINT('Ctrl Pts',(-0.4025,2.12558473189438,9.));
#75941=CARTESIAN_POINT('Ctrl Pts',(-0.399836030760712,2.15257982613705,
8.99479529221648));
#75942=CARTESIAN_POINT('Ctrl Pts',(-0.390233771050516,2.20174032246956,
8.97423762194434));
#75943=CARTESIAN_POINT('Ctrl Pts',(-0.383399376780438,2.22393542044062,
8.958907292034));
#75944=CARTESIAN_POINT('Ctrl Pts',(-0.370257522731817,2.25895374562877,
8.92388896684585));
#75945=CARTESIAN_POINT('Ctrl Pts',(-0.36301047494859,2.27424994956023,8.9017095986343));
#75946=CARTESIAN_POINT('Ctrl Pts',(-0.352420767781585,2.29478004505526,
8.85261753143099));
#75947=CARTESIAN_POINT('Ctrl Pts',(-0.349293930665851,2.3,8.82565270096287));
#75948=CARTESIAN_POINT('Ctrl Pts',(-0.349293930665851,2.3,8.77434729903714));
#75949=CARTESIAN_POINT('Ctrl Pts',(-0.352420767781585,2.29478004505526,
8.74738246856901));
#75950=CARTESIAN_POINT('Ctrl Pts',(-0.36301047494859,2.27424994956023,8.6982904013657));
#75951=CARTESIAN_POINT('Ctrl Pts',(-0.370257522731817,2.25895374562877,
8.67611103315415));
#75952=CARTESIAN_POINT('Ctrl Pts',(-0.383399376780438,2.22393542044062,
8.641092707966));
#75953=CARTESIAN_POINT('Ctrl Pts',(-0.390233771050516,2.20174032246956,
8.62576237805566));
#75954=CARTESIAN_POINT('Ctrl Pts',(-0.399836030760712,2.15257982613705,
8.60520470778352));
#75955=CARTESIAN_POINT('Ctrl Pts',(-0.4025,2.12558473189438,8.6));
#75956=CARTESIAN_POINT('Ctrl Pts',(-0.4025,2.1,8.6));
#75957=CARTESIAN_POINT('Origin',(-0.9,2.1,8.8));
#75958=CARTESIAN_POINT('',(0.349293930665851,1.9,8.8));
#75959=CARTESIAN_POINT('',(0.4025,2.1,9.));
#75960=CARTESIAN_POINT('Ctrl Pts',(0.349293930665851,1.9,8.8));
#75961=CARTESIAN_POINT('Ctrl Pts',(0.349293930665851,1.9,8.77434729903714));
#75962=CARTESIAN_POINT('Ctrl Pts',(0.352420767781585,1.90521995494474,8.74738246856901));
#75963=CARTESIAN_POINT('Ctrl Pts',(0.36301047494859,1.92575005043977,8.6982904013657));
#75964=CARTESIAN_POINT('Ctrl Pts',(0.370257522731817,1.94104625437123,8.67611103315415));
#75965=CARTESIAN_POINT('Ctrl Pts',(0.383399376780438,1.97606457955938,8.641092707966));
#75966=CARTESIAN_POINT('Ctrl Pts',(0.390233771050516,1.99825967753044,8.62576237805566));
#75967=CARTESIAN_POINT('Ctrl Pts',(0.399836030760712,2.04742017386295,8.60520470778352));
#75968=CARTESIAN_POINT('Ctrl Pts',(0.4025,2.07441526810562,8.6));
#75969=CARTESIAN_POINT('Ctrl Pts',(0.4025,2.12558473189438,8.6));
#75970=CARTESIAN_POINT('Ctrl Pts',(0.399836030760712,2.15257982613705,8.60520470778352));
#75971=CARTESIAN_POINT('Ctrl Pts',(0.390233771050516,2.20174032246956,8.62576237805566));
#75972=CARTESIAN_POINT('Ctrl Pts',(0.383399376780438,2.22393542044062,8.641092707966));
#75973=CARTESIAN_POINT('Ctrl Pts',(0.370257522731817,2.25895374562877,8.67611103315415));
#75974=CARTESIAN_POINT('Ctrl Pts',(0.36301047494859,2.27424994956023,8.6982904013657));
#75975=CARTESIAN_POINT('Ctrl Pts',(0.352420767781585,2.29478004505526,8.74738246856901));
#75976=CARTESIAN_POINT('Ctrl Pts',(0.349293930665851,2.3,8.77434729903714));
#75977=CARTESIAN_POINT('Ctrl Pts',(0.349293930665851,2.3,8.82565270096287));
#75978=CARTESIAN_POINT('Ctrl Pts',(0.352420767781585,2.29478004505526,8.85261753143099));
#75979=CARTESIAN_POINT('Ctrl Pts',(0.36301047494859,2.27424994956023,8.9017095986343));
#75980=CARTESIAN_POINT('Ctrl Pts',(0.370257522731817,2.25895374562877,8.92388896684585));
#75981=CARTESIAN_POINT('Ctrl Pts',(0.383399376780438,2.22393542044062,8.958907292034));
#75982=CARTESIAN_POINT('Ctrl Pts',(0.390233771050516,2.20174032246956,8.97423762194434));
#75983=CARTESIAN_POINT('Ctrl Pts',(0.399836030760712,2.15257982613705,8.99479529221648));
#75984=CARTESIAN_POINT('Ctrl Pts',(0.4025,2.12558473189438,9.));
#75985=CARTESIAN_POINT('Ctrl Pts',(0.4025,2.1,9.));
#75986=CARTESIAN_POINT('Ctrl Pts',(0.4025,2.1,9.));
#75987=CARTESIAN_POINT('Ctrl Pts',(0.4025,2.07441526810562,9.));
#75988=CARTESIAN_POINT('Ctrl Pts',(0.399836030760712,2.04742017386295,8.99479529221648));
#75989=CARTESIAN_POINT('Ctrl Pts',(0.390233771050516,1.99825967753044,8.97423762194434));
#75990=CARTESIAN_POINT('Ctrl Pts',(0.383399376780438,1.97606457955938,8.958907292034));
#75991=CARTESIAN_POINT('Ctrl Pts',(0.370257522731817,1.94104625437123,8.92388896684585));
#75992=CARTESIAN_POINT('Ctrl Pts',(0.36301047494859,1.92575005043977,8.9017095986343));
#75993=CARTESIAN_POINT('Ctrl Pts',(0.352420767781585,1.90521995494474,8.85261753143099));
#75994=CARTESIAN_POINT('Ctrl Pts',(0.349293930665851,1.9,8.82565270096286));
#75995=CARTESIAN_POINT('Ctrl Pts',(0.349293930665851,1.9,8.8));
#75996=CARTESIAN_POINT('',(0.9,2.1,9.));
#75997=CARTESIAN_POINT('',(-0.9,2.1,9.));
#75998=CARTESIAN_POINT('Origin',(0.9,2.1,8.8));
#75999=CARTESIAN_POINT('Origin',(0.,2.1,9.4));
#76000=CARTESIAN_POINT('',(-0.4025,2.1,9.4));
#76001=CARTESIAN_POINT('Origin',(0.,2.1,9.4));
#76002=CARTESIAN_POINT('',(-0.4025,2.1,9.4));
#76003=CARTESIAN_POINT('',(-0.4025,2.1,9.4));
#76004=CARTESIAN_POINT('',(-0.4025,2.1,6.));
#76005=CARTESIAN_POINT('',(-0.4025,2.1,9.4));
#76006=CARTESIAN_POINT('Origin',(0.,2.1,6.));
#76007=CARTESIAN_POINT('Origin',(0.,2.1,9.2));
#76008=CARTESIAN_POINT('',(-0.9,2.73245553203368,9.2));
#76009=CARTESIAN_POINT('',(-0.9,2.9,9.2));
#76010=CARTESIAN_POINT('',(-1.1,2.1,9.2));
#76011=CARTESIAN_POINT('Origin',(0.,2.1,9.2));
#76012=CARTESIAN_POINT('Origin',(0.,2.1,9.2));
#76013=CARTESIAN_POINT('Origin',(0.,2.1,9.2));
#76014=CARTESIAN_POINT('Origin',(0.,2.1,9.2));
#76015=CARTESIAN_POINT('Origin',(0.,2.1,9.2));
#76016=CARTESIAN_POINT('',(0.9,1.46754446796632,9.2));
#76017=CARTESIAN_POINT('',(0.9,1.3,9.2));
#76018=CARTESIAN_POINT('Origin',(0.,2.1,9.2));
#76019=CARTESIAN_POINT('Origin',(0.,2.1,9.2));
#76020=CARTESIAN_POINT('Origin',(0.,2.1,9.2));
#76021=CARTESIAN_POINT('Origin',(0.,2.1,9.2));
#76022=CARTESIAN_POINT('',(-1.1,2.1,9.4));
#76023=CARTESIAN_POINT('Origin',(0.,2.1,9.4));
#76024=CARTESIAN_POINT('',(-1.1,2.1,9.2));
#76025=CARTESIAN_POINT('Origin',(0.,2.1,9.2));
#76026=CARTESIAN_POINT('Origin',(0.,2.1,9.2));
#76027=CARTESIAN_POINT('Origin',(0.,2.1,9.4));
#76028=CARTESIAN_POINT('Origin',(0.,2.1,9.2));
#76029=CARTESIAN_POINT('',(0.9,1.3,9.2));
#76030=CARTESIAN_POINT('Origin',(0.,2.1,9.2));
#76031=CARTESIAN_POINT('',(-0.9,2.9,9.2));
#76032=CARTESIAN_POINT('Origin',(0.9,1.3,6.));
#76033=CARTESIAN_POINT('',(0.9,1.3,6.));
#76034=CARTESIAN_POINT('Origin',(-0.9,2.9,6.));
#76035=CARTESIAN_POINT('',(-0.9,2.9,6.));
#76036=CARTESIAN_POINT('Origin',(0.,2.1,6.));
#76037=CARTESIAN_POINT('',(0.,0.,0.));
#76038=CARTESIAN_POINT('Ctrl Pts',(0.88,2.1,9.525));
#76039=CARTESIAN_POINT('Ctrl Pts',(0.879914606625585,2.17110785049955,9.52865476385635));
#76040=CARTESIAN_POINT('Ctrl Pts',(0.863232117186907,2.3095104036224,9.53591397312323));
#76041=CARTESIAN_POINT('Ctrl Pts',(0.7646146646842,2.57432753790838,9.55048599717583));
#76042=CARTESIAN_POINT('Ctrl Pts',(0.52875066403414,2.8457083400553,9.56867094599734));
#76043=CARTESIAN_POINT('Ctrl Pts',(0.127238756664634,3.00552936974926,9.59051359518968));
#76044=CARTESIAN_POINT('Ctrl Pts',(-0.302716205619033,2.96306288294985,
9.61235380295566));
#76045=CARTESIAN_POINT('Ctrl Pts',(-0.665427657999688,2.72799341501097,
9.63420407641812));
#76046=CARTESIAN_POINT('Ctrl Pts',(-0.879826065415376,2.3524940033895,9.65606121698024));
#76047=CARTESIAN_POINT('Ctrl Pts',(-0.89799221853441,1.92029343459682,9.67792905414005));
#76048=CARTESIAN_POINT('Ctrl Pts',(-0.715657796510551,1.52775201761214,
9.69980826165769));
#76049=CARTESIAN_POINT('Ctrl Pts',(-0.37329244035757,1.26252484692041,9.72170089413125));
#76050=CARTESIAN_POINT('Ctrl Pts',(0.0529042162174613,1.18397194405211,
9.7436083723133));
#76051=CARTESIAN_POINT('Ctrl Pts',(0.467926525737336,1.30987826775351,9.76553239226868));
#76052=CARTESIAN_POINT('Ctrl Pts',(0.77911594458734,1.61250328722602,9.78747453406851));
#76053=CARTESIAN_POINT('Ctrl Pts',(0.916833254715888,2.02450810034898,9.8094364412056));
#76054=CARTESIAN_POINT('Ctrl Pts',(0.84999015619955,2.45432327019144,9.83141968646686));
#76055=CARTESIAN_POINT('Ctrl Pts',(0.593134887517594,2.80556810401153,9.85342584950507));
#76056=CARTESIAN_POINT('Ctrl Pts',(0.159785468035136,3.02235194398505,9.87790429996245));
#76057=CARTESIAN_POINT('Ctrl Pts',(-0.382738476891779,2.97204316801605,
9.90486768286448));
#76058=CARTESIAN_POINT('Ctrl Pts',(-0.827943575417754,2.57464859578558,
9.93433214776037));
#76059=CARTESIAN_POINT('Ctrl Pts',(-0.928540642244484,2.0879125901631,9.95893043030863));
#76060=CARTESIAN_POINT('Ctrl Pts',(-0.82506221727755,1.71823863855703,9.97863755083128));
#76061=CARTESIAN_POINT('Ctrl Pts',(-0.665238898770628,1.47861418311032,
9.99343255715118));
#76062=CARTESIAN_POINT('Ctrl Pts',(-0.438025190317537,1.3012081221325,10.0082426633322));
#76063=CARTESIAN_POINT('Ctrl Pts',(-0.0759140953759721,1.16989403941721,
10.0280101634631));
#76064=CARTESIAN_POINT('Ctrl Pts',(0.353590617267489,1.22647296601624,10.0494595111079));
#76065=CARTESIAN_POINT('Ctrl Pts',(0.71282299611785,1.50640456177768,10.0726022736917));
#76066=CARTESIAN_POINT('Ctrl Pts',(0.895311256816217,1.85157831854142,10.0924697020734));
#76067=CARTESIAN_POINT('Ctrl Pts',(0.917661293713379,2.20976194577009,10.1107106042816));
#76068=CARTESIAN_POINT('Ctrl Pts',(0.819212469046223,2.51761130734418,10.127317066638));
#76069=CARTESIAN_POINT('Ctrl Pts',(0.591924394917487,2.83289082559773,10.1472698428113));
#76070=CARTESIAN_POINT('Ctrl Pts',(0.141288805504938,3.06103897732418,10.172258699084));
#76071=CARTESIAN_POINT('Ctrl Pts',(-0.458527011040082,2.95925151709148,
10.2023249565719));
#76072=CARTESIAN_POINT('Ctrl Pts',(-0.88162766536303,2.52027411449529,10.2324736532743));
#76073=CARTESIAN_POINT('Ctrl Pts',(-0.961653185964405,1.91393657438503,
10.2627077273853));
#76074=CARTESIAN_POINT('Ctrl Pts',(-0.665231767857691,1.37715957803001,
10.2930297792945));
#76075=CARTESIAN_POINT('Ctrl Pts',(-0.105988685338195,1.12026073865136,
10.3234425669733));
#76076=CARTESIAN_POINT('Ctrl Pts',(0.430538820721984,1.23255710504194,10.3505590141325));
#76077=CARTESIAN_POINT('Ctrl Pts',(0.777157271318668,1.54704609431923,10.3743479205533));
#76078=CARTESIAN_POINT('Ctrl Pts',(0.937973646848606,1.91510656924282,10.3947816504623));
#76079=CARTESIAN_POINT('Ctrl Pts',(0.932931736507626,2.31778957988939,10.4152592321293));
#76080=CARTESIAN_POINT('Ctrl Pts',(0.762578582228501,2.68366310973811,10.4357813746755));
#76081=CARTESIAN_POINT('Ctrl Pts',(0.455963235969408,2.94715653506223,10.4563486739678));
#76082=CARTESIAN_POINT('Ctrl Pts',(0.00240142086611935,3.08166579400621,
10.480397254692));
#76083=CARTESIAN_POINT('Ctrl Pts',(-0.538455390507358,2.94820992747045,
10.5079586157699));
#76084=CARTESIAN_POINT('Ctrl Pts',(-0.940666416691817,2.46401744657124,
10.5390713811047));
#76085=CARTESIAN_POINT('Ctrl Pts',(-0.976029443563649,1.83335883304997,
10.5702921359498));
#76086=CARTESIAN_POINT('Ctrl Pts',(-0.629306856593687,1.30317046301086,
10.6016225477596));
#76087=CARTESIAN_POINT('Ctrl Pts',(-0.0328763589810331,1.08144514613719,
10.6330641573791));
#76088=CARTESIAN_POINT('Ctrl Pts',(0.511901871764286,1.23876013099839,10.6611123163153));
#76089=CARTESIAN_POINT('Ctrl Pts',(0.845208777494887,1.59002857501027,10.6857282761483));
#76090=CARTESIAN_POINT('Ctrl Pts',(0.959937391714928,1.91692164410815,10.7033535735637));
#76091=CARTESIAN_POINT('Ctrl Pts',(0.964709509971458,2.19002072343591,10.7174794574177));
#76092=CARTESIAN_POINT('Ctrl Pts',(0.903969607200192,2.50338072207659,10.7339796596208));
#76093=CARTESIAN_POINT('Ctrl Pts',(0.708976511873778,2.79903473649909,10.7516978643424));
#76094=CARTESIAN_POINT('Ctrl Pts',(0.359111666410103,3.02058677865832,10.7730116718645));
#76095=CARTESIAN_POINT('Ctrl Pts',(-0.0055195068732309,3.09939687665217,
10.7919958841582));
#76096=CARTESIAN_POINT('Ctrl Pts',(-0.417331250225881,3.01093271757532,
10.8134054790171));
#76097=CARTESIAN_POINT('Ctrl Pts',(-0.756608961158023,2.76032613000462,
10.8348676292604));
#76098=CARTESIAN_POINT('Ctrl Pts',(-0.998865593098056,2.33000290793379,
10.8599683150449));
#76099=CARTESIAN_POINT('Ctrl Pts',(-0.988791187924089,1.74845036869023,
10.8887429491342));
#76100=CARTESIAN_POINT('Ctrl Pts',(-0.588714669350558,1.22669384301482,
10.9212338011637));
#76101=CARTESIAN_POINT('Ctrl Pts',(0.044909234496707,1.04388405761621,10.9538443040117));
#76102=CARTESIAN_POINT('Ctrl Pts',(0.665762350574508,1.27382859359802,10.9865746011287));
#76103=CARTESIAN_POINT('Ctrl Pts',(1.02994927065475,1.82963242200099,11.0194247010519));
#76104=CARTESIAN_POINT('Ctrl Pts',(0.99292771913683,2.49532007970257,11.0523944801788));
#76105=CARTESIAN_POINT('Ctrl Pts',(0.566047404042377,3.01118540039736,11.0854836852924));
#76106=CARTESIAN_POINT('Ctrl Pts',(-0.0131656805453273,3.1545072720966,
11.1150021335127));
#76107=CARTESIAN_POINT('Ctrl Pts',(-0.501834747536299,3.00971245930524,
11.1409075995603));
#76108=CARTESIAN_POINT('Ctrl Pts',(-0.833654637909307,2.72466132918788,
11.1631647757637));
#76109=CARTESIAN_POINT('Ctrl Pts',(-1.01904932840502,2.32688792491809,11.1854742337572));
#76110=CARTESIAN_POINT('Ctrl Pts',(-1.0247320303861,1.8873087550975,11.2078357472338));
#76111=CARTESIAN_POINT('Ctrl Pts',(-0.848433071641297,1.48323440703255,
11.2302490424206));
#76112=CARTESIAN_POINT('Ctrl Pts',(-0.5209916303453,1.18686010809674,11.2527138516101));
#76113=CARTESIAN_POINT('Ctrl Pts',(-0.0994474829318688,1.05086828612434,
11.2752298585268));
#76114=CARTESIAN_POINT('Ctrl Pts',(0.341286571712092,1.10081439784123,11.297796723956));
#76115=CARTESIAN_POINT('Ctrl Pts',(0.787934060544661,1.36522529701193,11.3241836591263));
#76116=CARTESIAN_POINT('Ctrl Pts',(1.08440822726537,1.89981767692546,11.3544236935599));
#76117=CARTESIAN_POINT('Ctrl Pts',(0.99437189083192,2.58466520846377,11.3885550724356));
#76118=CARTESIAN_POINT('Ctrl Pts',(0.51422832678732,3.08343949927552,11.4227963300144));
#76119=CARTESIAN_POINT('Ctrl Pts',(-0.170956362315584,3.20042729316684,
11.4571457685877));
#76120=CARTESIAN_POINT('Ctrl Pts',(-0.792809143568463,2.88603885152724,
11.49160167588));
#76121=CARTESIAN_POINT('Ctrl Pts',(-1.10815562220614,2.26212033857722,11.5261621918766));
#76122=CARTESIAN_POINT('Ctrl Pts',(-0.990980784814367,1.57098681332194,
11.5608252913622));
#76123=CARTESIAN_POINT('Ctrl Pts',(-0.484736723033935,1.08260154598769,
11.5955889188738));
#76124=CARTESIAN_POINT('Ctrl Pts',(0.214307763377102,0.991032096532327,
11.6304507824074));
#76125=CARTESIAN_POINT('Ctrl Pts',(0.833298379906107,1.33271197734595,11.6654086518246));
#76126=CARTESIAN_POINT('Ctrl Pts',(1.12908711130714,1.97705558535849,11.7004600148669));
#76127=CARTESIAN_POINT('Ctrl Pts',(0.984170425255086,2.67277304384029,11.7356024461146));
#76128=CARTESIAN_POINT('Ctrl Pts',(0.452808643636702,3.14802102155422,11.7708333087139));
#76129=CARTESIAN_POINT('Ctrl Pts',(-0.198836507924274,3.20872213800758,
11.8032068201948));
#76130=CARTESIAN_POINT('Ctrl Pts',(-0.720833985617695,2.9475724124579,11.8326976979388));
#76131=CARTESIAN_POINT('Ctrl Pts',(-1.03122512713103,2.52323917223077,11.8592848682016));
#76132=CARTESIAN_POINT('Ctrl Pts',(-1.11221371795246,2.00254397936835,11.8859162010712));
#76133=CARTESIAN_POINT('Ctrl Pts',(-0.944978677865563,1.50212478400673,
11.9125904181942));
#76134=CARTESIAN_POINT('Ctrl Pts',(-0.566096651435205,1.13364169683645,
11.9393062323883));
#76135=CARTESIAN_POINT('Ctrl Pts',(-0.0596069971212731,0.97996909355213,
11.966062281935));
#76136=CARTESIAN_POINT('Ctrl Pts',(0.461675051948685,1.07603593590851,11.9928572469173));
#76137=CARTESIAN_POINT('Ctrl Pts',(0.88129231323125,1.40110770643291,12.0196896905075));
#76138=CARTESIAN_POINT('Ctrl Pts',(1.10519737818586,1.88315811002375,12.0465583931276));
#76139=CARTESIAN_POINT('Ctrl Pts',(1.08283365883886,2.41488670097258,12.0734615789711));
#76140=CARTESIAN_POINT('Ctrl Pts',(0.818591168747924,2.87760074176854,12.100398642491));
#76141=CARTESIAN_POINT('Ctrl Pts',(0.370893737846914,3.16774776724325,12.1273662612715));
#76142=CARTESIAN_POINT('Ctrl Pts',(-0.160578831483255,3.22009488317826,
12.154367120808));
#76143=CARTESIAN_POINT('Ctrl Pts',(-0.657438304412148,3.02243699025829,
12.181390412703));
#76144=CARTESIAN_POINT('Ctrl Pts',(-0.949764066307816,2.68573447988004,
12.2039450357004));
#76145=CARTESIAN_POINT('Ctrl Pts',(-1.07182425162092,2.35796849387404,12.2219800536891));
#76146=CARTESIAN_POINT('Ctrl Pts',(-1.09256785760649,2.18550272007321,12.2310256553714));
#76147=CARTESIAN_POINT('Ctrl Pts',(-1.09265261173395,2.09796323888708,12.2355247810852));
#76148=CARTESIAN_POINT('Ctrl Pts',(0.88,2.1,9.55791192303761));
#76149=CARTESIAN_POINT('Ctrl Pts',(0.879783916285541,2.17106190544998,9.56156549634868));
#76150=CARTESIAN_POINT('Ctrl Pts',(0.862819487639945,2.30936028696044,9.56882270408062));
#76151=CARTESIAN_POINT('Ctrl Pts',(0.763769645522231,2.57374536624056,9.58338184659129));
#76152=CARTESIAN_POINT('Ctrl Pts',(0.527681439909107,2.84421258618503,9.60154403506069));
#76153=CARTESIAN_POINT('Ctrl Pts',(0.126836189332554,3.00282054305338,9.6233360843192));
#76154=CARTESIAN_POINT('Ctrl Pts',(-0.301578089003487,2.9596327314869,9.64510671305593));
#76155=CARTESIAN_POINT('Ctrl Pts',(-0.662248104445556,2.72485823025643,
9.66686668449843));
#76156=CARTESIAN_POINT('Ctrl Pts',(-0.87477101414986,2.35090800902427,9.68861370251383));
#76157=CARTESIAN_POINT('Ctrl Pts',(-0.891962086690084,1.92134378925048,
9.71035132236448));
#76158=CARTESIAN_POINT('Ctrl Pts',(-0.71013501547485,1.53195117584763,9.73208047576603));
#76159=CARTESIAN_POINT('Ctrl Pts',(-0.369972269812193,1.2695301574022,9.75380324748816));
#76160=CARTESIAN_POINT('Ctrl Pts',(0.0525992830413849,1.19253118829567,
9.77552119527361));
#76161=CARTESIAN_POINT('Ctrl Pts',(0.463319878103491,1.31804354326137,9.79723612745198));
#76162=CARTESIAN_POINT('Ctrl Pts',(0.770594784068131,1.61807714145974,9.81894973497212));
#76163=CARTESIAN_POINT('Ctrl Pts',(0.90590391628519,2.02562383372829,9.84066384510364));
#76164=CARTESIAN_POINT('Ctrl Pts',(0.839026217634196,2.44999742219886,9.86238006152402));
#76165=CARTESIAN_POINT('Ctrl Pts',(0.584857943541199,2.79609540610752,9.88410036302005));
#76166=CARTESIAN_POINT('Ctrl Pts',(0.15715540696274,3.00896823215133,9.90823975031835));
#76167=CARTESIAN_POINT('Ctrl Pts',(-0.377152993385563,2.95829410746318,
9.93480658955309));
#76168=CARTESIAN_POINT('Ctrl Pts',(-0.814397042063615,2.56634291336892,
9.96380668194593));
#76169=CARTESIAN_POINT('Ctrl Pts',(-0.912281798203633,2.08773618372905,
9.9879885560003));
#76170=CARTESIAN_POINT('Ctrl Pts',(-0.80994027967792,1.72488593264374,10.007344749781));
#76171=CARTESIAN_POINT('Ctrl Pts',(-0.652597501593231,1.48997710639104,
10.0218694825692));
#76172=CARTESIAN_POINT('Ctrl Pts',(-0.429334265664847,1.31636286686092,
10.036401726932));
#76173=CARTESIAN_POINT('Ctrl Pts',(-0.0739971908554309,1.18829325899891,
10.0557871102574));
#76174=CARTESIAN_POINT('Ctrl Pts',(0.346806406792938,1.24460770613069,10.0768146985648));
#76175=CARTESIAN_POINT('Ctrl Pts',(0.697974642411667,1.51937892964619,10.0994750183564));
#76176=CARTESIAN_POINT('Ctrl Pts',(0.87586983164938,1.85746669220029,10.1189161511382));
#76177=CARTESIAN_POINT('Ctrl Pts',(0.897034042189538,2.20777551093713,10.1367564439922));
#76178=CARTESIAN_POINT('Ctrl Pts',(0.800234096584245,2.5084630157536,10.152988370211));
#76179=CARTESIAN_POINT('Ctrl Pts',(0.577596139139017,2.81603174879275,10.1724819296167));
#76180=CARTESIAN_POINT('Ctrl Pts',(0.137179583427464,3.03788753933788,10.1968844302235));
#76181=CARTESIAN_POINT('Ctrl Pts',(-0.447719726782846,2.93741039885078,
10.2262174469579));
#76182=CARTESIAN_POINT('Ctrl Pts',(-0.8592452583341,2.50872159304617,10.2556077729931));
#76183=CARTESIAN_POINT('Ctrl Pts',(-0.935997001543472,1.91804036079765,
10.2850576889373));
#76184=CARTESIAN_POINT('Ctrl Pts',(-0.646471737706749,1.3962267816677,10.3145716941238));
#76185=CARTESIAN_POINT('Ctrl Pts',(-0.102097088466362,1.14747264463815,
10.3441525825305));
#76186=CARTESIAN_POINT('Ctrl Pts',(0.419131076191686,1.25764685588435,10.3705107921544));
#76187=CARTESIAN_POINT('Ctrl Pts',(0.755233370608568,1.56377441619041,10.3936200727939));
#76188=CARTESIAN_POINT('Ctrl Pts',(0.910698712173214,1.92145284521483,10.4134626290806));
#76189=CARTESIAN_POINT('Ctrl Pts',(0.905060795811563,2.3122898350333,10.433339759045));
#76190=CARTESIAN_POINT('Ctrl Pts',(0.739099621706325,2.66695860331452,10.453252117855));
#76191=CARTESIAN_POINT('Ctrl Pts',(0.441230372512847,2.92195825542685,10.4732014482075));
#76192=CARTESIAN_POINT('Ctrl Pts',(0.00121674788033055,3.05154102121814,
10.4965196435521));
#76193=CARTESIAN_POINT('Ctrl Pts',(-0.522748489859997,2.92119140764988,
10.5232357617401));
#76194=CARTESIAN_POINT('Ctrl Pts',(-0.911497386825926,2.45137002542038,
10.5533776932785));
#76195=CARTESIAN_POINT('Ctrl Pts',(-0.944589337394057,1.84057261493696,
10.5836150456035));
#76196=CARTESIAN_POINT('Ctrl Pts',(-0.607970601887274,1.32795366098775,
10.6139463426483));
#76197=CARTESIAN_POINT('Ctrl Pts',(-0.0303722616549957,1.11446027835103,
10.6443758271437));
#76198=CARTESIAN_POINT('Ctrl Pts',(0.496414421501777,1.26764280902697,10.6715139458982));
#76199=CARTESIAN_POINT('Ctrl Pts',(0.818195108939898,1.60801290269984,10.6953251867043));
#76200=CARTESIAN_POINT('Ctrl Pts',(0.928577482097722,1.92437513921087,10.7123719721017));
#76201=CARTESIAN_POINT('Ctrl Pts',(0.932712814366555,2.18849028957719,10.7260329283826));
#76202=CARTESIAN_POINT('Ctrl Pts',(0.873425627776733,2.49140923636693,10.7419890654634));
#76203=CARTESIAN_POINT('Ctrl Pts',(0.684360362767623,2.77694456454821,10.7591217708996));
#76204=CARTESIAN_POINT('Ctrl Pts',(0.345706151983871,2.99053966910833,10.779728973541));
#76205=CARTESIAN_POINT('Ctrl Pts',(-0.00695621592430146,3.06609903601776,
10.7980830429247));
#76206=CARTESIAN_POINT('Ctrl Pts',(-0.404919858613662,2.97985927827303,
10.8187806195429));
#76207=CARTESIAN_POINT('Ctrl Pts',(-0.732470914203224,2.73700800230651,
10.8395282778942));
#76208=CARTESIAN_POINT('Ctrl Pts',(-0.965916457583696,2.32059708248666,
10.8637928468312));
#76209=CARTESIAN_POINT('Ctrl Pts',(-0.955180521436829,1.75843199962428,
10.8916085044493));
#76210=CARTESIAN_POINT('Ctrl Pts',(-0.567524852982291,1.25471553979666,
10.9230176634458));
#76211=CARTESIAN_POINT('Ctrl Pts',(0.0453742137555828,1.07904710642372,
10.9545445596419));
#76212=CARTESIAN_POINT('Ctrl Pts',(0.645298788561736,1.30242661576631,10.9861905897209));
#76213=CARTESIAN_POINT('Ctrl Pts',(0.996561212876046,1.84052731934913,11.0179569335076));
#76214=CARTESIAN_POINT('Ctrl Pts',(0.95965217440279,2.48434133424897,11.0498444512395));
#76215=CARTESIAN_POINT('Ctrl Pts',(0.545822723695986,2.98271084435086,11.081854458347));
#76216=CARTESIAN_POINT('Ctrl Pts',(-0.014904284913205,3.12045730942825,
11.1104164211207));
#76217=CARTESIAN_POINT('Ctrl Pts',(-0.487661806414971,2.97950014590718,
11.1354897161336));
#76218=CARTESIAN_POINT('Ctrl Pts',(-0.808440019610243,2.70298642271134,
11.157036944517));
#76219=CARTESIAN_POINT('Ctrl Pts',(-0.987310850925297,2.31750955387077,
11.1786378910855));
#76220=CARTESIAN_POINT('Ctrl Pts',(-0.992098225376437,1.89173243381715,
11.2002962144121));
#76221=CARTESIAN_POINT('Ctrl Pts',(-0.82064376921839,1.5005573687953,11.2220077836223));
#76222=CARTESIAN_POINT('Ctrl Pts',(-0.502851712636325,1.21388588160114,
11.2437762289073));
#76223=CARTESIAN_POINT('Ctrl Pts',(-0.0940215246938652,1.08275155627072,
11.2655990874032));
#76224=CARTESIAN_POINT('Ctrl Pts',(0.333245621813066,1.13189689359355,11.2874794932251));
#76225=CARTESIAN_POINT('Ctrl Pts',(0.766035799756981,1.38907373699405,11.3130716739573));
#76226=CARTESIAN_POINT('Ctrl Pts',(1.05285688105598,1.90823270195865,11.3424078568475));
#76227=CARTESIAN_POINT('Ctrl Pts',(0.964393978317041,2.57292853569788,11.375537780296));
#76228=CARTESIAN_POINT('Ctrl Pts',(0.497259385622897,3.05663886627931,11.408792079458));
#76229=CARTESIAN_POINT('Ctrl Pts',(-0.168799592857434,3.16928654041918,
11.4421680598492));
#76230=CARTESIAN_POINT('Ctrl Pts',(-0.773028708878503,2.86260976094568,
11.4756720319812));
#76231=CARTESIAN_POINT('Ctrl Pts',(-1.07892178246083,2.25506720291879,11.5092937866771));
#76232=CARTESIAN_POINT('Ctrl Pts',(-0.963794044402426,1.58234479055142,
11.5430382284851));
#76233=CARTESIAN_POINT('Ctrl Pts',(-0.469862016813641,1.10729279591243,
11.5768999608508));
#76234=CARTESIAN_POINT('Ctrl Pts',(0.211814495863296,1.019066613562,11.610886222149));
#76235=CARTESIAN_POINT('Ctrl Pts',(0.815201055217733,1.35332341694216,11.6449854463145));
#76236=CARTESIAN_POINT('Ctrl Pts',(1.10303660712102,1.98284539338398,11.6792011961435));
#76237=CARTESIAN_POINT('Ctrl Pts',(0.960427736142072,2.66238095948827,11.7135308697322));
#76238=CARTESIAN_POINT('Ctrl Pts',(0.440172394309644,3.12630195146006,11.7479736075752));
#76239=CARTESIAN_POINT('Ctrl Pts',(-0.197583641464606,3.18475546487694,
11.7796461293911));
#76240=CARTESIAN_POINT('Ctrl Pts',(-0.708367033845548,2.92823812698208,
11.8085215502503));
#76241=CARTESIAN_POINT('Ctrl Pts',(-1.01186730074176,2.51199019692748,11.8345688321747));
#76242=CARTESIAN_POINT('Ctrl Pts',(-1.0904966249175,2.00135053161119,11.8606756249931));
#76243=CARTESIAN_POINT('Ctrl Pts',(-0.925680523765739,1.51065297779157,
11.8868406034525));
#76244=CARTESIAN_POINT('Ctrl Pts',(-0.553184670058425,1.14947860398362,
11.9130629946836));
#76245=CARTESIAN_POINT('Ctrl Pts',(-0.055415031446615,0.999273750331867,
11.9393416867785));
#76246=CARTESIAN_POINT('Ctrl Pts',(0.456850692462456,1.09447748037705,11.965675683592));
#76247=CARTESIAN_POINT('Ctrl Pts',(0.869118461065415,1.41484540483791,11.9920638498054));
#76248=CARTESIAN_POINT('Ctrl Pts',(1.08879853435095,1.88964775701972,12.0185051663876));
#76249=CARTESIAN_POINT('Ctrl Pts',(1.06599737677219,2.41333580572711,12.0449982756185));
#76250=CARTESIAN_POINT('Ctrl Pts',(0.804891629262968,2.86900603669412,12.0715424339268));
#76251=CARTESIAN_POINT('Ctrl Pts',(0.362923366288464,3.15451545410712,12.0981353818834));
#76252=CARTESIAN_POINT('Ctrl Pts',(-0.161668688010658,3.20541279760317,
12.1247781162622));
#76253=CARTESIAN_POINT('Ctrl Pts',(-0.652085894169137,3.00945265230991,
12.1514642275061));
#76254=CARTESIAN_POINT('Ctrl Pts',(-0.940446471327969,2.67628514499842,
12.1737473845505));
#76255=CARTESIAN_POINT('Ctrl Pts',(-1.06066013461824,2.35191836336405,12.1915846173031));
#76256=CARTESIAN_POINT('Ctrl Pts',(-1.08088861775694,2.18131633339423,12.2005290550795));
#76257=CARTESIAN_POINT('Ctrl Pts',(-1.08084165385376,2.0946891367405,12.2049801218611));
#76258=CARTESIAN_POINT('Ctrl Pts',(0.91153047167304,2.1,9.62353994288304));
#76259=CARTESIAN_POINT('Ctrl Pts',(0.91105364478002,2.17348405122035,9.62732031744799));
#76260=CARTESIAN_POINT('Ctrl Pts',(0.892967745079117,2.31673902258848,9.63483964861492));
#76261=CARTESIAN_POINT('Ctrl Pts',(0.789521176264839,2.58987098214541,9.64989741724387));
#76262=CARTESIAN_POINT('Ctrl Pts',(0.544564452912013,2.86843394076872,9.668658841039));
#76263=CARTESIAN_POINT('Ctrl Pts',(0.130536318539686,3.03042695712525,9.69112807964226));
#76264=CARTESIAN_POINT('Ctrl Pts',(-0.310330783421158,2.98427236214618,
9.71353513800462));
#76265=CARTESIAN_POINT('Ctrl Pts',(-0.680015491769051,2.74157537674839,
9.73588959548194));
#76266=CARTESIAN_POINT('Ctrl Pts',(-0.896499318571394,2.357167057499,9.75818908021112));
#76267=CARTESIAN_POINT('Ctrl Pts',(-0.912376566341135,1.91732632552379,
9.78043662951247));
#76268=CARTESIAN_POINT('Ctrl Pts',(-0.725024155965477,1.52017204573209,
9.80263291027502));
#76269=CARTESIAN_POINT('Ctrl Pts',(-0.377066297404346,1.25391115517105,
9.82477967943719));
#76270=CARTESIAN_POINT('Ctrl Pts',(0.0533471125557414,1.17723280759371,
9.84687824938293));
#76271=CARTESIAN_POINT('Ctrl Pts',(0.470060182466133,1.30637765174259,9.86893017531943));
#76272=CARTESIAN_POINT('Ctrl Pts',(0.78036781679815,1.61178376947083,9.89093697531718));
#76273=CARTESIAN_POINT('Ctrl Pts',(0.915629767908127,2.02466884923936,9.91290023450542));
#76274=CARTESIAN_POINT('Ctrl Pts',(0.846390455638519,2.45290065637925,9.93482156821705));
#76275=CARTESIAN_POINT('Ctrl Pts',(0.58887797324273,2.80063439575845,9.95670251565969));
#76276=CARTESIAN_POINT('Ctrl Pts',(0.157895298284613,3.01298640312374,9.98097182074651));
#76277=CARTESIAN_POINT('Ctrl Pts',(-0.377917255020538,2.95989571059473,
10.0076141443979));
#76278=CARTESIAN_POINT('Ctrl Pts',(-0.813700360743258,2.56591121504782,
10.0366162055263));
#76279=CARTESIAN_POINT('Ctrl Pts',(-0.90933677990633,2.08797029208528,10.0607376094115));
#76280=CARTESIAN_POINT('Ctrl Pts',(-0.806016864557925,1.72706447977729,
10.0800087547882));
#76281=CARTESIAN_POINT('Ctrl Pts',(-0.648638252475412,1.49408849163869,
10.0944489361237));
#76282=CARTESIAN_POINT('Ctrl Pts',(-0.426263420033854,1.32255523282061,
10.1088766557053));
#76283=CARTESIAN_POINT('Ctrl Pts',(-0.073366716764664,1.19694055764828,
10.1280985439345));
#76284=CARTESIAN_POINT('Ctrl Pts',(0.342755481993835,1.25443301936784,10.1488935550027));
#76285=CARTESIAN_POINT('Ctrl Pts',(0.688405486121672,1.52715182432036,10.1712661011271));
#76286=CARTESIAN_POINT('Ctrl Pts',(0.862394009352625,1.86110195503896,10.1904256185386));
#76287=CARTESIAN_POINT('Ctrl Pts',(0.881814193602376,2.20582919186377,10.2079731409895));
#76288=CARTESIAN_POINT('Ctrl Pts',(0.785548217129111,2.5008254907576,10.2239156985126));
#76289=CARTESIAN_POINT('Ctrl Pts',(0.56591941828687,2.80169942910186,10.2430370586467));
#76290=CARTESIAN_POINT('Ctrl Pts',(0.133807769973548,3.01703821882315,10.2669184653035));
#76291=CARTESIAN_POINT('Ctrl Pts',(-0.436917678576326,2.91645318725037,
10.2955546153329));
#76292=CARTESIAN_POINT('Ctrl Pts',(-0.835922416842069,2.4971875235335,10.3241712524374));
#76293=CARTESIAN_POINT('Ctrl Pts',(-0.908007865198345,1.92302512682405,
10.3527740090878));
#76294=CARTESIAN_POINT('Ctrl Pts',(-0.625265349485015,1.41856922050494,
10.3813664070234));
#76295=CARTESIAN_POINT('Ctrl Pts',(-0.0980075253033923,1.18038116079578,
10.4099539128241));
#76296=CARTESIAN_POINT('Ctrl Pts',(0.404142738693815,1.28877534199984,10.4353631479262));
#76297=CARTESIAN_POINT('Ctrl Pts',(0.726402174614211,1.58472143067419,10.4576006853765));
#76298=CARTESIAN_POINT('Ctrl Pts',(0.874385876809216,1.92902833247871,10.4766638408478));
#76299=CARTESIAN_POINT('Ctrl Pts',(0.867435595716759,2.30398797603964,10.4957315864257));
#76300=CARTESIAN_POINT('Ctrl Pts',(0.707054269343606,2.64311684354316,10.5148056321417));
#76301=CARTESIAN_POINT('Ctrl Pts',(0.421116724846305,2.8858766210418,10.5338865299558));
#76302=CARTESIAN_POINT('Ctrl Pts',(0.000306317622067648,3.00793566462754,
10.5561570667423));
#76303=CARTESIAN_POINT('Ctrl Pts',(-0.498728080378487,2.88150683444137,
10.581622031038));
#76304=CARTESIAN_POINT('Ctrl Pts',(-0.866739074640701,2.43287565356016,
10.6103008121439));
#76305=CARTESIAN_POINT('Ctrl Pts',(-0.89567648973,1.85273981720578,10.6390059526166));
#76306=CARTESIAN_POINT('Ctrl Pts',(-0.57458622137938,1.36824600602171,10.6677477437704));
#76307=CARTESIAN_POINT('Ctrl Pts',(-0.0273166520720773,1.16859943191723,
10.6965289270857));
#76308=CARTESIAN_POINT('Ctrl Pts',(0.469506483946871,1.31533648442313,10.7221489581215));
#76309=CARTESIAN_POINT('Ctrl Pts',(0.771641137123773,1.63753656926365,10.7446015563863));
#76310=CARTESIAN_POINT('Ctrl Pts',(0.874414726399044,1.93595303744339,10.7606572590965));
#76311=CARTESIAN_POINT('Ctrl Pts',(0.877323346348476,2.18455153451786,10.7735139397468));
#76312=CARTESIAN_POINT('Ctrl Pts',(0.820424570946683,2.46929223171017,10.7885230217106));
#76313=CARTESIAN_POINT('Ctrl Pts',(0.64164599771704,2.73689268744519,10.8046210998245));
#76314=CARTESIAN_POINT('Ctrl Pts',(0.322885446846539,2.93618132347737,10.8239692642255));
#76315=CARTESIAN_POINT('Ctrl Pts',(-0.00823321698495057,3.00572801835655,
10.8411845128887));
#76316=CARTESIAN_POINT('Ctrl Pts',(-0.380918433916755,2.92340325825145,
10.8605837425962));
#76317=CARTESIAN_POINT('Ctrl Pts',(-0.686732400828136,2.69475762437649,
10.8800100296679));
#76318=CARTESIAN_POINT('Ctrl Pts',(-0.903601656768487,2.30426172271222,
10.9027121258681));
#76319=CARTESIAN_POINT('Ctrl Pts',(-0.891411633732064,1.77884460545719,
10.9287080284181));
#76320=CARTESIAN_POINT('Ctrl Pts',(-0.527555828750873,1.31001811981728,
10.958031197091));
#76321=CARTESIAN_POINT('Ctrl Pts',(0.0447580861818993,1.14848673179254,
10.9874336854073));
#76322=CARTESIAN_POINT('Ctrl Pts',(0.602941681277028,1.35888446381741,11.0169200010601));
#76323=CARTESIAN_POINT('Ctrl Pts',(0.927970988373135,1.86117278345443,11.0464932429883));
#76324=CARTESIAN_POINT('Ctrl Pts',(0.891255966367144,2.45997746423432,11.0761567696705));
#76325=CARTESIAN_POINT('Ctrl Pts',(0.504702358672154,2.92177668715295,11.105914324334));
#76326=CARTESIAN_POINT('Ctrl Pts',(-0.0167793435795264,3.04771529211323,
11.1324507777199));
#76327=CARTESIAN_POINT('Ctrl Pts',(-0.455338690749746,2.91511037606382,
11.1557367370154));
#76328=CARTESIAN_POINT('Ctrl Pts',(-0.752183284487268,2.65723389205797,
11.1757423237457));
#76329=CARTESIAN_POINT('Ctrl Pts',(-0.916841848233799,2.29878925378214,
11.1957925332484));
#76330=CARTESIAN_POINT('Ctrl Pts',(-0.919776969791426,1.90364303364972,
11.2158918338139));
#76331=CARTESIAN_POINT('Ctrl Pts',(-0.759308358911334,1.54129526233824,
11.2360370757184));
#76332=CARTESIAN_POINT('Ctrl Pts',(-0.463475971789943,1.27646148633192,
11.2562322548172));
#76333=CARTESIAN_POINT('Ctrl Pts',(-0.0837713729081205,1.15625183292691,
11.2764761143988));
#76334=CARTESIAN_POINT('Ctrl Pts',(0.312377222380745,1.20332878815849,11.2967717707931));
#76335=CARTESIAN_POINT('Ctrl Pts',(0.712912934890082,1.4433776123106,11.3205098526284));
#76336=CARTESIAN_POINT('Ctrl Pts',(0.977159827924982,1.92592825997509,11.3477225173613));
#76337=CARTESIAN_POINT('Ctrl Pts',(0.892810604480596,2.54223408268594,11.3784572591806));
#76338=CARTESIAN_POINT('Ctrl Pts',(0.457739726643327,2.98944426773445,11.4093130261963));
#76339=CARTESIAN_POINT('Ctrl Pts',(-0.160800171609709,3.09173229952906,
11.4402913214941));
#76340=CARTESIAN_POINT('Ctrl Pts',(-0.720733679185758,2.80499075517892,
11.4713968913498));
#76341=CARTESIAN_POINT('Ctrl Pts',(-1.00281663250133,2.23968124921094,11.5026276832156));
#76342=CARTESIAN_POINT('Ctrl Pts',(-0.89360612273627,1.61492108193344,11.5339875295911));
#76343=CARTESIAN_POINT('Ctrl Pts',(-0.432776176189375,1.17483510359387,
11.5654765787301));
#76344=CARTESIAN_POINT('Ctrl Pts',(0.201746101425125,1.09496619635988,11.5970988524765));
#76345=CARTESIAN_POINT('Ctrl Pts',(0.762475338330419,1.4081509930752,11.6288524812263));
#76346=CARTESIAN_POINT('Ctrl Pts',(1.028668635657,1.9956937457661,11.6607399754007));
#76347=CARTESIAN_POINT('Ctrl Pts',(0.893491389235042,2.62901163607681,11.6927620183401));
#76348=CARTESIAN_POINT('Ctrl Pts',(0.406345553247394,3.06044896638264,11.7249195550277));
#76349=CARTESIAN_POINT('Ctrl Pts',(-0.189814472656564,3.11306137855792,
11.7545217329727));
#76350=CARTESIAN_POINT('Ctrl Pts',(-0.666752905623271,2.87149615924449,
11.7815329051351));
#76351=CARTESIAN_POINT('Ctrl Pts',(-0.949541402730192,2.48086457287139,
11.8059197450728));
#76352=CARTESIAN_POINT('Ctrl Pts',(-1.021591881002,2.00217060603226,11.8303836532157));
#76353=CARTESIAN_POINT('Ctrl Pts',(-0.865475264992205,1.5425140203653,11.8549246178449));
#76354=CARTESIAN_POINT('Ctrl Pts',(-0.514682296535199,1.20465835352623,
11.8795426851172));
#76355=CARTESIAN_POINT('Ctrl Pts',(-0.0465088282181845,1.06508734362675,
11.9042378039794));
#76356=CARTESIAN_POINT('Ctrl Pts',(0.434999468617669,1.15623157178554,11.9290098923686));
#76357=CARTESIAN_POINT('Ctrl Pts',(0.822155795806256,1.45914698732355,11.953858817131));
#76358=CARTESIAN_POINT('Ctrl Pts',(1.02773081257076,1.90734105827644,11.9787843903828));
#76359=CARTESIAN_POINT('Ctrl Pts',(1.00458945105254,2.40139718661437,12.0037864018186));
#76360=CARTESIAN_POINT('Ctrl Pts',(0.756530865593507,2.83103044687003,12.0288645331178));
#76361=CARTESIAN_POINT('Ctrl Pts',(0.337665092123472,3.0996729282449,12.054018544057));
#76362=CARTESIAN_POINT('Ctrl Pts',(-0.159203321446335,3.14628016851133,
12.0792478546339));
#76363=CARTESIAN_POINT('Ctrl Pts',(-0.623545249266301,2.95897818066081,
12.1045524799382));
#76364=CARTESIAN_POINT('Ctrl Pts',(-0.896243240370551,2.64197021732172,
12.1257012707751));
#76365=CARTESIAN_POINT('Ctrl Pts',(-1.0094947193235,2.33329207765941,12.142657782671));
#76366=CARTESIAN_POINT('Ctrl Pts',(-1.02817517058789,2.17121348557861,12.1511526949405));
#76367=CARTESIAN_POINT('Ctrl Pts',(-1.0278656018829,2.08874423191622,12.1553877468729));
#76368=CARTESIAN_POINT('Ctrl Pts',(1.01797127075135,2.1,9.6476237796153));
#76369=CARTESIAN_POINT('Ctrl Pts',(1.01739759936018,2.18170177247089,9.6518273032171));
#76370=CARTESIAN_POINT('Ctrl Pts',(0.997075497366153,2.34197250729824,9.66024085688616));
#76371=CARTESIAN_POINT('Ctrl Pts',(0.881531712257153,2.64643874397719,9.67702980010063));
#76372=CARTESIAN_POINT('Ctrl Pts',(0.607964326124389,2.95729913578499,9.69797635490342));
#76373=CARTESIAN_POINT('Ctrl Pts',(0.146117437660257,3.13759906306215,9.7230321873618));
#76374=CARTESIAN_POINT('Ctrl Pts',(-0.345304308274442,3.08590135078223,
9.74801368543017));
#76375=CARTESIAN_POINT('Ctrl Pts',(-0.756976146008362,2.81525529634975,
9.77291797455823));
#76376=CARTESIAN_POINT('Ctrl Pts',(-0.997717508088822,2.38715531499302,
9.79774602149462));
#76377=CARTESIAN_POINT('Ctrl Pts',(-1.01506151072978,1.89783538729067,9.82249714066535));
#76378=CARTESIAN_POINT('Ctrl Pts',(-0.806515684265896,1.45651892696938,
9.84717145196844));
#76379=CARTESIAN_POINT('Ctrl Pts',(-0.419883171833556,1.16108253062822,
9.87176878241307));
#76380=CARTESIAN_POINT('Ctrl Pts',(0.0577202993719235,1.07634276501048,
9.89628915431694));
#76381=CARTESIAN_POINT('Ctrl Pts',(0.519484551037105,1.21981225012954,9.920732569481));
#76382=CARTESIAN_POINT('Ctrl Pts',(0.862788216351348,1.5581888500835,9.94509910118577));
#76383=CARTESIAN_POINT('Ctrl Pts',(1.01202267624069,2.01488089045114,9.96938887034206));
#76384=CARTESIAN_POINT('Ctrl Pts',(0.935188214037597,2.4877796210854,9.99360202114725));
#76385=CARTESIAN_POINT('Ctrl Pts',(0.650855911768474,2.87110216479637,10.0177388018848));
#76386=CARTESIAN_POINT('Ctrl Pts',(0.175957669185131,3.10461154539347,10.0444727503347));
#76387=CARTESIAN_POINT('Ctrl Pts',(-0.413167711787148,3.04566930798458,
10.0737725308512));
#76388=CARTESIAN_POINT('Ctrl Pts',(-0.890919517513664,2.61284831774276,
10.1056022275272));
#76389=CARTESIAN_POINT('Ctrl Pts',(-0.995095843058391,2.08946109816007,
10.1320154342246));
#76390=CARTESIAN_POINT('Ctrl Pts',(-0.881857808909978,1.69509979853437,
10.1530795785575));
#76391=CARTESIAN_POINT('Ctrl Pts',(-0.709848962015113,1.4408985803547,10.1688450423686));
#76392=CARTESIAN_POINT('Ctrl Pts',(-0.467231119511972,1.2540641047854,10.1845779386659));
#76393=CARTESIAN_POINT('Ctrl Pts',(-0.0828134109998774,1.11758673889094,
10.2055113384881));
#76394=CARTESIAN_POINT('Ctrl Pts',(0.369452164886118,1.18058988554342,10.2281221188686));
#76395=CARTESIAN_POINT('Ctrl Pts',(0.7440178520349,1.47670100636996,10.252386384903));
#76396=CARTESIAN_POINT('Ctrl Pts',(0.932024497398691,1.83837824126288,10.2731281089248));
#76397=CARTESIAN_POINT('Ctrl Pts',(0.952644215160796,2.21088284443421,10.2920911026948));
#76398=CARTESIAN_POINT('Ctrl Pts',(0.848525607611788,2.52898866039414,10.3092894684908));
#76399=CARTESIAN_POINT('Ctrl Pts',(0.611667175977124,2.85284466806143,10.3298862729762));
#76400=CARTESIAN_POINT('Ctrl Pts',(0.146965686342124,3.08368825181904,10.3555582533163));
#76401=CARTESIAN_POINT('Ctrl Pts',(-0.464353171151464,2.975108638042,10.386243371414));
#76402=CARTESIAN_POINT('Ctrl Pts',(-0.889867125642017,2.52677225013601,
10.416811145006));
#76403=CARTESIAN_POINT('Ctrl Pts',(-0.965740853436312,1.91549196386248,
10.4472632931353));
#76404=CARTESIAN_POINT('Ctrl Pts',(-0.665009451066436,1.3807587525135,10.4776028117676));
#76405=CARTESIAN_POINT('Ctrl Pts',(-0.107204061616131,1.12977374293364,
10.5078318049331));
#76406=CARTESIAN_POINT('Ctrl Pts',(0.42164025457547,1.24476928475959,10.534607434734));
#76407=CARTESIAN_POINT('Ctrl Pts',(0.759718865620174,1.55601522514066,10.5579665142426));
#76408=CARTESIAN_POINT('Ctrl Pts',(0.914324817649136,1.91696166575999,10.5779435538898));
#76409=CARTESIAN_POINT('Ctrl Pts',(0.906569512809831,2.3088532786035,10.5978754983735));
#76410=CARTESIAN_POINT('Ctrl Pts',(0.738905867542777,2.6621948935939,10.6177631360867));
#76411=CARTESIAN_POINT('Ctrl Pts',(0.441235879468831,2.91426160241039,10.637607949746));
#76412=CARTESIAN_POINT('Ctrl Pts',(0.00456059090871799,3.04028767733564,
10.6607115176031));
#76413=CARTESIAN_POINT('Ctrl Pts',(-0.511236862099568,2.90870901173369,
10.6870502515913));
#76414=CARTESIAN_POINT('Ctrl Pts',(-0.889437964423829,2.44600479875113,
10.7165883937909));
#76415=CARTESIAN_POINT('Ctrl Pts',(-0.918086783201766,1.85081981438801,
10.7460453215445));
#76416=CARTESIAN_POINT('Ctrl Pts',(-0.589115930172112,1.35637751165594,
10.7754190974754));
#76417=CARTESIAN_POINT('Ctrl Pts',(-0.0318173159979765,1.15422575921844,
10.8047148729315));
#76418=CARTESIAN_POINT('Ctrl Pts',(0.471469629709559,1.30389074576235,10.8306915854604));
#76419=CARTESIAN_POINT('Ctrl Pts',(0.776137002363046,1.62977906851438,10.8533714866067));
#76420=CARTESIAN_POINT('Ctrl Pts',(0.879201460171853,1.93054705157793,10.8695469973497));
#76421=CARTESIAN_POINT('Ctrl Pts',(0.881792886165801,2.1804515005481,10.8824726714454));
#76422=CARTESIAN_POINT('Ctrl Pts',(0.824281002588274,2.46622964067337,10.8975414512373));
#76423=CARTESIAN_POINT('Ctrl Pts',(0.644771590343777,2.73390655574528,10.9136676846433));
#76424=CARTESIAN_POINT('Ctrl Pts',(0.326172155862462,2.93244834317385,10.932988933727));
#76425=CARTESIAN_POINT('Ctrl Pts',(-0.00389180032462818,3.00123878482214,
10.9501482361413));
#76426=CARTESIAN_POINT('Ctrl Pts',(-0.374069531768034,2.91882600059989,
10.9694246322533));
#76427=CARTESIAN_POINT('Ctrl Pts',(-0.676770714493534,2.69175674503232,
10.9886811485452));
#76428=CARTESIAN_POINT('Ctrl Pts',(-0.890457839169829,2.30547459389054,
11.0111195762753));
#76429=CARTESIAN_POINT('Ctrl Pts',(-0.877420955696323,1.78796824742822,
11.0367326718632));
#76430=CARTESIAN_POINT('Ctrl Pts',(-0.519542383046932,1.32879774668238,
11.0655040102286));
#76431=CARTESIAN_POINT('Ctrl Pts',(0.0399490643477976,1.17212920136542,
11.0942383879097));
#76432=CARTESIAN_POINT('Ctrl Pts',(0.582718196329541,1.37801627095207,11.1229395555505));
#76433=CARTESIAN_POINT('Ctrl Pts',(0.896745247812362,1.86556201558046,11.1516121597076));
#76434=CARTESIAN_POINT('Ctrl Pts',(0.860059296447071,2.44367223802959,11.1802608561107));
#76435=CARTESIAN_POINT('Ctrl Pts',(0.487287812128845,2.88705936152277,11.2088896613278));
#76436=CARTESIAN_POINT('Ctrl Pts',(-0.0126793677166393,3.00666626742902,
11.2343251238526));
#76437=CARTESIAN_POINT('Ctrl Pts',(-0.431368788585849,2.8792260766813,11.256572216763));
#76438=CARTESIAN_POINT('Ctrl Pts',(-0.713776887062524,2.63297361864757,
11.2756367991276));
#76439=CARTESIAN_POINT('Ctrl Pts',(-0.869675700701866,2.29192787722306,
11.2947015047042));
#76440=CARTESIAN_POINT('Ctrl Pts',(-0.871754349920706,1.91719764545345,
11.3137629349912));
#76441=CARTESIAN_POINT('Ctrl Pts',(-0.719284033324151,1.57464106746168,
11.3328277507209));
#76442=CARTESIAN_POINT('Ctrl Pts',(-0.439566572325031,1.32517731125754,
11.3518929564459));
#76443=CARTESIAN_POINT('Ctrl Pts',(-0.0817424075530357,1.21263403993146,
11.3709626858035));
#76444=CARTESIAN_POINT('Ctrl Pts',(0.290412185317624,1.25756731850338,11.3900351084129));
#76445=CARTESIAN_POINT('Ctrl Pts',(0.6655187140127,1.48335758138164,11.4122929276818));
#76446=CARTESIAN_POINT('Ctrl Pts',(0.911646236291874,1.93514475264904,11.4377467160272));
#76447=CARTESIAN_POINT('Ctrl Pts',(0.831748897734901,2.5094592535539,11.4664011327166));
#76448=CARTESIAN_POINT('Ctrl Pts',(0.42653080354753,2.92417639523713,11.4950808407273));
#76449=CARTESIAN_POINT('Ctrl Pts',(-0.14681541068467,3.01769219474351,11.5237915175372));
#76450=CARTESIAN_POINT('Ctrl Pts',(-0.663565009681244,2.75164209798711,
11.5525329012227));
#76451=CARTESIAN_POINT('Ctrl Pts',(-0.922343659292911,2.23017004462751,
11.5813153753167));
#76452=CARTESIAN_POINT('Ctrl Pts',(-0.82072898896079,1.65621568500738,11.6101398171542));
#76453=CARTESIAN_POINT('Ctrl Pts',(-0.397384311892478,1.25368822232143,
11.6390127119604));
#76454=CARTESIAN_POINT('Ctrl Pts',(0.183049465176804,1.18189553873558,11.6679338789258));
#76455=CARTESIAN_POINT('Ctrl Pts',(0.694090218061655,1.46877497685727,11.6969126968832));
#76456=CARTESIAN_POINT('Ctrl Pts',(0.935321267131387,2.00426367937146,11.725950863301));
#76457=CARTESIAN_POINT('Ctrl Pts',(0.811264797020236,2.57949055623937,11.7550527002716));
#76458=CARTESIAN_POINT('Ctrl Pts',(0.368614734530845,2.96985351560571,11.7842218445857));
#76459=CARTESIAN_POINT('Ctrl Pts',(-0.171225999656093,3.01635946820556,
11.8110263031446));
#76460=CARTESIAN_POINT('Ctrl Pts',(-0.601966326773585,2.79712243250774,
11.8354476933365));
#76461=CARTESIAN_POINT('Ctrl Pts',(-0.856635786021019,2.44387729840415,
11.8574712161541));
#76462=CARTESIAN_POINT('Ctrl Pts',(-0.920780349043476,2.01195470589779,
11.8795401240644));
#76463=CARTESIAN_POINT('Ctrl Pts',(-0.779294306257107,1.59802697812281,
11.901656095375));
#76464=CARTESIAN_POINT('Ctrl Pts',(-0.462897586535699,1.29448147638559,
11.9238205287533));
#76465=CARTESIAN_POINT('Ctrl Pts',(-0.0415426238937191,1.1697542653126,
11.9460349558951));
#76466=CARTESIAN_POINT('Ctrl Pts',(0.391061638465007,1.25250459967951,11.968300755167));
#76467=CARTESIAN_POINT('Ctrl Pts',(0.738250016927639,1.52522229421188,11.9906194062099));
#76468=CARTESIAN_POINT('Ctrl Pts',(0.921992585201663,1.92784239197626,12.012992073041));
#76469=CARTESIAN_POINT('Ctrl Pts',(0.900393282784436,2.37097208359455,12.0354205108322));
#76470=CARTESIAN_POINT('Ctrl Pts',(0.677271806505565,2.75575131201869,12.0579050641389));
#76471=CARTESIAN_POINT('Ctrl Pts',(0.301444205308227,2.99578096804062,12.0804491519056));
#76472=CARTESIAN_POINT('Ctrl Pts',(-0.143737457268676,3.03675145400947,
12.1030492099952));
#76473=CARTESIAN_POINT('Ctrl Pts',(-0.559307355611989,2.86815774679212,
12.1257171734423));
#76474=CARTESIAN_POINT('Ctrl Pts',(-0.802911717332437,2.58405107780456,
12.1446443351558));
#76475=CARTESIAN_POINT('Ctrl Pts',(-0.903878021992128,2.30723336901298,
12.159841505477));
#76476=CARTESIAN_POINT('Ctrl Pts',(-0.920298150261432,2.16243836817539,
12.1674290389266));
#76477=CARTESIAN_POINT('Ctrl Pts',(-0.919891595085131,2.08831921315703,
12.1712341381108));
#76478=CARTESIAN_POINT('Ctrl Pts',(1.10362653322406,2.1,9.57968132589776));
#76479=CARTESIAN_POINT('Ctrl Pts',(1.10332385859517,2.18836737691272,9.58422494608045));
#76480=CARTESIAN_POINT('Ctrl Pts',(1.08191344062549,2.3625059514978,9.59336230827583));
#76481=CARTESIAN_POINT('Ctrl Pts',(0.957835600463251,2.69310587840379,9.61156968419157));
#76482=CARTESIAN_POINT('Ctrl Pts',(0.661841991943411,3.03223916038163,9.63434167170328));
#76483=CARTESIAN_POINT('Ctrl Pts',(0.159943307176907,3.23039051797218,9.66161187516289));
#76484=CARTESIAN_POINT('Ctrl Pts',(-0.376051688795035,3.17620291801981,
9.68885171355759));
#76485=CARTESIAN_POINT('Ctrl Pts',(-0.826750739733302,2.88245239593225,
9.71604756503803));
#76486=CARTESIAN_POINT('Ctrl Pts',(-1.09190901430628,2.41533590672408,9.74320319226711));
#76487=CARTESIAN_POINT('Ctrl Pts',(-1.11305483350507,1.87947767032364,9.77031460500698));
#76488=CARTESIAN_POINT('Ctrl Pts',(-0.88625766736864,1.39450346688661,9.79738131769857));
#76489=CARTESIAN_POINT('Ctrl Pts',(-0.462890049527857,1.06828884415501,
9.82440133351827));
#76490=CARTESIAN_POINT('Ctrl Pts',(0.0620431770221235,0.972966819483573,
9.85137337108375));
#76491=CARTESIAN_POINT('Ctrl Pts',(0.571236025368607,1.12891854941223,9.87829586868765));
#76492=CARTESIAN_POINT('Ctrl Pts',(0.951314593883381,1.50051940417938,9.9051673999022));
#76493=CARTESIAN_POINT('Ctrl Pts',(1.11812369875706,2.0040613394318,9.93198652208759));
#76494=CARTESIAN_POINT('Ctrl Pts',(1.03532433897197,2.52711479570303,9.95875180884655));
#76495=CARTESIAN_POINT('Ctrl Pts',(0.722426325350036,2.95256083044233,9.9854620047878));
#76496=CARTESIAN_POINT('Ctrl Pts',(0.197440843038474,3.21337088955047,10.0150770435447));
#76497=CARTESIAN_POINT('Ctrl Pts',(-0.456162767182428,3.15073737091323,
10.047572536222));
#76498=CARTESIAN_POINT('Ctrl Pts',(-0.988651479746515,2.67238263836449,
10.0829168835724));
#76499=CARTESIAN_POINT('Ctrl Pts',(-1.10688911431785,2.09107215671169,10.1122789590279));
#76500=CARTESIAN_POINT('Ctrl Pts',(-0.982706695062194,1.65185618948298,
10.1357121466742));
#76501=CARTESIAN_POINT('Ctrl Pts',(-0.792422518102662,1.3681585717153,10.1532592369429));
#76502=CARTESIAN_POINT('Ctrl Pts',(-0.523124675612585,1.15901941614237,
10.1707779412534));
#76503=CARTESIAN_POINT('Ctrl Pts',(-0.0955313023476177,1.0052357524766,
10.1940973000699));
#76504=CARTESIAN_POINT('Ctrl Pts',(0.408862852638258,1.07334669481587,10.2193005196674));
#76505=CARTESIAN_POINT('Ctrl Pts',(0.827965416044339,1.40185468333059,10.2463619074908));
#76506=CARTESIAN_POINT('Ctrl Pts',(1.03939646109892,1.80450850302264,10.2695041218372));
#76507=CARTESIAN_POINT('Ctrl Pts',(1.06413743020716,2.22016319496911,10.2906690517014));
#76508=CARTESIAN_POINT('Ctrl Pts',(0.949371402568083,2.57577634655705,10.3098696021912));
#76509=CARTESIAN_POINT('Ctrl Pts',(0.68639441872527,2.93849673521478,10.3328687806801));
#76510=CARTESIAN_POINT('Ctrl Pts',(0.168455748548128,3.19850041638645,10.3615416008252));
#76511=CARTESIAN_POINT('Ctrl Pts',(-0.514981141538362,3.08006574061132,
10.395821174426));
#76512=CARTESIAN_POINT('Ctrl Pts',(-0.992484975124322,2.58115298612403,
10.4299727529598));
#76513=CARTESIAN_POINT('Ctrl Pts',(-1.08011179202778,1.89857319405739,10.4639941490101));
#76514=CARTESIAN_POINT('Ctrl Pts',(-0.746677452129509,1.2998396969781,10.4978844286978));
#76515=CARTESIAN_POINT('Ctrl Pts',(-0.124919825186299,1.01695088669628,
10.5316419697814));
#76516=CARTESIAN_POINT('Ctrl Pts',(0.465959941776284,1.14285421449709,10.5615302638894));
#76517=CARTESIAN_POINT('Ctrl Pts',(0.84465605145784,1.48855843425709,10.587594536741));
#76518=CARTESIAN_POINT('Ctrl Pts',(1.0187956561827,1.8904143255726,10.6098754554049));
#76519=CARTESIAN_POINT('Ctrl Pts',(1.01199111001941,2.3273475800656,10.6320960171808));
#76520=CARTESIAN_POINT('Ctrl Pts',(0.826831590311268,2.72185411327491,10.6542558772749));
#76521=CARTESIAN_POINT('Ctrl Pts',(0.496525135839689,3.00395863731658,10.6763551851293));
#76522=CARTESIAN_POINT('Ctrl Pts',(0.0111327324295966,3.14626897049278,
10.7020667852219));
#76523=CARTESIAN_POINT('Ctrl Pts',(-0.562996470319803,3.00232707281753,
10.7313506493589));
#76524=CARTESIAN_POINT('Ctrl Pts',(-0.985170581520541,2.49014805337043,
10.7641569125056));
#76525=CARTESIAN_POINT('Ctrl Pts',(-1.01964968628344,1.83010686065805,10.796826521172));
#76526=CARTESIAN_POINT('Ctrl Pts',(-0.657524636731054,1.2809574776055,10.82935855228));
#76527=CARTESIAN_POINT('Ctrl Pts',(-0.0421227513948548,1.05489108814208,
10.8617537289328));
#76528=CARTESIAN_POINT('Ctrl Pts',(0.514174199288179,1.21785062909781,10.8904278519412));
#76529=CARTESIAN_POINT('Ctrl Pts',(0.85154389222315,1.57569141984744,10.9154296374838));
#76530=CARTESIAN_POINT('Ctrl Pts',(0.966417014836512,1.90635215236884,10.9332377402664));
#76531=CARTESIAN_POINT('Ctrl Pts',(0.970453646751313,2.18120687331145,10.9474542331084));
#76532=CARTESIAN_POINT('Ctrl Pts',(0.90859469374289,2.4956012577166,10.9640168231539));
#76533=CARTESIAN_POINT('Ctrl Pts',(0.712752704384257,2.79023506214752,10.9817165375888));
#76534=CARTESIAN_POINT('Ctrl Pts',(0.364433695189235,3.00937789540993,11.002897218119));
#76535=CARTESIAN_POINT('Ctrl Pts',(0.0034024942377313,3.08620224921852,
11.0216801159058));
#76536=CARTESIAN_POINT('Ctrl Pts',(-0.401645366979633,2.99780965747371,
11.0427525334315));
#76537=CARTESIAN_POINT('Ctrl Pts',(-0.733040599057254,2.75137242952113,
11.0637659149067));
#76538=CARTESIAN_POINT('Ctrl Pts',(-0.967642155109252,2.33143421543358,
11.0882140885227));
#76539=CARTESIAN_POINT('Ctrl Pts',(-0.955682954326625,1.76869539969966,
11.1160579226578));
#76540=CARTESIAN_POINT('Ctrl Pts',(-0.569539517922979,1.26924071592032,
11.1472543095408));
#76541=CARTESIAN_POINT('Ctrl Pts',(0.0348519939173318,1.09745482173835,
11.1783238828312));
#76542=CARTESIAN_POINT('Ctrl Pts',(0.62100013835726,1.31719642390597,11.2092686904388));
#76543=CARTESIAN_POINT('Ctrl Pts',(0.96064358272864,1.84006069348993,11.2400905755795));
#76544=CARTESIAN_POINT('Ctrl Pts',(0.923712874736882,2.45983807259137,11.2707915176385));
#76545=CARTESIAN_POINT('Ctrl Pts',(0.527253109689211,2.93507386065005,11.3013740167069));
#76546=CARTESIAN_POINT('Ctrl Pts',(-0.00465921901833066,3.06447451657243,
11.3284545295349));
#76547=CARTESIAN_POINT('Ctrl Pts',(-0.449822784075272,2.93095416511392,
11.3520772589442));
#76548=CARTESIAN_POINT('Ctrl Pts',(-0.750117905009269,2.67126179915912,
11.3722760149046));
#76549=CARTESIAN_POINT('Ctrl Pts',(-0.916368328645713,2.31143790952571,
11.3924246439911));
#76550=CARTESIAN_POINT('Ctrl Pts',(-0.920169991093076,1.91625186699829,
11.4125264404411));
#76551=CARTESIAN_POINT('Ctrl Pts',(-0.761222390223333,1.55523216818356,
11.4325793615504));
#76552=CARTESIAN_POINT('Ctrl Pts',(-0.468713235571315,1.29223530601167,
11.4525866575616));
#76553=CARTESIAN_POINT('Ctrl Pts',(-0.0945728793433094,1.17291557007476,
11.4725475641567));
#76554=CARTESIAN_POINT('Ctrl Pts',(0.294277762638305,1.21828642696366,11.4924650411748));
#76555=CARTESIAN_POINT('Ctrl Pts',(0.686000429294125,1.45195139999478,11.515651150288));
#76556=CARTESIAN_POINT('Ctrl Pts',(0.943285829534123,1.92015599730346,11.5420752789794));
#76557=CARTESIAN_POINT('Ctrl Pts',(0.862784257153681,2.51453311516829,11.5717107622048));
#76558=CARTESIAN_POINT('Ctrl Pts',(0.446786716728484,2.94334169871474,11.6012565534465));
#76559=CARTESIAN_POINT('Ctrl Pts',(-0.141294894410705,3.04141484108333,
11.6307150656786));
#76560=CARTESIAN_POINT('Ctrl Pts',(-0.670496611937673,2.7713159237941,11.6600938870429));
#76561=CARTESIAN_POINT('Ctrl Pts',(-0.935835849607687,2.24134218677815,
11.6893911557916));
#76562=CARTESIAN_POINT('Ctrl Pts',(-0.834835581082013,1.65900363230969,
11.7186141015149));
#76563=CARTESIAN_POINT('Ctrl Pts',(-0.408739935114945,1.25103259511225,
11.7477640283533));
#76564=CARTESIAN_POINT('Ctrl Pts',(0.17478220598524,1.17681438957091,11.7768498186601));
#76565=CARTESIAN_POINT('Ctrl Pts',(0.687633529056747,1.46239191516575,11.8058695158234));
#76566=CARTESIAN_POINT('Ctrl Pts',(0.930087435743391,1.99572519490728,11.8348301864855));
#76567=CARTESIAN_POINT('Ctrl Pts',(0.808788711597153,2.56759105376501,11.8637352173148));
#76568=CARTESIAN_POINT('Ctrl Pts',(0.372142364372509,2.95527860777237,11.8925892923752));
#76569=CARTESIAN_POINT('Ctrl Pts',(-0.159618674117736,3.00289391958003,
11.9189950219207));
#76570=CARTESIAN_POINT('Ctrl Pts',(-0.583320569409584,2.78916288240356,
11.94297075703));
#76571=CARTESIAN_POINT('Ctrl Pts',(-0.833868275993026,2.44427205908894,
11.9645263067009));
#76572=CARTESIAN_POINT('Ctrl Pts',(-0.897983936371958,2.02295745107859,
11.9860615833256));
#76573=CARTESIAN_POINT('Ctrl Pts',(-0.761752582443683,1.61969407972814,
12.0075782437171));
#76574=CARTESIAN_POINT('Ctrl Pts',(-0.455842358238346,1.32411057372178,
12.0290782429238));
#76575=CARTESIAN_POINT('Ctrl Pts',(-0.048683049811289,1.20201416224315,
12.0505634713502));
#76576=CARTESIAN_POINT('Ctrl Pts',(0.36885285869097,1.28035488007001,12.0720357864435));
#76577=CARTESIAN_POINT('Ctrl Pts',(0.703682538373774,1.54146396668747,12.0934971695462));
#76578=CARTESIAN_POINT('Ctrl Pts',(0.881249234813493,1.92696228266429,12.1149492451026));
#76579=CARTESIAN_POINT('Ctrl Pts',(0.862077846834763,2.35080266214842,12.1363944669441));
#76580=CARTESIAN_POINT('Ctrl Pts',(0.650581145027489,2.71849457060569,12.1578334355429));
#76581=CARTESIAN_POINT('Ctrl Pts',(0.293950474197431,2.94800565088334,12.179270942516));
#76582=CARTESIAN_POINT('Ctrl Pts',(-0.12814443883228,2.98834258470624,12.2007023996387));
#76583=CARTESIAN_POINT('Ctrl Pts',(-0.521799371244013,2.83016779854685,
12.222144175476));
#76584=CARTESIAN_POINT('Ctrl Pts',(-0.752511019951562,2.562980435684,12.2399948578996));
#76585=CARTESIAN_POINT('Ctrl Pts',(-0.848550148047341,2.30251473117147,
12.2543110264422));
#76586=CARTESIAN_POINT('Ctrl Pts',(-0.864472773112078,2.16656466527785,
12.2614376415572));
#76587=CARTESIAN_POINT('Ctrl Pts',(-0.864339839017289,2.09666417179271,
12.2650284080295));
#76588=CARTESIAN_POINT('Ctrl Pts',(1.10329394384097,2.1,9.47044698901065));
#76589=CARTESIAN_POINT('Ctrl Pts',(1.10342577318052,2.18844051481166,9.47499047623415));
#76590=CARTESIAN_POINT('Ctrl Pts',(1.08292697012135,2.36279317326597,9.48413095460293));
#76591=CARTESIAN_POINT('Ctrl Pts',(0.960358942581555,2.69455029900241,9.50236886786829));
#76592=CARTESIAN_POINT('Ctrl Pts',(0.665197290461623,3.03649933706296,9.52521501416534));
#76593=CARTESIAN_POINT('Ctrl Pts',(0.161391500207772,3.23853294280124,9.55264408464405));
#76594=CARTESIAN_POINT('Ctrl Pts',(-0.3793961911153,3.18679347595313,9.58010840950997));
#76595=CARTESIAN_POINT('Ctrl Pts',(-0.836587092669218,2.89228198671027,
9.60759595890492));
#76596=CARTESIAN_POINT('Ctrl Pts',(-1.10781716561319,2.42036554420295,9.63510948939038));
#76597=CARTESIAN_POINT('Ctrl Pts',(-1.13221150762356,1.87614146775605,9.66264511777613));
#76598=CARTESIAN_POINT('Ctrl Pts',(-0.903913086637555,1.38105914971141,
9.69020192194118));
#76599=CARTESIAN_POINT('Ctrl Pts',(-0.473548122300964,1.04575615380141,
9.717777663979));
#76600=CARTESIAN_POINT('Ctrl Pts',(0.0630410671544533,0.945336835228206,
9.74537069120911));
#76601=CARTESIAN_POINT('Ctrl Pts',(0.586155308009602,1.10248110373778,9.77297906556861));
#76602=CARTESIAN_POINT('Ctrl Pts',(0.97896721945666,1.48242126689961,9.80060095834541));
#76603=CARTESIAN_POINT('Ctrl Pts',(1.15366073282743,2.00041306644017,9.82823441377605));
#76604=CARTESIAN_POINT('Ctrl Pts',(1.07104056272652,2.54117175963957,9.85587763787474));
#76605=CARTESIAN_POINT('Ctrl Pts',(0.749438508422974,2.98341757445515,9.88352858181668));
#76606=CARTESIAN_POINT('Ctrl Pts',(0.206071066343861,3.25703059287624,9.91425882120625));
#76607=CARTESIAN_POINT('Ctrl Pts',(-0.474407586679752,3.19565870375735,
9.94806588138852));
#76608=CARTESIAN_POINT('Ctrl Pts',(-1.03300889611883,2.69951233227857,9.9849483264369));
#76609=CARTESIAN_POINT('Ctrl Pts',(-1.16019631587872,2.09158946634905,10.0156839772865));
#76610=CARTESIAN_POINT('Ctrl Pts',(-1.03231832446509,1.63001844177956,10.0402706670585));
#76611=CARTESIAN_POINT('Ctrl Pts',(-0.833926194436441,1.3308462035937,10.0587080269736));
#76612=CARTESIAN_POINT('Ctrl Pts',(-0.551677262472857,1.10925403577857,
10.0771425266126));
#76613=CARTESIAN_POINT('Ctrl Pts',(-0.10187955485641,0.944796612224074,
10.101718548257));
#76614=CARTESIAN_POINT('Ctrl Pts',(0.431214416355967,1.01375057212635,10.1283277734834));
#76615=CARTESIAN_POINT('Ctrl Pts',(0.876826776842245,1.35918124772021,10.1569777420977));
#76616=CARTESIAN_POINT('Ctrl Pts',(1.10339080843243,1.78510336459368,10.1815245804526));
#76617=CARTESIAN_POINT('Ctrl Pts',(1.13206152107633,2.22668002384982,10.2040138041529));
#76618=CARTESIAN_POINT('Ctrl Pts',(1.01189652022592,2.60586469879454,10.2244501669362));
#76619=CARTESIAN_POINT('Ctrl Pts',(0.733641827560973,2.99397501004058,10.2489638393176));
#76620=CARTESIAN_POINT('Ctrl Pts',(0.182030027737687,3.27476674135432,10.2795811045697));
#76621=CARTESIAN_POINT('Ctrl Pts',(-0.550583503416367,3.15205884217581,
10.3162865257328));
#76622=CARTESIAN_POINT('Ctrl Pts',(-1.06629714487458,2.61925513593017,10.3529493854541));
#76623=CARTESIAN_POINT('Ctrl Pts',(-1.16476552168883,1.88502805076137,10.389566510702));
#76624=CARTESIAN_POINT('Ctrl Pts',(-0.808598434657076,1.23689007105085,
10.4261328995388));
#76625=CARTESIAN_POINT('Ctrl Pts',(-0.137754182673855,0.927075763803486,
10.4626450549438));
#76626=CARTESIAN_POINT('Ctrl Pts',(0.503690057736241,1.05996953035151,10.495046832965));
#76627=CARTESIAN_POINT('Ctrl Pts',(0.917146925299477,1.4332859468041,10.5233599744073));
#76628=CARTESIAN_POINT('Ctrl Pts',(1.10898999507462,1.86945446726646,10.547598536504));
#76629=CARTESIAN_POINT('Ctrl Pts',(1.10417701875731,2.34555607374905,10.5718072285612));
#76630=CARTESIAN_POINT('Ctrl Pts',(0.904506920874453,2.77711621170411,10.5959851258615));
#76631=CARTESIAN_POINT('Ctrl Pts',(0.545286687123858,3.08732878341821,10.6201303114132));
#76632=CARTESIAN_POINT('Ctrl Pts',(0.015076277217216,3.24595196324875,10.6482602553399));
#76633=CARTESIAN_POINT('Ctrl Pts',(-0.614985359098582,3.09176141069313,
10.6803476073743));
#76634=CARTESIAN_POINT('Ctrl Pts',(-1.08173166535535,2.53202576584709,10.7163683911006));
#76635=CARTESIAN_POINT('Ctrl Pts',(-1.12377096357778,1.80620962017753,10.7522995324198));
#76636=CARTESIAN_POINT('Ctrl Pts',(-0.728194421216213,1.19884669077671,
10.7881432926498));
#76637=CARTESIAN_POINT('Ctrl Pts',(-0.0504048859193792,0.945479795171635,
10.823894484474));
#76638=CARTESIAN_POINT('Ctrl Pts',(0.565533637893201,1.12211398585112,10.8555867339139));
#76639=CARTESIAN_POINT('Ctrl Pts',(0.941120756083501,1.51607388859285,10.8832566231257));
#76640=CARTESIAN_POINT('Ctrl Pts',(1.07041286826489,1.88164852196315,10.9029829474289));
#76641=CARTESIAN_POINT('Ctrl Pts',(1.07656705582405,2.18629511203114,10.918741283468));
#76642=CARTESIAN_POINT('Ctrl Pts',(1.0098967166809,2.53531809348986,10.9371081667145));
#76643=CARTESIAN_POINT('Ctrl Pts',(0.794402553909074,2.86352027212041,10.9567496467229));
#76644=CARTESIAN_POINT('Ctrl Pts',(0.40889178297773,3.10906836029478,10.9802745270439));
#76645=CARTESIAN_POINT('Ctrl Pts',(0.00815355763257491,3.19668782334102,
11.001147248245));
#76646=CARTESIAN_POINT('Ctrl Pts',(-0.442857467235114,3.10091996763833,
11.0245823977996));
#76647=CARTESIAN_POINT('Ctrl Pts',(-0.813178211939382,2.8287505972283,11.0479657008531));
#76648=CARTESIAN_POINT('Ctrl Pts',(-1.0770401110669,2.36262856096914,11.0751885334277));
#76649=CARTESIAN_POINT('Ctrl Pts',(-1.06728995829791,1.73552287386719,11.1062128575312));
#76650=CARTESIAN_POINT('Ctrl Pts',(-0.63990437237774,1.17614522551949,11.1409983119522));
#76651=CARTESIAN_POINT('Ctrl Pts',(0.0333343650464638,0.980625242717132,
11.1756633724409));
#76652=CARTESIAN_POINT('Ctrl Pts',(0.689032879068862,1.2221713856248,11.2102063445392));
#76653=CARTESIAN_POINT('Ctrl Pts',(1.07164646520174,1.80387086382317,11.2446250685247));
#76654=CARTESIAN_POINT('Ctrl Pts',(1.03435973521343,2.49637056796218,11.2789176920495));
#76655=CARTESIAN_POINT('Ctrl Pts',(0.594514117701379,3.02979345316445,11.3130826051129));
#76656=CARTESIAN_POINT('Ctrl Pts',(0.00113517293498442,3.17775143047368,
11.3433361512686));
#76657=CARTESIAN_POINT('Ctrl Pts',(-0.496970892975936,3.0314653783563,11.3697238228033));
#76658=CARTESIAN_POINT('Ctrl Pts',(-0.83402502340684,2.74335862335544,11.3922835866429));
#76659=CARTESIAN_POINT('Ctrl Pts',(-1.02198410458089,2.34262871620902,11.4147839634241));
#76660=CARTESIAN_POINT('Ctrl Pts',(-1.02877477377512,1.90148026772762,11.4372257172929));
#76661=CARTESIAN_POINT('Ctrl Pts',(-0.853709064146416,1.4975378686245,11.4596074513842));
#76662=CARTESIAN_POINT('Ctrl Pts',(-0.529071349327787,1.20223601985623,
11.4819297012752));
#76663=CARTESIAN_POINT('Ctrl Pts',(-0.11260310159066,1.06675150648581,11.5041917957278));
#76664=CARTESIAN_POINT('Ctrl Pts',(0.321122066438537,1.1148034009953,11.5263938697568));
#76665=CARTESIAN_POINT('Ctrl Pts',(0.759040101660253,1.37258360382036,11.5522258911492));
#76666=CARTESIAN_POINT('Ctrl Pts',(1.04846654712675,1.8921835768978,11.58164708954));
#76667=CARTESIAN_POINT('Ctrl Pts',(0.962728469055807,2.55372914824236,11.614609496841));
#76668=CARTESIAN_POINT('Ctrl Pts',(0.503342729250649,3.03274480310301,11.6474349234281));
#76669=CARTESIAN_POINT('Ctrl Pts',(-0.148505353019908,3.1452972651178,11.6801237007564));
#76670=CARTESIAN_POINT('Ctrl Pts',(-0.736533824900539,2.84942649920226,
11.7126750368427));
#76671=CARTESIAN_POINT('Ctrl Pts',(-1.03342940126492,2.26482068051217,11.745090293276));
#76672=CARTESIAN_POINT('Ctrl Pts',(-0.925579138077888,1.62102516068567,
11.7773689257223));
#76673=CARTESIAN_POINT('Ctrl Pts',(-0.458390819496423,1.16854747640426,
11.8095122649012));
#76674=CARTESIAN_POINT('Ctrl Pts',(0.183210697649094,1.08318585175787,11.8415193363785));
#76675=CARTESIAN_POINT('Ctrl Pts',(0.748201733912437,1.39356481279695,11.873392966908));
#76676=CARTESIAN_POINT('Ctrl Pts',(1.01723547526947,1.97645989455456,11.9051330348159));
#76677=CARTESIAN_POINT('Ctrl Pts',(0.888207762276212,2.60244725135778,11.9367408674874));
#76678=CARTESIAN_POINT('Ctrl Pts',(0.414384154620261,3.02802732512881,11.9682174550523));
#76679=CARTESIAN_POINT('Ctrl Pts',(-0.163856583091941,3.08315384425318,
11.9969524799254));
#76680=CARTESIAN_POINT('Ctrl Pts',(-0.625132545752562,2.8538826750464,12.0229809361921));
#76681=CARTESIAN_POINT('Ctrl Pts',(-0.898760814954354,2.48188517101083,
12.0463353731295));
#76682=CARTESIAN_POINT('Ctrl Pts',(-0.970771244314516,2.02685423369152,
12.0696190747675));
#76683=CARTESIAN_POINT('Ctrl Pts',(-0.826406949387474,1.59098975034858,
12.0928329249704));
#76684=CARTESIAN_POINT('Ctrl Pts',(-0.499049475939726,1.2708959531523,12.1159776792298));
#76685=CARTESIAN_POINT('Ctrl Pts',(-0.0626016196059707,1.13717969866151,
12.1390542406761));
#76686=CARTESIAN_POINT('Ctrl Pts',(0.385226093706194,1.21844555315156,12.1620634870285));
#76687=CARTESIAN_POINT('Ctrl Pts',(0.744754606260194,1.49538834431159,12.185006400522));
#76688=CARTESIAN_POINT('Ctrl Pts',(0.936522631770819,1.90527961517333,12.207883870885));
#76689=CARTESIAN_POINT('Ctrl Pts',(0.91881495290156,2.35618381608074,12.2306971148174));
#76690=CARTESIAN_POINT('Ctrl Pts',(0.696757628070805,2.74758982982809,12.2534467581132));
#76691=CARTESIAN_POINT('Ctrl Pts',(0.320833811302139,2.99270696188793,12.2761349035034));
#76692=CARTESIAN_POINT('Ctrl Pts',(-0.124410755624645,3.03790832724789,
12.2987604893976));
#76693=CARTESIAN_POINT('Ctrl Pts',(-0.539746151577512,2.87395543188906,
12.3213296615096));
#76694=CARTESIAN_POINT('Ctrl Pts',(-0.783698509639943,2.59482193107452,
12.3400818248544));
#76695=CARTESIAN_POINT('Ctrl Pts',(-0.885939222791815,2.32279867038604,
12.3550664384198));
#76696=CARTESIAN_POINT('Ctrl Pts',(-0.903545681379915,2.18053231680427,
12.3625321136959));
#76697=CARTESIAN_POINT('Ctrl Pts',(-0.903850662021443,2.10752472519568,
12.3662864655665));
#76698=CARTESIAN_POINT('Ctrl Pts',(1.01808846413663,2.1,9.40201563814839));
#76699=CARTESIAN_POINT('Ctrl Pts',(1.01849147315277,2.18187084999355,9.4062191032581));
#76700=CARTESIAN_POINT('Ctrl Pts',(1.00016468627035,2.3426709426765,9.41464624341828));
#76701=CARTESIAN_POINT('Ctrl Pts',(0.887959809092518,2.64978712715063,9.43151018353515));
#76702=CARTESIAN_POINT('Ctrl Pts',(0.616026983517424,2.96710958003378,9.45264823379221));
#76703=CARTESIAN_POINT('Ctrl Pts',(0.149681573429148,3.15618792747452,9.47808179434013));
#76704=CARTESIAN_POINT('Ctrl Pts',(-0.352742227679569,3.10999193585024,
9.50359165643347));
#76705=CARTESIAN_POINT('Ctrl Pts',(-0.779178834210184,2.83755635812446,
9.52917339308576));
#76706=CARTESIAN_POINT('Ctrl Pts',(-1.03368228547638,2.39854156595712,9.55482813234504));
#76707=CARTESIAN_POINT('Ctrl Pts',(-1.05836131638902,1.89026860758708,9.58055443664554));
#76708=CARTESIAN_POINT('Ctrl Pts',(-0.846398546230643,1.42609608037824,
9.60635194366284));
#76709=CARTESIAN_POINT('Ctrl Pts',(-0.443933659380153,1.11013820065356,
9.63221975165276));
#76710=CARTESIAN_POINT('Ctrl Pts',(0.060006795418124,1.01391119317184,9.65815713286428));
#76711=CARTESIAN_POINT('Ctrl Pts',(0.553199930523459,1.16010058198549,9.68416322309809));
#76712=CARTESIAN_POINT('Ctrl Pts',(0.925230037674651,1.51732024200242,9.71023712611624));
#76713=CARTESIAN_POINT('Ctrl Pts',(1.09223473206028,2.00662699744739,9.73637791838438));
#76714=CARTESIAN_POINT('Ctrl Pts',(1.01578661403362,2.51946066235026,9.7625845501904));
#76715=CARTESIAN_POINT('Ctrl Pts',(0.711807865852075,2.94065805894325,9.78885616674331));
#76716=CARTESIAN_POINT('Ctrl Pts',(0.195466465705237,3.20300136333676,9.81811742809755));
#76717=CARTESIAN_POINT('Ctrl Pts',(-0.454284428104067,3.14688041935705,
9.85039646117044));
#76718=CARTESIAN_POINT('Ctrl Pts',(-0.990904714535579,2.67389174673884,
9.88571961297832));
#76719=CARTESIAN_POINT('Ctrl Pts',(-1.11525049429439,2.0905406551952,9.91524168134052));
#76720=CARTESIAN_POINT('Ctrl Pts',(-0.993670801030545,1.64585078282452,
9.93890924685948));
#76721=CARTESIAN_POINT('Ctrl Pts',(-0.803398272469515,1.35680145571654,
9.95668588659143));
#76722=CARTESIAN_POINT('Ctrl Pts',(-0.53159624646191,1.1419345970454,9.9744877201366));
#76723=CARTESIAN_POINT('Ctrl Pts',(-0.0971947775474125,0.981435858570208,
9.99825497858405));
#76724=CARTESIAN_POINT('Ctrl Pts',(0.419876807688296,1.04636718067241,10.0240633709415));
#76725=CARTESIAN_POINT('Ctrl Pts',(0.854104544531309,1.3805764433043,10.0519092585744));
#76726=CARTESIAN_POINT('Ctrl Pts',(1.07618290863117,1.79461751641221,10.0758179007607));
#76727=CARTESIAN_POINT('Ctrl Pts',(1.10564735137013,2.22550932349764,10.0977724598916));
#76728=CARTESIAN_POINT('Ctrl Pts',(0.989379762615938,2.59666957522658,10.1177580068108));
#76729=CARTESIAN_POINT('Ctrl Pts',(0.718140672799282,2.97766165579312,10.1417684970196));
#76730=CARTESIAN_POINT('Ctrl Pts',(0.177586859431589,3.25534176641867,10.1718391004231));
#76731=CARTESIAN_POINT('Ctrl Pts',(-0.544435702047864,3.13714319493199,
10.2080002287153));
#76732=CARTESIAN_POINT('Ctrl Pts',(-1.05596381191167,2.61253695386886,10.2442383709031));
#76733=CARTESIAN_POINT('Ctrl Pts',(-1.15623610986888,1.88502159145336,10.2805478018072));
#76734=CARTESIAN_POINT('Ctrl Pts',(-0.804336483382359,1.23911640326094,
10.3169262073463));
#76735=CARTESIAN_POINT('Ctrl Pts',(-0.136064293128745,0.927548352344434,
10.3533681275973));
#76736=CARTESIAN_POINT('Ctrl Pts',(0.506589586259768,1.05829532972237,10.3858164770831));
#76737=CARTESIAN_POINT('Ctrl Pts',(0.922867748799537,1.43166467517946,10.4142415645016));
#76738=CARTESIAN_POINT('Ctrl Pts',(1.11730226007746,1.86981865291231,10.438630689779));
#76739=CARTESIAN_POINT('Ctrl Pts',(1.11403495869486,2.34983756540438,10.4630417784934));
#76740=CARTESIAN_POINT('Ctrl Pts',(0.913723012313798,2.78652223706922,10.4874730015013));
#76741=CARTESIAN_POINT('Ctrl Pts',(0.551021545416392,3.10182228274919,10.5119244230016));
#76742=CARTESIAN_POINT('Ctrl Pts',(0.013529462665198,3.26453500307753,10.5404732227107));
#76743=CARTESIAN_POINT('Ctrl Pts',(-0.628149467334066,3.10992083738902,
10.5731348155084));
#76744=CARTESIAN_POINT('Ctrl Pts',(-1.10657260761457,2.54025825386416,10.6099062024022));
#76745=CARTESIAN_POINT('Ctrl Pts',(-1.15226055649189,1.79710936281507,10.6467151568618));
#76746=CARTESIAN_POINT('Ctrl Pts',(-0.748039471794684,1.17173686798412,
10.6835472472171));
#76747=CARTESIAN_POINT('Ctrl Pts',(-0.0504322098357749,0.908172355319504,
10.7204008353388));
#76748=CARTESIAN_POINT('Ctrl Pts',(0.587022329317992,1.08860382749987,10.7531780000451));
#76749=CARTESIAN_POINT('Ctrl Pts',(0.977623526768163,1.49569753576227,10.7818595776347));
#76750=CARTESIAN_POINT('Ctrl Pts',(1.11310778908442,1.87497891739192,10.8023509990786));
#76751=CARTESIAN_POINT('Ctrl Pts',(1.12046223639042,2.19187203555034,10.8187452228828));
#76752=CARTESIAN_POINT('Ctrl Pts',(1.05212955853369,2.55551285791366,10.8378724581563));
#76753=CARTESIAN_POINT('Ctrl Pts',(0.828422471948326,2.89870154904047,10.8583706541313));
#76754=CARTESIAN_POINT('Ctrl Pts',(0.426210055904798,3.15660019807515,10.882962075538));
#76755=CARTESIAN_POINT('Ctrl Pts',(0.00684383801692521,3.24968595364557,
10.9048257846384));
#76756=CARTESIAN_POINT('Ctrl Pts',(-0.466666320548942,3.15068796905064,
10.9294144771045));
#76757=CARTESIAN_POINT('Ctrl Pts',(-0.856906713548406,2.86577133671657,
10.9540037275576));
#76758=CARTESIAN_POINT('Ctrl Pts',(-1.13638351667166,2.37565790313556,10.9826820301581));
#76759=CARTESIAN_POINT('Ctrl Pts',(-1.12833605417664,1.71342840453131,11.0154509173227));
#76760=CARTESIAN_POINT('Ctrl Pts',(-0.677747788827833,1.11953149901379,
11.0522941233115));
#76761=CARTESIAN_POINT('Ctrl Pts',(0.0365114000399167,0.909493602222418,
11.089114442782));
#76762=CARTESIAN_POINT('Ctrl Pts',(0.735632783038763,1.16438673028385,11.1259060987032));
#76763=CARTESIAN_POINT('Ctrl Pts',(1.14626123588364,1.78418254458883,11.1626653494639));
#76764=CARTESIAN_POINT('Ctrl Pts',(1.10878693579106,2.52576163259184,11.199387935191));
#76765=CARTESIAN_POINT('Ctrl Pts',(0.638505315593813,3.09994605928972,11.2360689579805));
#76766=CARTESIAN_POINT('Ctrl Pts',(0.000388937624618915,3.26127843969028,
11.2686352489648));
#76767=CARTESIAN_POINT('Ctrl Pts',(-0.537295130790837,3.10515441545699,
11.2970961241536));
#76768=CARTESIAN_POINT('Ctrl Pts',(-0.902326569558736,2.79504264556167,
11.321466686552));
#76769=CARTESIAN_POINT('Ctrl Pts',(-1.10702206613895,2.36207264168374,11.3458150885241));
#76770=CARTESIAN_POINT('Ctrl Pts',(-1.11582534620937,1.88404100367201,11.3701349236063));
#76771=CARTESIAN_POINT('Ctrl Pts',(-0.92714626992851,1.44502786548751,11.3944306657383));
#76772=CARTESIAN_POINT('Ctrl Pts',(-0.575234030805921,1.12296279796943,
11.4186966137304));
#76773=CARTESIAN_POINT('Ctrl Pts',(-0.122301439670659,0.974089924588524,
11.4429344521201));
#76774=CARTESIAN_POINT('Ctrl Pts',(0.350698910575724,1.02504698840166,11.4671397665887));
#76775=CARTESIAN_POINT('Ctrl Pts',(0.829626204585101,1.30502543792218,11.4953420353212));
#76776=CARTESIAN_POINT('Ctrl Pts',(1.14797444119283,1.87226857357097,11.5275224305495));
#76777=CARTESIAN_POINT('Ctrl Pts',(1.05633168246765,2.59750084748831,11.5636455196149));
#76778=CARTESIAN_POINT('Ctrl Pts',(0.553638646075477,3.1250179729032,11.5996873965931));
#76779=CARTESIAN_POINT('Ctrl Pts',(-0.162948539643825,3.25108529062911,
11.6356449906589));
#76780=CARTESIAN_POINT('Ctrl Pts',(-0.811875649077865,2.92712517435771,
11.6715113968855));
#76781=CARTESIAN_POINT('Ctrl Pts',(-1.14156475071156,2.28295218061495,11.7072878404216));
#76782=CARTESIAN_POINT('Ctrl Pts',(-1.02457300660032,1.57095426196459,11.7429684336749));
#76783=CARTESIAN_POINT('Ctrl Pts',(-0.50896482368733,1.06845768586892,11.7785514654893));
#76784=CARTESIAN_POINT('Ctrl Pts',(0.201950061013787,0.971635667064493,
11.8140308939266));
#76785=CARTESIAN_POINT('Ctrl Pts',(0.830092077866532,1.31418559574247,11.8494070790025));
#76786=CARTESIAN_POINT('Ctrl Pts',(1.13102929259564,1.96096587182398,11.8846756079773));
#76787=CARTESIAN_POINT('Ctrl Pts',(0.989640144721045,2.65772453000089,11.9198339961118));
#76788=CARTESIAN_POINT('Ctrl Pts',(0.463528782418964,3.13318244291783,11.9548794729567));
#76789=CARTESIAN_POINT('Ctrl Pts',(-0.180643818085227,3.19657377969004,
11.9868989323603));
#76790=CARTESIAN_POINT('Ctrl Pts',(-0.695759946330833,2.94245729787198,
12.0159212297607));
#76791=CARTESIAN_POINT('Ctrl Pts',(-1.00225603443216,2.52836906250513,12.0419741998133));
#76792=CARTESIAN_POINT('Ctrl Pts',(-1.0841398197529,2.02076436880105,12.067959038582));
#76793=CARTESIAN_POINT('Ctrl Pts',(-0.924413211899146,1.53365759447729,
12.0938749146687));
#76794=CARTESIAN_POINT('Ctrl Pts',(-0.559890490376635,1.17509145179636,
12.1197209721359));
#76795=CARTESIAN_POINT('Ctrl Pts',(-0.072807828290282,1.02427278181782,
12.1454964045519));
#76796=CARTESIAN_POINT('Ctrl Pts',(0.427779769373155,1.11357160449807,12.1712004795833));
#76797=CARTESIAN_POINT('Ctrl Pts',(0.830406625455885,1.42180327791402,12.1968324522623));
#76798=CARTESIAN_POINT('Ctrl Pts',(1.04604179276681,1.87914271463228,12.2223917784092));
#76799=CARTESIAN_POINT('Ctrl Pts',(1.0277660461579,2.38298464567033,12.2478776032662));
#76800=CARTESIAN_POINT('Ctrl Pts',(0.781008026681809,2.8209661818624,12.2732899139927));
#76801=CARTESIAN_POINT('Ctrl Pts',(0.361964742171805,3.09601225930596,12.2986269545876));
#76802=CARTESIAN_POINT('Ctrl Pts',(-0.135051905121615,3.14792186037528,
12.3238910279141));
#76803=CARTESIAN_POINT('Ctrl Pts',(-0.599169179978984,2.96639048631031,
12.3490755266133));
#76804=CARTESIAN_POINT('Ctrl Pts',(-0.872329085896608,2.65555401105702,
12.3700076951713));
#76805=CARTESIAN_POINT('Ctrl Pts',(-0.987186930662794,2.35280215564241,
12.3867018682132));
#76806=CARTESIAN_POINT('Ctrl Pts',(-1.00734475680216,2.1938536174253,12.3950458365239));
#76807=CARTESIAN_POINT('Ctrl Pts',(-1.00792254912715,2.11275466044563,12.399218420322));
#76808=CARTESIAN_POINT('Ctrl Pts',(0.91151736992197,2.1,9.42670848231352));
#76809=CARTESIAN_POINT('Ctrl Pts',(0.911823420998916,2.17362491053193,9.43048908397653));
#76810=CARTESIAN_POINT('Ctrl Pts',(0.895347124119438,2.31730678590831,9.43801854237646));
#76811=CARTESIAN_POINT('Ctrl Pts',(0.794579867967047,2.59257652833862,9.45313636445175));
#76812=CARTESIAN_POINT('Ctrl Pts',(0.550963083297487,2.87631544921428,9.47204749845912));
#76813=CARTESIAN_POINT('Ctrl Pts',(0.133338376315858,3.04534834085169,9.49481696675561));
#76814=CARTESIAN_POINT('Ctrl Pts',(-0.316337071035398,3.00360019165658,
9.51764429868788));
#76815=CARTESIAN_POINT('Ctrl Pts',(-0.697852287982864,2.75946460258789,
9.54053895344277));
#76816=CARTESIAN_POINT('Ctrl Pts',(-0.92536205909537,2.36630063622663,9.56349815370946));
#76817=CARTESIAN_POINT('Ctrl Pts',(-0.947113368346999,1.91126111235727,
9.58652454997213));
#76818=CARTESIAN_POINT('Ctrl Pts',(-0.757015060211982,1.49578039572229,
9.60961831114713));
#76819=CARTESIAN_POINT('Ctrl Pts',(-0.396358747913306,1.21306670653134,
9.63278064943303));
#76820=CARTESIAN_POINT('Ctrl Pts',(0.0551732428288623,1.12718000131706,
9.65601225612881));
#76821=CARTESIAN_POINT('Ctrl Pts',(0.49708518307227,1.25850738740212,9.67931399514674));
#76822=CARTESIAN_POINT('Ctrl Pts',(0.830423146364994,1.57902226351323,9.70268662125709));
#76823=CARTESIAN_POINT('Ctrl Pts',(0.979930563037809,2.01805620160245,9.72613085605719));
#76824=CARTESIAN_POINT('Ctrl Pts',(0.910998864375581,2.47830509041408,9.7496474409599));
#76825=CARTESIAN_POINT('Ctrl Pts',(0.637734783618045,2.85640303606092,9.77323687378395));
#76826=CARTESIAN_POINT('Ctrl Pts',(0.173523797700195,3.09187348306677,9.79952935747188));
#76827=CARTESIAN_POINT('Ctrl Pts',(-0.410880580350844,3.0410434612312,9.82855484641837));
#76828=CARTESIAN_POINT('Ctrl Pts',(-0.893848108644005,2.61486947154893,
9.86035120685577));
#76829=CARTESIAN_POINT('Ctrl Pts',(-1.00564790149701,2.08885706686107,9.88696162003044));
#76830=CARTESIAN_POINT('Ctrl Pts',(-0.895641403689991,1.68759787522274,
9.90831870119292));
#76831=CARTESIAN_POINT('Ctrl Pts',(-0.723619481364688,1.42668451757006,
9.92436981039727));
#76832=CARTESIAN_POINT('Ctrl Pts',(-0.477850636379282,1.23267673421399,
9.94045464349453));
#76833=CARTESIAN_POINT('Ctrl Pts',(-0.0848771837976218,1.08780369054343,
9.96194746341766));
#76834=CARTESIAN_POINT('Ctrl Pts',(0.383154730739405,1.14683810870481,9.98529839642391));
#76835=CARTESIAN_POINT('Ctrl Pts',(0.776637852479867,1.45010231186482,10.0105410364593));
#76836=CARTESIAN_POINT('Ctrl Pts',(0.977937556035125,1.82603682057697,10.0322382469778));
#76837=CARTESIAN_POINT('Ctrl Pts',(1.00444635088653,2.2175629630189,10.0521814854967));
#76838=CARTESIAN_POINT('Ctrl Pts',(0.898438243730871,2.55509140919191,10.0703571117377));
#76839=CARTESIAN_POINT('Ctrl Pts',(0.651244318262303,2.90177081482339,10.0922139208646));
#76840=CARTESIAN_POINT('Ctrl Pts',(0.158339685169272,3.15464181054521,10.1196160727346));
#76841=CARTESIAN_POINT('Ctrl Pts',(-0.501122892267541,3.04634299070764,
10.1526379701481));
#76842=CARTESIAN_POINT('Ctrl Pts',(-0.969070720895698,2.56593515914924,
10.1857954825801));
#76843=CARTESIAN_POINT('Ctrl Pts',(-1.06071133600343,1.8985992051744,10.2190895515771));
#76844=CARTESIAN_POINT('Ctrl Pts',(-0.736953419031971,1.30502857084314,
10.2525184902282));
#76845=CARTESIAN_POINT('Ctrl Pts',(-0.121148835224608,1.01827893534673,
10.2860825462925));
#76846=CARTESIAN_POINT('Ctrl Pts',(0.47221947385328,1.13929533837934,10.3160345510646));
#76847=CARTESIAN_POINT('Ctrl Pts',(0.857163625188424,1.48504003896708,10.342331316347));
#76848=CARTESIAN_POINT('Ctrl Pts',(1.03707230738368,1.89123285220792,10.3649291186041));
#76849=CARTESIAN_POINT('Ctrl Pts',(1.03371636024308,2.33683112285088,10.3875856008764));
#76850=CARTESIAN_POINT('Ctrl Pts',(0.847165070768552,2.74276914283382,10.4103006996458));
#76851=CARTESIAN_POINT('Ctrl Pts',(0.509096081609499,3.03621370669456,10.4330730167258));
#76852=CARTESIAN_POINT('Ctrl Pts',(0.00747313066928684,3.18768097202426,
10.4597069040333));
#76853=CARTESIAN_POINT('Ctrl Pts',(-0.592445775936991,3.04278169853641,
10.4902356001833));
#76854=CARTESIAN_POINT('Ctrl Pts',(-1.04079931784978,2.50841253236762,10.5247114910065));
#76855=CARTESIAN_POINT('Ctrl Pts',(-1.08338436932414,1.80968101920642,10.5593052753001));
#76856=CARTESIAN_POINT('Ctrl Pts',(-0.70198015959148,1.22024016156732,10.5940225156454));
#76857=CARTESIAN_POINT('Ctrl Pts',(-0.0422454376537824,0.971372674300962,
10.6288588284583));
#76858=CARTESIAN_POINT('Ctrl Pts',(0.562108044450436,1.14276665195793,10.6599259800063));
#76859=CARTESIAN_POINT('Ctrl Pts',(0.933125339905673,1.53006298438199,10.6871887581118));
#76860=CARTESIAN_POINT('Ctrl Pts',(1.06188618556298,1.89141140995871,10.7067031606361));
#76861=CARTESIAN_POINT('Ctrl Pts',(1.06861205324963,2.19370567757229,10.7223396178189));
#76862=CARTESIAN_POINT('Ctrl Pts',(1.00304025429932,2.54085849191131,10.7406013583902));
#76863=CARTESIAN_POINT('Ctrl Pts',(0.78883783544409,2.86897570776504,10.760201975507));
#76864=CARTESIAN_POINT('Ctrl Pts',(0.403053119117575,3.11584641273972,10.7837746681186));
#76865=CARTESIAN_POINT('Ctrl Pts',(0.000362036933634016,3.20485996514675,
10.8047589130325));
#76866=CARTESIAN_POINT('Ctrl Pts',(-0.455152490817227,3.10924210303583,
10.8284161801311));
#76867=CARTESIAN_POINT('Ctrl Pts',(-0.831125997851916,2.83422752561369,
10.8521153778398));
#76868=CARTESIAN_POINT('Ctrl Pts',(-1.10072731360356,2.36050560413651,10.8798183647944));
#76869=CARTESIAN_POINT('Ctrl Pts',(-1.09252964318303,1.71909233641417,10.9115478665288));
#76870=CARTESIAN_POINT('Ctrl Pts',(-0.654361811393719,1.14228170583733,
10.9473395695622));
#76871=CARTESIAN_POINT('Ctrl Pts',(0.0420042139168913,0.937977236263047,
10.983221779786));
#76872=CARTESIAN_POINT('Ctrl Pts',(0.725507027710317,1.18765705960442,11.0191917529181));
#76873=CARTESIAN_POINT('Ctrl Pts',(1.12796260215576,1.79594785111174,11.055245666088));
#76874=CARTESIAN_POINT('Ctrl Pts',(1.09061376681782,2.52577506847939,11.0913797672831));
#76875=CARTESIAN_POINT('Ctrl Pts',(0.625902914242613,3.09240832046028,11.1275906675829));
#76876=CARTESIAN_POINT('Ctrl Pts',(-0.00630633598939572,3.25178721005664,
11.1598420116462));
#76877=CARTESIAN_POINT('Ctrl Pts',(-0.540240864569795,3.09619033576691,
11.1881081914955));
#76878=CARTESIAN_POINT('Ctrl Pts',(-0.903308708901617,2.78712934837545,
11.2123665462451));
#76879=CARTESIAN_POINT('Ctrl Pts',(-1.10707609254612,2.35500603102821,11.2366515647841));
#76880=CARTESIAN_POINT('Ctrl Pts',(-1.11540058169363,1.87706321585021,11.2609655395252));
#76881=CARTESIAN_POINT('Ctrl Pts',(-0.925908271596444,1.43740578510329,
11.285303445506));
#76882=CARTESIAN_POINT('Ctrl Pts',(-0.572210730312777,1.11438275513905,
11.309667110669));
#76883=CARTESIAN_POINT('Ctrl Pts',(-0.116275510175771,0.965056470550933,
11.3340534145616));
#76884=CARTESIAN_POINT('Ctrl Pts',(0.360700243291035,1.01696185361064,11.3584631352109));
#76885=CARTESIAN_POINT('Ctrl Pts',(0.844446227881871,1.30044236766626,11.3869657989611));
#76886=CARTESIAN_POINT('Ctrl Pts',(1.16657608619672,1.87553441489441,11.4195706490173));
#76887=CARTESIAN_POINT('Ctrl Pts',(1.07280974558895,2.61279947948096,11.4562923059314));
#76888=CARTESIAN_POINT('Ctrl Pts',(0.55961199987561,3.15041796179706,11.4930495823791));
#76889=CARTESIAN_POINT('Ctrl Pts',(-0.173736551317003,3.27879187689283,
11.5298376714367));
#76890=CARTESIAN_POINT('Ctrl Pts',(-0.839605484416093,2.94563868032413,
11.5666541180967));
#76891=CARTESIAN_POINT('Ctrl Pts',(-1.17851839519367,2.28198286935752,11.603492067794));
#76892=CARTESIAN_POINT('Ctrl Pts',(-1.0569823061534,1.54658256971973,11.640348201911));
#76893=CARTESIAN_POINT('Ctrl Pts',(-0.522199558365981,1.02637377533744,
11.6772175075259));
#76894=CARTESIAN_POINT('Ctrl Pts',(0.216893871560646,0.926443560152882,
11.7140965345869));
#76895=CARTESIAN_POINT('Ctrl Pts',(0.871476025423946,1.28425104909088,11.7509795818237));
#76896=CARTESIAN_POINT('Ctrl Pts',(1.18551994913662,1.96099154468725,11.787862507617));
#76897=CARTESIAN_POINT('Ctrl Pts',(1.03644815019712,2.69171293013048,11.824740942292));
#76898=CARTESIAN_POINT('Ctrl Pts',(0.482409520039158,3.19134922941584,11.8616103433384));
#76899=CARTESIAN_POINT('Ctrl Pts',(-0.197372192715649,3.25749187034555,
11.8953948352799));
#76900=CARTESIAN_POINT('Ctrl Pts',(-0.741930590032224,2.98797239484732,
11.926094816338));
#76901=CARTESIAN_POINT('Ctrl Pts',(-1.06625417361505,2.54857764239091,11.9537127158612));
#76902=CARTESIAN_POINT('Ctrl Pts',(-1.15252001058213,2.00922868658725,11.9813166994033));
#76903=CARTESIAN_POINT('Ctrl Pts',(-0.981783734819453,1.49092372364447,
12.008904888169));
#76904=CARTESIAN_POINT('Ctrl Pts',(-0.592420461199662,1.10897317214394,
12.036475439748));
#76905=CARTESIAN_POINT('Ctrl Pts',(-0.071571264224261,0.948492450725194,
12.0640264518274));
#76906=CARTESIAN_POINT('Ctrl Pts',(0.464419135236049,1.04488560113194,12.091556134534));
#76907=CARTESIAN_POINT('Ctrl Pts',(0.89600235444067,1.37626327825661,12.1190625678794));
#76908=CARTESIAN_POINT('Ctrl Pts',(1.12713249773057,1.86831043871101,12.1465442073483));
#76909=CARTESIAN_POINT('Ctrl Pts',(1.10664927335543,2.41102174199376,12.1739987168217));
#76910=CARTESIAN_POINT('Ctrl Pts',(0.839640517933186,2.88329040026059,12.2014255755425));
#76911=CARTESIAN_POINT('Ctrl Pts',(0.386132852406335,3.17999397807018,12.2288202203781));
#76912=CARTESIAN_POINT('Ctrl Pts',(-0.152290410197637,3.23536449519144,
12.2561871890178));
#76913=CARTESIAN_POINT('Ctrl Pts',(-0.655550821832348,3.03769445607198,
12.2835107392738));
#76914=CARTESIAN_POINT('Ctrl Pts',(-0.951961764434413,2.69925795049044,
12.3062694694656));
#76915=CARTESIAN_POINT('Ctrl Pts',(-1.07634979864707,2.36980477421791,12.3244258281199));
#76916=CARTESIAN_POINT('Ctrl Pts',(-1.09803441854211,2.1963840236327,12.3335275999414));
#76917=CARTESIAN_POINT('Ctrl Pts',(-1.09851387392196,2.10832492681077,12.3380569618133));
#76918=CARTESIAN_POINT('Ctrl Pts',(0.88,2.1,9.49208807696239));
#76919=CARTESIAN_POINT('Ctrl Pts',(0.88004530066288,2.17110443853451,9.49574149503588));
#76920=CARTESIAN_POINT('Ctrl Pts',(0.863615235646394,2.30953923705568,9.50300212441786));
#76921=CARTESIAN_POINT('Ctrl Pts',(0.765462544235921,2.57462340525805,9.51758083803204));
#76922=CARTESIAN_POINT('Ctrl Pts',(0.529819591157008,2.84681044164821,9.5357938837476));
#76923=CARTESIAN_POINT('Ctrl Pts',(0.12778461713841,3.00776193746932,9.55768645918373));
#76924=CARTESIAN_POINT('Ctrl Pts',(-0.303559189553242,2.96604809729294,
9.57959800515177));
#76925=CARTESIAN_POINT('Ctrl Pts',(-0.668168144789344,2.7308027674258,9.60153880818797));
#76926=CARTESIAN_POINT('Ctrl Pts',(-0.884366875518534,2.35394413226399,
9.62350665193357));
#76927=CARTESIAN_POINT('Ctrl Pts',(-0.90352025454572,1.91932181682493,9.6455048808308));
#76928=CARTESIAN_POINT('Ctrl Pts',(-0.72078437125489,1.52382494797329,9.66753430657136));
#76929=CARTESIAN_POINT('Ctrl Pts',(-0.376394911298066,1.25592019629859,
9.68959681841591));
#76930=CARTESIAN_POINT('Ctrl Pts',(0.0532124427449469,1.17584944736387,
9.71169377532346));
#76931=CARTESIAN_POINT('Ctrl Pts',(0.472332248812248,1.30208619516318,9.73382675522453));
#76932=CARTESIAN_POINT('Ctrl Pts',(0.787286422179607,1.60715424951494,9.75599718708746));
#76933=CARTESIAN_POINT('Ctrl Pts',(0.927347587472474,2.02341832269235,9.77820662437522));
#76934=CARTESIAN_POINT('Ctrl Pts',(0.860575112492045,2.4584680844061,9.80045633596402));
#76935=CARTESIAN_POINT('Ctrl Pts',(0.601155266029929,2.81469328323033,9.82274803545432));
#76936=CARTESIAN_POINT('Ctrl Pts',(0.162372489010935,3.0352765216471,9.84756385390868));
#76937=CARTESIAN_POINT('Ctrl Pts',(-0.388150801165923,2.98535810090146,
9.87492859407763));
#76938=CARTESIAN_POINT('Ctrl Pts',(-0.841141613414809,2.58266182781169,
9.90486455365364));
#76939=CARTESIAN_POINT('Ctrl Pts',(-0.944423152013141,2.08801695854391,
9.92987876914174));
#76940=CARTESIAN_POINT('Ctrl Pts',(-0.839850650288727,1.71170647032559,
9.94993165014419));
#76941=CARTESIAN_POINT('Ctrl Pts',(-0.677623291964419,1.46747623780434,
9.96499472728963));
#76942=CARTESIAN_POINT('Ctrl Pts',(-0.44655290394383,1.28636379874863,9.98008084963806));
#76943=CARTESIAN_POINT('Ctrl Pts',(-0.0778471165786419,1.15186841586681,
10.0002245579097));
#76944=CARTESIAN_POINT('Ctrl Pts',(0.360306690446967,1.20869984432036,10.0221099156808));
#76945=CARTESIAN_POINT('Ctrl Pts',(0.727434680359908,1.49366178825316,10.0457287929528));
#76946=CARTESIAN_POINT('Ctrl Pts',(0.914446196367802,1.84575615010426,10.0660175354139));
#76947=CARTESIAN_POINT('Ctrl Pts',(0.937977426449006,2.21168850001371,10.0846590915643));
#76948=CARTESIAN_POINT('Ctrl Pts',(0.837928158967066,2.52657011588598,10.1016371890881));
#76949=CARTESIAN_POINT('Ctrl Pts',(0.606093172372672,2.84942473726904,10.122044518861));
#76950=CARTESIAN_POINT('Ctrl Pts',(0.145376230198328,3.08381718275388,10.147626054432));
#76951=CARTESIAN_POINT('Ctrl Pts',(-0.46914671489129,2.98076716295159,10.1784259790307));
#76952=CARTESIAN_POINT('Ctrl Pts',(-0.903690880659961,2.53167055598801,
10.2093356131282));
#76953=CARTESIAN_POINT('Ctrl Pts',(-0.986972114311235,1.90988467649814,
10.2403547285203));
#76954=CARTESIAN_POINT('Ctrl Pts',(-0.683752522804138,1.35832101547673,
10.2714868311644));
#76955=CARTESIAN_POINT('Ctrl Pts',(-0.109813487751821,1.09335411156601,
10.3027322600927));
#76956=CARTESIAN_POINT('Ctrl Pts',(0.441878190810725,1.20774702806893,10.3306109818244));
#76957=CARTESIAN_POINT('Ctrl Pts',(0.798907968654179,1.53050023949423,10.3550769566962));
#76958=CARTESIAN_POINT('Ctrl Pts',(0.965032703288519,1.90884357252065,10.3761014912007));
#76959=CARTESIAN_POINT('Ctrl Pts',(0.960597360585514,2.323268162612,10.3971783739586));
#76960=CARTESIAN_POINT('Ctrl Pts',(0.785897643856786,2.70024077531878,10.4183074156142));
#76961=CARTESIAN_POINT('Ctrl Pts',(0.470625209333448,2.97216502173762,10.4394903861049));
#76962=CARTESIAN_POINT('Ctrl Pts',(0.00362841706809864,3.11156549341437,
10.4642669695311));
#76963=CARTESIAN_POINT('Ctrl Pts',(-0.554041350695444,2.97505278451906,
10.492678523291));
#76964=CARTESIAN_POINT('Ctrl Pts',(-0.969608931768246,2.47660542892771,
10.5247571910533));
#76965=CARTESIAN_POINT('Ctrl Pts',(-1.00726653710962,1.82619792265918,10.5569658388182));
#76966=CARTESIAN_POINT('Ctrl Pts',(-0.65050065906872,1.27853344965516,10.5892959338387));
#76967=CARTESIAN_POINT('Ctrl Pts',(-0.035343368509533,1.04859916693606,
10.6217508876492));
#76968=CARTESIAN_POINT('Ctrl Pts',(0.527368249504387,1.21002444550603,10.6507128983937));
#76969=CARTESIAN_POINT('Ctrl Pts',(0.872149475938407,1.57212693960115,10.6761311036372));
#76970=CARTESIAN_POINT('Ctrl Pts',(0.991208146851818,1.90950718557218,10.6943339612799));
#76971=CARTESIAN_POINT('Ctrl Pts',(0.996618420282601,2.19155347984175,10.7089238607875));
#76972=CARTESIAN_POINT('Ctrl Pts',(0.934433485677006,2.51531393887681,10.7259668475802));
#76973=CARTESIAN_POINT('Ctrl Pts',(0.733532233043949,2.8210729242721,10.7442719027377));
#76974=CARTESIAN_POINT('Ctrl Pts',(0.372500390277194,3.05055151027295,10.7662896596735));
#76975=CARTESIAN_POINT('Ctrl Pts',(-0.00407736089083116,3.13262070332373,
10.7859052812708));
#76976=CARTESIAN_POINT('Ctrl Pts',(-0.429697688628497,3.04193960479491,
10.808025020752));
#76977=CARTESIAN_POINT('Ctrl Pts',(-0.780690595728469,2.78360253048668,
10.8302023050984));
#76978=CARTESIAN_POINT('Ctrl Pts',(-1.0317479290845,2.33939629334436,10.8561382785999));
#76979=CARTESIAN_POINT('Ctrl Pts',(-1.02235302842942,1.73847951063121,10.8858727969815));
#76980=CARTESIAN_POINT('Ctrl Pts',(-0.609877440485562,1.19869136833044,
10.9194453166195));
#76981=CARTESIAN_POINT('Ctrl Pts',(0.0444562651571831,1.00873193799866,
10.9531396787437));
#76982=CARTESIAN_POINT('Ctrl Pts',(0.686241226456731,1.24523149613666,10.9869542078945));
#76983=CARTESIAN_POINT('Ctrl Pts',(1.06336671190863,1.81874075355131,11.0208880789452));
#76984=CARTESIAN_POINT('Ctrl Pts',(1.02624403939236,2.50632313928255,11.0549398755566));
#76985=CARTESIAN_POINT('Ctrl Pts',(0.586303974101457,3.03971411671832,11.0891082207085));
#76986=CARTESIAN_POINT('Ctrl Pts',(-0.0114201944887836,3.18863269329433,
11.1195823360316));
#76987=CARTESIAN_POINT('Ctrl Pts',(-0.516038343262635,3.0399955245707,11.1463206001162));
#76988=CARTESIAN_POINT('Ctrl Pts',(-0.858934951304874,2.74638434222921,
11.1692889561686));
#76989=CARTESIAN_POINT('Ctrl Pts',(-1.05087415829708,2.33628887027357,11.1923064654593));
#76990=CARTESIAN_POINT('Ctrl Pts',(-1.05745931905409,1.88285594553982,11.2153729875302));
#76991=CARTESIAN_POINT('Ctrl Pts',(-0.87630769190474,1.46584630314957,11.2384871521497));
#76992=CARTESIAN_POINT('Ctrl Pts',(-0.539183017509096,1.15973291652138,
11.2616491583461));
#76993=CARTESIAN_POINT('Ctrl Pts',(-0.104881518069885,1.018866539415,11.2848576413368));
#76994=CARTESIAN_POINT('Ctrl Pts',(0.349386797262332,1.06962249267029,11.3081130241157));
#76995=CARTESIAN_POINT('Ctrl Pts',(0.809972444245432,1.34130820500274,11.3352974299965));
#76996=CARTESIAN_POINT('Ctrl Pts',(1.11614064498991,1.89139132293948,11.3664379798849));
#76997=CARTESIAN_POINT('Ctrl Pts',(1.02453105287773,2.59650367918193,11.4015700842448));
#76998=CARTESIAN_POINT('Ctrl Pts',(0.531295143907132,3.11042556597401,11.4367980923007));
#76999=CARTESIAN_POINT('Ctrl Pts',(-0.173129048624275,3.2317907557564,11.4721176408173));
#77000=CARTESIAN_POINT('Ctrl Pts',(-0.812751586742188,2.90961035470477,
11.5075304282483));
#77001=CARTESIAN_POINT('Ctrl Pts',(-1.13763474000058,2.26920222604431,11.5430275630626));
#77002=CARTESIAN_POINT('Ctrl Pts',(-1.0183897866875,1.55950706457121,11.5786099463847));
#77003=CARTESIAN_POINT('Ctrl Pts',(-0.499742430458015,1.05767695948834,
11.6142714083728));
#77004=CARTESIAN_POINT('Ctrl Pts',(0.216875431514358,0.962745864867631,
11.6500148062663));
#77005=CARTESIAN_POINT('Ctrl Pts',(0.851628626733939,1.31191607717112,11.6858294674315));
#77006=CARTESIAN_POINT('Ctrl Pts',(1.15545700022636,1.97124830788862,11.721715748643));
#77007=CARTESIAN_POINT('Ctrl Pts',(1.00820496754727,2.68333851027724,11.7576694901916));
#77008=CARTESIAN_POINT('Ctrl Pts',(0.465592530984764,3.17005424157605,11.793687902103));
#77009=CARTESIAN_POINT('Ctrl Pts',(-0.200114414825182,3.23303114166232,
11.8267591746644));
#77010=CARTESIAN_POINT('Ctrl Pts',(-0.73349915290536,2.96717013530568,11.8568679625751));
#77011=CARTESIAN_POINT('Ctrl Pts',(-1.05088301096295,2.53462253501223,11.8839956498509));
#77012=CARTESIAN_POINT('Ctrl Pts',(-1.1342639661375,2.00370734901977,11.9111524047389));
#77013=CARTESIAN_POINT('Ctrl Pts',(-0.964560539044214,1.49340428201235,
11.9383363187367));
#77014=CARTESIAN_POINT('Ctrl Pts',(-0.579170342282215,1.11748888725573,
11.9655459647886));
#77015=CARTESIAN_POINT('Ctrl Pts',(-0.0637901249951442,0.960293629116356,
11.9927796193207));
#77016=CARTESIAN_POINT('Ctrl Pts',(0.466690930572303,1.05725236797281,12.0200357099596));
#77017=CARTESIAN_POINT('Ctrl Pts',(0.893812980941284,1.3871367670854,12.0473125059984));
#77018=CARTESIAN_POINT('Ctrl Pts',(1.12203809139043,1.87660228457252,12.074608533169));
#77019=CARTESIAN_POINT('Ctrl Pts',(1.10012614833113,2.41656001477662,12.1019217271321));
#77020=CARTESIAN_POINT('Ctrl Pts',(0.83268402875598,2.88648791750582,12.1292512722902));
#77021=CARTESIAN_POINT('Ctrl Pts',(0.379131566217826,3.18138175025283,12.1565934803869));
#77022=CARTESIAN_POINT('Ctrl Pts',(-0.159356724291243,3.23521048606865,
12.1839510331369));
#77023=CARTESIAN_POINT('Ctrl Pts',(-0.662789041493893,3.03578242415445,
12.211312326472));
#77024=CARTESIAN_POINT('Ctrl Pts',(-0.959078027836141,2.69544897818908,
12.2341338236766));
#77025=CARTESIAN_POINT('Ctrl Pts',(-1.08301523558641,2.36413115081123,12.2523724677113));
#77026=CARTESIAN_POINT('Ctrl Pts',(-1.10424709743569,2.18973503538251,12.2615198955416));
#77027=CARTESIAN_POINT('Ctrl Pts',(-1.10446356961415,2.10123734103367,12.2660694403094));
#77028=CARTESIAN_POINT('Ctrl Pts',(0.88,2.1,9.525));
#77029=CARTESIAN_POINT('Ctrl Pts',(0.879914606625585,2.17110785049955,9.52865476385635));
#77030=CARTESIAN_POINT('Ctrl Pts',(0.863232117186907,2.3095104036224,9.53591397312323));
#77031=CARTESIAN_POINT('Ctrl Pts',(0.7646146646842,2.57432753790838,9.55048599717583));
#77032=CARTESIAN_POINT('Ctrl Pts',(0.52875066403414,2.8457083400553,9.56867094599734));
#77033=CARTESIAN_POINT('Ctrl Pts',(0.127238756664634,3.00552936974926,9.59051359518968));
#77034=CARTESIAN_POINT('Ctrl Pts',(-0.302716205619033,2.96306288294985,
9.61235380295566));
#77035=CARTESIAN_POINT('Ctrl Pts',(-0.665427657999688,2.72799341501097,
9.63420407641812));
#77036=CARTESIAN_POINT('Ctrl Pts',(-0.879826065415376,2.3524940033895,9.65606121698024));
#77037=CARTESIAN_POINT('Ctrl Pts',(-0.89799221853441,1.92029343459682,9.67792905414005));
#77038=CARTESIAN_POINT('Ctrl Pts',(-0.715657796510551,1.52775201761214,
9.69980826165769));
#77039=CARTESIAN_POINT('Ctrl Pts',(-0.37329244035757,1.26252484692041,9.72170089413125));
#77040=CARTESIAN_POINT('Ctrl Pts',(0.0529042162174613,1.18397194405211,
9.7436083723133));
#77041=CARTESIAN_POINT('Ctrl Pts',(0.467926525737336,1.30987826775351,9.76553239226868));
#77042=CARTESIAN_POINT('Ctrl Pts',(0.77911594458734,1.61250328722602,9.78747453406851));
#77043=CARTESIAN_POINT('Ctrl Pts',(0.916833254715888,2.02450810034898,9.8094364412056));
#77044=CARTESIAN_POINT('Ctrl Pts',(0.84999015619955,2.45432327019144,9.83141968646686));
#77045=CARTESIAN_POINT('Ctrl Pts',(0.593134887517594,2.80556810401153,9.85342584950507));
#77046=CARTESIAN_POINT('Ctrl Pts',(0.159785468035136,3.02235194398505,9.87790429996245));
#77047=CARTESIAN_POINT('Ctrl Pts',(-0.382738476891779,2.97204316801605,
9.90486768286448));
#77048=CARTESIAN_POINT('Ctrl Pts',(-0.827943575417754,2.57464859578558,
9.93433214776037));
#77049=CARTESIAN_POINT('Ctrl Pts',(-0.928540642244484,2.0879125901631,9.95893043030863));
#77050=CARTESIAN_POINT('Ctrl Pts',(-0.82506221727755,1.71823863855703,9.97863755083128));
#77051=CARTESIAN_POINT('Ctrl Pts',(-0.665238898770628,1.47861418311032,
9.99343255715118));
#77052=CARTESIAN_POINT('Ctrl Pts',(-0.438025190317537,1.3012081221325,10.0082426633322));
#77053=CARTESIAN_POINT('Ctrl Pts',(-0.0759140953759721,1.16989403941721,
10.0280101634631));
#77054=CARTESIAN_POINT('Ctrl Pts',(0.353590617267489,1.22647296601624,10.0494595111079));
#77055=CARTESIAN_POINT('Ctrl Pts',(0.71282299611785,1.50640456177768,10.0726022736917));
#77056=CARTESIAN_POINT('Ctrl Pts',(0.895311256816217,1.85157831854142,10.0924697020734));
#77057=CARTESIAN_POINT('Ctrl Pts',(0.917661293713379,2.20976194577009,10.1107106042816));
#77058=CARTESIAN_POINT('Ctrl Pts',(0.819212469046223,2.51761130734418,10.127317066638));
#77059=CARTESIAN_POINT('Ctrl Pts',(0.591924394917487,2.83289082559773,10.1472698428113));
#77060=CARTESIAN_POINT('Ctrl Pts',(0.141288805504938,3.06103897732418,10.172258699084));
#77061=CARTESIAN_POINT('Ctrl Pts',(-0.458527011040082,2.95925151709148,
10.2023249565719));
#77062=CARTESIAN_POINT('Ctrl Pts',(-0.88162766536303,2.52027411449529,10.2324736532743));
#77063=CARTESIAN_POINT('Ctrl Pts',(-0.961653185964405,1.91393657438503,
10.2627077273853));
#77064=CARTESIAN_POINT('Ctrl Pts',(-0.665231767857691,1.37715957803001,
10.2930297792945));
#77065=CARTESIAN_POINT('Ctrl Pts',(-0.105988685338195,1.12026073865136,
10.3234425669733));
#77066=CARTESIAN_POINT('Ctrl Pts',(0.430538820721984,1.23255710504194,10.3505590141325));
#77067=CARTESIAN_POINT('Ctrl Pts',(0.777157271318668,1.54704609431923,10.3743479205533));
#77068=CARTESIAN_POINT('Ctrl Pts',(0.937973646848606,1.91510656924282,10.3947816504623));
#77069=CARTESIAN_POINT('Ctrl Pts',(0.932931736507626,2.31778957988939,10.4152592321293));
#77070=CARTESIAN_POINT('Ctrl Pts',(0.762578582228501,2.68366310973811,10.4357813746755));
#77071=CARTESIAN_POINT('Ctrl Pts',(0.455963235969408,2.94715653506223,10.4563486739678));
#77072=CARTESIAN_POINT('Ctrl Pts',(0.00240142086611935,3.08166579400621,
10.480397254692));
#77073=CARTESIAN_POINT('Ctrl Pts',(-0.538455390507358,2.94820992747045,
10.5079586157699));
#77074=CARTESIAN_POINT('Ctrl Pts',(-0.940666416691817,2.46401744657124,
10.5390713811047));
#77075=CARTESIAN_POINT('Ctrl Pts',(-0.976029443563649,1.83335883304997,
10.5702921359498));
#77076=CARTESIAN_POINT('Ctrl Pts',(-0.629306856593687,1.30317046301086,
10.6016225477596));
#77077=CARTESIAN_POINT('Ctrl Pts',(-0.0328763589810331,1.08144514613719,
10.6330641573791));
#77078=CARTESIAN_POINT('Ctrl Pts',(0.511901871764286,1.23876013099839,10.6611123163153));
#77079=CARTESIAN_POINT('Ctrl Pts',(0.845208777494887,1.59002857501027,10.6857282761483));
#77080=CARTESIAN_POINT('Ctrl Pts',(0.959937391714928,1.91692164410815,10.7033535735637));
#77081=CARTESIAN_POINT('Ctrl Pts',(0.964709509971458,2.19002072343591,10.7174794574177));
#77082=CARTESIAN_POINT('Ctrl Pts',(0.903969607200192,2.50338072207659,10.7339796596208));
#77083=CARTESIAN_POINT('Ctrl Pts',(0.708976511873778,2.79903473649909,10.7516978643424));
#77084=CARTESIAN_POINT('Ctrl Pts',(0.359111666410103,3.02058677865832,10.7730116718645));
#77085=CARTESIAN_POINT('Ctrl Pts',(-0.0055195068732309,3.09939687665217,
10.7919958841582));
#77086=CARTESIAN_POINT('Ctrl Pts',(-0.417331250225881,3.01093271757532,
10.8134054790171));
#77087=CARTESIAN_POINT('Ctrl Pts',(-0.756608961158023,2.76032613000462,
10.8348676292604));
#77088=CARTESIAN_POINT('Ctrl Pts',(-0.998865593098056,2.33000290793379,
10.8599683150449));
#77089=CARTESIAN_POINT('Ctrl Pts',(-0.988791187924089,1.74845036869023,
10.8887429491342));
#77090=CARTESIAN_POINT('Ctrl Pts',(-0.588714669350558,1.22669384301482,
10.9212338011637));
#77091=CARTESIAN_POINT('Ctrl Pts',(0.044909234496707,1.04388405761621,10.9538443040117));
#77092=CARTESIAN_POINT('Ctrl Pts',(0.665762350574508,1.27382859359802,10.9865746011287));
#77093=CARTESIAN_POINT('Ctrl Pts',(1.02994927065475,1.82963242200099,11.0194247010519));
#77094=CARTESIAN_POINT('Ctrl Pts',(0.99292771913683,2.49532007970257,11.0523944801788));
#77095=CARTESIAN_POINT('Ctrl Pts',(0.566047404042377,3.01118540039736,11.0854836852924));
#77096=CARTESIAN_POINT('Ctrl Pts',(-0.0131656805453273,3.1545072720966,
11.1150021335127));
#77097=CARTESIAN_POINT('Ctrl Pts',(-0.501834747536299,3.00971245930524,
11.1409075995603));
#77098=CARTESIAN_POINT('Ctrl Pts',(-0.833654637909307,2.72466132918788,
11.1631647757637));
#77099=CARTESIAN_POINT('Ctrl Pts',(-1.01904932840502,2.32688792491809,11.1854742337572));
#77100=CARTESIAN_POINT('Ctrl Pts',(-1.0247320303861,1.8873087550975,11.2078357472338));
#77101=CARTESIAN_POINT('Ctrl Pts',(-0.848433071641297,1.48323440703255,
11.2302490424206));
#77102=CARTESIAN_POINT('Ctrl Pts',(-0.5209916303453,1.18686010809674,11.2527138516101));
#77103=CARTESIAN_POINT('Ctrl Pts',(-0.0994474829318688,1.05086828612434,
11.2752298585268));
#77104=CARTESIAN_POINT('Ctrl Pts',(0.341286571712092,1.10081439784123,11.297796723956));
#77105=CARTESIAN_POINT('Ctrl Pts',(0.787934060544661,1.36522529701193,11.3241836591263));
#77106=CARTESIAN_POINT('Ctrl Pts',(1.08440822726537,1.89981767692546,11.3544236935599));
#77107=CARTESIAN_POINT('Ctrl Pts',(0.99437189083192,2.58466520846377,11.3885550724356));
#77108=CARTESIAN_POINT('Ctrl Pts',(0.51422832678732,3.08343949927552,11.4227963300144));
#77109=CARTESIAN_POINT('Ctrl Pts',(-0.170956362315584,3.20042729316684,
11.4571457685877));
#77110=CARTESIAN_POINT('Ctrl Pts',(-0.792809143568463,2.88603885152724,
11.49160167588));
#77111=CARTESIAN_POINT('Ctrl Pts',(-1.10815562220614,2.26212033857722,11.5261621918766));
#77112=CARTESIAN_POINT('Ctrl Pts',(-0.990980784814367,1.57098681332194,
11.5608252913622));
#77113=CARTESIAN_POINT('Ctrl Pts',(-0.484736723033935,1.08260154598769,
11.5955889188738));
#77114=CARTESIAN_POINT('Ctrl Pts',(0.214307763377102,0.991032096532327,
11.6304507824074));
#77115=CARTESIAN_POINT('Ctrl Pts',(0.833298379906107,1.33271197734595,11.6654086518246));
#77116=CARTESIAN_POINT('Ctrl Pts',(1.12908711130714,1.97705558535849,11.7004600148669));
#77117=CARTESIAN_POINT('Ctrl Pts',(0.984170425255086,2.67277304384029,11.7356024461146));
#77118=CARTESIAN_POINT('Ctrl Pts',(0.452808643636702,3.14802102155422,11.7708333087139));
#77119=CARTESIAN_POINT('Ctrl Pts',(-0.198836507924274,3.20872213800758,
11.8032068201948));
#77120=CARTESIAN_POINT('Ctrl Pts',(-0.720833985617695,2.9475724124579,11.8326976979388));
#77121=CARTESIAN_POINT('Ctrl Pts',(-1.03122512713103,2.52323917223077,11.8592848682016));
#77122=CARTESIAN_POINT('Ctrl Pts',(-1.11221371795246,2.00254397936835,11.8859162010712));
#77123=CARTESIAN_POINT('Ctrl Pts',(-0.944978677865563,1.50212478400673,
11.9125904181942));
#77124=CARTESIAN_POINT('Ctrl Pts',(-0.566096651435205,1.13364169683645,
11.9393062323883));
#77125=CARTESIAN_POINT('Ctrl Pts',(-0.0596069971212731,0.97996909355213,
11.966062281935));
#77126=CARTESIAN_POINT('Ctrl Pts',(0.461675051948685,1.07603593590851,11.9928572469173));
#77127=CARTESIAN_POINT('Ctrl Pts',(0.88129231323125,1.40110770643291,12.0196896905075));
#77128=CARTESIAN_POINT('Ctrl Pts',(1.10519737818586,1.88315811002375,12.0465583931276));
#77129=CARTESIAN_POINT('Ctrl Pts',(1.08283365883886,2.41488670097258,12.0734615789711));
#77130=CARTESIAN_POINT('Ctrl Pts',(0.818591168747924,2.87760074176854,12.100398642491));
#77131=CARTESIAN_POINT('Ctrl Pts',(0.370893737846914,3.16774776724325,12.1273662612715));
#77132=CARTESIAN_POINT('Ctrl Pts',(-0.160578831483255,3.22009488317826,
12.154367120808));
#77133=CARTESIAN_POINT('Ctrl Pts',(-0.657438304412148,3.02243699025829,
12.181390412703));
#77134=CARTESIAN_POINT('Ctrl Pts',(-0.949764066307816,2.68573447988004,
12.2039450357004));
#77135=CARTESIAN_POINT('Ctrl Pts',(-1.07182425162092,2.35796849387404,12.2219800536891));
#77136=CARTESIAN_POINT('Ctrl Pts',(-1.09256785760649,2.18550272007321,12.2310256553714));
#77137=CARTESIAN_POINT('Ctrl Pts',(-1.09265261173395,2.09796323888708,12.2355247810852));
#77138=CARTESIAN_POINT('',(0.88,2.1,9.525));
#77139=CARTESIAN_POINT('Ctrl Pts',(0.88,2.1,9.525));
#77140=CARTESIAN_POINT('Ctrl Pts',(0.88,2.1,9.52654752419537));
#77141=CARTESIAN_POINT('Ctrl Pts',(0.880034855304809,2.10000000001394,9.52809491473538));
#77142=CARTESIAN_POINT('Ctrl Pts',(0.880757639620712,2.10000000001394,9.54426404545797));
#77143=CARTESIAN_POINT('Ctrl Pts',(0.884474056104899,2.10000000001393,9.55873384801261));
#77144=CARTESIAN_POINT('Ctrl Pts',(0.896554877287777,2.10000000001393,9.58437291981711));
#77145=CARTESIAN_POINT('Ctrl Pts',(0.904632693604525,2.10000000001391,9.5957497323212));
#77146=CARTESIAN_POINT('Ctrl Pts',(0.926145942464148,2.10000000001391,9.61621866481436));
#77147=CARTESIAN_POINT('Ctrl Pts',(0.938680653436097,2.1000000000139,9.62308237886113));
#77148=CARTESIAN_POINT('Ctrl Pts',(0.963545489976373,2.1000000000139,9.63257445432811));
#77149=CARTESIAN_POINT('Ctrl Pts',(0.97799462547993,2.10000000001388,9.63514919539636));
#77150=CARTESIAN_POINT('Ctrl Pts',(1.00659276824775,2.10000000001388,9.6347066681337));
#77151=CARTESIAN_POINT('Ctrl Pts',(1.02034071065155,2.10000000001387,9.63174790532893));
#77152=CARTESIAN_POINT('Ctrl Pts',(1.04687463693244,2.10000000001387,9.62016351498204));
#77153=CARTESIAN_POINT('Ctrl Pts',(1.05918781850548,2.10000000001387,9.611590130133));
#77154=CARTESIAN_POINT('Ctrl Pts',(1.07740651951704,2.10000000001387,9.5928426732394));
#77155=CARTESIAN_POINT('Ctrl Pts',(1.08570485806481,2.10000000001386,9.58187096954533));
#77156=CARTESIAN_POINT('Ctrl Pts',(1.09719990931814,2.10000000001386,9.55415037431876));
#77157=CARTESIAN_POINT('Ctrl Pts',(1.09993578707158,2.10000000001386,9.53955469920238));
#77158=CARTESIAN_POINT('Ctrl Pts',(1.09986492944741,2.10000000001386,9.5103104176026));
#77159=CARTESIAN_POINT('Ctrl Pts',(1.0970064099584,2.10000000001386,9.49558664530564));
#77160=CARTESIAN_POINT('Ctrl Pts',(1.08515942970207,2.10000000001386,9.46742202035628));
#77161=CARTESIAN_POINT('Ctrl Pts',(1.07660754285019,2.10000000001387,9.45632598074318));
#77162=CARTESIAN_POINT('Ctrl Pts',(1.05826102775228,2.10000000001387,9.43763911093102));
#77163=CARTESIAN_POINT('Ctrl Pts',(1.04583977158587,2.10000000001387,9.42908030448567));
#77164=CARTESIAN_POINT('Ctrl Pts',(1.01700990292886,2.10000000001387,9.41681005498998));
#77165=CARTESIAN_POINT('Ctrl Pts',(1.00311689049416,2.10000000001388,9.41499747796185));
#77166=CARTESIAN_POINT('Ctrl Pts',(0.977374576676416,2.10000000001388,9.41483734650305));
#77167=CARTESIAN_POINT('Ctrl Pts',(0.963017667221115,2.1000000000139,9.41753459916267));
#77168=CARTESIAN_POINT('Ctrl Pts',(0.938227536233048,2.1000000000139,9.42720438574357));
#77169=CARTESIAN_POINT('Ctrl Pts',(0.925632691761865,2.10000000001391,9.43421015995138));
#77170=CARTESIAN_POINT('Ctrl Pts',(0.90406812267464,2.10000000001391,9.45502871027269));
#77171=CARTESIAN_POINT('Ctrl Pts',(0.896008094926436,2.10000000001392,9.46655439418273));
#77172=CARTESIAN_POINT('Ctrl Pts',(0.884146571951397,2.10000000001392,9.49234046373837));
#77173=CARTESIAN_POINT('Ctrl Pts',(0.88058305209276,2.10000000001394,9.50675642080951));
#77174=CARTESIAN_POINT('Ctrl Pts',(0.880021960842162,2.10000000001394,9.52254283629876));
#77175=CARTESIAN_POINT('Ctrl Pts',(0.88,2.1,9.52377137958177));
#77176=CARTESIAN_POINT('Ctrl Pts',(0.88,2.1,9.525));
#77177=CARTESIAN_POINT('',(-1.09265261173395,2.09796323888708,12.2355247810852));
#77178=CARTESIAN_POINT('Ctrl Pts',(0.88,2.1,9.525));
#77179=CARTESIAN_POINT('Ctrl Pts',(0.879914606625585,2.17110785049955,9.52865476385635));
#77180=CARTESIAN_POINT('Ctrl Pts',(0.863232117186907,2.3095104036224,9.53591397312323));
#77181=CARTESIAN_POINT('Ctrl Pts',(0.7646146646842,2.57432753790838,9.55048599717583));
#77182=CARTESIAN_POINT('Ctrl Pts',(0.52875066403414,2.8457083400553,9.56867094599734));
#77183=CARTESIAN_POINT('Ctrl Pts',(0.127238756664634,3.00552936974926,9.59051359518968));
#77184=CARTESIAN_POINT('Ctrl Pts',(-0.302716205619033,2.96306288294985,
9.61235380295566));
#77185=CARTESIAN_POINT('Ctrl Pts',(-0.665427657999688,2.72799341501097,
9.63420407641812));
#77186=CARTESIAN_POINT('Ctrl Pts',(-0.879826065415376,2.3524940033895,9.65606121698024));
#77187=CARTESIAN_POINT('Ctrl Pts',(-0.89799221853441,1.92029343459682,9.67792905414005));
#77188=CARTESIAN_POINT('Ctrl Pts',(-0.715657796510551,1.52775201761214,
9.69980826165769));
#77189=CARTESIAN_POINT('Ctrl Pts',(-0.37329244035757,1.26252484692041,9.72170089413125));
#77190=CARTESIAN_POINT('Ctrl Pts',(0.0529042162174613,1.18397194405211,
9.7436083723133));
#77191=CARTESIAN_POINT('Ctrl Pts',(0.467926525737336,1.30987826775351,9.76553239226868));
#77192=CARTESIAN_POINT('Ctrl Pts',(0.77911594458734,1.61250328722602,9.78747453406851));
#77193=CARTESIAN_POINT('Ctrl Pts',(0.916833254715888,2.02450810034898,9.8094364412056));
#77194=CARTESIAN_POINT('Ctrl Pts',(0.84999015619955,2.45432327019144,9.83141968646686));
#77195=CARTESIAN_POINT('Ctrl Pts',(0.593134887517594,2.80556810401153,9.85342584950507));
#77196=CARTESIAN_POINT('Ctrl Pts',(0.159785468035136,3.02235194398505,9.87790429996245));
#77197=CARTESIAN_POINT('Ctrl Pts',(-0.382738476891779,2.97204316801605,
9.90486768286448));
#77198=CARTESIAN_POINT('Ctrl Pts',(-0.827943575417754,2.57464859578558,
9.93433214776037));
#77199=CARTESIAN_POINT('Ctrl Pts',(-0.928540642244484,2.0879125901631,9.95893043030863));
#77200=CARTESIAN_POINT('Ctrl Pts',(-0.82506221727755,1.71823863855703,9.97863755083128));
#77201=CARTESIAN_POINT('Ctrl Pts',(-0.665238898770628,1.47861418311032,
9.99343255715118));
#77202=CARTESIAN_POINT('Ctrl Pts',(-0.438025190317537,1.3012081221325,10.0082426633322));
#77203=CARTESIAN_POINT('Ctrl Pts',(-0.0759140953759721,1.16989403941721,
10.0280101634631));
#77204=CARTESIAN_POINT('Ctrl Pts',(0.353590617267489,1.22647296601624,10.0494595111079));
#77205=CARTESIAN_POINT('Ctrl Pts',(0.71282299611785,1.50640456177768,10.0726022736917));
#77206=CARTESIAN_POINT('Ctrl Pts',(0.895311256816217,1.85157831854142,10.0924697020734));
#77207=CARTESIAN_POINT('Ctrl Pts',(0.917661293713379,2.20976194577009,10.1107106042816));
#77208=CARTESIAN_POINT('Ctrl Pts',(0.819212469046223,2.51761130734418,10.127317066638));
#77209=CARTESIAN_POINT('Ctrl Pts',(0.591924394917487,2.83289082559773,10.1472698428113));
#77210=CARTESIAN_POINT('Ctrl Pts',(0.141288805504938,3.06103897732418,10.172258699084));
#77211=CARTESIAN_POINT('Ctrl Pts',(-0.458527011040082,2.95925151709148,
10.2023249565719));
#77212=CARTESIAN_POINT('Ctrl Pts',(-0.88162766536303,2.52027411449529,10.2324736532743));
#77213=CARTESIAN_POINT('Ctrl Pts',(-0.961653185964405,1.91393657438503,
10.2627077273853));
#77214=CARTESIAN_POINT('Ctrl Pts',(-0.665231767857691,1.37715957803001,
10.2930297792945));
#77215=CARTESIAN_POINT('Ctrl Pts',(-0.105988685338195,1.12026073865136,
10.3234425669733));
#77216=CARTESIAN_POINT('Ctrl Pts',(0.430538820721984,1.23255710504194,10.3505590141325));
#77217=CARTESIAN_POINT('Ctrl Pts',(0.777157271318668,1.54704609431923,10.3743479205533));
#77218=CARTESIAN_POINT('Ctrl Pts',(0.937973646848606,1.91510656924282,10.3947816504623));
#77219=CARTESIAN_POINT('Ctrl Pts',(0.932931736507626,2.31778957988939,10.4152592321293));
#77220=CARTESIAN_POINT('Ctrl Pts',(0.762578582228501,2.68366310973811,10.4357813746755));
#77221=CARTESIAN_POINT('Ctrl Pts',(0.455963235969408,2.94715653506223,10.4563486739678));
#77222=CARTESIAN_POINT('Ctrl Pts',(0.00240142086611935,3.08166579400621,
10.480397254692));
#77223=CARTESIAN_POINT('Ctrl Pts',(-0.538455390507358,2.94820992747045,
10.5079586157699));
#77224=CARTESIAN_POINT('Ctrl Pts',(-0.940666416691817,2.46401744657124,
10.5390713811047));
#77225=CARTESIAN_POINT('Ctrl Pts',(-0.976029443563649,1.83335883304997,
10.5702921359498));
#77226=CARTESIAN_POINT('Ctrl Pts',(-0.629306856593687,1.30317046301086,
10.6016225477596));
#77227=CARTESIAN_POINT('Ctrl Pts',(-0.0328763589810331,1.08144514613719,
10.6330641573791));
#77228=CARTESIAN_POINT('Ctrl Pts',(0.511901871764286,1.23876013099839,10.6611123163153));
#77229=CARTESIAN_POINT('Ctrl Pts',(0.845208777494887,1.59002857501027,10.6857282761483));
#77230=CARTESIAN_POINT('Ctrl Pts',(0.959937391714928,1.91692164410815,10.7033535735637));
#77231=CARTESIAN_POINT('Ctrl Pts',(0.964709509971458,2.19002072343591,10.7174794574177));
#77232=CARTESIAN_POINT('Ctrl Pts',(0.903969607200192,2.50338072207659,10.7339796596208));
#77233=CARTESIAN_POINT('Ctrl Pts',(0.708976511873778,2.79903473649909,10.7516978643424));
#77234=CARTESIAN_POINT('Ctrl Pts',(0.359111666410103,3.02058677865832,10.7730116718645));
#77235=CARTESIAN_POINT('Ctrl Pts',(-0.0055195068732309,3.09939687665217,
10.7919958841582));
#77236=CARTESIAN_POINT('Ctrl Pts',(-0.417331250225881,3.01093271757532,
10.8134054790171));
#77237=CARTESIAN_POINT('Ctrl Pts',(-0.756608961158023,2.76032613000462,
10.8348676292604));
#77238=CARTESIAN_POINT('Ctrl Pts',(-0.998865593098056,2.33000290793379,
10.8599683150449));
#77239=CARTESIAN_POINT('Ctrl Pts',(-0.988791187924089,1.74845036869023,
10.8887429491342));
#77240=CARTESIAN_POINT('Ctrl Pts',(-0.588714669350558,1.22669384301482,
10.9212338011637));
#77241=CARTESIAN_POINT('Ctrl Pts',(0.044909234496707,1.04388405761621,10.9538443040117));
#77242=CARTESIAN_POINT('Ctrl Pts',(0.665762350574508,1.27382859359802,10.9865746011287));
#77243=CARTESIAN_POINT('Ctrl Pts',(1.02994927065475,1.82963242200099,11.0194247010519));
#77244=CARTESIAN_POINT('Ctrl Pts',(0.99292771913683,2.49532007970257,11.0523944801788));
#77245=CARTESIAN_POINT('Ctrl Pts',(0.566047404042377,3.01118540039736,11.0854836852924));
#77246=CARTESIAN_POINT('Ctrl Pts',(-0.0131656805453273,3.1545072720966,
11.1150021335127));
#77247=CARTESIAN_POINT('Ctrl Pts',(-0.501834747536299,3.00971245930524,
11.1409075995603));
#77248=CARTESIAN_POINT('Ctrl Pts',(-0.833654637909307,2.72466132918788,
11.1631647757637));
#77249=CARTESIAN_POINT('Ctrl Pts',(-1.01904932840502,2.32688792491809,11.1854742337572));
#77250=CARTESIAN_POINT('Ctrl Pts',(-1.0247320303861,1.8873087550975,11.2078357472338));
#77251=CARTESIAN_POINT('Ctrl Pts',(-0.848433071641297,1.48323440703255,
11.2302490424206));
#77252=CARTESIAN_POINT('Ctrl Pts',(-0.5209916303453,1.18686010809674,11.2527138516101));
#77253=CARTESIAN_POINT('Ctrl Pts',(-0.0994474829318688,1.05086828612434,
11.2752298585268));
#77254=CARTESIAN_POINT('Ctrl Pts',(0.341286571712092,1.10081439784123,11.297796723956));
#77255=CARTESIAN_POINT('Ctrl Pts',(0.787934060544661,1.36522529701193,11.3241836591263));
#77256=CARTESIAN_POINT('Ctrl Pts',(1.08440822726537,1.89981767692546,11.3544236935599));
#77257=CARTESIAN_POINT('Ctrl Pts',(0.99437189083192,2.58466520846377,11.3885550724356));
#77258=CARTESIAN_POINT('Ctrl Pts',(0.51422832678732,3.08343949927552,11.4227963300144));
#77259=CARTESIAN_POINT('Ctrl Pts',(-0.170956362315584,3.20042729316684,
11.4571457685877));
#77260=CARTESIAN_POINT('Ctrl Pts',(-0.792809143568463,2.88603885152724,
11.49160167588));
#77261=CARTESIAN_POINT('Ctrl Pts',(-1.10815562220614,2.26212033857722,11.5261621918766));
#77262=CARTESIAN_POINT('Ctrl Pts',(-0.990980784814367,1.57098681332194,
11.5608252913622));
#77263=CARTESIAN_POINT('Ctrl Pts',(-0.484736723033935,1.08260154598769,
11.5955889188738));
#77264=CARTESIAN_POINT('Ctrl Pts',(0.214307763377102,0.991032096532327,
11.6304507824074));
#77265=CARTESIAN_POINT('Ctrl Pts',(0.833298379906107,1.33271197734595,11.6654086518246));
#77266=CARTESIAN_POINT('Ctrl Pts',(1.12908711130714,1.97705558535849,11.7004600148669));
#77267=CARTESIAN_POINT('Ctrl Pts',(0.984170425255086,2.67277304384029,11.7356024461146));
#77268=CARTESIAN_POINT('Ctrl Pts',(0.452808643636702,3.14802102155422,11.7708333087139));
#77269=CARTESIAN_POINT('Ctrl Pts',(-0.198836507924274,3.20872213800758,
11.8032068201948));
#77270=CARTESIAN_POINT('Ctrl Pts',(-0.720833985617695,2.9475724124579,11.8326976979388));
#77271=CARTESIAN_POINT('Ctrl Pts',(-1.03122512713103,2.52323917223077,11.8592848682016));
#77272=CARTESIAN_POINT('Ctrl Pts',(-1.11221371795246,2.00254397936835,11.8859162010712));
#77273=CARTESIAN_POINT('Ctrl Pts',(-0.944978677865563,1.50212478400673,
11.9125904181942));
#77274=CARTESIAN_POINT('Ctrl Pts',(-0.566096651435205,1.13364169683645,
11.9393062323883));
#77275=CARTESIAN_POINT('Ctrl Pts',(-0.0596069971212731,0.97996909355213,
11.966062281935));
#77276=CARTESIAN_POINT('Ctrl Pts',(0.461675051948685,1.07603593590851,11.9928572469173));
#77277=CARTESIAN_POINT('Ctrl Pts',(0.88129231323125,1.40110770643291,12.0196896905075));
#77278=CARTESIAN_POINT('Ctrl Pts',(1.10519737818586,1.88315811002375,12.0465583931276));
#77279=CARTESIAN_POINT('Ctrl Pts',(1.08283365883886,2.41488670097258,12.0734615789711));
#77280=CARTESIAN_POINT('Ctrl Pts',(0.818591168747924,2.87760074176854,12.100398642491));
#77281=CARTESIAN_POINT('Ctrl Pts',(0.370893737846914,3.16774776724325,12.1273662612715));
#77282=CARTESIAN_POINT('Ctrl Pts',(-0.160578831483255,3.22009488317826,
12.154367120808));
#77283=CARTESIAN_POINT('Ctrl Pts',(-0.657438304412148,3.02243699025829,
12.181390412703));
#77284=CARTESIAN_POINT('Ctrl Pts',(-0.949764066307816,2.68573447988004,
12.2039450357004));
#77285=CARTESIAN_POINT('Ctrl Pts',(-1.07182425162092,2.35796849387404,12.2219800536891));
#77286=CARTESIAN_POINT('Ctrl Pts',(-1.09256785760649,2.18550272007321,12.2310256553714));
#77287=CARTESIAN_POINT('Ctrl Pts',(-1.09265261173395,2.09796323888708,12.2355247810852));
#77288=CARTESIAN_POINT('Ctrl Pts',(-1.09265261173395,2.09796323888708,12.2355247810852));
#77289=CARTESIAN_POINT('Ctrl Pts',(-1.09209725849391,2.09780929004959,12.2340885660349));
#77290=CARTESIAN_POINT('Ctrl Pts',(-1.09150942605389,2.09765599988943,12.2326649833975));
#77291=CARTESIAN_POINT('Ctrl Pts',(-1.08503237448485,2.09606086603517,12.217918236082));
#77292=CARTESIAN_POINT('Ctrl Pts',(-1.07637147919497,2.09469021271178,12.2058229006299));
#77293=CARTESIAN_POINT('Ctrl Pts',(-1.05589660811711,2.09236330772606,12.1863633679792));
#77294=CARTESIAN_POINT('Ctrl Pts',(-1.04427559806097,2.09138110303581,12.1787037088208));
#77295=CARTESIAN_POINT('Ctrl Pts',(-1.01685371830238,2.08974317821197,12.1674274156938));
#77296=CARTESIAN_POINT('Ctrl Pts',(-1.00269310527362,2.08929246375968,12.1655556665659));
#77297=CARTESIAN_POINT('Ctrl Pts',(-0.976082721926214,2.08880858272302,
12.1656694650394));
#77298=CARTESIAN_POINT('Ctrl Pts',(-0.961674722252946,2.08881998593982,
12.1684652160567));
#77299=CARTESIAN_POINT('Ctrl Pts',(-0.935145584204836,2.089393532376,12.1791388039753));
#77300=CARTESIAN_POINT('Ctrl Pts',(-0.923377726165856,2.08994242930189,
12.1868184150991));
#77301=CARTESIAN_POINT('Ctrl Pts',(-0.902773358098951,2.09158615536369,
12.2070916862902));
#77302=CARTESIAN_POINT('Ctrl Pts',(-0.894359321703738,2.09266703294608,
12.2194671888421));
#77303=CARTESIAN_POINT('Ctrl Pts',(-0.884085346464909,2.09486938130549,
12.2434042584418));
#77304=CARTESIAN_POINT('Ctrl Pts',(-0.880278658103152,2.09611450652452,
12.2565647862241));
#77305=CARTESIAN_POINT('Ctrl Pts',(-0.879499381119838,2.0990850140734,12.2864166942923));
#77306=CARTESIAN_POINT('Ctrl Pts',(-0.882184130880262,2.10058766003656,
12.3009443552539));
#77307=CARTESIAN_POINT('Ctrl Pts',(-0.892745023046883,2.10349559053314,
12.3280597480034));
#77308=CARTESIAN_POINT('Ctrl Pts',(-0.900696465100613,2.10490739378147,
12.3406986555977));
#77309=CARTESIAN_POINT('Ctrl Pts',(-0.921859448736967,2.10748987243997,
12.3625860027947));
#77310=CARTESIAN_POINT('Ctrl Pts',(-0.93382210431347,2.10843536774309,12.3698149566619));
#77311=CARTESIAN_POINT('Ctrl Pts',(-0.957649249474271,2.10995464694397,
12.3805737978547));
#77312=CARTESIAN_POINT('Ctrl Pts',(-0.972312296243169,2.11057609115668,
12.384059431092));
#77313=CARTESIAN_POINT('Ctrl Pts',(-1.00361986077531,2.11126293040044,12.3851010665202));
#77314=CARTESIAN_POINT('Ctrl Pts',(-1.0172353688322,2.11118600372854,12.3817975452729));
#77315=CARTESIAN_POINT('Ctrl Pts',(-1.04131570492226,2.11072528877995,12.3727081273419));
#77316=CARTESIAN_POINT('Ctrl Pts',(-1.05374570140234,2.11019113143425,12.3650526793176));
#77317=CARTESIAN_POINT('Ctrl Pts',(-1.0734098354843,2.10877015968504,12.3471820879167));
#77318=CARTESIAN_POINT('Ctrl Pts',(-1.08264928283733,2.10784001388133,12.3361603629656));
#77319=CARTESIAN_POINT('Ctrl Pts',(-1.095302396531,2.10536967950763,12.3091004509308));
#77320=CARTESIAN_POINT('Ctrl Pts',(-1.09868788747203,2.10407385649719,12.2955113107553));
#77321=CARTESIAN_POINT('Ctrl Pts',(-1.10050339267094,2.10128901138116,12.2673232691602));
#77322=CARTESIAN_POINT('Ctrl Pts',(-1.09865549775466,2.09978891927082,12.252665387318));
#77323=CARTESIAN_POINT('Ctrl Pts',(-1.09351390934533,2.09820808595437,12.2378130887736));
#77324=CARTESIAN_POINT('Ctrl Pts',(-1.09309352137022,2.09808546294386,12.2366650302271));
#77325=CARTESIAN_POINT('Ctrl Pts',(-1.09265261173395,2.09796323888708,12.2355247810852));
#77326=CARTESIAN_POINT('Origin',(-0.990000000000001,2.10000000000001,12.275));
#77327=CARTESIAN_POINT('Origin',(0.99,2.1,9.525));
#77328=CARTESIAN_POINT('',(0.,0.,0.));
#77329=CARTESIAN_POINT('Origin',(0.,0.,0.35));
#77330=CARTESIAN_POINT('',(-0.4,-4.89858719658941E-17,0.03));
#77331=CARTESIAN_POINT('Origin',(0.,0.,0.03));
#77332=CARTESIAN_POINT('',(-0.4,-4.89858719658941E-17,0.67));
#77333=CARTESIAN_POINT('',(-0.4,-4.89858719658941E-17,0.35));
#77334=CARTESIAN_POINT('Origin',(0.,0.,0.67));
#77335=CARTESIAN_POINT('Origin',(0.,0.,0.015));
#77336=CARTESIAN_POINT('',(-0.43,-5.26598123633362E-17,8.67361737988404E-18));
#77337=CARTESIAN_POINT('',(-0.415,5.08228421646152E-17,0.015));
#77338=CARTESIAN_POINT('Origin',(0.,0.,0.));
#77339=CARTESIAN_POINT('Origin',(0.62,0.,0.));
#77340=CARTESIAN_POINT('',(-0.62,-7.59281015471359E-17,0.));
#77341=CARTESIAN_POINT('Origin',(0.,0.,0.));
#77342=CARTESIAN_POINT('Origin',(0.,0.,0.02));
#77343=CARTESIAN_POINT('',(-0.62,-7.59281015471359E-17,0.04));
#77344=CARTESIAN_POINT('Origin',(0.,0.,0.04));
#77345=CARTESIAN_POINT('',(-0.62,-7.59281015471359E-17,0.02));
#77346=CARTESIAN_POINT('Origin',(0.92,0.,0.04));
#77347=CARTESIAN_POINT('',(-0.92,-1.12667505521556E-16,0.04));
#77348=CARTESIAN_POINT('Origin',(0.,0.,0.04));
#77349=CARTESIAN_POINT('Origin',(0.,0.,0.02));
#77350=CARTESIAN_POINT('',(-0.92,-1.12667505521556E-16,0.));
#77351=CARTESIAN_POINT('Origin',(0.,0.,0.));
#77352=CARTESIAN_POINT('',(-0.92,-1.12667505521556E-16,0.02));
#77353=CARTESIAN_POINT('Origin',(1.07,0.,0.));
#77354=CARTESIAN_POINT('',(-1.07,-1.31037207508767E-16,6.93889390390723E-18));
#77355=CARTESIAN_POINT('Origin',(0.,0.,0.));
#77356=CARTESIAN_POINT('Origin',(0.,0.,0.015));
#77357=CARTESIAN_POINT('',(-1.1,-1.34711147906209E-16,0.03));
#77358=CARTESIAN_POINT('Origin',(0.,0.,0.03));
#77359=CARTESIAN_POINT('',(-1.085,-1.32874177707488E-16,0.015));
#77360=CARTESIAN_POINT('Origin',(0.,0.,0.35));
#77361=CARTESIAN_POINT('',(-1.1,-1.34711147906209E-16,0.67));
#77362=CARTESIAN_POINT('Origin',(0.,0.,0.67));
#77363=CARTESIAN_POINT('',(-1.1,-1.34711147906209E-16,0.35));
#77364=CARTESIAN_POINT('Origin',(0.,0.,0.685));
#77365=CARTESIAN_POINT('',(-1.07,-1.31037207508767E-16,0.7));
#77366=CARTESIAN_POINT('',(-1.085,1.32874177707488E-16,0.685));
#77367=CARTESIAN_POINT('Origin',(0.,0.,0.7));
#77368=CARTESIAN_POINT('Origin',(0.92,0.,0.7));
#77369=CARTESIAN_POINT('',(-0.92,-1.12667505521556E-16,0.7));
#77370=CARTESIAN_POINT('Origin',(0.,0.,0.7));
#77371=CARTESIAN_POINT('Origin',(0.,0.,0.68));
#77372=CARTESIAN_POINT('',(-0.92,-1.12667505521556E-16,0.66));
#77373=CARTESIAN_POINT('Origin',(0.,0.,0.66));
#77374=CARTESIAN_POINT('',(-0.92,-1.12667505521556E-16,0.68));
#77375=CARTESIAN_POINT('Origin',(0.62,0.,0.66));
#77376=CARTESIAN_POINT('',(-0.62,-7.59281015471359E-17,0.66));
#77377=CARTESIAN_POINT('Origin',(0.,0.,0.66));
#77378=CARTESIAN_POINT('Origin',(0.,0.,0.68));
#77379=CARTESIAN_POINT('',(-0.62,-7.59281015471359E-17,0.7));
#77380=CARTESIAN_POINT('Origin',(0.,0.,0.7));
#77381=CARTESIAN_POINT('',(-0.62,-7.59281015471359E-17,0.68));
#77382=CARTESIAN_POINT('Origin',(0.43,0.,0.7));
#77383=CARTESIAN_POINT('',(-0.43,-5.26598123633362E-17,0.7));
#77384=CARTESIAN_POINT('Origin',(0.,0.,0.7));
#77385=CARTESIAN_POINT('Origin',(0.,0.,0.685));
#77386=CARTESIAN_POINT('',(-0.415,-5.08228421646152E-17,0.685));
#77387=CARTESIAN_POINT('',(0.,0.,0.));
#77388=CARTESIAN_POINT('Origin',(0.989949493661167,0.897918471982869,13.75));
#77389=CARTESIAN_POINT('',(0.949277528782289,0.938590436861746,13.15));
#77390=CARTESIAN_POINT('',(0.949277528782289,0.938590436861746,13.6));
#77391=CARTESIAN_POINT('',(0.949277528782289,0.938590436861746,13.15));
#77392=CARTESIAN_POINT('',(0.82731493398826,1.06055303165577,13.15));
#77393=CARTESIAN_POINT('',(0.82731493398826,1.06055303165577,13.15));
#77394=CARTESIAN_POINT('',(0.82731493398826,1.06055303165577,13.75));
#77395=CARTESIAN_POINT('',(0.82731493398826,1.06055303165577,13.75));
#77396=CARTESIAN_POINT('',(0.906628408599113,0.981239557044922,13.75));
#77397=CARTESIAN_POINT('',(0.591941738241592,1.29592622740244,13.75));
#77398=CARTESIAN_POINT('Ctrl Pts',(0.94927752878229,0.938590436861745,13.6));
#77399=CARTESIAN_POINT('Ctrl Pts',(0.9275177734406,0.960350192203436,13.6765467245383));
#77400=CARTESIAN_POINT('Ctrl Pts',(0.906628408599113,0.981239557044923,
13.75));
#77401=CARTESIAN_POINT('Origin',(1.03944696834422,1.27268506601174,13.75));
#77402=CARTESIAN_POINT('',(1.16140956313825,1.15072247121771,13.6));
#77403=CARTESIAN_POINT('',(1.16140956313825,1.15072247121771,13.15));
#77404=CARTESIAN_POINT('',(1.16140956313825,1.15072247121771,13.15));
#77405=CARTESIAN_POINT('',(1.11876044295508,1.19337159140089,13.75));
#77406=CARTESIAN_POINT('Ctrl Pts',(1.11876044295508,1.19337159140089,13.75));
#77407=CARTESIAN_POINT('Ctrl Pts',(1.13964980776901,1.17248222658696,13.6765467246352));
#77408=CARTESIAN_POINT('Ctrl Pts',(1.16140956313825,1.15072247121771,13.6));
#77409=CARTESIAN_POINT('',(1.03944696834422,1.27268506601174,13.75));
#77410=CARTESIAN_POINT('',(0.722756492761103,1.58937554159486,13.75));
#77411=CARTESIAN_POINT('',(1.03944696834422,1.27268506601174,13.15));
#77412=CARTESIAN_POINT('',(1.03944696834422,1.27268506601174,13.75));
#77413=CARTESIAN_POINT('',(1.20208152801713,1.11005050633883,13.15));
#77414=CARTESIAN_POINT('Origin',(0.82731493398826,1.06055303165577,13.75));
#77415=CARTESIAN_POINT('',(1.03034794257725,1.26358604024477,13.75));
#77416=CARTESIAN_POINT('',(1.03944696834422,1.27268506601174,13.15));
#77417=CARTESIAN_POINT('Origin',(1.0146982310027,1.0853017689973,13.15));
#77418=CARTESIAN_POINT('Origin',(0.,2.1,13.15));
#77419=CARTESIAN_POINT('Origin',(0.6,2.1,13.75));
#77420=CARTESIAN_POINT('',(1.4321661914736,1.95,13.75));
#77421=CARTESIAN_POINT('Origin',(0.,2.1,13.75));
#77422=CARTESIAN_POINT('',(1.32,1.95,13.75));
#77423=CARTESIAN_POINT('',(1.075,1.95,13.75));
#77424=CARTESIAN_POINT('',(1.32,2.25,13.75));
#77425=CARTESIAN_POINT('',(1.32,2.025,13.75));
#77426=CARTESIAN_POINT('',(1.4321661914736,2.25,13.75));
#77427=CARTESIAN_POINT('',(0.96,2.25,13.75));
#77428=CARTESIAN_POINT('',(1.11876044295508,3.00662840859911,13.75));
#77429=CARTESIAN_POINT('Origin',(0.,2.1,13.75));
#77430=CARTESIAN_POINT('',(1.03944696834422,2.92731493398826,13.75));
#77431=CARTESIAN_POINT('',(0.804073772597556,2.69194173824159,13.75));
#77432=CARTESIAN_POINT('',(0.827314933988261,3.13944696834422,13.75));
#77433=CARTESIAN_POINT('',(1.13641395975523,2.83034794257725,13.75));
#77434=CARTESIAN_POINT('',(0.906628408599113,3.21876044295508,13.75));
#77435=CARTESIAN_POINT('',(0.510624458405139,2.8227564927611,13.75));
#77436=CARTESIAN_POINT('',(0.15,3.5321661914736,13.75));
#77437=CARTESIAN_POINT('Origin',(0.,2.1,13.75));
#77438=CARTESIAN_POINT('',(0.15,3.42,13.75));
#77439=CARTESIAN_POINT('',(0.15,2.875,13.75));
#77440=CARTESIAN_POINT('',(-0.15,3.42,13.75));
#77441=CARTESIAN_POINT('',(0.375,3.42,13.75));
#77442=CARTESIAN_POINT('',(-0.15,3.5321661914736,13.75));
#77443=CARTESIAN_POINT('',(-0.15,2.76,13.75));
#77444=CARTESIAN_POINT('',(-0.906628408599113,3.21876044295508,13.75));
#77445=CARTESIAN_POINT('Origin',(0.,2.1,13.75));
#77446=CARTESIAN_POINT('',(-0.82731493398826,3.13944696834423,13.75));
#77447=CARTESIAN_POINT('',(-0.291941738241592,2.60407377259756,13.75));
#77448=CARTESIAN_POINT('',(-1.03944696834422,2.92731493398826,13.75));
#77449=CARTESIAN_POINT('',(-0.730347942577251,3.23641395975523,13.75));
#77450=CARTESIAN_POINT('',(-1.11876044295508,3.00662840859911,13.75));
#77451=CARTESIAN_POINT('',(-0.422756492761103,2.31062445840514,13.75));
#77452=CARTESIAN_POINT('',(-1.4321661914736,2.25,13.75));
#77453=CARTESIAN_POINT('Origin',(0.,2.1,13.75));
#77454=CARTESIAN_POINT('',(-1.32,2.25,13.75));
#77455=CARTESIAN_POINT('',(-0.475,2.25,13.75));
#77456=CARTESIAN_POINT('',(-1.32,1.95,13.75));
#77457=CARTESIAN_POINT('',(-1.32,2.175,13.75));
#77458=CARTESIAN_POINT('',(-1.4321661914736,1.95,13.75));
#77459=CARTESIAN_POINT('',(-0.36,1.95,13.75));
#77460=CARTESIAN_POINT('',(-1.11876044295508,1.19337159140089,13.75));
#77461=CARTESIAN_POINT('Origin',(0.,2.1,13.75));
#77462=CARTESIAN_POINT('',(-1.03944696834423,1.27268506601174,13.75));
#77463=CARTESIAN_POINT('',(-0.504073772597556,1.80805826175841,13.75));
#77464=CARTESIAN_POINT('',(-0.827314933988261,1.06055303165578,13.75));
#77465=CARTESIAN_POINT('',(-0.836413959755234,1.06965205742275,13.75));
#77466=CARTESIAN_POINT('',(-0.906628408599113,0.981239557044923,13.75));
#77467=CARTESIAN_POINT('',(-0.210624458405139,1.6772435072389,13.75));
#77468=CARTESIAN_POINT('',(-0.15,0.667833808526399,13.75));
#77469=CARTESIAN_POINT('Origin',(0.,2.1,13.75));
#77470=CARTESIAN_POINT('',(-0.15,0.78,13.75));
#77471=CARTESIAN_POINT('',(-0.15,1.325,13.75));
#77472=CARTESIAN_POINT('',(0.149999999999999,0.78,13.75));
#77473=CARTESIAN_POINT('',(0.225,0.78,13.75));
#77474=CARTESIAN_POINT('',(0.149999999999999,0.667833808526399,13.75));
#77475=CARTESIAN_POINT('',(0.15,1.44,13.75));
#77476=CARTESIAN_POINT('Origin',(0.,2.1,13.75));
#77477=CARTESIAN_POINT('',(-0.6,2.1,13.75));
#77478=CARTESIAN_POINT('Origin',(0.,2.1,13.75));
#77479=CARTESIAN_POINT('Origin',(0.,2.1,13.675));
#77480=CARTESIAN_POINT('',(1.49248115565993,1.95,13.6));
#77481=CARTESIAN_POINT('Origin',(0.,2.1,13.6));
#77482=CARTESIAN_POINT('Ctrl Pts',(1.49248115565993,1.95,13.6));
#77483=CARTESIAN_POINT('Ctrl Pts',(1.46170821455344,1.95,13.6765467245093));
#77484=CARTESIAN_POINT('Ctrl Pts',(1.4321661914736,1.95,13.75));
#77485=CARTESIAN_POINT('Origin',(0.,2.1,13.675));
#77486=CARTESIAN_POINT('',(0.149999999999999,0.60751884434007,13.6));
#77487=CARTESIAN_POINT('Ctrl Pts',(0.149999999999999,0.667833808526398,
13.75));
#77488=CARTESIAN_POINT('Ctrl Pts',(0.149999999999999,0.638291785446644,
13.6765467245096));
#77489=CARTESIAN_POINT('Ctrl Pts',(0.149999999999999,0.607518844340069,
13.6));
#77490=CARTESIAN_POINT('Origin',(0.,2.1,13.6));
#77491=CARTESIAN_POINT('Origin',(-0.15,0.55,13.75));
#77492=CARTESIAN_POINT('',(-0.15,0.60751884434007,13.15));
#77493=CARTESIAN_POINT('',(-0.15,0.60751884434007,13.6));
#77494=CARTESIAN_POINT('',(-0.15,0.60751884434007,13.15));
#77495=CARTESIAN_POINT('',(-0.15,0.78,13.15));
#77496=CARTESIAN_POINT('',(-0.15,0.78,13.15));
#77497=CARTESIAN_POINT('',(-0.15,0.78,13.75));
#77498=CARTESIAN_POINT('Ctrl Pts',(-0.15,0.607518844340069,13.6));
#77499=CARTESIAN_POINT('Ctrl Pts',(-0.15,0.63829178544613,13.6765467245083));
#77500=CARTESIAN_POINT('Ctrl Pts',(-0.15,0.667833808526399,13.75));
#77501=CARTESIAN_POINT('Origin',(0.149999999999999,0.78,13.75));
#77502=CARTESIAN_POINT('',(0.149999999999999,0.60751884434007,13.15));
#77503=CARTESIAN_POINT('',(0.149999999999999,0.60751884434007,13.15));
#77504=CARTESIAN_POINT('',(0.149999999999999,0.78,13.15));
#77505=CARTESIAN_POINT('',(0.149999999999999,0.78,13.75));
#77506=CARTESIAN_POINT('',(0.149999999999999,0.55,13.15));
#77507=CARTESIAN_POINT('Origin',(-0.15,0.78,13.75));
#77508=CARTESIAN_POINT('',(0.149999999999999,0.78,13.15));
#77509=CARTESIAN_POINT('Origin',(-4.44089209850063E-16,0.665,13.15));
#77510=CARTESIAN_POINT('Origin',(0.,2.1,13.15));
#77511=CARTESIAN_POINT('Origin',(0.,2.1,13.675));
#77512=CARTESIAN_POINT('',(-0.94927752878229,0.938590436861747,13.6));
#77513=CARTESIAN_POINT('Ctrl Pts',(-0.906628408599113,0.981239557044923,
13.75));
#77514=CARTESIAN_POINT('Ctrl Pts',(-0.927517773496767,0.960350192147269,
13.6765467243408));
#77515=CARTESIAN_POINT('Ctrl Pts',(-0.94927752878229,0.938590436861746,
13.6));
#77516=CARTESIAN_POINT('Origin',(0.,2.1,13.6));
#77517=CARTESIAN_POINT('Origin',(-1.20208152801713,1.11005050633883,13.75));
#77518=CARTESIAN_POINT('',(-1.16140956313825,1.15072247121771,13.15));
#77519=CARTESIAN_POINT('',(-1.16140956313825,1.15072247121771,13.6));
#77520=CARTESIAN_POINT('',(-1.16140956313825,1.15072247121771,13.15));
#77521=CARTESIAN_POINT('',(-1.03944696834423,1.27268506601174,13.15));
#77522=CARTESIAN_POINT('',(-1.03944696834423,1.27268506601174,13.15));
#77523=CARTESIAN_POINT('',(-1.03944696834423,1.27268506601174,13.75));
#77524=CARTESIAN_POINT('Ctrl Pts',(-1.16140956313825,1.15072247121771,13.6));
#77525=CARTESIAN_POINT('Ctrl Pts',(-1.13964980779618,1.17248222655978,13.6765467245397));
#77526=CARTESIAN_POINT('Ctrl Pts',(-1.11876044295508,1.19337159140089,13.75));
#77527=CARTESIAN_POINT('Origin',(-0.827314933988261,1.06055303165578,13.75));
#77528=CARTESIAN_POINT('',(-0.94927752878229,0.938590436861747,13.15));
#77529=CARTESIAN_POINT('',(-0.94927752878229,0.938590436861747,13.15));
#77530=CARTESIAN_POINT('',(-0.827314933988261,1.06055303165578,13.15));
#77531=CARTESIAN_POINT('',(-0.827314933988261,1.06055303165578,13.75));
#77532=CARTESIAN_POINT('',(-0.989949493661167,0.897918471982869,13.15));
#77533=CARTESIAN_POINT('Origin',(-1.03944696834423,1.27268506601174,13.75));
#77534=CARTESIAN_POINT('',(-0.827314933988261,1.06055303165578,13.15));
#77535=CARTESIAN_POINT('Origin',(-1.0146982310027,1.0853017689973,13.15));
#77536=CARTESIAN_POINT('Origin',(0.,2.1,13.15));
#77537=CARTESIAN_POINT('Origin',(0.,2.1,13.675));
#77538=CARTESIAN_POINT('',(-1.49248115565993,1.95,13.6));
#77539=CARTESIAN_POINT('Ctrl Pts',(-1.4321661914736,1.95,13.75));
#77540=CARTESIAN_POINT('Ctrl Pts',(-1.46170821455336,1.95,13.6765467245096));
#77541=CARTESIAN_POINT('Ctrl Pts',(-1.49248115565993,1.95,13.6));
#77542=CARTESIAN_POINT('Origin',(0.,2.1,13.6));
#77543=CARTESIAN_POINT('Origin',(-1.55,2.25,13.75));
#77544=CARTESIAN_POINT('',(-1.49248115565993,2.25,13.15));
#77545=CARTESIAN_POINT('',(-1.49248115565993,2.25,13.6));
#77546=CARTESIAN_POINT('',(-1.49248115565993,2.25,13.15));
#77547=CARTESIAN_POINT('',(-1.32,2.25,13.15));
#77548=CARTESIAN_POINT('',(-1.32,2.25,13.15));
#77549=CARTESIAN_POINT('',(-1.32,2.25,13.75));
#77550=CARTESIAN_POINT('Ctrl Pts',(-1.49248115565993,2.25,13.6));
#77551=CARTESIAN_POINT('Ctrl Pts',(-1.46170821455336,2.25,13.6765467245096));
#77552=CARTESIAN_POINT('Ctrl Pts',(-1.4321661914736,2.25,13.75));
#77553=CARTESIAN_POINT('Origin',(-1.32,1.95,13.75));
#77554=CARTESIAN_POINT('',(-1.49248115565993,1.95,13.15));
#77555=CARTESIAN_POINT('',(-1.49248115565993,1.95,13.15));
#77556=CARTESIAN_POINT('',(-1.32,1.95,13.15));
#77557=CARTESIAN_POINT('',(-1.32,1.95,13.75));
#77558=CARTESIAN_POINT('',(-1.55,1.95,13.15));
#77559=CARTESIAN_POINT('Origin',(-1.32,2.25,13.75));
#77560=CARTESIAN_POINT('',(-1.32,1.95,13.15));
#77561=CARTESIAN_POINT('Origin',(-1.435,2.1,13.15));
#77562=CARTESIAN_POINT('',(-1.5,2.1,13.15));
#77563=CARTESIAN_POINT('Origin',(0.,2.1,13.15));
#77564=CARTESIAN_POINT('Origin',(0.,2.1,13.15));
#77565=CARTESIAN_POINT('Origin',(0.,2.1,13.675));
#77566=CARTESIAN_POINT('',(-1.16140956313825,3.04927752878229,13.6));
#77567=CARTESIAN_POINT('Ctrl Pts',(-1.11876044295508,3.00662840859911,13.75));
#77568=CARTESIAN_POINT('Ctrl Pts',(-1.13964980785287,3.02751777349691,13.6765467243403));
#77569=CARTESIAN_POINT('Ctrl Pts',(-1.16140956313825,3.04927752878229,13.6));
#77570=CARTESIAN_POINT('Origin',(0.,2.1,13.6));
#77571=CARTESIAN_POINT('Origin',(-0.989949493661166,3.30208152801713,13.75));
#77572=CARTESIAN_POINT('',(-0.949277528782289,3.26140956313825,13.15));
#77573=CARTESIAN_POINT('',(-0.949277528782289,3.26140956313825,13.6));
#77574=CARTESIAN_POINT('',(-0.949277528782289,3.26140956313825,13.15));
#77575=CARTESIAN_POINT('',(-0.82731493398826,3.13944696834423,13.15));
#77576=CARTESIAN_POINT('',(-0.82731493398826,3.13944696834423,13.15));
#77577=CARTESIAN_POINT('',(-0.82731493398826,3.13944696834423,13.75));
#77578=CARTESIAN_POINT('Ctrl Pts',(-0.94927752878229,3.26140956313825,13.6));
#77579=CARTESIAN_POINT('Ctrl Pts',(-0.927517773384816,3.23964980774078,
13.6765467247345));
#77580=CARTESIAN_POINT('Ctrl Pts',(-0.906628408599113,3.21876044295508,
13.75));
#77581=CARTESIAN_POINT('Origin',(-1.03944696834422,2.92731493398826,13.75));
#77582=CARTESIAN_POINT('',(-1.16140956313825,3.04927752878229,13.15));
#77583=CARTESIAN_POINT('',(-1.16140956313825,3.04927752878229,13.15));
#77584=CARTESIAN_POINT('',(-1.03944696834422,2.92731493398826,13.15));
#77585=CARTESIAN_POINT('',(-1.03944696834422,2.92731493398826,13.75));
#77586=CARTESIAN_POINT('',(-1.20208152801713,3.08994949366117,13.15));
#77587=CARTESIAN_POINT('Origin',(-0.82731493398826,3.13944696834423,13.75));
#77588=CARTESIAN_POINT('',(-1.03944696834422,2.92731493398826,13.15));
#77589=CARTESIAN_POINT('Origin',(-1.0146982310027,3.1146982310027,13.15));
#77590=CARTESIAN_POINT('Origin',(0.,2.1,13.15));
#77591=CARTESIAN_POINT('Origin',(0.,2.1,13.675));
#77592=CARTESIAN_POINT('',(-0.15,3.59248115565993,13.6));
#77593=CARTESIAN_POINT('Ctrl Pts',(-0.15,3.5321661914736,13.75));
#77594=CARTESIAN_POINT('Ctrl Pts',(-0.15,3.56170821455336,13.6765467245096));
#77595=CARTESIAN_POINT('Ctrl Pts',(-0.15,3.59248115565993,13.6));
#77596=CARTESIAN_POINT('Origin',(0.,2.1,13.6));
#77597=CARTESIAN_POINT('Origin',(0.15,3.65,13.75));
#77598=CARTESIAN_POINT('',(0.15,3.59248115565993,13.15));
#77599=CARTESIAN_POINT('',(0.15,3.59248115565993,13.6));
#77600=CARTESIAN_POINT('',(0.15,3.59248115565993,13.15));
#77601=CARTESIAN_POINT('',(0.15,3.42,13.15));
#77602=CARTESIAN_POINT('',(0.15,3.42,13.15));
#77603=CARTESIAN_POINT('',(0.15,3.42,13.75));
#77604=CARTESIAN_POINT('Ctrl Pts',(0.15,3.59248115565993,13.6));
#77605=CARTESIAN_POINT('Ctrl Pts',(0.15,3.56170821455336,13.6765467245096));
#77606=CARTESIAN_POINT('Ctrl Pts',(0.15,3.5321661914736,13.75));
#77607=CARTESIAN_POINT('Origin',(-0.15,3.42,13.75));
#77608=CARTESIAN_POINT('',(-0.15,3.59248115565993,13.15));
#77609=CARTESIAN_POINT('',(-0.15,3.59248115565993,13.15));
#77610=CARTESIAN_POINT('',(-0.15,3.42,13.15));
#77611=CARTESIAN_POINT('',(-0.15,3.42,13.75));
#77612=CARTESIAN_POINT('',(-0.15,3.65,13.15));
#77613=CARTESIAN_POINT('Origin',(0.15,3.42,13.75));
#77614=CARTESIAN_POINT('',(-0.15,3.42,13.15));
#77615=CARTESIAN_POINT('Origin',(0.,3.535,13.15));
#77616=CARTESIAN_POINT('Origin',(0.,2.1,13.15));
#77617=CARTESIAN_POINT('Origin',(0.,2.1,13.675));
#77618=CARTESIAN_POINT('',(0.94927752878229,3.26140956313825,13.6));
#77619=CARTESIAN_POINT('Ctrl Pts',(0.906628408599113,3.21876044295508,13.75));
#77620=CARTESIAN_POINT('Ctrl Pts',(0.92751777344062,3.23964980779658,13.6765467245382));
#77621=CARTESIAN_POINT('Ctrl Pts',(0.94927752878229,3.26140956313825,13.6));
#77622=CARTESIAN_POINT('Origin',(0.,2.1,13.6));
#77623=CARTESIAN_POINT('Origin',(0.827314933988261,3.13944696834422,13.75));
#77624=CARTESIAN_POINT('',(0.827314933988261,3.13944696834422,13.15));
#77625=CARTESIAN_POINT('',(0.827314933988261,3.13944696834422,13.75));
#77626=CARTESIAN_POINT('',(0.94927752878229,3.26140956313825,13.15));
#77627=CARTESIAN_POINT('',(0.989949493661167,3.30208152801713,13.15));
#77628=CARTESIAN_POINT('',(0.94927752878229,3.26140956313825,13.15));
#77629=CARTESIAN_POINT('Origin',(1.20208152801713,3.08994949366117,13.75));
#77630=CARTESIAN_POINT('',(1.16140956313825,3.04927752878229,13.6));
#77631=CARTESIAN_POINT('Ctrl Pts',(1.16140956313825,3.04927752878229,13.6));
#77632=CARTESIAN_POINT('Ctrl Pts',(1.13964980779658,3.02751777344062,13.6765467245382));
#77633=CARTESIAN_POINT('Ctrl Pts',(1.11876044295508,3.00662840859911,13.75));
#77634=CARTESIAN_POINT('',(1.16140956313825,3.04927752878229,13.15));
#77635=CARTESIAN_POINT('',(1.16140956313825,3.04927752878229,13.15));
#77636=CARTESIAN_POINT('',(1.03944696834422,2.92731493398826,13.15));
#77637=CARTESIAN_POINT('',(1.03944696834422,2.92731493398826,13.15));
#77638=CARTESIAN_POINT('',(1.03944696834422,2.92731493398826,13.75));
#77639=CARTESIAN_POINT('Origin',(1.03944696834422,2.92731493398826,13.75));
#77640=CARTESIAN_POINT('',(0.827314933988261,3.13944696834422,13.15));
#77641=CARTESIAN_POINT('Origin',(1.0146982310027,3.1146982310027,13.15));
#77642=CARTESIAN_POINT('Origin',(0.,2.1,13.15));
#77643=CARTESIAN_POINT('Origin',(0.,2.1,13.675));
#77644=CARTESIAN_POINT('',(1.49248115565993,2.25,13.6));
#77645=CARTESIAN_POINT('Ctrl Pts',(1.4321661914736,2.25,13.75));
#77646=CARTESIAN_POINT('Ctrl Pts',(1.46170821455344,2.25,13.6765467245093));
#77647=CARTESIAN_POINT('Ctrl Pts',(1.49248115565993,2.25,13.6));
#77648=CARTESIAN_POINT('Origin',(0.,2.1,13.6));
#77649=CARTESIAN_POINT('Origin',(1.32,2.25,13.75));
#77650=CARTESIAN_POINT('',(1.32,2.25,13.15));
#77651=CARTESIAN_POINT('',(1.32,2.25,13.75));
#77652=CARTESIAN_POINT('',(1.49248115565993,2.25,13.15));
#77653=CARTESIAN_POINT('',(1.55,2.25,13.15));
#77654=CARTESIAN_POINT('',(1.49248115565993,2.25,13.15));
#77655=CARTESIAN_POINT('Origin',(1.55,1.95,13.75));
#77656=CARTESIAN_POINT('',(1.49248115565993,1.95,13.15));
#77657=CARTESIAN_POINT('',(1.49248115565993,1.95,13.15));
#77658=CARTESIAN_POINT('',(1.32,1.95,13.15));
#77659=CARTESIAN_POINT('',(1.32,1.95,13.15));
#77660=CARTESIAN_POINT('',(1.32,1.95,13.75));
#77661=CARTESIAN_POINT('Origin',(1.32,1.95,13.75));
#77662=CARTESIAN_POINT('',(1.32,2.25,13.15));
#77663=CARTESIAN_POINT('Origin',(1.435,2.1,13.15));
#77664=CARTESIAN_POINT('Origin',(0.,2.1,13.15));
#77665=CARTESIAN_POINT('Origin',(0.,2.1,13.035));
#77666=CARTESIAN_POINT('',(-1.1,2.1,12.7));
#77667=CARTESIAN_POINT('Origin',(0.,2.1,12.7));
#77668=CARTESIAN_POINT('',(-1.1,2.1,13.42));
#77669=CARTESIAN_POINT('',(-1.1,2.1,13.035));
#77670=CARTESIAN_POINT('Origin',(0.,2.1,13.42));
#77671=CARTESIAN_POINT('Origin',(0.,2.1,13.42));
#77672=CARTESIAN_POINT('',(-0.46,2.1,13.42));
#77673=CARTESIAN_POINT('Origin',(0.,2.1,13.42));
#77674=CARTESIAN_POINT('Origin',(0.,2.1,13.1));
#77675=CARTESIAN_POINT('',(-0.46,2.1,13.5));
#77676=CARTESIAN_POINT('',(-0.46,2.1,13.1));
#77677=CARTESIAN_POINT('Origin',(0.,2.1,13.5));
#77678=CARTESIAN_POINT('Origin',(1.5,2.1,12.7));
#77679=CARTESIAN_POINT('',(-1.5,2.1,12.7));
#77680=CARTESIAN_POINT('Origin',(0.,2.1,12.7));
#77681=CARTESIAN_POINT('Origin',(0.,2.1,13.15));
#77682=CARTESIAN_POINT('',(-1.5,2.1,13.15));
#77683=CARTESIAN_POINT('Origin',(0.,2.1,13.625));
#77684=CARTESIAN_POINT('',(-0.6,2.1,13.5));
#77685=CARTESIAN_POINT('Origin',(0.,2.1,13.5));
#77686=CARTESIAN_POINT('',(-0.6,2.1,13.625));
#77687=CARTESIAN_POINT('Origin',(0.46,2.1,13.5));
#77688=CARTESIAN_POINT('',(0.,0.,0.));
#77689=CARTESIAN_POINT('Origin',(0.25,3.66,12.85));
#77690=CARTESIAN_POINT('',(0.25,3.66009615088302,12.85));
#77691=CARTESIAN_POINT('',(0.25,3.66009615088302,13.25));
#77692=CARTESIAN_POINT('',(0.25,3.66009615088302,12.85));
#77693=CARTESIAN_POINT('',(0.25,3.9,12.85));
#77694=CARTESIAN_POINT('',(0.25,3.66,12.85));
#77695=CARTESIAN_POINT('',(0.25,3.9,13.25));
#77696=CARTESIAN_POINT('',(0.25,3.9,12.85));
#77697=CARTESIAN_POINT('',(0.25,3.66,13.25));
#77698=CARTESIAN_POINT('Origin',(-0.25,3.9,12.85));
#77699=CARTESIAN_POINT('',(-0.25,3.66009615088302,13.25));
#77700=CARTESIAN_POINT('',(-0.25,3.66009615088302,12.85));
#77701=CARTESIAN_POINT('',(-0.25,3.66009615088302,12.85));
#77702=CARTESIAN_POINT('',(-0.25,3.9,13.25));
#77703=CARTESIAN_POINT('',(-0.25,3.9,13.25));
#77704=CARTESIAN_POINT('',(-0.25,3.9,12.85));
#77705=CARTESIAN_POINT('',(-0.25,3.9,12.85));
#77706=CARTESIAN_POINT('',(-0.25,3.9,12.85));
#77707=CARTESIAN_POINT('Origin',(0.25,3.9,12.85));
#77708=CARTESIAN_POINT('',(0.25,3.9,12.85));
#77709=CARTESIAN_POINT('',(0.25,3.9,13.25));
#77710=CARTESIAN_POINT('Origin',(0.,2.1,13.25));
#77711=CARTESIAN_POINT('Origin',(0.,2.1,13.25));
#77712=CARTESIAN_POINT('',(-1.5,2.1,13.25));
#77713=CARTESIAN_POINT('Origin',(0.,2.1,13.25));
#77714=CARTESIAN_POINT('Origin',(0.,2.1,12.85));
#77715=CARTESIAN_POINT('',(-1.5,2.1,12.85));
#77716=CARTESIAN_POINT('Origin',(0.,2.1,12.85));
#77717=CARTESIAN_POINT('',(-1.5,2.1,12.85));
#77718=CARTESIAN_POINT('Origin',(0.,2.1,12.85));
#77719=CARTESIAN_POINT('Origin',(0.,2.1,12.85));
#77720=CARTESIAN_POINT('Origin',(0.,2.1,12.85));
#77721=CARTESIAN_POINT('',(0.,0.,0.));
#77722=CARTESIAN_POINT('Origin',(0.,0.,0.45));
#77723=CARTESIAN_POINT('',(-0.302,-3.69843333342501E-17,0.04));
#77724=CARTESIAN_POINT('Origin',(0.,0.,0.04));
#77725=CARTESIAN_POINT('',(-0.302,-3.69843333342501E-17,0.86));
#77726=CARTESIAN_POINT('',(-0.302,-3.69843333342501E-17,0.45));
#77727=CARTESIAN_POINT('Origin',(0.,0.,0.86));
#77728=CARTESIAN_POINT('Origin',(0.,0.,0.02));
#77729=CARTESIAN_POINT('',(-0.342,-4.18829205308395E-17,-3.46944695195361E-18));
#77730=CARTESIAN_POINT('',(-0.322,3.94336269325448E-17,0.02));
#77731=CARTESIAN_POINT('Origin',(0.,0.,0.));
#77732=CARTESIAN_POINT('Origin',(0.86,0.,0.));
#77733=CARTESIAN_POINT('',(-0.86,-1.05319624726672E-16,0.));
#77734=CARTESIAN_POINT('Origin',(0.,0.,0.));
#77735=CARTESIAN_POINT('Origin',(0.,0.,0.025));
#77736=CARTESIAN_POINT('',(-0.86,-1.05319624726672E-16,0.05));
#77737=CARTESIAN_POINT('Origin',(0.,0.,0.05));
#77738=CARTESIAN_POINT('',(-0.86,-1.05319624726672E-16,0.025));
#77739=CARTESIAN_POINT('Origin',(0.94,0.,0.05));
#77740=CARTESIAN_POINT('',(-0.94,-1.15116799119851E-16,0.05));
#77741=CARTESIAN_POINT('Origin',(0.,0.,0.05));
#77742=CARTESIAN_POINT('Origin',(0.,0.,0.025));
#77743=CARTESIAN_POINT('',(-0.94,-1.15116799119851E-16,0.));
#77744=CARTESIAN_POINT('Origin',(0.,0.,0.));
#77745=CARTESIAN_POINT('',(-0.94,-1.15116799119851E-16,0.025));
#77746=CARTESIAN_POINT('Origin',(0.95,0.,0.));
#77747=CARTESIAN_POINT('',(-0.95,-1.16341445918999E-16,-6.93889390390723E-18));
#77748=CARTESIAN_POINT('Origin',(0.,0.,0.));
#77749=CARTESIAN_POINT('Origin',(0.,0.,0.025));
#77750=CARTESIAN_POINT('',(-1.,-1.22464679914735E-16,0.05));
#77751=CARTESIAN_POINT('Origin',(0.,0.,0.05));
#77752=CARTESIAN_POINT('',(-0.975,-1.19403062916867E-16,0.025));
#77753=CARTESIAN_POINT('Origin',(0.,0.,0.45));
#77754=CARTESIAN_POINT('',(-1.,-1.22464679914735E-16,0.85));
#77755=CARTESIAN_POINT('Origin',(0.,0.,0.85));
#77756=CARTESIAN_POINT('',(-1.,-1.22464679914735E-16,0.45));
#77757=CARTESIAN_POINT('Origin',(0.,0.,0.875));
#77758=CARTESIAN_POINT('',(-0.95,-1.16341445918999E-16,0.9));
#77759=CARTESIAN_POINT('',(-0.975,1.19403062916867E-16,0.875));
#77760=CARTESIAN_POINT('Origin',(0.,0.,0.9));
#77761=CARTESIAN_POINT('Origin',(0.94,0.,0.9));
#77762=CARTESIAN_POINT('',(-0.94,-1.15116799119851E-16,0.9));
#77763=CARTESIAN_POINT('Origin',(0.,0.,0.9));
#77764=CARTESIAN_POINT('Origin',(0.,0.,0.875));
#77765=CARTESIAN_POINT('',(-0.94,-1.15116799119851E-16,0.85));
#77766=CARTESIAN_POINT('Origin',(0.,0.,0.85));
#77767=CARTESIAN_POINT('',(-0.94,-1.15116799119851E-16,0.875));
#77768=CARTESIAN_POINT('Origin',(0.86,0.,0.85));
#77769=CARTESIAN_POINT('',(-0.86,-1.05319624726672E-16,0.85));
#77770=CARTESIAN_POINT('Origin',(0.,0.,0.85));
#77771=CARTESIAN_POINT('Origin',(0.,0.,0.875));
#77772=CARTESIAN_POINT('',(-0.86,-1.05319624726672E-16,0.9));
#77773=CARTESIAN_POINT('Origin',(0.,0.,0.9));
#77774=CARTESIAN_POINT('',(-0.86,-1.05319624726672E-16,0.875));
#77775=CARTESIAN_POINT('Origin',(0.342,0.,0.9));
#77776=CARTESIAN_POINT('',(-0.342,-4.18829205308395E-17,0.9));
#77777=CARTESIAN_POINT('Origin',(0.,0.,0.9));
#77778=CARTESIAN_POINT('Origin',(0.,0.,0.88));
#77779=CARTESIAN_POINT('',(-0.322,-3.94336269325448E-17,0.88));
#77780=CARTESIAN_POINT('',(0.,0.,0.));
#77781=CARTESIAN_POINT('Origin',(0.,0.,0.4));
#77782=CARTESIAN_POINT('',(-0.202,-2.47378653427765E-17,0.03));
#77783=CARTESIAN_POINT('Origin',(0.,0.,0.03));
#77784=CARTESIAN_POINT('',(-0.202,-2.47378653427765E-17,0.77));
#77785=CARTESIAN_POINT('',(-0.202,-2.47378653427765E-17,0.4));
#77786=CARTESIAN_POINT('Origin',(0.,0.,0.77));
#77787=CARTESIAN_POINT('Origin',(0.,0.,0.015));
#77788=CARTESIAN_POINT('',(-0.232,-2.84118057402186E-17,8.67361737988404E-18));
#77789=CARTESIAN_POINT('',(-0.217,2.65748355414976E-17,0.015));
#77790=CARTESIAN_POINT('Origin',(0.,0.,0.));
#77791=CARTESIAN_POINT('Origin',(0.32,0.,0.));
#77792=CARTESIAN_POINT('',(-0.32,-3.91886975727153E-17,2.08166817117217E-17));
#77793=CARTESIAN_POINT('Origin',(0.,0.,0.));
#77794=CARTESIAN_POINT('Origin',(0.,0.,0.015));
#77795=CARTESIAN_POINT('',(-0.35,-4.28626379701574E-17,0.03));
#77796=CARTESIAN_POINT('Origin',(0.,0.,0.03));
#77797=CARTESIAN_POINT('',(-0.335,-4.10256677714363E-17,0.015));
#77798=CARTESIAN_POINT('Origin',(0.,0.,0.4));
#77799=CARTESIAN_POINT('',(-0.35,-4.28626379701574E-17,0.77));
#77800=CARTESIAN_POINT('Origin',(0.,0.,0.77));
#77801=CARTESIAN_POINT('',(-0.35,-4.28626379701574E-17,0.4));
#77802=CARTESIAN_POINT('Origin',(0.,0.,0.785));
#77803=CARTESIAN_POINT('',(-0.32,-3.91886975727153E-17,0.8));
#77804=CARTESIAN_POINT('',(-0.335,4.10256677714363E-17,0.785));
#77805=CARTESIAN_POINT('Origin',(0.,0.,0.8));
#77806=CARTESIAN_POINT('Origin',(0.232,0.,0.8));
#77807=CARTESIAN_POINT('',(-0.232,-2.84118057402186E-17,0.8));
#77808=CARTESIAN_POINT('Origin',(0.,0.,0.8));
#77809=CARTESIAN_POINT('Origin',(0.,0.,0.785));
#77810=CARTESIAN_POINT('',(-0.217,-2.65748355414976E-17,0.785));
#77811=CARTESIAN_POINT('',(0.,0.,0.));
#77812=CARTESIAN_POINT('Origin',(0.55,0.27,0.));
#77813=CARTESIAN_POINT('',(0.55,-0.27,-3.30654635769785E-17));
#77814=CARTESIAN_POINT('Origin',(0.55,0.,0.));
#77815=CARTESIAN_POINT('Origin',(0.565,0.,0.));
#77816=CARTESIAN_POINT('',(0.58,-0.3,-3.67394039744206E-17));
#77817=CARTESIAN_POINT('Origin',(0.58,0.,0.));
#77818=CARTESIAN_POINT('',(0.565,-0.285,-3.49024337756996E-17));
#77819=CARTESIAN_POINT('Origin',(1.59,0.,0.));
#77820=CARTESIAN_POINT('',(2.6,-0.3,-3.67394039744206E-17));
#77821=CARTESIAN_POINT('Origin',(2.6,0.,0.));
#77822=CARTESIAN_POINT('',(1.59,-0.3,-3.67394039744206E-17));
#77823=CARTESIAN_POINT('Origin',(2.6,0.25,0.));
#77824=CARTESIAN_POINT('',(2.6,-0.25,-3.06161699786838E-17));
#77825=CARTESIAN_POINT('Origin',(2.6,0.,0.));
#77826=CARTESIAN_POINT('Origin',(2.637,0.,0.));
#77827=CARTESIAN_POINT('',(2.674,-0.25,-3.06161699786838E-17));
#77828=CARTESIAN_POINT('Origin',(2.674,0.,0.));
#77829=CARTESIAN_POINT('',(2.637,-0.25,-3.06161699786838E-17));
#77830=CARTESIAN_POINT('Origin',(2.674,0.3,0.));
#77831=CARTESIAN_POINT('',(2.674,-0.3,-3.67394039744206E-17));
#77832=CARTESIAN_POINT('Origin',(2.674,0.,0.));
#77833=CARTESIAN_POINT('Origin',(2.697,0.,0.));
#77834=CARTESIAN_POINT('',(2.72,-0.3,-3.67394039744206E-17));
#77835=CARTESIAN_POINT('Origin',(2.72,0.,0.));
#77836=CARTESIAN_POINT('',(2.697,-0.3,-3.67394039744206E-17));
#77837=CARTESIAN_POINT('Origin',(2.735,0.,0.));
#77838=CARTESIAN_POINT('',(2.75,-0.27,-3.30654635769785E-17));
#77839=CARTESIAN_POINT('',(2.735,-0.285,3.49024337756996E-17));
#77840=CARTESIAN_POINT('Origin',(2.75,0.,0.));
#77841=CARTESIAN_POINT('Origin',(2.75,0.,0.));
#77842=CARTESIAN_POINT('',(0.,0.,0.));
#77843=CARTESIAN_POINT('Origin',(0.55,0.17,0.));
#77844=CARTESIAN_POINT('',(0.55,-0.17,-2.0818995585505E-17));
#77845=CARTESIAN_POINT('Origin',(0.55,0.,0.));
#77846=CARTESIAN_POINT('Origin',(0.565,0.,0.));
#77847=CARTESIAN_POINT('',(0.58,-0.2,-2.44929359829471E-17));
#77848=CARTESIAN_POINT('Origin',(0.58,0.,0.));
#77849=CARTESIAN_POINT('',(0.565,-0.185,-2.2655965784226E-17));
#77850=CARTESIAN_POINT('Origin',(1.59,0.,0.));
#77851=CARTESIAN_POINT('',(2.6,-0.2,-2.44929359829471E-17));
#77852=CARTESIAN_POINT('Origin',(2.6,0.,0.));
#77853=CARTESIAN_POINT('',(1.59,-0.2,-2.44929359829471E-17));
#77854=CARTESIAN_POINT('Origin',(2.6,0.16,0.));
#77855=CARTESIAN_POINT('',(2.6,-0.16,-1.95943487863577E-17));
#77856=CARTESIAN_POINT('Origin',(2.6,0.,0.));
#77857=CARTESIAN_POINT('Origin',(2.632,0.,0.));
#77858=CARTESIAN_POINT('',(2.664,-0.16,-1.95943487863577E-17));
#77859=CARTESIAN_POINT('Origin',(2.664,0.,0.));
#77860=CARTESIAN_POINT('',(2.632,-0.16,-1.95943487863577E-17));
#77861=CARTESIAN_POINT('Origin',(2.664,0.2,0.));
#77862=CARTESIAN_POINT('',(2.664,-0.2,-2.44929359829471E-17));
#77863=CARTESIAN_POINT('Origin',(2.664,0.,0.));
#77864=CARTESIAN_POINT('Origin',(2.692,0.,0.));
#77865=CARTESIAN_POINT('',(2.72,-0.2,-2.44929359829471E-17));
#77866=CARTESIAN_POINT('Origin',(2.72,0.,0.));
#77867=CARTESIAN_POINT('',(2.692,-0.2,-2.44929359829471E-17));
#77868=CARTESIAN_POINT('Origin',(2.735,0.,0.));
#77869=CARTESIAN_POINT('',(2.75,-0.17,-2.0818995585505E-17));
#77870=CARTESIAN_POINT('',(2.735,-0.185,2.2655965784226E-17));
#77871=CARTESIAN_POINT('Origin',(2.75,0.,0.));
#77872=CARTESIAN_POINT('Origin',(2.75,0.,0.));
#77873=CARTESIAN_POINT('',(0.,0.,0.));
#77874=CARTESIAN_POINT('Origin',(0.,0.,1.5));
#77875=CARTESIAN_POINT('',(-0.2,-2.44929359829471E-17,1.6));
#77876=CARTESIAN_POINT('Origin',(0.,0.,1.6));
#77877=CARTESIAN_POINT('',(-0.3,-3.67394039744206E-17,1.5));
#77878=CARTESIAN_POINT('Origin',(-0.2,-2.44929359829471E-17,1.5));
#77879=CARTESIAN_POINT('Origin',(0.,0.,1.5));
#77880=CARTESIAN_POINT('Origin',(0.,0.,0.82));
#77881=CARTESIAN_POINT('',(-0.3,-3.67394039744206E-17,0.04));
#77882=CARTESIAN_POINT('',(-0.3,-3.67394039744206E-17,0.82));
#77883=CARTESIAN_POINT('Origin',(0.,0.,0.04));
#77884=CARTESIAN_POINT('Origin',(0.,0.,1.6));
#77885=CARTESIAN_POINT('Origin',(0.26,0.,0.));
#77886=CARTESIAN_POINT('',(-0.26,-3.18408167778312E-17,-6.93889390390723E-18));
#77887=CARTESIAN_POINT('Origin',(0.,0.,0.));
#77888=CARTESIAN_POINT('Origin',(0.,0.,0.02));
#77889=CARTESIAN_POINT('',(-0.28,-3.42901103761259E-17,0.02));
#77890=CARTESIAN_POINT('',(0.,0.,0.));
#77891=CARTESIAN_POINT('Origin',(0.,0.,-1.10400562256037));
#77892=CARTESIAN_POINT('',(0.10234224283772,0.117140376604078,-0.940688754930896));
#77893=CARTESIAN_POINT('',(0.10234224283772,0.117140376604078,-0.954511891220802));
#77894=CARTESIAN_POINT('',(0.10234224283772,0.117140376604078,-1.10400562256037));
#77895=CARTESIAN_POINT('',(-0.0903576739864822,-0.126614743421738,-0.974595553498516));
#77896=CARTESIAN_POINT('Ctrl Pts',(-0.0903576739864822,-0.126614743421738,
-0.974595553498516));
#77897=CARTESIAN_POINT('Ctrl Pts',(-0.0821020793447133,-0.132506287400316,
-0.973865238560292));
#77898=CARTESIAN_POINT('Ctrl Pts',(-0.0732355876927443,-0.137609834113344,
-0.973134923622068));
#77899=CARTESIAN_POINT('Ctrl Pts',(-0.0639336210870726,-0.141803718550307,
-0.972404608683844));
#77900=CARTESIAN_POINT('Ctrl Pts',(-0.0546429158501588,-0.145992525686826,
-0.971675177896917));
#77901=CARTESIAN_POINT('Ctrl Pts',(-0.0449185996211577,-0.149273384832242,
-0.970945747109989));
#77902=CARTESIAN_POINT('Ctrl Pts',(-0.0349613681409583,-0.151570133066222,
-0.970216316323061));
#77903=CARTESIAN_POINT('Ctrl Pts',(-0.0250122354972982,-0.153865013211813,
-0.969487478827624));
#77904=CARTESIAN_POINT('Ctrl Pts',(-0.0148314833881561,-0.155177149067038,
-0.968758641332187));
#77905=CARTESIAN_POINT('Ctrl Pts',(-0.00463218640829535,-0.155481012824971,
-0.968029803836751));
#77906=CARTESIAN_POINT('Ctrl Pts',(0.00559025742364215,-0.155785566188224,
-0.967299312276947));
#77907=CARTESIAN_POINT('Ctrl Pts',(0.0158303791967561,-0.155077282770819,
-0.966568820717144));
#77908=CARTESIAN_POINT('Ctrl Pts',(0.0258748256235762,-0.153382840953444,
-0.965838329157341));
#77909=CARTESIAN_POINT('Ctrl Pts',(0.0326789164752719,-0.152235028960784,
-0.96534349542255));
#77910=CARTESIAN_POINT('Ctrl Pts',(0.039393259145739,-0.150635817813979,
-0.964848661687758));
#77911=CARTESIAN_POINT('Ctrl Pts',(0.045955143606566,-0.148606619220343,
-0.964353827952967));
#77912=CARTESIAN_POINT('Ctrl Pts',(0.0557528548327958,-0.145576772846209,
-0.963614979521936));
#77913=CARTESIAN_POINT('Ctrl Pts',(0.0652846037394777,-0.141563026261673,
-0.962876131090906));
#77914=CARTESIAN_POINT('Ctrl Pts',(0.0743438561876921,-0.13663379357664,
-0.962137282659876));
#77915=CARTESIAN_POINT('Ctrl Pts',(0.0834049481319706,-0.131703560002827,
-0.96139828420446));
#77916=CARTESIAN_POINT('Ctrl Pts',(0.091992485818785,-0.125857799939113,
-0.960659285749044));
#77917=CARTESIAN_POINT('Ctrl Pts',(0.099920187723521,-0.119213080596453,
-0.959920287293628));
#77918=CARTESIAN_POINT('Ctrl Pts',(0.107829175180873,-0.112584047041681,
-0.959183033347261));
#77919=CARTESIAN_POINT('Ctrl Pts',(0.11508071757252,-0.105160402097257,
-0.958445779400894));
#77920=CARTESIAN_POINT('Ctrl Pts',(0.121522063240699,-0.0970988704657448,
-0.957708525454528));
#77921=CARTESIAN_POINT('Ctrl Pts',(0.12798627142293,-0.0890087257322975,
-0.956968654744587));
#77922=CARTESIAN_POINT('Ctrl Pts',(0.13363394877096,-0.0802768955027428,
-0.956228784034647));
#77923=CARTESIAN_POINT('Ctrl Pts',(0.138353019634039,-0.0710932096486248,
-0.955488913324707));
#77924=CARTESIAN_POINT('Ctrl Pts',(0.143072090497117,-0.0619095237945068,
-0.954749042614766));
#77925=CARTESIAN_POINT('Ctrl Pts',(0.146862245092671,-0.0522748617005637,
-0.954009171904826));
#77926=CARTESIAN_POINT('Ctrl Pts',(0.149660270154457,-0.0423981843631897,
-0.953269301194886));
#77927=CARTESIAN_POINT('Ctrl Pts',(0.152445749361897,-0.0325657923172453,
-0.952532747935632));
#77928=CARTESIAN_POINT('Ctrl Pts',(0.154268738348244,-0.0224202029068401,
-0.951796194676377));
#77929=CARTESIAN_POINT('Ctrl Pts',(0.155073160606334,-0.0121703475530541,
-0.951059641417123));
#77930=CARTESIAN_POINT('Ctrl Pts',(0.155880880035407,-0.00187848002803857,
-0.950320069168764));
#77931=CARTESIAN_POINT('Ctrl Pts',(0.155661426215852,0.00851759185665578,
-0.949580496920404));
#77932=CARTESIAN_POINT('Ctrl Pts',(0.154410120702099,0.0187967317574963,
-0.948840924672044));
#77933=CARTESIAN_POINT('Ctrl Pts',(0.153166842230774,0.0290099316531165,
-0.948106096730931));
#77934=CARTESIAN_POINT('Ctrl Pts',(0.150905032779441,0.0391067646233177,
-0.947371268789817));
#77935=CARTESIAN_POINT('Ctrl Pts',(0.147672136222049,0.0488747653049779,
-0.946636440848704));
#77936=CARTESIAN_POINT('Ctrl Pts',(0.144407930591391,0.0587373644507617,
-0.945894496446721));
#77937=CARTESIAN_POINT('Ctrl Pts',(0.140153999677468,0.0682638040917823,
-0.945152552044738));
#77938=CARTESIAN_POINT('Ctrl Pts',(0.135009692886142,0.0772540311361782,
-0.944410607642755));
#77939=CARTESIAN_POINT('Ctrl Pts',(0.129865386094816,0.0862442581805741,
-0.943668663240772));
#77940=CARTESIAN_POINT('Ctrl Pts',(0.123831294364284,0.0946975055529981,
-0.942926718838789));
#77941=CARTESIAN_POINT('Ctrl Pts',(0.117050458195957,0.102445071800046,
-0.942184774436806));
#77942=CARTESIAN_POINT('Ctrl Pts',(0.112492945464506,0.107652339890906,
-0.94168610126817));
#77943=CARTESIAN_POINT('Ctrl Pts',(0.107575895728917,0.112567881699699,
-0.941187428099533));
#77944=CARTESIAN_POINT('Ctrl Pts',(0.10234224283772,0.117140376604078,-0.940688754930896));
#77945=CARTESIAN_POINT('',(0.0903606778650181,-0.126612599672285,-0.9746));
#77946=CARTESIAN_POINT('Origin',(0.,0.,-0.9746));
#77947=CARTESIAN_POINT('Ctrl Pts',(0.0903606778650178,-0.126612599672286,
-0.9746));
#77948=CARTESIAN_POINT('Ctrl Pts',(0.0989423350469826,-0.120488056284229,
-0.973844886200287));
#77949=CARTESIAN_POINT('Ctrl Pts',(0.106910670833421,-0.113479022235499,
-0.973089772400574));
#77950=CARTESIAN_POINT('Ctrl Pts',(0.11409063599182,-0.105731401574849,
-0.972334658600861));
#77951=CARTESIAN_POINT('Ctrl Pts',(0.121274299065747,-0.0979797906376286,
-0.971579155892987));
#77952=CARTESIAN_POINT('Ctrl Pts',(0.127668165389618,-0.0894894421859699,
-0.970823653185113));
#77953=CARTESIAN_POINT('Ctrl Pts',(0.133134293154607,-0.0804429144562979,
-0.970068150477239));
#77954=CARTESIAN_POINT('Ctrl Pts',(0.138600356882239,-0.0713964927094613,
-0.96931265662031));
#77955=CARTESIAN_POINT('Ctrl Pts',(0.143138276591898,-0.0617946583516004,
-0.968557162763381));
#77956=CARTESIAN_POINT('Ctrl Pts',(0.146655326515842,-0.0518460963287661,
-0.967801668906452));
#77957=CARTESIAN_POINT('Ctrl Pts',(0.150183534797359,-0.0418659710313748,
-0.967043778134273));
#77958=CARTESIAN_POINT('Ctrl Pts',(0.15268414454631,-0.031537752234968,
-0.966285887362093));
#77959=CARTESIAN_POINT('Ctrl Pts',(0.154114131731867,-0.0210864150706726,
-0.965527996589914));
#77960=CARTESIAN_POINT('Ctrl Pts',(0.155379873755172,-0.011835495354623,
-0.964857155473916));
#77961=CARTESIAN_POINT('Ctrl Pts',(0.155807551061526,-0.00248871112968671,
-0.964186314357918));
#77962=CARTESIAN_POINT('Ctrl Pts',(0.155401438548432,0.00679671958212004,
-0.96351547324192));
#77963=CARTESIAN_POINT('Ctrl Pts',(0.154947224274956,0.0171819577333334,
-0.96276517474016));
#77964=CARTESIAN_POINT('Ctrl Pts',(0.15344503494107,0.0275697639167967,
-0.962014876238401));
#77965=CARTESIAN_POINT('Ctrl Pts',(0.150904946143938,0.0377292953723635,
-0.961264577736641));
#77966=CARTESIAN_POINT('Ctrl Pts',(0.148439190723746,0.0475915174259657,
-0.960536236034742));
#77967=CARTESIAN_POINT('Ctrl Pts',(0.144995737284637,0.0572376793730887,
-0.959807894332843));
#77968=CARTESIAN_POINT('Ctrl Pts',(0.140635976190268,0.0664629573597977,
-0.959079552630945));
#77969=CARTESIAN_POINT('Ctrl Pts',(0.136079069165201,0.07610539719902,-0.958318275729254));
#77970=CARTESIAN_POINT('Ctrl Pts',(0.130521124612019,0.0852868296405983,
-0.957556998827564));
#77971=CARTESIAN_POINT('Ctrl Pts',(0.124088333471531,0.0937970575031978,
-0.956795721925873));
#77972=CARTESIAN_POINT('Ctrl Pts',(0.117655542331043,0.102307285365797,
-0.956034445024183));
#77973=CARTESIAN_POINT('Ctrl Pts',(0.110348660155481,0.110145395632112,
-0.955273168122492));
#77974=CARTESIAN_POINT('Ctrl Pts',(0.10234224283772,0.117140376604078,-0.954511891220802));
#77975=CARTESIAN_POINT('Origin',(0.,0.,-1.10400562256037));
#77976=CARTESIAN_POINT('',(0.10234224283772,0.117140376604078,-0.870692680653027));
#77977=CARTESIAN_POINT('',(0.102342240207423,0.117140378902094,-0.884408356863363));
#77978=CARTESIAN_POINT('',(0.10234224283772,0.117140376604078,-1.10400562256037));
#77979=CARTESIAN_POINT('',(-0.155549990439246,5.45376069021774E-5,-0.915194377445425));
#77980=CARTESIAN_POINT('Ctrl Pts',(-0.155549990439274,5.45375255761138E-5,
-0.91519437743963));
#77981=CARTESIAN_POINT('Ctrl Pts',(-0.155553695565796,-0.0105130925417861,
-0.914441312361376));
#77982=CARTESIAN_POINT('Ctrl Pts',(-0.154476175611492,-0.0210724552290184,
-0.913688247283122));
#77983=CARTESIAN_POINT('Ctrl Pts',(-0.152348281357228,-0.0313975105302782,
-0.912935182204868));
#77984=CARTESIAN_POINT('Ctrl Pts',(-0.150212869444931,-0.0417590433185059,
-0.912179456615772));
#77985=CARTESIAN_POINT('Ctrl Pts',(-0.147019895179501,-0.051883773121568,
-0.911423731026675));
#77986=CARTESIAN_POINT('Ctrl Pts',(-0.142850970898113,-0.0615581238624639,
-0.910668005437579));
#77987=CARTESIAN_POINT('Ctrl Pts',(-0.139657291957392,-0.0689693331195593,
-0.910089068345908));
#77988=CARTESIAN_POINT('Ctrl Pts',(-0.135891972280923,-0.0761164594459378,
-0.909510131254238));
#77989=CARTESIAN_POINT('Ctrl Pts',(-0.131609697969464,-0.08291374976677,
-0.908931194162567));
#77990=CARTESIAN_POINT('Ctrl Pts',(-0.126153759250654,-0.091574007552026,
-0.908193584877298));
#77991=CARTESIAN_POINT('Ctrl Pts',(-0.119819100241729,-0.0997255876699728,
-0.907455975592029));
#77992=CARTESIAN_POINT('Ctrl Pts',(-0.11272431583233,-0.107186898080564,
-0.90671836630676));
#77993=CARTESIAN_POINT('Ctrl Pts',(-0.10561318980285,-0.114665394341068,
-0.905979058064904));
#77994=CARTESIAN_POINT('Ctrl Pts',(-0.0977389649286095,-0.121449664158534,
-0.905239749823048));
#77995=CARTESIAN_POINT('Ctrl Pts',(-0.0892626926281267,-0.127389066268564,
-0.904500441581192));
#77996=CARTESIAN_POINT('Ctrl Pts',(-0.0808251947826937,-0.133301298760633,
-0.903764515282857));
#77997=CARTESIAN_POINT('Ctrl Pts',(-0.0717919070181361,-0.138375838170688,
-0.903028588984522));
#77998=CARTESIAN_POINT('Ctrl Pts',(-0.0623530724919041,-0.142505778306774,
-0.902292662686187));
#77999=CARTESIAN_POINT('Ctrl Pts',(-0.0528491738308247,-0.146664187104025,
-0.90155166347257));
#78000=CARTESIAN_POINT('Ctrl Pts',(-0.0429349806278062,-0.149864532282499,
-0.900810664258953));
#78001=CARTESIAN_POINT('Ctrl Pts',(-0.0328243966067401,-0.152047234395774,
-0.900069665045336));
#78002=CARTESIAN_POINT('Ctrl Pts',(-0.022713812585674,-0.154229936509049,
-0.89932866583172));
#78003=CARTESIAN_POINT('Ctrl Pts',(-0.0124077867892572,-0.155394922432058,
-0.898587666618103));
#78004=CARTESIAN_POINT('Ctrl Pts',(-0.00212611195938367,-0.15553546909929,
-0.897846667404486));
#78005=CARTESIAN_POINT('Ctrl Pts',(0.0081081454405522,-0.155675367587907,
-0.897109085560012));
#78006=CARTESIAN_POINT('Ctrl Pts',(0.0183942801159778,-0.15480133283454,
-0.896371503715537));
#78007=CARTESIAN_POINT('Ctrl Pts',(0.0285154184472853,-0.152913941191692,
-0.895633921871063));
#78008=CARTESIAN_POINT('Ctrl Pts',(0.0386603406337221,-0.151022114331388,
-0.894894606769008));
#78009=CARTESIAN_POINT('Ctrl Pts',(0.048638551484433,-0.148112187289814,
-0.894155291666953));
#78010=CARTESIAN_POINT('Ctrl Pts',(0.0582359863388471,-0.144237208774787,
-0.893415976564898));
#78011=CARTESIAN_POINT('Ctrl Pts',(0.0677890842962877,-0.140380131347479,
-0.892680076848101));
#78012=CARTESIAN_POINT('Ctrl Pts',(0.0769640506140051,-0.135567245221165,
-0.891944177131304));
#78013=CARTESIAN_POINT('Ctrl Pts',(0.0855676359870254,-0.129899892885221,
-0.891208277414506));
#78014=CARTESIAN_POINT('Ctrl Pts',(0.0942311165291288,-0.124193086413391,
-0.890467254619823));
#78015=CARTESIAN_POINT('Ctrl Pts',(0.102314429869336,-0.117620382437007,
-0.889726231825139));
#78016=CARTESIAN_POINT('Ctrl Pts',(0.109651105763752,-0.110328770068312,
-0.888985209030456));
#78017=CARTESIAN_POINT('Ctrl Pts',(0.116987781658168,-0.103037157699618,
-0.888244186235772));
#78018=CARTESIAN_POINT('Ctrl Pts',(0.123577241802067,-0.0950273934776604,
-0.887503163441089));
#78019=CARTESIAN_POINT('Ctrl Pts',(0.129294154728679,-0.0864801945707602,
-0.886762140646405));
#78020=CARTESIAN_POINT('Ctrl Pts',(0.134984233931287,-0.0779731140248378,
-0.886024596022792));
#78021=CARTESIAN_POINT('Ctrl Pts',(0.139852269637792,-0.0688704151456475,
-0.885287051399179));
#78022=CARTESIAN_POINT('Ctrl Pts',(0.1437806382265,-0.0593542801420444,
-0.884549506775566));
#78023=CARTESIAN_POINT('Ctrl Pts',(0.147718486439882,-0.0498151815630685,
-0.883810182368296));
#78024=CARTESIAN_POINT('Ctrl Pts',(0.15071163599617,-0.0398614498671554,
-0.883070857961026));
#78025=CARTESIAN_POINT('Ctrl Pts',(0.152687987532983,-0.0297015313263073,
-0.882331533553756));
#78026=CARTESIAN_POINT('Ctrl Pts',(0.154655078065095,-0.0195892212456017,
-0.881595673553847));
#78027=CARTESIAN_POINT('Ctrl Pts',(0.155614697529464,-0.00927356739940421,
-0.880859813553937));
#78028=CARTESIAN_POINT('Ctrl Pts',(0.155546601845199,0.00102818014534441,
-0.880123953554028));
#78029=CARTESIAN_POINT('Ctrl Pts',(0.155478025272198,0.011402678179368,
-0.879382896943078));
#78030=CARTESIAN_POINT('Ctrl Pts',(0.154367154022987,0.0217621226354572,
-0.878641840332127));
#78031=CARTESIAN_POINT('Ctrl Pts',(0.152246624058229,0.0318867991945324,
-0.877900783721177));
#78032=CARTESIAN_POINT('Ctrl Pts',(0.15012609409347,0.0420114757536077,
-0.877159727110227));
#78033=CARTESIAN_POINT('Ctrl Pts',(0.146996225216177,0.0519004868433207,
-0.876418670499277));
#78034=CARTESIAN_POINT('Ctrl Pts',(0.142940364535494,0.0613502623177764,
-0.875677613888326));
#78035=CARTESIAN_POINT('Ctrl Pts',(0.138903416737029,0.0707559725482313,
-0.874940012898144));
#78036=CARTESIAN_POINT('Ctrl Pts',(0.133919123239017,0.0797964660534999,
-0.874202411907961));
#78037=CARTESIAN_POINT('Ctrl Pts',(0.128076264758454,0.0882738517655276,
-0.873464810917779));
#78038=CARTESIAN_POINT('Ctrl Pts',(0.12224578062805,0.0967332835703058,
-0.872728772062459));
#78039=CARTESIAN_POINT('Ctrl Pts',(0.115560796270105,0.104631174276986,
-0.871992733207139));
#78040=CARTESIAN_POINT('Ctrl Pts',(0.108154991620488,0.111795797271508,
-0.871256694351819));
#78041=CARTESIAN_POINT('Ctrl Pts',(0.106263345437786,0.113625839026497,
-0.871068689785555));
#78042=CARTESIAN_POINT('Ctrl Pts',(0.104324881639651,0.115408201007507,
-0.870880685219291));
#78043=CARTESIAN_POINT('Ctrl Pts',(0.10234224283772,0.117140376604078,-0.870692680653027));
#78044=CARTESIAN_POINT('Ctrl Pts',(0.10234224283772,0.117140376604078,-0.940688754930896));
#78045=CARTESIAN_POINT('Ctrl Pts',(0.0946113887193601,0.123894605781591,
-0.939952143313806));
#78046=CARTESIAN_POINT('Ctrl Pts',(0.0861883742852771,0.129898311105041,
-0.939215531696717));
#78047=CARTESIAN_POINT('Ctrl Pts',(0.0772432491414857,0.135015861890618,
-0.938478920079627));
#78048=CARTESIAN_POINT('Ctrl Pts',(0.0683023925004671,0.140130970644432,
-0.937742659964465));
#78049=CARTESIAN_POINT('Ctrl Pts',(0.0588406921375984,0.1443602554083,-0.937006399849303));
#78050=CARTESIAN_POINT('Ctrl Pts',(0.0490562919704071,0.147611932844585,
-0.936270139734141));
#78051=CARTESIAN_POINT('Ctrl Pts',(0.0392744119919948,0.15086277273939,
-0.935534069259064));
#78052=CARTESIAN_POINT('Ctrl Pts',(0.0291708820205725,0.153136232213258,
-0.934797998783987));
#78053=CARTESIAN_POINT('Ctrl Pts',(0.0189595642724556,0.154390211550469,
-0.93406192830891));
#78054=CARTESIAN_POINT('Ctrl Pts',(0.00872456505581199,0.155647099040471,
-0.93332415078385));
#78055=CARTESIAN_POINT('Ctrl Pts',(-0.00161779436127116,0.15587973642895,
-0.93258637325879));
#78056=CARTESIAN_POINT('Ctrl Pts',(-0.0118498928897874,0.155097977222466,
-0.93184859573373));
#78057=CARTESIAN_POINT('Ctrl Pts',(-0.0153094593003107,0.154833657260698,
-0.931599146382062));
#78058=CARTESIAN_POINT('Ctrl Pts',(-0.0187564643405992,0.154453813501656,
-0.931349697030394));
#78059=CARTESIAN_POINT('Ctrl Pts',(-0.0221827247955545,0.153960154652575,
-0.931100247678727));
#78060=CARTESIAN_POINT('Ctrl Pts',(-0.0323154695014615,0.152500219205368,
-0.930362531842254));
#78061=CARTESIAN_POINT('Ctrl Pts',(-0.0423409400692818,0.150030283649637,
-0.929624816005781));
#78062=CARTESIAN_POINT('Ctrl Pts',(-0.0520449532400662,0.14658487419321,
-0.928887100169308));
#78063=CARTESIAN_POINT('Ctrl Pts',(-0.0617695627278741,0.143132152015315,
-0.928147818565253));
#78064=CARTESIAN_POINT('Ctrl Pts',(-0.0711704273079884,0.138699984168947,
-0.927408536961198));
#78065=CARTESIAN_POINT('Ctrl Pts',(-0.0800444925456803,0.133374216822835,
-0.926669255357143));
#78066=CARTESIAN_POINT('Ctrl Pts',(-0.0888796922985958,0.128071774584683,
-0.925933211563173));
#78067=CARTESIAN_POINT('Ctrl Pts',(-0.0971918959959097,0.121884019072182,
-0.925197167769204));
#78068=CARTESIAN_POINT('Ctrl Pts',(-0.104806016875265,0.114941295132522,
-0.924461123975234));
#78069=CARTESIAN_POINT('Ctrl Pts',(-0.112470378808711,0.107952760287768,
-0.923720223466136));
#78070=CARTESIAN_POINT('Ctrl Pts',(-0.119426704616414,0.100199888626462,
-0.922979322957038));
#78071=CARTESIAN_POINT('Ctrl Pts',(-0.125533638113307,0.0918537326516312,
-0.92223842244794));
#78072=CARTESIAN_POINT('Ctrl Pts',(-0.131640571610199,0.0835075766768,-0.921497521938842));
#78073=CARTESIAN_POINT('Ctrl Pts',(-0.136897660774886,0.0745689720957777,
-0.920756621429744));
#78074=CARTESIAN_POINT('Ctrl Pts',(-0.141209383237786,0.0652358228705983,
-0.920015720920646));
#78075=CARTESIAN_POINT('Ctrl Pts',(-0.145885740973675,0.0551133845747866,
-0.919212163674776));
#78076=CARTESIAN_POINT('Ctrl Pts',(-0.149481238527706,0.0444612846556873,
-0.918408606428906));
#78077=CARTESIAN_POINT('Ctrl Pts',(-0.151896399595966,0.0335154634427567,
-0.917605049183036));
#78078=CARTESIAN_POINT('Ctrl Pts',(-0.154311560664225,0.0225696422298262,
-0.916801491937166));
#78079=CARTESIAN_POINT('Ctrl Pts',(-0.155546036882257,0.011330715400011,
-0.915997934691295));
#78080=CARTESIAN_POINT('Ctrl Pts',(-0.155549990439246,5.45376069020738E-5,
-0.915194377445425));
#78081=CARTESIAN_POINT('',(-0.155549963323784,0.000106817458056085,-0.929005622560371));
#78082=CARTESIAN_POINT('Ctrl Pts',(0.10234224283772,0.117140376604078,-0.954511891220802));
#78083=CARTESIAN_POINT('Ctrl Pts',(0.0950470821490095,0.123513952721795,
-0.953818242975148));
#78084=CARTESIAN_POINT('Ctrl Pts',(0.0871722852291945,0.129187673667992,
-0.953124594729494));
#78085=CARTESIAN_POINT('Ctrl Pts',(0.0788756227046464,0.134068783253054,
-0.952430946483841));
#78086=CARTESIAN_POINT('Ctrl Pts',(0.0700399201463668,0.13926702198102,
-0.951692231420943));
#78087=CARTESIAN_POINT('Ctrl Pts',(0.0606559263352574,0.14360701660631,
-0.950953516358044));
#78088=CARTESIAN_POINT('Ctrl Pts',(0.0509130047566652,0.146981864346074,
-0.950214801295146));
#78089=CARTESIAN_POINT('Ctrl Pts',(0.0411659057623924,0.150358159099627,
-0.949475769497697));
#78090=CARTESIAN_POINT('Ctrl Pts',(0.0310603979437165,0.152768056474797,
-0.948736737700248));
#78091=CARTESIAN_POINT('Ctrl Pts',(0.0208080947762397,0.154151956496773,
-0.947997705902799));
#78092=CARTESIAN_POINT('Ctrl Pts',(0.0105837859788066,0.155532077718154,
-0.947260692064561));
#78093=CARTESIAN_POINT('Ctrl Pts',(0.000214397467965564,0.155891654329331,
-0.946523678226324));
#78094=CARTESIAN_POINT('Ctrl Pts',(-0.010081436783493,0.155222959424115,
-0.945786664388086));
#78095=CARTESIAN_POINT('Ctrl Pts',(-0.0204195563472874,0.154551518168071,
-0.945046623611031));
#78096=CARTESIAN_POINT('Ctrl Pts',(-0.0306825824822815,0.152843406969938,
-0.944306582833977));
#78097=CARTESIAN_POINT('Ctrl Pts',(-0.0406543023893487,0.150143365478583,
-0.943566542056923));
#78098=CARTESIAN_POINT('Ctrl Pts',(-0.0506260222964158,0.147443323987229,
-0.942826501279868));
#78099=CARTESIAN_POINT('Ctrl Pts',(-0.0603055729763678,0.143751713730547,
-0.942086460502814));
#78100=CARTESIAN_POINT('Ctrl Pts',(-0.0694954311322223,0.139162450221842,
-0.941346419725759));
#78101=CARTESIAN_POINT('Ctrl Pts',(-0.0786704779145675,0.134580583268645,
-0.940607571678797));
#78102=CARTESIAN_POINT('Ctrl Pts',(-0.0874231978033075,0.129071120965396,
-0.939868723631834));
#78103=CARTESIAN_POINT('Ctrl Pts',(-0.0955609209755141,0.122735133039858,
-0.939129875584871));
#78104=CARTESIAN_POINT('Ctrl Pts',(-0.103700301814298,0.11639785446395,
-0.938390877033439));
#78105=CARTESIAN_POINT('Ctrl Pts',(-0.111223634830413,0.109234181245416,
-0.937651878482006));
#78106=CARTESIAN_POINT('Ctrl Pts',(-0.117966058921268,0.101389404981901,
-0.936912879930574));
#78107=CARTESIAN_POINT('Ctrl Pts',(-0.124692561830681,0.0935631529323152,
-0.936175626408802));
#78108=CARTESIAN_POINT('Ctrl Pts',(-0.130641222457451,0.0850597003544771,
-0.93543837288703));
#78109=CARTESIAN_POINT('Ctrl Pts',(-0.135686790429376,0.0760585130210588,
-0.934701119365258));
#78110=CARTESIAN_POINT('Ctrl Pts',(-0.140750272183004,0.0670253678771716,
-0.933961248298995));
#78111=CARTESIAN_POINT('Ctrl Pts',(-0.144903792076823,0.0574917680180006,
-0.933221377232732));
#78112=CARTESIAN_POINT('Ctrl Pts',(-0.148067614915439,0.0476632343977336,
-0.932481506166469));
#78113=CARTESIAN_POINT('Ctrl Pts',(-0.151231437754054,0.0378347007774667,
-0.931741635100206));
#78114=CARTESIAN_POINT('Ctrl Pts',(-0.153405400787358,0.0277121514410604,
-0.931001764033943));
#78115=CARTESIAN_POINT('Ctrl Pts',(-0.154561090975207,0.017512043186154,
-0.93026189296768));
#78116=CARTESIAN_POINT('Ctrl Pts',(-0.155215195656062,0.011738922824918,
-0.929843136165244));
#78117=CARTESIAN_POINT('Ctrl Pts',(-0.15554596577893,0.00592813137733295,
-0.929424379362807));
#78118=CARTESIAN_POINT('Ctrl Pts',(-0.155549963323784,0.000106817458056085,
-0.929005622560371));
#78119=CARTESIAN_POINT('Ctrl Pts',(-0.155549958606928,0.000113478556899634,
-0.92890670318866));
#78120=CARTESIAN_POINT('Ctrl Pts',(-0.15555842151029,-0.0114869885586137,
-0.928125533282183));
#78121=CARTESIAN_POINT('Ctrl Pts',(-0.154269217954487,-0.0230528665738872,
-0.927379180799272));
#78122=CARTESIAN_POINT('Ctrl Pts',(-0.150513718193053,-0.0396298028538525,
-0.926241852967461));
#78123=CARTESIAN_POINT('Ctrl Pts',(-0.149049117672017,-0.044824673419037,
-0.925875717519125));
#78124=CARTESIAN_POINT('Ctrl Pts',(-0.146757293093334,-0.0515863198642148,
-0.925379644446853));
#78125=CARTESIAN_POINT('Ctrl Pts',(-0.146168987948676,-0.0532304236852607,
-0.92525746973569));
#78126=CARTESIAN_POINT('Ctrl Pts',(-0.145139226726601,-0.0559623497425928,
-0.92505165225389));
#78127=CARTESIAN_POINT('Ctrl Pts',(-0.1447128985104,-0.0570557323292614,
-0.924968516834851));
#78128=CARTESIAN_POINT('Ctrl Pts',(-0.143846311692037,-0.0592060112854775,
-0.924803451688519));
#78129=CARTESIAN_POINT('Ctrl Pts',(-0.143406674663571,-0.0602630790138749,
-0.92472154729743));
#78130=CARTESIAN_POINT('Ctrl Pts',(-0.142406127794732,-0.062595839297176,
-0.924539060713868));
#78131=CARTESIAN_POINT('Ctrl Pts',(-0.141839668107321,-0.0638690272896489,
-0.924438294737681));
#78132=CARTESIAN_POINT('Ctrl Pts',(-0.139797417899609,-0.0682980312682417,
-0.92408355206488));
#78133=CARTESIAN_POINT('Ctrl Pts',(-0.138232886602676,-0.0714115161349304,
-0.923826580298416));
#78134=CARTESIAN_POINT('Ctrl Pts',(-0.130724420504484,-0.0851808277748374,
-0.922654677420037));
#78135=CARTESIAN_POINT('Ctrl Pts',(-0.123644260256459,-0.0951664776931758,
-0.921701866914742));
#78136=CARTESIAN_POINT('Ctrl Pts',(-0.112873075524329,-0.107100517719257,
-0.920460860689665));
#78137=CARTESIAN_POINT('Ctrl Pts',(-0.110166837651926,-0.109882318244648,
-0.920163377955844));
#78138=CARTESIAN_POINT('Ctrl Pts',(-0.106160694170145,-0.113703354844055,
-0.919745763824101));
#78139=CARTESIAN_POINT('Ctrl Pts',(-0.104943898542185,-0.114827368496542,
-0.919621728517606));
#78140=CARTESIAN_POINT('Ctrl Pts',(-0.102757422110185,-0.116783329100972,
-0.919404088725975));
#78141=CARTESIAN_POINT('Ctrl Pts',(-0.101795024295629,-0.11762315700496,
-0.919310026777228));
#78142=CARTESIAN_POINT('Ctrl Pts',(-0.100304733027344,-0.118891652662218,
-0.919167140697068));
#78143=CARTESIAN_POINT('Ctrl Pts',(-0.0997842198864589,-0.119328848352267,
-0.919117741711322));
#78144=CARTESIAN_POINT('Ctrl Pts',(-0.0987712684934094,-0.120168395810172,
-0.919022611287186));
#78145=CARTESIAN_POINT('Ctrl Pts',(-0.0982792248757209,-0.120571144173996,
-0.918976856533665));
#78146=CARTESIAN_POINT('Ctrl Pts',(-0.0971327282583652,-0.121497894651514,
-0.918871269731137));
#78147=CARTESIAN_POINT('Ctrl Pts',(-0.0964764885396974,-0.122019640005255,
-0.918811595098707));
#78148=CARTESIAN_POINT('Ctrl Pts',(-0.0942898170734549,-0.123729489257913,
-0.918615135912167));
#78149=CARTESIAN_POINT('Ctrl Pts',(-0.0927413373229463,-0.124894360761535,
-0.918479834861871));
#78150=CARTESIAN_POINT('Ctrl Pts',(-0.0820325027653891,-0.132641238757061,
-0.917566724344907));
#78151=CARTESIAN_POINT('Ctrl Pts',(-0.0722004711885394,-0.13823959997331,
-0.916837193149984));
#78152=CARTESIAN_POINT('Ctrl Pts',(-0.0569487009972901,-0.144848753469477,
-0.9157381921726));
#78153=CARTESIAN_POINT('Ctrl Pts',(-0.0519434028377933,-0.146718071010014,
-0.915382582329865));
#78154=CARTESIAN_POINT('Ctrl Pts',(-0.0434263309068883,-0.149408378661567,
-0.914775915053912));
#78155=CARTESIAN_POINT('Ctrl Pts',(-0.0399642777693343,-0.150371416958858,
-0.914528938529619));
#78156=CARTESIAN_POINT('Ctrl Pts',(-0.0349849308613356,-0.151572417561809,
-0.914171389992701));
#78157=CARTESIAN_POINT('Ctrl Pts',(-0.0334924983206864,-0.151909168314297,
-0.914063935441392));
#78158=CARTESIAN_POINT('Ctrl Pts',(-0.030876305638117,-0.152459056533917,
-0.913874941381056));
#78159=CARTESIAN_POINT('Ctrl Pts',(-0.0297546925034738,-0.152681918762541,
-0.913793715666761));
#78160=CARTESIAN_POINT('Ctrl Pts',(-0.0274188034895556,-0.153119339201618,
-0.913624087053861));
#78161=CARTESIAN_POINT('Ctrl Pts',(-0.0262042337487496,-0.153331864905213,
-0.913535626270902));
#78162=CARTESIAN_POINT('Ctrl Pts',(-0.023017402475677,-0.153850527967523,
-0.913302773887562));
#78163=CARTESIAN_POINT('Ctrl Pts',(-0.0210416083350701,-0.154133175567375,
-0.913157661256946));
#78164=CARTESIAN_POINT('Ctrl Pts',(-0.00974461085087905,-0.155528014957357,
-0.912323311217469));
#78165=CARTESIAN_POINT('Ctrl Pts',(-0.000344868758064268,-0.15583242440491,
-0.91160938709679));
#78166=CARTESIAN_POINT('Ctrl Pts',(0.0165438813602932,-0.154851060657897,
-0.910302674155081));
#78167=CARTESIAN_POINT('Ctrl Pts',(0.0240228052629501,-0.153868324355632,
-0.909715929865619));
#78168=CARTESIAN_POINT('Ctrl Pts',(0.0349236227189631,-0.151621494124985,
-0.908867518524567));
#78169=CARTESIAN_POINT('Ctrl Pts',(0.0384201141209241,-0.150773460572484,
-0.908596564898194));
#78170=CARTESIAN_POINT('Ctrl Pts',(0.0429060754647373,-0.149519218539199,
-0.908252953211336));
#78171=CARTESIAN_POINT('Ctrl Pts',(0.0439248875361686,-0.149223096214924,
-0.90817518938402));
#78172=CARTESIAN_POINT('Ctrl Pts',(0.0455875894249146,-0.14872131949046,
-0.908048815918406));
#78173=CARTESIAN_POINT('Ctrl Pts',(0.0462332895240024,-0.148521857539368,
-0.907999873114021));
#78174=CARTESIAN_POINT('Ctrl Pts',(0.0474454915087443,-0.148138727028628,
-0.90790826866143));
#78175=CARTESIAN_POINT('Ctrl Pts',(0.048012273645673,-0.147956002642827,
-0.907865553136803));
#78176=CARTESIAN_POINT('Ctrl Pts',(0.0495232473370512,-0.147459284270958,
-0.907751952195431));
#78177=CARTESIAN_POINT('Ctrl Pts',(0.0504655201013391,-0.147139471121678,
-0.907681394870265));
#78178=CARTESIAN_POINT('Ctrl Pts',(0.0540083180363241,-0.145898985756029,
-0.907416961297221));
#78179=CARTESIAN_POINT('Ctrl Pts',(0.0565874327973771,-0.14491817422107,
-0.907226194084785));
#78180=CARTESIAN_POINT('Ctrl Pts',(0.0686888153355076,-0.13994374572501,
-0.906333231584437));
#78181=CARTESIAN_POINT('Ctrl Pts',(0.0778246251406242,-0.135076913950358,
-0.905664045626618));
#78182=CARTESIAN_POINT('Ctrl Pts',(0.0916292727235142,-0.125854113764415,
-0.904565446489061));
#78183=CARTESIAN_POINT('Ctrl Pts',(0.0966309803781564,-0.122055822292311,
-0.904146332832308));
#78184=CARTESIAN_POINT('Ctrl Pts',(0.103502439801638,-0.116149951043788,
-0.903525641945619));
#78185=CARTESIAN_POINT('Ctrl Pts',(0.105566244601748,-0.114277436758061,
-0.903332825297031));
#78186=CARTESIAN_POINT('Ctrl Pts',(0.108582479215364,-0.111389315733298,
-0.903040393862723));
#78187=CARTESIAN_POINT('Ctrl Pts',(0.109573450010169,-0.110414642525321,
-0.902942508744874));
#78188=CARTESIAN_POINT('Ctrl Pts',(0.111343262674267,-0.108626645195505,
-0.902764281958235));
#78189=CARTESIAN_POINT('Ctrl Pts',(0.112126595735637,-0.107817886257278,
-0.902684144553977));
#78190=CARTESIAN_POINT('Ctrl Pts',(0.113800234515506,-0.106051957897308,
-0.902510139443805));
#78191=CARTESIAN_POINT('Ctrl Pts',(0.114687386248433,-0.105091933053241,
-0.9024161456162));
#78192=CARTESIAN_POINT('Ctrl Pts',(0.117100294653814,-0.102413879437565,
-0.902155505899546));
#78193=CARTESIAN_POINT('Ctrl Pts',(0.118600190079188,-0.100673112524103,
-0.901987813116794));
#78194=CARTESIAN_POINT('Ctrl Pts',(0.127276947925487,-0.09013983597288,
-0.900982625261368));
#78195=CARTESIAN_POINT('Ctrl Pts',(0.133511321274578,-0.0806179077762679,
-0.900108617563444));
#78196=CARTESIAN_POINT('Ctrl Pts',(0.141241602570841,-0.0654156670434553,
-0.898786769142857));
#78197=CARTESIAN_POINT('Ctrl Pts',(0.143547438384335,-0.0601875377353895,
-0.898344602034502));
#78198=CARTESIAN_POINT('Ctrl Pts',(0.146648259301679,-0.0519577249634245,
-0.897676800378137));
#78199=CARTESIAN_POINT('Ctrl Pts',(0.147649821725688,-0.0490392744700454,
-0.897445261816214));
#78200=CARTESIAN_POINT('Ctrl Pts',(0.148862017529785,-0.0451321805692637,
-0.89714384082322));
#78201=CARTESIAN_POINT('Ctrl Pts',(0.149150723171202,-0.0441687209002071,
-0.897070192712309));
#78202=CARTESIAN_POINT('Ctrl Pts',(0.149613954053185,-0.042566484172706,
-0.896948915333778));
#78203=CARTESIAN_POINT('Ctrl Pts',(0.149793778122319,-0.0419292847221374,
-0.8969009968103));
#78204=CARTESIAN_POINT('Ctrl Pts',(0.150129414352071,-0.0407102469382308,
-0.896809943620297));
#78205=CARTESIAN_POINT('Ctrl Pts',(0.150285923951169,-0.0401286226355811,
-0.89676676747304));
#78206=CARTESIAN_POINT('Ctrl Pts',(0.150702927809063,-0.0385422795841766,
-0.896649695699459));
#78207=CARTESIAN_POINT('Ctrl Pts',(0.150956756701925,-0.0375358165755575,
-0.896576168407868));
#78208=CARTESIAN_POINT('Ctrl Pts',(0.151931342057554,-0.0335015846534703,
-0.896284155252757));
#78209=CARTESIAN_POINT('Ctrl Pts',(0.152571283944592,-0.0304548090914521,
-0.896069688485559));
#78210=CARTESIAN_POINT('Ctrl Pts',(0.154680206779767,-0.0186654885958557,
-0.895255817057433));
#78211=CARTESIAN_POINT('Ctrl Pts',(0.15549249588109,-0.00982221229263341,
-0.894678100031022));
#78212=CARTESIAN_POINT('Ctrl Pts',(0.155596368136116,0.00705547200853701,
-0.893564403954027));
#78213=CARTESIAN_POINT('Ctrl Pts',(0.155026478307746,0.0150591704219786,
-0.893031400062748));
#78214=CARTESIAN_POINT('Ctrl Pts',(0.153494542755068,0.0253136736343002,
-0.892317405356613));
#78215=CARTESIAN_POINT('Ctrl Pts',(0.153093419290391,0.0276362205882911,
-0.892153659271439));
#78216=CARTESIAN_POINT('Ctrl Pts',(0.152388489219965,0.0312290467472916,
-0.891896699176937));
#78217=CARTESIAN_POINT('Ctrl Pts',(0.152121177132059,0.0325061885045768,
-0.89180463454713));
#78218=CARTESIAN_POINT('Ctrl Pts',(0.151593684669239,0.0348772314423096,
-0.891632287084306));
#78219=CARTESIAN_POINT('Ctrl Pts',(0.151337647220616,0.0359719740527535,
-0.891552141177227));
#78220=CARTESIAN_POINT('Ctrl Pts',(0.150738960129293,0.0384121845790077,
-0.891372166065112));
#78221=CARTESIAN_POINT('Ctrl Pts',(0.150390121939428,0.0397560186280247,
-0.8912721442879));
#78222=CARTESIAN_POINT('Ctrl Pts',(0.149449828631076,0.0431887009147026,
-0.891014230151929));
#78223=CARTESIAN_POINT('Ctrl Pts',(0.148832564837417,0.0452700997887852,
-0.890855525713056));
#78224=CARTESIAN_POINT('Ctrl Pts',(0.145471409157558,0.0557908465162443,
-0.890041107666606));
#78225=CARTESIAN_POINT('Ctrl Pts',(0.142052888732019,0.0639959328316331,
-0.889364166383715));
#78226=CARTESIAN_POINT('Ctrl Pts',(0.134522879154025,0.0784510369806034,
-0.888103850397088));
#78227=CARTESIAN_POINT('Ctrl Pts',(0.130623917018437,0.0847842466628702,
-0.887525118175059));
#78228=CARTESIAN_POINT('Ctrl Pts',(0.124875396044254,0.0927781560968537,
-0.886774399550553));
#78229=CARTESIAN_POINT('Ctrl Pts',(0.123417829154911,0.0947084555639051,
-0.886591479859804));
#78230=CARTESIAN_POINT('Ctrl Pts',(0.120843059062481,0.0979578529855939,
-0.886281675226426));
#78231=CARTESIAN_POINT('Ctrl Pts',(0.119747820664398,0.0992937358630493,
-0.886153739821052));
#78232=CARTESIAN_POINT('Ctrl Pts',(0.118106938789238,0.101228497572341,
-0.885967932821096));
#78233=CARTESIAN_POINT('Ctrl Pts',(0.117578552177343,0.101841749082174,
-0.885908960179795));
#78234=CARTESIAN_POINT('Ctrl Pts',(0.116627582185086,0.1029281884201,-0.885804385885963));
#78235=CARTESIAN_POINT('Ctrl Pts',(0.116206864855181,0.103402947254518,
-0.885758657679481));
#78236=CARTESIAN_POINT('Ctrl Pts',(0.115257902278136,0.104460697390482,
-0.885656704705278));
#78237=CARTESIAN_POINT('Ctrl Pts',(0.114728125867569,0.105042270265658,
-0.885600593770631));
#78238=CARTESIAN_POINT('Ctrl Pts',(0.113105532242885,0.10679658470307,-0.885431073735817));
#78239=CARTESIAN_POINT('Ctrl Pts',(0.111998939130881,0.107956519409209,
-0.885318628931571));
#78240=CARTESIAN_POINT('Ctrl Pts',(0.108131847055068,0.111886540242922,
-0.884935505996942));
#78241=CARTESIAN_POINT('Ctrl Pts',(0.105285666458265,0.114568790529068,
-0.884670242381571));
#78242=CARTESIAN_POINT('Ctrl Pts',(0.102342240207423,0.117140378902094,
-0.884408356863363));
#78243=CARTESIAN_POINT('Origin',(0.,0.,-1.10400562256037));
#78244=CARTESIAN_POINT('',(0.10234224283772,0.117140376604078,-0.800700826369365));
#78245=CARTESIAN_POINT('',(0.102342242814364,0.117140376624483,-0.814640372754811));
#78246=CARTESIAN_POINT('',(0.10234224283772,0.117140376604078,-1.10400562256037));
#78247=CARTESIAN_POINT('',(-0.155549936897438,-0.000140111395033391,-0.845194377435982));
#78248=CARTESIAN_POINT('Ctrl Pts',(-0.155549936897438,-0.000140111395033152,
-0.845194377435982));
#78249=CARTESIAN_POINT('Ctrl Pts',(-0.155538319828762,-0.0130372372788212,
-0.84427092949535));
#78250=CARTESIAN_POINT('Ctrl Pts',(-0.1539193025723,-0.0258623074908684,
-0.843347481554718));
#78251=CARTESIAN_POINT('Ctrl Pts',(-0.150765547234312,-0.0382825321411526,
-0.842424033614087));
#78252=CARTESIAN_POINT('Ctrl Pts',(-0.148246611384062,-0.0482026894732453,
-0.841686466531606));
#78253=CARTESIAN_POINT('Ctrl Pts',(-0.144735020415677,-0.0579100309946745,
-0.840948899449126));
#78254=CARTESIAN_POINT('Ctrl Pts',(-0.140287561326135,-0.0671952575496648,
-0.840211332366645));
#78255=CARTESIAN_POINT('Ctrl Pts',(-0.135829539592097,-0.0765025363698251,
-0.839472013574092));
#78256=CARTESIAN_POINT('Ctrl Pts',(-0.130431466357588,-0.0853847925415279,
-0.838732694781539));
#78257=CARTESIAN_POINT('Ctrl Pts',(-0.124200087059014,-0.0936490302914732,
-0.837993375988985));
#78258=CARTESIAN_POINT('Ctrl Pts',(-0.117997662165273,-0.101874867861623,
-0.837257492476904));
#78259=CARTESIAN_POINT('Ctrl Pts',(-0.110970216967241,-0.109487670969301,
-0.836521608964823));
#78260=CARTESIAN_POINT('Ctrl Pts',(-0.103265733734167,-0.116327085136455,
-0.835785725452742));
#78261=CARTESIAN_POINT('Ctrl Pts',(-0.0955073009417575,-0.12321439133858,
-0.835044689019953));
#78262=CARTESIAN_POINT('Ctrl Pts',(-0.0870630130899514,-0.129316795090957,
-0.834303652587163));
#78263=CARTESIAN_POINT('Ctrl Pts',(-0.0781180168921039,-0.134511627515412,
-0.833562616154374));
#78264=CARTESIAN_POINT('Ctrl Pts',(-0.0691730206942564,-0.139706459939867,
-0.832821579721584));
#78265=CARTESIAN_POINT('Ctrl Pts',(-0.0597281969952501,-0.143993358605103,
-0.832080543288795));
#78266=CARTESIAN_POINT('Ctrl Pts',(-0.0499906020627426,-0.14729814053614,
-0.831339506856006));
#78267=CARTESIAN_POINT('Ctrl Pts',(-0.0402986120533905,-0.150587444895245,
-0.830601940983432));
#78268=CARTESIAN_POINT('Ctrl Pts',(-0.0302445674700445,-0.152928295698067,
-0.829864375110859));
#78269=CARTESIAN_POINT('Ctrl Pts',(-0.0200349361239818,-0.154254347862574,
-0.829126809238286));
#78270=CARTESIAN_POINT('Ctrl Pts',(-0.00980103609139822,-0.155583552104095,
-0.828387490143256));
#78271=CARTESIAN_POINT('Ctrl Pts',(0.000588290641111029,-0.15589286142406,
-0.827648171048226));
#78272=CARTESIAN_POINT('Ctrl Pts',(0.0109130440681473,-0.155166710247935,
-0.826908851953196));
#78273=CARTESIAN_POINT('Ctrl Pts',(0.0211898017065059,-0.154443934668007,
-0.826172969666928));
#78274=CARTESIAN_POINT('Ctrl Pts',(0.0314016544816177,-0.15269536639436,
-0.825437087380661));
#78275=CARTESIAN_POINT('Ctrl Pts',(0.0413335254017949,-0.14995780132377,
-0.824701205094393));
#78276=CARTESIAN_POINT('Ctrl Pts',(0.0513349739058709,-0.147201058279069,
-0.823960167594982));
#78277=CARTESIAN_POINT('Ctrl Pts',(0.0610515833788873,-0.143441647462304,
-0.823219130095571));
#78278=CARTESIAN_POINT('Ctrl Pts',(0.0702796451137023,-0.138768058221956,
-0.822478092596159));
#78279=CARTESIAN_POINT('Ctrl Pts',(0.079507706848517,-0.134094468981608,
-0.821737055096748));
#78280=CARTESIAN_POINT('Ctrl Pts',(0.0882464371862269,-0.128507242758074,
-0.820996017597337));
#78281=CARTESIAN_POINT('Ctrl Pts',(0.0963208635534173,-0.122139648535289,
-0.820254980097926));
#78282=CARTESIAN_POINT('Ctrl Pts',(0.104357457510738,-0.115801889426922,
-0.81951741470082));
#78283=CARTESIAN_POINT('Ctrl Pts',(0.111795714032649,-0.108643985892654,
-0.818779849303714));
#78284=CARTESIAN_POINT('Ctrl Pts',(0.118467555690701,-0.100802979860075,
-0.818042283906609));
#78285=CARTESIAN_POINT('Ctrl Pts',(0.125155261959505,-0.0929433291241313,
-0.817302964692712));
#78286=CARTESIAN_POINT('Ctrl Pts',(0.131072190559215,-0.0843979338543903,
-0.816563645478815));
#78287=CARTESIAN_POINT('Ctrl Pts',(0.1360854849751,-0.0753428382734008,
-0.815824326264918));
#78288=CARTESIAN_POINT('Ctrl Pts',(0.141075470205837,-0.0663298441294938,
-0.815088444496942));
#78289=CARTESIAN_POINT('Ctrl Pts',(0.145169750922882,-0.056812693240137,
-0.814352562728965));
#78290=CARTESIAN_POINT('Ctrl Pts',(0.148282068834788,-0.0469918137772452,
-0.813616680960989));
#78291=CARTESIAN_POINT('Ctrl Pts',(0.151416194104158,-0.0371021214761001,
-0.812875643024132));
#78292=CARTESIAN_POINT('Ctrl Pts',(0.153554242780962,-0.0269053291409457,
-0.812134605087275));
#78293=CARTESIAN_POINT('Ctrl Pts',(0.154659503832709,-0.0166204805652641,
-0.811393567150417));
#78294=CARTESIAN_POINT('Ctrl Pts',(0.155764764884456,-0.00633563198958233,
-0.81065252921356));
#78295=CARTESIAN_POINT('Ctrl Pts',(0.155837265691724,0.00403632070063776,
-0.809911491276702));
#78296=CARTESIAN_POINT('Ctrl Pts',(0.154893501714532,0.0142760508058142,
-0.809170453339845));
#78297=CARTESIAN_POINT('Ctrl Pts',(0.153954014253801,0.0244693812015213,
-0.808432773298618));
#78298=CARTESIAN_POINT('Ctrl Pts',(0.152000507162109,0.0346074596889915,
-0.807695093257391));
#78299=CARTESIAN_POINT('Ctrl Pts',(0.149056410292548,0.0444745888199042,
-0.806957413216164));
#78300=CARTESIAN_POINT('Ctrl Pts',(0.146118584279151,0.0543207012009377,
-0.806221304415843));
#78301=CARTESIAN_POINT('Ctrl Pts',(0.142194543330265,0.0638961073393962,
-0.805485195615522));
#78302=CARTESIAN_POINT('Ctrl Pts',(0.137358517895996,0.072996164703465,
-0.804749086815201));
#78303=CARTESIAN_POINT('Ctrl Pts',(0.132521054937009,0.0820989270899887,
-0.80401275920408));
#78304=CARTESIAN_POINT('Ctrl Pts',(0.126771460493011,0.0907252182537294,
-0.803276431592959));
#78305=CARTESIAN_POINT('Ctrl Pts',(0.12023091747951,0.0986931050379669,
-0.802540103981838));
#78306=CARTESIAN_POINT('Ctrl Pts',(0.114785028921007,0.105327450746598,
-0.801927011444347));
#78307=CARTESIAN_POINT('Ctrl Pts',(0.108791818876103,0.111505563943781,
-0.801313918906856));
#78308=CARTESIAN_POINT('Ctrl Pts',(0.10234224283772,0.117140376604078,-0.800700826369366));
#78309=CARTESIAN_POINT('Ctrl Pts',(0.10234224283772,0.117140376604078,-0.870692680653027));
#78310=CARTESIAN_POINT('Ctrl Pts',(0.0945823687409577,0.123919959718149,
-0.869956847296794));
#78311=CARTESIAN_POINT('Ctrl Pts',(0.0861434261176855,0.129927435099362,
-0.86922101394056));
#78312=CARTESIAN_POINT('Ctrl Pts',(0.0772043632031639,0.135038101298833,
-0.868485180584327));
#78313=CARTESIAN_POINT('Ctrl Pts',(0.06824357246428,0.14016118979118,-0.867747558667248));
#78314=CARTESIAN_POINT('Ctrl Pts',(0.0587810565339102,0.144382678263256,
-0.867009936750168));
#78315=CARTESIAN_POINT('Ctrl Pts',(0.0490207580366101,0.147623737188557,
-0.866272314833089));
#78316=CARTESIAN_POINT('Ctrl Pts',(0.0416141796594417,0.150083206738787,
-0.865712572265475));
#78317=CARTESIAN_POINT('Ctrl Pts',(0.0340367145713927,0.15197906578916,
-0.86515282969786));
#78318=CARTESIAN_POINT('Ctrl Pts',(0.0263818859332598,0.153296440254184,
-0.864593087130246));
#78319=CARTESIAN_POINT('Ctrl Pts',(0.0162951940079565,0.155032331546741,
-0.8638555198895));
#78320=CARTESIAN_POINT('Ctrl Pts',(0.00599895782048205,0.155774870891324,
-0.863117952648755));
#78321=CARTESIAN_POINT('Ctrl Pts',(-0.00429252786504568,0.15549076083333,
-0.86238038540801));
#78322=CARTESIAN_POINT('Ctrl Pts',(-0.014608452899512,0.155205976094823,
-0.861641066655023));
#78323=CARTESIAN_POINT('Ctrl Pts',(-0.0249186737362951,0.15388953793924,
-0.860901747902036));
#78324=CARTESIAN_POINT('Ctrl Pts',(-0.0350034587763083,0.151560418228821,
-0.860162429149049));
#78325=CARTESIAN_POINT('Ctrl Pts',(-0.0450413890419768,0.149242119807902,
-0.859426545334259));
#78326=CARTESIAN_POINT('Ctrl Pts',(-0.0548550642084026,0.145920735726236,
-0.858690661519468));
#78327=CARTESIAN_POINT('Ctrl Pts',(-0.0642377884513287,0.141666188749759,
-0.857954777704678));
#78328=CARTESIAN_POINT('Ctrl Pts',(-0.0736862073268392,0.137381852887539,
-0.857213741482593));
#78329=CARTESIAN_POINT('Ctrl Pts',(-0.0826967467014411,0.132151616254013,
-0.856472705260507));
#78330=CARTESIAN_POINT('Ctrl Pts',(-0.0910820121346721,0.126094684921687,
-0.855731669038422));
#78331=CARTESIAN_POINT('Ctrl Pts',(-0.0994672775679031,0.12003775358936,
-0.854990632816337));
#78332=CARTESIAN_POINT('Ctrl Pts',(-0.107226579556024,0.113154784688802,
-0.854249596594251));
#78333=CARTESIAN_POINT('Ctrl Pts',(-0.114207897837056,0.105604727979577,
-0.853508560372166));
#78334=CARTESIAN_POINT('Ctrl Pts',(-0.121078206097479,0.0981747248071135,
-0.852779307375394));
#78335=CARTESIAN_POINT('Ctrl Pts',(-0.127248819633919,0.0900404725511059,
-0.852050054378621));
#78336=CARTESIAN_POINT('Ctrl Pts',(-0.13257631495945,0.0813592232741483,
-0.851320801381849));
#78337=CARTESIAN_POINT('Ctrl Pts',(-0.137892545783061,0.0726963297052993,
-0.850593090323882));
#78338=CARTESIAN_POINT('Ctrl Pts',(-0.142368631298909,0.0634894916783257,
-0.849865379265916));
#78339=CARTESIAN_POINT('Ctrl Pts',(-0.145903110021304,0.0539266630351919,
-0.84913766820795));
#78340=CARTESIAN_POINT('Ctrl Pts',(-0.149439269993569,0.0443592856295196,
-0.848409610998764));
#78341=CARTESIAN_POINT('Ctrl Pts',(-0.152032558253122,0.0344364565318959,
-0.847681553789577));
#78342=CARTESIAN_POINT('Ctrl Pts',(-0.153629756766561,0.0243659667538019,
-0.846953496580391));
#78343=CARTESIAN_POINT('Ctrl Pts',(-0.154916131170997,0.0162552527870187,
-0.846367123533471));
#78344=CARTESIAN_POINT('Ctrl Pts',(-0.155557313527155,0.00804933460988067,
-0.84578075048655));
#78345=CARTESIAN_POINT('Ctrl Pts',(-0.155549936897484,-0.000140111344081384,
-0.84519437743963));
#78346=CARTESIAN_POINT('Ctrl Pts',(0.102342240207423,0.117140378902094,
-0.884408356863363));
#78347=CARTESIAN_POINT('Ctrl Pts',(0.0997671282763309,0.119390181457651,
-0.884179241381932));
#78348=CARTESIAN_POINT('Ctrl Pts',(0.0971175853369499,0.121555284170953,
-0.883952710064294));
#78349=CARTESIAN_POINT('Ctrl Pts',(0.0890846091051486,0.127688771197036,
-0.883285685527337));
#78350=CARTESIAN_POINT('Ctrl Pts',(0.0835155932020043,0.131398754954517,
-0.882847875137769));
#78351=CARTESIAN_POINT('Ctrl Pts',(0.0725185033115193,0.137742517529728,
-0.882001156533603));
#78352=CARTESIAN_POINT('Ctrl Pts',(0.0671425600539784,0.140441440762792,
-0.881594546776866));
#78353=CARTESIAN_POINT('Ctrl Pts',(0.0599616565701782,0.143539825929432,
-0.881051536440173));
#78354=CARTESIAN_POINT('Ctrl Pts',(0.0582865847286211,0.144228136828107,
-0.880924901066003));
#78355=CARTESIAN_POINT('Ctrl Pts',(0.055488758935558,0.14532110402266,-0.880713222267803));
#78356=CARTESIAN_POINT('Ctrl Pts',(0.0543726526414778,0.145742375941171,
-0.880628737717708));
#78357=CARTESIAN_POINT('Ctrl Pts',(0.0521746009066699,0.146543263309774,
-0.880462214047268));
#78358=CARTESIAN_POINT('Ctrl Pts',(0.0510930837640482,0.146923836268053,
-0.880380212840648));
#78359=CARTESIAN_POINT('Ctrl Pts',(0.0487055126520772,0.147734444401238,
-0.880198994134006));
#78360=CARTESIAN_POINT('Ctrl Pts',(0.0473977770678758,0.148159183077436,
-0.880099610653952));
#78361=CARTESIAN_POINT('Ctrl Pts',(0.0429029277076668,0.149553463774429,
-0.879757494595172));
#78362=CARTESIAN_POINT('Ctrl Pts',(0.0396905910409664,0.15043787298108,
-0.879512077143425));
#78363=CARTESIAN_POINT('Ctrl Pts',(0.0244892534603979,0.154102291398103,
-0.878345747661989));
#78364=CARTESIAN_POINT('Ctrl Pts',(0.0122272967379565,0.155555917668405,
-0.877385815592969));
#78365=CARTESIAN_POINT('Ctrl Pts',(-0.00395682392747703,0.155548108973284,
-0.876137357943913));
#78366=CARTESIAN_POINT('Ctrl Pts',(-0.00783742415145313,0.155400930795403,
-0.875839861719982));
#78367=CARTESIAN_POINT('Ctrl Pts',(-0.0141161428952155,0.154926969635022,
-0.875365066384795));
#78368=CARTESIAN_POINT('Ctrl Pts',(-0.0165192227783718,0.154689199107901,
-0.875184920615359));
#78369=CARTESIAN_POINT('Ctrl Pts',(-0.0198307495234539,0.154283483517612,
-0.874939683428125));
#78370=CARTESIAN_POINT('Ctrl Pts',(-0.0207445615505518,0.15416327445371,
-0.874872329212308));
#78371=CARTESIAN_POINT('Ctrl Pts',(-0.022297935207071,0.153944870448678,
-0.87475843765664));
#78372=CARTESIAN_POINT('Ctrl Pts',(-0.0229380407323316,0.153850795921362,
-0.874711681576258));
#78373=CARTESIAN_POINT('Ctrl Pts',(-0.0242864240581363,0.153644024918888,
-0.874613579798878));
#78374=CARTESIAN_POINT('Ctrl Pts',(-0.024994534615702,0.153530420701988,
-0.87456228389501));
#78375=CARTESIAN_POINT('Ctrl Pts',(-0.026945898851513,0.153203499061469,
-0.874421477394967));
#78376=CARTESIAN_POINT('Ctrl Pts',(-0.0281874157381815,0.1529799446005,
-0.874332510943112));
#78377=CARTESIAN_POINT('Ctrl Pts',(-0.0370025397288145,0.15128168122978,
-0.873704341384225));
#78378=CARTESIAN_POINT('Ctrl Pts',(-0.0444609586518216,0.149260146615439,
-0.873191099903673));
#78379=CARTESIAN_POINT('Ctrl Pts',(-0.0575259777953991,0.144652046449809,
-0.872276380153128));
#78380=CARTESIAN_POINT('Ctrl Pts',(-0.0631866447456239,0.142270514328931,
-0.871874391579915));
#78381=CARTESIAN_POINT('Ctrl Pts',(-0.0726669278005061,0.137604323624873,
-0.871171998524482));
#78382=CARTESIAN_POINT('Ctrl Pts',(-0.0765563933905407,0.135478952118518,
-0.870874802023289));
#78383=CARTESIAN_POINT('Ctrl Pts',(-0.0830527535334971,0.131559904896758,
-0.870357239933504));
#78384=CARTESIAN_POINT('Ctrl Pts',(-0.0857054190130834,0.129847400029952,
-0.870139485435968));
#78385=CARTESIAN_POINT('Ctrl Pts',(-0.089502773244607,0.127228835022822,
-0.869817003896838));
#78386=CARTESIAN_POINT('Ctrl Pts',(-0.0906898368429427,0.126385426850809,
-0.869714599276118));
#78387=CARTESIAN_POINT('Ctrl Pts',(-0.092777725646137,0.124857421873039,
-0.869531510048099));
#78388=CARTESIAN_POINT('Ctrl Pts',(-0.0936832633564158,0.124179419458814,
-0.869451082492525));
#78389=CARTESIAN_POINT('Ctrl Pts',(-0.0955837069435231,0.122723883948887,
-0.869280064118647));
#78390=CARTESIAN_POINT('Ctrl Pts',(-0.096576696592691,0.121943996271376,
-0.869189384796161));
#78391=CARTESIAN_POINT('Ctrl Pts',(-0.0992330214888864,0.11980494010852,
-0.868943136814336));
#78392=CARTESIAN_POINT('Ctrl Pts',(-0.100877821880938,0.118423310335433,
-0.868786681553506));
#78393=CARTESIAN_POINT('Ctrl Pts',(-0.112088202102204,0.10860356397806,
-0.867691708277005));
#78394=CARTESIAN_POINT('Ctrl Pts',(-0.1206110683486,0.0990522134992969,
-0.866705139288486));
#78395=CARTESIAN_POINT('Ctrl Pts',(-0.131646621599032,0.0831200044697117,
-0.8652044475045));
#78396=CARTESIAN_POINT('Ctrl Pts',(-0.135070139394415,0.0774328280398601,
-0.86469354213076));
#78397=CARTESIAN_POINT('Ctrl Pts',(-0.138855693315738,0.0701245624971615,
-0.864079780611562));
#78398=CARTESIAN_POINT('Ctrl Pts',(-0.1395690434261,0.0686938168425374,
-0.863961574871956));
#78399=CARTESIAN_POINT('Ctrl Pts',(-0.140599945018185,0.0665437847546757,
-0.863787096766562));
#78400=CARTESIAN_POINT('Ctrl Pts',(-0.140934281721406,0.0658327284511854,
-0.863729900603186));
#78401=CARTESIAN_POINT('Ctrl Pts',(-0.141502424124003,0.0646002549072531,
-0.863631673002615));
#78402=CARTESIAN_POINT('Ctrl Pts',(-0.141738759784731,0.0640800512791535,
-0.863590493218231));
#78403=CARTESIAN_POINT('Ctrl Pts',(-0.142290043716558,0.0628486349069057,
-0.863493670488512));
#78404=CARTESIAN_POINT('Ctrl Pts',(-0.142602531019311,0.0621363473822941,
-0.863438175058531));
#78405=CARTESIAN_POINT('Ctrl Pts',(-0.143524812051775,0.0599904799806183,
-0.863272423990894));
#78406=CARTESIAN_POINT('Ctrl Pts',(-0.144118447906321,0.0585500027093065,
-0.863163071607694));
#78407=CARTESIAN_POINT('Ctrl Pts',(-0.147946243807693,0.048850569272976,
-0.862437886456258));
#78408=CARTESIAN_POINT('Ctrl Pts',(-0.150490969000253,0.0403358387532395,
-0.861854293833215));
#78409=CARTESIAN_POINT('Ctrl Pts',(-0.154456532512761,0.0212537731323482,
-0.860570491332088));
#78410=CARTESIAN_POINT('Ctrl Pts',(-0.155546637215152,0.0106653881160218,
-0.859872051404209));
#78411=CARTESIAN_POINT('Ctrl Pts',(-0.155550662972886,-0.00207321574764465,
-0.858991922614664));
#78412=CARTESIAN_POINT('Ctrl Pts',(-0.155507896198807,-0.00419528657780355,
-0.85884408058168));
#78413=CARTESIAN_POINT('Ctrl Pts',(-0.155370685355025,-0.00757186267443317,
-0.858606536825204));
#78414=CARTESIAN_POINT('Ctrl Pts',(-0.155304416114564,-0.00882729527448303,
-0.858517709903541));
#78415=CARTESIAN_POINT('Ctrl Pts',(-0.155149559113993,-0.0112115388778581,
-0.858347982177621));
#78416=CARTESIAN_POINT('Ctrl Pts',(-0.155063848826277,-0.0123404603062701,
-0.858267176330289));
#78417=CARTESIAN_POINT('Ctrl Pts',(-0.154838926148483,-0.0149284097686903,
-0.858080873451588));
#78418=CARTESIAN_POINT('Ctrl Pts',(-0.154691402416279,-0.0163865864669549,
-0.857975123887429));
#78419=CARTESIAN_POINT('Ctrl Pts',(-0.154154765621627,-0.021034101086388,
-0.857635478570857));
#78420=CARTESIAN_POINT('Ctrl Pts',(-0.153687459278953,-0.0242133691343534,
-0.857399194350234));
#78421=CARTESIAN_POINT('Ctrl Pts',(-0.152322614182279,-0.0318474405099905,
-0.856821904163447));
#78422=CARTESIAN_POINT('Ctrl Pts',(-0.151327704693815,-0.0362816411973021,
-0.8564782751213));
#78423=CARTESIAN_POINT('Ctrl Pts',(-0.148559496246306,-0.0465020596157439,
-0.855668085080076));
#78424=CARTESIAN_POINT('Ctrl Pts',(-0.14663977828123,-0.0522411195865409,
-0.85519905851238));
#78425=CARTESIAN_POINT('Ctrl Pts',(-0.141556398189741,-0.0649282239794905,
-0.854140253815778));
#78426=CARTESIAN_POINT('Ctrl Pts',(-0.138205332782677,-0.0717857935177119,
-0.853552062493638));
#78427=CARTESIAN_POINT('Ctrl Pts',(-0.133731201897603,-0.0794565829015627,
-0.852893974340787));
#78428=CARTESIAN_POINT('Ctrl Pts',(-0.133084644076084,-0.0805348415629863,
-0.852801479481863));
#78429=CARTESIAN_POINT('Ctrl Pts',(-0.132049377513543,-0.0822148234197764,
-0.852657522278592));
#78430=CARTESIAN_POINT('Ctrl Pts',(-0.131669481939945,-0.0828218743580949,
-0.852605536468524));
#78431=CARTESIAN_POINT('Ctrl Pts',(-0.130938461524903,-0.0839722587121252,
-0.852507114644129));
#78432=CARTESIAN_POINT('Ctrl Pts',(-0.130588133545813,-0.0845160359553828,
-0.852460635436555));
#78433=CARTESIAN_POINT('Ctrl Pts',(-0.129729846967908,-0.0858301853310774,
-0.852348382684133));
#78434=CARTESIAN_POINT('Ctrl Pts',(-0.129218407138713,-0.0865982521501915,
-0.852282835621129));
#78435=CARTESIAN_POINT('Ctrl Pts',(-0.12733852067511,-0.0893676755047455,
-0.852046532388373));
#78436=CARTESIAN_POINT('Ctrl Pts',(-0.125930088463256,-0.0913416374443751,
-0.851878178488348));
#78437=CARTESIAN_POINT('Ctrl Pts',(-0.122133443362587,-0.0964079005467835,
-0.851443969903988));
#78438=CARTESIAN_POINT('Ctrl Pts',(-0.119673813856034,-0.0994446770489137,
-0.851181539686132));
#78439=CARTESIAN_POINT('Ctrl Pts',(-0.108884178413976,-0.111785166226848,
-0.850090792539563));
#78440=CARTESIAN_POINT('Ctrl Pts',(-0.0995647974595149,-0.120160454955035,
-0.849285448836767));
#78441=CARTESIAN_POINT('Ctrl Pts',(-0.0869332712028222,-0.129023584407323,
-0.848234002348013));
#78442=CARTESIAN_POINT('Ctrl Pts',(-0.0844746116981484,-0.130646535008912,
-0.84803122726872));
#78443=CARTESIAN_POINT('Ctrl Pts',(-0.0806125329624861,-0.133041267370624,
-0.847714492311786));
#78444=CARTESIAN_POINT('Ctrl Pts',(-0.0792407124934048,-0.133862871799446,
-0.847602325732475));
#78445=CARTESIAN_POINT('Ctrl Pts',(-0.0768688834660482,-0.135234162530654,
-0.847408822482591));
#78446=CARTESIAN_POINT('Ctrl Pts',(-0.0758750260699779,-0.13579427180251,
-0.847327866271435));
#78447=CARTESIAN_POINT('Ctrl Pts',(-0.0738223906530052,-0.136921508926426,
-0.84716087214164));
#78448=CARTESIAN_POINT('Ctrl Pts',(-0.0727630277661404,-0.137487405277673,
-0.847074797433248));
#78449=CARTESIAN_POINT('Ctrl Pts',(-0.0700536867930569,-0.138894612808811,
-0.846854879198575));
#78450=CARTESIAN_POINT('Ctrl Pts',(-0.0683950827528329,-0.139718805495557,
-0.846720452145391));
#78451=CARTESIAN_POINT('Ctrl Pts',(-0.0608172248132356,-0.143317127094337,
-0.846106918717946));
#78452=CARTESIAN_POINT('Ctrl Pts',(-0.0547421791731601,-0.145745690069455,
-0.845616403006151));
#78453=CARTESIAN_POINT('Ctrl Pts',(-0.0426330918047611,-0.149722366343413,
-0.844642642465732));
#78454=CARTESIAN_POINT('Ctrl Pts',(-0.0366225663557615,-0.151304817116957,
-0.844161154393155));
#78455=CARTESIAN_POINT('Ctrl Pts',(-0.0234821047226767,-0.153935421569936,
-0.843122885561882));
#78456=CARTESIAN_POINT('Ctrl Pts',(-0.0163401850692006,-0.154856519753629,
-0.842567370507838));
#78457=CARTESIAN_POINT('Ctrl Pts',(-0.00756115771862474,-0.155374370978998,
-0.841911547290137));
#78458=CARTESIAN_POINT('Ctrl Pts',(-0.00596131666418646,-0.15544397541448,
-0.841793143905305));
#78459=CARTESIAN_POINT('Ctrl Pts',(-0.00357461197005635,-0.155510909334888,
-0.841618427000853));
#78460=CARTESIAN_POINT('Ctrl Pts',(-0.00278843905428665,-0.155526992678888,
-0.841561186546572));
#78461=CARTESIAN_POINT('Ctrl Pts',(-0.00136746486178335,-0.155545284206716,
-0.841458327982413));
#78462=CARTESIAN_POINT('Ctrl Pts',(-0.000732740710060755,-0.155549569351714,
-0.841412603273821));
#78463=CARTESIAN_POINT('Ctrl Pts',(0.000712877770075411,-0.155550479842053,
-0.841308956398088));
#78464=CARTESIAN_POINT('Ctrl Pts',(0.00152374054465577,-0.155544650392086,
-0.841251168197913));
#78465=CARTESIAN_POINT('Ctrl Pts',(0.00406633944534416,-0.155506485953609,
-0.841070951163574));
#78466=CARTESIAN_POINT('Ctrl Pts',(0.00579767349409387,-0.155451567759823,
-0.84094967271617));
#78467=CARTESIAN_POINT('Ctrl Pts',(0.00995174313134238,-0.155250296299062,
-0.840661354013299));
#78468=CARTESIAN_POINT('Ctrl Pts',(0.0123727255873134,-0.155076138383495,
-0.840495505375031));
#78469=CARTESIAN_POINT('Ctrl Pts',(0.0222313210250158,-0.154134576357237,
-0.839825477031806));
#78470=CARTESIAN_POINT('Ctrl Pts',(0.0296134357082729,-0.152888059379158,
-0.839335812474905));
#78471=CARTESIAN_POINT('Ctrl Pts',(0.0454168440599835,-0.149031448714727,
-0.838263783535376));
#78472=CARTESIAN_POINT('Ctrl Pts',(0.0537630446269459,-0.146227808723351,
-0.837681688765196));
#78473=CARTESIAN_POINT('Ctrl Pts',(0.0638237060851255,-0.141869906694057,
-0.836927208658677));
#78474=CARTESIAN_POINT('Ctrl Pts',(0.065801645290444,-0.140963394445596,
-0.836776261977263));
#78475=CARTESIAN_POINT('Ctrl Pts',(0.0690114468421759,-0.13941002868216,
-0.836526568133483));
#78476=CARTESIAN_POINT('Ctrl Pts',(0.0702548354752405,-0.13878758504794,
-0.836428652226879));
#78477=CARTESIAN_POINT('Ctrl Pts',(0.072489241070864,-0.137631315881724,
-0.836250429825517));
#78478=CARTESIAN_POINT('Ctrl Pts',(0.0734831363574897,-0.137103237497877,
-0.836170328421121));
#78479=CARTESIAN_POINT('Ctrl Pts',(0.0756174819075255,-0.135939338152933,
-0.835996471681533));
#78480=CARTESIAN_POINT('Ctrl Pts',(0.0767558242897936,-0.135299853929816,
-0.835902591035302));
#78481=CARTESIAN_POINT('Ctrl Pts',(0.0799261440184571,-0.133465984963104,
-0.83563778955541));
#78482=CARTESIAN_POINT('Ctrl Pts',(0.081939142236088,-0.132239681979833,
-0.835465738952083));
#78483=CARTESIAN_POINT('Ctrl Pts',(0.0906653730638681,-0.12664798013438,
-0.834702041913793));
#78484=CARTESIAN_POINT('Ctrl Pts',(0.0970626604596442,-0.121814305874785,
-0.834093700797114));
#78485=CARTESIAN_POINT('Ctrl Pts',(0.109690555364888,-0.110644374858337,
-0.832793313323083));
#78486=CARTESIAN_POINT('Ctrl Pts',(0.11580949203002,-0.104222662220506,
-0.832101436562797));
#78487=CARTESIAN_POINT('Ctrl Pts',(0.123303788589299,-0.0948775090641157,
-0.831191149830478));
#78488=CARTESIAN_POINT('Ctrl Pts',(0.125184911314852,-0.0923813142306498,
-0.830956398470307));
#78489=CARTESIAN_POINT('Ctrl Pts',(0.12759024427023,-0.0889809725565789,
-0.830649248111102));
#78490=CARTESIAN_POINT('Ctrl Pts',(0.128182283630052,-0.0881259679657376,
-0.830573043999079));
#78491=CARTESIAN_POINT('Ctrl Pts',(0.129104033436509,-0.0867658613867691,
-0.830453513456204));
#78492=CARTESIAN_POINT('Ctrl Pts',(0.129439444153673,-0.0862646885010198,
-0.830409826392481));
#78493=CARTESIAN_POINT('Ctrl Pts',(0.130137006505214,-0.0852091571824253,
-0.830318584407875));
#78494=CARTESIAN_POINT('Ctrl Pts',(0.130498548045944,-0.0846544146276616,
-0.830271073253424));
#78495=CARTESIAN_POINT('Ctrl Pts',(0.131400067594264,-0.0832516391280894,
-0.830151995174289));
#78496=CARTESIAN_POINT('Ctrl Pts',(0.131935399757691,-0.0824006287165008,
-0.83008072386194));
#78497=CARTESIAN_POINT('Ctrl Pts',(0.134077117150483,-0.0789215798138939,
-0.829793010548335));
#78498=CARTESIAN_POINT('Ctrl Pts',(0.135613648893791,-0.0762511014932603,
-0.829580549374698));
#78499=CARTESIAN_POINT('Ctrl Pts',(0.139763116065837,-0.0685166148901526,
-0.8289835013209));
#78500=CARTESIAN_POINT('Ctrl Pts',(0.142178651599012,-0.063352155181564,
-0.828606352145697));
#78501=CARTESIAN_POINT('Ctrl Pts',(0.148540432715208,-0.0475419960390593,
-0.827482470307737));
#78502=CARTESIAN_POINT('Ctrl Pts',(0.151610870149014,-0.0365870505274984,
-0.826740838813642));
#78503=CARTESIAN_POINT('Ctrl Pts',(0.153837466405655,-0.0231322715663798,
-0.825801211634254));
#78504=CARTESIAN_POINT('Ctrl Pts',(0.15416195283639,-0.0208604751253779,
-0.825641729459637));
#78505=CARTESIAN_POINT('Ctrl Pts',(0.154592091199917,-0.01728565339994,
-0.825389025731491));
#78506=CARTESIAN_POINT('Ctrl Pts',(0.154731781255011,-0.0159869997163653,
-0.825296865463052));
#78507=CARTESIAN_POINT('Ctrl Pts',(0.154961357265479,-0.0135663856183572,
-0.825124339333427));
#78508=CARTESIAN_POINT('Ctrl Pts',(0.155055452413844,-0.0124449033596596,
-0.825044110568599));
#78509=CARTESIAN_POINT('Ctrl Pts',(0.155238532158182,-0.0099364073161369,
-0.824863946016108));
#78510=CARTESIAN_POINT('Ctrl Pts',(0.155321111762918,-0.00854903891208235,
-0.82476381742091));
#78511=CARTESIAN_POINT('Ctrl Pts',(0.155513415667156,-0.00437615359388857,
-0.824461100002319));
#78512=CARTESIAN_POINT('Ctrl Pts',(0.155566857721069,-0.00158874614488409,
-0.824256801477925));
#78513=CARTESIAN_POINT('Ctrl Pts',(0.155496884209671,0.00749315129874472,
-0.823583938968423));
#78514=CARTESIAN_POINT('Ctrl Pts',(0.155066333305595,0.01377836360493,-0.823106678952239));
#78515=CARTESIAN_POINT('Ctrl Pts',(0.152919902704755,0.0303172211991329,
-0.821824647418094));
#78516=CARTESIAN_POINT('Ctrl Pts',(0.15055571301723,0.0404550463541575,
-0.821010353685325));
#78517=CARTESIAN_POINT('Ctrl Pts',(0.14632315326996,0.0528458036152662,
-0.820019322710012));
#78518=CARTESIAN_POINT('Ctrl Pts',(0.145380374323205,0.055386759401077,
-0.819816472250009));
#78519=CARTESIAN_POINT('Ctrl Pts',(0.144003986368269,0.0588186179126531,
-0.819544167215913));
#78520=CARTESIAN_POINT('Ctrl Pts',(0.143627618025319,0.0597317786338072,
-0.819471876184374));
#78521=CARTESIAN_POINT('Ctrl Pts',(0.143011233789928,0.0611877570533963,
-0.81935694636979));
#78522=CARTESIAN_POINT('Ctrl Pts',(0.142776772713994,0.061732874618455,
-0.819313992284588));
#78523=CARTESIAN_POINT('Ctrl Pts',(0.142269406538304,0.0628941375601393,
-0.819222669364491));
#78524=CARTESIAN_POINT('Ctrl Pts',(0.141995603917309,0.0635098818342275,
-0.819174356815171));
#78525=CARTESIAN_POINT('Ctrl Pts',(0.141280289800332,0.0650907718646905,
-0.819050552115307));
#78526=CARTESIAN_POINT('Ctrl Pts',(0.140832877692933,0.0660532330223818,
-0.81897540577497));
#78527=CARTESIAN_POINT('Ctrl Pts',(0.138811969690908,0.070286656294552,
-0.81864554852775));
#78528=CARTESIAN_POINT('Ctrl Pts',(0.13713398627255,0.0735068137515336,
-0.818396434174411));
#78529=CARTESIAN_POINT('Ctrl Pts',(0.13156671691883,0.0833352189627264,
-0.817632567730148));
#78530=CARTESIAN_POINT('Ctrl Pts',(0.127300638355638,0.0897169034577439,
-0.817131026333492));
#78531=CARTESIAN_POINT('Ctrl Pts',(0.116868924342838,0.103070635427417,
-0.816013980553107));
#78532=CARTESIAN_POINT('Ctrl Pts',(0.110514645519303,0.109856189988094,
-0.815398286312547));
#78533=CARTESIAN_POINT('Ctrl Pts',(0.103178831595365,0.116405503386327,
-0.814717693594607));
#78534=CARTESIAN_POINT('Ctrl Pts',(0.102761515737733,0.116774069697995,
-0.814679076198737));
#78535=CARTESIAN_POINT('Ctrl Pts',(0.102342242814364,0.117140376624483,
-0.814640372754811));
#78536=CARTESIAN_POINT('Origin',(0.,0.,-1.10400562256037));
#78537=CARTESIAN_POINT('',(0.10234224283772,0.117140376604078,-0.730690163752328));
#78538=CARTESIAN_POINT('',(0.102342226135012,0.11714039119676,-0.744524458909986));
#78539=CARTESIAN_POINT('',(0.10234224283772,0.117140376604078,-1.10400562256037));
#78540=CARTESIAN_POINT('',(-0.155549988636594,5.94571726719256E-5,-0.775194377434571));
#78541=CARTESIAN_POINT('Ctrl Pts',(-0.155549988636594,5.94571726719256E-5,
-0.775194377434571));
#78542=CARTESIAN_POINT('Ctrl Pts',(-0.15555386600914,-0.0100844031602943,
-0.774463862461081));
#78543=CARTESIAN_POINT('Ctrl Pts',(-0.154561163212359,-0.0202683545329286,
-0.773733347487591));
#78544=CARTESIAN_POINT('Ctrl Pts',(-0.152574549297427,-0.0302788607230699,
-0.7730028325141));
#78545=CARTESIAN_POINT('Ctrl Pts',(-0.150590323408965,-0.0402773336975079,
-0.772273195662463));
#78546=CARTESIAN_POINT('Ctrl Pts',(-0.147614646911284,-0.0501018361313886,
-0.771543558810827));
#78547=CARTESIAN_POINT('Ctrl Pts',(-0.143701919267921,-0.0595446126758421,
-0.77081392195919));
#78548=CARTESIAN_POINT('Ctrl Pts',(-0.139792442521125,-0.0689795436729801,
-0.7700848913276));
#78549=CARTESIAN_POINT('Ctrl Pts',(-0.134947811940159,-0.0780325003649032,
-0.769355860696011));
#78550=CARTESIAN_POINT('Ctrl Pts',(-0.129270866042447,-0.0865150027026283,
-0.768626830064421));
#78551=CARTESIAN_POINT('Ctrl Pts',(-0.123580591224642,-0.0950174211357128,
-0.767896087739395));
#78552=CARTESIAN_POINT('Ctrl Pts',(-0.117054652334967,-0.102945937307198,
-0.767165345414368));
#78553=CARTESIAN_POINT('Ctrl Pts',(-0.109838640819849,-0.110142069541335,
-0.766434603089342));
#78554=CARTESIAN_POINT('Ctrl Pts',(-0.104564595969931,-0.115401585004865,
-0.765900517495403));
#78555=CARTESIAN_POINT('Ctrl Pts',(-0.0989228665778733,-0.120270514573088,
-0.765366431901464));
#78556=CARTESIAN_POINT('Ctrl Pts',(-0.0929813870164388,-0.124700698348082,
-0.764832346307525));
#78557=CARTESIAN_POINT('Ctrl Pts',(-0.0847762750881243,-0.130818728943149,
-0.764094780515662));
#78558=CARTESIAN_POINT('Ctrl Pts',(-0.0759342485538406,-0.136146198466278,
-0.763357214723798));
#78559=CARTESIAN_POINT('Ctrl Pts',(-0.0666312496326838,-0.140556319930436,
-0.762619648931935));
#78560=CARTESIAN_POINT('Ctrl Pts',(-0.0573061358502367,-0.144976925027374,
-0.761880329816727));
#78561=CARTESIAN_POINT('Ctrl Pts',(-0.0475186300913685,-0.148475284583797,
-0.76114101070152));
#78562=CARTESIAN_POINT('Ctrl Pts',(-0.0374732079475383,-0.150968742414185,
-0.760401691586313));
#78563=CARTESIAN_POINT('Ctrl Pts',(-0.0274744847389166,-0.153450608713227,
-0.759665809401377));
#78564=CARTESIAN_POINT('Ctrl Pts',(-0.0172211422329046,-0.154936667906122,
-0.758929927216442));
#78565=CARTESIAN_POINT('Ctrl Pts',(-0.00692912148693312,-0.155395591235464,
-0.758194045031506));
#78566=CARTESIAN_POINT('Ctrl Pts',(0.0034350024266058,-0.15585772965993,
-0.757453007451163));
#78567=CARTESIAN_POINT('Ctrl Pts',(0.0138374003939213,-0.155278229143345,
-0.756711969870819));
#78568=CARTESIAN_POINT('Ctrl Pts',(0.0240570027497603,-0.153678440643761,
-0.755970932290476));
#78569=CARTESIAN_POINT('Ctrl Pts',(0.0342766051055992,-0.152078652144177,
-0.755229894710133));
#78570=CARTESIAN_POINT('Ctrl Pts',(0.0443124994057009,-0.149458849024487,
-0.754488857129789));
#78571=CARTESIAN_POINT('Ctrl Pts',(0.0539571410731116,-0.145891841537546,
-0.753747819549446));
#78572=CARTESIAN_POINT('Ctrl Pts',(0.0635565972037738,-0.142341545625118,
-0.753010253760173));
#78573=CARTESIAN_POINT('Ctrl Pts',(0.0728398182548613,-0.13782655163654,
-0.7522726879709));
#78574=CARTESIAN_POINT('Ctrl Pts',(0.0816046551225161,-0.132425385641633,
-0.751535122181627));
#78575=CARTESIAN_POINT('Ctrl Pts',(0.0903903275843545,-0.12701138010339,
-0.750795803065772));
#78576=CARTESIAN_POINT('Ctrl Pts',(0.0986542812351905,-0.120707344980565,
-0.750056483949917));
#78577=CARTESIAN_POINT('Ctrl Pts',(0.106215842921805,-0.113639769501748,
-0.749317164834062));
#78578=CARTESIAN_POINT('Ctrl Pts',(0.11374225254917,-0.106605049647507,
-0.748581282652327));
#78579=CARTESIAN_POINT('Ctrl Pts',(0.120572102713786,-0.0988145072758199,
-0.747845400470592));
#78580=CARTESIAN_POINT('Ctrl Pts',(0.126561526551945,-0.0904321983413054,
-0.747109518288857));
#78581=CARTESIAN_POINT('Ctrl Pts',(0.132592910752094,-0.0819911651076437,
-0.746368480705942));
#78582=CARTESIAN_POINT('Ctrl Pts',(0.137771484362896,-0.0729508066652424,
-0.745627443123026));
#78583=CARTESIAN_POINT('Ctrl Pts',(0.141994771738795,-0.0635081671822421,
-0.744886405540111));
#78584=CARTESIAN_POINT('Ctrl Pts',(0.146218059114693,-0.0540655276992418,
-0.744145367957196));
#78585=CARTESIAN_POINT('Ctrl Pts',(0.149485792662233,-0.0442215213286015,
-0.74340433037428));
#78586=CARTESIAN_POINT('Ctrl Pts',(0.151746022211242,-0.0341898704745336,
-0.742663292791365));
#78587=CARTESIAN_POINT('Ctrl Pts',(0.153995662520478,-0.0242052181902564,
-0.741925726990618));
#78588=CARTESIAN_POINT('Ctrl Pts',(0.15526397707335,-0.01396047585451,-0.741188161189871));
#78589=CARTESIAN_POINT('Ctrl Pts',(0.155506747828537,-0.00366795307928527,
-0.740450595389125));
#78590=CARTESIAN_POINT('Ctrl Pts',(0.155750095688758,0.00664903667386102,
-0.739711276276138));
#78591=CARTESIAN_POINT('Ctrl Pts',(0.154962848460286,0.0170131106572213,
-0.738971957163151));
#78592=CARTESIAN_POINT('Ctrl Pts',(0.153152710900332,0.0272038534748175,
-0.738232638050165));
#78593=CARTESIAN_POINT('Ctrl Pts',(0.151350988240431,0.0373472219468521,
-0.737496755856328));
#78594=CARTESIAN_POINT('Ctrl Pts',(0.148536024465825,0.0473179483910715,
-0.73676087366249));
#78595=CARTESIAN_POINT('Ctrl Pts',(0.144767075467698,0.0569060309679909,
-0.736024991468653));
#78596=CARTESIAN_POINT('Ctrl Pts',(0.140971722298303,0.0665612848901873,
-0.735283953896092));
#78597=CARTESIAN_POINT('Ctrl Pts',(0.136209300468937,0.0758276239839394,
-0.734542916323531));
#78598=CARTESIAN_POINT('Ctrl Pts',(0.130589273582521,0.0845117987336059,
-0.733801878750969));
#78599=CARTESIAN_POINT('Ctrl Pts',(0.124969246696105,0.0931959734832724,
-0.733060841178408));
#78600=CARTESIAN_POINT('Ctrl Pts',(0.118492235761233,0.101297261649368,
-0.732319803605846));
#78601=CARTESIAN_POINT('Ctrl Pts',(0.11130920650138,0.108655708768721,-0.731578766033285));
#78602=CARTESIAN_POINT('Ctrl Pts',(0.108438071747974,0.111596959944399,
-0.731282565272966));
#78603=CARTESIAN_POINT('Ctrl Pts',(0.105446013534655,0.114428699694826,
-0.730986364512647));
#78604=CARTESIAN_POINT('Ctrl Pts',(0.10234224283772,0.117140376604078,-0.730690163752328));
#78605=CARTESIAN_POINT('Ctrl Pts',(0.10234224283772,0.117140376604078,-0.800700826369366));
#78606=CARTESIAN_POINT('Ctrl Pts',(0.0945830959428436,0.123919324382374,
-0.79996324687108));
#78607=CARTESIAN_POINT('Ctrl Pts',(0.0861632602065998,0.129910446345868,
-0.799225667372795));
#78608=CARTESIAN_POINT('Ctrl Pts',(0.0772687420922595,0.135001274051321,
-0.79848808787451));
#78609=CARTESIAN_POINT('Ctrl Pts',(0.0756521792171102,0.135926522948071,
-0.798354034110262));
#78610=CARTESIAN_POINT('Ctrl Pts',(0.0740199996624193,0.136822156691536,
-0.798219980346014));
#78611=CARTESIAN_POINT('Ctrl Pts',(0.072373396601727,0.137687668163598,
-0.798085926581766));
#78612=CARTESIAN_POINT('Ctrl Pts',(0.0633137622828552,0.142449725044736,
-0.797348360794268));
#78613=CARTESIAN_POINT('Ctrl Pts',(0.0537484429186352,0.146331481039621,
-0.796610795006771));
#78614=CARTESIAN_POINT('Ctrl Pts',(0.0438710170354423,0.149235171337979,
-0.795873229219274));
#78615=CARTESIAN_POINT('Ctrl Pts',(0.0339701107040233,0.152145764239355,
-0.795133910102975));
#78616=CARTESIAN_POINT('Ctrl Pts',(0.0237564602461081,0.154073232376168,
-0.794394590986676));
#78617=CARTESIAN_POINT('Ctrl Pts',(0.0134449381321283,0.154967855178496,
-0.793655271870377));
#78618=CARTESIAN_POINT('Ctrl Pts',(0.00318135204152644,0.155858319074011,
-0.792919389687835));
#78619=CARTESIAN_POINT('Ctrl Pts',(-0.00717826886897367,0.155725435483212,
-0.792183507505293));
#78620=CARTESIAN_POINT('Ctrl Pts',(-0.017415740338501,0.154571971872206,
-0.791447625322752));
#78621=CARTESIAN_POINT('Ctrl Pts',(-0.0277249328908003,0.153410427392855,
-0.790706587739574));
#78622=CARTESIAN_POINT('Ctrl Pts',(-0.0379093125922557,0.151214040730291,
-0.789965550156396));
#78623=CARTESIAN_POINT('Ctrl Pts',(-0.0477538536585732,0.148038413801133,
-0.789224512573219));
#78624=CARTESIAN_POINT('Ctrl Pts',(-0.0575983947248908,0.144862786871975,
-0.788483474990041));
#78625=CARTESIAN_POINT('Ctrl Pts',(-0.0671022385762959,0.140708332135486,
-0.787742437406863));
#78626=CARTESIAN_POINT('Ctrl Pts',(-0.0760717523565394,0.135679368340973,
-0.787001399823686));
#78627=CARTESIAN_POINT('Ctrl Pts',(-0.0849992430142917,0.130673965774717,
-0.786263834080107));
#78628=CARTESIAN_POINT('Ctrl Pts',(-0.0934637703868424,0.124765063504695,
-0.785526268336529));
#78629=CARTESIAN_POINT('Ctrl Pts',(-0.101277923274961,0.118061783643613,
-0.784788702592951));
#78630=CARTESIAN_POINT('Ctrl Pts',(-0.109110652416689,0.111342568360163,
-0.784049383465672));
#78631=CARTESIAN_POINT('Ctrl Pts',(-0.116289110998618,0.103825685675319,
-0.783310064338393));
#78632=CARTESIAN_POINT('Ctrl Pts',(-0.122654588270765,0.0956642800429139,
-0.782570745211114));
#78633=CARTESIAN_POINT('Ctrl Pts',(-0.128990473306033,0.0875408156737357,
-0.781834863077765));
#78634=CARTESIAN_POINT('Ctrl Pts',(-0.134520343035544,0.0787795411156073,
-0.781098980944416));
#78635=CARTESIAN_POINT('Ctrl Pts',(-0.139127706543723,0.0695649608055928,
-0.780363098811067));
#78636=CARTESIAN_POINT('Ctrl Pts',(-0.143767348618724,0.0602858243897395,
-0.779622061186824));
#78637=CARTESIAN_POINT('Ctrl Pts',(-0.147471071797916,0.0505478495391549,
-0.77888102356258));
#78638=CARTESIAN_POINT('Ctrl Pts',(-0.150168418866794,0.0405616626267601,
-0.778139985938336));
#78639=CARTESIAN_POINT('Ctrl Pts',(-0.152865765935671,0.0305754757143654,
-0.777398948314093));
#78640=CARTESIAN_POINT('Ctrl Pts',(-0.15455661529663,0.0203420214609023,
-0.776657910689849));
#78641=CARTESIAN_POINT('Ctrl Pts',(-0.155223019478323,0.0100805120917568,
-0.775916873065605));
#78642=CARTESIAN_POINT('Ctrl Pts',(-0.155439596023901,0.00674559566620943,
-0.77567604119028));
#78643=CARTESIAN_POINT('Ctrl Pts',(-0.155548710365706,0.00340362539228194,
-0.775435209314955));
#78644=CARTESIAN_POINT('Ctrl Pts',(-0.155549988636567,5.94572429166567E-5,
-0.77519437743963));
#78645=CARTESIAN_POINT('',(-0.155549929833988,-0.000141245247018929,-0.789026374106901));
#78646=CARTESIAN_POINT('Ctrl Pts',(0.102342242814364,0.117140376624483,
-0.814640372754811));
#78647=CARTESIAN_POINT('Ctrl Pts',(0.101247987115879,0.118096396961982,
-0.814539361070758));
#78648=CARTESIAN_POINT('Ctrl Pts',(0.100140400890045,0.119037027434954,
-0.814437762401209));
#78649=CARTESIAN_POINT('Ctrl Pts',(0.0980683028869122,0.120747392027465,
-0.81424874066824));
#78650=CARTESIAN_POINT('Ctrl Pts',(0.097107512032578,0.121521420591653,
-0.814161500428143));
#78651=CARTESIAN_POINT('Ctrl Pts',(0.0952423368108456,0.122987791192865,
-0.81399284801475));
#78652=CARTESIAN_POINT('Ctrl Pts',(0.0943393533588697,0.123681792456681,
-0.813911508780979));
#78653=CARTESIAN_POINT('Ctrl Pts',(0.0922173013781256,0.125275967722571,
-0.813721023289307));
#78654=CARTESIAN_POINT('Ctrl Pts',(0.0909925561961174,0.126168352526021,
-0.813611585108866));
#78655=CARTESIAN_POINT('Ctrl Pts',(0.0868837031025962,0.129071236516884,
-0.813245951189801));
#78656=CARTESIAN_POINT('Ctrl Pts',(0.0839446808462585,0.131001713317316,
-0.812986820087241));
#78657=CARTESIAN_POINT('Ctrl Pts',(0.0765225369886381,0.135524537521265,
-0.812337797865434));
#78658=CARTESIAN_POINT('Ctrl Pts',(0.0719707794888592,0.137995640176101,
-0.811944305583081));
#78659=CARTESIAN_POINT('Ctrl Pts',(0.0580641705603296,0.144670006263189,
-0.810758696607579));
#78660=CARTESIAN_POINT('Ctrl Pts',(0.0484080750056315,0.148180695886636,
-0.809955167656746));
#78661=CARTESIAN_POINT('Ctrl Pts',(0.0357238872036029,0.151418885865566,
-0.808963026583044));
#78662=CARTESIAN_POINT('Ctrl Pts',(0.0329519874985958,0.152046190829675,
-0.80875007282081));
#78663=CARTESIAN_POINT('Ctrl Pts',(0.0291782851967918,0.152792147350082,
-0.808466653849693));
#78664=CARTESIAN_POINT('Ctrl Pts',(0.028190416146552,0.15297749245713,-0.808393059295612));
#78665=CARTESIAN_POINT('Ctrl Pts',(0.0266134420730029,0.153257570955974,
-0.80827660097801));
#78666=CARTESIAN_POINT('Ctrl Pts',(0.0260254897585766,0.153358508956619,
-0.808233407028251));
#78667=CARTESIAN_POINT('Ctrl Pts',(0.0247764292561043,0.153565553883757,
-0.808142144143772));
#78668=CARTESIAN_POINT('Ctrl Pts',(0.0241151862038325,0.153670779979575,
-0.808094127178692));
#78669=CARTESIAN_POINT('Ctrl Pts',(0.0224240763594421,0.153928708106129,
-0.807972035005134));
#78670=CARTESIAN_POINT('Ctrl Pts',(0.0213932958912589,0.154075349832642,
-0.807898287230063));
#78671=CARTESIAN_POINT('Ctrl Pts',(0.0169715942593336,0.154659162060053,
-0.807584500646974));
#78672=CARTESIAN_POINT('Ctrl Pts',(0.0135679637438788,0.154994857779847,
-0.807349407302497));
#78673=CARTESIAN_POINT('Ctrl Pts',(0.00332708986492769,0.155664906549473,
-0.806653897580513));
#78674=CARTESIAN_POINT('Ctrl Pts',(-0.00352409285299623,0.155660613162722,
-0.806204126969112));
#78675=CARTESIAN_POINT('Ctrl Pts',(-0.0199791529533464,0.154562960106711,
-0.805117866157702));
#78676=CARTESIAN_POINT('Ctrl Pts',(-0.0295234485217771,0.153026834034583,
-0.804481723355181));
#78677=CARTESIAN_POINT('Ctrl Pts',(-0.040956746243398,0.150076717431665,
-0.803669014212957));
#78678=CARTESIAN_POINT('Ctrl Pts',(-0.0430384737204866,0.149493027210443,
-0.803518998861588));
#78679=CARTESIAN_POINT('Ctrl Pts',(-0.0464341781460082,0.148464109851312,
-0.803270523055676));
#78680=CARTESIAN_POINT('Ctrl Pts',(-0.0477556039096431,0.148044340958285,
-0.80317287967734));
#78681=CARTESIAN_POINT('Ctrl Pts',(-0.0501389954308398,0.147251994300334,
-0.802994943111323));
#78682=CARTESIAN_POINT('Ctrl Pts',(-0.0512028761965604,0.146885445284617,
-0.80291485185034));
#78683=CARTESIAN_POINT('Ctrl Pts',(-0.0534953528867185,0.1460676644918,
-0.802740775802747));
#78684=CARTESIAN_POINT('Ctrl Pts',(-0.0547224094469159,0.145612407101328,
-0.802646663127608));
#78685=CARTESIAN_POINT('Ctrl Pts',(-0.0581571172396773,0.144288530681654,
-0.802380499465904));
#78686=CARTESIAN_POINT('Ctrl Pts',(-0.0603507658864985,0.143384846785658,
-0.802207299846554));
#78687=CARTESIAN_POINT('Ctrl Pts',(-0.0699657033930099,0.139164199672636,
-0.801433390857135));
#78688=CARTESIAN_POINT('Ctrl Pts',(-0.0771399352777933,0.135319132107625,
-0.800815449785842));
#78689=CARTESIAN_POINT('Ctrl Pts',(-0.0916372093746799,0.126020546836185,
-0.799486427765102));
#78690=CARTESIAN_POINT('Ctrl Pts',(-0.0988489298787561,0.120446894595726,
-0.798775394045735));
#78691=CARTESIAN_POINT('Ctrl Pts',(-0.107600153025353,0.112365172782629,
-0.797872836036262));
#78692=CARTESIAN_POINT('Ctrl Pts',(-0.109615917275998,0.110399629145226,
-0.797661919819693));
#78693=CARTESIAN_POINT('Ctrl Pts',(-0.112275236374755,0.107661864106398,
-0.797380736848244));
#78694=CARTESIAN_POINT('Ctrl Pts',(-0.112966170103791,0.106936664613663,
-0.797307400789476));
#78695=CARTESIAN_POINT('Ctrl Pts',(-0.114056935431468,0.1057694335537,-0.797191246418278));
#78696=CARTESIAN_POINT('Ctrl Pts',(-0.114461300448228,0.105331706177061,
-0.797148100879334));
#78697=CARTESIAN_POINT('Ctrl Pts',(-0.115315185736076,0.104396646546545,
-0.797056830079302));
#78698=CARTESIAN_POINT('Ctrl Pts',(-0.115764027862494,0.103898709158497,
-0.797008757626578));
#78699=CARTESIAN_POINT('Ctrl Pts',(-0.116812393927484,0.10272044267184,
-0.796896201714844));
#78700=CARTESIAN_POINT('Ctrl Pts',(-0.117409224795774,0.102037732011308,
-0.796831910585526));
#78701=CARTESIAN_POINT('Ctrl Pts',(-0.119320645519724,0.0998122936287535,
-0.79662516157429));
#78702=CARTESIAN_POINT('Ctrl Pts',(-0.120611122538167,0.0982490126800226,
-0.796484252002993));
#78703=CARTESIAN_POINT('Ctrl Pts',(-0.122382151175805,0.0960160863864426,
-0.796288231891698));
#78704=CARTESIAN_POINT('Ctrl Pts',(-0.122888437734998,0.0953672464496936,
-0.796231878543083));
#78705=CARTESIAN_POINT('Ctrl Pts',(-0.126446090409272,0.0907325006148665,
-0.795833370166034));
#78706=CARTESIAN_POINT('Ctrl Pts',(-0.129308308145013,0.0866046719690133,
-0.795499378150036));
#78707=CARTESIAN_POINT('Ctrl Pts',(-0.137060632348669,0.0741808571452341,
-0.794531469747891));
#78708=CARTESIAN_POINT('Ctrl Pts',(-0.141386272580957,0.0655616365079737,
-0.793904277177543));
#78709=CARTESIAN_POINT('Ctrl Pts',(-0.146358028189157,0.0528342593432668,
-0.792980698981075));
#78710=CARTESIAN_POINT('Ctrl Pts',(-0.147681003810113,0.049014773027456,
-0.792704063434883));
#78711=CARTESIAN_POINT('Ctrl Pts',(-0.149328838784549,0.0435818773564268,
-0.792308650382566));
#78712=CARTESIAN_POINT('Ctrl Pts',(-0.149779191414869,0.0420080419823773,
-0.792193890879958));
#78713=CARTESIAN_POINT('Ctrl Pts',(-0.150502804418005,0.0393195215335305,
-0.791997333286324));
#78714=CARTESIAN_POINT('Ctrl Pts',(-0.150788725864499,0.0382083621246268,
-0.791915947757818));
#78715=CARTESIAN_POINT('Ctrl Pts',(-0.151346192988089,0.0359381325070211,
-0.791749312714464));
#78716=CARTESIAN_POINT('Ctrl Pts',(-0.151616776667209,0.0347789072338163,
-0.791664038493042));
#78717=CARTESIAN_POINT('Ctrl Pts',(-0.152134325830938,0.0324407173661172,
-0.791491615906685));
#78718=CARTESIAN_POINT('Ctrl Pts',(-0.152380954422049,0.0312617628735881,
-0.791404463267835));
#78719=CARTESIAN_POINT('Ctrl Pts',(-0.15294585172281,0.0283957093218414,
-0.791192031437218));
#78720=CARTESIAN_POINT('Ctrl Pts',(-0.153249921783962,0.0267060088715932,
-0.791066319562526));
#78721=CARTESIAN_POINT('Ctrl Pts',(-0.154880940457497,0.0166945391990566,
-0.790318513571554));
#78722=CARTESIAN_POINT('Ctrl Pts',(-0.155557588103049,0.00828257885722836,
-0.789676994178376));
#78723=CARTESIAN_POINT('Ctrl Pts',(-0.155549935820354,-0.000141302101484485,
-0.789026380191115));
#78724=CARTESIAN_POINT('Ctrl Pts',(-0.155549935871255,-0.000141246056687843,
-0.789026384519706));
#78725=CARTESIAN_POINT('Ctrl Pts',(-0.155540361813676,-0.0106848610596033,
-0.788212054034337));
#78726=CARTESIAN_POINT('Ctrl Pts',(-0.15445882295033,-0.0212010662537019,
-0.787386500385918));
#78727=CARTESIAN_POINT('Ctrl Pts',(-0.152093774235884,-0.0326273994928223,
-0.786516650549246));
#78728=CARTESIAN_POINT('Ctrl Pts',(-0.151854274310337,-0.033724514967364,
-0.786433438329619));
#78729=CARTESIAN_POINT('Ctrl Pts',(-0.151387612508525,-0.0357563748508333,
-0.786280015877868));
#78730=CARTESIAN_POINT('Ctrl Pts',(-0.151163621620343,-0.0366917863787319,
-0.786209656527296));
#78731=CARTESIAN_POINT('Ctrl Pts',(-0.150772843442499,-0.0382593713036209,
-0.786092271465715));
#78732=CARTESIAN_POINT('Ctrl Pts',(-0.15061072380648,-0.0388926696503636,
-0.786044993520268));
#78733=CARTESIAN_POINT('Ctrl Pts',(-0.150266476782737,-0.0402029838497188,
-0.785947498336013));
#78734=CARTESIAN_POINT('Ctrl Pts',(-0.150083757949649,-0.0408798190591607,
-0.785897314452474));
#78735=CARTESIAN_POINT('Ctrl Pts',(-0.149579387694897,-0.0426991564627536,
-0.78576283827918));
#78736=CARTESIAN_POINT('Ctrl Pts',(-0.149249217960623,-0.043839278603837,
-0.785679012369898));
#78737=CARTESIAN_POINT('Ctrl Pts',(-0.147493071270416,-0.0496535661741509,
-0.785253278113192));
#78738=CARTESIAN_POINT('Ctrl Pts',(-0.145860302366329,-0.0542629286958753,
-0.784921564565051));
#78739=CARTESIAN_POINT('Ctrl Pts',(-0.140804862483097,-0.0666471977348302,
-0.784026898361794));
#78740=CARTESIAN_POINT('Ctrl Pts',(-0.136958713094505,-0.0742305790355904,
-0.78347456109652));
#78741=CARTESIAN_POINT('Ctrl Pts',(-0.128887350463018,-0.0873600570599175,
-0.782452563088397));
#78742=CARTESIAN_POINT('Ctrl Pts',(-0.124872549919944,-0.0930083740591326,
-0.781987736428872));
#78743=CARTESIAN_POINT('Ctrl Pts',(-0.119239431260928,-0.0999084792263256,
-0.781371409933041));
#78744=CARTESIAN_POINT('Ctrl Pts',(-0.117954269111278,-0.101422561448616,
-0.781232939892915));
#78745=CARTESIAN_POINT('Ctrl Pts',(-0.116592486349677,-0.102966013317513,
-0.781088197856267));
#78746=CARTESIAN_POINT('Ctrl Pts',(-0.116544412000777,-0.103020424203474,
-0.781083090606553));
#78747=CARTESIAN_POINT('Ctrl Pts',(-0.116448794084408,-0.103128492647877,
-0.781072937459522));
#78748=CARTESIAN_POINT('Ctrl Pts',(-0.116401251481458,-0.103182151039102,
-0.781067891602064));
#78749=CARTESIAN_POINT('Ctrl Pts',(-0.116306096630273,-0.103289396964021,
-0.781057797343336));
#78750=CARTESIAN_POINT('Ctrl Pts',(-0.116258484400569,-0.103342984490548,
-0.781052748943587));
#78751=CARTESIAN_POINT('Ctrl Pts',(-0.116162552829664,-0.103450805197948,
-0.78104258202524));
#78752=CARTESIAN_POINT('Ctrl Pts',(-0.116114232511959,-0.103505037481928,
-0.781037463467647));
#78753=CARTESIAN_POINT('Ctrl Pts',(-0.116016173118801,-0.103614939308742,
-0.781027081064067));
#78754=CARTESIAN_POINT('Ctrl Pts',(-0.115966431922367,-0.103670606925235,
-0.781021817132265));
#78755=CARTESIAN_POINT('Ctrl Pts',(-0.115864695375924,-0.103784300045495,
-0.781011056018143));
#78756=CARTESIAN_POINT('Ctrl Pts',(-0.115812696472497,-0.103842322326781,
-0.781005558691186));
#78757=CARTESIAN_POINT('Ctrl Pts',(-0.115705414504048,-0.103961850664916,
-0.78099422262899));
#78758=CARTESIAN_POINT('Ctrl Pts',(-0.115650125949224,-0.104023351739451,
-0.780988383669284));
#78759=CARTESIAN_POINT('Ctrl Pts',(-0.115534932447873,-0.10415128365,-0.780976224775889));
#78760=CARTESIAN_POINT('Ctrl Pts',(-0.115475019207543,-0.104217706943855,
-0.780969904501767));
#78761=CARTESIAN_POINT('Ctrl Pts',(-0.114649175765539,-0.105131698443217,
-0.780882836392923));
#78762=CARTESIAN_POINT('Ctrl Pts',(-0.113874007494642,-0.105970834725577,
-0.780801707822105));
#78763=CARTESIAN_POINT('Ctrl Pts',(-0.112249175796799,-0.107691334773083,
-0.780632823909134));
#78764=CARTESIAN_POINT('Ctrl Pts',(-0.111398212217701,-0.108571355381265,
-0.780545016185137));
#78765=CARTESIAN_POINT('Ctrl Pts',(-0.109155225321393,-0.110836799659655,
-0.780315155031285));
#78766=CARTESIAN_POINT('Ctrl Pts',(-0.107747233539381,-0.11220602651901,
-0.780172409007194));
#78767=CARTESIAN_POINT('Ctrl Pts',(-0.100563045108552,-0.118932493504905,
-0.779451315632692));
#78768=CARTESIAN_POINT('Ctrl Pts',(-0.0944125420257412,-0.123871304973134,
-0.778856016829919));
#78769=CARTESIAN_POINT('Ctrl Pts',(-0.0820500672480588,-0.132340997422237,
-0.777703411444543));
#78770=CARTESIAN_POINT('Ctrl Pts',(-0.0759160979816154,-0.135952549266159,
-0.777149526854872));
#78771=CARTESIAN_POINT('Ctrl Pts',(-0.0646969383402677,-0.141561403034217,
-0.776182943557273));
#78772=CARTESIAN_POINT('Ctrl Pts',(-0.0597124762297606,-0.143735026533935,
-0.77576852311152));
#78773=CARTESIAN_POINT('Ctrl Pts',(-0.053514326589391,-0.146059658514288,
-0.775278701711074));
#78774=CARTESIAN_POINT('Ctrl Pts',(-0.0523999236604124,-0.146463153121103,
-0.775191614930757));
#78775=CARTESIAN_POINT('Ctrl Pts',(-0.050619487413628,-0.147084876565803,
-0.775054152215269));
#78776=CARTESIAN_POINT('Ctrl Pts',(-0.0499564302855662,-0.147311399915856,
-0.775003325200406));
#78777=CARTESIAN_POINT('Ctrl Pts',(-0.0486788244400447,-0.147738256041039,
-0.774906121333233));
#78778=CARTESIAN_POINT('Ctrl Pts',(-0.0480645264175407,-0.147939249579884,
-0.774859709962524));
#78779=CARTESIAN_POINT('Ctrl Pts',(-0.0465378184976351,-0.148428263307493,
-0.774745133454824));
#78780=CARTESIAN_POINT('Ctrl Pts',(-0.0456239496969946,-0.148711711830498,
-0.774677226394651));
#78781=CARTESIAN_POINT('Ctrl Pts',(-0.0423337696441344,-0.149699019311516,
-0.774434968570961));
#78782=CARTESIAN_POINT('Ctrl Pts',(-0.0399431932220235,-0.150354539262761,
-0.77426309639432));
#78783=CARTESIAN_POINT('Ctrl Pts',(-0.0284462463219715,-0.153213515720549,
-0.773451669167112));
#78784=CARTESIAN_POINT('Ctrl Pts',(-0.019168107651984,-0.154648600244095,
-0.772840966160701));
#78785=CARTESIAN_POINT('Ctrl Pts',(-0.00157081811658123,-0.15576134675307,
-0.771678043984229));
#78786=CARTESIAN_POINT('Ctrl Pts',(0.00670230030455253,-0.155624936353979,
-0.771129289911328));
#78787=CARTESIAN_POINT('Ctrl Pts',(0.0173029677610404,-0.154603097077782,
-0.770396184701846));
#78788=CARTESIAN_POINT('Ctrl Pts',(0.019675335927424,-0.154319118797238,
-0.770230237335172));
#78789=CARTESIAN_POINT('Ctrl Pts',(0.0233390549807971,-0.153794709972185,
-0.769970529580591));
#78790=CARTESIAN_POINT('Ctrl Pts',(0.0246355499457885,-0.153592362422327,
-0.76987795714009));
#78791=CARTESIAN_POINT('Ctrl Pts',(0.0270385882975622,-0.153186105583339,
-0.769705051736707));
#78792=CARTESIAN_POINT('Ctrl Pts',(0.0281457866905497,-0.15298654441234,
-0.769624860864986));
#78793=CARTESIAN_POINT('Ctrl Pts',(0.0306082602684932,-0.152515072832981,
-0.769445290773247));
#78794=CARTESIAN_POINT('Ctrl Pts',(0.0319622568503667,-0.152237074812078,
-0.769345724736426));
#78795=CARTESIAN_POINT('Ctrl Pts',(0.0354097445539801,-0.151481230192004,
-0.769090011064117));
#78796=CARTESIAN_POINT('Ctrl Pts',(0.0374973116462244,-0.150978024507789,
-0.76893307687826));
#78797=CARTESIAN_POINT('Ctrl Pts',(0.0495751899860725,-0.147800728363296,
-0.768012496422411));
#78798=CARTESIAN_POINT('Ctrl Pts',(0.0592876576204334,-0.144179255168847,
-0.767219055379777));
#78799=CARTESIAN_POINT('Ctrl Pts',(0.0742654154855587,-0.136823785911608,
-0.7659262439432));
#78800=CARTESIAN_POINT('Ctrl Pts',(0.0797870575307063,-0.133679216994205,
-0.765433391095634));
#78801=CARTESIAN_POINT('Ctrl Pts',(0.0869641792978983,-0.128988320546768,
-0.764781252227293));
#78802=CARTESIAN_POINT('Ctrl Pts',(0.0888008267869434,-0.127730848093961,
-0.764613311690958));
#78803=CARTESIAN_POINT('Ctrl Pts',(0.0919303011013704,-0.125488090789782,
-0.764326081944204));
#78804=CARTESIAN_POINT('Ctrl Pts',(0.0932358179562072,-0.124521178874232,
-0.764205923840216));
#78805=CARTESIAN_POINT('Ctrl Pts',(0.0951539725622292,-0.123053440510008,
-0.764029153775479));
#78806=CARTESIAN_POINT('Ctrl Pts',(0.0957782768439896,-0.122568142161201,
-0.763971583962522));
#78807=CARTESIAN_POINT('Ctrl Pts',(0.0968475330359851,-0.121723804822965,
-0.763872958779872));
#78808=CARTESIAN_POINT('Ctrl Pts',(0.0972942356299957,-0.121367050967584,
-0.763831751121603));
#78809=CARTESIAN_POINT('Ctrl Pts',(0.098340598422019,-0.120521895377861,
-0.763735212085814));
#78810=CARTESIAN_POINT('Ctrl Pts',(0.0989385960178016,-0.120031474409887,
-0.763680024391608));
#78811=CARTESIAN_POINT('Ctrl Pts',(0.100676177529508,-0.1185846658575,-0.763519536724081));
#78812=CARTESIAN_POINT('Ctrl Pts',(0.101805766505949,-0.11761633401134,
-0.763415038428798));
#78813=CARTESIAN_POINT('Ctrl Pts',(0.111789903690692,-0.108805873041389,
-0.762488049101127));
#78814=CARTESIAN_POINT('Ctrl Pts',(0.119738237295135,-0.0999926950713225,
-0.761723909468899));
#78815=CARTESIAN_POINT('Ctrl Pts',(0.130940314683007,-0.0842968972731342,
-0.760449307373388));
#78816=CARTESIAN_POINT('Ctrl Pts',(0.134827341827729,-0.0779288240368804,
-0.759951811849063));
#78817=CARTESIAN_POINT('Ctrl Pts',(0.139289708612341,-0.0692776632389138,
-0.759280782714919));
#78818=CARTESIAN_POINT('Ctrl Pts',(0.140291708173744,-0.06722539136633,
-0.759121986540296));
#78819=CARTESIAN_POINT('Ctrl Pts',(0.141788728516491,-0.0639798783776641,
-0.758871022961164));
#78820=CARTESIAN_POINT('Ctrl Pts',(0.142314707461589,-0.0628012120356809,
-0.758779914810016));
#78821=CARTESIAN_POINT('Ctrl Pts',(0.143272316272515,-0.0605814799807456,
-0.758608322154654));
#78822=CARTESIAN_POINT('Ctrl Pts',(0.14370742048909,-0.0595419977928306,
-0.758527961760874));
#78823=CARTESIAN_POINT('Ctrl Pts',(0.144661787581648,-0.0571905621563504,
-0.758346116107824));
#78824=CARTESIAN_POINT('Ctrl Pts',(0.145174564354448,-0.0558761023018297,
-0.758244421455909));
#78825=CARTESIAN_POINT('Ctrl Pts',(0.146457315468574,-0.0524509728805534,
-0.757979237575435));
#78826=CARTESIAN_POINT('Ctrl Pts',(0.147199543685678,-0.0503303405854174,
-0.757814858431232));
#78827=CARTESIAN_POINT('Ctrl Pts',(0.152077968222773,-0.0353598014627387,
-0.756652562841552));
#78828=CARTESIAN_POINT('Ctrl Pts',(0.154571177575083,-0.0220371597327425,
-0.755601291625571));
#78829=CARTESIAN_POINT('Ctrl Pts',(0.1556411458181,-0.00263213073898166,
-0.754100906639943));
#78830=CARTESIAN_POINT('Ctrl Pts',(0.15562816859051,0.00331412458608902,
-0.753646471357276));
#78831=CARTESIAN_POINT('Ctrl Pts',(0.155203207089608,0.0104510875541612,
-0.753117187221257));
#78832=CARTESIAN_POINT('Ctrl Pts',(0.155117393446305,0.0116556943521194,
-0.753028415403978));
#78833=CARTESIAN_POINT('Ctrl Pts',(0.154959232546414,0.0135623186404717,
-0.752888925637902));
#78834=CARTESIAN_POINT('Ctrl Pts',(0.154896124563317,0.0142650231751105,
-0.752837734528911));
#78835=CARTESIAN_POINT('Ctrl Pts',(0.15476627017511,0.0156082939101141,
-0.75274032895042));
#78836=CARTESIAN_POINT('Ctrl Pts',(0.154700324040586,0.0162489071035265,
-0.752694075113463));
#78837=CARTESIAN_POINT('Ctrl Pts',(0.15452795744682,0.0178270320719447,
-0.752580586249592));
#78838=CARTESIAN_POINT('Ctrl Pts',(0.154416979653269,0.0187640405495154,
-0.752513598066399));
#78839=CARTESIAN_POINT('Ctrl Pts',(0.153994269122355,0.0220748593060364,
-0.752278116796344));
#78840=CARTESIAN_POINT('Ctrl Pts',(0.153636250419674,0.0244425543690881,
-0.752111926428026));
#78841=CARTESIAN_POINT('Ctrl Pts',(0.15137788180538,0.0373537521860477,
-0.751213138636186));
#78842=CARTESIAN_POINT('Ctrl Pts',(0.14844670491002,0.0476884769169512,
-0.750519487289276));
#78843=CARTESIAN_POINT('Ctrl Pts',(0.142080865755604,0.0636444168829828,
-0.749383222567223));
#78844=CARTESIAN_POINT('Ctrl Pts',(0.139313940396103,0.0694924297117077,
-0.748951702793932));
#78845=CARTESIAN_POINT('Ctrl Pts',(0.134870605302023,0.0775448084152426,
-0.748321329422321));
#78846=CARTESIAN_POINT('Ctrl Pts',(0.133486896015562,0.079903219840317,
-0.748132051624624));
#78847=CARTESIAN_POINT('Ctrl Pts',(0.131312494053935,0.08339505442286,-0.747843935807861));
#78848=CARTESIAN_POINT('Ctrl Pts',(0.130567630321665,0.0845564893583829,
-0.747746752090606));
#78849=CARTESIAN_POINT('Ctrl Pts',(0.129187608247858,0.086646579928307,
-0.747569294831481));
#78850=CARTESIAN_POINT('Ctrl Pts',(0.128557630741107,0.087578555568169,
-0.747489217874907));
#78851=CARTESIAN_POINT('Ctrl Pts',(0.127169876883921,0.0895843290581817,
-0.747314758014028));
#78852=CARTESIAN_POINT('Ctrl Pts',(0.126408494455939,0.0906555124269333,
-0.747220242767586));
#78853=CARTESIAN_POINT('Ctrl Pts',(0.124258508827839,0.0936005593540994,
-0.746956544887662));
#78854=CARTESIAN_POINT('Ctrl Pts',(0.122841248641737,0.0954529636806026,
-0.746786273784501));
#78855=CARTESIAN_POINT('Ctrl Pts',(0.115629787882961,0.104451873060104,
-0.745936484925558));
#78856=CARTESIAN_POINT('Ctrl Pts',(0.109256642187624,0.111099462666316,
-0.745234706993985));
#78857=CARTESIAN_POINT('Ctrl Pts',(0.102342226135006,0.117140391196766,
-0.744524458909986));
#78858=CARTESIAN_POINT('Origin',(0.,0.,-1.10400562256037));
#78859=CARTESIAN_POINT('',(0.102342242837719,0.117140376604078,-0.660690965868517));
#78860=CARTESIAN_POINT('',(0.102342242758987,0.117140376672865,-0.674376033428004));
#78861=CARTESIAN_POINT('',(0.10234224283772,0.117140376604078,-1.10400562256037));
#78862=CARTESIAN_POINT('',(-0.15554997247323,9.25395981759249E-5,-0.705194377443794));
#78863=CARTESIAN_POINT('Ctrl Pts',(-0.155549972473265,9.25395397988971E-5,
-0.70519437743963));
#78864=CARTESIAN_POINT('Ctrl Pts',(-0.155556164015641,-0.0103148414372451,
-0.704452036543397));
#78865=CARTESIAN_POINT('Ctrl Pts',(-0.154513525352864,-0.0207250453155431,
-0.703709695647164));
#78866=CARTESIAN_POINT('Ctrl Pts',(-0.152446462480172,-0.0309172860594462,
-0.702967354750931));
#78867=CARTESIAN_POINT('Ctrl Pts',(-0.150292093954745,-0.0415400121275881,
-0.70219365991895));
#78868=CARTESIAN_POINT('Ctrl Pts',(-0.147024820678378,-0.0519248668138346,
-0.701419965086969));
#78869=CARTESIAN_POINT('Ctrl Pts',(-0.142730557982281,-0.061836803912125,
-0.700646270254988));
#78870=CARTESIAN_POINT('Ctrl Pts',(-0.138436295286185,-0.0717487410104155,
-0.699872575423007));
#78871=CARTESIAN_POINT('Ctrl Pts',(-0.13311562594688,-0.0811868260858244,
-0.699098880591026));
#78872=CARTESIAN_POINT('Ctrl Pts',(-0.126907404165646,-0.0899461687229495,
-0.698325185759045));
#78873=CARTESIAN_POINT('Ctrl Pts',(-0.120989086182212,-0.0982964785023233,
-0.69758761996337));
#78874=CARTESIAN_POINT('Ctrl Pts',(-0.114221086521816,-0.106091191222701,
-0.696850054167695));
#78875=CARTESIAN_POINT('Ctrl Pts',(-0.106731669265914,-0.113155438560025,
-0.69611248837202));
#78876=CARTESIAN_POINT('Ctrl Pts',(-0.0992244483991311,-0.120236478807459,
-0.695373169257765));
#78877=CARTESIAN_POINT('Ctrl Pts',(-0.0909929491436147,-0.126582832737307,
-0.694633850143511));
#78878=CARTESIAN_POINT('Ctrl Pts',(-0.0822061882775618,-0.132052811817371,
-0.693894531029256));
#78879=CARTESIAN_POINT('Ctrl Pts',(-0.0734602750557194,-0.137497362214135,
-0.69315864884069));
#78880=CARTESIAN_POINT('Ctrl Pts',(-0.0641650414194839,-0.142073172211821,
-0.692422766652123));
#78881=CARTESIAN_POINT('Ctrl Pts',(-0.0545162404005626,-0.14568384273003,
-0.691686884463557));
#78882=CARTESIAN_POINT('Ctrl Pts',(-0.0447998425313615,-0.149319808614363,
-0.690945846886458));
#78883=CARTESIAN_POINT('Ctrl Pts',(-0.0347257889390185,-0.151976714260062,
-0.690204809309359));
#78884=CARTESIAN_POINT('Ctrl Pts',(-0.0245109579853446,-0.153606690735269,
-0.68946377173226));
#78885=CARTESIAN_POINT('Ctrl Pts',(-0.0142961270316707,-0.155236667210476,
-0.688722734155162));
#78886=CARTESIAN_POINT('Ctrl Pts',(-0.00394147099037896,-0.155839693150005,
-0.687981696578063));
#78887=CARTESIAN_POINT('Ctrl Pts',(0.00633312724545194,-0.15542102174189,
-0.687240659000964));
#78888=CARTESIAN_POINT('Ctrl Pts',(0.0165595887075161,-0.155004311820773,
-0.686503093205183));
#78889=CARTESIAN_POINT('Ctrl Pts',(0.0267827483270296,-0.153572399386593,
-0.685765527409402));
#78890=CARTESIAN_POINT('Ctrl Pts',(0.0367860928839178,-0.151137638827447,
-0.685027961613621));
#78891=CARTESIAN_POINT('Ctrl Pts',(0.0468132170800498,-0.148697090431302,
-0.684288642499393));
#78892=CARTESIAN_POINT('Ctrl Pts',(0.056618543836475,-0.14524899597409,
-0.683549323385165));
#78893=CARTESIAN_POINT('Ctrl Pts',(0.0659911969356596,-0.140857958337465,
-0.682810004270937));
#78894=CARTESIAN_POINT('Ctrl Pts',(0.0753202787130791,-0.136487333631066,
-0.68207412208227));
#78895=CARTESIAN_POINT('Ctrl Pts',(0.0842198547940364,-0.131182906131836,
-0.681338239893603));
#78896=CARTESIAN_POINT('Ctrl Pts',(0.0925024753279771,-0.125056365524499,
-0.680602357704937));
#78897=CARTESIAN_POINT('Ctrl Pts',(0.100843121624735,-0.118886904057669,
-0.679861320127928));
#78898=CARTESIAN_POINT('Ctrl Pts',(0.108557362934198,-0.11188431993569,
-0.679120282550919));
#78899=CARTESIAN_POINT('Ctrl Pts',(0.115486949262858,-0.104204448321355,
-0.678379244973911));
#78900=CARTESIAN_POINT('Ctrl Pts',(0.122416535591518,-0.0965245767070206,
-0.677638207396902));
#78901=CARTESIAN_POINT('Ctrl Pts',(0.128560930459896,-0.0881682046654229,
-0.676897169819893));
#78902=CARTESIAN_POINT('Ctrl Pts',(0.133804802816841,-0.0793226149540368,
-0.676156132242885));
#78903=CARTESIAN_POINT('Ctrl Pts',(0.139024107490351,-0.0705184670690396,
-0.675418566446912));
#78904=CARTESIAN_POINT('Ctrl Pts',(0.143390134454677,-0.0611642608263117,
-0.67468100065094));
#78905=CARTESIAN_POINT('Ctrl Pts',(0.14679534359319,-0.0514483196942064,
-0.673943434854968));
#78906=CARTESIAN_POINT('Ctrl Pts',(0.150208647487746,-0.0417092821324859,
-0.673204115740787));
#78907=CARTESIAN_POINT('Ctrl Pts',(0.152656113760471,-0.0316076141012754,
-0.672464796626607));
#78908=CARTESIAN_POINT('Ctrl Pts',(0.154077094241808,-0.0213553630266754,
-0.671725477512427));
#78909=CARTESIAN_POINT('Ctrl Pts',(0.155491468910191,-0.0111507723202771,
-0.670989595323556));
#78910=CARTESIAN_POINT('Ctrl Pts',(0.155888749203406,-0.000797918900235615,
-0.670253713134686));
#78911=CARTESIAN_POINT('Ctrl Pts',(0.155260536823854,0.00948515709772491,
-0.669517830945815));
#78912=CARTESIAN_POINT('Ctrl Pts',(0.154627923361372,0.0198402734943268,
-0.66877679336898));
#78913=CARTESIAN_POINT('Ctrl Pts',(0.152955437516772,0.0301236821901649,
-0.668035755792145));
#78914=CARTESIAN_POINT('Ctrl Pts',(0.150287607839454,0.040117794429585,
-0.667294718215309));
#78915=CARTESIAN_POINT('Ctrl Pts',(0.147619778162136,0.0501119066690056,
-0.666553680638474));
#78916=CARTESIAN_POINT('Ctrl Pts',(0.143956972646875,0.059815843895503,
-0.665812643061639));
#78917=CARTESIAN_POINT('Ctrl Pts',(0.139393467325035,0.0690308899486625,
-0.665071605484804));
#78918=CARTESIAN_POINT('Ctrl Pts',(0.134850423137525,0.0782046190137071,
-0.664333890456828));
#78919=CARTESIAN_POINT('Ctrl Pts',(0.129381001077389,0.0869620440593471,
-0.663596175428853));
#78920=CARTESIAN_POINT('Ctrl Pts',(0.123084657699114,0.0951103019608916,
-0.662858460400877));
#78921=CARTESIAN_POINT('Ctrl Pts',(0.116918189018237,0.103090485717538,
-0.662135962223424));
#78922=CARTESIAN_POINT('Ctrl Pts',(0.109959136079929,0.11048571182954,-0.66141346404597));
#78923=CARTESIAN_POINT('Ctrl Pts',(0.102342242837719,0.117140376604078,
-0.660690965868517));
#78924=CARTESIAN_POINT('Ctrl Pts',(0.10234224283772,0.117140376604078,-0.730690163752328));
#78925=CARTESIAN_POINT('Ctrl Pts',(0.094621461509984,0.123885805468548,
-0.729953349882094));
#78926=CARTESIAN_POINT('Ctrl Pts',(0.0862069888207784,0.129885566877293,
-0.729216536011859));
#78927=CARTESIAN_POINT('Ctrl Pts',(0.0772670487836427,0.135002243211978,
-0.728479722141624));
#78928=CARTESIAN_POINT('Ctrl Pts',(0.0683342552066571,0.140114829348813,
-0.727743497269854));
#78929=CARTESIAN_POINT('Ctrl Pts',(0.0588775918214991,0.144345209434971,
-0.727007272398085));
#78930=CARTESIAN_POINT('Ctrl Pts',(0.0490940272787818,0.147599386806146,
-0.726271047526315));
#78931=CARTESIAN_POINT('Ctrl Pts',(0.0393158995224998,0.150851755811125,
-0.725535231779193));
#78932=CARTESIAN_POINT('Ctrl Pts',(0.029212111985139,0.153128710345636,
-0.724799416032071));
#78933=CARTESIAN_POINT('Ctrl Pts',(0.0189961027279428,0.154385720133533,
-0.724063600284949));
#78934=CARTESIAN_POINT('Ctrl Pts',(0.00875568083771532,0.155645733728287,
-0.72332602619958));
#78935=CARTESIAN_POINT('Ctrl Pts',(-0.00159657035185435,0.155880862690202,
-0.722588452114211));
#78936=CARTESIAN_POINT('Ctrl Pts',(-0.0118424412810255,0.155098546364901,
-0.721850878028841));
#78937=CARTESIAN_POINT('Ctrl Pts',(-0.0181242715147549,0.154618901600822,
-0.721398665110962));
#78938=CARTESIAN_POINT('Ctrl Pts',(-0.0243661104056406,0.153757839952673,
-0.720946452193084));
#78939=CARTESIAN_POINT('Ctrl Pts',(-0.0305193452349855,0.152526627401342,
-0.720494239275205));
#78940=CARTESIAN_POINT('Ctrl Pts',(-0.0405553600408,0.150518501962128,-0.719756673480126));
#78941=CARTESIAN_POINT('Ctrl Pts',(-0.0504296230703562,0.147508137328358,
-0.719019107685047));
#78942=CARTESIAN_POINT('Ctrl Pts',(-0.0599302045978709,0.143541537809992,
-0.718281541889969));
#78943=CARTESIAN_POINT('Ctrl Pts',(-0.069453370623341,0.139565509010012,
-0.717542222775565));
#78944=CARTESIAN_POINT('Ctrl Pts',(-0.0786001636476661,0.134628914473355,
-0.716802903661162));
#78945=CARTESIAN_POINT('Ctrl Pts',(-0.0871723787096418,0.128828486330092,
-0.716063584546758));
#78946=CARTESIAN_POINT('Ctrl Pts',(-0.0957047434925588,0.123055023058627,
-0.715327702358844));
#78947=CARTESIAN_POINT('Ctrl Pts',(-0.103667086401764,0.116426259922342,
-0.71459182017093));
#78948=CARTESIAN_POINT('Ctrl Pts',(-0.110891692655501,0.109081781246906,
-0.713855937983016));
#78949=CARTESIAN_POINT('Ctrl Pts',(-0.118166912528549,0.101685849158695,
-0.713114900405367));
#78950=CARTESIAN_POINT('Ctrl Pts',(-0.124693343388765,0.0935648021931653,
-0.712373862827719));
#78951=CARTESIAN_POINT('Ctrl Pts',(-0.130339004140216,0.0848972702725871,
-0.71163282525007));
#78952=CARTESIAN_POINT('Ctrl Pts',(-0.135984664891667,0.0762297383520086,
-0.710891787672421));
#78953=CARTESIAN_POINT('Ctrl Pts',(-0.140749148507157,0.067016582644528,
-0.710150750094773));
#78954=CARTESIAN_POINT('Ctrl Pts',(-0.144547776091199,0.0574607946959366,
-0.709409712517124));
#78955=CARTESIAN_POINT('Ctrl Pts',(-0.148790588070324,0.0467876211138281,
-0.70858202329467));
#78956=CARTESIAN_POINT('Ctrl Pts',(-0.151855992978236,0.0356211012833882,
-0.707754334072216));
#78957=CARTESIAN_POINT('Ctrl Pts',(-0.153653437845324,0.0242161833969177,
-0.706926644849762));
#78958=CARTESIAN_POINT('Ctrl Pts',(-0.154907392861616,0.0162597479835195,
-0.706349222381106));
#78959=CARTESIAN_POINT('Ctrl Pts',(-0.155545156440655,0.00818781718077903,
-0.70577179991245));
#78960=CARTESIAN_POINT('Ctrl Pts',(-0.15554997247323,9.25395981750804E-5,
-0.705194377443794));
#78961=CARTESIAN_POINT('Ctrl Pts',(0.102342226135006,0.117140391196766,
-0.744524458909986));
#78962=CARTESIAN_POINT('Ctrl Pts',(0.0992816917559716,0.11981429298515,
-0.744210081142987));
#78963=CARTESIAN_POINT('Ctrl Pts',(0.0961151016480072,0.122369357141659,
-0.74389430617453));
#78964=CARTESIAN_POINT('Ctrl Pts',(0.087743192154423,0.128597967857729,
-0.743087731012877));
#78965=CARTESIAN_POINT('Ctrl Pts',(0.0824082290926953,0.132080306284147,
-0.742599763532665));
#78966=CARTESIAN_POINT('Ctrl Pts',(0.0758110869509018,0.135830693983384,
-0.742037792075191));
#78967=CARTESIAN_POINT('Ctrl Pts',(0.0747407077159392,0.136422597797972,
-0.741947858731752));
#78968=CARTESIAN_POINT('Ctrl Pts',(0.073039099563667,0.137337521776461,
-0.741806972700145));
#78969=CARTESIAN_POINT('Ctrl Pts',(0.072412480296711,0.137668942406708,
-0.741755531400762));
#78970=CARTESIAN_POINT('Ctrl Pts',(0.071213587964429,0.13829258918564,-0.741657977164177));
#78971=CARTESIAN_POINT('Ctrl Pts',(0.0706417418346042,0.138585568014733,
-0.741611821584449));
#78972=CARTESIAN_POINT('Ctrl Pts',(0.0692333889481668,0.139296139332652,
-0.741499033309447));
#78973=CARTESIAN_POINT('Ctrl Pts',(0.0683948839642774,0.139709758215228,
-0.74143264023381));
#78974=CARTESIAN_POINT('Ctrl Pts',(0.0654442578128729,0.141132314963904,
-0.74120147566794));
#78975=CARTESIAN_POINT('Ctrl Pts',(0.0633130232656981,0.142101174413875,
-0.741038898343776));
#78976=CARTESIAN_POINT('Ctrl Pts',(0.0512567778007329,0.147256808209453,
-0.740139076246891));
#78977=CARTESIAN_POINT('Ctrl Pts',(0.0409388087412304,0.15045228295911,
-0.739441712389885));
#78978=CARTESIAN_POINT('Ctrl Pts',(0.0252155040855959,0.153582646212186,
-0.738381362479128));
#78979=CARTESIAN_POINT('Ctrl Pts',(0.020010149512094,0.154347136340895,
-0.738030994124772));
#78980=CARTESIAN_POINT('Ctrl Pts',(0.0112395068769008,0.155184081548472,
-0.737432382908579));
#78981=CARTESIAN_POINT('Ctrl Pts',(0.00769238439801505,0.155400288626378,
-0.737188081701392));
#78982=CARTESIAN_POINT('Ctrl Pts',(0.00262051371842576,0.155535364082152,
-0.736833883427955));
#78983=CARTESIAN_POINT('Ctrl Pts',(0.00109938221013814,0.155553552335351,
-0.736727033071687));
#78984=CARTESIAN_POINT('Ctrl Pts',(-0.00156142240452312,0.155546338365351,
-0.736538916565582));
#78985=CARTESIAN_POINT('Ctrl Pts',(-0.00270102273462084,0.155530722913021,
-0.736457959507899));
#78986=CARTESIAN_POINT('Ctrl Pts',(-0.00507123498229626,0.155472187697642,
-0.73628872077709));
#78987=CARTESIAN_POINT('Ctrl Pts',(-0.00630171035188463,0.155427175416405,
-0.736200379666704));
#78988=CARTESIAN_POINT('Ctrl Pts',(-0.00952720508736266,0.155270818578288,
-0.735967477137352));
#78989=CARTESIAN_POINT('Ctrl Pts',(-0.0115207809893011,0.155135636327244,
-0.735822188510033));
#78990=CARTESIAN_POINT('Ctrl Pts',(-0.022211329520695,0.154203529350073,
-0.735035506198311));
#78991=CARTESIAN_POINT('Ctrl Pts',(-0.0308307132378416,0.152713756217094,
-0.734372952943605));
#78992=CARTESIAN_POINT('Ctrl Pts',(-0.04550645091284,0.148883837758629,
-0.733202833956973));
#78993=CARTESIAN_POINT('Ctrl Pts',(-0.05162765390214,0.146873479861896,
-0.732701743721254));
#78994=CARTESIAN_POINT('Ctrl Pts',(-0.062443237373995,0.142561408318975,
-0.731805336973281));
#78995=CARTESIAN_POINT('Ctrl Pts',(-0.0671804717886798,0.140391271214905,
-0.731408739860987));
#78996=CARTESIAN_POINT('Ctrl Pts',(-0.0728414383288936,0.137445642443011,
-0.730936667598119));
#78997=CARTESIAN_POINT('Ctrl Pts',(-0.073876381750402,0.136892148072412,
-0.73085044695573));
#78998=CARTESIAN_POINT('Ctrl Pts',(-0.0755168808649026,0.135990774057516,
-0.73071402694491));
#78999=CARTESIAN_POINT('Ctrl Pts',(-0.0761265053878712,0.135650452092503,
-0.730663387689268));
#79000=CARTESIAN_POINT('Ctrl Pts',(-0.0772971901348672,0.134986541327693,
-0.730566280688034));
#79001=CARTESIAN_POINT('Ctrl Pts',(-0.0778585501977418,0.134663536726079,
-0.730519780964233));
#79002=CARTESIAN_POINT('Ctrl Pts',(-0.0791160054150711,0.133929509934786,
-0.730415730943672));
#79003=CARTESIAN_POINT('Ctrl Pts',(-0.0798109578556671,0.133516542139265,
-0.730358301957721));
#79004=CARTESIAN_POINT('Ctrl Pts',(-0.0822660292145733,0.132031624421179,
-0.730155574334149));
#79005=CARTESIAN_POINT('Ctrl Pts',(-0.0840081188800761,0.130930082144696,
-0.730012001848213));
#79006=CARTESIAN_POINT('Ctrl Pts',(-0.0938409267653244,0.124435599499604,
-0.729200137205314));
#79007=CARTESIAN_POINT('Ctrl Pts',(-0.101434615885145,0.118327515291702,
-0.728566227933881));
#79008=CARTESIAN_POINT('Ctrl Pts',(-0.114454298389645,0.105674413602827,
-0.727369211543443));
#79009=CARTESIAN_POINT('Ctrl Pts',(-0.120011455342144,0.0993181504842108,
-0.726809894187585));
#79010=CARTESIAN_POINT('Ctrl Pts',(-0.126459721081835,0.0906065595270534,
-0.726064006081659));
#79011=CARTESIAN_POINT('Ctrl Pts',(-0.127848147299566,0.0886366732353807,
-0.72589665562401));
#79012=CARTESIAN_POINT('Ctrl Pts',(-0.129923354084219,0.0855421378597002,
-0.725635233860369));
#79013=CARTESIAN_POINT('Ctrl Pts',(-0.130642584522529,0.0844396246227322,
-0.725542376527022));
#79014=CARTESIAN_POINT('Ctrl Pts',(-0.13195027207576,0.0823783550099891,
-0.725369206656714));
#79015=CARTESIAN_POINT('Ctrl Pts',(-0.13254249286479,0.0814220801689962,
-0.725289039655962));
#79016=CARTESIAN_POINT('Ctrl Pts',(-0.133836605675194,0.0792809053538552,
-0.725109867626132));
#79017=CARTESIAN_POINT('Ctrl Pts',(-0.134533229737273,0.0780929500259457,
-0.725010679803009));
#79018=CARTESIAN_POINT('Ctrl Pts',(-0.136266799344912,0.0750446377506869,
-0.724756636720924));
#79019=CARTESIAN_POINT('Ctrl Pts',(-0.137281447262741,0.0731720005984846,
-0.724601012552606));
#79020=CARTESIAN_POINT('Ctrl Pts',(-0.144331719028053,0.0594968841098366,
-0.723467199148181));
#79021=CARTESIAN_POINT('Ctrl Pts',(-0.14887408473509,0.0469882461764634,
-0.722437247337514));
#79022=CARTESIAN_POINT('Ctrl Pts',(-0.153061670915404,0.0283272572319096,
-0.720958902415645));
#79023=CARTESIAN_POINT('Ctrl Pts',(-0.154022297012498,0.0225267498717688,
-0.720508196758153));
#79024=CARTESIAN_POINT('Ctrl Pts',(-0.154815110970317,0.0151783165606813,
-0.719957806148216));
#79025=CARTESIAN_POINT('Ctrl Pts',(-0.154955668860915,0.0136689801187794,
-0.719845851519961));
#79026=CARTESIAN_POINT('Ctrl Pts',(-0.155134296591403,0.0113905548423789,
-0.719678726132901));
#79027=CARTESIAN_POINT('Ctrl Pts',(-0.155188752518389,0.0106228940196766,
-0.719622737674124));
#79028=CARTESIAN_POINT('Ctrl Pts',(-0.155277781995037,0.00922046481166052,
-0.71952107550627));
#79029=CARTESIAN_POINT('Ctrl Pts',(-0.155314163911447,0.00858586456539685,
-0.719475309689463));
#79030=CARTESIAN_POINT('Ctrl Pts',(-0.155388410088042,0.0071352464649925,
-0.719371221166804));
#79031=CARTESIAN_POINT('Ctrl Pts',(-0.155423738172151,0.00631913149340646,
-0.719313036946951));
#79032=CARTESIAN_POINT('Ctrl Pts',(-0.155516790167648,0.00369041454213425,
-0.719126724232841));
#79033=CARTESIAN_POINT('Ctrl Pts',(-0.155549248849663,0.00187699144480572,
-0.718999878131621));
#79034=CARTESIAN_POINT('Ctrl Pts',(-0.155553661810709,-0.00896411500264388,
-0.718249377611239));
#79035=CARTESIAN_POINT('Ctrl Pts',(-0.154771460006158,-0.0179759038482187,
-0.717657240668742));
#79036=CARTESIAN_POINT('Ctrl Pts',(-0.151558321205572,-0.0362971868528248,
-0.716432030666671));
#79037=CARTESIAN_POINT('Ctrl Pts',(-0.149038636047285,-0.0455507027420927,
-0.715800666335872));
#79038=CARTESIAN_POINT('Ctrl Pts',(-0.144926839144654,-0.0565392993009497,
-0.714993137958498));
#79039=CARTESIAN_POINT('Ctrl Pts',(-0.144126662870719,-0.058548999524496,
-0.714843046080432));
#79040=CARTESIAN_POINT('Ctrl Pts',(-0.142745120489696,-0.0618187374853886,
-0.71459447008077));
#79041=CARTESIAN_POINT('Ctrl Pts',(-0.142188321550449,-0.0630888795504469,
-0.71449680419558));
#79042=CARTESIAN_POINT('Ctrl Pts',(-0.141149103598201,-0.0653758310489519,
-0.714318843939308));
#79043=CARTESIAN_POINT('Ctrl Pts',(-0.140672485639194,-0.0663951835227835,
-0.714238751754864));
#79044=CARTESIAN_POINT('Ctrl Pts',(-0.139617800852295,-0.0685885151165409,
-0.714064693602544));
#79045=CARTESIAN_POINT('Ctrl Pts',(-0.139035899206212,-0.0697605422836783,
-0.713970599958849));
#79046=CARTESIAN_POINT('Ctrl Pts',(-0.137358187712264,-0.0730352834106492,
-0.713704548575875));
#79047=CARTESIAN_POINT('Ctrl Pts',(-0.136229029170661,-0.0751204021982916,
-0.713531443769468));
#79048=CARTESIAN_POINT('Ctrl Pts',(-0.131024625489795,-0.0842274218719544,
-0.712758381064827));
#79049=CARTESIAN_POINT('Ctrl Pts',(-0.126451529956137,-0.090948803060077,
-0.712141236413024));
#79050=CARTESIAN_POINT('Ctrl Pts',(-0.115699175673375,-0.104364197036007,
-0.710814612431317));
#79051=CARTESIAN_POINT('Ctrl Pts',(-0.109413625780804,-0.110936252433604,
-0.710105190608367));
#79052=CARTESIAN_POINT('Ctrl Pts',(-0.100455876751058,-0.11879598308888,
-0.709202028793471));
#79053=CARTESIAN_POINT('Ctrl Pts',(-0.0982699620206477,-0.120610471543629,
-0.708989160596649));
#79054=CARTESIAN_POINT('Ctrl Pts',(-0.0952449155553769,-0.122984626572255,
-0.708705836099892));
#79055=CARTESIAN_POINT('Ctrl Pts',(-0.0944483887885326,-0.123597387956105,
-0.708632252926842));
#79056=CARTESIAN_POINT('Ctrl Pts',(-0.093169661825641,-0.124561520660955,
-0.708515808394829));
#79057=CARTESIAN_POINT('Ctrl Pts',(-0.0926912991225362,-0.124917898690775,
-0.708472616972283));
#79058=CARTESIAN_POINT('Ctrl Pts',(-0.0916716508948487,-0.125668449692673,
-0.708381354556019));
#79059=CARTESIAN_POINT('Ctrl Pts',(-0.0911298455352361,-0.12606189796134,
-0.708333335566216));
#79060=CARTESIAN_POINT('Ctrl Pts',(-0.0897390442549637,-0.127058217444576,
-0.708211231123739));
#79061=CARTESIAN_POINT('Ctrl Pts',(-0.088886486288689,-0.127656098149074,
-0.70813747323873));
#79062=CARTESIAN_POINT('Ctrl Pts',(-0.085207969919963,-0.130181040967754,
-0.707823573278467));
#79063=CARTESIAN_POINT('Ctrl Pts',(-0.0823246481788521,-0.132023323810313,
-0.707588381127736));
#79064=CARTESIAN_POINT('Ctrl Pts',(-0.0734929468294431,-0.137264322270465,
-0.706892411792521));
#79065=CARTESIAN_POINT('Ctrl Pts',(-0.0673783989063612,-0.140366918619535,
-0.70644229674957));
#79066=CARTESIAN_POINT('Ctrl Pts',(-0.0522131573940497,-0.146841813022872,
-0.705356164979361));
#79067=CARTESIAN_POINT('Ctrl Pts',(-0.0430158029548496,-0.14979433680602,
-0.704720488039432));
#79068=CARTESIAN_POINT('Ctrl Pts',(-0.0314940139511692,-0.152343702801222,
-0.703908283545025));
#79069=CARTESIAN_POINT('Ctrl Pts',(-0.0293736650130515,-0.152766697052541,
-0.703758260061269));
#79070=CARTESIAN_POINT('Ctrl Pts',(-0.0258801966423407,-0.153388201423256,
-0.703509773536445));
#79071=CARTESIAN_POINT('Ctrl Pts',(-0.0245119736761926,-0.153612785408959,
-0.703412127693914));
#79072=CARTESIAN_POINT('Ctrl Pts',(-0.0220282374517586,-0.153986445673217,
-0.703234188432255));
#79073=CARTESIAN_POINT('Ctrl Pts',(-0.0209137490155912,-0.154141764870638,
-0.703154096967158));
#79074=CARTESIAN_POINT('Ctrl Pts',(-0.018499593368276,-0.154451547002176,
-0.702980022532081));
#79075=CARTESIAN_POINT('Ctrl Pts',(-0.0171994743716018,-0.154601724487356,
-0.702885911695391));
#79076=CARTESIAN_POINT('Ctrl Pts',(-0.013537886368753,-0.154977919076282,
-0.702619759232182));
#79077=CARTESIAN_POINT('Ctrl Pts',(-0.0111730113793886,-0.155166337987278,
-0.702446569133172));
#79078=CARTESIAN_POINT('Ctrl Pts',(-0.000690454988465145,-0.15576065332838,
-0.701672744691906));
#79079=CARTESIAN_POINT('Ctrl Pts',(0.00744628704844008,-0.155583976301972,
-0.701054883192174));
#79080=CARTESIAN_POINT('Ctrl Pts',(0.0245800810837738,-0.153864665123797,
-0.699726116744724));
#79081=CARTESIAN_POINT('Ctrl Pts',(0.0335323763558437,-0.152164727380259,
-0.699015260521745));
#79082=CARTESIAN_POINT('Ctrl Pts',(0.0449962346101666,-0.148926419812295,
-0.698112652310696));
#79083=CARTESIAN_POINT('Ctrl Pts',(0.0476863441962586,-0.148086983494662,
-0.69790153632695));
#79084=CARTESIAN_POINT('Ctrl Pts',(0.0513003490112249,-0.146850538171774,
-0.69762013390306));
#79085=CARTESIAN_POINT('Ctrl Pts',(0.052245213838097,-0.146517043861462,
-0.697546772307117));
#79086=CARTESIAN_POINT('Ctrl Pts',(0.0537468637978994,-0.145970655620525,
-0.697430587846476));
#79087=CARTESIAN_POINT('Ctrl Pts',(0.0543057417739201,-0.145763658409669,
-0.697387437464682));
#79088=CARTESIAN_POINT('Ctrl Pts',(0.0554906265918142,-0.145317040043381,
-0.69729616726777));
#79089=CARTESIAN_POINT('Ctrl Pts',(0.0561163036812781,-0.145076573807682,
-0.697248100178752));
#79090=CARTESIAN_POINT('Ctrl Pts',(0.0577130080627482,-0.144451037754202,
-0.697125714880949));
#79091=CARTESIAN_POINT('Ctrl Pts',(0.0586817675402088,-0.144060209367745,
-0.69705172723954));
#79092=CARTESIAN_POINT('Ctrl Pts',(0.062836518384689,-0.142335183730982,
-0.696735258029877));
#79093=CARTESIAN_POINT('Ctrl Pts',(0.0659817778331868,-0.140904726098666,
-0.696497827620692));
#79094=CARTESIAN_POINT('Ctrl Pts',(0.0753252473259032,-0.136273767735801,
-0.695791369067072));
#79095=CARTESIAN_POINT('Ctrl Pts',(0.0813585486116721,-0.132760056858453,
-0.695333379222897));
#79096=CARTESIAN_POINT('Ctrl Pts',(0.0949808041973258,-0.123548099193227,
-0.69425016844738));
#79097=CARTESIAN_POINT('Ctrl Pts',(0.10232384661509,-0.117538452668813,
-0.693625146920701));
#79098=CARTESIAN_POINT('Ctrl Pts',(0.110617496272003,-0.109381242221885,
-0.692824501079762));
#79099=CARTESIAN_POINT('Ctrl Pts',(0.112128606983927,-0.107831634280888,
-0.692674322245122));
#79100=CARTESIAN_POINT('Ctrl Pts',(0.114554371860651,-0.105237933512922,
-0.692425632495276));
#79101=CARTESIAN_POINT('Ctrl Pts',(0.115488284277159,-0.104212200520695,
-0.692327941136988));
#79102=CARTESIAN_POINT('Ctrl Pts',(0.117154716485394,-0.102332014455273,
-0.692149954195518));
#79103=CARTESIAN_POINT('Ctrl Pts',(0.1178919269267,-0.101481831978777,-0.692069861094677));
#79104=CARTESIAN_POINT('Ctrl Pts',(0.11946610854211,-0.0996261153610942,
-0.691895823614201));
#79105=CARTESIAN_POINT('Ctrl Pts',(0.120299742235132,-0.0986178775755117,
-0.6918017518011));
#79106=CARTESIAN_POINT('Ctrl Pts',(0.122607331319527,-0.0957541633233396,
-0.69153582871228));
#79107=CARTESIAN_POINT('Ctrl Pts',(0.124051690325616,-0.0938754199841913,
-0.691362832151772));
#79108=CARTESIAN_POINT('Ctrl Pts',(0.13024551285702,-0.0854261765480031,
-0.690590735168407));
#79109=CARTESIAN_POINT('Ctrl Pts',(0.134519313446427,-0.078524154440994,
-0.689974499134471));
#79110=CARTESIAN_POINT('Ctrl Pts',(0.142386524940968,-0.0632759399475228,
-0.688650589229111));
#79111=CARTESIAN_POINT('Ctrl Pts',(0.14582736188566,-0.054883112506267,
-0.687942984071129));
#79112=CARTESIAN_POINT('Ctrl Pts',(0.149371571018636,-0.0434990583616816,
-0.687039115483485));
#79113=CARTESIAN_POINT('Ctrl Pts',(0.150148550342963,-0.0407363439128798,
-0.686824020709226));
#79114=CARTESIAN_POINT('Ctrl Pts',(0.151094810050685,-0.0369753728078855,
-0.68653825692992));
#79115=CARTESIAN_POINT('Ctrl Pts',(0.151331398607144,-0.0359948295965663,
-0.686464394777725));
#79116=CARTESIAN_POINT('Ctrl Pts',(0.1516928580781,-0.0344301602855888,
-0.68634762258654));
#79117=CARTESIAN_POINT('Ctrl Pts',(0.151823926665111,-0.0338475176866469,
-0.686304379269762));
#79118=CARTESIAN_POINT('Ctrl Pts',(0.152094641011558,-0.0326108853392737,
-0.686213125168673));
#79119=CARTESIAN_POINT('Ctrl Pts',(0.152233431733234,-0.031956720221502,
-0.686165165485197));
#79120=CARTESIAN_POINT('Ctrl Pts',(0.152576706513767,-0.0302857519195269,
-0.686043408601166));
#79121=CARTESIAN_POINT('Ctrl Pts',(0.152775252392319,-0.0292677390666102,
-0.685969935264158));
#79122=CARTESIAN_POINT('Ctrl Pts',(0.153577288613936,-0.0249246596223963,
-0.685659179920169));
#79123=CARTESIAN_POINT('Ctrl Pts',(0.15408256936247,-0.021582124176489,
-0.685426725433824));
#79124=CARTESIAN_POINT('Ctrl Pts',(0.15526350892157,-0.0115725283598531,
-0.684743383860581));
#79125=CARTESIAN_POINT('Ctrl Pts',(0.155617879627099,-0.00487532178759307,
-0.684302714685869));
#79126=CARTESIAN_POINT('Ctrl Pts',(0.155423827038618,0.0116698071832762,
-0.683212862552858));
#79127=CARTESIAN_POINT('Ctrl Pts',(0.154373856334072,0.021480989589612,
-0.682564274530648));
#79128=CARTESIAN_POINT('Ctrl Pts',(0.151971952110645,0.0332413467680238,
-0.681738078002183));
#79129=CARTESIAN_POINT('Ctrl Pts',(0.151496082440588,0.0353468187923684,
-0.681588294671204));
#79130=CARTESIAN_POINT('Ctrl Pts',(0.15064308674465,0.0387863696871938,
-0.681340122326159));
#79131=CARTESIAN_POINT('Ctrl Pts',(0.150291653241152,0.0401265598385105,
-0.681242546870685));
#79132=CARTESIAN_POINT('Ctrl Pts',(0.149622452714608,0.0425463302414749,
-0.681064681269375));
#79133=CARTESIAN_POINT('Ctrl Pts',(0.149310779876542,0.0436275081232486,
-0.680984592260407));
#79134=CARTESIAN_POINT('Ctrl Pts',(0.148611042109735,0.0459594998364188,
-0.680810460322217));
#79135=CARTESIAN_POINT('Ctrl Pts',(0.148218857986491,0.0472089759043598,
-0.68071628885366));
#79136=CARTESIAN_POINT('Ctrl Pts',(0.14707077305594,0.050711306430118,-0.680449779850171));
#79137=CARTESIAN_POINT('Ctrl Pts',(0.146278987571426,0.0529519172039678,
-0.680276288879838));
#79138=CARTESIAN_POINT('Ctrl Pts',(0.142542109101753,0.0628022705402446,
-0.679499772072352));
#79139=CARTESIAN_POINT('Ctrl Pts',(0.139052670189038,0.0701904238856169,
-0.678879375835245));
#79140=CARTESIAN_POINT('Ctrl Pts',(0.130450778171729,0.0852190527600437,
-0.677543024598288));
#79141=CARTESIAN_POINT('Ctrl Pts',(0.125207673137088,0.092750961464185,
-0.676827087688327));
#79142=CARTESIAN_POINT('Ctrl Pts',(0.117576555293586,0.101877607908888,
-0.675926408963144));
#79143=CARTESIAN_POINT('Ctrl Pts',(0.115765689306785,0.103930750023422,
-0.675721458039828));
#79144=CARTESIAN_POINT('Ctrl Pts',(0.113226325296756,0.106661072918307,
-0.675446835871534));
#79145=CARTESIAN_POINT('Ctrl Pts',(0.112544252705924,0.107380522143752,
-0.675374268366817));
#79146=CARTESIAN_POINT('Ctrl Pts',(0.111442515048659,0.108520602799092,
-0.675259014619525));
#79147=CARTESIAN_POINT('Ctrl Pts',(0.111027251853162,0.108945421060729,
-0.675216009940731));
#79148=CARTESIAN_POINT('Ctrl Pts',(0.110136438899788,0.109846347764342,
-0.675124702884842));
#79149=CARTESIAN_POINT('Ctrl Pts',(0.109660210500655,0.110321772865897,
-0.675076455859219));
#79150=CARTESIAN_POINT('Ctrl Pts',(0.108428117954813,0.111535925678154,
-0.674953027409561));
#79151=CARTESIAN_POINT('Ctrl Pts',(0.107667767571077,0.112270082695363,
-0.674878187746555));
#79152=CARTESIAN_POINT('Ctrl Pts',(0.105408197655482,0.114407742129455,
-0.674659442644647));
#79153=CARTESIAN_POINT('Ctrl Pts',(0.103888656900956,0.115789318258862,
-0.674516986467108));
#79154=CARTESIAN_POINT('Ctrl Pts',(0.102342242758987,0.117140376672865,
-0.674376033428004));
#79155=CARTESIAN_POINT('Origin',(0.,0.,-1.10400562256037));
#79156=CARTESIAN_POINT('',(0.10234224283772,0.117140376604078,-0.590700225539723));
#79157=CARTESIAN_POINT('',(0.102342242827937,0.117140376612625,-0.604616163143584));
#79158=CARTESIAN_POINT('',(0.10234224283772,0.117140376604078,-1.10400562256037));
#79159=CARTESIAN_POINT('',(-0.15554994586618,-0.000129772988789563,-0.635194377433095));
#79160=CARTESIAN_POINT('Ctrl Pts',(-0.15554994586618,-0.000129772988788979,
-0.635194377433095));
#79161=CARTESIAN_POINT('Ctrl Pts',(-0.155539597239793,-0.0125339588620959,
-0.634307833869035));
#79162=CARTESIAN_POINT('Ctrl Pts',(-0.154041489336815,-0.0248731108772741,
-0.633421290304974));
#79163=CARTESIAN_POINT('Ctrl Pts',(-0.151125138991674,-0.0368374112112568,
-0.632534746740914));
#79164=CARTESIAN_POINT('Ctrl Pts',(-0.150339236238879,-0.0400615699901928,
-0.632295839564131));
#79165=CARTESIAN_POINT('Ctrl Pts',(-0.149450609198663,-0.0432586255057535,
-0.632056932387348));
#79166=CARTESIAN_POINT('Ctrl Pts',(-0.148461201799215,-0.0464227752329896,
-0.631818025210565));
#79167=CARTESIAN_POINT('Ctrl Pts',(-0.14540665540244,-0.0561912913706129,
-0.631080459414702));
#79168=CARTESIAN_POINT('Ctrl Pts',(-0.141372495840606,-0.0656933397014203,
-0.630342893618839));
#79169=CARTESIAN_POINT('Ctrl Pts',(-0.13642680457351,-0.0747230185007366,
-0.629605327822976));
#79170=CARTESIAN_POINT('Ctrl Pts',(-0.131469356563795,-0.0837741623701181,
-0.628866008708768));
#79171=CARTESIAN_POINT('Ctrl Pts',(-0.125596353745635,-0.0923498038083296,
-0.628126689594561));
#79172=CARTESIAN_POINT('Ctrl Pts',(-0.118924876618117,-0.100263035169327,
-0.627387370480353));
#79173=CARTESIAN_POINT('Ctrl Pts',(-0.112284413661745,-0.108139479727783,
-0.626651488291597));
#79174=CARTESIAN_POINT('Ctrl Pts',(-0.104853482495447,-0.115358944218995,
-0.625915606102841));
#79175=CARTESIAN_POINT('Ctrl Pts',(-0.0967885641346958,-0.121769357199354,
-0.625179723914085));
#79176=CARTESIAN_POINT('Ctrl Pts',(-0.0886671451745217,-0.128224679769585,
-0.624438686337151));
#79177=CARTESIAN_POINT('Ctrl Pts',(-0.0799035567255813,-0.133858969506248,
-0.623697648760218));
#79178=CARTESIAN_POINT('Ctrl Pts',(-0.0706893423499887,-0.138559804337788,
-0.622956611183284));
#79179=CARTESIAN_POINT('Ctrl Pts',(-0.0614751279743957,-0.143260639169328,
-0.622215573606351));
#79180=CARTESIAN_POINT('Ctrl Pts',(-0.0518111869380719,-0.147027705085406,
-0.621474536029418));
#79181=CARTESIAN_POINT('Ctrl Pts',(-0.0419083040406783,-0.149798186078584,
-0.620733498452484));
#79182=CARTESIAN_POINT('Ctrl Pts',(-0.0320518164171601,-0.152555687293471,
-0.619995932656616));
#79183=CARTESIAN_POINT('Ctrl Pts',(-0.0218853754879639,-0.154346453801442,
-0.619258366860748));
#79184=CARTESIAN_POINT('Ctrl Pts',(-0.01161875068525,-0.155115463872929,
-0.618520801064879));
#79185=CARTESIAN_POINT('Ctrl Pts',(-0.00132772038320625,-0.155886302011103,
-0.617781481950673));
#79186=CARTESIAN_POINT('Ctrl Pts',(0.0090630569164229,-0.155630303401892,
-0.617042162836467));
#79187=CARTESIAN_POINT('Ctrl Pts',(0.0193330602770041,-0.154343886436508,
-0.616302843722261));
#79188=CARTESIAN_POINT('Ctrl Pts',(0.0295553207411928,-0.153063449729333,
-0.615566961533499));
#79189=CARTESIAN_POINT('Ctrl Pts',(0.0396570018576745,-0.150762266520526,
-0.614831079344738));
#79190=CARTESIAN_POINT('Ctrl Pts',(0.0494253453003874,-0.147488771579187,
-0.614095197155977));
#79191=CARTESIAN_POINT('Ctrl Pts',(0.0592621230699126,-0.144192343432852,
-0.613354159579048));
#79192=CARTESIAN_POINT('Ctrl Pts',(0.0687599697457468,-0.13991021640765,
-0.612613122002119));
#79193=CARTESIAN_POINT('Ctrl Pts',(0.0777202887948234,-0.134741824277576,
-0.611872084425191));
#79194=CARTESIAN_POINT('Ctrl Pts',(0.0866806078439001,-0.129573432147503,
-0.611131046848262));
#79195=CARTESIAN_POINT('Ctrl Pts',(0.0951026462021396,-0.123519358158803,
-0.610390009271333));
#79196=CARTESIAN_POINT('Ctrl Pts',(0.102818935575983,-0.116722187209724,
-0.609648971694404));
#79197=CARTESIAN_POINT('Ctrl Pts',(0.110499073925748,-0.109956861190085,
-0.608911405898533));
#79198=CARTESIAN_POINT('Ctrl Pts',(0.117537168754883,-0.10240513376983,
-0.608173840102662));
#79199=CARTESIAN_POINT('Ctrl Pts',(0.123772841973527,-0.0942129825968604,
-0.607436274306792));
#79200=CARTESIAN_POINT('Ctrl Pts',(0.13002333843946,-0.0860013572984187,
-0.606696955192586));
#79201=CARTESIAN_POINT('Ctrl Pts',(0.13546691439087,-0.0771469081885431,
-0.60595763607838));
#79202=CARTESIAN_POINT('Ctrl Pts',(0.139980481331036,-0.0678326421889309,
-0.605218316964175));
#79203=CARTESIAN_POINT('Ctrl Pts',(0.144473065730982,-0.0585616760812977,
-0.604482434775411));
#79204=CARTESIAN_POINT('Ctrl Pts',(0.148043859148208,-0.0488359966751181,
-0.603746552586647));
#79205=CARTESIAN_POINT('Ctrl Pts',(0.150617627849007,-0.0388604256427797,
-0.603010670397883));
#79206=CARTESIAN_POINT('Ctrl Pts',(0.153209427665242,-0.0288149685042174,
-0.602269632820956));
#79207=CARTESIAN_POINT('Ctrl Pts',(0.15478992868617,-0.0185170211427482,
-0.60152859524403));
#79208=CARTESIAN_POINT('Ctrl Pts',(0.155334383310592,-0.00818729879253237,
-0.600787557667103));
#79209=CARTESIAN_POINT('Ctrl Pts',(0.155878837935013,0.00214242355768306,
-0.600046520090177));
#79210=CARTESIAN_POINT('Ctrl Pts',(0.155387325267977,0.0125029716737622,
-0.599305482513251));
#79211=CARTESIAN_POINT('Ctrl Pts',(0.153888240661186,0.0226762405659494,
-0.598564444936324));
#79212=CARTESIAN_POINT('Ctrl Pts',(0.152396068484794,0.0328025994886629,
-0.597826824358445));
#79213=CARTESIAN_POINT('Ctrl Pts',(0.149894543880813,0.0428186757317106,
-0.597089203780566));
#79214=CARTESIAN_POINT('Ctrl Pts',(0.1464187785058,0.0525104161178468,-0.596351583202687));
#79215=CARTESIAN_POINT('Ctrl Pts',(0.142950456108193,0.0621814026852035,
-0.595615542159875));
#79216=CARTESIAN_POINT('Ctrl Pts',(0.138512269623156,0.0715285415126396,
-0.594879501117063));
#79217=CARTESIAN_POINT('Ctrl Pts',(0.133189436101435,0.0803515812599966,
-0.594143460074251));
#79218=CARTESIAN_POINT('Ctrl Pts',(0.127867291225759,0.0891734795191949,
-0.593407514257366));
#79219=CARTESIAN_POINT('Ctrl Pts',(0.121661170840324,0.0974706005783878,
-0.59267156844048));
#79220=CARTESIAN_POINT('Ctrl Pts',(0.11470174867881,0.105068127184333,-0.591935622623595));
#79221=CARTESIAN_POINT('Ctrl Pts',(0.110807598843997,0.109319328834541,
-0.591523823595638));
#79222=CARTESIAN_POINT('Ctrl Pts',(0.106678376741718,0.113352018722323,
-0.59111202456768));
#79223=CARTESIAN_POINT('Ctrl Pts',(0.10234224283772,0.117140376604078,-0.590700225539723));
#79224=CARTESIAN_POINT('Ctrl Pts',(0.102342242837719,0.117140376604078,
-0.660690965868517));
#79225=CARTESIAN_POINT('Ctrl Pts',(0.0945841693280625,0.123918386595985,
-0.659955076078148));
#79226=CARTESIAN_POINT('Ctrl Pts',(0.0861441868282826,0.129927390680792,
-0.659219186287779));
#79227=CARTESIAN_POINT('Ctrl Pts',(0.0771999187120617,0.135040642218745,
-0.658483296497409));
#79228=CARTESIAN_POINT('Ctrl Pts',(0.0680918118152083,0.140247556970519,
-0.657733926868962));
#79229=CARTESIAN_POINT('Ctrl Pts',(0.0584615751935578,0.144525004141135,
-0.656984557240514));
#79230=CARTESIAN_POINT('Ctrl Pts',(0.0485226794565229,0.147788200064686,
-0.656235187612067));
#79231=CARTESIAN_POINT('Ctrl Pts',(0.0385837837194877,0.151051395988236,
-0.655485817983619));
#79232=CARTESIAN_POINT('Ctrl Pts',(0.0283372194356101,0.153300157887608,
-0.654736448355172));
#79233=CARTESIAN_POINT('Ctrl Pts',(0.0180083972417708,0.154504045671246,
-0.653987078726724));
#79234=CARTESIAN_POINT('Ctrl Pts',(0.00784227137744584,0.155688970196551,
-0.653249512930864));
#79235=CARTESIAN_POINT('Ctrl Pts',(-0.00247908354990559,0.155870624577179,
-0.652511947135003));
#79236=CARTESIAN_POINT('Ctrl Pts',(-0.0127398803529513,0.155027410313765,
-0.651774381339143));
#79237=CARTESIAN_POINT('Ctrl Pts',(-0.0230250688013239,0.154182191587769,
-0.651035062224935));
#79238=CARTESIAN_POINT('Ctrl Pts',(-0.0332484744830392,0.152307154402499,
-0.650295743110727));
#79239=CARTESIAN_POINT('Ctrl Pts',(-0.0431917212150337,0.149433188142671,
-0.649556423996518));
#79240=CARTESIAN_POINT('Ctrl Pts',(-0.0530887440673171,0.146572582294614,
-0.648820541807766));
#79241=CARTESIAN_POINT('Ctrl Pts',(-0.0627073101166465,0.142722570256699,
-0.648084659619013));
#79242=CARTESIAN_POINT('Ctrl Pts',(-0.071844831253178,0.137964208120086,
-0.64734877743026));
#79243=CARTESIAN_POINT('Ctrl Pts',(-0.0810463673491841,0.133172510207304,
-0.646607739853325));
#79244=CARTESIAN_POINT('Ctrl Pts',(-0.0897592437340419,0.127460112423326,
-0.645866702276389));
#79245=CARTESIAN_POINT('Ctrl Pts',(-0.0978028222610833,0.120956233645757,
-0.645125664699453));
#79246=CARTESIAN_POINT('Ctrl Pts',(-0.105846400788125,0.114452354868188,
-0.644384627122517));
#79247=CARTESIAN_POINT('Ctrl Pts',(-0.113220028681602,0.107157688757977,
-0.643643589545581));
#79248=CARTESIAN_POINT('Ctrl Pts',(-0.119780550983552,0.0992392165732715,
-0.642902551968645));
#79249=CARTESIAN_POINT('Ctrl Pts',(-0.126276902004641,0.0913981983593276,
-0.642168762797902));
#79250=CARTESIAN_POINT('Ctrl Pts',(-0.132025858922605,0.0828853067841873,
-0.641434973627158));
#79251=CARTESIAN_POINT('Ctrl Pts',(-0.136891903116717,0.0738675122166936,
-0.640701184456415));
#79252=CARTESIAN_POINT('Ctrl Pts',(-0.141747285352497,0.0648694764812375,
-0.639969003086433));
#79253=CARTESIAN_POINT('Ctrl Pts',(-0.145723079744574,0.0553695093407535,
-0.639236821716451));
#79254=CARTESIAN_POINT('Ctrl Pts',(-0.148727361559918,0.0455628623269607,
-0.638504640346469));
#79255=CARTESIAN_POINT('Ctrl Pts',(-0.151731044320082,0.0357581707631058,
-0.637772604973791));
#79256=CARTESIAN_POINT('Ctrl Pts',(-0.153763287048736,0.0256478034881993,
-0.637040569601112));
#79257=CARTESIAN_POINT('Ctrl Pts',(-0.15478141922985,0.0154439231153664,
-0.636308534228433));
#79258=CARTESIAN_POINT('Ctrl Pts',(-0.155297951137016,0.0102671593441833,
-0.635937148632165));
#79259=CARTESIAN_POINT('Ctrl Pts',(-0.155554281048676,0.00506651542239916,
-0.635565763035898));
#79260=CARTESIAN_POINT('Ctrl Pts',(-0.155549945866256,-0.000129772897362374,
-0.63519437743963));
#79261=CARTESIAN_POINT('',(-0.155549974362134,8.93081152335447E-5,-0.649113732242943));
#79262=CARTESIAN_POINT('Ctrl Pts',(0.102342242758987,0.117140376672865,
-0.674376033428004));
#79263=CARTESIAN_POINT('Ctrl Pts',(0.101191146679549,0.118146056846915,
-0.674271112963107));
#79264=CARTESIAN_POINT('Ctrl Pts',(0.100025160633051,0.119134827817089,
-0.674167025422502));
#79265=CARTESIAN_POINT('Ctrl Pts',(0.0930757671449147,0.124854012298398,
-0.673558102406125));
#79266=CARTESIAN_POINT('Ctrl Pts',(0.0869719332770196,0.129180186700844,
-0.673068760632657));
#79267=CARTESIAN_POINT('Ctrl Pts',(0.0730551137837119,0.137608702257919,
-0.671996546687483));
#79268=CARTESIAN_POINT('Ctrl Pts',(0.0651575809181942,0.141519146308847,
-0.671413937645293));
#79269=CARTESIAN_POINT('Ctrl Pts',(0.0549485145970029,0.145537603928452,
-0.670658934752614));
#79270=CARTESIAN_POINT('Ctrl Pts',(0.0529081943963351,0.146291679847769,
-0.67050802655823));
#79271=CARTESIAN_POINT('Ctrl Pts',(0.0495389084353664,0.147457220899202,
-0.67025838283206));
#79272=CARTESIAN_POINT('Ctrl Pts',(0.0482190047314951,0.147894093207751,
-0.670160477969575));
#79273=CARTESIAN_POINT('Ctrl Pts',(0.0458203554904981,0.148652494745097,
-0.669982266902835));
#79274=CARTESIAN_POINT('Ctrl Pts',(0.0447436272982595,0.148980122386781,
-0.669902165658211));
#79275=CARTESIAN_POINT('Ctrl Pts',(0.0424101767448871,0.149662568761497,
-0.669728299214583));
#79276=CARTESIAN_POINT('Ctrl Pts',(0.0411523602496633,0.150013301523527,
-0.669634408596997));
#79277=CARTESIAN_POINT('Ctrl Pts',(0.0376115687397058,0.150952742944754,
-0.669369549457639));
#79278=CARTESIAN_POINT('Ctrl Pts',(0.0353194967195086,0.151505421476829,
-0.669197450384273));
#79279=CARTESIAN_POINT('Ctrl Pts',(0.0251858815772117,0.15370645654733,
-0.668433319164996));
#79280=CARTESIAN_POINT('Ctrl Pts',(0.0172373973561568,0.154799353730613,
-0.66782456991791));
#79281=CARTESIAN_POINT('Ctrl Pts',(0.000392267604439727,0.15580189340765,
-0.666522944935293));
#79282=CARTESIAN_POINT('Ctrl Pts',(-0.008485581668265,0.155571157436399,
-0.665830232916812));
#79283=CARTESIAN_POINT('Ctrl Pts',(-0.0203867252573994,0.154239614684418,
-0.66492033771237));
#79284=CARTESIAN_POINT('Ctrl Pts',(-0.0234670678594841,0.153801096306821,
-0.664686682487581));
#79285=CARTESIAN_POINT('Ctrl Pts',(-0.0275554599292424,0.153093360696824,
-0.664380717088592));
#79286=CARTESIAN_POINT('Ctrl Pts',(-0.0285767324465484,0.152906020090096,
-0.66430463731119));
#79287=CARTESIAN_POINT('Ctrl Pts',(-0.0301878069677704,0.152593781302567,
-0.664185252924315));
#79288=CARTESIAN_POINT('Ctrl Pts',(-0.0307788671257554,0.152475660855673,
-0.664141589164485));
#79289=CARTESIAN_POINT('Ctrl Pts',(-0.032018106000498,0.152220505403247,
-0.664050347060237));
#79290=CARTESIAN_POINT('Ctrl Pts',(-0.0326661224021602,0.152082759880494,
-0.664002812867636));
#79291=CARTESIAN_POINT('Ctrl Pts',(-0.0342968378213496,0.151725223235351,
-0.663883597824645));
#79292=CARTESIAN_POINT('Ctrl Pts',(-0.0352783423295761,0.151500017010828,
-0.663812214000121));
#79293=CARTESIAN_POINT('Ctrl Pts',(-0.0392668640684486,0.150543985878361,
-0.663523382118335));
#79294=CARTESIAN_POINT('Ctrl Pts',(-0.0422541634248812,0.149732986187034,
-0.663309953831452));
#79295=CARTESIAN_POINT('Ctrl Pts',(-0.050709472318709,0.147164266272489,
-0.662708948812627));
#79296=CARTESIAN_POINT('Ctrl Pts',(-0.0561072127042601,0.145192155724305,
-0.662328927186861));
#79297=CARTESIAN_POINT('Ctrl Pts',(-0.0717400525541236,0.138478159013006,
-0.661207040752277));
#79298=CARTESIAN_POINT('Ctrl Pts',(-0.0815809885868729,0.132918564187561,
-0.660469954097329));
#79299=CARTESIAN_POINT('Ctrl Pts',(-0.0926031280196733,0.125003022254412,
-0.659535073818111));
#79300=CARTESIAN_POINT('Ctrl Pts',(-0.0944416294060303,0.123619871327327,
-0.659375195560815));
#79301=CARTESIAN_POINT('Ctrl Pts',(-0.0972757672319868,0.121387548376986,
-0.659122002252391));
#79302=CARTESIAN_POINT('Ctrl Pts',(-0.0982925610520427,0.120565683542686,
-0.659029755389586));
#79303=CARTESIAN_POINT('Ctrl Pts',(-0.100111459381183,0.119057182614937,
-0.658862089527016));
#79304=CARTESIAN_POINT('Ctrl Pts',(-0.100917170555288,0.118375004196761,
-0.658786853466611));
#79305=CARTESIAN_POINT('Ctrl Pts',(-0.101832265207055,0.117584080284343,
-0.658700266580737));
#79306=CARTESIAN_POINT('Ctrl Pts',(-0.101948523075608,0.117483295901606,
-0.658689244925735));
#79307=CARTESIAN_POINT('Ctrl Pts',(-0.102109658066315,0.117343188084639,
-0.658673939155643));
#79308=CARTESIAN_POINT('Ctrl Pts',(-0.102154662707767,0.117304010789618,
-0.658669661075927));
#79309=CARTESIAN_POINT('Ctrl Pts',(-0.102221014918879,0.117246182933686,
-0.658663348980168));
#79310=CARTESIAN_POINT('Ctrl Pts',(-0.102242379994868,0.117227552378049,
-0.658661315790858));
#79311=CARTESIAN_POINT('Ctrl Pts',(-0.10233817386207,0.117143973078278,
-0.658652196388826));
#79312=CARTESIAN_POINT('Ctrl Pts',(-0.102412545721494,0.117078959410936,
-0.658645107493641));
#79313=CARTESIAN_POINT('Ctrl Pts',(-0.102555142941754,0.116954065327314,
-0.658631498586842));
#79314=CARTESIAN_POINT('Ctrl Pts',(-0.102623377938085,0.116894195924784,
-0.658624979033036));
#79315=CARTESIAN_POINT('Ctrl Pts',(-0.102755691774694,0.116777898585883,
-0.658612322483519));
#79316=CARTESIAN_POINT('Ctrl Pts',(-0.102819776654293,0.116721477539218,
-0.658606185774921));
#79317=CARTESIAN_POINT('Ctrl Pts',(-0.102945281708731,0.116610797914942,
-0.658594154497396));
#79318=CARTESIAN_POINT('Ctrl Pts',(-0.103006705531186,0.116556543497196,
-0.658588260102407));
#79319=CARTESIAN_POINT('Ctrl Pts',(-0.10312807706735,0.116449167605556,
-0.658576600821216));
#79320=CARTESIAN_POINT('Ctrl Pts',(-0.103188026688685,0.116396048316458,
-0.658570836026945));
#79321=CARTESIAN_POINT('Ctrl Pts',(-0.103307457246567,0.116290060238851,
-0.658559339784915));
#79322=CARTESIAN_POINT('Ctrl Pts',(-0.103366938694209,0.116237192060248,
-0.658553608363612));
#79323=CARTESIAN_POINT('Ctrl Pts',(-0.103486340718961,0.116130901266918,
-0.658542091519896));
#79324=CARTESIAN_POINT('Ctrl Pts',(-0.103546260561809,0.116077477867538,
-0.658536306065882));
#79325=CARTESIAN_POINT('Ctrl Pts',(-0.103667407098685,0.115969297456227,
-0.658524596969065));
#79326=CARTESIAN_POINT('Ctrl Pts',(-0.103728631824934,0.115914538288926,
-0.65851867323754));
#79327=CARTESIAN_POINT('Ctrl Pts',(-0.103853263511517,0.115802890355983,
-0.658506601945836));
#79328=CARTESIAN_POINT('Ctrl Pts',(-0.103916667162697,0.115745997954731,
-0.658500454235187));
#79329=CARTESIAN_POINT('Ctrl Pts',(-0.105506390801845,0.114317172176548,
-0.658346143786108));
#79330=CARTESIAN_POINT('Ctrl Pts',(-0.107005387180538,0.112915281193089,
-0.658196734748946));
#79331=CARTESIAN_POINT('Ctrl Pts',(-0.110296800040051,0.109712676984326,
-0.657859612855542));
#79332=CARTESIAN_POINT('Ctrl Pts',(-0.112073683441505,0.107896912522107,
-0.657671291284155));
#79333=CARTESIAN_POINT('Ctrl Pts',(-0.11762458060116,0.101939446039894,
-0.657062122102572));
#79334=CARTESIAN_POINT('Ctrl Pts',(-0.12121931945391,0.0976373808579105,
-0.656634953057946));
#79335=CARTESIAN_POINT('Ctrl Pts',(-0.129548842673277,0.0864980587898974,
-0.655563254996515));
#79336=CARTESIAN_POINT('Ctrl Pts',(-0.133982769905782,0.0794571283625117,
-0.654914572160442));
#79337=CARTESIAN_POINT('Ctrl Pts',(-0.13962530764626,0.0686696853378198,
-0.653984048898601));
#79338=CARTESIAN_POINT('Ctrl Pts',(-0.141289192072979,0.065177619195162,
-0.653691947808538));
#79339=CARTESIAN_POINT('Ctrl Pts',(-0.143262478660383,0.0606044928527206,
-0.65332399864148));
#79340=CARTESIAN_POINT('Ctrl Pts',(-0.143692652832446,0.0595773787399836,
-0.65324228330971));
#79341=CARTESIAN_POINT('Ctrl Pts',(-0.144369644865931,0.0579109449523117,
-0.653111291884689));
#79342=CARTESIAN_POINT('Ctrl Pts',(-0.144623323584781,0.0572744814716124,
-0.653061632451789));
#79343=CARTESIAN_POINT('Ctrl Pts',(-0.145114513979685,0.0560180422748632,
-0.652964356018714));
#79344=CARTESIAN_POINT('Ctrl Pts',(-0.145352275943719,0.0553981871207527,
-0.652916726655579));
#79345=CARTESIAN_POINT('Ctrl Pts',(-0.145943082203899,0.0538279396423758,
-0.652796934779546));
#79346=CARTESIAN_POINT('Ctrl Pts',(-0.146290825206794,0.0528755608367879,
-0.652725075346112));
#79347=CARTESIAN_POINT('Ctrl Pts',(-0.147682944950127,0.0489440087403064,
-0.652431423930231));
#79348=CARTESIAN_POINT('Ctrl Pts',(-0.148645902061094,0.0459365581875476,
-0.652213822481557));
#79349=CARTESIAN_POINT('Ctrl Pts',(-0.153510914817863,0.0289814762591141,
-0.651015006652198));
#79350=CARTESIAN_POINT('Ctrl Pts',(-0.155541659225333,0.0145719708928448,
-0.65009394675668));
#79351=CARTESIAN_POINT('Ctrl Pts',(-0.155549974362134,8.93081152335447E-5,
-0.649113732242943));
#79352=CARTESIAN_POINT('Ctrl Pts',(-0.155549974470581,8.91190302388376E-5,
-0.649113719445304));
#79353=CARTESIAN_POINT('Ctrl Pts',(-0.155551459251949,-0.00250244534429518,
-0.648938317303811));
#79354=CARTESIAN_POINT('Ctrl Pts',(-0.155488178294614,-0.0050935523913905,
-0.648761442142846));
#79355=CARTESIAN_POINT('Ctrl Pts',(-0.15526486225176,-0.00961000152068747,
-0.648449601131202));
#79356=CARTESIAN_POINT('Ctrl Pts',(-0.155133636844657,-0.0115361927770886,
-0.648315482084797));
#79357=CARTESIAN_POINT('Ctrl Pts',(-0.154869829583466,-0.0145735789585794,
-0.648101942028573));
#79358=CARTESIAN_POINT('Ctrl Pts',(-0.154761045520123,-0.0156866820434499,
-0.648023251010666));
#79359=CARTESIAN_POINT('Ctrl Pts',(-0.154524027502421,-0.0178685763627349,
-0.647868091716286));
#79360=CARTESIAN_POINT('Ctrl Pts',(-0.154396683232695,-0.0189374020972839,
-0.647791655193124));
#79361=CARTESIAN_POINT('Ctrl Pts',(-0.154102257738286,-0.0212077358565061,
-0.647628333460605));
#79362=CARTESIAN_POINT('Ctrl Pts',(-0.153932194339202,-0.0224087771374998,
-0.647541359647675));
#79363=CARTESIAN_POINT('Ctrl Pts',(-0.153458170911275,-0.0254959172861875,
-0.647316260655064));
#79364=CARTESIAN_POINT('Ctrl Pts',(-0.153133487550905,-0.0273785757199024,
-0.647177495841913));
#79365=CARTESIAN_POINT('Ctrl Pts',(-0.15148296628841,-0.0359979460366745,
-0.646535030361311));
#79366=CARTESIAN_POINT('Ctrl Pts',(-0.149746862360095,-0.0426473206902234,
-0.646018716962129));
#79367=CARTESIAN_POINT('Ctrl Pts',(-0.144312107398187,-0.058962539639381,
-0.64470210320504));
#79368=CARTESIAN_POINT('Ctrl Pts',(-0.140078185731863,-0.0684153254219521,
-0.64389211107294));
#79369=CARTESIAN_POINT('Ctrl Pts',(-0.133156074428233,-0.0804866501165299,
-0.642831117833079));
#79370=CARTESIAN_POINT('Ctrl Pts',(-0.131266632263183,-0.0835327296734139,
-0.642561128678344));
#79371=CARTESIAN_POINT('Ctrl Pts',(-0.128685650421676,-0.0873894904439736,
-0.642218760198617));
#79372=CARTESIAN_POINT('Ctrl Pts',(-0.128088849172488,-0.0882619201353838,
-0.642141279424662));
#79373=CARTESIAN_POINT('Ctrl Pts',(-0.127097607787183,-0.0896797268575393,
-0.642015393009744));
#79374=CARTESIAN_POINT('Ctrl Pts',(-0.126708451022431,-0.0902287304665876,
-0.641966654610755));
#79375=CARTESIAN_POINT('Ctrl Pts',(-0.125969069580601,-0.0912575963176893,
-0.641875355922972));
#79376=CARTESIAN_POINT('Ctrl Pts',(-0.125619637324001,-0.0917380080832283,
-0.641832742045428));
#79377=CARTESIAN_POINT('Ctrl Pts',(-0.124679801572681,-0.0930146878238521,
-0.641719506095405));
#79378=CARTESIAN_POINT('Ctrl Pts',(-0.124084512211861,-0.093807350648264,
-0.64164920991549));
#79379=CARTESIAN_POINT('Ctrl Pts',(-0.121817588251036,-0.0967665517765677,
-0.64138658344035));
#79380=CARTESIAN_POINT('Ctrl Pts',(-0.120096352535078,-0.0988946849955261,
-0.641197315738529));
#79381=CARTESIAN_POINT('Ctrl Pts',(-0.112374116134005,-0.107943259892743,
-0.640385261101784));
#79382=CARTESIAN_POINT('Ctrl Pts',(-0.10582425465258,-0.114371969822372,
-0.639788240768916));
#79383=CARTESIAN_POINT('Ctrl Pts',(-0.092441879549769,-0.125366956881615,
-0.638645681777124));
#79384=CARTESIAN_POINT('Ctrl Pts',(-0.085740558252307,-0.130041951416835,
-0.638103409703136));
#79385=CARTESIAN_POINT('Ctrl Pts',(-0.0766544227550917,-0.135371889386149,
-0.637378149651699));
#79386=CARTESIAN_POINT('Ctrl Pts',(-0.0745776265641524,-0.136527013981853,
-0.637213074924721));
#79387=CARTESIAN_POINT('Ctrl Pts',(-0.071316542888142,-0.138244233817961,
-0.636954433447759));
#79388=CARTESIAN_POINT('Ctrl Pts',(-0.0701501798635377,-0.138839726131943,
-0.636862038587155));
#79389=CARTESIAN_POINT('Ctrl Pts',(-0.0679679455006226,-0.139919358764587,
-0.636689296592742));
#79390=CARTESIAN_POINT('Ctrl Pts',(-0.066954063558749,-0.140407342487198,
-0.6366090893944));
#79391=CARTESIAN_POINT('Ctrl Pts',(-0.0646801518762896,-0.141471551896206,
-0.636429264155266));
#79392=CARTESIAN_POINT('Ctrl Pts',(-0.063417551680542,-0.142042021783284,
-0.636329456733153));
#79393=CARTESIAN_POINT('Ctrl Pts',(-0.0601688684370673,-0.143457898255239,
-0.636072675100242));
#79394=CARTESIAN_POINT('Ctrl Pts',(-0.0581725614188709,-0.144278943511313,
-0.63591490297013));
#79395=CARTESIAN_POINT('Ctrl Pts',(-0.0469785878072871,-0.148612740066354,
-0.635029941825449));
#79396=CARTESIAN_POINT('Ctrl Pts',(-0.0374820739757276,-0.151287033083471,
-0.634276050847694));
#79397=CARTESIAN_POINT('Ctrl Pts',(-0.0212056352631647,-0.154243379994563,
-0.632994961965968));
#79398=CARTESIAN_POINT('Ctrl Pts',(-0.014542268405264,-0.155013640728622,
-0.632474093920613));
#79399=CARTESIAN_POINT('Ctrl Pts',(-0.00447444041750365,-0.155522357958324,
-0.631706721570313));
#79400=CARTESIAN_POINT('Ctrl Pts',(-0.0010941409852425,-0.155582876009482,
-0.631452454292036));
#79401=CARTESIAN_POINT('Ctrl Pts',(0.00332277466916035,-0.155517964800422,
-0.631126720858724));
#79402=CARTESIAN_POINT('Ctrl Pts',(0.00435968517377682,-0.155492351926568,
-0.631050722395967));
#79403=CARTESIAN_POINT('Ctrl Pts',(0.00606460273096834,-0.155433169761592,
-0.630926619248101));
#79404=CARTESIAN_POINT('Ctrl Pts',(0.00673277000123357,-0.155405661189494,
-0.630878198849048));
#79405=CARTESIAN_POINT('Ctrl Pts',(0.0079972616151005,-0.155345430989557,
-0.630786999597896));
#79406=CARTESIAN_POINT('Ctrl Pts',(0.00859360916398867,-0.155313582910381,
-0.630744171762612));
#79407=CARTESIAN_POINT('Ctrl Pts',(0.0101966026689352,-0.1552187136034,
-0.630629505179566));
#79408=CARTESIAN_POINT('Ctrl Pts',(0.0112028652170258,-0.155149333584473,
-0.630558007685805));
#79409=CARTESIAN_POINT('Ctrl Pts',(0.0150684457240935,-0.154845002855718,
-0.630284959795451));
#79410=CARTESIAN_POINT('Ctrl Pts',(0.0179219250079935,-0.15454073942436,
-0.630086793148586));
#79411=CARTESIAN_POINT('Ctrl Pts',(0.0297375545020742,-0.152949133652808,
-0.629274254225004));
#79412=CARTESIAN_POINT('Ctrl Pts',(0.0385876831871622,-0.150959528372375,
-0.628684145181647));
#79413=CARTESIAN_POINT('Ctrl Pts',(0.0549392729532534,-0.145750459846946,
-0.62755191391849));
#79414=CARTESIAN_POINT('Ctrl Pts',(0.0624584030346325,-0.142690034231669,
-0.627012955238379));
#79415=CARTESIAN_POINT('Ctrl Pts',(0.0718226847182252,-0.137996084902389,
-0.626291705810336));
#79416=CARTESIAN_POINT('Ctrl Pts',(0.0739164034357701,-0.136886017425754,
-0.626127080638367));
#79417=CARTESIAN_POINT('Ctrl Pts',(0.0771253805785011,-0.135089561497619,
-0.625868988568626));
#79418=CARTESIAN_POINT('Ctrl Pts',(0.078258762798155,-0.13443615516184,
-0.625776685326374));
#79419=CARTESIAN_POINT('Ctrl Pts',(0.0803514556195962,-0.133194265480418,
-0.625604027226321));
#79420=CARTESIAN_POINT('Ctrl Pts',(0.0813128884728513,-0.13260951256942,
-0.625523811189525));
#79421=CARTESIAN_POINT('Ctrl Pts',(0.0834451585095739,-0.131280738420449,
-0.62534385225559));
#79422=CARTESIAN_POINT('Ctrl Pts',(0.0846125442178338,-0.130531390438542,
-0.625243918636892));
#79423=CARTESIAN_POINT('Ctrl Pts',(0.0875752582063992,-0.128573172861007,
-0.624986578062361));
#79424=CARTESIAN_POINT('Ctrl Pts',(0.0893556074004888,-0.127342299298565,
-0.624828367207782));
#79425=CARTESIAN_POINT('Ctrl Pts',(0.0987857444887335,-0.1205274829385,
-0.623970521423895));
#79426=CARTESIAN_POINT('Ctrl Pts',(0.105937948927599,-0.114291699787246,
-0.623246388771629));
#79427=CARTESIAN_POINT('Ctrl Pts',(0.117294928123706,-0.102402814555705,
-0.621973771851205));
#79428=CARTESIAN_POINT('Ctrl Pts',(0.121767641019183,-0.0970416665268637,
-0.621431172570384));
#79429=CARTESIAN_POINT('Ctrl Pts',(0.12789512220191,-0.0886034443560276,
-0.620636854616848));
#79430=CARTESIAN_POINT('Ctrl Pts',(0.129831164101717,-0.0857415051591593,
-0.620376844467932));
#79431=CARTESIAN_POINT('Ctrl Pts',(0.132226596468878,-0.0819330262774496,
-0.620045018648924));
#79432=CARTESIAN_POINT('Ctrl Pts',(0.132773836970716,-0.0810432105931554,
-0.619968466270191));
#79433=CARTESIAN_POINT('Ctrl Pts',(0.133657451309003,-0.0795734721546524,
-0.619843697371071));
#79434=CARTESIAN_POINT('Ctrl Pts',(0.133999104310011,-0.0789967838365404,
-0.619795158787579));
#79435=CARTESIAN_POINT('Ctrl Pts',(0.134637472493181,-0.0779032006465429,
-0.619703925990048));
#79436=CARTESIAN_POINT('Ctrl Pts',(0.134934962843697,-0.0773867786173892,
-0.619661181046791));
#79437=CARTESIAN_POINT('Ctrl Pts',(0.13572461285842,-0.0759976041322065,
-0.619547064480951));
#79438=CARTESIAN_POINT('Ctrl Pts',(0.136211331025798,-0.0751217665464271,
-0.619476028189553));
#79439=CARTESIAN_POINT('Ctrl Pts',(0.138034211728411,-0.0717655628918832,
-0.619207031457263));
#79440=CARTESIAN_POINT('Ctrl Pts',(0.139311452478313,-0.0692536012179142,
-0.619012327884833));
#79441=CARTESIAN_POINT('Ctrl Pts',(0.144419866941461,-0.0584927917705782,
-0.618199996887239));
#79442=CARTESIAN_POINT('Ctrl Pts',(0.147592273629558,-0.04995052663425,
-0.617607210752402));
#79443=CARTESIAN_POINT('Ctrl Pts',(0.152151716982168,-0.0333422605614492,
-0.616470976073304));
#79444=CARTESIAN_POINT('Ctrl Pts',(0.153685494673246,-0.02534951036745,
-0.615930731204967));
#79445=CARTESIAN_POINT('Ctrl Pts',(0.154851298654041,-0.0149166021801462,
-0.615207924904403));
#79446=CARTESIAN_POINT('Ctrl Pts',(0.155060757134233,-0.0125534968938902,
-0.615043124944915));
#79447=CARTESIAN_POINT('Ctrl Pts',(0.155301798614254,-0.00888069085844641,
-0.614784819258134));
#79448=CARTESIAN_POINT('Ctrl Pts',(0.15537101826593,-0.00757375865328602,
-0.614692480384588));
#79449=CARTESIAN_POINT('Ctrl Pts',(0.155469066251677,-0.00514180273128026,
-0.614519789692284));
#79450=CARTESIAN_POINT('Ctrl Pts',(0.155502193026476,-0.00401703113108116,
-0.61443957712816));
#79451=CARTESIAN_POINT('Ctrl Pts',(0.155548891444341,-0.00150575205152136,
-0.614259670362665));
#79452=CARTESIAN_POINT('Ctrl Pts',(0.155556132862643,-0.000119238764841339,
-0.614159785962396));
#79453=CARTESIAN_POINT('Ctrl Pts',(0.155527226552163,0.00342907291418397,
-0.613902663430653));
#79454=CARTESIAN_POINT('Ctrl Pts',(0.155464544200951,0.00559029285697034,
-0.61374462373537));
#79455=CARTESIAN_POINT('Ctrl Pts',(0.154876635500673,0.0173764369529321,
-0.612874569885442));
#79456=CARTESIAN_POINT('Ctrl Pts',(0.153502720513309,0.0269363891684311,
-0.612137081877608));
#79457=CARTESIAN_POINT('Ctrl Pts',(0.149654764192167,0.0429671871826022,
-0.610860707820909));
#79458=CARTESIAN_POINT('Ctrl Pts',(0.147617576798016,0.0495155091307251,
-0.610327938452325));
#79459=CARTESIAN_POINT('Ctrl Pts',(0.143925777929179,0.0591005442025626,
-0.60954578105697));
#79460=CARTESIAN_POINT('Ctrl Pts',(0.142591209242072,0.0622515466705997,
-0.609288341104641));
#79461=CARTESIAN_POINT('Ctrl Pts',(0.140716190379459,0.0663011351181469,
-0.608959239596094));
#79462=CARTESIAN_POINT('Ctrl Pts',(0.14026919316207,0.0672416564308969,
-0.608882933308951));
#79463=CARTESIAN_POINT('Ctrl Pts',(0.13951929437926,0.068779483312375,-0.608758460284638));
#79464=CARTESIAN_POINT('Ctrl Pts',(0.139221928508128,0.0693794314145882,
-0.608709974308017));
#79465=CARTESIAN_POINT('Ctrl Pts',(0.13865234277528,0.0705101847287545,
-0.608618756965748));
#79466=CARTESIAN_POINT('Ctrl Pts',(0.138380928248831,0.0710413755265428,
-0.608575975642808));
#79467=CARTESIAN_POINT('Ctrl Pts',(0.137644104688197,0.0724631816651877,
-0.60846161706615));
#79468=CARTESIAN_POINT('Ctrl Pts',(0.137173100200892,0.0733508893903533,
-0.608390377746996));
#79469=CARTESIAN_POINT('Ctrl Pts',(0.135338214724856,0.0767296232912663,
-0.608119605517211));
#79470=CARTESIAN_POINT('Ctrl Pts',(0.133914723007637,0.0791878584081466,
-0.607923384763523));
#79471=CARTESIAN_POINT('Ctrl Pts',(0.127047033176055,0.0903322845749481,
-0.607030912771506));
#79472=CARTESIAN_POINT('Ctrl Pts',(0.120819624200894,0.0985064803861634,
-0.606366581606531));
#79473=CARTESIAN_POINT('Ctrl Pts',(0.11030473340754,0.109797387405944,-0.605345710376678));
#79474=CARTESIAN_POINT('Ctrl Pts',(0.106590097086477,0.113406990932573,
-0.605000559159934));
#79475=CARTESIAN_POINT('Ctrl Pts',(0.102582667496328,0.116929997632619,
-0.604637895112637));
#79476=CARTESIAN_POINT('Ctrl Pts',(0.102462535204728,0.117035280556151,
-0.604627032087788));
#79477=CARTESIAN_POINT('Ctrl Pts',(0.102342242827937,0.117140376612625,
-0.604616163143584));
#79478=CARTESIAN_POINT('Origin',(0.,0.,-1.10400562256037));
#79479=CARTESIAN_POINT('',(0.10234224283772,0.117140376604078,-0.520692779095311));
#79480=CARTESIAN_POINT('',(0.102342237477092,0.117140381287507,-0.534570457414543));
#79481=CARTESIAN_POINT('',(0.10234224283772,0.117140376604078,-1.10400562256037));
#79482=CARTESIAN_POINT('',(-0.155549999681985,9.9465836413514E-6,-0.565194377435295));
#79483=CARTESIAN_POINT('Ctrl Pts',(-0.155549999681985,9.9465836413514E-6,
-0.565194377435295));
#79484=CARTESIAN_POINT('Ctrl Pts',(-0.155550652961944,-0.0102063951447715,
-0.564458166637774));
#79485=CARTESIAN_POINT('Ctrl Pts',(-0.154540483344138,-0.0204614277915781,
-0.563721955840253));
#79486=CARTESIAN_POINT('Ctrl Pts',(-0.152522697323478,-0.0305389800283305,
-0.562985745042732));
#79487=CARTESIAN_POINT('Ctrl Pts',(-0.150507519952113,-0.0406035037282293,
-0.56225048603879));
#79488=CARTESIAN_POINT('Ctrl Pts',(-0.147487397691107,-0.0504900784062613,
-0.561515227034848));
#79489=CARTESIAN_POINT('Ctrl Pts',(-0.143517271214654,-0.059988293550488,
-0.560779968030905));
#79490=CARTESIAN_POINT('Ctrl Pts',(-0.139551022262881,-0.0694772320220811,
-0.560045427136311));
#79491=CARTESIAN_POINT('Ctrl Pts',(-0.134636952228676,-0.0785776981356956,
-0.559310886241716));
#79492=CARTESIAN_POINT('Ctrl Pts',(-0.12887853867428,-0.0870983626090755,
-0.558576345347122));
#79493=CARTESIAN_POINT('Ctrl Pts',(-0.123105816881007,-0.0956401988342802,
-0.557839979299386));
#79494=CARTESIAN_POINT('Ctrl Pts',(-0.116485094228212,-0.103598584776286,
-0.557103613251651));
#79495=CARTESIAN_POINT('Ctrl Pts',(-0.109163042999335,-0.110811698584244,
-0.556367247203916));
#79496=CARTESIAN_POINT('Ctrl Pts',(-0.102067003550593,-0.117802163213564,
-0.555653610770612));
#79497=CARTESIAN_POINT('Ctrl Pts',(-0.0943130906390056,-0.124092347201511,
-0.554939974337308));
#79498=CARTESIAN_POINT('Ctrl Pts',(-0.0860640892451476,-0.12957150551878,
-0.554226337904004));
#79499=CARTESIAN_POINT('Ctrl Pts',(-0.0775384857385886,-0.13523438871304,
-0.553488772108135));
#79500=CARTESIAN_POINT('Ctrl Pts',(-0.0684198911666055,-0.140073252100748,
-0.552751206312266));
#79501=CARTESIAN_POINT('Ctrl Pts',(-0.0588908807238225,-0.143971061910276,
-0.552013640516397));
#79502=CARTESIAN_POINT('Ctrl Pts',(-0.0493392182155014,-0.147878137471352,
-0.551274321402191));
#79503=CARTESIAN_POINT('Ctrl Pts',(-0.0393759886201371,-0.150839192048426,
-0.550535002287985));
#79504=CARTESIAN_POINT('Ctrl Pts',(-0.0292098589783628,-0.152782808713756,
-0.549795683173779));
#79505=CARTESIAN_POINT('Ctrl Pts',(-0.0190909893478124,-0.154717389949807,
-0.549059800985017));
#79506=CARTESIAN_POINT('Ctrl Pts',(-0.00877201741954846,-0.155643793686536,
-0.548323918796255));
#79507=CARTESIAN_POINT('Ctrl Pts',(0.00152973184211935,-0.155542477865345,
-0.547588036607493));
#79508=CARTESIAN_POINT('Ctrl Pts',(0.0119036523250068,-0.155440452253383,
-0.546846999030565));
#79509=CARTESIAN_POINT('Ctrl Pts',(0.0222591580446818,-0.154296247452144,
-0.546105961453637));
#79510=CARTESIAN_POINT('Ctrl Pts',(0.0323766671306018,-0.152143202035169,
-0.545364923876708));
#79511=CARTESIAN_POINT('Ctrl Pts',(0.0424941762165218,-0.149990156618194,
-0.54462388629978));
#79512=CARTESIAN_POINT('Ctrl Pts',(0.0523727924363232,-0.146828593152129,
-0.543882848722852));
#79513=CARTESIAN_POINT('Ctrl Pts',(0.0618092367599878,-0.142742498055582,
-0.543141811145923));
#79514=CARTESIAN_POINT('Ctrl Pts',(0.0712014710871692,-0.138675546424905,
-0.542404245350054));
#79515=CARTESIAN_POINT('Ctrl Pts',(0.0802254889893704,-0.133662516726816,
-0.541666679554185));
#79516=CARTESIAN_POINT('Ctrl Pts',(0.0886837096846341,-0.127792809408713,
-0.540929113758316));
#79517=CARTESIAN_POINT('Ctrl Pts',(0.0971620369975398,-0.121909148805992,
-0.54018979464411));
#79518=CARTESIAN_POINT('Ctrl Pts',(0.105071027690536,-0.11516514002809,
-0.539450475529904));
#79519=CARTESIAN_POINT('Ctrl Pts',(0.112237152853552,-0.107696908123346,
-0.538711156415698));
#79520=CARTESIAN_POINT('Ctrl Pts',(0.119369964339924,-0.100263394320381,
-0.537975274226936));
#79521=CARTESIAN_POINT('Ctrl Pts',(0.125766153760101,-0.0921130466933787,
-0.537239392038174));
#79522=CARTESIAN_POINT('Ctrl Pts',(0.1312909864909,-0.0834175003596152,
-0.536503509849412));
#79523=CARTESIAN_POINT('Ctrl Pts',(0.136854524679874,-0.0746610354204685,
-0.535762472272484));
#79524=CARTESIAN_POINT('Ctrl Pts',(0.141533929313437,-0.0653524976398771,
-0.535021434695556));
#79525=CARTESIAN_POINT('Ctrl Pts',(0.145237589286669,-0.0556942111731263,
-0.534280397118628));
#79526=CARTESIAN_POINT('Ctrl Pts',(0.148941249259901,-0.0460359247063756,
-0.5335393595417));
#79527=CARTESIAN_POINT('Ctrl Pts',(0.151668947076162,-0.0360288169028614,
-0.532798321964772));
#79528=CARTESIAN_POINT('Ctrl Pts',(0.153380429140839,-0.0258891184973931,
-0.532057284387844));
#79529=CARTESIAN_POINT('Ctrl Pts',(0.155083892865825,-0.0157969248527707,
-0.531319718591975));
#79530=CARTESIAN_POINT('Ctrl Pts',(0.155793341611836,-0.00549837891997462,
-0.530582152796106));
#79531=CARTESIAN_POINT('Ctrl Pts',(0.155476165663079,0.00479211964654155,
-0.529844587000237));
#79532=CARTESIAN_POINT('Ctrl Pts',(0.155158235733579,0.0151070804643411,
-0.529105267886031));
#79533=CARTESIAN_POINT('Ctrl Pts',(0.153808675124117,0.0254130241057423,
-0.528365948771825));
#79534=CARTESIAN_POINT('Ctrl Pts',(0.151447160819724,0.0354902800727829,
-0.527626629657619));
#79535=CARTESIAN_POINT('Ctrl Pts',(0.149096624655142,0.0455206891819837,
-0.526890747468857));
#79536=CARTESIAN_POINT('Ctrl Pts',(0.145743732290646,0.0553236233514978,
-0.526154865280095));
#79537=CARTESIAN_POINT('Ctrl Pts',(0.141459069430118,0.0646926129937966,
-0.525418983091334));
#79538=CARTESIAN_POINT('Ctrl Pts',(0.137144389400339,0.0741272392000329,
-0.524677945514405));
#79539=CARTESIAN_POINT('Ctrl Pts',(0.131885215706989,0.0831209478566759,
-0.523936907937477));
#79540=CARTESIAN_POINT('Ctrl Pts',(0.125801356714249,0.0914867266266224,
-0.523195870360549));
#79541=CARTESIAN_POINT('Ctrl Pts',(0.119717497721509,0.0998525053965686,
-0.522454832783621));
#79542=CARTESIAN_POINT('Ctrl Pts',(0.112809612786503,0.107589666871735,
-0.521713795206692));
#79543=CARTESIAN_POINT('Ctrl Pts',(0.105237140814391,0.114546700926792,
-0.520972757629764));
#79544=CARTESIAN_POINT('Ctrl Pts',(0.104283464657723,0.115422868910494,
-0.520879431451613));
#79545=CARTESIAN_POINT('Ctrl Pts',(0.103318400484365,0.116287535202872,
-0.520786105273462));
#79546=CARTESIAN_POINT('Ctrl Pts',(0.10234224283772,0.117140376604078,-0.520692779095311));
#79547=CARTESIAN_POINT('Ctrl Pts',(0.10234224283772,0.117140376604078,-0.590700225539723));
#79548=CARTESIAN_POINT('Ctrl Pts',(0.0945759900385656,0.123925532610504,
-0.589962670975134));
#79549=CARTESIAN_POINT('Ctrl Pts',(0.0861446319710369,0.129924196060971,
-0.589225116410546));
#79550=CARTESIAN_POINT('Ctrl Pts',(0.0772334289168642,0.135021479616184,
-0.588487561845957));
#79551=CARTESIAN_POINT('Ctrl Pts',(0.0731752806521563,0.137342774764389,
-0.588151680623386));
#79552=CARTESIAN_POINT('Ctrl Pts',(0.0690179807080798,0.13947775775794,
-0.587815799400815));
#79553=CARTESIAN_POINT('Ctrl Pts',(0.0647804987047992,0.141418844174168,
-0.587479918178244));
#79554=CARTESIAN_POINT('Ctrl Pts',(0.0554753587439913,0.145681300218828,
-0.586742352382375));
#79555=CARTESIAN_POINT('Ctrl Pts',(0.0457131421812634,0.149037264109502,
-0.586004786586507));
#79556=CARTESIAN_POINT('Ctrl Pts',(0.0356924565438694,0.151399640177459,
-0.585267220790638));
#79557=CARTESIAN_POINT('Ctrl Pts',(0.0256479500460458,0.153767632011904,
-0.584527901676432));
#79558=CARTESIAN_POINT('Ctrl Pts',(0.0153446128696165,0.155136949800867,
-0.583788582562226));
#79559=CARTESIAN_POINT('Ctrl Pts',(0.00499970289725095,0.155469628773401,
-0.583049263448019));
#79560=CARTESIAN_POINT('Ctrl Pts',(-0.00529711595503014,0.155800761197492,
-0.582313381259257));
#79561=CARTESIAN_POINT('Ctrl Pts',(-0.0156341898672312,0.155104838447875,
-0.581577499070495));
#79562=CARTESIAN_POINT('Ctrl Pts',(-0.0257938077430798,0.153396486211755,
-0.580841616881734));
#79563=CARTESIAN_POINT('Ctrl Pts',(-0.0360246011067592,0.151676165729852,
-0.580100579304805));
#79564=CARTESIAN_POINT('Ctrl Pts',(-0.0460745035593139,0.148929319532569,
-0.579359541727877));
#79565=CARTESIAN_POINT('Ctrl Pts',(-0.0557318303393841,0.145223157888204,
-0.578618504150949));
#79566=CARTESIAN_POINT('Ctrl Pts',(-0.0653891571194546,0.141516996243838,
-0.57787746657402));
#79567=CARTESIAN_POINT('Ctrl Pts',(-0.0746530733419271,0.136851977681057,
-0.577136428997092));
#79568=CARTESIAN_POINT('Ctrl Pts',(-0.0833359041818016,0.131342794146468,
-0.576395391420164));
#79569=CARTESIAN_POINT('Ctrl Pts',(-0.0919780557247169,0.125859421285511,
-0.575657825624295));
#79570=CARTESIAN_POINT('Ctrl Pts',(-0.100108806789627,0.119499055496214,
-0.574920259828425));
#79571=CARTESIAN_POINT('Ctrl Pts',(-0.107546956153075,0.112380846776524,
-0.574182694032556));
#79572=CARTESIAN_POINT('Ctrl Pts',(-0.115002787252504,0.105245716873743,
-0.57344337491835));
#79573=CARTESIAN_POINT('Ctrl Pts',(-0.121761947599551,0.0973496710543972,
-0.572704055804144));
#79574=CARTESIAN_POINT('Ctrl Pts',(-0.127674287438919,0.0888542560993244,
-0.571964736689938));
#79575=CARTESIAN_POINT('Ctrl Pts',(-0.133559142162814,0.0803983343850622,
-0.571228854501176));
#79576=CARTESIAN_POINT('Ctrl Pts',(-0.138604496885118,0.0713493675232609,
-0.570492972312413));
#79577=CARTESIAN_POINT('Ctrl Pts',(-0.142704064190848,0.0618979205096121,
-0.569757090123651));
#79578=CARTESIAN_POINT('Ctrl Pts',(-0.146832351937288,0.0523802592583791,
-0.569016052546723));
#79579=CARTESIAN_POINT('Ctrl Pts',(-0.150001158894252,0.0424553226940098,
-0.568275014969795));
#79580=CARTESIAN_POINT('Ctrl Pts',(-0.152151583490725,0.0323372562420647,
-0.567533977392867));
#79581=CARTESIAN_POINT('Ctrl Pts',(-0.154302008087198,0.02221918979012,
-0.566792939815939));
#79582=CARTESIAN_POINT('Ctrl Pts',(-0.155433980268412,0.0119089433842917,
-0.566051902239011));
#79583=CARTESIAN_POINT('Ctrl Pts',(-0.155541497310893,0.00162638073205886,
-0.565310864662084));
#79584=CARTESIAN_POINT('Ctrl Pts',(-0.155547131016045,0.00108759241670174,
-0.565272035587932));
#79585=CARTESIAN_POINT('Ctrl Pts',(-0.155549965226619,0.000548774778162832,
-0.565233206513781));
#79586=CARTESIAN_POINT('Ctrl Pts',(-0.155549999681981,9.94664380414222E-6,
-0.56519437743963));
#79587=CARTESIAN_POINT('Ctrl Pts',(0.102342242827937,0.117140376612625,
-0.604616163143584));
#79588=CARTESIAN_POINT('Ctrl Pts',(0.0998150425810934,0.119348320182694,
-0.604387819509448));
#79589=CARTESIAN_POINT('Ctrl Pts',(0.0972171874948015,0.121473785577786,
-0.604156835154237));
#79590=CARTESIAN_POINT('Ctrl Pts',(0.0933494900658883,0.124434607298007,
-0.603816750628649));
#79591=CARTESIAN_POINT('Ctrl Pts',(0.0921328779487807,0.125338068064333,
-0.603710300531447));
#79592=CARTESIAN_POINT('Ctrl Pts',(0.089979157887175,0.12688912730739,-0.603522643187757));
#79593=CARTESIAN_POINT('Ctrl Pts',(0.0890477598874706,0.12754448563957,
-0.603441740309642));
#79594=CARTESIAN_POINT('Ctrl Pts',(0.0870925289375224,0.12888838602375,
-0.603272373972136));
#79595=CARTESIAN_POINT('Ctrl Pts',(0.0860675356096406,0.129575089431532,
-0.603183848682771));
#79596=CARTESIAN_POINT('Ctrl Pts',(0.0833515654433992,0.131348233833454,
-0.602949896444857));
#79597=CARTESIAN_POINT('Ctrl Pts',(0.0816475618471532,0.132414187079245,
-0.602803730197593));
#79598=CARTESIAN_POINT('Ctrl Pts',(0.071979906474285,0.138204303641591,
-0.601977470121882));
#79599=CARTESIAN_POINT('Ctrl Pts',(0.0636288439327093,0.142242226887767,
-0.60127335976255));
#79600=CARTESIAN_POINT('Ctrl Pts',(0.0477839774950291,0.148227862987484,
-0.599964745161302));
#79601=CARTESIAN_POINT('Ctrl Pts',(0.0404068131036379,0.150406457570353,
-0.599365867859013));
#79602=CARTESIAN_POINT('Ctrl Pts',(0.0293474793061623,0.152799640421348,
-0.598502774539392));
#79603=CARTESIAN_POINT('Ctrl Pts',(0.0257700240752542,0.153443524964562,
-0.598228886167105));
#79604=CARTESIAN_POINT('Ctrl Pts',(0.0211221815468206,0.154112890609183,
-0.597882412887712));
#79605=CARTESIAN_POINT('Ctrl Pts',(0.0200698099466869,0.154253468355781,
-0.59780458073061));
#79606=CARTESIAN_POINT('Ctrl Pts',(0.0183471744985145,0.154465652691051,
-0.59767827085864));
#79607=CARTESIAN_POINT('Ctrl Pts',(0.0176777600081493,0.154543694536126,
-0.597629456313642));
#79608=CARTESIAN_POINT('Ctrl Pts',(0.0164180600914171,0.154682260957708,
-0.597538129693187));
#79609=CARTESIAN_POINT('Ctrl Pts',(0.0158278981167646,0.15474376312115,
-0.597495562978908));
#79610=CARTESIAN_POINT('Ctrl Pts',(0.0142547836392661,0.154898607173697,
-0.597382647552801));
#79611=CARTESIAN_POINT('Ctrl Pts',(0.0132712494284984,0.154985971730992,
-0.597312621305776));
#79612=CARTESIAN_POINT('Ctrl Pts',(0.00958792636806592,0.155277829880607,
-0.597052279371541));
#79613=CARTESIAN_POINT('Ctrl Pts',(0.00688360760620281,0.155421204888379,
-0.596864958160466));
#79614=CARTESIAN_POINT('Ctrl Pts',(-0.00620469275255882,0.15577277024577,
-0.595970848623132));
#79615=CARTESIAN_POINT('Ctrl Pts',(-0.0165888740100899,0.155011304330156,
-0.595297961995004));
#79616=CARTESIAN_POINT('Ctrl Pts',(-0.0319408257475522,0.152324022328808,
-0.594266841627171));
#79617=CARTESIAN_POINT('Ctrl Pts',(-0.0370127121583655,0.15117168092893,
-0.593920310074924));
#79618=CARTESIAN_POINT('Ctrl Pts',(-0.0454116615595252,0.148815366142515,
-0.593327470087366));
#79619=CARTESIAN_POINT('Ctrl Pts',(-0.0487725891355586,0.147747973333673,
-0.593084997483356));
#79620=CARTESIAN_POINT('Ctrl Pts',(-0.0535234700514198,0.146059377216428,
-0.592732974518025));
#79621=CARTESIAN_POINT('Ctrl Pts',(-0.0549452297824081,0.145530494944406,
-0.592626417803915));
#79622=CARTESIAN_POINT('Ctrl Pts',(-0.0574206648089724,0.144568209673151,
-0.592438638260483));
#79623=CARTESIAN_POINT('Ctrl Pts',(-0.0584777532867934,0.144143859532027,
-0.592357721056862));
#79624=CARTESIAN_POINT('Ctrl Pts',(-0.0606692766908525,0.143236035548666,
-0.59218838925527));
#79625=CARTESIAN_POINT('Ctrl Pts',(-0.0618028094756738,0.142750606281139,
-0.592099913468413));
#79626=CARTESIAN_POINT('Ctrl Pts',(-0.0647655474086041,0.141439927650801,
-0.591866243367773));
#79627=CARTESIAN_POINT('Ctrl Pts',(-0.0665847082572372,0.140592692544722,
-0.591720313012288));
#79628=CARTESIAN_POINT('Ctrl Pts',(-0.0762840186394345,0.13584497829176,
-0.590928551740038));
#79629=CARTESIAN_POINT('Ctrl Pts',(-0.0838378225090265,0.131317481324936,
-0.590261266066728));
#79630=CARTESIAN_POINT('Ctrl Pts',(-0.0963137362461794,0.122322938234272,
-0.589074461510489));
#79631=CARTESIAN_POINT('Ctrl Pts',(-0.101409337993056,0.118132904568405,
-0.588561285514936));
#79632=CARTESIAN_POINT('Ctrl Pts',(-0.109875602360243,0.110218616444432,
-0.587669892211835));
#79633=CARTESIAN_POINT('Ctrl Pts',(-0.113361117766913,0.106630479186699,
-0.587289611919188));
#79634=CARTESIAN_POINT('Ctrl Pts',(-0.117436684371496,0.102008715945132,
-0.586833887023946));
#79635=CARTESIAN_POINT('Ctrl Pts',(-0.118195529853454,0.101128482148289,
-0.586748527041274));
#79636=CARTESIAN_POINT('Ctrl Pts',(-0.119392774864695,0.0997078320408923,
-0.586613143448292));
#79637=CARTESIAN_POINT('Ctrl Pts',(-0.119837519380592,0.0991728564655517,
-0.586562690970635));
#79638=CARTESIAN_POINT('Ctrl Pts',(-0.120690219920308,0.0981330451347261,
-0.58646567493535));
#79639=CARTESIAN_POINT('Ctrl Pts',(-0.121098627389087,0.0976286136213852,
-0.586419081957774));
#79640=CARTESIAN_POINT('Ctrl Pts',(-0.12201199976512,0.0964859404853927,
-0.586314556959513));
#79641=CARTESIAN_POINT('Ctrl Pts',(-0.122515145201835,0.0958462522484865,
-0.586256749872446));
#79642=CARTESIAN_POINT('Ctrl Pts',(-0.124296687781666,0.0935442846325675,
-0.58605112161421));
#79643=CARTESIAN_POINT('Ctrl Pts',(-0.125546529077658,0.0918600561001543,
-0.58590509206591));
#79644=CARTESIAN_POINT('Ctrl Pts',(-0.132378116478352,0.0822541056238159,
-0.585093434538568));
#79645=CARTESIAN_POINT('Ctrl Pts',(-0.137244675340278,0.0738488055202322,
-0.584461666518785));
#79646=CARTESIAN_POINT('Ctrl Pts',(-0.143863392622656,0.0594707889023248,
-0.583418043644269));
#79647=CARTESIAN_POINT('Ctrl Pts',(-0.146096925250789,0.0537506359950271,
-0.58301172543894));
#79648=CARTESIAN_POINT('Ctrl Pts',(-0.14919736666206,0.0441746031745235,
-0.582330250654473));
#79649=CARTESIAN_POINT('Ctrl Pts',(-0.150265767300542,0.0403911468521191,
-0.582060756532267));
#79650=CARTESIAN_POINT('Ctrl Pts',(-0.151560640401428,0.035038036523898,
-0.581676722930967));
#79651=CARTESIAN_POINT('Ctrl Pts',(-0.151908216563964,0.0334990319844365,
-0.581566010055453));
#79652=CARTESIAN_POINT('Ctrl Pts',(-0.152468265765353,0.0308309850849261,
-0.58137341197574));
#79653=CARTESIAN_POINT('Ctrl Pts',(-0.152691755866943,0.0297043644808611,
-0.581291881994168));
#79654=CARTESIAN_POINT('Ctrl Pts',(-0.153125091452318,0.0273856497022283,
-0.581123616003314));
#79655=CARTESIAN_POINT('Ctrl Pts',(-0.15333353923917,0.0261933776743655,
-0.581036841893671));
#79656=CARTESIAN_POINT('Ctrl Pts',(-0.153833001250387,0.023125976408806,
-0.580812886185986));
#79657=CARTESIAN_POINT('Ctrl Pts',(-0.154103647294522,0.0212477848560813,
-0.580675077451669));
#79658=CARTESIAN_POINT('Ctrl Pts',(-0.155151431861578,0.0128969787120623,
-0.580059072281348));
#79659=CARTESIAN_POINT('Ctrl Pts',(-0.155555484778032,0.0063850521473003,
-0.579569611269345));
#79660=CARTESIAN_POINT('Ctrl Pts',(-0.155544704558447,-0.00629461430374163,
-0.578600509511741));
#79661=CARTESIAN_POINT('Ctrl Pts',(-0.155173271014237,-0.0124509474070228,
-0.578122674400401));
#79662=CARTESIAN_POINT('Ctrl Pts',(-0.153582229072617,-0.025683818750784,
-0.577090070143279));
#79663=CARTESIAN_POINT('Ctrl Pts',(-0.152235975584404,-0.0327320539478683,
-0.576536569310194));
#79664=CARTESIAN_POINT('Ctrl Pts',(-0.150000131164609,-0.0412107456605931,
-0.575882667976528));
#79665=CARTESIAN_POINT('Ctrl Pts',(-0.149568073470682,-0.042752272818136,
-0.575764296136786));
#79666=CARTESIAN_POINT('Ctrl Pts',(-0.148888440711779,-0.0450405682797534,
-0.575589619869348));
#79667=CARTESIAN_POINT('Ctrl Pts',(-0.148658891058573,-0.0457925184823436,
-0.575532388915344));
#79668=CARTESIAN_POINT('Ctrl Pts',(-0.148233731198725,-0.047148343390999,
-0.575429542628247));
#79669=CARTESIAN_POINT('Ctrl Pts',(-0.148040117251705,-0.0477527912165003,
-0.575383820772694));
#79670=CARTESIAN_POINT('Ctrl Pts',(-0.147590721842001,-0.0491267628697209,
-0.575280175421845));
#79671=CARTESIAN_POINT('Ctrl Pts',(-0.147332616790405,-0.0498954918868905,
-0.575222385944596));
#79672=CARTESIAN_POINT('Ctrl Pts',(-0.146504349781652,-0.0522998883581296,
-0.575042156789933));
#79673=CARTESIAN_POINT('Ctrl Pts',(-0.145912848620371,-0.0539281381255683,
-0.57492086776839));
#79674=CARTESIAN_POINT('Ctrl Pts',(-0.144427542935354,-0.0578133031334713,
-0.574632518032726));
#79675=CARTESIAN_POINT('Ctrl Pts',(-0.143507854474433,-0.0600598886467181,
-0.574466649324829));
#79676=CARTESIAN_POINT('Ctrl Pts',(-0.139541509471743,-0.0691367819357211,
-0.573796476482044));
#79677=CARTESIAN_POINT('Ctrl Pts',(-0.136056627786375,-0.0757650086505105,
-0.573306694306837));
#79678=CARTESIAN_POINT('Ctrl Pts',(-0.127469274359271,-0.0895801442974672,
-0.5722347070958));
#79679=CARTESIAN_POINT('Ctrl Pts',(-0.122206869638777,-0.0966357789101716,
-0.571652773847899));
#79680=CARTESIAN_POINT('Ctrl Pts',(-0.114933689027951,-0.104836940258661,
-0.570898453780815));
#79681=CARTESIAN_POINT('Ctrl Pts',(-0.113456041177236,-0.106434312367979,
-0.57074749112664));
#79682=CARTESIAN_POINT('Ctrl Pts',(-0.11097996972815,-0.109000836748831,
-0.570497776178663));
#79683=CARTESIAN_POINT('Ctrl Pts',(-0.110001157464275,-0.109988550440371,
-0.570399855386544));
#79684=CARTESIAN_POINT('Ctrl Pts',(-0.108206392304892,-0.111751715270577,
-0.570221627566613));
#79685=CARTESIAN_POINT('Ctrl Pts',(-0.107395005374523,-0.112531692874178,
-0.570141525683205));
#79686=CARTESIAN_POINT('Ctrl Pts',(-0.105624239608196,-0.114197316590045,
-0.569967671848425));
#79687=CARTESIAN_POINT('Ctrl Pts',(-0.104662037190724,-0.1150798196411,
-0.569873794627664));
#79688=CARTESIAN_POINT('Ctrl Pts',(-0.101932136969279,-0.117521044822269,
-0.569609014083028));
#79689=CARTESIAN_POINT('Ctrl Pts',(-0.100140026492689,-0.119051797543412,
-0.569436981292475));
#79690=CARTESIAN_POINT('Ctrl Pts',(-0.0921100907692925,-0.125601049043539,
-0.568673435472315));
#79691=CARTESIAN_POINT('Ctrl Pts',(-0.0855258502945346,-0.130173675227222,
-0.56806523586275));
#79692=CARTESIAN_POINT('Ctrl Pts',(-0.0709828988432958,-0.138692350175944,
-0.566765240122859));
#79693=CARTESIAN_POINT('Ctrl Pts',(-0.0629778727260717,-0.142505907178222,
-0.566073614822845));
#79694=CARTESIAN_POINT('Ctrl Pts',(-0.0517632843281505,-0.146717930584924,
-0.565163263321706));
#79695=CARTESIAN_POINT('Ctrl Pts',(-0.0488019630281979,-0.147729348496298,
-0.564928232088351));
#79696=CARTESIAN_POINT('Ctrl Pts',(-0.0448177151643822,-0.148957232881636,
-0.56462077811129));
#79697=CARTESIAN_POINT('Ctrl Pts',(-0.0438204265777912,-0.149253660563125,
-0.564544541332005));
#79698=CARTESIAN_POINT('Ctrl Pts',(-0.0422403782342652,-0.149706101111725,
-0.564424971556788));
#79699=CARTESIAN_POINT('Ctrl Pts',(-0.0416595789651382,-0.149868761845605,
-0.56438127755662));
#79700=CARTESIAN_POINT('Ctrl Pts',(-0.0404392606509832,-0.150202886274518,
-0.564290032953742));
#79701=CARTESIAN_POINT('Ctrl Pts',(-0.039799567153663,-0.150373652378502,
-0.564242526025334));
#79702=CARTESIAN_POINT('Ctrl Pts',(-0.0381861888625993,-0.150793326917575,
-0.564123477247869));
#79703=CARTESIAN_POINT('Ctrl Pts',(-0.0372111231790342,-0.151036899184065,
-0.56405223068352));
#79704=CARTESIAN_POINT('Ctrl Pts',(-0.0332416388601625,-0.151987704146258,
-0.563764772207036));
#79705=CARTESIAN_POINT('Ctrl Pts',(-0.0302286892110962,-0.152615524265053,
-0.563552532101712));
#79706=CARTESIAN_POINT('Ctrl Pts',(-0.02160007002832,-0.154147898263196,
-0.562956388272049));
#79707=CARTESIAN_POINT('Ctrl Pts',(-0.0159505497784476,-0.154834514566911,
-0.562579895229941));
#79708=CARTESIAN_POINT('Ctrl Pts',(0.00106119114059613,-0.155960783817813,
-0.561455529620654));
#79709=CARTESIAN_POINT('Ctrl Pts',(0.0124449446903201,-0.155466981141138,
-0.560712833677624));
#79710=CARTESIAN_POINT('Ctrl Pts',(0.0259392871278621,-0.153389093894875,
-0.559772109246303));
#79711=CARTESIAN_POINT('Ctrl Pts',(0.0281975611766819,-0.152990056392549,
-0.559612735041083));
#79712=CARTESIAN_POINT('Ctrl Pts',(0.0317266371894681,-0.152285679263893,
-0.559360163509361));
#79713=CARTESIAN_POINT('Ctrl Pts',(0.033003875630759,-0.152013984965058,
-0.559268025550888));
#79714=CARTESIAN_POINT('Ctrl Pts',(0.0353753058407222,-0.151478239049472,
-0.55909551804472));
#79715=CARTESIAN_POINT('Ctrl Pts',(0.0364703522725195,-0.151218327105364,
-0.559015285303121));
#79716=CARTESIAN_POINT('Ctrl Pts',(0.0389115969426395,-0.150610833003047,
-0.558835081450299));
#79717=CARTESIAN_POINT('Ctrl Pts',(0.0402561341864923,-0.15025704250793,
-0.558734917168882));
#79718=CARTESIAN_POINT('Ctrl Pts',(0.0442841879615979,-0.149139189274522,
-0.558431980549979));
#79719=CARTESIAN_POINT('Ctrl Pts',(0.0469519357936611,-0.148320939061457,
-0.558227494882442));
#79720=CARTESIAN_POINT('Ctrl Pts',(0.0556324181781097,-0.145400815980659,
-0.557548958222977));
#79721=CARTESIAN_POINT('Ctrl Pts',(0.0615376109355467,-0.143001635756755,
-0.557065955972878));
#79722=CARTESIAN_POINT('Ctrl Pts',(0.0769143144703095,-0.135625238282909,
-0.555754570580502));
#79723=CARTESIAN_POINT('Ctrl Pts',(0.0860479915653236,-0.13002217573752,
-0.554915985248314));
#79724=CARTESIAN_POINT('Ctrl Pts',(0.0964558301335115,-0.122057055398578,
-0.553927138374224));
#79725=CARTESIAN_POINT('Ctrl Pts',(0.0983420769699213,-0.120542479916192,
-0.553746551922497));
#79726=CARTESIAN_POINT('Ctrl Pts',(0.100917076410527,-0.11837416872505,
-0.553498915186564));
#79727=CARTESIAN_POINT('Ctrl Pts',(0.101636228897111,-0.117757280999884,
-0.553429630342887));
#79728=CARTESIAN_POINT('Ctrl Pts',(0.102835169580987,-0.116709665321775,
-0.553313975101571));
#79729=CARTESIAN_POINT('Ctrl Pts',(0.103317989862954,-0.116282462637515,
-0.553267360018536));
#79730=CARTESIAN_POINT('Ctrl Pts',(0.104322518439007,-0.115382452340274,
-0.553170312582002));
#79731=CARTESIAN_POINT('Ctrl Pts',(0.104843693628346,-0.114909086324636,
-0.553119922095313));
#79732=CARTESIAN_POINT('Ctrl Pts',(0.106244988726247,-0.113618865714547,
-0.552984268454093));
#79733=CARTESIAN_POINT('Ctrl Pts',(0.107118915540285,-0.112795312141819,
-0.552899485811856));
#79734=CARTESIAN_POINT('Ctrl Pts',(0.112140182493943,-0.107952470386524,
-0.552410658544606));
#79735=CARTESIAN_POINT('Ctrl Pts',(0.116071130535236,-0.103714344768788,
-0.552021071111647));
#79736=CARTESIAN_POINT('Ctrl Pts',(0.127771880500659,-0.0895983175565992,
-0.550801144690868));
#79737=CARTESIAN_POINT('Ctrl Pts',(0.134585420876852,-0.0789953923914177,
-0.549991173429477));
#79738=CARTESIAN_POINT('Ctrl Pts',(0.141445265457289,-0.0648021435883795,
-0.548916354524087));
#79739=CARTESIAN_POINT('Ctrl Pts',(0.142750716424631,-0.0618733503971363,
-0.548695302793198));
#79740=CARTESIAN_POINT('Ctrl Pts',(0.144513363343115,-0.0575655238094397,
-0.548369962007351));
#79741=CARTESIAN_POINT('Ctrl Pts',(0.145043267398054,-0.0562170085453605,
-0.548268093072449));
#79742=CARTESIAN_POINT('Ctrl Pts',(0.145953929252702,-0.0538009041046105,
-0.548085424254409));
#79743=CARTESIAN_POINT('Ctrl Pts',(0.146342006493826,-0.0527361712577901,
-0.548004873608401));
#79744=CARTESIAN_POINT('Ctrl Pts',(0.14713471586338,-0.0504851340585873,
-0.54783441585946));
#79745=CARTESIAN_POINT('Ctrl Pts',(0.147536710531374,-0.049297994374511,
-0.547744428581373));
#79746=CARTESIAN_POINT('Ctrl Pts',(0.148574856803444,-0.0461057405625223,
-0.547502135221473));
#79747=CARTESIAN_POINT('Ctrl Pts',(0.149184732420357,-0.0440924279311382,
-0.54734899106169));
#79748=CARTESIAN_POINT('Ctrl Pts',(0.150447093215428,-0.0395986207361951,
-0.547006260523453));
#79749=CARTESIAN_POINT('Ctrl Pts',(0.151079420568643,-0.0371131503261315,
-0.54681609388495));
#79750=CARTESIAN_POINT('Ctrl Pts',(0.152916292400254,-0.0290653332460022,
-0.546198316229022));
#79751=CARTESIAN_POINT('Ctrl Pts',(0.153877064957146,-0.0234525791267074,
-0.545764181616794));
#79752=CARTESIAN_POINT('Ctrl Pts',(0.155504131332962,-0.00932767940001892,
-0.544668174776928));
#79753=CARTESIAN_POINT('Ctrl Pts',(0.155781643987323,-0.000789154788085012,
-0.544001998455278));
#79754=CARTESIAN_POINT('Ctrl Pts',(0.155181025019761,0.0112834596666922,
-0.543080149951416));
#79755=CARTESIAN_POINT('Ctrl Pts',(0.154882255201368,0.0148309997396616,
-0.542811890607801));
#79756=CARTESIAN_POINT('Ctrl Pts',(0.154333748704033,0.0194441924848779,
-0.542468909787829));
#79757=CARTESIAN_POINT('Ctrl Pts',(0.15419418634321,0.0205215907113379,
-0.542389229236602));
#79758=CARTESIAN_POINT('Ctrl Pts',(0.153949031747173,0.0222701482681936,
-0.542260691081167));
#79759=CARTESIAN_POINT('Ctrl Pts',(0.153850313246199,0.0229422109061236,
-0.542211474762342));
#79760=CARTESIAN_POINT('Ctrl Pts',(0.153645683185368,0.0242745476771696,
-0.542114306414622));
#79761=CARTESIAN_POINT('Ctrl Pts',(0.153539910632097,0.0249348251851772,
-0.542066348810515));
#79762=CARTESIAN_POINT('Ctrl Pts',(0.153259254136351,0.0266172662342378,
-0.541944604137886));
#79763=CARTESIAN_POINT('Ctrl Pts',(0.153078396773061,0.0276384231683491,
-0.541871140802929));
#79764=CARTESIAN_POINT('Ctrl Pts',(0.152265011550628,0.0319777861595062,
-0.541560495253131));
#79765=CARTESIAN_POINT('Ctrl Pts',(0.151534651927442,0.035276987411654,
-0.541328136315055));
#79766=CARTESIAN_POINT('Ctrl Pts',(0.149038396369547,0.0450351849884393,
-0.540645231566677));
#79767=CARTESIAN_POINT('Ctrl Pts',(0.146962418313323,0.0514069224264616,
-0.540204888470714));
#79768=CARTESIAN_POINT('Ctrl Pts',(0.140831904942345,0.0667777361337516,
-0.53911490405296));
#79769=CARTESIAN_POINT('Ctrl Pts',(0.136320700492746,0.0755614194340932,
-0.538465868207829));
#79770=CARTESIAN_POINT('Ctrl Pts',(0.129845872110923,0.0856767779354075,
-0.537639186394091));
#79771=CARTESIAN_POINT('Ctrl Pts',(0.128644645664169,0.0874700814795016,
-0.537489412179961));
#79772=CARTESIAN_POINT('Ctrl Pts',(0.126611729710743,0.0903725171093484,
-0.53724125176283));
#79773=CARTESIAN_POINT('Ctrl Pts',(0.125801811569393,0.0914965897499306,
-0.537143678980386));
#79774=CARTESIAN_POINT('Ctrl Pts',(0.124307101756696,0.0935137049932858,
-0.536965816175157));
#79775=CARTESIAN_POINT('Ctrl Pts',(0.123627421022325,0.0944104296098886,
-0.536885727258208));
#79776=CARTESIAN_POINT('Ctrl Pts',(0.122135746598557,0.0963347130909257,
-0.536711593129439));
#79777=CARTESIAN_POINT('Ctrl Pts',(0.121320389871812,0.0973595416558567,
-0.536617419352683));
#79778=CARTESIAN_POINT('Ctrl Pts',(0.11898933642018,0.100214706676362,-0.536350896770465));
#79779=CARTESIAN_POINT('Ctrl Pts',(0.117444555326744,0.102020708158709,
-0.536177394340382));
#79780=CARTESIAN_POINT('Ctrl Pts',(0.111628066576439,0.108513526864028,
-0.535534890508366));
#79781=CARTESIAN_POINT('Ctrl Pts',(0.107113838418182,0.112971568523782,
-0.535056291621251));
#79782=CARTESIAN_POINT('Ctrl Pts',(0.102342237477092,0.117140381287507,
-0.534570457414543));
#79783=CARTESIAN_POINT('Origin',(0.,0.,-1.10400562256037));
#79784=CARTESIAN_POINT('',(0.102342242837719,0.117140376604078,-0.450689508133418));
#79785=CARTESIAN_POINT('',(0.102342242837722,0.117140376604076,-0.464360489961668));
#79786=CARTESIAN_POINT('',(0.10234224283772,0.117140376604078,-1.10400562256037));
#79787=CARTESIAN_POINT('',(-0.155549952262899,0.00012186471943091,-0.495194377443475));
#79788=CARTESIAN_POINT('Ctrl Pts',(-0.155549952262941,0.000121864665597637,
-0.49519437743963));
#79789=CARTESIAN_POINT('Ctrl Pts',(-0.155558009308424,-0.0101622733503201,
-0.494459817921359));
#79790=CARTESIAN_POINT('Ctrl Pts',(-0.154541823275545,-0.020459514100615,
-0.493725258403087));
#79791=CARTESIAN_POINT('Ctrl Pts',(-0.152519911581845,-0.0305528897334775,
-0.492990698884816));
#79792=CARTESIAN_POINT('Ctrl Pts',(-0.150498488090658,-0.0406438282612177,
-0.492256316730276));
#79793=CARTESIAN_POINT('Ctrl Pts',(-0.14747202429582,-0.0505300918992016,
-0.491521934575736));
#79794=CARTESIAN_POINT('Ctrl Pts',(-0.14350997916094,-0.0600057362360169,
-0.490787552421196));
#79795=CARTESIAN_POINT('Ctrl Pts',(-0.13953818484467,-0.0695046967573508,
-0.490051363213835));
#79796=CARTESIAN_POINT('Ctrl Pts',(-0.134626631384355,-0.0785901876366601,
-0.489315174006475));
#79797=CARTESIAN_POINT('Ctrl Pts',(-0.128891766837023,-0.0870787858300196,
-0.488578984799115));
#79798=CARTESIAN_POINT('Ctrl Pts',(-0.126659152731622,-0.090383443491096,
-0.488292382317918));
#79799=CARTESIAN_POINT('Ctrl Pts',(-0.124302218888701,-0.0935979598096855,
-0.48800577983672));
#79800=CARTESIAN_POINT('Ctrl Pts',(-0.12182947505027,-0.0967128818150698,
-0.487719177355523));
#79801=CARTESIAN_POINT('Ctrl Pts',(-0.115465917869771,-0.104729071760014,
-0.486981611559654));
#79802=CARTESIAN_POINT('Ctrl Pts',(-0.108284142641196,-0.112144290598278,
-0.486244045763785));
#79803=CARTESIAN_POINT('Ctrl Pts',(-0.100421731041853,-0.118790902153985,
-0.485506479967916));
#79804=CARTESIAN_POINT('Ctrl Pts',(-0.0925406291636104,-0.125453313826762,
-0.48476716085371));
#79805=CARTESIAN_POINT('Ctrl Pts',(-0.0839762638384047,-0.131342747989288,
-0.484027841739504));
#79806=CARTESIAN_POINT('Ctrl Pts',(-0.0749051052335867,-0.13632691484056,
-0.483288522625298));
#79807=CARTESIAN_POINT('Ctrl Pts',(-0.0658761163701119,-0.141287911440259,
-0.482552640436536));
#79808=CARTESIAN_POINT('Ctrl Pts',(-0.0563458515628692,-0.145351586900182,
-0.481816758247774));
#79809=CARTESIAN_POINT('Ctrl Pts',(-0.046515015375013,-0.148432327491899,
-0.481080876059012));
#79810=CARTESIAN_POINT('Ctrl Pts',(-0.0366153070533836,-0.15153465090466,
-0.480339838482084));
#79811=CARTESIAN_POINT('Ctrl Pts',(-0.0264117019067965,-0.153639917004201,
-0.479598800905156));
#79812=CARTESIAN_POINT('Ctrl Pts',(-0.0161233600777818,-0.154712118981682,
-0.478857763328227));
#79813=CARTESIAN_POINT('Ctrl Pts',(-0.00583501824876717,-0.155784320959164,
-0.478116725751299));
#79814=CARTESIAN_POINT('Ctrl Pts',(0.00453710823583818,-0.155823489254566,
-0.477375688174371));
#79815=CARTESIAN_POINT('Ctrl Pts',(0.0147737473089751,-0.154846823959843,
-0.476634650597443));
#79816=CARTESIAN_POINT('Ctrl Pts',(0.0249624274516175,-0.1538747343684,
-0.475897084801575));
#79817=CARTESIAN_POINT('Ctrl Pts',(0.035092615732708,-0.151889123318184,
-0.475159519005706));
#79818=CARTESIAN_POINT('Ctrl Pts',(0.0449487908546564,-0.148914098394693,
-0.474421953209837));
#79819=CARTESIAN_POINT('Ctrl Pts',(0.0548283957677845,-0.145932001335019,
-0.473682634095631));
#79820=CARTESIAN_POINT('Ctrl Pts',(0.0644317526577002,-0.141955907193368,
-0.472943314981425));
#79821=CARTESIAN_POINT('Ctrl Pts',(0.073551809557291,-0.137061788295819,
-0.472203995867219));
#79822=CARTESIAN_POINT('Ctrl Pts',(0.0826294693985506,-0.132190421037506,
-0.471468113678456));
#79823=CARTESIAN_POINT('Ctrl Pts',(0.0912274894724173,-0.12640998365361,
-0.470732231489695));
#79824=CARTESIAN_POINT('Ctrl Pts',(0.0991647695623966,-0.119842191976102,
-0.469996349300932));
#79825=CARTESIAN_POINT('Ctrl Pts',(0.107157656053065,-0.113228388156963,
-0.469255311724004));
#79826=CARTESIAN_POINT('Ctrl Pts',(0.114479768525023,-0.10581675053189,
-0.468514274147076));
#79827=CARTESIAN_POINT('Ctrl Pts',(0.120981563548319,-0.0977714875687383,
-0.467773236570147));
#79828=CARTESIAN_POINT('Ctrl Pts',(0.127483358571616,-0.0897262246055862,
-0.467032198993219));
#79829=CARTESIAN_POINT('Ctrl Pts',(0.133164343251696,-0.0810481513728482,
-0.466291161416291));
#79830=CARTESIAN_POINT('Ctrl Pts',(0.137919539375875,-0.0719305439875612,
-0.465550123839363));
#79831=CARTESIAN_POINT('Ctrl Pts',(0.1426524572778,-0.0628556528390921,
-0.464812558043494));
#79832=CARTESIAN_POINT('Ctrl Pts',(0.146503453739732,-0.0532779082140079,
-0.464074992247625));
#79833=CARTESIAN_POINT('Ctrl Pts',(0.149375386541972,-0.043391201820604,
-0.463337426451756));
#79834=CARTESIAN_POINT('Ctrl Pts',(0.152254146413029,-0.0334809930580413,
-0.46259810733755));
#79835=CARTESIAN_POINT('Ctrl Pts',(0.154148781561352,-0.0232612011896585,
-0.461858788223344));
#79836=CARTESIAN_POINT('Ctrl Pts',(0.155010262191423,-0.0129468573540533,
-0.461119469109138));
#79837=CARTESIAN_POINT('Ctrl Pts',(0.155867737995108,-0.00268046254355246,
-0.460383586920376));
#79838=CARTESIAN_POINT('Ctrl Pts',(0.155701562959268,0.00767867793224059,
-0.459647704731614));
#79839=CARTESIAN_POINT('Ctrl Pts',(0.15451520569386,0.0179123898289444,
-0.458911822542852));
#79840=CARTESIAN_POINT('Ctrl Pts',(0.15332053713583,0.0282177962958025,
-0.458170784965923));
#79841=CARTESIAN_POINT('Ctrl Pts',(0.151091432852774,0.0383950649584938,
-0.457429747388995));
#79842=CARTESIAN_POINT('Ctrl Pts',(0.147884185479266,0.0482293498311369,
-0.456688709812067));
#79843=CARTESIAN_POINT('Ctrl Pts',(0.144676938105758,0.0580636347037796,
-0.455947672235139));
#79844=CARTESIAN_POINT('Ctrl Pts',(0.140491962857972,0.0675540785365748,
-0.455206634658211));
#79845=CARTESIAN_POINT('Ctrl Pts',(0.135434200201137,0.0765073847146694,
-0.454465597081283));
#79846=CARTESIAN_POINT('Ctrl Pts',(0.130399918229487,0.0854191251297956,
-0.453727999774537));
#79847=CARTESIAN_POINT('Ctrl Pts',(0.124463551504147,0.0938649610089448,
-0.452990402467791));
#79848=CARTESIAN_POINT('Ctrl Pts',(0.117734838928666,0.101657809352952,
-0.452252805161044));
#79849=CARTESIAN_POINT('Ctrl Pts',(0.112981126538093,0.107163314204765,
-0.451731706151836));
#79850=CARTESIAN_POINT('Ctrl Pts',(0.107832998207033,0.112343258516708,
-0.451210607142627));
#79851=CARTESIAN_POINT('Ctrl Pts',(0.102342242837719,0.117140376604078,
-0.450689508133418));
#79852=CARTESIAN_POINT('Ctrl Pts',(0.10234224283772,0.117140376604078,-0.520692779095311));
#79853=CARTESIAN_POINT('Ctrl Pts',(0.0946302156526187,0.123878157221058,
-0.519955465787922));
#79854=CARTESIAN_POINT('Ctrl Pts',(0.0862227979175108,0.129874812435311,
-0.519218152480532));
#79855=CARTESIAN_POINT('Ctrl Pts',(0.0772864419209033,0.134991141913856,
-0.518480839173142));
#79856=CARTESIAN_POINT('Ctrl Pts',(0.0683602118696518,0.140101673987649,
-0.517744361328693));
#79857=CARTESIAN_POINT('Ctrl Pts',(0.0589069874449303,0.144333325515883,
-0.517007883484243));
#79858=CARTESIAN_POINT('Ctrl Pts',(0.0491225935715261,0.147589882108519,
-0.516271405639794));
#79859=CARTESIAN_POINT('Ctrl Pts',(0.0393465649702998,0.150843654473271,
-0.515535557454954));
#79860=CARTESIAN_POINT('Ctrl Pts',(0.0292408044890006,0.153123682619629,
-0.514799709270114));
#79861=CARTESIAN_POINT('Ctrl Pts',(0.0190183539682938,0.154382980643388,
-0.514063861085274));
#79862=CARTESIAN_POINT('Ctrl Pts',(0.00877063935525566,0.155645390936703,
-0.513326194301611));
#79863=CARTESIAN_POINT('Ctrl Pts',(-0.00159341339709402,0.155881936068079,
-0.512588527517949));
#79864=CARTESIAN_POINT('Ctrl Pts',(-0.0118549561801268,0.155097590290653,
-0.511850860734286));
#79865=CARTESIAN_POINT('Ctrl Pts',(-0.0209555468299898,0.154401982427467,
-0.511196650780085));
#79866=CARTESIAN_POINT('Ctrl Pts',(-0.0299750383140325,0.152904264678107,
-0.510542440825884));
#79867=CARTESIAN_POINT('Ctrl Pts',(-0.0387668291020293,0.150641745413992,
-0.509888230871683));
#79868=CARTESIAN_POINT('Ctrl Pts',(-0.0486788216176196,0.148090948363304,
-0.509150665075814));
#79869=CARTESIAN_POINT('Ctrl Pts',(-0.0583748114869105,0.144548188661075,
-0.508413099279945));
#79870=CARTESIAN_POINT('Ctrl Pts',(-0.0676456836184205,0.14007092484808,
-0.507675533484076));
#79871=CARTESIAN_POINT('Ctrl Pts',(-0.0769385941771473,0.135583017823609,
-0.50693621436987));
#79872=CARTESIAN_POINT('Ctrl Pts',(-0.0858034640196526,0.130156428576783,
-0.506196895255664));
#79873=CARTESIAN_POINT('Ctrl Pts',(-0.0940476405090025,0.123898522245786,
-0.505457576141458));
#79874=CARTESIAN_POINT('Ctrl Pts',(-0.102253491707691,0.117669707489838,
-0.504721693952696));
#79875=CARTESIAN_POINT('Ctrl Pts',(-0.109843662867018,0.110617849060189,
-0.503985811763934));
#79876=CARTESIAN_POINT('Ctrl Pts',(-0.11665827623603,0.102891443209035,
-0.503249929575173));
#79877=CARTESIAN_POINT('Ctrl Pts',(-0.123520630911542,0.095110908284094,
-0.502508891998244));
#79878=CARTESIAN_POINT('Ctrl Pts',(-0.129595880763075,0.0866470414031206,
-0.501767854421316));
#79879=CARTESIAN_POINT('Ctrl Pts',(-0.13476195171955,0.0776853838809952,
-0.501026816844388));
#79880=CARTESIAN_POINT('Ctrl Pts',(-0.139928022676026,0.0687237263588701,
-0.50028577926746));
#79881=CARTESIAN_POINT('Ctrl Pts',(-0.144184555132574,0.0592651602194179,
-0.499544741690532));
#79882=CARTESIAN_POINT('Ctrl Pts',(-0.147458031757348,0.0495169806253255,
-0.498803704113603));
#79883=CARTESIAN_POINT('Ctrl Pts',(-0.151288986780027,0.0381086701778544,
-0.497936466631032));
#79884=CARTESIAN_POINT('Ctrl Pts',(-0.153798378570084,0.0262354219127821,
-0.49706922914846));
#79885=CARTESIAN_POINT('Ctrl Pts',(-0.154901888298272,0.0141847630092929,
-0.496201991665888));
#79886=CARTESIAN_POINT('Ctrl Pts',(-0.15532926531208,0.0095176771784699,
-0.495866120258417));
#79887=CARTESIAN_POINT('Ctrl Pts',(-0.155546268242293,0.0048242037730633,
-0.495530248850946));
#79888=CARTESIAN_POINT('Ctrl Pts',(-0.155549952262899,0.000121864719431378,
-0.495194377443475));
#79889=CARTESIAN_POINT('',(-0.155550041019322,1.41736229090128E-5,-0.508861193595026));
#79890=CARTESIAN_POINT('Ctrl Pts',(0.102342237477092,0.117140381287507,
-0.534570457414543));
#79891=CARTESIAN_POINT('Ctrl Pts',(0.100972985009001,0.11833665843562,-0.53443104305554));
#79892=CARTESIAN_POINT('Ctrl Pts',(0.099582537413719,0.119509120344162,
-0.534291061491653));
#79893=CARTESIAN_POINT('Ctrl Pts',(0.0910650113077797,0.12643931883346,
-0.533443640854567));
#79894=CARTESIAN_POINT('Ctrl Pts',(0.083461465507216,0.131582412293558,
-0.532727509774035));
#79895=CARTESIAN_POINT('Ctrl Pts',(0.0730585353124558,0.137352564776124,
-0.531826903790369));
#79896=CARTESIAN_POINT('Ctrl Pts',(0.0706330556814563,0.138615476567551,
-0.531622187174736));
#79897=CARTESIAN_POINT('Ctrl Pts',(0.0672847028607753,0.140248184179539,
-0.531347823242492));
#79898=CARTESIAN_POINT('Ctrl Pts',(0.066389875766124,0.140673981023601,
-0.531275286370639));
#79899=CARTESIAN_POINT('Ctrl Pts',(0.0649522473807156,0.141341292145939,
-0.53116006848315));
#79900=CARTESIAN_POINT('Ctrl Pts',(0.0644120444808691,0.141588289992462,
-0.531117069380187));
#79901=CARTESIAN_POINT('Ctrl Pts',(0.0632567773252321,0.142108534416606,
-0.531025760612177));
#79902=CARTESIAN_POINT('Ctrl Pts',(0.0626413246593988,0.142380897318929,
-0.530977506401075));
#79903=CARTESIAN_POINT('Ctrl Pts',(0.0610544408627348,0.143070876713611,
-0.530854036524967));
#79904=CARTESIAN_POINT('Ctrl Pts',(0.060080464341022,0.143482606888423,
-0.530779163067255));
#79905=CARTESIAN_POINT('Ctrl Pts',(0.0557840135391806,0.145247428329257,
-0.530452524179679));
#79906=CARTESIAN_POINT('Ctrl Pts',(0.0524192264193203,0.146495395938009,
-0.530206221484216));
#79907=CARTESIAN_POINT('Ctrl Pts',(0.0419033837321235,0.14998681017549,
-0.529456603350951));
#79908=CARTESIAN_POINT('Ctrl Pts',(0.0346310201241065,0.151830972795735,
-0.528965941728836));
#79909=CARTESIAN_POINT('Ctrl Pts',(0.0186234321116583,0.154679700136369,
-0.527894424596587));
#79910=CARTESIAN_POINT('Ctrl Pts',(0.0098798350303917,0.155483135521406,
-0.527313858958294));
#79911=CARTESIAN_POINT('Ctrl Pts',(-0.00106187168404021,0.155561617941926,
-0.52656091235647));
#79912=CARTESIAN_POINT('Ctrl Pts',(-0.00323943187548442,0.155531507547467,
-0.526409831115701));
#79913=CARTESIAN_POINT('Ctrl Pts',(-0.00680575629684839,0.155407268769235,
-0.526159961086687));
#79914=CARTESIAN_POINT('Ctrl Pts',(-0.00819520409637836,0.155340194133129,
-0.526062005613909));
#79915=CARTESIAN_POINT('Ctrl Pts',(-0.0107068963187317,0.155185152766832,
-0.525883741305979));
#79916=CARTESIAN_POINT('Ctrl Pts',(-0.0118294527090561,0.155103620833324,
-0.52580363801748));
#79917=CARTESIAN_POINT('Ctrl Pts',(-0.014251682553711,0.154901244769546,
-0.525629811562684));
#79918=CARTESIAN_POINT('Ctrl Pts',(-0.015550908827485,0.154776209831949,
-0.525535963451272));
#79919=CARTESIAN_POINT('Ctrl Pts',(-0.0191892884190071,0.154379787061373,
-0.52527135364745));
#79920=CARTESIAN_POINT('Ctrl Pts',(-0.0215239862790297,0.154071620818185,
-0.525099464843616));
#79921=CARTESIAN_POINT('Ctrl Pts',(-0.0317467551654107,0.152485393445081,
-0.524337189325797));
#79922=CARTESIAN_POINT('Ctrl Pts',(-0.0395354857256762,0.150653780798415,
-0.52373018215175));
#79923=CARTESIAN_POINT('Ctrl Pts',(-0.0555541012174266,0.145558767542852,
-0.522433716972169));
#79924=CARTESIAN_POINT('Ctrl Pts',(-0.0637175524584717,0.142174865096296,
-0.521744445263524));
#79925=CARTESIAN_POINT('Ctrl Pts',(-0.074362447957927,0.136660379959468,
-0.520833097448303));
#79926=CARTESIAN_POINT('Ctrl Pts',(-0.0771297120980275,0.135117889188147,
-0.520595075639688));
#79927=CARTESIAN_POINT('Ctrl Pts',(-0.0807448497918674,0.132955494285235,
-0.520284390647942));
#79928=CARTESIAN_POINT('Ctrl Pts',(-0.0816361451931318,0.132410098501259,
-0.520207816058779));
#79929=CARTESIAN_POINT('Ctrl Pts',(-0.08303389605275,0.131535316210601,
-0.520087847219453));
#79930=CARTESIAN_POINT('Ctrl Pts',(-0.0835440242877966,0.131211902445967,
-0.520044087966065));
#79931=CARTESIAN_POINT('Ctrl Pts',(-0.0846086541113812,0.130528216796133,
-0.519952836610549));
#79932=CARTESIAN_POINT('Ctrl Pts',(-0.0851627645760028,0.130167366445384,
-0.519905387161339));
#79933=CARTESIAN_POINT('Ctrl Pts',(-0.086549685208956,0.129251522339377,
-0.519786690484115));
#79934=CARTESIAN_POINT('Ctrl Pts',(-0.0873794913445005,0.128691991468806,
-0.519715734858861));
#79935=CARTESIAN_POINT('Ctrl Pts',(-0.0907074415816844,0.12640095307398,
-0.519431162204748));
#79936=CARTESIAN_POINT('Ctrl Pts',(-0.0931601692250964,0.124604280814668,
-0.519221417207531));
#79937=CARTESIAN_POINT('Ctrl Pts',(-0.0999549049263591,0.119314119128767,
-0.518635385214551));
#79938=CARTESIAN_POINT('Ctrl Pts',(-0.104164225798949,0.115657533772781,
-0.518266213084619));
#79939=CARTESIAN_POINT('Ctrl Pts',(-0.116474491421627,0.103745288172068,
-0.517136154309814));
#79940=CARTESIAN_POINT('Ctrl Pts',(-0.123857889293638,0.094808131090732,
-0.516381337922129));
#79941=CARTESIAN_POINT('Ctrl Pts',(-0.131427543632126,0.0832332438251946,
-0.515428168475849));
#79942=CARTESIAN_POINT('Ctrl Pts',(-0.132630050004187,0.0813033887961411,
-0.515270110518713));
#79943=CARTESIAN_POINT('Ctrl Pts',(-0.134453751119969,0.078228418935022,
-0.515019162931181));
#79944=CARTESIAN_POINT('Ctrl Pts',(-0.135103627418985,0.0771006251247367,
-0.514927309788746));
#79945=CARTESIAN_POINT('Ctrl Pts',(-0.136289053530319,0.0749824232971751,
-0.514755059438723));
#79946=CARTESIAN_POINT('Ctrl Pts',(-0.13682815511352,0.0739940927532846,
-0.514674795551276));
#79947=CARTESIAN_POINT('Ctrl Pts',(-0.138011506786804,0.0717675042519225,
-0.514494158071738));
#79948=CARTESIAN_POINT('Ctrl Pts',(-0.138649905627462,0.0705262653712839,
-0.514393586993931));
#79949=CARTESIAN_POINT('Ctrl Pts',(-0.140527208063637,0.0667521978346223,
-0.514088078786667));
#79950=CARTESIAN_POINT('Ctrl Pts',(-0.141713970661791,0.064194242275946,
-0.513881384751377));
#79951=CARTESIAN_POINT('Ctrl Pts',(-0.14565902497044,0.055047766844389,
-0.513143136466566));
#79952=CARTESIAN_POINT('Ctrl Pts',(-0.148032186792093,0.0483037830308538,
-0.512599771579437));
#79953=CARTESIAN_POINT('Ctrl Pts',(-0.152929736687253,0.0305760956604584,
-0.511181624682878));
#79954=CARTESIAN_POINT('Ctrl Pts',(-0.154740495121597,0.0194372652676603,
-0.510298573659076));
#79955=CARTESIAN_POINT('Ctrl Pts',(-0.155411548403831,0.0067255792362609,
-0.509350833115812));
#79956=CARTESIAN_POINT('Ctrl Pts',(-0.155468393194625,0.00524994551898382,
-0.509241768242182));
#79957=CARTESIAN_POINT('Ctrl Pts',(-0.155521244365075,0.00307206358973816,
-0.509082413826389));
#79958=CARTESIAN_POINT('Ctrl Pts',(-0.155533522240653,0.00237034460314847,
-0.509031316513663));
#79959=CARTESIAN_POINT('Ctrl Pts',(-0.155544885369041,0.00131108100834932,
-0.508954580178308));
#79960=CARTESIAN_POINT('Ctrl Pts',(-0.155547487800726,0.00095359563289769,
-0.508928750972098));
#79961=CARTESIAN_POINT('Ctrl Pts',(-0.155549601171384,0.000402122783404505,
-0.5088890140095));
#79962=CARTESIAN_POINT('Ctrl Pts',(-0.155549981691975,0.000208144073060478,
-0.508875057311901));
#79963=CARTESIAN_POINT('Ctrl Pts',(-0.155549999355145,1.41638460410301E-5,
-0.508861120692133));
#79964=CARTESIAN_POINT('Ctrl Pts',(-0.155549999353784,1.41787797109209E-5,
-0.508861121765051));
#79965=CARTESIAN_POINT('Ctrl Pts',(-0.155550034413735,-0.000370450604623472,
-0.50883348784606));
#79966=CARTESIAN_POINT('Ctrl Pts',(-0.155548642861194,-0.000755085092070137,
-0.508805932927192));
#79967=CARTESIAN_POINT('Ctrl Pts',(-0.15554031328278,-0.00189188609293203,
-0.508724717404013));
#79968=CARTESIAN_POINT('Ctrl Pts',(-0.155529346035297,-0.00264402552005807,
-0.508671272805648));
#79969=CARTESIAN_POINT('Ctrl Pts',(-0.155468844606933,-0.00541450384071664,
-0.508475381088768));
#79970=CARTESIAN_POINT('Ctrl Pts',(-0.155385471574864,-0.00743200523510162,
-0.508334625547325));
#79971=CARTESIAN_POINT('Ctrl Pts',(-0.154637454033681,-0.0197252235025581,
-0.507485393419724));
#79972=CARTESIAN_POINT('Ctrl Pts',(-0.152993023103531,-0.0299167630772429,
-0.506816062842887));
#79973=CARTESIAN_POINT('Ctrl Pts',(-0.148459062233549,-0.0470138635843441,
-0.505648838352569));
#79974=CARTESIAN_POINT('Ctrl Pts',(-0.146058844217895,-0.0540110537988211,
-0.505157706628213));
#79975=CARTESIAN_POINT('Ctrl Pts',(-0.142099170703203,-0.0633335686225085,
-0.50446353461855));
#79976=CARTESIAN_POINT('Ctrl Pts',(-0.140961194292705,-0.0658274667872572,
-0.50427379150135));
#79977=CARTESIAN_POINT('Ctrl Pts',(-0.139151676349582,-0.0695307181344438,
-0.503985111314698));
#79978=CARTESIAN_POINT('Ctrl Pts',(-0.138528885218867,-0.0707633912287268,
-0.503887838584097));
#79979=CARTESIAN_POINT('Ctrl Pts',(-0.137369148222479,-0.072984828500458,
-0.503710288796056));
#79980=CARTESIAN_POINT('Ctrl Pts',(-0.136837725112853,-0.0739763809579472,
-0.503630209358879));
#79981=CARTESIAN_POINT('Ctrl Pts',(-0.135662788977779,-0.076112643426853,
-0.503455825248715));
#79982=CARTESIAN_POINT('Ctrl Pts',(-0.135015446170418,-0.0772551351242384,
-0.503361389106862));
#79983=CARTESIAN_POINT('Ctrl Pts',(-0.133180924276198,-0.0803993778312663,
-0.503098136186209));
#79984=CARTESIAN_POINT('Ctrl Pts',(-0.131963212608777,-0.082382813664458,
-0.502928236890759));
#79985=CARTESIAN_POINT('Ctrl Pts',(-0.124772601438793,-0.0935263411314294,
-0.501951018768577));
#79986=CARTESIAN_POINT('Ctrl Pts',(-0.117892342550067,-0.102062195073166,
-0.501110184720737));
#79987=CARTESIAN_POINT('Ctrl Pts',(-0.105975381679225,-0.114019415587182,
-0.499801921796356));
#79988=CARTESIAN_POINT('Ctrl Pts',(-0.101536394896655,-0.117989729688908,
-0.499340669040918));
#79989=CARTESIAN_POINT('Ctrl Pts',(-0.094408515298715,-0.123664139030447,
-0.498648437197397));
#79990=CARTESIAN_POINT('Ctrl Pts',(-0.0918767790759331,-0.125556552478788,
-0.49841111727248));
#79991=CARTESIAN_POINT('Ctrl Pts',(-0.0884585223649684,-0.127952806954091,
-0.498103474783591));
#79992=CARTESIAN_POINT('Ctrl Pts',(-0.0876223977134649,-0.128526832027958,
-0.4980291994366));
#79993=CARTESIAN_POINT('Ctrl Pts',(-0.0862296874233603,-0.129463061560662,
-0.497907161751027));
#79994=CARTESIAN_POINT('Ctrl Pts',(-0.085676301758152,-0.129829945225983,
-0.497859103306455));
#79995=CARTESIAN_POINT('Ctrl Pts',(-0.0846172703227035,-0.130522341558059,
-0.497767977953007));
#79996=CARTESIAN_POINT('Ctrl Pts',(-0.0841120603441055,-0.130848482681996,
-0.497724867699783));
#79997=CARTESIAN_POINT('Ctrl Pts',(-0.0827357067193459,-0.131725729802363,
-0.497608360770412));
#79998=CARTESIAN_POINT('Ctrl Pts',(-0.0818609364035401,-0.132271131773049,
-0.497535325332885));
#79999=CARTESIAN_POINT('Ctrl Pts',(-0.0783785078636803,-0.134394574351762,
-0.497248285123059));
#80000=CARTESIAN_POINT('Ctrl Pts',(-0.0757299472252032,-0.135904636535277,
-0.497038122408536));
#80001=CARTESIAN_POINT('Ctrl Pts',(-0.0641716661516806,-0.142051601800993,
-0.496147809065415));
#80002=CARTESIAN_POINT('Ctrl Pts',(-0.0548683034964049,-0.145897783318279,
-0.495496639247763));
#80003=CARTESIAN_POINT('Ctrl Pts',(-0.0393185507335059,-0.150626687133778,
-0.494421052898173));
#80004=CARTESIAN_POINT('Ctrl Pts',(-0.0332764171580743,-0.152075692279265,
-0.494006310708521));
#80005=CARTESIAN_POINT('Ctrl Pts',(-0.0244223047690646,-0.153646048911707,
-0.493390333417223));
#80006=CARTESIAN_POINT('Ctrl Pts',(-0.0216679392285962,-0.154058612567299,
-0.493197633867709));
#80007=CARTESIAN_POINT('Ctrl Pts',(-0.0175251316291427,-0.154565851287285,
-0.492905370004744));
#80008=CARTESIAN_POINT('Ctrl Pts',(-0.0161439817324513,-0.154716205537186,
-0.492807534477192));
#80009=CARTESIAN_POINT('Ctrl Pts',(-0.0136407136312016,-0.154954832039317,
-0.492629396279327));
#80010=CARTESIAN_POINT('Ctrl Pts',(-0.0125192870006524,-0.155049464277307,
-0.4925492977643));
#80011=CARTESIAN_POINT('Ctrl Pts',(-0.0100938961351406,-0.155227648622655,
-0.492375376192672));
#80012=CARTESIAN_POINT('Ctrl Pts',(-0.00878971719479617,-0.15530695514263,
-0.49228142706628));
#80013=CARTESIAN_POINT('Ctrl Pts',(-0.00519070321734847,-0.155480332747356,
-0.492020907865705));
#80014=CARTESIAN_POINT('Ctrl Pts',(-0.0028946297216905,-0.155540018496285,
-0.491853291530051));
#80015=CARTESIAN_POINT('Ctrl Pts',(0.0107255689918021,-0.155592396912694,
-0.490850098128626));
#80016=CARTESIAN_POINT('Ctrl Pts',(0.0220182511160713,-0.154399279535811,
-0.489978190746555));
#80017=CARTESIAN_POINT('Ctrl Pts',(0.0386583392054416,-0.15077777371226,
-0.488658457201511));
#80018=CARTESIAN_POINT('Ctrl Pts',(0.0441667417124337,-0.149257194507259,
-0.488216301165911));
#80019=CARTESIAN_POINT('Ctrl Pts',(0.0525026422809281,-0.146454045001594,
-0.487548545037632));
#80020=CARTESIAN_POINT('Ctrl Pts',(0.0553963414385408,-0.145384191888921,
-0.487317047741923));
#80021=CARTESIAN_POINT('Ctrl Pts',(0.0591891372278691,-0.143852216441358,
-0.487015661120233));
#80022=CARTESIAN_POINT('Ctrl Pts',(0.0601180949935887,-0.143466473218072,
-0.48694200989087));
#80023=CARTESIAN_POINT('Ctrl Pts',(0.0616523874747325,-0.142811848853248,
-0.486820717962775));
#80024=CARTESIAN_POINT('Ctrl Pts',(0.0622598513655658,-0.142548069163766,
-0.486772788210085));
#80025=CARTESIAN_POINT('Ctrl Pts',(0.06341715585927,-0.142036722021429,
-0.486681677161189));
#80026=CARTESIAN_POINT('Ctrl Pts',(0.0639672691093097,-0.141789825360126,
-0.486638454646653));
#80027=CARTESIAN_POINT('Ctrl Pts',(0.0654617826044792,-0.141108603554031,
-0.486521228380729));
#80028=CARTESIAN_POINT('Ctrl Pts',(0.066403308574594,-0.140667991184,-0.486447593753718));
#80029=CARTESIAN_POINT('Ctrl Pts',(0.0701535193260073,-0.138866933587541,
-0.486154886550108));
#80030=CARTESIAN_POINT('Ctrl Pts',(0.0729256007070044,-0.137431442932353,
-0.485939850573176));
#80031=CARTESIAN_POINT('Ctrl Pts',(0.0833909415714472,-0.131606169821783,
-0.485125963779368));
#80032=CARTESIAN_POINT('Ctrl Pts',(0.0907476807267762,-0.126645634115458,
-0.484548681889078));
#80033=CARTESIAN_POINT('Ctrl Pts',(0.103876513570282,-0.11605861886476,
-0.483435689760726));
#80034=CARTESIAN_POINT('Ctrl Pts',(0.109712144847356,-0.110558385142392,
-0.482902947248217));
#80035=CARTESIAN_POINT('Ctrl Pts',(0.1166835994487,-0.102889726689243,-0.482189222872197));
#80036=CARTESIAN_POINT('Ctrl Pts',(0.118229199977226,-0.101109908029082,
-0.482025447479451));
#80037=CARTESIAN_POINT('Ctrl Pts',(0.12056718469128,-0.0982906978328778,
-0.481768394091764));
#80038=CARTESIAN_POINT('Ctrl Pts',(0.121387959170355,-0.0972752306023971,
-0.481676264259538));
#80039=CARTESIAN_POINT('Ctrl Pts',(0.122892239417772,-0.0953654375535408,
-0.481503764131974));
#80040=CARTESIAN_POINT('Ctrl Pts',(0.123579014082919,-0.0944737865534997,
-0.481423530543508));
#80041=CARTESIAN_POINT('Ctrl Pts',(0.125092488453999,-0.0924640749466919,
-0.481243314523684));
#80042=CARTESIAN_POINT('Ctrl Pts',(0.12591398426824,-0.091342236437221,
-0.481143138800704));
#80043=CARTESIAN_POINT('Ctrl Pts',(0.127981988686494,-0.088437243570197,
-0.480884724783558));
#80044=CARTESIAN_POINT('Ctrl Pts',(0.129206288073323,-0.0866387310763382,
-0.480725671051356));
#80045=CARTESIAN_POINT('Ctrl Pts',(0.135190534387713,-0.0774387271699103,
-0.479916339863465));
#80046=CARTESIAN_POINT('Ctrl Pts',(0.139353300328491,-0.0696695706587878,
-0.479245260513665));
#80047=CARTESIAN_POINT('Ctrl Pts',(0.145794376233024,-0.0547320931331457,
-0.477987681289525));
#80048=CARTESIAN_POINT('Ctrl Pts',(0.148254273165585,-0.0476684220848824,
-0.477405629889092));
#80049=CARTESIAN_POINT('Ctrl Pts',(0.15082799391562,-0.0381130222986628,
-0.476651100529235));
#80050=CARTESIAN_POINT('Ctrl Pts',(0.151404014657583,-0.0357562846715602,
-0.47646762093376));
#80051=CARTESIAN_POINT('Ctrl Pts',(0.152296328759981,-0.0316958744410001,
-0.476156951728635));
#80052=CARTESIAN_POINT('Ctrl Pts',(0.152639711373453,-0.0299986562386409,
-0.47602870633689));
#80053=CARTESIAN_POINT('Ctrl Pts',(0.153102180125304,-0.0274987676104102,
-0.475842499786221));
#80054=CARTESIAN_POINT('Ctrl Pts',(0.153243428496939,-0.0267004022310868,
-0.475783433355032));
#80055=CARTESIAN_POINT('Ctrl Pts',(0.153484116848531,-0.0252751105644787,
-0.475678740258841));
#80056=CARTESIAN_POINT('Ctrl Pts',(0.15358596945583,-0.0246486382811247,
-0.475632986189785));
#80057=CARTESIAN_POINT('Ctrl Pts',(0.153805418384035,-0.0232446561843723,
-0.475531033161508));
#80058=CARTESIAN_POINT('Ctrl Pts',(0.153920957334319,-0.0224668584677605,
-0.475474947448035));
#80059=CARTESIAN_POINT('Ctrl Pts',(0.154253878660928,-0.0201024354085416,
-0.475305560196372));
#80060=CARTESIAN_POINT('Ctrl Pts',(0.154452670520549,-0.0185132406739496,
-0.475193221040861));
#80061=CARTESIAN_POINT('Ctrl Pts',(0.155410549127436,-0.00976008077510311,
-0.474581340573928));
#80062=CARTESIAN_POINT('Ctrl Pts',(0.155695886995841,-0.00255227474429615,
-0.47410250908144));
#80063=CARTESIAN_POINT('Ctrl Pts',(0.155294125701423,0.0108809466628106,
-0.473215299998125));
#80064=CARTESIAN_POINT('Ctrl Pts',(0.154733401815542,0.0170948305963474,
-0.472806936328222));
#80065=CARTESIAN_POINT('Ctrl Pts',(0.153151746601219,0.0275539486532268,
-0.472103326869293));
#80066=CARTESIAN_POINT('Ctrl Pts',(0.152322497727317,0.0318202766477223,
-0.471811685215285));
#80067=CARTESIAN_POINT('Ctrl Pts',(0.150594349094953,0.0390747748456741,
-0.471302720845007));
#80068=CARTESIAN_POINT('Ctrl Pts',(0.149782138188398,0.0420809324082278,
-0.471087887347038));
#80069=CARTESIAN_POINT('Ctrl Pts',(0.148460678986912,0.0464470430144603,
-0.470768915289218));
#80070=CARTESIAN_POINT('Ctrl Pts',(0.148021698981767,0.0478275798202348,
-0.470667025688643));
#80071=CARTESIAN_POINT('Ctrl Pts',(0.147205965746631,0.0502740878637355,
-0.470484508878888));
#80072=CARTESIAN_POINT('Ctrl Pts',(0.146836747216872,0.0513424756543966,
-0.470404132772739));
#80073=CARTESIAN_POINT('Ctrl Pts',(0.146029109669307,0.0535995012085676,
-0.470232855494985));
#80074=CARTESIAN_POINT('Ctrl Pts',(0.145587749733694,0.0547869907292133,
-0.470141862063698));
#80075=CARTESIAN_POINT('Ctrl Pts',(0.144351756042345,0.0579920222648916,
-0.469893805071429));
#80076=CARTESIAN_POINT('Ctrl Pts',(0.143529387203179,0.0599984854298684,
-0.469735832298064));
#80077=CARTESIAN_POINT('Ctrl Pts',(0.137640669489281,0.0735515851616843,
-0.468649795239274));
#80078=CARTESIAN_POINT('Ctrl Pts',(0.131229319903731,0.0844602341709095,
-0.46767498093543));
#80079=CARTESIAN_POINT('Ctrl Pts',(0.119492943675741,0.0998117965549145,
-0.466178528546635));
#80080=CARTESIAN_POINT('Ctrl Pts',(0.115069603996479,0.104880704764188,
-0.465660516783328));
#80081=CARTESIAN_POINT('Ctrl Pts',(0.109198510417998,0.110788414591302,
-0.465039328019619));
#80082=CARTESIAN_POINT('Ctrl Pts',(0.108047499253096,0.111911241269032,
-0.464920424820589));
#80083=CARTESIAN_POINT('Ctrl Pts',(0.106307044207402,0.113557188451459,
-0.464745125340443));
#80084=CARTESIAN_POINT('Ctrl Pts',(0.105730743316155,0.114093964285778,
-0.464687793261765));
#80085=CARTESIAN_POINT('Ctrl Pts',(0.104729214258366,0.115012698505431,
-0.464589418457173));
#80086=CARTESIAN_POINT('Ctrl Pts',(0.104305931785258,0.115396714692346,
-0.46454822598989));
#80087=CARTESIAN_POINT('Ctrl Pts',(0.103370776179674,0.116235769656211,
-0.464458058118187));
#80088=CARTESIAN_POINT('Ctrl Pts',(0.102858006390457,0.116689768536294,
-0.464409157882756));
#80089=CARTESIAN_POINT('Ctrl Pts',(0.102342242837716,0.117140376604081,
-0.464360489961667));
#80090=CARTESIAN_POINT('Origin',(0.,0.,-1.10400562256037));
#80091=CARTESIAN_POINT('',(0.102342242837719,0.117140376604078,-0.380699116973164));
#80092=CARTESIAN_POINT('',(0.102342226162682,0.117140391172586,-0.39458065504025));
#80093=CARTESIAN_POINT('',(0.10234224283772,0.117140376604078,-1.10400562256037));
#80094=CARTESIAN_POINT('',(-0.155549964438899,-0.000105181068850209,-0.425194377435439));
#80095=CARTESIAN_POINT('Ctrl Pts',(-0.155549964438899,-0.000105181068849798,
-0.425194377435439));
#80096=CARTESIAN_POINT('Ctrl Pts',(-0.15554199223784,-0.0118950935007836,
-0.424353019449778));
#80097=CARTESIAN_POINT('Ctrl Pts',(-0.154189456344414,-0.0236317205017142,
-0.423511661464117));
#80098=CARTESIAN_POINT('Ctrl Pts',(-0.151552560981598,-0.0350374622357128,
-0.422670303478456));
#80099=CARTESIAN_POINT('Ctrl Pts',(-0.150029091611429,-0.0416271428202483,
-0.422184207921318));
#80100=CARTESIAN_POINT('Ctrl Pts',(-0.148077844605863,-0.0481067002624013,
-0.421698112364181));
#80101=CARTESIAN_POINT('Ctrl Pts',(-0.145717689281867,-0.0544257065213981,
-0.421212016807043));
#80102=CARTESIAN_POINT('Ctrl Pts',(-0.142136562455347,-0.0640137038031714,
-0.420474451011174));
#80103=CARTESIAN_POINT('Ctrl Pts',(-0.137591758783405,-0.0732823674305032,
-0.419736885215305));
#80104=CARTESIAN_POINT('Ctrl Pts',(-0.132162453570186,-0.0820298016961415,
-0.418999319419436));
#80105=CARTESIAN_POINT('Ctrl Pts',(-0.126720241982456,-0.0907980300888769,
-0.41826000030523));
#80106=CARTESIAN_POINT('Ctrl Pts',(-0.120389682031306,-0.0990416821244272,
-0.417520681191024));
#80107=CARTESIAN_POINT('Ctrl Pts',(-0.11329784291094,-0.106580492078653,
-0.416781362076818));
#80108=CARTESIAN_POINT('Ctrl Pts',(-0.1062389721284,-0.114084255829891,
-0.416045479888056));
#80109=CARTESIAN_POINT('Ctrl Pts',(-0.098426521213838,-0.120889034757036,
-0.415309597699294));
#80110=CARTESIAN_POINT('Ctrl Pts',(-0.0900250076149486,-0.126851489955493,
-0.414573715510532));
#80111=CARTESIAN_POINT('Ctrl Pts',(-0.081564635323124,-0.13285571647474,
-0.413832677933604));
#80112=CARTESIAN_POINT('Ctrl Pts',(-0.0725076815596746,-0.13800521080565,
-0.413091640356676));
#80113=CARTESIAN_POINT('Ctrl Pts',(-0.0630515187879494,-0.142198131065541,
-0.412350602779747));
#80114=CARTESIAN_POINT('Ctrl Pts',(-0.0535953560162242,-0.146391051325432,
-0.411609565202819));
#80115=CARTESIAN_POINT('Ctrl Pts',(-0.043740899244311,-0.149627132860022,
-0.410868527625891));
#80116=CARTESIAN_POINT('Ctrl Pts',(-0.0337020367136042,-0.151855112595378,
-0.410127490048963));
#80117=CARTESIAN_POINT('Ctrl Pts',(-0.023710206524963,-0.154072654185505,
-0.409389924253095));
#80118=CARTESIAN_POINT('Ctrl Pts',(-0.0134614412551567,-0.155308039266046,
-0.408652358457228));
#80119=CARTESIAN_POINT('Ctrl Pts',(-0.00316819151771157,-0.155517732308914,
-0.40791479266136));
#80120=CARTESIAN_POINT('Ctrl Pts',(0.00714952701103393,-0.155727923827525,
-0.407175473547153));
#80121=CARTESIAN_POINT('Ctrl Pts',(0.0175110175694432,-0.154907374263842,
-0.406436154432947));
#80122=CARTESIAN_POINT('Ctrl Pts',(0.027695890656914,-0.153064496669607,
-0.40569683531874));
#80123=CARTESIAN_POINT('Ctrl Pts',(0.0378334165991526,-0.151230186191758,
-0.404960953129979));
#80124=CARTESIAN_POINT('Ctrl Pts',(0.0477950452169169,-0.148383194653096,
-0.404225070941218));
#80125=CARTESIAN_POINT('Ctrl Pts',(0.0573709661843662,-0.14458345250779,
-0.403489188752457));
#80126=CARTESIAN_POINT('Ctrl Pts',(0.0670139734197114,-0.140757090414349,
-0.402748151175528));
#80127=CARTESIAN_POINT('Ctrl Pts',(0.0762649600205053,-0.135964914473338,
-0.402007113598599));
#80128=CARTESIAN_POINT('Ctrl Pts',(0.0849310292404507,-0.130317008760015,
-0.40126607602167));
#80129=CARTESIAN_POINT('Ctrl Pts',(0.0935970984603964,-0.124669103046691,
-0.40052503844474));
#80130=CARTESIAN_POINT('Ctrl Pts',(0.101677530059382,-0.11816609088751,
-0.399784000867811));
#80131=CARTESIAN_POINT('Ctrl Pts',(0.109012855546433,-0.110959451267626,
-0.399042963290882));
#80132=CARTESIAN_POINT('Ctrl Pts',(0.1163138148355,-0.103786574948962,-0.398305397495011));
#80133=CARTESIAN_POINT('Ctrl Pts',(0.122930924860931,-0.0958633672169234,
-0.39756783169914));
#80134=CARTESIAN_POINT('Ctrl Pts',(0.128711981306915,-0.0873443093054628,
-0.396830265903269));
#80135=CARTESIAN_POINT('Ctrl Pts',(0.134506780299418,-0.0788050001560606,
-0.396090946789064));
#80136=CARTESIAN_POINT('Ctrl Pts',(0.13946090297529,-0.0696676889163956,
-0.395351627674858));
#80137=CARTESIAN_POINT('Ctrl Pts',(0.143461392679693,-0.0601218039516679,
-0.394612308560653));
#80138=CARTESIAN_POINT('Ctrl Pts',(0.14744328502258,-0.0506202956225042,
-0.393876426371889));
#80139=CARTESIAN_POINT('Ctrl Pts',(0.150480027741536,-0.0407148628101957,
-0.393140544183125));
#80140=CARTESIAN_POINT('Ctrl Pts',(0.152507634197353,-0.0306141145801488,
-0.392404661994361));
#80141=CARTESIAN_POINT('Ctrl Pts',(0.154549445506174,-0.0204426032868703,
-0.391663624417434));
#80142=CARTESIAN_POINT('Ctrl Pts',(0.155567726303639,-0.010073957880923,
-0.390922586840508));
#80143=CARTESIAN_POINT('Ctrl Pts',(0.155549765518353,0.000270087366504549,
-0.390181549263582));
#80144=CARTESIAN_POINT('Ctrl Pts',(0.155531804733066,0.0106141326139321,
-0.389440511686656));
#80145=CARTESIAN_POINT('Ctrl Pts',(0.154477732960773,0.0209326341847206,
-0.388699474109729));
#80146=CARTESIAN_POINT('Ctrl Pts',(0.152427761566985,0.0310093534869439,
-0.387958436532803));
#80147=CARTESIAN_POINT('Ctrl Pts',(0.150387355153145,0.0410390557340294,
-0.387220856569766));
#80148=CARTESIAN_POINT('Ctrl Pts',(0.147345195883627,0.0509037798324544,
-0.386483276606728));
#80149=CARTESIAN_POINT('Ctrl Pts',(0.143347972080018,0.0603917328824605,
-0.385745696643691));
#80150=CARTESIAN_POINT('Ctrl Pts',(0.139359353640141,0.0698592599340547,
-0.385009704568691));
#80151=CARTESIAN_POINT('Ctrl Pts',(0.134420035713166,0.0789507499674971,
-0.384273712493692));
#80152=CARTESIAN_POINT('Ctrl Pts',(0.128625973318703,0.0874709179545767,
-0.383537720418693));
#80153=CARTESIAN_POINT('Ctrl Pts',(0.122834693202875,0.0959869946012906,
-0.382802081763261));
#80154=CARTESIAN_POINT('Ctrl Pts',(0.116189977295208,0.103931512126628,
-0.382066443107829));
#80155=CARTESIAN_POINT('Ctrl Pts',(0.10883162232711,0.111137214656699,-0.381330804452397));
#80156=CARTESIAN_POINT('Ctrl Pts',(0.106725433975545,0.11319970916797,-0.381120241959319));
#80157=CARTESIAN_POINT('Ctrl Pts',(0.10456102684995,0.115201887598262,-0.380909679466242));
#80158=CARTESIAN_POINT('Ctrl Pts',(0.102342242837719,0.117140376604078,
-0.380699116973164));
#80159=CARTESIAN_POINT('Ctrl Pts',(0.102342242837719,0.117140376604078,
-0.450689508133418));
#80160=CARTESIAN_POINT('Ctrl Pts',(0.0945869527699116,0.123915954781355,
-0.449953493924327));
#80161=CARTESIAN_POINT('Ctrl Pts',(0.0861470817054412,0.129925828488917,
-0.449217479715235));
#80162=CARTESIAN_POINT('Ctrl Pts',(0.0771988637065197,0.135041245337942,
-0.448481465506144));
#80163=CARTESIAN_POINT('Ctrl Pts',(0.0682526309237161,0.140155527300894,
-0.447745614586242));
#80164=CARTESIAN_POINT('Ctrl Pts',(0.058799090187575,0.144375305689882,
-0.447009763666341));
#80165=CARTESIAN_POINT('Ctrl Pts',(0.0490395970987759,0.147617480050263,
-0.44627391274644));
#80166=CARTESIAN_POINT('Ctrl Pts',(0.0392574537660712,0.150867178985883,
-0.445536354032633));
#80167=CARTESIAN_POINT('Ctrl Pts',(0.0291688402668807,0.153134515555881,
-0.444798795318827));
#80168=CARTESIAN_POINT('Ctrl Pts',(0.0189889153761444,0.154386604317984,
-0.44406123660502));
#80169=CARTESIAN_POINT('Ctrl Pts',(0.0158596541469504,0.154771490538738,
-0.443834514511081));
#80170=CARTESIAN_POINT('Ctrl Pts',(0.0127217996521047,0.155060815621456,
-0.443607792417142));
#80171=CARTESIAN_POINT('Ctrl Pts',(0.00958162925438207,0.155254613074239,
-0.443381070323204));
#80172=CARTESIAN_POINT('Ctrl Pts',(-0.000633882777645995,0.155885069374354,
-0.442643504527335));
#80173=CARTESIAN_POINT('Ctrl Pts',(-0.0109498481215258,0.155505299869314,
-0.441905938731466));
#80174=CARTESIAN_POINT('Ctrl Pts',(-0.0211496244755702,0.154105470002016,
-0.441168372935597));
#80175=CARTESIAN_POINT('Ctrl Pts',(-0.0313736474188955,0.152702312502947,
-0.440429053821391));
#80176=CARTESIAN_POINT('Ctrl Pts',(-0.041479989427979,0.150274218729261,
-0.439689734707185));
#80177=CARTESIAN_POINT('Ctrl Pts',(-0.0512522767152041,0.14686390513502,
-0.438950415592979));
#80178=CARTESIAN_POINT('Ctrl Pts',(-0.0609791348742219,0.143469445308576,
-0.438214533404217));
#80179=CARTESIAN_POINT('Ctrl Pts',(-0.0703741556842587,0.13910218191845,
-0.437478651215455));
#80180=CARTESIAN_POINT('Ctrl Pts',(-0.0792394575613944,0.133854065554155,
-0.436742769026693));
#80181=CARTESIAN_POINT('Ctrl Pts',(-0.0881668673045523,0.128569182330418,
-0.436001731449764));
#80182=CARTESIAN_POINT('Ctrl Pts',(-0.0965562831422183,0.122391528630175,
-0.435260693872836));
#80183=CARTESIAN_POINT('Ctrl Pts',(-0.104234359520524,0.115459953210393,
-0.434519656295908));
#80184=CARTESIAN_POINT('Ctrl Pts',(-0.11191243589883,0.108528377790611,
-0.433778618718979));
#80185=CARTESIAN_POINT('Ctrl Pts',(-0.11887855872073,0.100843608776628,
-0.433037581142051));
#80186=CARTESIAN_POINT('Ctrl Pts',(-0.124998863260372,0.0925801635536185,
-0.432296543565123));
#80187=CARTESIAN_POINT('Ctrl Pts',(-0.131118548775831,0.0843175541178476,
-0.431555580938743));
#80188=CARTESIAN_POINT('Ctrl Pts',(-0.136438394268224,0.0754146803388129,
-0.430814618312363));
#80189=CARTESIAN_POINT('Ctrl Pts',(-0.140830805721119,0.0660491230822964,
-0.430073655685982));
#80190=CARTESIAN_POINT('Ctrl Pts',(-0.145212958838233,0.0567054387837563,
-0.429334423554003));
#80191=CARTESIAN_POINT('Ctrl Pts',(-0.14867151697737,0.0469019995313918,
-0.428595191422023));
#80192=CARTESIAN_POINT('Ctrl Pts',(-0.151123982145288,0.0368421568390167,
-0.427855959290043));
#80193=CARTESIAN_POINT('Ctrl Pts',(-0.153574248969686,0.0267913315998867,
-0.427117389791803));
#80194=CARTESIAN_POINT('Ctrl Pts',(-0.155019961917213,0.0164854361025983,
-0.426378820293564));
#80195=CARTESIAN_POINT('Ctrl Pts',(-0.155428695874673,0.00614190513589349,
-0.425640250795324));
#80196=CARTESIAN_POINT('Ctrl Pts',(-0.155510946577613,0.00406044682454401,
-0.425491626343426));
#80197=CARTESIAN_POINT('Ctrl Pts',(-0.15555137271386,0.00197748689463135,
-0.425343001891527));
#80198=CARTESIAN_POINT('Ctrl Pts',(-0.155549964438939,-0.000105181010130192,
-0.425194377439629));
#80199=CARTESIAN_POINT('Ctrl Pts',(0.102342242837716,0.117140376604081,
-0.464360489961667));
#80200=CARTESIAN_POINT('Ctrl Pts',(0.102273383127856,0.117200537390247,
-0.464353992296394));
#80201=CARTESIAN_POINT('Ctrl Pts',(0.10220447005422,0.117260637735246,-0.4643474987721));
#80202=CARTESIAN_POINT('Ctrl Pts',(0.101002868152768,0.118306712630067,
-0.464234433445973));
#80203=CARTESIAN_POINT('Ctrl Pts',(0.0998559583886079,0.119276341474565,
-0.464128972645868));
#80204=CARTESIAN_POINT('Ctrl Pts',(0.0914084520228417,0.126210824756935,
-0.463368331933307));
#80205=CARTESIAN_POINT('Ctrl Pts',(0.0835920180079179,0.131518445458895,
-0.462750010536962));
#80206=CARTESIAN_POINT('Ctrl Pts',(0.0674381492762283,0.140461802163869,
-0.461533810153033));
#80207=CARTESIAN_POINT('Ctrl Pts',(0.0591689174924994,0.144140340351055,
-0.460938180434492));
#80208=CARTESIAN_POINT('Ctrl Pts',(0.0480187542505892,0.147978427119094,
-0.460130162411003));
#80209=CARTESIAN_POINT('Ctrl Pts',(0.0453865098418074,0.148806850643875,
-0.45993918702109));
#80210=CARTESIAN_POINT('Ctrl Pts',(0.0414025381178753,0.149945153824693,
-0.459649012662938));
#80211=CARTESIAN_POINT('Ctrl Pts',(0.0400663387427968,0.150307709713359,
-0.459551504752954));
#80212=CARTESIAN_POINT('Ctrl Pts',(0.0376357935218256,0.150932486575182,
-0.459373709758614));
#80213=CARTESIAN_POINT('Ctrl Pts',(0.0365430915322467,0.151200763219292,
-0.459293623026787));
#80214=CARTESIAN_POINT('Ctrl Pts',(0.0341717262928903,0.151755766435899,
-0.459119435513835));
#80215=CARTESIAN_POINT('Ctrl Pts',(0.0328921665741747,0.152038234364553,
-0.459025205544927));
#80216=CARTESIAN_POINT('Ctrl Pts',(0.029343224387433,0.152774780692246,
-0.458763111187242));
#80217=CARTESIAN_POINT('Ctrl Pts',(0.0270671280667928,0.153194412272351,
-0.458594179714592));
#80218=CARTESIAN_POINT('Ctrl Pts',(0.0138089107062163,0.155334076441763,
-0.45760478160228));
#80219=CARTESIAN_POINT('Ctrl Pts',(0.00267887631684841,0.155923374265372,
-0.456749511995822));
#80220=CARTESIAN_POINT('Ctrl Pts',(-0.0142447024928887,0.155006311867815,
-0.455436053330004));
#80221=CARTESIAN_POINT('Ctrl Pts',(-0.0200506514537917,0.154362711522413,
-0.454983830980701));
#80222=CARTESIAN_POINT('Ctrl Pts',(-0.0288880445425049,0.152875914483139,
-0.454303147399978));
#80223=CARTESIAN_POINT('Ctrl Pts',(-0.0319530889213901,0.152264794739188,
-0.454068555978212));
#80224=CARTESIAN_POINT('Ctrl Pts',(-0.0359822441043171,0.151334402043461,
-0.453763842364232));
#80225=CARTESIAN_POINT('Ctrl Pts',(-0.0369644019649006,0.151097505817334,
-0.453689857362875));
#80226=CARTESIAN_POINT('Ctrl Pts',(-0.0385873217286234,0.150689285796646,
-0.453568166781194));
#80227=CARTESIAN_POINT('Ctrl Pts',(-0.0392294072950517,0.150523406534299,
-0.453520168378703));
#80228=CARTESIAN_POINT('Ctrl Pts',(-0.0404523919771729,0.150199097777176,
-0.453429050557898));
#80229=CARTESIAN_POINT('Ctrl Pts',(-0.0410334616694395,0.150041394442107,
-0.453385888778444));
#80230=CARTESIAN_POINT('Ctrl Pts',(-0.042610685521492,0.149603485142612,
-0.453269050917933));
#80231=CARTESIAN_POINT('Ctrl Pts',(-0.0436050051765083,0.14931670021704,
-0.45319573969795));
#80232=CARTESIAN_POINT('Ctrl Pts',(-0.0475482651125873,0.148136621786212,
-0.452906107010234));
#80233=CARTESIAN_POINT('Ctrl Pts',(-0.0504734535386896,0.147165654402174,
-0.452693715955252));
#80234=CARTESIAN_POINT('Ctrl Pts',(-0.0617153359925256,0.143059401321248,
-0.451880076352907));
#80235=CARTESIAN_POINT('Ctrl Pts',(-0.0697866059163284,0.139300503670522,
-0.451300806194502));
#80236=CARTESIAN_POINT('Ctrl Pts',(-0.0844501399166961,0.130875334844449,
-0.450184824916392));
#80237=CARTESIAN_POINT('Ctrl Pts',(-0.0910866090001889,0.126346298564955,
-0.449651112211696));
#80238=CARTESIAN_POINT('Ctrl Pts',(-0.0991837315935736,0.119849717939578,
-0.448936213283125));
#80239=CARTESIAN_POINT('Ctrl Pts',(-0.100989815815044,0.118331836767116,
-0.448772304710144));
#80240=CARTESIAN_POINT('Ctrl Pts',(-0.103741101150282,0.115910708216065,
-0.44851508852352));
#80241=CARTESIAN_POINT('Ctrl Pts',(-0.104710660537534,0.115035584634023,
-0.448422931494508));
#80242=CARTESIAN_POINT('Ctrl Pts',(-0.106494951341316,0.113383836859246,
-0.448250406662965));
#80243=CARTESIAN_POINT('Ctrl Pts',(-0.107312501171839,0.112610372936681,
-0.448170175899296));
#80244=CARTESIAN_POINT('Ctrl Pts',(-0.109120812231424,0.110861998572991,
-0.447990000553222));
#80245=CARTESIAN_POINT('Ctrl Pts',(-0.110107032500817,0.109882553447126,
-0.447889863085197));
#80246=CARTESIAN_POINT('Ctrl Pts',(-0.112601669766067,0.107337745938541,
-0.447631618782498));
#80247=CARTESIAN_POINT('Ctrl Pts',(-0.114090592093974,0.105753787907573,
-0.447472698339076));
#80248=CARTESIAN_POINT('Ctrl Pts',(-0.121453755798805,0.097584124337845,
-0.446661682269395));
#80249=CARTESIAN_POINT('Ctrl Pts',(-0.126792271660576,0.0905392176756994,
-0.445988649653727));
#80250=CARTESIAN_POINT('Ctrl Pts',(-0.135485092709898,0.07677984111134,
-0.444730370860713));
#80251=CARTESIAN_POINT('Ctrl Pts',(-0.139008039593366,0.0702006063947223,
-0.444149640067028));
#80252=CARTESIAN_POINT('Ctrl Pts',(-0.143033222847984,0.061181452160883,
-0.443396609619197));
#80253=CARTESIAN_POINT('Ctrl Pts',(-0.14396889553151,0.0589460038775934,
-0.443213343113782));
#80254=CARTESIAN_POINT('Ctrl Pts',(-0.145482480732827,0.0550785168834813,
-0.442902993349576));
#80255=CARTESIAN_POINT('Ctrl Pts',(-0.146086069110067,0.0534570508601559,
-0.44277485697675));
#80256=CARTESIAN_POINT('Ctrl Pts',(-0.146932540071791,0.0510616100265278,
-0.442588777164272));
#80257=CARTESIAN_POINT('Ctrl Pts',(-0.147196599843968,0.0502953320134109,
-0.442529730500426));
#80258=CARTESIAN_POINT('Ctrl Pts',(-0.14765675025871,0.0489253455026532,
-0.442425057813741));
#80259=CARTESIAN_POINT('Ctrl Pts',(-0.147855149226051,0.0483224608308629,
-0.442379304609632));
#80260=CARTESIAN_POINT('Ctrl Pts',(-0.148291151917845,0.0469697285999913,
-0.442277335645265));
#80261=CARTESIAN_POINT('Ctrl Pts',(-0.148526764896833,0.0462192743552451,
-0.44222123333554));
#80262=CARTESIAN_POINT('Ctrl Pts',(-0.149225133434975,0.0439343889128088,
-0.442051742500243));
#80263=CARTESIAN_POINT('Ctrl Pts',(-0.149669894145649,0.0423945077254265,
-0.441939318076861));
#80264=CARTESIAN_POINT('Ctrl Pts',(-0.152011041710859,0.0337922473756497,
-0.441319826793158));
#80265=CARTESIAN_POINT('Ctrl Pts',(-0.153431612341769,0.0266090104343941,
-0.440834124095532));
#80266=CARTESIAN_POINT('Ctrl Pts',(-0.155141457102581,0.0129719579906293,
-0.439927036330913));
#80267=CARTESIAN_POINT('Ctrl Pts',(-0.155545019498552,0.0065489010164554,
-0.439505840719987));
#80268=CARTESIAN_POINT('Ctrl Pts',(-0.155554687920093,-0.00604830111625869,
-0.438666773939041));
#80269=CARTESIAN_POINT('Ctrl Pts',(-0.155192595328809,-0.0122101478716149,
-0.438250224472298));
#80270=CARTESIAN_POINT('Ctrl Pts',(-0.154245906872207,-0.0201861980903193,
-0.437693067194438));
#80271=CARTESIAN_POINT('Ctrl Pts',(-0.153992741246545,-0.0220344618013044,
-0.437562714821551));
#80272=CARTESIAN_POINT('Ctrl Pts',(-0.153521630372683,-0.0250671192107265,
-0.437346543927467));
#80273=CARTESIAN_POINT('Ctrl Pts',(-0.153323056712552,-0.0262543632955327,
-0.437261336221811));
#80274=CARTESIAN_POINT('Ctrl Pts',(-0.152907496161228,-0.0285731949652815,
-0.437093717823636));
#80275=CARTESIAN_POINT('Ctrl Pts',(-0.152691675561865,-0.0297049143416587,
-0.437011349035311));
#80276=CARTESIAN_POINT('Ctrl Pts',(-0.152146413066709,-0.0324010368771696,
-0.43681372331183));
#80277=CARTESIAN_POINT('Ctrl Pts',(-0.151805391623711,-0.0339629345239154,
-0.436698106679225));
#80278=CARTESIAN_POINT('Ctrl Pts',(-0.150508872076115,-0.0394907939181744,
-0.436284738665284));
#80279=CARTESIAN_POINT('Ctrl Pts',(-0.149421590564192,-0.0434237960688197,
-0.435982888599719));
#80280=CARTESIAN_POINT('Ctrl Pts',(-0.146200630768544,-0.053512430439989,
-0.435187868835745));
#80281=CARTESIAN_POINT('Ctrl Pts',(-0.143832785339941,-0.0595845520368354,
-0.434688508265065));
#80282=CARTESIAN_POINT('Ctrl Pts',(-0.136826691907896,-0.0746785114488359,
-0.433401553096011));
#80283=CARTESIAN_POINT('Ctrl Pts',(-0.131673966068072,-0.0834291387637996,
-0.432609997655158));
#80284=CARTESIAN_POINT('Ctrl Pts',(-0.124851345500854,-0.0927903661990848,
-0.431748100419001));
#80285=CARTESIAN_POINT('Ctrl Pts',(-0.123979763315437,-0.0939517387796647,
-0.431640918226325));
#80286=CARTESIAN_POINT('Ctrl Pts',(-0.122623809719798,-0.095706793057841,
-0.431478759439734));
#80287=CARTESIAN_POINT('Ctrl Pts',(-0.122151130530738,-0.0963093470219964,
-0.431423052111199));
#80288=CARTESIAN_POINT('Ctrl Pts',(-0.121277780371052,-0.0974058877887452,
-0.431321648888495));
#80289=CARTESIAN_POINT('Ctrl Pts',(-0.120878516117451,-0.0979009262303392,
-0.431275864187193));
#80290=CARTESIAN_POINT('Ctrl Pts',(-0.119947627560858,-0.0990407361073701,
-0.431170418168864));
#80291=CARTESIAN_POINT('Ctrl Pts',(-0.119413829548268,-0.0996836905545983,
-0.431110911452802));
#80292=CARTESIAN_POINT('Ctrl Pts',(-0.117668387066577,-0.101751916325438,
-0.430919290288429));
#80293=CARTESIAN_POINT('Ctrl Pts',(-0.116436154482214,-0.103159703961293,
-0.430788542640987));
#80294=CARTESIAN_POINT('Ctrl Pts',(-0.11336641697481,-0.106541678731171,
-0.430472658602986));
#80295=CARTESIAN_POINT('Ctrl Pts',(-0.111502353107589,-0.108491017162094,
-0.430289040084084));
#80296=CARTESIAN_POINT('Ctrl Pts',(-0.102961046808947,-0.116970225698991,
-0.429477907951531));
#80297=CARTESIAN_POINT('Ctrl Pts',(-0.0957543248465152,-0.122939578218008,
-0.4288715835954));
#80298=CARTESIAN_POINT('Ctrl Pts',(-0.0820289690876509,-0.13236500040725,
-0.427768400687438));
#80299=CARTESIAN_POINT('Ctrl Pts',(-0.075719136167067,-0.13607291230543,
-0.42727796413229));
#80300=CARTESIAN_POINT('Ctrl Pts',(-0.0674299815768194,-0.140188391398987,
-0.426636830968148));
#80301=CARTESIAN_POINT('Ctrl Pts',(-0.0656714199494314,-0.141020748534759,
-0.426501022953783));
#80302=CARTESIAN_POINT('Ctrl Pts',(-0.0627851718758298,-0.142321164525712,
-0.426278197111946));
#80303=CARTESIAN_POINT('Ctrl Pts',(-0.061666736694328,-0.142809331323208,
-0.426191868511892));
#80304=CARTESIAN_POINT('Ctrl Pts',(-0.0594889580944578,-0.143729520219288,
-0.426023742695757));
#80305=CARTESIAN_POINT('Ctrl Pts',(-0.058430361601978,-0.14416311536826,
-0.425942005044496));
#80306=CARTESIAN_POINT('Ctrl Pts',(-0.0559271320274577,-0.145156323844406,
-0.425748639461388));
#80307=CARTESIAN_POINT('Ctrl Pts',(-0.0544787547995319,-0.145706099404677,
-0.425636692351353));
#80308=CARTESIAN_POINT('Ctrl Pts',(-0.0495107717165426,-0.147507420714917,
-0.425252350959622));
#80309=CARTESIAN_POINT('Ctrl Pts',(-0.045954659809813,-0.148653693519369,
-0.424976590046232));
#80310=CARTESIAN_POINT('Ctrl Pts',(-0.03690491349467,-0.151215023822785,
-0.424272773075451));
#80311=CARTESIAN_POINT('Ctrl Pts',(-0.0313689887452169,-0.152459605212025,
-0.423840241952703));
#80312=CARTESIAN_POINT('Ctrl Pts',(-0.0174172111038909,-0.154804133058094,
-0.422749811353617));
#80313=CARTESIAN_POINT('Ctrl Pts',(-0.00895560974873443,-0.155523240595038,
-0.422087640583578));
#80314=CARTESIAN_POINT('Ctrl Pts',(0.00315134924843414,-0.155560407106869,
-0.421163818662137));
#80315=CARTESIAN_POINT('Ctrl Pts',(0.00677983169964172,-0.155444555774993,
-0.420890131226195));
#80316=CARTESIAN_POINT('Ctrl Pts',(0.0114915123117164,-0.155128790577476,
-0.420541444965241));
#80317=CARTESIAN_POINT('Ctrl Pts',(0.0125810207736793,-0.155044234389489,
-0.420461286123524));
#80318=CARTESIAN_POINT('Ctrl Pts',(0.0143475853713237,-0.15488838740217,
-0.420332171300241));
#80319=CARTESIAN_POINT('Ctrl Pts',(0.0150252003981042,-0.154824123310057,
-0.420282850866333));
#80320=CARTESIAN_POINT('Ctrl Pts',(0.0163664661775842,-0.154688030640773,
-0.420185661353746));
#80321=CARTESIAN_POINT('Ctrl Pts',(0.0170301157202365,-0.154616374400829,
-0.420137785079173));
#80322=CARTESIAN_POINT('Ctrl Pts',(0.0187179169767573,-0.154423138459113,
-0.420016519502882));
#80323=CARTESIAN_POINT('Ctrl Pts',(0.0197413814980716,-0.15429563867892,
-0.419943448843378));
#80324=CARTESIAN_POINT('Ctrl Pts',(0.0240559714763751,-0.153714506495937,
-0.419637075019275));
#80325=CARTESIAN_POINT('Ctrl Pts',(0.0273336454300653,-0.153165645457995,
-0.419408431574137));
#80326=CARTESIAN_POINT('Ctrl Pts',(0.0369608400545467,-0.151234584568491,
-0.418742316226919));
#80327=CARTESIAN_POINT('Ctrl Pts',(0.0432443585596993,-0.149559154453393,
-0.418314471503221));
#80328=CARTESIAN_POINT('Ctrl Pts',(0.0590104423181322,-0.144278152126124,
-0.417219228716014));
#80329=CARTESIAN_POINT('Ctrl Pts',(0.0682774551253329,-0.140130566603647,
-0.416552929954819));
#80330=CARTESIAN_POINT('Ctrl Pts',(0.0789448092232963,-0.134045340375308,
-0.415707536708337));
#80331=CARTESIAN_POINT('Ctrl Pts',(0.080792149342832,-0.132940076803219,
-0.415558148656184));
#80332=CARTESIAN_POINT('Ctrl Pts',(0.0837883610557263,-0.131061923947238,
-0.415310493492284));
#80333=CARTESIAN_POINT('Ctrl Pts',(0.0849509410998604,-0.130311376115607,
-0.415213033963486));
#80334=CARTESIAN_POINT('Ctrl Pts',(0.0870403383383378,-0.128922643001383,
-0.415035289493543));
#80335=CARTESIAN_POINT('Ctrl Pts',(0.0879705482491184,-0.128289714694196,
-0.414955204343035));
#80336=CARTESIAN_POINT('Ctrl Pts',(0.0899695493219107,-0.126897601253898,
-0.414780976780436));
#80337=CARTESIAN_POINT('Ctrl Pts',(0.0910357652332837,-0.126134889160652,
-0.414686704714272));
#80338=CARTESIAN_POINT('Ctrl Pts',(0.0940125791763811,-0.123948036147847,
-0.414419603700523));
#80339=CARTESIAN_POINT('Ctrl Pts',(0.0959001988389162,-0.122493393351473,
-0.414245613055288));
#80340=CARTESIAN_POINT('Ctrl Pts',(0.104141878542834,-0.115834881100149,
-0.41346460617345));
#80341=CARTESIAN_POINT('Ctrl Pts',(0.110110429949034,-0.110176702456328,
-0.412839979123223));
#80342=CARTESIAN_POINT('Ctrl Pts',(0.121804284386646,-0.0971874513485076,
-0.411490932749007));
#80343=CARTESIAN_POINT('Ctrl Pts',(0.127377024367968,-0.0897596194853495,
-0.410766481811189));
#80344=CARTESIAN_POINT('Ctrl Pts',(0.133626246672558,-0.0796656117833917,
-0.409868924107657));
#80345=CARTESIAN_POINT('Ctrl Pts',(0.134941269304232,-0.0774173063837144,
-0.409674157451417));
#80346=CARTESIAN_POINT('Ctrl Pts',(0.136669366128138,-0.0742848156534651,
-0.409410795660582));
#80347=CARTESIAN_POINT('Ctrl Pts',(0.137131435116893,-0.0734283263261997,
-0.409339589299091));
#80348=CARTESIAN_POINT('Ctrl Pts',(0.137888375438125,-0.0719931944092857,
-0.409221675717405));
#80349=CARTESIAN_POINT('Ctrl Pts',(0.13818771070766,-0.0714169503242614,
-0.409174702458611));
#80350=CARTESIAN_POINT('Ctrl Pts',(0.138800005163743,-0.0702199705311602,
-0.409077921025874));
#80351=CARTESIAN_POINT('Ctrl Pts',(0.139112426231255,-0.0695989842828882,
-0.409028145195357));
#80352=CARTESIAN_POINT('Ctrl Pts',(0.13993486665706,-0.0679365892857792,
-0.408895991464965));
#80353=CARTESIAN_POINT('Ctrl Pts',(0.14043743392055,-0.0668915124230873,
-0.40881405257143));
#80354=CARTESIAN_POINT('Ctrl Pts',(0.143025587441762,-0.0613517310240737,
-0.408385173481009));
#80355=CARTESIAN_POINT('Ctrl Pts',(0.144907436430801,-0.0567644205456595,
-0.408048821671189));
#80356=CARTESIAN_POINT('Ctrl Pts',(0.148781770544489,-0.0458640519402042,
-0.407275160728713));
#80357=CARTESIAN_POINT('Ctrl Pts',(0.150596840885279,-0.0394984105807963,
-0.406842326235232));
#80358=CARTESIAN_POINT('Ctrl Pts',(0.153872789005679,-0.0244256797164644,
-0.405824766218257));
#80359=CARTESIAN_POINT('Ctrl Pts',(0.155008993320746,-0.0156726452948194,
-0.405238624081585));
#80360=CARTESIAN_POINT('Ctrl Pts',(0.155486962600614,-0.00486291610375301,
-0.404489776173616));
#80361=CARTESIAN_POINT('Ctrl Pts',(0.155536818973617,-0.0028532078328083,
-0.404349561852821));
#80362=CARTESIAN_POINT('Ctrl Pts',(0.155554402840785,0.000390639397702419,
-0.404121348660314));
#80363=CARTESIAN_POINT('Ctrl Pts',(0.155546410520769,0.00162445670713242,
-0.404034104909804));
#80364=CARTESIAN_POINT('Ctrl Pts',(0.155502817372158,0.00399665008138526,
-0.403865451645369));
#80365=CARTESIAN_POINT('Ctrl Pts',(0.155469389821721,0.005134990243521,
-0.403784115134633));
#80366=CARTESIAN_POINT('Ctrl Pts',(0.155362365034471,0.00778676847194762,
-0.40359364518516));
#80367=CARTESIAN_POINT('Ctrl Pts',(0.155279148357151,0.00929967837408699,
-0.40348421995326));
#80368=CARTESIAN_POINT('Ctrl Pts',(0.154929577813954,0.0143171410907361,
-0.40311867601386));
#80369=CARTESIAN_POINT('Ctrl Pts',(0.154566572808116,0.017813634039671,
-0.402859623878621));
#80370=CARTESIAN_POINT('Ctrl Pts',(0.15337715702905,0.0264201262367326,
-0.402210856217068));
#80371=CARTESIAN_POINT('Ctrl Pts',(0.152413572980783,0.0315066504079926,
-0.401817543260454));
#80372=CARTESIAN_POINT('Ctrl Pts',(0.148794420336471,0.0464842311849151,
-0.400633233020501));
#80373=CARTESIAN_POINT('Ctrl Pts',(0.145414353709923,0.0561714395871313,
-0.399830857396631));
#80374=CARTESIAN_POINT('Ctrl Pts',(0.139905571106592,0.0680469579368619,
-0.398838574306083));
#80375=CARTESIAN_POINT('Ctrl Pts',(0.138632683588476,0.0706040997296308,
-0.398624512466365));
#80376=CARTESIAN_POINT('Ctrl Pts',(0.136816662605184,0.0740136283129232,
-0.398339879864655));
#80377=CARTESIAN_POINT('Ctrl Pts',(0.136334679761057,0.0748977408188562,
-0.398266146777899));
#80378=CARTESIAN_POINT('Ctrl Pts',(0.135553360973311,0.0762983950045594,
-0.398149526203277));
#80379=CARTESIAN_POINT('Ctrl Pts',(0.135259588628421,0.076817982711238,
-0.398106306925722));
#80380=CARTESIAN_POINT('Ctrl Pts',(0.134630163198465,0.0779164254625724,
-0.3980150491823));
#80381=CARTESIAN_POINT('Ctrl Pts',(0.134293750849438,0.0784948324457345,
-0.397967062234209));
#80382=CARTESIAN_POINT('Ctrl Pts',(0.13342544065371,0.0799658292976259,
-0.397845145390837));
#80383=CARTESIAN_POINT('Ctrl Pts',(0.132888301077491,0.0808553131223326,
-0.39777154106279));
#80384=CARTESIAN_POINT('Ctrl Pts',(0.130556589902209,0.0846305307915819,
-0.397459343169993));
#80385=CARTESIAN_POINT('Ctrl Pts',(0.12867648790279,0.087462651802643,-0.397225633072002));
#80386=CARTESIAN_POINT('Ctrl Pts',(0.12277937583617,0.0957435321447507,
-0.396536526870984));
#80387=CARTESIAN_POINT('Ctrl Pts',(0.118497975758745,0.100994265393113,
-0.39609155030182));
#80388=CARTESIAN_POINT('Ctrl Pts',(0.110232646575901,0.109878865735452,
-0.395292274098939));
#80389=CARTESIAN_POINT('Ctrl Pts',(0.10637872970927,0.113613812895561,-0.394939070889565));
#80390=CARTESIAN_POINT('Ctrl Pts',(0.102342226162682,0.117140391172586,
-0.39458065504025));
#80391=CARTESIAN_POINT('Origin',(0.,0.,-1.10400562256037));
#80392=CARTESIAN_POINT('',(0.102342242837719,0.117140376604078,-0.310696206146068));
#80393=CARTESIAN_POINT('',(0.102342232991206,0.117140385206698,-0.324608715049314));
#80394=CARTESIAN_POINT('',(0.10234224283772,0.117140376604078,-1.10400562256037));
#80395=CARTESIAN_POINT('',(-0.155549994568677,-4.11057744446486E-5,-0.355194377443546));
#80396=CARTESIAN_POINT('Ctrl Pts',(-0.155549994568662,-4.11058288203373E-5,
-0.355194377439629));
#80397=CARTESIAN_POINT('Ctrl Pts',(-0.155549396009725,-0.00230613349326641,
-0.355031203712607));
#80398=CARTESIAN_POINT('Ctrl Pts',(-0.155499326836065,-0.00457044143846376,
-0.354868029985585));
#80399=CARTESIAN_POINT('Ctrl Pts',(-0.155399866787252,-0.00683256192830994,
-0.354704856258563));
#80400=CARTESIAN_POINT('Ctrl Pts',(-0.154950294840852,-0.0170576314285913,
-0.353967290462704));
#80401=CARTESIAN_POINT('Ctrl Pts',(-0.153485536234328,-0.0272761366067171,
-0.353229724666845));
#80402=CARTESIAN_POINT('Ctrl Pts',(-0.151018641087833,-0.0372716050631629,
-0.352492158870986));
#80403=CARTESIAN_POINT('Ctrl Pts',(-0.148545881715323,-0.0472908344347134,
-0.351752839756777));
#80404=CARTESIAN_POINT('Ctrl Pts',(-0.145066294261912,-0.0570850296203176,
-0.351013520642569));
#80405=CARTESIAN_POINT('Ctrl Pts',(-0.140645158956177,-0.0664435231018924,
-0.35027420152836));
#80406=CARTESIAN_POINT('Ctrl Pts',(-0.136244576497222,-0.0757585110878595,
-0.349538319339607));
#80407=CARTESIAN_POINT('Ctrl Pts',(-0.130911576344366,-0.0846409946880161,
-0.348802437150854));
#80408=CARTESIAN_POINT('Ctrl Pts',(-0.124758450002192,-0.0929038839502992,
-0.348066554962102));
#80409=CARTESIAN_POINT('Ctrl Pts',(-0.1185622165495,-0.101224660741753,
-0.347325517385165));
#80410=CARTESIAN_POINT('Ctrl Pts',(-0.111534877784764,-0.108916358423386,
-0.346584479808228));
#80411=CARTESIAN_POINT('Ctrl Pts',(-0.103832776624706,-0.115821228617227,
-0.345843442231292));
#80412=CARTESIAN_POINT('Ctrl Pts',(-0.0961306754646478,-0.122726098811068,
-0.345102404654355));
#80413=CARTESIAN_POINT('Ctrl Pts',(-0.0877546006943488,-0.128843607569754,
-0.344361367077418));
#80414=CARTESIAN_POINT('Ctrl Pts',(-0.0788922047367165,-0.134059026297299,
-0.343620329500482));
#80415=CARTESIAN_POINT('Ctrl Pts',(-0.0700713293439948,-0.139250010646957,
-0.342882763704648));
#80416=CARTESIAN_POINT('Ctrl Pts',(-0.0607031405623345,-0.143585954003829,
-0.342145197908815));
#80417=CARTESIAN_POINT('Ctrl Pts',(-0.0509763064828735,-0.146959922010609,
-0.341407632112981));
#80418=CARTESIAN_POINT('Ctrl Pts',(-0.0412263500771315,-0.150341910508792,
-0.340668312998766));
#80419=CARTESIAN_POINT('Ctrl Pts',(-0.0311168689297538,-0.152756901008259,
-0.339928993884551));
#80420=CARTESIAN_POINT('Ctrl Pts',(-0.0208601042734006,-0.154144927096881,
-0.339189674770336));
#80421=CARTESIAN_POINT('Ctrl Pts',(-0.0106510209703367,-0.155526500569642,
-0.33845379258161));
#80422=CARTESIAN_POINT('Ctrl Pts',(-0.00029694429549402,-0.155890508456486,
-0.337717910392884));
#80423=CARTESIAN_POINT('Ctrl Pts',(0.00998405975226561,-0.155229253205906,
-0.336982028204158));
#80424=CARTESIAN_POINT('Ctrl Pts',(0.0203370896869163,-0.154563365382897,
-0.336240990627199));
#80425=CARTESIAN_POINT('Ctrl Pts',(0.0306150705144891,-0.152857840989834,
-0.335499953050239));
#80426=CARTESIAN_POINT('Ctrl Pts',(0.0406005577015138,-0.150157907598388,
-0.33475891547328));
#80427=CARTESIAN_POINT('Ctrl Pts',(0.0505860448885384,-0.147457974206942,
-0.334017877896321));
#80428=CARTESIAN_POINT('Ctrl Pts',(0.060278161065648,-0.143764002633356,
-0.333276840319362));
#80429=CARTESIAN_POINT('Ctrl Pts',(0.0694784940677451,-0.139170907024702,
-0.332535802742402));
#80430=CARTESIAN_POINT('Ctrl Pts',(0.0786357232622493,-0.134599330192524,
-0.331798236946424));
#80431=CARTESIAN_POINT('Ctrl Pts',(0.087373843924104,-0.129103093918329,
-0.331060671150446));
#80432=CARTESIAN_POINT('Ctrl Pts',(0.0955004280601591,-0.122782208565925,
-0.330323105354468));
#80433=CARTESIAN_POINT('Ctrl Pts',(0.103646330456298,-0.116446297403765,
-0.329583786240289));
#80434=CARTESIAN_POINT('Ctrl Pts',(0.111176962586784,-0.109282264469586,
-0.32884446712611));
#80435=CARTESIAN_POINT('Ctrl Pts',(0.117926453096682,-0.101435467958875,
-0.328105148011931));
#80436=CARTESIAN_POINT('Ctrl Pts',(0.124644566770364,-0.0936251494087723,
-0.327369265823062));
#80437=CARTESIAN_POINT('Ctrl Pts',(0.130588174796864,-0.0851391062085926,
-0.326633383634192));
#80438=CARTESIAN_POINT('Ctrl Pts',(0.135632073353664,-0.076156044919535,
-0.325897501445322));
#80439=CARTESIAN_POINT('Ctrl Pts',(0.140711308074736,-0.0671100507768938,
-0.325156463868489));
#80440=CARTESIAN_POINT('Ctrl Pts',(0.144877701622766,-0.0575608692355155,
-0.324415426291655));
#80441=CARTESIAN_POINT('Ctrl Pts',(0.148050778424439,-0.0477155059484613,
-0.323674388714822));
#80442=CARTESIAN_POINT('Ctrl Pts',(0.151223855226112,-0.0378701426614064,
-0.322933351137988));
#80443=CARTESIAN_POINT('Ctrl Pts',(0.153403448524948,-0.0277295354314074,
-0.322192313561155));
#80444=CARTESIAN_POINT('Ctrl Pts',(0.154561120375391,-0.0175117836985256,
-0.321451275984322));
#80445=CARTESIAN_POINT('Ctrl Pts',(0.155713378648865,-0.0073418128505561,
-0.320713703693404));
#80446=CARTESIAN_POINT('Ctrl Pts',(0.155861855353249,0.00298016479531421,
-0.319976131402487));
#80447=CARTESIAN_POINT('Ctrl Pts',(0.154985645239039,0.0132382880252213,
-0.31923855911157));
#80448=CARTESIAN_POINT('Ctrl Pts',(0.154110671345499,0.0234819383521538,
-0.318502027441043));
#80449=CARTESIAN_POINT('Ctrl Pts',(0.152213864886687,0.0336609894596978,
-0.317765495770516));
#80450=CARTESIAN_POINT('Ctrl Pts',(0.149326363322342,0.0435596110740663,
-0.31702896409999));
#80451=CARTESIAN_POINT('Ctrl Pts',(0.146441745391506,0.0534483473268699,
-0.316293167974486));
#80452=CARTESIAN_POINT('Ctrl Pts',(0.142568636922808,0.0630563155655001,
-0.315557371848983));
#80453=CARTESIAN_POINT('Ctrl Pts',(0.137788530039798,0.0721811851487048,
-0.31482157572348));
#80454=CARTESIAN_POINT('Ctrl Pts',(0.132997950743386,0.0813260457925393,
-0.314084167591929));
#80455=CARTESIAN_POINT('Ctrl Pts',(0.127296846994873,0.0899848734962369,
-0.313346759460377));
#80456=CARTESIAN_POINT('Ctrl Pts',(0.120812856293013,0.0979798767825501,
-0.312609351328826));
#80457=CARTESIAN_POINT('Ctrl Pts',(0.115205461488811,0.104894004508611,
-0.311971636267907));
#80458=CARTESIAN_POINT('Ctrl Pts',(0.109013547816566,0.11131184562285,-0.311333921206987));
#80459=CARTESIAN_POINT('Ctrl Pts',(0.102342242837719,0.117140376604078,
-0.310696206146068));
#80460=CARTESIAN_POINT('Ctrl Pts',(0.102342242837719,0.117140376604078,
-0.380699116973164));
#80461=CARTESIAN_POINT('Ctrl Pts',(0.0945698035973211,0.123930937529717,
-0.379961512873473));
#80462=CARTESIAN_POINT('Ctrl Pts',(0.0861280069020955,0.129936518309589,
-0.379223908773781));
#80463=CARTESIAN_POINT('Ctrl Pts',(0.0772013106887236,0.1350398464452,-0.378486304674089));
#80464=CARTESIAN_POINT('Ctrl Pts',(0.0706967556260747,0.138758453874802,
-0.377948839707633));
#80465=CARTESIAN_POINT('Ctrl Pts',(0.0639354807636149,0.141998879591595,
-0.377411374741178));
#80466=CARTESIAN_POINT('Ctrl Pts',(0.0569959733123979,0.144731688051278,
-0.376873909774722));
#80467=CARTESIAN_POINT('Ctrl Pts',(0.0474728533778924,0.148481934434403,
-0.376136343978859));
#80468=CARTESIAN_POINT('Ctrl Pts',(0.0375426173799939,0.151302178905618,
-0.375398778182996));
#80469=CARTESIAN_POINT('Ctrl Pts',(0.0274083143440573,0.153116252582204,
-0.374661212387134));
#80470=CARTESIAN_POINT('Ctrl Pts',(0.0172499203598626,0.154934638618005,
-0.373921893272926));
#80471=CARTESIAN_POINT('Ctrl Pts',(0.00688737479814154,0.15574175549937,
-0.373182574158718));
#80472=CARTESIAN_POINT('Ctrl Pts',(-0.0034603217118658,0.155511506563503,
-0.372443255044511));
#80473=CARTESIAN_POINT('Ctrl Pts',(-0.013759914147707,0.155282328002272,
-0.371707372855755));
#80474=CARTESIAN_POINT('Ctrl Pts',(-0.024043862791822,0.154025424734984,
-0.370971490666999));
#80475=CARTESIAN_POINT('Ctrl Pts',(-0.0340955737290129,0.151767237413381,
-0.370235608478243));
#80476=CARTESIAN_POINT('Ctrl Pts',(-0.0442177041878638,0.149493229852616,
-0.36949457090131));
#80477=CARTESIAN_POINT('Ctrl Pts',(-0.0541034007564343,0.146204049606232,
-0.368753533324376));
#80478=CARTESIAN_POINT('Ctrl Pts',(-0.0635449458789444,0.141978316489674,
-0.368012495747443));
#80479=CARTESIAN_POINT('Ctrl Pts',(-0.0729864910014544,0.137752583373116,
-0.367271458170509));
#80480=CARTESIAN_POINT('Ctrl Pts',(-0.0819830759570848,0.132590800628203,
-0.366530420593576));
#80481=CARTESIAN_POINT('Ctrl Pts',(-0.0903535391157341,0.126617694139727,
-0.365789383016643));
#80482=CARTESIAN_POINT('Ctrl Pts',(-0.0986278299880834,0.120713215551097,
-0.365056859577655));
#80483=CARTESIAN_POINT('Ctrl Pts',(-0.106353689299282,0.113970697276645,
-0.364324336138668));
#80484=CARTESIAN_POINT('Ctrl Pts',(-0.113357974871389,0.106516534083012,
-0.363591812699681));
#80485=CARTESIAN_POINT('Ctrl Pts',(-0.120352862561989,0.0990723723865641,
-0.362860272111609));
#80486=CARTESIAN_POINT('Ctrl Pts',(-0.126627387258907,0.090919072982288,
-0.362128731523536));
#80487=CARTESIAN_POINT('Ctrl Pts',(-0.132043043414792,0.0822218777805478,
-0.361397190935464));
#80488=CARTESIAN_POINT('Ctrl Pts',(-0.137453576521634,0.0735329098658196,
-0.360666342362948));
#80489=CARTESIAN_POINT('Ctrl Pts',(-0.14200634180813,0.0643018565896784,
-0.359935493790432));
#80490=CARTESIAN_POINT('Ctrl Pts',(-0.145606530111015,0.0547223984217612,
-0.359204645217917));
#80491=CARTESIAN_POINT('Ctrl Pts',(-0.149215067776358,0.0451207240913367,
-0.358472101700825));
#80492=CARTESIAN_POINT('Ctrl Pts',(-0.151866301606515,0.0351699238834797,
-0.357739558183735));
#80493=CARTESIAN_POINT('Ctrl Pts',(-0.153514574585645,0.0250814251945219,
-0.357007014666644));
#80494=CARTESIAN_POINT('Ctrl Pts',(-0.154874093797856,0.0167602866673107,
-0.356402802258944));
#80495=CARTESIAN_POINT('Ctrl Pts',(-0.155552210956479,0.00834601538551534,
-0.355798589851245));
#80496=CARTESIAN_POINT('Ctrl Pts',(-0.155549994568677,-4.11057744457694E-5,
-0.355194377443546));
#80497=CARTESIAN_POINT('',(-0.155549931546106,-0.000109021168048467,-0.369108945921202));
#80498=CARTESIAN_POINT('Ctrl Pts',(0.102342226162682,0.117140391172586,
-0.39458065504025));
#80499=CARTESIAN_POINT('Ctrl Pts',(0.0990436577238993,0.120022256546226,
-0.394287763136437));
#80500=CARTESIAN_POINT('Ctrl Pts',(0.0956231589673669,0.122764977425907,
-0.393991420093704));
#80501=CARTESIAN_POINT('Ctrl Pts',(0.0903485245596155,0.126639696980803,
-0.393540936964394));
#80502=CARTESIAN_POINT('Ctrl Pts',(0.0885812435961712,0.12788209903274,
-0.393391038034195));
#80503=CARTESIAN_POINT('Ctrl Pts',(0.0856385464428394,0.129860551344907,
-0.393142714453109));
#80504=CARTESIAN_POINT('Ctrl Pts',(0.0844781070580761,0.130618423819413,
-0.393045105112036));
#80505=CARTESIAN_POINT('Ctrl Pts',(0.0823574844704538,0.131963303171459,
-0.392867204059805));
#80506=CARTESIAN_POINT('Ctrl Pts',(0.0814007533674989,0.132555595364566,
-0.39278711387893));
#80507=CARTESIAN_POINT('Ctrl Pts',(0.0793171639663523,0.133814438430755,
-0.392613009675623));
#80508=CARTESIAN_POINT('Ctrl Pts',(0.078188155400012,0.134477241918941,
-0.392518867438061));
#80509=CARTESIAN_POINT('Ctrl Pts',(0.07498842592508,0.136301781505302,-0.392252530350849));
#80510=CARTESIAN_POINT('Ctrl Pts',(0.0728993597881388,0.137430425535494,
-0.392079184460036));
#80511=CARTESIAN_POINT('Ctrl Pts',(0.0635335214936542,0.142216800621858,
-0.391303966956571));
#80512=CARTESIAN_POINT('Ctrl Pts',(0.0560029286093983,0.145347038301092,
-0.390684794156728));
#80513=CARTESIAN_POINT('Ctrl Pts',(0.0395855453188601,0.15070536664108,
-0.389352105625249));
#80514=CARTESIAN_POINT('Ctrl Pts',(0.0306754390533624,0.152768287796585,
-0.388638622687398));
#80515=CARTESIAN_POINT('Ctrl Pts',(0.0188869811684354,0.154424054806561,
-0.387737018241808));
#80516=CARTESIAN_POINT('Ctrl Pts',(0.0161282484375128,0.154736513865307,
-0.387529097745903));
#80517=CARTESIAN_POINT('Ctrl Pts',(0.012369643410878,0.155060592593653,
-0.38725120623545));
#80518=CARTESIAN_POINT('Ctrl Pts',(0.0113760217546522,0.155136654989613,
-0.387178253388668));
#80519=CARTESIAN_POINT('Ctrl Pts',(0.00978805789541216,0.155242875568239,
-0.387062548268217));
#80520=CARTESIAN_POINT('Ctrl Pts',(0.00919417575328183,0.155279179725827,
-0.387019473160543));
#80521=CARTESIAN_POINT('Ctrl Pts',(0.00792951129614141,0.155349207917511,
-0.386928185776871));
#80522=CARTESIAN_POINT('Ctrl Pts',(0.00725868685187888,0.155381997211835,
-0.386880027570973));
#80523=CARTESIAN_POINT('Ctrl Pts',(0.00553778242150198,0.155454944210573,
-0.386757112616538));
#80524=CARTESIAN_POINT('Ctrl Pts',(0.00448744754675826,0.155488808882294,
-0.38668269210849));
#80525=CARTESIAN_POINT('Ctrl Pts',(-8.07190659825778E-5,0.155589765267076,
-0.386361306897857));
#80526=CARTESIAN_POINT('Ctrl Pts',(-0.00360020104933071,0.155548142426236,
-0.386119590138954));
#80527=CARTESIAN_POINT('Ctrl Pts',(-0.0143271742175793,0.15505692897941,
-0.385392607819279));
#80528=CARTESIAN_POINT('Ctrl Pts',(-0.0215075612017889,0.154225024524725,
-0.384919135256757));
#80529=CARTESIAN_POINT('Ctrl Pts',(-0.0375912449433175,0.15121602819075,
-0.383841136058655));
#80530=CARTESIAN_POINT('Ctrl Pts',(-0.0464111308382953,0.148745987082825,
-0.383236715655148));
#80531=CARTESIAN_POINT('Ctrl Pts',(-0.0569893384070287,0.144750515467279,
-0.382458484074722));
#80532=CARTESIAN_POINT('Ctrl Pts',(-0.0589998242090271,0.14394275384838,
-0.382308152321243));
#80533=CARTESIAN_POINT('Ctrl Pts',(-0.0622693977844241,0.142549116734279,
-0.382059262538946));
#80534=CARTESIAN_POINT('Ctrl Pts',(-0.0635387135022984,0.141987887682433,
-0.38196152639137));
#80535=CARTESIAN_POINT('Ctrl Pts',(-0.0658233426026664,0.140940967878594,
-0.381783492496763));
#80536=CARTESIAN_POINT('Ctrl Pts',(-0.0668412282902948,0.14046109403529,
-0.381703397751886));
#80537=CARTESIAN_POINT('Ctrl Pts',(-0.0690305245835815,0.139399782213281,
-0.381529396467118));
#80538=CARTESIAN_POINT('Ctrl Pts',(-0.0701999806319685,0.138814535017395,
-0.381435362918814));
#80539=CARTESIAN_POINT('Ctrl Pts',(-0.0734651460869936,0.137128690553749,
-0.381169664662358));
#80540=CARTESIAN_POINT('Ctrl Pts',(-0.0755432311339703,0.135994943136918,
-0.380996857790056));
#80541=CARTESIAN_POINT('Ctrl Pts',(-0.0846034272654175,0.130780200743782,
-0.38022645054959));
#80542=CARTESIAN_POINT('Ctrl Pts',(-0.0912859822725921,0.126206314224676,
-0.379611803845602));
#80543=CARTESIAN_POINT('Ctrl Pts',(-0.104600923792216,0.115480243469031,
-0.378292636901898));
#80544=CARTESIAN_POINT('Ctrl Pts',(-0.11111530560378,0.109226538509883,
-0.377588205168478));
#80545=CARTESIAN_POINT('Ctrl Pts',(-0.118974670922404,0.100246478885924,
-0.376683087222946));
#80546=CARTESIAN_POINT('Ctrl Pts',(-0.120835654242549,0.0979952867029918,
-0.376464083483152));
#80547=CARTESIAN_POINT('Ctrl Pts',(-0.123256753588523,0.0948926001915009,
-0.3761740456901));
#80548=CARTESIAN_POINT('Ctrl Pts',(-0.123873391639172,0.0940862150702452,
-0.376099700640623));
#80549=CARTESIAN_POINT('Ctrl Pts',(-0.124840921635155,0.0927949612724498,
-0.375982360741999));
#80550=CARTESIAN_POINT('Ctrl Pts',(-0.125196972401435,0.092314022154407,
-0.375939027030337));
#80551=CARTESIAN_POINT('Ctrl Pts',(-0.125944168409434,0.0912924650202418,
-0.375847783525183));
#80552=CARTESIAN_POINT('Ctrl Pts',(-0.126334628020549,0.0907513610036011,
-0.375799923285292));
#80553=CARTESIAN_POINT('Ctrl Pts',(-0.127319037323205,0.0893684873260986,
-0.375678752510074));
#80554=CARTESIAN_POINT('Ctrl Pts',(-0.127908142124847,0.0885232801066856,
-0.375605759611428));
#80555=CARTESIAN_POINT('Ctrl Pts',(-0.13035514298136,0.0849370568688732,
-0.375300222864133));
#80556=CARTESIAN_POINT('Ctrl Pts',(-0.132133810621604,0.0821427223688853,
-0.375072307040431));
#80557=CARTESIAN_POINT('Ctrl Pts',(-0.139060122653014,0.0704533237310836,
-0.37415043720196));
#80558=CARTESIAN_POINT('Ctrl Pts',(-0.143409704206191,0.0611152806725299,
-0.373485179801227));
#80559=CARTESIAN_POINT('Ctrl Pts',(-0.149188600306762,0.0446149124210833,
-0.372326264867267));
#80560=CARTESIAN_POINT('Ctrl Pts',(-0.151094752297982,0.0376574724873536,
-0.371842494210479));
#80561=CARTESIAN_POINT('Ctrl Pts',(-0.152891690232485,0.0286995658878011,
-0.371209412667761));
#80562=CARTESIAN_POINT('Ctrl Pts',(-0.153236290544166,0.0267987446228151,
-0.371074544120154));
#80563=CARTESIAN_POINT('Ctrl Pts',(-0.1537402154161,0.0236903111726044,
-0.370852865714455));
#80564=CARTESIAN_POINT('Ctrl Pts',(-0.153920918368918,0.0224863384572335,
-0.370766731333539));
#80565=CARTESIAN_POINT('Ctrl Pts',(-0.154235002444943,0.0202121132415971,
-0.370603454356239));
#80566=CARTESIAN_POINT('Ctrl Pts',(-0.154371421961385,0.0191423476949558,
-0.37052641230921));
#80567=CARTESIAN_POINT('Ctrl Pts',(-0.154626313842322,0.0169632011293798,
-0.370368952586842));
#80568=CARTESIAN_POINT('Ctrl Pts',(-0.154743995850993,0.0158537930265916,
-0.370288514897042));
#80569=CARTESIAN_POINT('Ctrl Pts',(-0.155045129489924,0.0126909564207269,
-0.370058366089622));
#80570=CARTESIAN_POINT('Ctrl Pts',(-0.155199699647872,0.0106350850549925,
-0.369907773453013));
#80571=CARTESIAN_POINT('Ctrl Pts',(-0.155473109177032,0.00568405776425027,
-0.369542574006086));
#80572=CARTESIAN_POINT('Ctrl Pts',(-0.155551995357722,0.00278758824431477,
-0.369326834733086));
#80573=CARTESIAN_POINT('Ctrl Pts',(-0.155549961666794,-0.000109203749030585,
-0.369108984688673));
#80574=CARTESIAN_POINT('Ctrl Pts',(-0.155549961792102,-0.00010902511433882,
-0.369108998122695));
#80575=CARTESIAN_POINT('Ctrl Pts',(-0.155542653148416,-0.0105365238885239,
-0.368324809893432));
#80576=CARTESIAN_POINT('Ctrl Pts',(-0.15448680998581,-0.0209362629403968,
-0.367513221839129));
#80577=CARTESIAN_POINT('Ctrl Pts',(-0.151223083365885,-0.0369033025256532,
-0.366253479600695));
#80578=CARTESIAN_POINT('Ctrl Pts',(-0.149722407424921,-0.0425850820425572,
-0.365803003141355));
#80579=CARTESIAN_POINT('Ctrl Pts',(-0.147434623044069,-0.0496097853025308,
-0.365252855596421));
#80580=CARTESIAN_POINT('Ctrl Pts',(-0.146944304424871,-0.0510438117500759,
-0.365140926057862));
#80581=CARTESIAN_POINT('Ctrl Pts',(-0.146173516486474,-0.0531949029040052,
-0.364973830280732));
#80582=CARTESIAN_POINT('Ctrl Pts',(-0.145908570677525,-0.0539173783381018,
-0.364917846756262));
#80583=CARTESIAN_POINT('Ctrl Pts',(-0.145414988546055,-0.055233030569196,
-0.364816189164675));
#80584=CARTESIAN_POINT('Ctrl Pts',(-0.145188069653475,-0.0558267948138428,
-0.364770423047617));
#80585=CARTESIAN_POINT('Ctrl Pts',(-0.144661198834578,-0.0571804810871024,
-0.364666328478205));
#80586=CARTESIAN_POINT('Ctrl Pts',(-0.144358892602902,-0.0579394517623867,
-0.364608138578518));
#80587=CARTESIAN_POINT('Ctrl Pts',(-0.14336612934982,-0.0603758713943324,
-0.364421787290871));
#80588=CARTESIAN_POINT('Ctrl Pts',(-0.142652276322684,-0.0620437078753656,
-0.36429490905641));
#80589=CARTESIAN_POINT('Ctrl Pts',(-0.137233938959937,-0.0741147869673015,
-0.36337894392607));
#80590=CARTESIAN_POINT('Ctrl Pts',(-0.131425327857237,-0.0839857652447746,
-0.362640696120224));
#80591=CARTESIAN_POINT('Ctrl Pts',(-0.121383113407584,-0.0974196486601801,
-0.361531852553697));
#80592=CARTESIAN_POINT('Ctrl Pts',(-0.117959703263889,-0.101537924356356,
-0.361175471631034));
#80593=CARTESIAN_POINT('Ctrl Pts',(-0.112656087883774,-0.10728704729976,
-0.360644251882682));
#80594=CARTESIAN_POINT('Ctrl Pts',(-0.11093818388441,-0.109062472791636,
-0.36047508461122));
#80595=CARTESIAN_POINT('Ctrl Pts',(-0.107749454920902,-0.112204653810063,
-0.360165417271889));
#80596=CARTESIAN_POINT('Ctrl Pts',(-0.10629304237743,-0.113585289009196,
-0.360025524307564));
#80597=CARTESIAN_POINT('Ctrl Pts',(-0.10475027792264,-0.114992123175167,
-0.359878721077568));
#80598=CARTESIAN_POINT('Ctrl Pts',(-0.104690127592689,-0.115046887405898,
-0.359872999568864));
#80599=CARTESIAN_POINT('Ctrl Pts',(-0.104571434833511,-0.115154781780456,
-0.35986171371752));
#80600=CARTESIAN_POINT('Ctrl Pts',(-0.104512894798335,-0.115207914532271,
-0.359856149483805));
#80601=CARTESIAN_POINT('Ctrl Pts',(-0.104396606719464,-0.115313299625932,
-0.359845100284993));
#80602=CARTESIAN_POINT('Ctrl Pts',(-0.104338859887233,-0.115365553275455,
-0.359839615375602));
#80603=CARTESIAN_POINT('Ctrl Pts',(-0.104223327877295,-0.115469937572198,
-0.359828645790369));
#80604=CARTESIAN_POINT('Ctrl Pts',(-0.10416554277042,-0.115522068264251,
-0.359823161118577));
#80605=CARTESIAN_POINT('Ctrl Pts',(-0.104049041172718,-0.115627011410977,
-0.359812107249289));
#80606=CARTESIAN_POINT('Ctrl Pts',(-0.103990323539663,-0.115679822557228,
-0.359806538000588));
#80607=CARTESIAN_POINT('Ctrl Pts',(-0.103870938541682,-0.115787034103212,
-0.359795218576086));
#80608=CARTESIAN_POINT('Ctrl Pts',(-0.103810268603674,-0.11584143158791,
-0.359789468283536));
#80609=CARTESIAN_POINT('Ctrl Pts',(-0.103685746681135,-0.11595290323976,
-0.359777670377251));
#80610=CARTESIAN_POINT('Ctrl Pts',(-0.103621890260409,-0.116009972387555,
-0.359771622561006));
#80611=CARTESIAN_POINT('Ctrl Pts',(-0.103489413391929,-0.116128171696093,
-0.359759080469007));
#80612=CARTESIAN_POINT('Ctrl Pts',(-0.103420785852836,-0.116189293823484,
-0.359752585868001));
#80613=CARTESIAN_POINT('Ctrl Pts',(-0.103276611891727,-0.11631747134407,
-0.359738947381961));
#80614=CARTESIAN_POINT('Ctrl Pts',(-0.103201054265141,-0.116384514013635,
-0.359731802980783));
#80615=CARTESIAN_POINT('Ctrl Pts',(-0.103082980207387,-0.116489076341719,
-0.359720643304648));
#80616=CARTESIAN_POINT('Ctrl Pts',(-0.103040508365672,-0.116526646528217,
-0.359716630099068));
#80617=CARTESIAN_POINT('Ctrl Pts',(-0.102887193138994,-0.116662118354606,
-0.359702146741765));
#80618=CARTESIAN_POINT('Ctrl Pts',(-0.102776230987178,-0.116759884869776,
-0.359691671072001));
#80619=CARTESIAN_POINT('Ctrl Pts',(-0.101872250324765,-0.117554076923857,
-0.359606382287122));
#80620=CARTESIAN_POINT('Ctrl Pts',(-0.101072320041888,-0.118242557521096,
-0.35953124684217));
#80621=CARTESIAN_POINT('Ctrl Pts',(-0.0992683042712271,-0.119763547879234,
-0.359362503688229));
#80622=CARTESIAN_POINT('Ctrl Pts',(-0.0982606396411751,-0.120591666958241,
-0.35926872546181));
#80623=CARTESIAN_POINT('Ctrl Pts',(-0.0954584838310542,-0.122836094655481,
-0.359009163135727));
#80624=CARTESIAN_POINT('Ctrl Pts',(-0.0936430651259912,-0.124225615786324,
-0.358842345334207));
#80625=CARTESIAN_POINT('Ctrl Pts',(-0.0825803194243243,-0.132312726648769,
-0.357833172999869));
#80626=CARTESIAN_POINT('Ctrl Pts',(-0.0726506007022807,-0.138014361313446,
-0.356953777414982));
#80627=CARTESIAN_POINT('Ctrl Pts',(-0.0570041682774519,-0.144838952004175,
-0.355630933133603));
#80628=CARTESIAN_POINT('Ctrl Pts',(-0.0516997333702246,-0.146816013035286,
-0.355193016087507));
#80629=CARTESIAN_POINT('Ctrl Pts',(-0.0433711088026882,-0.149412704096979,
-0.354530721261272));
#80630=CARTESIAN_POINT('Ctrl Pts',(-0.0404164722410028,-0.150238880127184,
-0.354300543782726));
#80631=CARTESIAN_POINT('Ctrl Pts',(-0.0364647364669028,-0.151218825785667,
-0.354000578153947));
#80632=CARTESIAN_POINT('Ctrl Pts',(-0.0354880160944418,-0.151451018923379,
-0.353927070777786));
#80633=CARTESIAN_POINT('Ctrl Pts',(-0.0338637287992436,-0.151820579674609,
-0.353805950541589));
#80634=CARTESIAN_POINT('Ctrl Pts',(-0.0332174232508073,-0.151963296206719,
-0.353758050249479));
#80635=CARTESIAN_POINT('Ctrl Pts',(-0.0319802285685722,-0.152228221795555,
-0.353666941481153));
#80636=CARTESIAN_POINT('Ctrl Pts',(-0.0313895104195222,-0.15235112470573,
-0.353623692283379));
#80637=CARTESIAN_POINT('Ctrl Pts',(-0.029777191571018,-0.15267680274454,
-0.353506295921824));
#80638=CARTESIAN_POINT('Ctrl Pts',(-0.0287542224859087,-0.152872764346402,
-0.353432519753503));
#80639=CARTESIAN_POINT('Ctrl Pts',(-0.0246413713855004,-0.153617882264129,
-0.353138455034306));
#80640=CARTESIAN_POINT('Ctrl Pts',(-0.0215369327324756,-0.154083791293826,
-0.352922250454496));
#80641=CARTESIAN_POINT('Ctrl Pts',(-0.00963984795243291,-0.155502630997381,
-0.352108250244894));
#80642=CARTESIAN_POINT('Ctrl Pts',(-0.000785440330262356,-0.155799239028749,
-0.35153184413112));
#80643=CARTESIAN_POINT('Ctrl Pts',(0.0160374348858264,-0.154927806413076,
-0.350420169597972));
#80644=CARTESIAN_POINT('Ctrl Pts',(0.0239833473702748,-0.153898023917492,
-0.349887855353378));
#80645=CARTESIAN_POINT('Ctrl Pts',(0.0341206325625117,-0.151779895178607,
-0.349174649464466));
#80646=CARTESIAN_POINT('Ctrl Pts',(0.0364156590466672,-0.151245670729985,
-0.349010932925888));
#80647=CARTESIAN_POINT('Ctrl Pts',(0.0399620276865986,-0.150334770387596,
-0.34875395148283));
#80648=CARTESIAN_POINT('Ctrl Pts',(0.0412223140658205,-0.149994091493247,
-0.348661833671514));
#80649=CARTESIAN_POINT('Ctrl Pts',(0.0435608363179875,-0.149330247297556,
-0.348489344454473));
#80650=CARTESIAN_POINT('Ctrl Pts',(0.044640148570971,-0.149011161436979,
-0.348409109608831));
#80651=CARTESIAN_POINT('Ctrl Pts',(0.047045129668025,-0.148271683854432,
-0.348228875568988));
#80652=CARTESIAN_POINT('Ctrl Pts',(0.0483687993967947,-0.147845173988204,
-0.348128682903362));
#80653=CARTESIAN_POINT('Ctrl Pts',(0.05174884891782,-0.146705812922677,
-0.347870193709787));
#80654=CARTESIAN_POINT('Ctrl Pts',(0.0537962463238277,-0.145967468676788,
-0.347711080932915));
#80655=CARTESIAN_POINT('Ctrl Pts',(0.0640313780522109,-0.142031835015903,
-0.346902426588634));
#80656=CARTESIAN_POINT('Ctrl Pts',(0.0719519185206624,-0.138188043754406,
-0.346232137904868));
#80657=CARTESIAN_POINT('Ctrl Pts',(0.0859306156531535,-0.129875442579227,
-0.344974849207563));
#80658=CARTESIAN_POINT('Ctrl Pts',(0.092073040237872,-0.12559563029979,
-0.34439227034945));
#80659=CARTESIAN_POINT('Ctrl Pts',(0.0997699866967528,-0.119363483845766,
-0.343637142450146));
#80660=CARTESIAN_POINT('Ctrl Pts',(0.101620112134122,-0.117792383723186,
-0.343453577881046));
#80661=CARTESIAN_POINT('Ctrl Pts',(0.104726399546585,-0.115026881370939,
-0.343142781308017));
#80662=CARTESIAN_POINT('Ctrl Pts',(0.106000731012999,-0.113853624795944,
-0.343014492457252));
#80663=CARTESIAN_POINT('Ctrl Pts',(0.10784252430731,-0.112100177971014,
-0.342828235387536));
#80664=CARTESIAN_POINT('Ctrl Pts',(0.108425418402785,-0.111536490315506,
-0.34276916107942));
#80665=CARTESIAN_POINT('Ctrl Pts',(0.109456684545443,-0.110523479636222,
-0.34266445984756));
#80666=CARTESIAN_POINT('Ctrl Pts',(0.109906745022687,-0.110075940991269,
-0.342618705431));
#80667=CARTESIAN_POINT('Ctrl Pts',(0.110908166404592,-0.109067865296914,
-0.342516758740405));
#80668=CARTESIAN_POINT('Ctrl Pts',(0.111458031290368,-0.108505888997843,
-0.342460679630619));
#80669=CARTESIAN_POINT('Ctrl Pts',(0.113114534367614,-0.106787019441468,
-0.342291333584569));
#80670=CARTESIAN_POINT('Ctrl Pts',(0.114207636129837,-0.105617147165904,
-0.342179028347387));
#80671=CARTESIAN_POINT('Ctrl Pts',(0.12009771164027,-0.0991149995571928,
-0.341569373443823));
#80672=CARTESIAN_POINT('Ctrl Pts',(0.124540094552274,-0.0934720997648663,
-0.341092545368906));
#80673=CARTESIAN_POINT('Ctrl Pts',(0.132051587551712,-0.0824395851387343,
-0.340211365473669));
#80674=CARTESIAN_POINT('Ctrl Pts',(0.135218759772714,-0.0771348982962128,
-0.339806971979551));
#80675=CARTESIAN_POINT('Ctrl Pts',(0.140088132991576,-0.067752906633184,
-0.339104154631879));
#80676=CARTESIAN_POINT('Ctrl Pts',(0.141947379860386,-0.0637658085816957,
-0.338809087848357));
#80677=CARTESIAN_POINT('Ctrl Pts',(0.144840508881559,-0.0568057317678934,
-0.338294816194288));
#80678=CARTESIAN_POINT('Ctrl Pts',(0.145957712059494,-0.0538702904695179,
-0.338078175521387));
#80679=CARTESIAN_POINT('Ctrl Pts',(0.147460838479355,-0.0495299469889708,
-0.337757032366953));
#80680=CARTESIAN_POINT('Ctrl Pts',(0.147917137293856,-0.0481501274878945,
-0.337654824280176));
#80681=CARTESIAN_POINT('Ctrl Pts',(0.148694010371156,-0.0456855851358198,
-0.337471954782896));
#80682=CARTESIAN_POINT('Ctrl Pts',(0.149022217171528,-0.0446033639563307,
-0.337391548169827));
#80683=CARTESIAN_POINT('Ctrl Pts',(0.14969226569751,-0.0423039746789782,
-0.337220435732902));
#80684=CARTESIAN_POINT('Ctrl Pts',(0.150031125278164,-0.0410860311691848,
-0.337129639994901));
#80685=CARTESIAN_POINT('Ctrl Pts',(0.150907518066628,-0.0377805498923967,
-0.336882717647996));
#80686=CARTESIAN_POINT('Ctrl Pts',(0.151416546195022,-0.0356858184531165,
-0.336725696019932));
#80687=CARTESIAN_POINT('Ctrl Pts',(0.154623214881198,-0.0211826545236121,
-0.335634251274153));
#80688=CARTESIAN_POINT('Ctrl Pts',(0.15583553642611,-0.00849719880153343,
-0.334652288712062));
#80689=CARTESIAN_POINT('Ctrl Pts',(0.15531397539444,0.0108523768537028,
-0.33315343211067));
#80690=CARTESIAN_POINT('Ctrl Pts',(0.154706565903961,0.0174957403968025,
-0.33263991250157));
#80691=CARTESIAN_POINT('Ctrl Pts',(0.153426806796225,0.025662887203259,
-0.332023414601149));
#80692=CARTESIAN_POINT('Ctrl Pts',(0.153154362516311,0.027241706852262,
-0.331904950436275));
#80693=CARTESIAN_POINT('Ctrl Pts',(0.152711876709184,0.0295889109378865,
-0.331730165861789));
#80694=CARTESIAN_POINT('Ctrl Pts',(0.152560329467402,0.0303606140017147,
-0.331672917317838));
#80695=CARTESIAN_POINT('Ctrl Pts',(0.152288559736134,0.0316910658216855,
-0.331574630145222));
#80696=CARTESIAN_POINT('Ctrl Pts',(0.152171104159477,0.0322503359465934,
-0.331533442670949));
#80697=CARTESIAN_POINT('Ctrl Pts',(0.151886605889724,0.0335688202852624,
-0.331436644139672));
#80698=CARTESIAN_POINT('Ctrl Pts',(0.151716951205872,0.0343274457151024,
-0.331381180143353));
#80699=CARTESIAN_POINT('Ctrl Pts',(0.151190835544041,0.036599895343702,
-0.331215646391797));
#80700=CARTESIAN_POINT('Ctrl Pts',(0.150817339662266,0.0381097314066112,
-0.331106476125294));
#80701=CARTESIAN_POINT('Ctrl Pts',(0.147475092643408,0.0508008930098569,
-0.330193714210232));
#80702=CARTESIAN_POINT('Ctrl Pts',(0.143289710270429,0.0616260588405502,
-0.329445335627954));
#80703=CARTESIAN_POINT('Ctrl Pts',(0.135398109976251,0.0767687806790433,
-0.328317183312199));
#80704=CARTESIAN_POINT('Ctrl Pts',(0.132597455023029,0.0815107476335337,
-0.327951115804574));
#80705=CARTESIAN_POINT('Ctrl Pts',(0.127524281588751,0.0891446919271814,
-0.327329011072885));
#80706=CARTESIAN_POINT('Ctrl Pts',(0.125390025838851,0.0921225077589712,
-0.327077364656587));
#80707=CARTESIAN_POINT('Ctrl Pts',(0.122213151198575,0.0962398785543149,
-0.326714442097121));
#80708=CARTESIAN_POINT('Ctrl Pts',(0.121255518858464,0.097443662698613,
-0.326606430612682));
#80709=CARTESIAN_POINT('Ctrl Pts',(0.119555932733026,0.0995162608485024,
-0.326416976070397));
#80710=CARTESIAN_POINT('Ctrl Pts',(0.118821955032776,0.100391484206639,
-0.326335855864047));
#80711=CARTESIAN_POINT('Ctrl Pts',(0.117281325562466,0.102188025277145,
-0.326166956704383));
#80712=CARTESIAN_POINT('Ctrl Pts',(0.116473302885723,0.103108056876523,
-0.326079125046549));
#80713=CARTESIAN_POINT('Ctrl Pts',(0.114340211832302,0.105479767645434,
-0.325849126929599));
#80714=CARTESIAN_POINT('Ctrl Pts',(0.112998379782944,0.106915999448697,
-0.325706266327592));
#80715=CARTESIAN_POINT('Ctrl Pts',(0.108654866342163,0.11139196732859,-0.32524927132002));
#80716=CARTESIAN_POINT('Ctrl Pts',(0.105556299437616,0.114332346488649,
-0.324931146127184));
#80717=CARTESIAN_POINT('Ctrl Pts',(0.102342232991206,0.117140385206698,
-0.324608715049314));
#80718=CARTESIAN_POINT('Origin',(0.,0.,-1.10400562256037));
#80719=CARTESIAN_POINT('',(0.102342242837721,0.117140376604077,-0.240688435831897));
#80720=CARTESIAN_POINT('',(0.102342242833752,0.117140376607545,-0.254368055082067));
#80721=CARTESIAN_POINT('',(0.10234224283772,0.117140376604078,-1.10400562256037));
#80722=CARTESIAN_POINT('',(-0.155549938814025,0.00013796721713873,-0.285194377443525));
#80723=CARTESIAN_POINT('Ctrl Pts',(-0.155549938814074,0.000137967162685264,
-0.285194377439629));
#80724=CARTESIAN_POINT('Ctrl Pts',(-0.155558981668482,-0.010057324401557,
-0.284464910207374));
#80725=CARTESIAN_POINT('Ctrl Pts',(-0.154561332613283,-0.0202748323328174,
-0.283735442975119));
#80726=CARTESIAN_POINT('Ctrl Pts',(-0.152570315678244,-0.0303001860364103,
-0.283005975742864));
#80727=CARTESIAN_POINT('Ctrl Pts',(-0.150580816435515,-0.0403178977144842,
-0.282277064561534));
#80728=CARTESIAN_POINT('Ctrl Pts',(-0.147599629776064,-0.0501428167204543,
-0.281548153380204));
#80729=CARTESIAN_POINT('Ctrl Pts',(-0.143691318078789,-0.0595701906055402,
-0.280819242198874));
#80730=CARTESIAN_POINT('Ctrl Pts',(-0.139773730282771,-0.0690199396893853,
-0.280088600998903));
#80731=CARTESIAN_POINT('Ctrl Pts',(-0.134925019610267,-0.0780693952167697,
-0.279357959798932));
#80732=CARTESIAN_POINT('Ctrl Pts',(-0.129257441688844,-0.0865350580288423,
-0.27862731859896));
#80733=CARTESIAN_POINT('Ctrl Pts',(-0.125342359471028,-0.0923830174917879,
-0.278122602049974));
#80734=CARTESIAN_POINT('Ctrl Pts',(-0.12103754189237,-0.0979528910724632,
-0.277617885500988));
#80735=CARTESIAN_POINT('Ctrl Pts',(-0.116391161322095,-0.103193507867957,
-0.277113168952002));
#80736=CARTESIAN_POINT('Ctrl Pts',(-0.109601189038108,-0.110851865218201,
-0.276375603157067));
#80737=CARTESIAN_POINT('Ctrl Pts',(-0.102026882713366,-0.117865655153864,
-0.275638037362132));
#80738=CARTESIAN_POINT('Ctrl Pts',(-0.0938147346389066,-0.124074969533067,
-0.274900471567197));
#80739=CARTESIAN_POINT('Ctrl Pts',(-0.0855830648899174,-0.130299044510017,
-0.274161152452757));
#80740=CARTESIAN_POINT('Ctrl Pts',(-0.0767111678007134,-0.13571413733421,
-0.273421833338317));
#80741=CARTESIAN_POINT('Ctrl Pts',(-0.0673824449105403,-0.14019774826251,
-0.272682514223878));
#80742=CARTESIAN_POINT('Ctrl Pts',(-0.05809708913432,-0.144660515901933,
-0.271946632036085));
#80743=CARTESIAN_POINT('Ctrl Pts',(-0.0483599847136722,-0.148200036035695,
-0.271210749848292));
#80744=CARTESIAN_POINT('Ctrl Pts',(-0.0383761940370499,-0.150741733541945,
-0.2704748676605));
#80745=CARTESIAN_POINT('Ctrl Pts',(-0.0283224596450145,-0.153301237487933,
-0.269733830082737));
#80746=CARTESIAN_POINT('Ctrl Pts',(-0.0180194862842248,-0.154848636445333,
-0.268992792504974));
#80747=CARTESIAN_POINT('Ctrl Pts',(-0.00768806758017188,-0.155359892240188,
-0.268251754927211));
#80748=CARTESIAN_POINT('Ctrl Pts',(0.0026433511238818,-0.155871148035042,
-0.267510717349448));
#80749=CARTESIAN_POINT('Ctrl Pts',(0.0130022662074183,-0.155346342822456,
-0.266769679771685));
#80750=CARTESIAN_POINT('Ctrl Pts',(0.023170665058325,-0.153814572719086,
-0.266028642193922));
#80751=CARTESIAN_POINT('Ctrl Pts',(0.0332914247445106,-0.152289978991203,
-0.265291076392959));
#80752=CARTESIAN_POINT('Ctrl Pts',(0.0432986755703804,-0.149756542950667,
-0.264553510591997));
#80753=CARTESIAN_POINT('Ctrl Pts',(0.0529785256937023,-0.146250054069466,
-0.263815944791035));
#80754=CARTESIAN_POINT('Ctrl Pts',(0.0626813863702148,-0.142735229702913,
-0.263076625678102));
#80755=CARTESIAN_POINT('Ctrl Pts',(0.0720543656097244,-0.138242897588601,
-0.262337306565169));
#80756=CARTESIAN_POINT('Ctrl Pts',(0.0808948481806159,-0.132860174762173,
-0.261597987452237));
#80757=CARTESIAN_POINT('Ctrl Pts',(0.0896942334457746,-0.127502474936909,
-0.260862105258429));
#80758=CARTESIAN_POINT('Ctrl Pts',(0.0979652636911245,-0.121263126769864,
-0.26012622306462));
#80759=CARTESIAN_POINT('Ctrl Pts',(0.105533724046101,-0.114273512193165,
-0.259390340870812));
#80760=CARTESIAN_POINT('Ctrl Pts',(0.11315520685431,-0.107234930390026,
-0.258649303298317));
#80761=CARTESIAN_POINT('Ctrl Pts',(0.120063530842511,-0.0994361637182063,
-0.257908265725822));
#80762=CARTESIAN_POINT('Ctrl Pts',(0.126118301512676,-0.0910493081992267,
-0.257167228153327));
#80763=CARTESIAN_POINT('Ctrl Pts',(0.132173072182841,-0.0826624526802466,
-0.256426190580832));
#80764=CARTESIAN_POINT('Ctrl Pts',(0.137373841683401,-0.07368834897487,
-0.255685153008337));
#80765=CARTESIAN_POINT('Ctrl Pts',(0.141626295177241,-0.0643256948222792,
-0.254944115435842));
#80766=CARTESIAN_POINT('Ctrl Pts',(0.145858825795763,-0.0550069049921559,
-0.254206549647149));
#80767=CARTESIAN_POINT('Ctrl Pts',(0.149183400078978,-0.0452339540653752,
-0.253468983858457));
#80768=CARTESIAN_POINT('Ctrl Pts',(0.151513561061112,-0.0352057284341728,
-0.252731418069765));
#80769=CARTESIAN_POINT('Ctrl Pts',(0.153849261257435,-0.0251536638965008,
-0.251992098953765));
#80770=CARTESIAN_POINT('Ctrl Pts',(0.155185460769777,-0.0148459793914166,
-0.251252779837765));
#80771=CARTESIAN_POINT('Ctrl Pts',(0.15548489321086,-0.00450005368940009,
-0.250513460721764));
#80772=CARTESIAN_POINT('Ctrl Pts',(0.155782933655481,0.0057977760483914,
-0.249777578539952));
#80773=CARTESIAN_POINT('Ctrl Pts',(0.155053794881369,0.0161325600513416,
-0.24904169635814));
#80774=CARTESIAN_POINT('Ctrl Pts',(0.153312802145975,0.0262866353523834,
-0.248305814176328));
#80775=CARTESIAN_POINT('Ctrl Pts',(0.151559612463294,0.0365118474931549,
-0.247564776593234));
#80776=CARTESIAN_POINT('Ctrl Pts',(0.148780483665354,0.0465528707681876,
-0.246823739010139));
#80777=CARTESIAN_POINT('Ctrl Pts',(0.14504330595665,0.0561982374916302,
-0.246082701427045));
#80778=CARTESIAN_POINT('Ctrl Pts',(0.141306128247946,0.0658436042150729,
-0.24534166384395));
#80779=CARTESIAN_POINT('Ctrl Pts',(0.136611362837868,0.0750924809795906,
-0.244600626260856));
#80780=CARTESIAN_POINT('Ctrl Pts',(0.131074304207541,0.083757562503389,
-0.243859588677762));
#80781=CARTESIAN_POINT('Ctrl Pts',(0.12556327654748,0.0923819075108227,
-0.243122034880659));
#80782=CARTESIAN_POINT('Ctrl Pts',(0.119176932545119,0.100492053151117,
-0.242384481083557));
#80783=CARTESIAN_POINT('Ctrl Pts',(0.112034997693936,0.107907190639548,
-0.241646927286454));
#80784=CARTESIAN_POINT('Ctrl Pts',(0.108941219517684,0.11111931606685,-0.241327430134935));
#80785=CARTESIAN_POINT('Ctrl Pts',(0.105706230923814,0.11420135510192,-0.241007932983416));
#80786=CARTESIAN_POINT('Ctrl Pts',(0.102342242837721,0.117140376604077,
-0.240688435831897));
#80787=CARTESIAN_POINT('Ctrl Pts',(0.102342242837719,0.117140376604078,
-0.310696206146068));
#80788=CARTESIAN_POINT('Ctrl Pts',(0.101193397674604,0.118144090217394,
-0.310586387172793));
#80789=CARTESIAN_POINT('Ctrl Pts',(0.10003037851299,0.119130383226153,-0.310476568199517));
#80790=CARTESIAN_POINT('Ctrl Pts',(0.0988537724225576,0.120098851692384,
-0.310366749226242));
#80791=CARTESIAN_POINT('Ctrl Pts',(0.0909514548046981,0.126603276142732,
-0.309629183430565));
#80792=CARTESIAN_POINT('Ctrl Pts',(0.0823750481708025,0.132348588583837,
-0.308891617634889));
#80793=CARTESIAN_POINT('Ctrl Pts',(0.0732942129935362,0.137199711521775,
-0.308154051839212));
#80794=CARTESIAN_POINT('Ctrl Pts',(0.0641917911359939,0.142062366398989,
-0.307414732724958));
#80795=CARTESIAN_POINT('Ctrl Pts',(0.0545832879531424,0.146026008005004,
-0.306675413610704));
#80796=CARTESIAN_POINT('Ctrl Pts',(0.0446689805157271,0.148998270727165,
-0.305936094496449));
#80797=CARTESIAN_POINT('Ctrl Pts',(0.034800762428978,0.151956716078851,
-0.305200212307883));
#80798=CARTESIAN_POINT('Ctrl Pts',(0.0246304694614635,0.153932708599576,
-0.304464330119317));
#80799=CARTESIAN_POINT('Ctrl Pts',(0.0143722920902381,0.154884601300687,
-0.303728447930751));
#80800=CARTESIAN_POINT('Ctrl Pts',(0.00404224874535361,0.155843162700663,
-0.302987410353653));
#80801=CARTESIAN_POINT('Ctrl Pts',(-0.00637597069568843,0.155763118524284,
-0.302246372776555));
#80802=CARTESIAN_POINT('Ctrl Pts',(-0.0166605270868574,0.154655194989331,
-0.301505335199457));
#80803=CARTESIAN_POINT('Ctrl Pts',(-0.0269450834780264,0.153547271454379,
-0.300764297622359));
#80804=CARTESIAN_POINT('Ctrl Pts',(-0.0370950523170257,0.151411697858038,
-0.30002326004526));
#80805=CARTESIAN_POINT('Ctrl Pts',(-0.0468996365405047,0.1483112490419,
-0.299282222468162));
#80806=CARTESIAN_POINT('Ctrl Pts',(-0.0566582860298873,0.145225325909738,
-0.298544656671538));
#80807=CARTESIAN_POINT('Ctrl Pts',(-0.066147320962248,0.141160651001074,
-0.297807090874913));
#80808=CARTESIAN_POINT('Ctrl Pts',(-0.0751610594652361,0.136185967118728,
-0.297069525078289));
#80809=CARTESIAN_POINT('Ctrl Pts',(-0.08419622513386,0.131199457579858,
-0.296330205964271));
#80810=CARTESIAN_POINT('Ctrl Pts',(-0.0927529485620364,0.125298926055274,
-0.295590886850254));
#80811=CARTESIAN_POINT('Ctrl Pts',(-0.100644699324042,0.118602053093415,
-0.294851567736237));
#80812=CARTESIAN_POINT('Ctrl Pts',(-0.108499763151951,0.111936312353595,
-0.294115685546729));
#80813=CARTESIAN_POINT('Ctrl Pts',(-0.115695310022657,0.104482218782449,
-0.29337980335722));
#80814=CARTESIAN_POINT('Ctrl Pts',(-0.122079772151376,0.0963967412907104,
-0.292643921167712));
#80815=CARTESIAN_POINT('Ctrl Pts',(-0.128508962053125,0.0882546191835279,
-0.29190288359144));
#80816=CARTESIAN_POINT('Ctrl Pts',(-0.134115059660229,0.0794729694098018,
-0.291161846015168));
#80817=CARTESIAN_POINT('Ctrl Pts',(-0.138786259034236,0.0702436958259034,
-0.290420808438897));
#80818=CARTESIAN_POINT('Ctrl Pts',(-0.143457458408242,0.0610144222420051,
-0.289679770862625));
#80819=CARTESIAN_POINT('Ctrl Pts',(-0.147193448430352,0.0513384251183174,
-0.288938733286353));
#80820=CARTESIAN_POINT('Ctrl Pts',(-0.149932090804099,0.0414266900332545,
-0.288197695710081));
#80821=CARTESIAN_POINT('Ctrl Pts',(-0.153348034962215,0.0290636542878144,
-0.287273389928547));
#80822=CARTESIAN_POINT('Ctrl Pts',(-0.155235267497647,0.0162607764979687,
-0.286349084147013));
#80823=CARTESIAN_POINT('Ctrl Pts',(-0.155513782640199,0.00335647269272036,
-0.285424778365478));
#80824=CARTESIAN_POINT('Ctrl Pts',(-0.155536924385028,0.0022842577204016,
-0.28534797805816));
#80825=CARTESIAN_POINT('Ctrl Pts',(-0.15554898675718,0.00121135542526031,
-0.285271177750843));
#80826=CARTESIAN_POINT('Ctrl Pts',(-0.155549938814025,0.00013796721713873,
-0.285194377443525));
#80827=CARTESIAN_POINT('Ctrl Pts',(0.102342232991206,0.117140385206698,
-0.324608715049314));
#80828=CARTESIAN_POINT('Ctrl Pts',(0.0995774578652578,0.119555890837902,
-0.324331356308046));
#80829=CARTESIAN_POINT('Ctrl Pts',(0.0967272170089489,0.121873470857469,
-0.324050827145225));
#80830=CARTESIAN_POINT('Ctrl Pts',(0.0881603394717722,0.128349042152045,
-0.323224633791954));
#80831=CARTESIAN_POINT('Ctrl Pts',(0.082240427910377,0.132220387384085,
-0.322674244551114));
#80832=CARTESIAN_POINT('Ctrl Pts',(0.071360191489484,0.138321297100539,
-0.321713079532888));
#80833=CARTESIAN_POINT('Ctrl Pts',(0.0665070957496949,0.140719143160135,
-0.321300593597109));
#80834=CARTESIAN_POINT('Ctrl Pts',(0.0604511146818696,0.143327830066916,
-0.320812693485542));
#80835=CARTESIAN_POINT('Ctrl Pts',(0.0593584397561002,0.143783796003625,
-0.320725697203665));
#80836=CARTESIAN_POINT('Ctrl Pts',(0.0576112097965569,0.144489589795576,
-0.320588343478885));
#80837=CARTESIAN_POINT('Ctrl Pts',(0.0569600158959998,0.144747537782999,
-0.320537536129179));
#80838=CARTESIAN_POINT('Ctrl Pts',(0.055704460043638,0.145235097513607,
-0.320440342721329));
#80839=CARTESIAN_POINT('Ctrl Pts',(0.0551003781941231,0.145465352440342,
-0.320393922408553));
#80840=CARTESIAN_POINT('Ctrl Pts',(0.0537421817022358,0.145973374991262,
-0.32029028344851));
#80841=CARTESIAN_POINT('Ctrl Pts',(0.0529873029674625,0.1462490823832,-0.320233182970691));
#80842=CARTESIAN_POINT('Ctrl Pts',(0.0503171665215763,0.147200918594917,
-0.320032857854654));
#80843=CARTESIAN_POINT('Ctrl Pts',(0.0483907426641921,0.147845408125118,
-0.319891306619007));
#80844=CARTESIAN_POINT('Ctrl Pts',(0.037146669369087,0.151363792084599,
-0.319079222922563));
#80845=CARTESIAN_POINT('Ctrl Pts',(0.0275869269328072,0.153394520744539,
-0.318443514261546));
#80846=CARTESIAN_POINT('Ctrl Pts',(0.00996605592697227,0.155435699051433,
-0.317273987897849));
#80847=CARTESIAN_POINT('Ctrl Pts',(0.00197493010693328,0.15574228330505,
-0.316744404252176));
#80848=CARTESIAN_POINT('Ctrl Pts',(-0.00868910705218733,0.155330367386536,
-0.316012520815531));
#80849=CARTESIAN_POINT('Ctrl Pts',(-0.0113710324962245,0.155157087395567,
-0.31582640497958));
#80850=CARTESIAN_POINT('Ctrl Pts',(-0.0154122327222227,0.154790648241365,
-0.31554212674005));
#80851=CARTESIAN_POINT('Ctrl Pts',(-0.0167757348444684,0.154648815735772,
-0.315445551206598));
#80852=CARTESIAN_POINT('Ctrl Pts',(-0.0191455544922464,0.154370596764007,
-0.315276462152372));
#80853=CARTESIAN_POINT('Ctrl Pts',(-0.0201527566995663,0.154242340849208,
-0.315204206953287));
#80854=CARTESIAN_POINT('Ctrl Pts',(-0.0224269743602169,0.153930089316516,
-0.315040136548382));
#80855=CARTESIAN_POINT('Ctrl Pts',(-0.0236931044695245,0.153740294639807,
-0.314948144186946));
#80856=CARTESIAN_POINT('Ctrl Pts',(-0.0271037225009013,0.153185907214702,
-0.314698513826376));
#80857=CARTESIAN_POINT('Ctrl Pts',(-0.0292430693355967,0.152791936817779,
-0.314539968537613));
#80858=CARTESIAN_POINT('Ctrl Pts',(-0.0434940865710232,0.149857295025282,
-0.313470124199063));
#80859=CARTESIAN_POINT('Ctrl Pts',(-0.0552715078738923,0.145924252600084,
-0.312514075675306));
#80860=CARTESIAN_POINT('Ctrl Pts',(-0.0726673527218893,0.13770422422792,
-0.311023801793443));
#80861=CARTESIAN_POINT('Ctrl Pts',(-0.0786780474767305,0.1343606366774,
-0.310493805978386));
#80862=CARTESIAN_POINT('Ctrl Pts',(-0.0858115077254709,0.129749073358664,
-0.309860125724757));
#80863=CARTESIAN_POINT('Ctrl Pts',(-0.0871607618905411,0.128846571659886,
-0.309740067524514));
#80864=CARTESIAN_POINT('Ctrl Pts',(-0.089145772785032,0.127473363930259,
-0.309563414446321));
#80865=CARTESIAN_POINT('Ctrl Pts',(-0.0897924172014102,0.127018696271568,
-0.309505863481106));
#80866=CARTESIAN_POINT('Ctrl Pts',(-0.090900706063731,0.126226744147712,
-0.309407258180593));
#80867=CARTESIAN_POINT('Ctrl Pts',(-0.0913639874433515,0.12589182313022,
-0.30936605175881));
#80868=CARTESIAN_POINT('Ctrl Pts',(-0.092449840084606,0.125097673794527,
-0.309269497766083));
#80869=CARTESIAN_POINT('Ctrl Pts',(-0.0930708453419837,0.124636345964435,
-0.309214294074079));
#80870=CARTESIAN_POINT('Ctrl Pts',(-0.0949145776288989,0.123245222629986,
-0.309050358604073));
#80871=CARTESIAN_POINT('Ctrl Pts',(-0.0961270438172292,0.122301896376435,
-0.308942500840184));
#80872=CARTESIAN_POINT('Ctrl Pts',(-0.104559697708476,0.115538203302102,
-0.308190389339393));
#80873=CARTESIAN_POINT('Ctrl Pts',(-0.111261626617918,0.109099517511102,
-0.307581627383203));
#80874=CARTESIAN_POINT('Ctrl Pts',(-0.124178709282525,0.0942531972055352,
-0.306285432700813));
#80875=CARTESIAN_POINT('Ctrl Pts',(-0.130201534157377,0.0857411244615418,
-0.305599675402478));
#80876=CARTESIAN_POINT('Ctrl Pts',(-0.136335538792383,0.0749171971863099,
-0.304739042475821));
#80877=CARTESIAN_POINT('Ctrl Pts',(-0.137306451000273,0.073122523324995,
-0.304596777117482));
#80878=CARTESIAN_POINT('Ctrl Pts',(-0.138810265976411,0.0702071969106137,
-0.30436605391616));
#80879=CARTESIAN_POINT('Ctrl Pts',(-0.139365570234347,0.0690983220680937,
-0.304278382663857));
#80880=CARTESIAN_POINT('Ctrl Pts',(-0.140404384719368,0.0669604629035755,
-0.304109455066016));
#80881=CARTESIAN_POINT('Ctrl Pts',(-0.140889990564759,0.0659325812769539,
-0.304028277768552));
#80882=CARTESIAN_POINT('Ctrl Pts',(-0.141979783254097,0.0635587915278226,
-0.303840854867683));
#80883=CARTESIAN_POINT('Ctrl Pts',(-0.142576167346247,0.0622094451136279,
-0.303734351537556));
#80884=CARTESIAN_POINT('Ctrl Pts',(-0.144470081348812,0.0577540359266274,
-0.303382682284045));
#80885=CARTESIAN_POINT('Ctrl Pts',(-0.145685909611661,0.0546145183717806,
-0.30313484369636));
#80886=CARTESIAN_POINT('Ctrl Pts',(-0.150542807238968,0.0407534885815632,
-0.302039767954119));
#80887=CARTESIAN_POINT('Ctrl Pts',(-0.153108529579124,0.0296932287765719,
-0.301160347188309));
#80888=CARTESIAN_POINT('Ctrl Pts',(-0.15518460883441,0.0123180975927828,
-0.299806634002793));
#80889=CARTESIAN_POINT('Ctrl Pts',(-0.155551542164629,0.00614258291340502,
-0.299331611971668));
#80890=CARTESIAN_POINT('Ctrl Pts',(-0.155549607151914,-0.00158917287991982,
-0.298755512407639));
#80891=CARTESIAN_POINT('Ctrl Pts',(-0.155526044074766,-0.00313940290399828,
-0.298640952897414));
#80892=CARTESIAN_POINT('Ctrl Pts',(-0.155455903163095,-0.00546510875804829,
-0.298470757023469));
#80893=CARTESIAN_POINT('Ctrl Pts',(-0.155426689375158,-0.00624095670408139,
-0.298414259485607));
#80894=CARTESIAN_POINT('Ctrl Pts',(-0.155365886810345,-0.00758751276029682,
-0.298316724405288));
#80895=CARTESIAN_POINT('Ctrl Pts',(-0.155336960708364,-0.00815829635502679,
-0.298275546326686));
#80896=CARTESIAN_POINT('Ctrl Pts',(-0.155260699360192,-0.00951513483507425,
-0.298178048271776));
#80897=CARTESIAN_POINT('Ctrl Pts',(-0.155210540536866,-0.0103010064552261,
-0.298121883632185));
#80898=CARTESIAN_POINT('Ctrl Pts',(-0.155039855924804,-0.0126897229362202,
-0.297952003431668));
#80899=CARTESIAN_POINT('Ctrl Pts',(-0.154900448596701,-0.014291170111211,
-0.29783925844996));
#80900=CARTESIAN_POINT('Ctrl Pts',(-0.154050247483862,-0.0225702676408501,
-0.297260989561896));
#80901=CARTESIAN_POINT('Ctrl Pts',(-0.152932323938379,-0.029199679994003,
-0.296813291170937));
#80902=CARTESIAN_POINT('Ctrl Pts',(-0.148491034362419,-0.0480140174521139,
-0.295535466929416));
#80903=CARTESIAN_POINT('Ctrl Pts',(-0.14411061745827,-0.0598918201436837,
-0.294715751762492));
#80904=CARTESIAN_POINT('Ctrl Pts',(-0.137353600519461,-0.0730375795244298,
-0.293695187238585));
#80905=CARTESIAN_POINT('Ctrl Pts',(-0.136322691964313,-0.0749441289201565,
-0.293544292359504));
#80906=CARTESIAN_POINT('Ctrl Pts',(-0.134626723801917,-0.077929789500584,
-0.29330300189276));
#80907=CARTESIAN_POINT('Ctrl Pts',(-0.133987704337724,-0.0790234254538095,
-0.293213530962021));
#80908=CARTESIAN_POINT('Ctrl Pts',(-0.132753243559565,-0.081078089996767,
-0.29304329492563));
#80909=CARTESIAN_POINT('Ctrl Pts',(-0.132160539180629,-0.0820406735305506,
-0.292962633102756));
#80910=CARTESIAN_POINT('Ctrl Pts',(-0.130784268687581,-0.084222189254922,
-0.292777691705462));
#80911=CARTESIAN_POINT('Ctrl Pts',(-0.129994066217153,-0.0854367870712042,
-0.292673172805494));
#80912=CARTESIAN_POINT('Ctrl Pts',(-0.12745166189055,-0.0892277055727707,
-0.292341921080406));
#80913=CARTESIAN_POINT('Ctrl Pts',(-0.125639061034569,-0.091762374399115,
-0.292112964695512));
#80914=CARTESIAN_POINT('Ctrl Pts',(-0.121116916493584,-0.097700602095763,
-0.291557922715467));
#80915=CARTESIAN_POINT('Ctrl Pts',(-0.118338422613799,-0.101048141916091,
-0.291229481986223));
#80916=CARTESIAN_POINT('Ctrl Pts',(-0.111247974901332,-0.108896691394552,
-0.290421482821475));
#80917=CARTESIAN_POINT('Ctrl Pts',(-0.106798718969604,-0.113263530635705,
-0.28993854592397));
#80918=CARTESIAN_POINT('Ctrl Pts',(-0.0966667491466219,-0.122078690107172,
-0.288898026968516));
#80919=CARTESIAN_POINT('Ctrl Pts',(-0.0909112997371471,-0.126423188949271,
-0.288341710379856));
#80920=CARTESIAN_POINT('Ctrl Pts',(-0.0835330513956159,-0.131227268664951,
-0.287685127246972));
#80921=CARTESIAN_POINT('Ctrl Pts',(-0.0821776383292283,-0.132080289980819,
-0.287566712739405));
#80922=CARTESIAN_POINT('Ctrl Pts',(-0.0801373742888518,-0.133320748503863,
-0.287391986417021));
#80923=CARTESIAN_POINT('Ctrl Pts',(-0.0794624155207532,-0.133724138921695,
-0.28733474733288));
#80924=CARTESIAN_POINT('Ctrl Pts',(-0.0782371391933199,-0.134443874520561,
-0.287231893103517));
#80925=CARTESIAN_POINT('Ctrl Pts',(-0.0776879175883482,-0.13476198589118,
-0.28718617134235));
#80926=CARTESIAN_POINT('Ctrl Pts',(-0.0764326942394409,-0.135478791919709,
-0.287082534534691));
#80927=CARTESIAN_POINT('Ctrl Pts',(-0.0757255044505087,-0.135875339416135,
-0.287024753405496));
#80928=CARTESIAN_POINT('Ctrl Pts',(-0.073498390652203,-0.137101375362434,
-0.286844578444149));
#80929=CARTESIAN_POINT('Ctrl Pts',(-0.0719676365458002,-0.137911060075139,
-0.286723334284815));
#80930=CARTESIAN_POINT('Ctrl Pts',(-0.0682606318143345,-0.139793323386092,
-0.286435113261444));
#80931=CARTESIAN_POINT('Ctrl Pts',(-0.0660721427909364,-0.140840904593983,
-0.286269326981563));
#80932=CARTESIAN_POINT('Ctrl Pts',(-0.0570478087702293,-0.14490397422584,
-0.285599738520941));
#80933=CARTESIAN_POINT('Ctrl Pts',(-0.0500231310482297,-0.147476491644343,
-0.285110432888552));
#80934=CARTESIAN_POINT('Ctrl Pts',(-0.0343819299477129,-0.151957568813729,
-0.284038200592309));
#80935=CARTESIAN_POINT('Ctrl Pts',(-0.0257341202640613,-0.153658548126121,
-0.283455536359174));
#80936=CARTESIAN_POINT('Ctrl Pts',(-0.0148274964742767,-0.154856961367827,
-0.282700477575218));
#80937=CARTESIAN_POINT('Ctrl Pts',(-0.01266085682664,-0.155049137545369,
-0.282549573702179));
#80938=CARTESIAN_POINT('Ctrl Pts',(-0.00910386767394617,-0.155289584281115,
-0.28229993562745));
#80939=CARTESIAN_POINT('Ctrl Pts',(-0.00771559456445765,-0.155364747520493,
-0.28220203202903));
#80940=CARTESIAN_POINT('Ctrl Pts',(-0.00520200674194078,-0.155467064983784,
-0.282023822291512));
#80941=CARTESIAN_POINT('Ctrl Pts',(-0.00407703817784952,-0.155500632820194,
-0.281943721097383));
#80942=CARTESIAN_POINT('Ctrl Pts',(-0.0016462645624265,-0.155546769269533,
-0.281769853652271));
#80943=CARTESIAN_POINT('Ctrl Pts',(-0.000340476043106266,-0.155555107603514,
-0.28167596197086));
#80944=CARTESIAN_POINT('Ctrl Pts',(0.00332283652720539,-0.155532375392482,
-0.281411096590015));
#80945=CARTESIAN_POINT('Ctrl Pts',(0.00567968293065076,-0.155464147375873,
-0.28123899225281));
#80946=CARTESIAN_POINT('Ctrl Pts',(0.0160363573838207,-0.154928523796453,
-0.280474814526348));
#80947=CARTESIAN_POINT('Ctrl Pts',(0.0239935958899593,-0.153896991398887,
-0.279866021609797));
#80948=CARTESIAN_POINT('Ctrl Pts',(0.0405129523280155,-0.15044302565002,
-0.278564267130008));
#80949=CARTESIAN_POINT('Ctrl Pts',(0.049020061628579,-0.147889969579086,
-0.277871468719104));
#80950=CARTESIAN_POINT('Ctrl Pts',(0.0601541550801836,-0.143481518347877,
-0.276961609693985));
#80951=CARTESIAN_POINT('Ctrl Pts',(0.0630101143312593,-0.14225047333252,
-0.276728063734208));
#80952=CARTESIAN_POINT('Ctrl Pts',(0.066768016638625,-0.140495238597484,
-0.276422216591579));
#80953=CARTESIAN_POINT('Ctrl Pts',(0.0677041737846811,-0.140046510567872,
-0.276346149323808));
#80954=CARTESIAN_POINT('Ctrl Pts',(0.0691766534402561,-0.139322490511125,
-0.276226779705948));
#80955=CARTESIAN_POINT('Ctrl Pts',(0.069715967472237,-0.139053405769155,
-0.27618311835309));
#80956=CARTESIAN_POINT('Ctrl Pts',(0.07084480534099,-0.138481966247615,
-0.27609187642972));
#80957=CARTESIAN_POINT('Ctrl Pts',(0.0714339857500194,-0.138178967748704,
-0.276044340049154));
#80958=CARTESIAN_POINT('Ctrl Pts',(0.0729138774641495,-0.137405906871741,
-0.275925111684539));
#80959=CARTESIAN_POINT('Ctrl Pts',(0.073802013731886,-0.136930930328859,
-0.275853716865926));
#80960=CARTESIAN_POINT('Ctrl Pts',(0.0774012105278814,-0.134960882246662,
-0.275564774646624));
#80961=CARTESIAN_POINT('Ctrl Pts',(0.0800721628053102,-0.133393549532656,
-0.275351250883022));
#80962=CARTESIAN_POINT('Ctrl Pts',(0.0875618131086776,-0.128692471420388,
-0.274749853935152));
#80963=CARTESIAN_POINT('Ctrl Pts',(0.0922562062560516,-0.125369953687317,
-0.274369547563549));
#80964=CARTESIAN_POINT('Ctrl Pts',(0.105574175569846,-0.114789910879557,
-0.273247978516741));
#80965=CARTESIAN_POINT('Ctrl Pts',(0.113604320642675,-0.10684874957738,
-0.272511461397408));
#80966=CARTESIAN_POINT('Ctrl Pts',(0.122158618889659,-0.0963243175115933,
-0.271577118846981));
#80967=CARTESIAN_POINT('Ctrl Pts',(0.123570746881867,-0.0945059357202949,
-0.271417131269575));
#80968=CARTESIAN_POINT('Ctrl Pts',(0.125720932240138,-0.0916065494053033,
-0.27116380311641));
#80969=CARTESIAN_POINT('Ctrl Pts',(0.126486621492542,-0.0905463809065521,
-0.27107153264621));
#80970=CARTESIAN_POINT('Ctrl Pts',(0.127886149705519,-0.0885562056881211,
-0.270898904482829));
#80971=CARTESIAN_POINT('Ctrl Pts',(0.12852344300986,-0.0876287243311157,
-0.270818685211601));
#80972=CARTESIAN_POINT('Ctrl Pts',(0.129924074026566,-0.0855421734960147,
-0.270638678097841));
#80973=CARTESIAN_POINT('Ctrl Pts',(0.130682067086161,-0.0843796513964934,
-0.270538699051406));
#80974=CARTESIAN_POINT('Ctrl Pts',(0.132909728695237,-0.0808610961356502,
-0.270236928755979));
#80975=CARTESIAN_POINT('Ctrl Pts',(0.134331895257323,-0.0784758112442404,
-0.270033443760925));
#80976=CARTESIAN_POINT('Ctrl Pts',(0.138601560385234,-0.0708582085333875,
-0.269386563920474));
#80977=CARTESIAN_POINT('Ctrl Pts',(0.141212578133769,-0.065500161864576,
-0.268935605584176));
#80978=CARTESIAN_POINT('Ctrl Pts',(0.14428338561334,-0.0581560703844953,
-0.268324542680345));
#80979=CARTESIAN_POINT('Ctrl Pts',(0.145021115880139,-0.0562912028906115,
-0.268169990125387));
#80980=CARTESIAN_POINT('Ctrl Pts',(0.149213374758756,-0.0450639062517173,
-0.26724399780844));
#80981=CARTESIAN_POINT('Ctrl Pts',(0.15179661786613,-0.035400515145278,
-0.266463598253098));
#80982=CARTESIAN_POINT('Ctrl Pts',(0.153738558825832,-0.0237411520744586,
-0.265578875701345));
#80983=CARTESIAN_POINT('Ctrl Pts',(0.154008600880754,-0.0219211861052032,
-0.265442434793654));
#80984=CARTESIAN_POINT('Ctrl Pts',(0.154352431084631,-0.0192822260481019,
-0.265247379978161));
#80985=CARTESIAN_POINT('Ctrl Pts',(0.15445210589775,-0.0184668429123928,
-0.265187495217724));
#80986=CARTESIAN_POINT('Ctrl Pts',(0.154617484667173,-0.0170188245750852,
-0.265081870649495));
#80987=CARTESIAN_POINT('Ctrl Pts',(0.15468577438873,-0.0163865252033171,
-0.265035994837533));
#80988=CARTESIAN_POINT('Ctrl Pts',(0.154827760440746,-0.014991789578896,
-0.264935349332066));
#80989=CARTESIAN_POINT('Ctrl Pts',(0.154899705816366,-0.0142292080456393,
-0.264880675224894));
#80990=CARTESIAN_POINT('Ctrl Pts',(0.155095657690461,-0.0119742217889823,
-0.264719965119066));
#80991=CARTESIAN_POINT('Ctrl Pts',(0.155203753663212,-0.0104804723997598,
-0.264614752809675));
#80992=CARTESIAN_POINT('Ctrl Pts',(0.155620548156694,-0.0032771565080258,
-0.264112366097192));
#80993=CARTESIAN_POINT('Ctrl Pts',(0.155635884889912,0.00244554408657134,
-0.263728214927522));
#80994=CARTESIAN_POINT('Ctrl Pts',(0.15462532416037,0.0216907172833835,
-0.262448752975366));
#80995=CARTESIAN_POINT('Ctrl Pts',(0.152149161910106,0.0350726613191967,
-0.261574306215701));
#80996=CARTESIAN_POINT('Ctrl Pts',(0.147269646702286,0.050126018370757,
-0.260483685098901));
#80997=CARTESIAN_POINT('Ctrl Pts',(0.146521673775424,0.0522720265913844,
-0.260325709870193));
#80998=CARTESIAN_POINT('Ctrl Pts',(0.14527186664726,0.0556199675975706,
-0.260074864363362));
#80999=CARTESIAN_POINT('Ctrl Pts',(0.144801470889826,0.0568333518285932,
-0.259983029142518));
#81000=CARTESIAN_POINT('Ctrl Pts',(0.143895840188974,0.0590851685460495,
-0.259810794872113));
#81001=CARTESIAN_POINT('Ctrl Pts',(0.14346444475922,0.0601250607830885,
-0.259730528922739));
#81002=CARTESIAN_POINT('Ctrl Pts',(0.142472874223701,0.0624438288473355,
-0.25954986365613));
#81003=CARTESIAN_POINT('Ctrl Pts',(0.141906698627159,0.0637200149156635,
-0.259449266577453));
#81004=CARTESIAN_POINT('Ctrl Pts',(0.140144667671015,0.0675517201084837,
-0.259143593520673));
#81005=CARTESIAN_POINT('Ctrl Pts',(0.138896449057761,0.0700823608466168,
-0.258936757824729));
#81006=CARTESIAN_POINT('Ctrl Pts',(0.134228034344481,0.078931951923188,
-0.258195197389933));
#81007=CARTESIAN_POINT('Ctrl Pts',(0.130440122460054,0.0850456811818212,
-0.257648494844447));
#81008=CARTESIAN_POINT('Ctrl Pts',(0.121127845779657,0.0979823111246914,
-0.256419249406507));
#81009=CARTESIAN_POINT('Ctrl Pts',(0.115420774050056,0.104644819969919,
-0.255735028883777));
#81010=CARTESIAN_POINT('Ctrl Pts',(0.106967115260322,0.11297574982386,-0.254832118582925));
#81011=CARTESIAN_POINT('Ctrl Pts',(0.104685744149188,0.115092925611983,
-0.254598006970998));
#81012=CARTESIAN_POINT('Ctrl Pts',(0.102342242833752,0.117140376607545,
-0.254368055082067));
#81013=CARTESIAN_POINT('Origin',(0.,0.,-1.10400562256037));
#81014=CARTESIAN_POINT('',(0.10234224283772,0.117140376604078,-0.170697633677947));
#81015=CARTESIAN_POINT('',(0.102342242826532,0.117140376613853,-0.184536881298507));
#81016=CARTESIAN_POINT('',(0.10234224283772,0.117140376604078,-1.10400562256037));
#81017=CARTESIAN_POINT('',(-0.155549984535534,-6.93613367895633E-5,-0.215194377432725));
#81018=CARTESIAN_POINT('Ctrl Pts',(-0.155549984535534,-6.93613367884616E-5,
-0.215194377432725));
#81019=CARTESIAN_POINT('Ctrl Pts',(-0.155544924241764,-0.0114175944321142,
-0.214385432002025));
#81020=CARTESIAN_POINT('Ctrl Pts',(-0.154293756121922,-0.0227244664062756,
-0.213576486571325));
#81021=CARTESIAN_POINT('Ctrl Pts',(-0.151848298219052,-0.0337327263644348,
-0.212767541140625));
#81022=CARTESIAN_POINT('Ctrl Pts',(-0.149670179599569,-0.0435375551267021,
-0.212047030228257));
#81023=CARTESIAN_POINT('Ctrl Pts',(-0.146545503580168,-0.053105400351191,
-0.211326519315889));
#81024=CARTESIAN_POINT('Ctrl Pts',(-0.14254312808969,-0.0622676411501693,
-0.210606008403521));
#81025=CARTESIAN_POINT('Ctrl Pts',(-0.138446014228048,-0.071646757095313,
-0.209868442612018));
#81026=CARTESIAN_POINT('Ctrl Pts',(-0.133404010521729,-0.0806546181908517,
-0.209130876820515));
#81027=CARTESIAN_POINT('Ctrl Pts',(-0.127507151897742,-0.0890939319758985,
-0.208393311029012));
#81028=CARTESIAN_POINT('Ctrl Pts',(-0.121596275402187,-0.0975533074962367,
-0.207653991913714));
#81029=CARTESIAN_POINT('Ctrl Pts',(-0.114826884814375,-0.105440584507109,
-0.206914672798417));
#81030=CARTESIAN_POINT('Ctrl Pts',(-0.107335662132136,-0.112582672444101,
-0.206175353683119));
#81031=CARTESIAN_POINT('Ctrl Pts',(-0.0998792645099848,-0.119691558372276,
-0.205439471501111));
#81032=CARTESIAN_POINT('Ctrl Pts',(-0.0917084040091688,-0.126061522420267,
-0.204703589319102));
#81033=CARTESIAN_POINT('Ctrl Pts',(-0.0829951478406017,-0.131558382229779,
-0.203967707137094));
#81034=CARTESIAN_POINT('Ctrl Pts',(-0.0742208488565232,-0.137093751615132,
-0.203226669555152));
#81035=CARTESIAN_POINT('Ctrl Pts',(-0.0648973211481259,-0.141743217842826,
-0.20248563197321));
#81036=CARTESIAN_POINT('Ctrl Pts',(-0.0552271822349882,-0.145415820468006,
-0.201744594391268));
#81037=CARTESIAN_POINT('Ctrl Pts',(-0.04555704332185,-0.149088423093186,
-0.201003556809326));
#81038=CARTESIAN_POINT('Ctrl Pts',(-0.0355412212476219,-0.151783947600411,
-0.200262519227384));
#81039=CARTESIAN_POINT('Ctrl Pts',(-0.0253960749986721,-0.153462835483585,
-0.199521481645442));
#81040=CARTESIAN_POINT('Ctrl Pts',(-0.0152984561802915,-0.155133858203917,
-0.198783915636147));
#81041=CARTESIAN_POINT('Ctrl Pts',(-0.00499768058454571,-0.155810207328269,
-0.198046349626853));
#81042=CARTESIAN_POINT('Ctrl Pts',(0.00529174832921784,-0.155459962368515,
-0.197308783617558));
#81043=CARTESIAN_POINT('Ctrl Pts',(0.0156056332226933,-0.155108884944327,
-0.196569464556709));
#81044=CARTESIAN_POINT('Ctrl Pts',(0.0259071855506799,-0.15372621134018,
-0.195830145495859));
#81045=CARTESIAN_POINT('Ctrl Pts',(0.0359767993225822,-0.151332324407255,
-0.195090826435009));
#81046=CARTESIAN_POINT('Ctrl Pts',(0.0459996053868997,-0.148949565245671,
-0.19435494403332));
#81047=CARTESIAN_POINT('Ctrl Pts',(0.0557917163008593,-0.145565185573833,
-0.193619061631631));
#81048=CARTESIAN_POINT('Ctrl Pts',(0.0651468902848729,-0.141250434286804,
-0.192883179229942));
#81049=CARTESIAN_POINT('Ctrl Pts',(0.0745675989473153,-0.136905457390013,
-0.192142141839512));
#81050=CARTESIAN_POINT('Ctrl Pts',(0.0835443572856849,-0.131617409202288,
-0.191401104449082));
#81051=CARTESIAN_POINT('Ctrl Pts',(0.0918905391417884,-0.125506698292288,
-0.190660067058652));
#81052=CARTESIAN_POINT('Ctrl Pts',(0.100236720997892,-0.119395987382288,
-0.189919029668222));
#81053=CARTESIAN_POINT('Ctrl Pts',(0.107951641088085,-0.112463275310278,
-0.189177992277792));
#81054=CARTESIAN_POINT('Ctrl Pts',(0.114884302548217,-0.104868486820444,
-0.188436954887361));
#81055=CARTESIAN_POINT('Ctrl Pts',(0.121784482046381,-0.097309282591043,
-0.187699389518243));
#81056=CARTESIAN_POINT('Ctrl Pts',(0.127961030407077,-0.0890380370869365,
-0.186961824149124));
#81057=CARTESIAN_POINT('Ctrl Pts',(0.133270367378195,-0.0802172779323822,
-0.186224258780005));
#81058=CARTESIAN_POINT('Ctrl Pts',(0.138592329386306,-0.0713755439534292,
-0.185484939559112));
#81059=CARTESIAN_POINT('Ctrl Pts',(0.143042345846606,-0.0619823981288728,
-0.184745620338218));
#81060=CARTESIAN_POINT('Ctrl Pts',(0.14651792591867,-0.0522331301425736,
-0.184006301117324));
#81061=CARTESIAN_POINT('Ctrl Pts',(0.14997734635418,-0.0425291911730338,
-0.183270419345621));
#81062=CARTESIAN_POINT('Ctrl Pts',(0.152471055355108,-0.0324733116894837,
-0.182534537573919));
#81063=CARTESIAN_POINT('Ctrl Pts',(0.153946502728169,-0.0222772708778693,
-0.181798655802216));
#81064=CARTESIAN_POINT('Ctrl Pts',(0.155432288260647,-0.0120097884836756,
-0.181057617856727));
#81065=CARTESIAN_POINT('Ctrl Pts',(0.155885338135254,-0.00160111105110903,
-0.180316579911238));
#81066=CARTESIAN_POINT('Ctrl Pts',(0.155305015513463,0.00872666352984315,
-0.179575541965749));
#81067=CARTESIAN_POINT('Ctrl Pts',(0.154724692891672,0.0190544381107961,
-0.178834504020259));
#81068=CARTESIAN_POINT('Ctrl Pts',(0.153111179475993,0.0293003748119713,
-0.17809346607477));
#81069=CARTESIAN_POINT('Ctrl Pts',(0.150516384009077,0.039250740691509,
-0.177352428129281));
#81070=CARTESIAN_POINT('Ctrl Pts',(0.147933773686665,0.0491543797104302,
-0.176614870093697));
#81071=CARTESIAN_POINT('Ctrl Pts',(0.144359921071405,0.0588388340894559,
-0.175877312058113));
#81072=CARTESIAN_POINT('Ctrl Pts',(0.139852954270346,0.0680951810472411,
-0.17513975402253));
#81073=CARTESIAN_POINT('Ctrl Pts',(0.135328906002627,0.0773866096883254,
-0.174399400631766));
#81074=CARTESIAN_POINT('Ctrl Pts',(0.129864919948991,0.0862457725237679,
-0.173659047241002));
#81075=CARTESIAN_POINT('Ctrl Pts',(0.12356946561236,0.0944795727566328,
-0.172918693850239));
#81076=CARTESIAN_POINT('Ctrl Pts',(0.117274011275729,0.102713372989497,
-0.172178340459475));
#81077=CARTESIAN_POINT('Ctrl Pts',(0.110147633291769,0.110321027132533,
-0.171437987068711));
#81078=CARTESIAN_POINT('Ctrl Pts',(0.10234224283772,0.117140376604078,-0.170697633677947));
#81079=CARTESIAN_POINT('Ctrl Pts',(0.102342242837721,0.117140376604077,
-0.240688435831897));
#81080=CARTESIAN_POINT('Ctrl Pts',(0.0945907992358971,0.123912594232521,
-0.239952236984707));
#81081=CARTESIAN_POINT('Ctrl Pts',(0.0861522819330473,0.129922626667033,
-0.239216038137517));
#81082=CARTESIAN_POINT('Ctrl Pts',(0.077201467392696,0.135039756858543,
-0.238479839290327));
#81083=CARTESIAN_POINT('Ctrl Pts',(0.0682553086659258,0.140154225347687,
-0.237744023380866));
#81084=CARTESIAN_POINT('Ctrl Pts',(0.0587981892741572,0.144376258801276,
-0.237008207471405));
#81085=CARTESIAN_POINT('Ctrl Pts',(0.0490306936084764,0.147620437556159,
-0.236272391561943));
#81086=CARTESIAN_POINT('Ctrl Pts',(0.039239939646621,0.150872341328067,
-0.235534823532498));
#81087=CARTESIAN_POINT('Ctrl Pts',(0.0291382295232789,0.153141489378281,
-0.234797255503053));
#81088=CARTESIAN_POINT('Ctrl Pts',(0.0189409422343509,0.154392497250595,
-0.234059687473607));
#81089=CARTESIAN_POINT('Ctrl Pts',(0.0130207218573329,0.15511879259637,
-0.233631478955632));
#81090=CARTESIAN_POINT('Ctrl Pts',(0.00706846490628639,0.155502887085559,
-0.233203270437657));
#81091=CARTESIAN_POINT('Ctrl Pts',(0.00112651773548907,0.155545920736584,
-0.232775061919681));
#81092=CARTESIAN_POINT('Ctrl Pts',(-0.00910816235334534,0.155620043854584,
-0.232037496090364));
#81093=CARTESIAN_POINT('Ctrl Pts',(-0.019388222831283,0.154679973770776,
-0.231299930261046));
#81094=CARTESIAN_POINT('Ctrl Pts',(-0.0294968071169101,0.15272766897294,
-0.230562364431728));
#81095=CARTESIAN_POINT('Ctrl Pts',(-0.0396294206387574,0.150770723328093,
-0.229823045325885));
#81096=CARTESIAN_POINT('Ctrl Pts',(-0.0495888031548398,0.147796755498571,
-0.229083726220041));
#81097=CARTESIAN_POINT('Ctrl Pts',(-0.0591612233517547,0.143860182648027,
-0.228344407114197));
#81098=CARTESIAN_POINT('Ctrl Pts',(-0.068689144095095,0.139941909802832,
-0.227608524892187));
#81099=CARTESIAN_POINT('Ctrl Pts',(-0.0778328285156711,0.135070313602817,
-0.226872642670177));
#81100=CARTESIAN_POINT('Ctrl Pts',(-0.0863996868963797,0.129347967143699,
-0.226136760448167));
#81101=CARTESIAN_POINT('Ctrl Pts',(-0.0950265616007538,0.123585531986723,
-0.225395722900406));
#81102=CARTESIAN_POINT('Ctrl Pts',(-0.103067699695561,0.116960896736977,
-0.224654685352646));
#81103=CARTESIAN_POINT('Ctrl Pts',(-0.110357561019662,0.10962212927047,
-0.223913647804885));
#81104=CARTESIAN_POINT('Ctrl Pts',(-0.117647422343763,0.102283361803962,
-0.223172610257124));
#81105=CARTESIAN_POINT('Ctrl Pts',(-0.124185433295616,0.0942312225561094,
-0.222431572709363));
#81106=CARTESIAN_POINT('Ctrl Pts',(-0.129847415376793,0.0856472487588859,
-0.221690535161602));
#81107=CARTESIAN_POINT('Ctrl Pts',(-0.135586640544162,0.0769461688637659,
-0.220939388075105));
#81108=CARTESIAN_POINT('Ctrl Pts',(-0.140467434326455,0.0676358586772041,
-0.220188240988607));
#81109=CARTESIAN_POINT('Ctrl Pts',(-0.144370123305893,0.0579056991723721,
-0.21943709390211));
#81110=CARTESIAN_POINT('Ctrl Pts',(-0.148263561630633,0.0481986033413841,
-0.218687727280918));
#81111=CARTESIAN_POINT('Ctrl Pts',(-0.151183090597988,0.0380744094506218,
-0.217938360659726));
#81112=CARTESIAN_POINT('Ctrl Pts',(-0.15305544994819,0.0277458418714797,
-0.217188994038534));
#81113=CARTESIAN_POINT('Ctrl Pts',(-0.154716692448818,0.0185818662536416,
-0.216524121838899));
#81114=CARTESIAN_POINT('Ctrl Pts',(-0.155554143584908,0.00925775084187499,
-0.215859249639264));
#81115=CARTESIAN_POINT('Ctrl Pts',(-0.155549984535578,-6.93612399397573E-5,
-0.215194377439629));
#81116=CARTESIAN_POINT('',(-0.155549939620994,0.000137054387354205,-0.229033329119584));
#81117=CARTESIAN_POINT('Ctrl Pts',(0.102342242833752,0.117140376607545,
-0.254368055082067));
#81118=CARTESIAN_POINT('Ctrl Pts',(0.102237155459024,0.117232188482618,
-0.254357743570756));
#81119=CARTESIAN_POINT('Ctrl Pts',(0.102131943151496,0.117323860156174,
-0.254347440447633));
#81120=CARTESIAN_POINT('Ctrl Pts',(0.101230699495509,0.118106984331783,
-0.254259361857058));
#81121=CARTESIAN_POINT('Ctrl Pts',(0.100427751951031,0.118790492334365,
-0.254182072473187));
#81122=CARTESIAN_POINT('Ctrl Pts',(0.0991525990076992,0.119853792747519,
-0.254061258475514));
#81123=CARTESIAN_POINT('Ctrl Pts',(0.098685037457719,0.120239065787949,
-0.254017360350847));
#81124=CARTESIAN_POINT('Ctrl Pts',(0.09770379834357,0.12103803228153,-0.253926088736467));
#81125=CARTESIAN_POINT('Ctrl Pts',(0.0971897210145893,0.121451206760199,
-0.253878755764946));
#81126=CARTESIAN_POINT('Ctrl Pts',(0.0958957476446415,0.122477722284622,
-0.253760779619929));
#81127=CARTESIAN_POINT('Ctrl Pts',(0.0951125639313814,0.12308690909447,
-0.253690420536054));
#81128=CARTESIAN_POINT('Ctrl Pts',(0.0919662299546577,0.125486269452311,
-0.253411660576555));
#81129=CARTESIAN_POINT('Ctrl Pts',(0.0895577780559352,0.127216345240533,
-0.253206934893019));
#81130=CARTESIAN_POINT('Ctrl Pts',(0.0826721827140387,0.131869967987762,
-0.252640863873219));
#81131=CARTESIAN_POINT('Ctrl Pts',(0.078091516219679,0.134633211558832,
-0.252286067737515));
#81132=CARTESIAN_POINT('Ctrl Pts',(0.0628318062082967,0.142797077335476,
-0.251143612545098));
#81133=CARTESIAN_POINT('Ctrl Pts',(0.0516720087248723,0.147203298417664,
-0.250364046703397));
#81134=CARTESIAN_POINT('Ctrl Pts',(0.0379652838529928,0.150862204128483,
-0.249385698727708));
#81135=CARTESIAN_POINT('Ctrl Pts',(0.0358004580935539,0.151390533900714,
-0.2492307252812));
#81136=CARTESIAN_POINT('Ctrl Pts',(0.0323638731944192,0.152151407938639,
-0.248983584670104));
#81137=CARTESIAN_POINT('Ctrl Pts',(0.0310992300763334,0.15241492359857,
-0.24889240123796));
#81138=CARTESIAN_POINT('Ctrl Pts',(0.028736195244139,0.152876679222919,
-0.248721505364394));
#81139=CARTESIAN_POINT('Ctrl Pts',(0.0276386608629597,0.153078908653628,
-0.248641925078218));
#81140=CARTESIAN_POINT('Ctrl Pts',(0.0251557270309056,0.153508836596325,
-0.248461379400763));
#81141=CARTESIAN_POINT('Ctrl Pts',(0.023769246937255,0.153729620363511,
-0.248360203079257));
#81142=CARTESIAN_POINT('Ctrl Pts',(0.0195461659202881,0.154343611202967,
-0.248050842254632));
#81143=CARTESIAN_POINT('Ctrl Pts',(0.0167016696748106,0.154677261298513,
-0.247840834539995));
#81144=CARTESIAN_POINT('Ctrl Pts',(0.00606029667304388,0.155628518483842,
-0.247048609468335));
#81145=CARTESIAN_POINT('Ctrl Pts',(-0.00176950607963955,0.155736317986571,
-0.246451824251603));
#81146=CARTESIAN_POINT('Ctrl Pts',(-0.0195188630475428,0.154641871805015,
-0.245077820488252));
#81147=CARTESIAN_POINT('Ctrl Pts',(-0.0293830388359485,0.153074341744745,
-0.244298571100877));
#81148=CARTESIAN_POINT('Ctrl Pts',(-0.0408252246802439,0.150108438451841,
-0.243413628989057));
#81149=CARTESIAN_POINT('Ctrl Pts',(-0.0426121913330136,0.149610976221383,
-0.243276049838723));
#81150=CARTESIAN_POINT('Ctrl Pts',(-0.0451796869573198,0.148846489365071,
-0.243079684867336));
#81151=CARTESIAN_POINT('Ctrl Pts',(-0.0459675843097169,0.148605056386415,
-0.24301960537448));
#81152=CARTESIAN_POINT('Ctrl Pts',(-0.0473603025091855,0.148166153214888,
-0.242913770474043));
#81153=CARTESIAN_POINT('Ctrl Pts',(-0.0479658806957881,0.14797121866722,
-0.242867876934328));
#81154=CARTESIAN_POINT('Ctrl Pts',(-0.0492960128460711,0.147534027269328,
-0.242767354683724));
#81155=CARTESIAN_POINT('Ctrl Pts',(-0.0500199972454502,0.147290142323381,
-0.242712819787466));
#81156=CARTESIAN_POINT('Ctrl Pts',(-0.0521482624463817,0.146555701857846,
-0.242552951865193));
#81157=CARTESIAN_POINT('Ctrl Pts',(-0.0535473843819025,0.146050310071637,
-0.242448429625248));
#81158=CARTESIAN_POINT('Ctrl Pts',(-0.0646625466860618,0.141854072276852,
-0.241621031911769));
#81159=CARTESIAN_POINT('Ctrl Pts',(-0.0739950524959171,0.137217410717385,
-0.240943368765056));
#81160=CARTESIAN_POINT('Ctrl Pts',(-0.0908053356306465,0.126647928935881,
-0.239634617721139));
#81161=CARTESIAN_POINT('Ctrl Pts',(-0.0983372909981724,0.120892724275524,
-0.239007317317134));
#81162=CARTESIAN_POINT('Ctrl Pts',(-0.106763368528717,0.113143016164262,
-0.238214769340962));
#81163=CARTESIAN_POINT('Ctrl Pts',(-0.108201373991743,0.111768604766045,
-0.238075993724116));
#81164=CARTESIAN_POINT('Ctrl Pts',(-0.110484879049356,0.109500709862623,
-0.23784954042197));
#81165=CARTESIAN_POINT('Ctrl Pts',(-0.111346857856541,0.108624081350539,
-0.237762596087138));
#81166=CARTESIAN_POINT('Ctrl Pts',(-0.112988180000601,0.106914798452867,
-0.237594124907835));
#81167=CARTESIAN_POINT('Ctrl Pts',(-0.113768937480959,0.106083607054832,
-0.237512666749974));
#81168=CARTESIAN_POINT('Ctrl Pts',(-0.114602093295998,0.105176855859264,
-0.237424277959772));
#81169=CARTESIAN_POINT('Ctrl Pts',(-0.114663660870459,0.105109731576027,
-0.237417737558879));
#81170=CARTESIAN_POINT('Ctrl Pts',(-0.114781783749357,0.104980720362508,
-0.237405172379322));
#81171=CARTESIAN_POINT('Ctrl Pts',(-0.114838348066653,0.104918841691026,
-0.237399147982927));
#81172=CARTESIAN_POINT('Ctrl Pts',(-0.114947899103571,0.104798803341607,
-0.237387465783282));
#81173=CARTESIAN_POINT('Ctrl Pts',(-0.115000891789213,0.104740649118675,
-0.237381808233095));
#81174=CARTESIAN_POINT('Ctrl Pts',(-0.115104396697849,0.104626889489676,
-0.237370745090582));
#81175=CARTESIAN_POINT('Ctrl Pts',(-0.115154912813204,0.10457128763866,
-0.237365339663611));
#81176=CARTESIAN_POINT('Ctrl Pts',(-0.115254344789724,0.104461685875046,
-0.237354688200212));
#81177=CARTESIAN_POINT('Ctrl Pts',(-0.115303263032921,0.104407688139778,
-0.237349442265415));
#81178=CARTESIAN_POINT('Ctrl Pts',(-0.115400240900896,0.104300489165329,
-0.237339031225641));
#81179=CARTESIAN_POINT('Ctrl Pts',(-0.115448301721761,0.104247289027779,
-0.237333866172464));
#81180=CARTESIAN_POINT('Ctrl Pts',(-0.115544221827175,0.104140964154906,
-0.237323546735965));
#81181=CARTESIAN_POINT('Ctrl Pts',(-0.115592081296024,0.104087839608585,
-0.237318392362079));
#81182=CARTESIAN_POINT('Ctrl Pts',(-0.115688211050713,0.103980986438307,
-0.237308028344029));
#81183=CARTESIAN_POINT('Ctrl Pts',(-0.115736480577164,0.103927257157961,
-0.237302818669999));
#81184=CARTESIAN_POINT('Ctrl Pts',(-0.117098131177028,0.10240946549878,
-0.237155698925889));
#81185=CARTESIAN_POINT('Ctrl Pts',(-0.118383605708921,0.100920722324515,
-0.237012642916754));
#81186=CARTESIAN_POINT('Ctrl Pts',(-0.124009026173209,0.0941503677472277,
-0.236367264788718));
#81187=CARTESIAN_POINT('Ctrl Pts',(-0.12802564726391,0.0886111735369072,
-0.235852578010242));
#81188=CARTESIAN_POINT('Ctrl Pts',(-0.136232845254982,0.0755646620245248,
-0.234671654804108));
#81189=CARTESIAN_POINT('Ctrl Pts',(-0.14019241443196,0.0679373527464534,
-0.234001868060932));
#81190=CARTESIAN_POINT('Ctrl Pts',(-0.145400353804564,0.0554862429682903,
-0.232963939940484));
#81191=CARTESIAN_POINT('Ctrl Pts',(-0.147081964161305,0.0508614987340524,
-0.23258986046351));
#81192=CARTESIAN_POINT('Ctrl Pts',(-0.148894400814737,0.0450296775245204,
-0.232137950298299));
#81193=CARTESIAN_POINT('Ctrl Pts',(-0.149234053959582,0.0438909081540693,
-0.232050627790585));
#81194=CARTESIAN_POINT('Ctrl Pts',(-0.149753378550969,0.0420739822696501,
-0.231912881457015));
#81195=CARTESIAN_POINT('Ctrl Pts',(-0.149941562166702,0.0413983376266898,
-0.231862003485077));
#81196=CARTESIAN_POINT('Ctrl Pts',(-0.150296267755695,0.0400906663571473,
-0.231764226763451));
#81197=CARTESIAN_POINT('Ctrl Pts',(-0.150463385272501,0.0394588309787067,
-0.231717298211734));
#81198=CARTESIAN_POINT('Ctrl Pts',(-0.150866375972795,0.0378954156587527,
-0.231601915238833));
#81199=CARTESIAN_POINT('Ctrl Pts',(-0.151097613494102,0.0369626466520453,
-0.231533718070885));
#81200=CARTESIAN_POINT('Ctrl Pts',(-0.15157997871462,0.0349366646199434,
-0.231386862628883));
#81201=CARTESIAN_POINT('Ctrl Pts',(-0.151827958302424,0.033842750092484,
-0.231308365104121));
#81202=CARTESIAN_POINT('Ctrl Pts',(-0.154371560420178,0.0220309853340326,
-0.230468374167616));
#81203=CARTESIAN_POINT('Ctrl Pts',(-0.155540279718414,0.011100565239248,
-0.229756731682557));
#81204=CARTESIAN_POINT('Ctrl Pts',(-0.155549939620994,0.000137054387354205,
-0.229033329119584));
#81205=CARTESIAN_POINT('Ctrl Pts',(-0.155549939882158,0.000136757657850698,
-0.229033309540554));
#81206=CARTESIAN_POINT('Ctrl Pts',(-0.155557403485862,-0.0083524423307012,
-0.228473168697887));
#81207=CARTESIAN_POINT('Ctrl Pts',(-0.154869933188093,-0.0168271466045379,
-0.227908318305866));
#81208=CARTESIAN_POINT('Ctrl Pts',(-0.153243276817333,-0.0267340190266168,
-0.22721470303172));
#81209=CARTESIAN_POINT('Ctrl Pts',(-0.15296901012999,-0.0282611272572615,
-0.227106867729416));
#81210=CARTESIAN_POINT('Ctrl Pts',(-0.152453204345113,-0.0309051481942851,
-0.226918411679549));
#81211=CARTESIAN_POINT('Ctrl Pts',(-0.152222112306578,-0.0320239926151563,
-0.226838116476382));
#81212=CARTESIAN_POINT('Ctrl Pts',(-0.151733107294955,-0.0342665390317804,
-0.2266760134888));
#81213=CARTESIAN_POINT('Ctrl Pts',(-0.151474984114997,-0.0353901201575002,
-0.226594203765093));
#81214=CARTESIAN_POINT('Ctrl Pts',(-0.150955709809273,-0.0375406282955948,
-0.226436434284313));
#81215=CARTESIAN_POINT('Ctrl Pts',(-0.150696506976857,-0.0385679631268124,
-0.226360540991574));
#81216=CARTESIAN_POINT('Ctrl Pts',(-0.149985613206859,-0.0412689133903112,
-0.226159582701926));
#81217=CARTESIAN_POINT('Ctrl Pts',(-0.149516417080251,-0.0429377218322032,
-0.226033962908637));
#81218=CARTESIAN_POINT('Ctrl Pts',(-0.147647967485752,-0.0491809071161105,
-0.225558315230642));
#81219=CARTESIAN_POINT('Ctrl Pts',(-0.146065979461878,-0.0536973441504225,
-0.225202529143145));
#81220=CARTESIAN_POINT('Ctrl Pts',(-0.139888913410187,-0.0690279396012791,
-0.223953633819794));
#81221=CARTESIAN_POINT('Ctrl Pts',(-0.134279465761447,-0.079389786415519,
-0.223032841083095));
#81222=CARTESIAN_POINT('Ctrl Pts',(-0.125612159491976,-0.0918093520851595,
-0.221871110024715));
#81223=CARTESIAN_POINT('Ctrl Pts',(-0.123574478575888,-0.0945342439882163,
-0.221612471314857));
#81224=CARTESIAN_POINT('Ctrl Pts',(-0.120347638588512,-0.0985665013289709,
-0.22122626320443));
#81225=CARTESIAN_POINT('Ctrl Pts',(-0.119222955075185,-0.09992395591849,
-0.221095619837041));
#81226=CARTESIAN_POINT('Ctrl Pts',(-0.117538262149019,-0.10188837115776,
-0.220905977802767));
#81227=CARTESIAN_POINT('Ctrl Pts',(-0.116996153766251,-0.102510405967401,
-0.220845839183806));
#81228=CARTESIAN_POINT('Ctrl Pts',(-0.116031795710695,-0.103599329503717,
-0.220740449489436));
#81229=CARTESIAN_POINT('Ctrl Pts',(-0.115611629324614,-0.104068006141586,
-0.220695054914599));
#81230=CARTESIAN_POINT('Ctrl Pts',(-0.114670355893549,-0.10510521719659,
-0.220594519134982));
#81231=CARTESIAN_POINT('Ctrl Pts',(-0.114147853103979,-0.105672441541926,
-0.220539482272171));
#81232=CARTESIAN_POINT('Ctrl Pts',(-0.112580394799073,-0.107348867415279,
-0.220376566581818));
#81233=CARTESIAN_POINT('Ctrl Pts',(-0.111523299424275,-0.108446663233632,
-0.220269545700896));
#81234=CARTESIAN_POINT('Ctrl Pts',(-0.102194224272893,-0.117854217550899,
-0.219347532677652));
#81235=CARTESIAN_POINT('Ctrl Pts',(-0.0930221980872955,-0.125220719277211,
-0.218589637170017));
#81236=CARTESIAN_POINT('Ctrl Pts',(-0.0785111661517927,-0.134392610567397,
-0.217455164562992));
#81237=CARTESIAN_POINT('Ctrl Pts',(-0.0737652996666542,-0.137054919197883,
-0.217093281842978));
#81238=CARTESIAN_POINT('Ctrl Pts',(-0.0656320267208734,-0.141072478193257,
-0.21647742071298));
#81239=CARTESIAN_POINT('Ctrl Pts',(-0.0623188670872072,-0.142567045411504,
-0.216227710838994));
#81240=CARTESIAN_POINT('Ctrl Pts',(-0.0575372971903637,-0.144525479932043,
-0.215867086318529));
#81241=CARTESIAN_POINT('Ctrl Pts',(-0.0561095000501191,-0.145085763008879,
-0.215759378120908));
#81242=CARTESIAN_POINT('Ctrl Pts',(-0.0536049651461639,-0.146026070938215,
-0.215570273908284));
#81243=CARTESIAN_POINT('Ctrl Pts',(-0.052531877187648,-0.146415530034946,
-0.215489197142546));
#81244=CARTESIAN_POINT('Ctrl Pts',(-0.0502974488675162,-0.147198752444298,
-0.21532021353111));
#81245=CARTESIAN_POINT('Ctrl Pts',(-0.049135548228123,-0.147590663070567,
-0.215232252251104));
#81246=CARTESIAN_POINT('Ctrl Pts',(-0.0460916251194266,-0.148577455324181,
-0.215001514945841));
#81247=CARTESIAN_POINT('Ctrl Pts',(-0.0442027535375522,-0.149150306923946,
-0.214858036415914));
#81248=CARTESIAN_POINT('Ctrl Pts',(-0.034276544533934,-0.151955587125157,
-0.214102143810755));
#81249=CARTESIAN_POINT('Ctrl Pts',(-0.0260813924090781,-0.153574415346355,
-0.213470539638956));
#81250=CARTESIAN_POINT('Ctrl Pts',(-0.00939294721645679,-0.155496443600946,
-0.212176306844333));
#81251=CARTESIAN_POINT('Ctrl Pts',(-0.000923772004820798,-0.155777146693495,
-0.211515546075902));
#81252=CARTESIAN_POINT('Ctrl Pts',(0.010101252058171,-0.155243078568984,
-0.210672504753077));
#81253=CARTESIAN_POINT('Ctrl Pts',(0.0126729175716424,-0.155054337058813,
-0.210477167404917));
#81254=CARTESIAN_POINT('Ctrl Pts',(0.0170406186608072,-0.154624376046576,
-0.210148806440922));
#81255=CARTESIAN_POINT('Ctrl Pts',(0.0188392632569873,-0.15441555379036,
-0.21001457408816));
#81256=CARTESIAN_POINT('Ctrl Pts',(0.0214516866833292,-0.154065921958476,
-0.209821426830301));
#81257=CARTESIAN_POINT('Ctrl Pts',(0.0222685642728098,-0.153949973358863,
-0.209761291640913));
#81258=CARTESIAN_POINT('Ctrl Pts',(0.0237069678870701,-0.153734115796125,
-0.209655905590652));
#81259=CARTESIAN_POINT('Ctrl Pts',(0.0243288589255325,-0.153636927062771,
-0.209610511268554));
#81260=CARTESIAN_POINT('Ctrl Pts',(0.0257114010003854,-0.153412258696651,
-0.20950997314202));
#81261=CARTESIAN_POINT('Ctrl Pts',(0.0264717131956665,-0.153282894437996,
-0.209454933711705));
#81262=CARTESIAN_POINT('Ctrl Pts',(0.0287315571414647,-0.152881074107881,
-0.209292002426701));
#81263=CARTESIAN_POINT('Ctrl Pts',(0.0302281324291441,-0.15259222017744,
-0.209184968762462));
#81264=CARTESIAN_POINT('Ctrl Pts',(0.0432066406658109,-0.149888790417328,
-0.208262390664449));
#81265=CARTESIAN_POINT('Ctrl Pts',(0.0543871075947379,-0.146203925198292,
-0.207504017805518));
#81266=CARTESIAN_POINT('Ctrl Pts',(0.0699832823718536,-0.139023960870183,
-0.206369329884208));
#81267=CARTESIAN_POINT('Ctrl Pts',(0.074795790312722,-0.136495071689835,
-0.206007773205395));
#81268=CARTESIAN_POINT('Ctrl Pts',(0.0825877823424298,-0.131864509135969,
-0.205392399099184));
#81269=CARTESIAN_POINT('Ctrl Pts',(0.0856435118087766,-0.129900639144443,
-0.20514284075657));
#81270=CARTESIAN_POINT('Ctrl Pts',(0.0898877077246374,-0.126958079102895,
-0.204782396098733));
#81271=CARTESIAN_POINT('Ctrl Pts',(0.0911348435151286,-0.126065831426822,
-0.204674711698476));
#81272=CARTESIAN_POINT('Ctrl Pts',(0.0932870104334786,-0.124477464814844,
-0.204485634928572));
#81273=CARTESIAN_POINT('Ctrl Pts',(0.0941979615284775,-0.123789537039849,
-0.204404561525463));
#81274=CARTESIAN_POINT('Ctrl Pts',(0.0960716829542772,-0.122341890440374,
-0.204235571095911));
#81275=CARTESIAN_POINT('Ctrl Pts',(0.097033201752121,-0.121580689344235,
-0.204147599498362));
#81276=CARTESIAN_POINT('Ctrl Pts',(0.0995190138411277,-0.119564487308645,
-0.203916803451899));
#81277=CARTESIAN_POINT('Ctrl Pts',(0.101028545417739,-0.11829172874913,
-0.2037732758329));
#81278=CARTESIAN_POINT('Ctrl Pts',(0.108806358007299,-0.111476398101642,
-0.203015445949056));
#81279=CARTESIAN_POINT('Ctrl Pts',(0.114643112071185,-0.105464332792143,
-0.202381825626085));
#81280=CARTESIAN_POINT('Ctrl Pts',(0.125338765815816,-0.0925051439589563,
-0.201087160056976));
#81281=CARTESIAN_POINT('Ctrl Pts',(0.130171555052273,-0.0855708806996168,
-0.200428109296607));
#81282=CARTESIAN_POINT('Ctrl Pts',(0.135713906457741,-0.0760537205247465,
-0.199586974583617));
#81283=CARTESIAN_POINT('Ctrl Pts',(0.136954342961365,-0.0737966279380717,
-0.199391877921633));
#81284=CARTESIAN_POINT('Ctrl Pts',(0.13896982461374,-0.0699032364407014,
-0.199063874439057));
#81285=CARTESIAN_POINT('Ctrl Pts',(0.13977337725737,-0.0682823430078759,
-0.198929762072994));
#81286=CARTESIAN_POINT('Ctrl Pts',(0.140901889114958,-0.0659025063917623,
-0.198736753539964));
#81287=CARTESIAN_POINT('Ctrl Pts',(0.141249341834933,-0.0651544796425545,
-0.198676639442777));
#81288=CARTESIAN_POINT('Ctrl Pts',(0.141851440910951,-0.0638307713815762,
-0.198571275867086));
#81289=CARTESIAN_POINT('Ctrl Pts',(0.142108563670739,-0.063256263270361,
-0.198525883161269));
#81290=CARTESIAN_POINT('Ctrl Pts',(0.142673062062243,-0.0619741475840294,
-0.198425330856019));
#81291=CARTESIAN_POINT('Ctrl Pts',(0.142978669216799,-0.0612657965183183,
-0.198370275827079));
#81292=CARTESIAN_POINT('Ctrl Pts',(0.143872750261244,-0.0591503203956359,
-0.198207249253159));
#81293=CARTESIAN_POINT('Ctrl Pts',(0.144445832949263,-0.0577367341288294,
-0.198100137394947));
#81294=CARTESIAN_POINT('Ctrl Pts',(0.149243661986275,-0.0453834110946092,
-0.197177911628806));
#81295=CARTESIAN_POINT('Ctrl Pts',(0.152240098771118,-0.0340052756533205,
-0.196419897912158));
#81296=CARTESIAN_POINT('Ctrl Pts',(0.154711781701462,-0.0170180312739999,
-0.195285447231123));
#81297=CARTESIAN_POINT('Ctrl Pts',(0.155211901335296,-0.0116020601934807,
-0.194923730210237));
#81298=CARTESIAN_POINT('Ctrl Pts',(0.155571653530076,-0.00254151124503676,
-0.194308116600976));
#81299=CARTESIAN_POINT('Ctrl Pts',(0.15558856928531,0.00109195674468064,
-0.194058483745806));
#81300=CARTESIAN_POINT('Ctrl Pts',(0.155431737667368,0.006255341675108,
-0.193697950665079));
#81301=CARTESIAN_POINT('Ctrl Pts',(0.155362513388929,0.00778739452743881,
-0.19359025458497));
#81302=CARTESIAN_POINT('Ctrl Pts',(0.155202267414991,0.0104576196889015,
-0.193401164370465));
#81303=CARTESIAN_POINT('Ctrl Pts',(0.155121344088004,0.0115962969498585,
-0.193320089341715));
#81304=CARTESIAN_POINT('Ctrl Pts',(0.154927509288578,0.0139561140712787,
-0.193151102335572));
#81305=CARTESIAN_POINT('Ctrl Pts',(0.154812675239116,0.015177011601869,
-0.193063135854482));
#81306=CARTESIAN_POINT('Ctrl Pts',(0.15447533618745,0.0183594652606682,
-0.192832368840042));
#81307=CARTESIAN_POINT('Ctrl Pts',(0.15422990957344,0.0203183116072376,
-0.192688865464766));
#81308=CARTESIAN_POINT('Ctrl Pts',(0.152751053301781,0.0305404365768638,
-0.191931976267203));
#81309=CARTESIAN_POINT('Ctrl Pts',(0.150890823824713,0.0386978005737078,
-0.191299334524039));
#81310=CARTESIAN_POINT('Ctrl Pts',(0.145850529546059,0.0547248334167432,
-0.190004878172485));
#81311=CARTESIAN_POINT('Ctrl Pts',(0.142663486355955,0.0625644903227373,
-0.189344996716908));
#81312=CARTESIAN_POINT('Ctrl Pts',(0.137694367925235,0.0724065024140782,
-0.188502935737827));
#81313=CARTESIAN_POINT('Ctrl Pts',(0.136476130166284,0.0746773592631195,
-0.188307722077662));
#81314=CARTESIAN_POINT('Ctrl Pts',(0.134307119329309,0.07848996816095,-0.187979544826952));
#81315=CARTESIAN_POINT('Ctrl Pts',(0.133384833321598,0.0800472634360736,
-0.18784537413927));
#81316=CARTESIAN_POINT('Ctrl Pts',(0.13200286608517,0.0822904993063647,
-0.187652298192771));
#81317=CARTESIAN_POINT('Ctrl Pts',(0.131564610858871,0.0829893739089262,
-0.187592173859068));
#81318=CARTESIAN_POINT('Ctrl Pts',(0.130782178517708,0.084215321979754,
-0.187486799405406));
#81319=CARTESIAN_POINT('Ctrl Pts',(0.1304403358384,0.0847438346324271,-0.187441405944234));
#81320=CARTESIAN_POINT('Ctrl Pts',(0.129672446647997,0.0859153887086811,
-0.187340860633403));
#81321=CARTESIAN_POINT('Ctrl Pts',(0.129244814978104,0.0865573526913667,
-0.187285813258311));
#81322=CARTESIAN_POINT('Ctrl Pts',(0.127957761719587,0.0884586806772202,
-0.187122833303645));
#81323=CARTESIAN_POINT('Ctrl Pts',(0.127084551779746,0.0897086624777553,
-0.187015759680114));
#81324=CARTESIAN_POINT('Ctrl Pts',(0.119334929603154,0.100461770633756,
-0.186093360613191));
#81325=CARTESIAN_POINT('Ctrl Pts',(0.11142140059385,0.109173010098291,-0.185335170467301));
#81326=CARTESIAN_POINT('Ctrl Pts',(0.102515838399332,0.116988540786228,
-0.184552126385709));
#81327=CARTESIAN_POINT('Ctrl Pts',(0.10242908212953,0.117064507564331,-0.184544504392145));
#81328=CARTESIAN_POINT('Ctrl Pts',(0.102342242826532,0.117140376613853,
-0.184536881298507));
#81329=CARTESIAN_POINT('Origin',(0.,0.,-1.10400562256037));
#81330=CARTESIAN_POINT('',(0.10234224283772,0.117140376604078,-0.100698721018058));
#81331=CARTESIAN_POINT('',(0.102342241743611,0.11714037755997,-0.114635995609957));
#81332=CARTESIAN_POINT('',(0.10234224283772,0.117140376604078,-1.10400562256037));
#81333=CARTESIAN_POINT('',(-0.155549976200755,-8.60461765890906E-5,-0.145194377445451));
#81334=CARTESIAN_POINT('Ctrl Pts',(-0.15554997620071,-8.60462574926153E-5,
-0.145194377439629));
#81335=CARTESIAN_POINT('Ctrl Pts',(-0.155547169018751,-0.00516072468918725,
-0.144829200911433));
#81336=CARTESIAN_POINT('Ctrl Pts',(-0.155296045436501,-0.010228371777148,
-0.144464024383237));
#81337=CARTESIAN_POINT('Ctrl Pts',(-0.154798544359905,-0.0152713183469712,
-0.144098847855041));
#81338=CARTESIAN_POINT('Ctrl Pts',(-0.153793713525852,-0.0254568404417424,
-0.143361280334756));
#81339=CARTESIAN_POINT('Ctrl Pts',(-0.151775550772244,-0.0355806132571192,
-0.142623712814471));
#81340=CARTESIAN_POINT('Ctrl Pts',(-0.148768856287275,-0.0454271933865166,
-0.141886145294187));
#81341=CARTESIAN_POINT('Ctrl Pts',(-0.145755023185923,-0.0552971516671018,
-0.141146826611084));
#81342=CARTESIAN_POINT('Ctrl Pts',(-0.141748088156632,-0.0648876693193305,
-0.140407507927983));
#81343=CARTESIAN_POINT('Ctrl Pts',(-0.13682468791801,-0.0739919406161174,
-0.13966818924488));
#81344=CARTESIAN_POINT('Ctrl Pts',(-0.13192416200287,-0.083053913087579,
-0.13893230546731));
#81345=CARTESIAN_POINT('Ctrl Pts',(-0.126116108676144,-0.091633325525222,
-0.138196421689739));
#81346=CARTESIAN_POINT('Ctrl Pts',(-0.119522825148394,-0.0995494689516038,
-0.137460537912168));
#81347=CARTESIAN_POINT('Ctrl Pts',(-0.112883378136513,-0.107521037987988,
-0.1367195017763));
#81348=CARTESIAN_POINT('Ctrl Pts',(-0.105448260210238,-0.114819275876618,
-0.135978465640433));
#81349=CARTESIAN_POINT('Ctrl Pts',(-0.0973821576493404,-0.121295168376811,
-0.135237429504565));
#81350=CARTESIAN_POINT('Ctrl Pts',(-0.0893160550884423,-0.127771060877005,
-0.134496393368697));
#81351=CARTESIAN_POINT('Ctrl Pts',(-0.0806197845170057,-0.133424117721121,
-0.133755357232829));
#81352=CARTESIAN_POINT('Ctrl Pts',(-0.0714869563426234,-0.138149982167454,
-0.133014321096961));
#81353=CARTESIAN_POINT('Ctrl Pts',(-0.0623968021115963,-0.142853764596275,
-0.132276747517651));
#81354=CARTESIAN_POINT('Ctrl Pts',(-0.0528066258091951,-0.146673991821844,
-0.131539173938341));
#81355=CARTESIAN_POINT('Ctrl Pts',(-0.0429106352096175,-0.149514146106337,
-0.130801600359031));
#81356=CARTESIAN_POINT('Ctrl Pts',(-0.0329912509565894,-0.152361014381149,
-0.130062283190685));
#81357=CARTESIAN_POINT('Ctrl Pts',(-0.0227654554255227,-0.154222772693214,
-0.129322966022339));
#81358=CARTESIAN_POINT('Ctrl Pts',(-0.0124484318150597,-0.155051085276259,
-0.128583648853993));
#81359=CARTESIAN_POINT('Ctrl Pts',(-0.00217923318024209,-0.155875558183192,
-0.127847758819955));
#81360=CARTESIAN_POINT('Ctrl Pts',(0.00817942026916348,-0.155676067402559,
-0.127111868785917));
#81361=CARTESIAN_POINT('Ctrl Pts',(0.0184093627804832,-0.154456783153141,
-0.126375978751879));
#81362=CARTESIAN_POINT('Ctrl Pts',(0.0287107685240648,-0.153228981358937,
-0.12563494801638));
#81363=CARTESIAN_POINT('Ctrl Pts',(0.0388807135570937,-0.150967182408244,
-0.12489391728088));
#81364=CARTESIAN_POINT('Ctrl Pts',(0.0487045426096044,-0.147728365689157,
-0.12415288654538));
#81365=CARTESIAN_POINT('Ctrl Pts',(0.058528371662115,-0.14448954897007,
-0.12341185580988));
#81366=CARTESIAN_POINT('Ctrl Pts',(0.0680052289217426,-0.140274132387235,
-0.12267082507438));
#81367=CARTESIAN_POINT('Ctrl Pts',(0.0769421623588443,-0.135187670116565,
-0.121929794338881));
#81368=CARTESIAN_POINT('Ctrl Pts',(0.0858370381162951,-0.130125145005352,
-0.121192250933068));
#81369=CARTESIAN_POINT('Ctrl Pts',(0.094263193245769,-0.124162160084575,
-0.120454707527255));
#81370=CARTESIAN_POINT('Ctrl Pts',(0.102033927875157,-0.117409028879244,
-0.119717164121442));
#81371=CARTESIAN_POINT('Ctrl Pts',(0.109823430288772,-0.11063958759316,
-0.118977839409722));
#81372=CARTESIAN_POINT('Ctrl Pts',(0.116953545084801,-0.103076675214026,
-0.118238514698002));
#81373=CARTESIAN_POINT('Ctrl Pts',(0.123266536901705,-0.0948744611592639,
-0.117499189986282));
#81374=CARTESIAN_POINT('Ctrl Pts',(0.12954994540641,-0.0867106835014012,
-0.116763329824239));
#81375=CARTESIAN_POINT('Ctrl Pts',(0.135023300833802,-0.0779143198630106,
-0.116027469662196));
#81376=CARTESIAN_POINT('Ctrl Pts',(0.139571306722132,-0.068670611180305,
-0.115291609500154));
#81377=CARTESIAN_POINT('Ctrl Pts',(0.144151431740859,-0.0593616211651135,
-0.114550552513595));
#81378=CARTESIAN_POINT('Ctrl Pts',(0.147792654371947,-0.0495997892919083,
-0.113809495527036));
#81379=CARTESIAN_POINT('Ctrl Pts',(0.150425869185099,-0.0395962167373015,
-0.113068438540477));
#81380=CARTESIAN_POINT('Ctrl Pts',(0.153059083998252,-0.0295926441826946,
-0.112327381553918));
#81381=CARTESIAN_POINT('Ctrl Pts',(0.154684175489864,-0.0193482767603506,
-0.11158632456736));
#81382=CARTESIAN_POINT('Ctrl Pts',(0.155284614072203,-0.00908246290644956,
-0.110845267580801));
#81383=CARTESIAN_POINT('Ctrl Pts',(0.155882256621659,0.00113554663581544,
-0.110107661437948));
#81384=CARTESIAN_POINT('Ctrl Pts',(0.155469251660693,0.0114507651553898,
-0.109370055295096));
#81385=CARTESIAN_POINT('Ctrl Pts',(0.154036462806462,0.0216464922348542,
-0.108632449152243));
#81386=CARTESIAN_POINT('Ctrl Pts',(0.152605995913413,0.0318256962359578,
-0.107896038365445));
#81387=CARTESIAN_POINT('Ctrl Pts',(0.150159064761957,0.0418848710726706,
-0.107159627578647));
#81388=CARTESIAN_POINT('Ctrl Pts',(0.146738469077704,0.0516103109148915,
-0.106423216791849));
#81389=CARTESIAN_POINT('Ctrl Pts',(0.143321329611764,0.0613259240349885,
-0.105687550084937));
#81390=CARTESIAN_POINT('Ctrl Pts',(0.138932767306006,0.0707075924762563,
-0.104951883378026));
#81391=CARTESIAN_POINT('Ctrl Pts',(0.133665088257766,0.0795578197353582,
-0.104216216671114));
#81392=CARTESIAN_POINT('Ctrl Pts',(0.128388725433959,0.0884226366052783,
-0.103479337216707));
#81393=CARTESIAN_POINT('Ctrl Pts',(0.122230843509559,0.0967534740597384,
-0.102742457762299));
#81394=CARTESIAN_POINT('Ctrl Pts',(0.115328226724701,0.104380087279787,
-0.102005578307892));
#81395=CARTESIAN_POINT('Ctrl Pts',(0.11124762484323,0.108888692237149,-0.101569959211281));
#81396=CARTESIAN_POINT('Ctrl Pts',(0.106907560372334,0.11315178744888,-0.101134340114669));
#81397=CARTESIAN_POINT('Ctrl Pts',(0.10234224283772,0.117140376604078,-0.100698721018058));
#81398=CARTESIAN_POINT('Ctrl Pts',(0.10234224283772,0.117140376604078,-0.170697633677947));
#81399=CARTESIAN_POINT('Ctrl Pts',(0.0945586197976017,0.123940708500068,
-0.169959344960156));
#81400=CARTESIAN_POINT('Ctrl Pts',(0.0861005207429198,0.129956556556732,
-0.169221056242365));
#81401=CARTESIAN_POINT('Ctrl Pts',(0.0771519734397198,0.135068040240305,
-0.168482767524574));
#81402=CARTESIAN_POINT('Ctrl Pts',(0.0682034261365199,0.140179523923879,
-0.167744478806783));
#81403=CARTESIAN_POINT('Ctrl Pts',(0.05876529787386,0.144386293971583,-0.167006190088992));
#81404=CARTESIAN_POINT('Ctrl Pts',(0.049042847800632,0.147616400103796,
-0.166267901371201));
#81405=CARTESIAN_POINT('Ctrl Pts',(0.0393299004762808,0.15084334912158,
-0.16553033425879));
#81406=CARTESIAN_POINT('Ctrl Pts',(0.0292610015856663,0.153119533717959,
-0.16479276714638));
#81407=CARTESIAN_POINT('Ctrl Pts',(0.0190430417864429,0.154379937360785,
-0.164055200033969));
#81408=CARTESIAN_POINT('Ctrl Pts',(0.00880081501473634,0.155643334378132,
-0.163315881248898));
#81409=CARTESIAN_POINT('Ctrl Pts',(-0.00159027922619605,0.155885859586032,
-0.162576562463828));
#81410=CARTESIAN_POINT('Ctrl Pts',(-0.011910146200751,0.155093361938791,
-0.161837243678757));
#81411=CARTESIAN_POINT('Ctrl Pts',(-0.0221820614633852,0.154304546666426,
-0.161101360170661));
#81412=CARTESIAN_POINT('Ctrl Pts',(-0.0323824797595626,0.152490373977825,
-0.160365476662565));
#81413=CARTESIAN_POINT('Ctrl Pts',(-0.0422965644458576,0.149689021428017,
-0.159629593154469));
#81414=CARTESIAN_POINT('Ctrl Pts',(-0.0522800710443302,0.146868052821171,
-0.158888556730911));
#81415=CARTESIAN_POINT('Ctrl Pts',(-0.0619723009048204,0.143046271088191,
-0.158147520307353));
#81416=CARTESIAN_POINT('Ctrl Pts',(-0.0711701194738238,0.138313472207452,
-0.157406483883795));
#81417=CARTESIAN_POINT('Ctrl Pts',(-0.0803679380428271,0.133580673326713,
-0.156665447460237));
#81418=CARTESIAN_POINT('Ctrl Pts',(-0.0890705651706336,0.127937403751066,
-0.155924411036679));
#81419=CARTESIAN_POINT('Ctrl Pts',(-0.0971038891700634,0.121518053012909,
-0.155183374613121));
#81420=CARTESIAN_POINT('Ctrl Pts',(-0.105000973143479,0.115207570348742,
-0.154454905692334));
#81421=CARTESIAN_POINT('Ctrl Pts',(-0.112313136123349,0.108097583610356,
-0.153726436771547));
#81422=CARTESIAN_POINT('Ctrl Pts',(-0.11887533097625,0.100321773236357,
-0.15299796785076));
#81423=CARTESIAN_POINT('Ctrl Pts',(-0.125427954384414,0.0925573044547588,
-0.152270561455572));
#81424=CARTESIAN_POINT('Ctrl Pts',(-0.131232096894198,0.0841295966894995,
-0.151543155060384));
#81425=CARTESIAN_POINT('Ctrl Pts',(-0.136159342815408,0.0752092804384954,
-0.150815748665196));
#81426=CARTESIAN_POINT('Ctrl Pts',(-0.141082092447257,0.0662971042973398,
-0.150089006054542));
#81427=CARTESIAN_POINT('Ctrl Pts',(-0.145129060671767,0.0568940369707911,
-0.149362263443888));
#81428=CARTESIAN_POINT('Ctrl Pts',(-0.14821697669958,0.0471967193567106,
-0.148635520833233));
#81429=CARTESIAN_POINT('Ctrl Pts',(-0.151310928033582,0.0374804484160237,
-0.147907357810192));
#81430=CARTESIAN_POINT('Ctrl Pts',(-0.153441825858717,0.0274696985169037,
-0.147179194787151));
#81431=CARTESIAN_POINT('Ctrl Pts',(-0.154576475344867,0.0173757235808376,
-0.14645103176411));
#81432=CARTESIAN_POINT('Ctrl Pts',(-0.155229196476361,0.0115690398234625,
-0.146032146991224));
#81433=CARTESIAN_POINT('Ctrl Pts',(-0.155553196245258,0.0057349892904951,
-0.145613262218337));
#81434=CARTESIAN_POINT('Ctrl Pts',(-0.155549976200755,-8.60461765879318E-5,
-0.145194377445451));
#81435=CARTESIAN_POINT('Ctrl Pts',(0.102342242826532,0.117140376613853,
-0.184536881298507));
#81436=CARTESIAN_POINT('Ctrl Pts',(0.0983366947192182,0.120639911009267,
-0.184185258620294));
#81437=CARTESIAN_POINT('Ctrl Pts',(0.0941544952938237,0.123931513579687,
-0.18383113563115));
#81438=CARTESIAN_POINT('Ctrl Pts',(0.0868465589662623,0.129099457452717,
-0.183223466831916));
#81439=CARTESIAN_POINT('Ctrl Pts',(0.0838087104185499,0.131091919577572,
-0.18297387024936));
#81440=CARTESIAN_POINT('Ctrl Pts',(0.0793931506215579,0.133771752444894,
-0.182613380228226));
#81441=CARTESIAN_POINT('Ctrl Pts',(0.0780705466443553,0.134547922952287,
-0.182505689851712));
#81442=CARTESIAN_POINT('Ctrl Pts',(0.0757437695338512,0.135867534636086,
-0.182316606225206));
#81443=CARTESIAN_POINT('Ctrl Pts',(0.0747446708265066,0.136419718694302,
-0.182235532013308));
#81444=CARTESIAN_POINT('Ctrl Pts',(0.0726598507195555,0.137542184176541,
-0.182066543407407));
#81445=CARTESIAN_POINT('Ctrl Pts',(0.0715732851402894,0.138110720186298,
-0.181978574477041));
#81446=CARTESIAN_POINT('Ctrl Pts',(0.0687201973730012,0.139560863240983,
-0.18174779347322));
#81447=CARTESIAN_POINT('Ctrl Pts',(0.0669434637725879,0.140421764952022,
-0.181604278399122));
#81448=CARTESIAN_POINT('Ctrl Pts',(0.0575588653788898,0.144750410347913,
-0.180846929836045));
#81449=CARTESIAN_POINT('Ctrl Pts',(0.0496981348061524,0.147633863069435,
-0.180213810080176));
#81450=CARTESIAN_POINT('Ctrl Pts',(0.0347126592904053,0.151797900082725,
-0.179015456334295));
#81451=CARTESIAN_POINT('Ctrl Pts',(0.0276550827633492,0.153240876802733,
-0.178454710886467));
#81452=CARTESIAN_POINT('Ctrl Pts',(0.0156657943747679,0.154836675342816,
-0.177524870698505));
#81453=CARTESIAN_POINT('Ctrl Pts',(0.0107801874139766,0.155253376498215,
-0.177152336470884));
#81454=CARTESIAN_POINT('Ctrl Pts',(0.00472708396739653,0.155482456483989,
-0.176704406392737));
#81455=CARTESIAN_POINT('Ctrl Pts',(0.00357108416457462,0.155513302215766,
-0.176619478851091));
#81456=CARTESIAN_POINT('Ctrl Pts',(0.00172046394156059,0.155542035241058,
-0.176484616137419));
#81457=CARTESIAN_POINT('Ctrl Pts',(0.00102604211302602,0.155548166209317,
-0.176434257596174));
#81458=CARTESIAN_POINT('Ctrl Pts',(-0.000318162992916625,0.155551031645879,
-0.176337285112024));
#81459=CARTESIAN_POINT('Ctrl Pts',(-0.000967919269937373,0.155548345629575,
-0.176290643048398));
#81460=CARTESIAN_POINT('Ctrl Pts',(-0.00243424900611269,0.155533095634588,
-0.176185871312739));
#81461=CARTESIAN_POINT('Ctrl Pts',(-0.00325079182791444,0.155518172041095,
-0.176127868452708));
#81462=CARTESIAN_POINT('Ctrl Pts',(-0.00618614913599467,0.155441394310472,
-0.175920457760872));
#81463=CARTESIAN_POINT('Ctrl Pts',(-0.00830387491257301,0.155342660882586,
-0.175772883948787));
#81464=CARTESIAN_POINT('Ctrl Pts',(-0.0200681731245363,0.154552890995048,
-0.174961265175642));
#81465=CARTESIAN_POINT('Ctrl Pts',(-0.0296369762449393,0.153006601822503,
-0.174330769129431));
#81466=CARTESIAN_POINT('Ctrl Pts',(-0.0471386380210022,0.148473613491827,
-0.173138717343726));
#81467=CARTESIAN_POINT('Ctrl Pts',(-0.0550910692268391,0.14571003948883,
-0.172580904087223));
#81468=CARTESIAN_POINT('Ctrl Pts',(-0.0649829478118983,0.141346425787419,
-0.171836835981849));
#81469=CARTESIAN_POINT('Ctrl Pts',(-0.0671621333761477,0.140324061935305,
-0.171669683799163));
#81470=CARTESIAN_POINT('Ctrl Pts',(-0.0704945267629355,0.138665263978037,
-0.171408504112053));
#81471=CARTESIAN_POINT('Ctrl Pts',(-0.0716649068496607,0.138064023826466,
-0.17131568688325));
#81472=CARTESIAN_POINT('Ctrl Pts',(-0.0738214192480146,0.136921385507045,
-0.171142554245235));
#81473=CARTESIAN_POINT('Ctrl Pts',(-0.0748095846125761,0.136383993481202,
-0.17106238388637));
#81474=CARTESIAN_POINT('Ctrl Pts',(-0.0769950265987758,0.135164591590456,
-0.170883156048896));
#81475=CARTESIAN_POINT('Ctrl Pts',(-0.0781892312990778,0.134477302263918,
-0.170783915213729));
#81476=CARTESIAN_POINT('Ctrl Pts',(-0.0812078041497835,0.132686251089956,
-0.170529638504634));
#81477=CARTESIAN_POINT('Ctrl Pts',(-0.0830188421547394,0.131560707291047,
-0.170373831268357));
#81478=CARTESIAN_POINT('Ctrl Pts',(-0.0938167285571004,0.124538175138603,
-0.169424580496919));
#81479=CARTESIAN_POINT('Ctrl Pts',(-0.102194137706582,0.117760838976589,
-0.168598645922293));
#81480=CARTESIAN_POINT('Ctrl Pts',(-0.114105183857023,0.105889905119983,
-0.167295493259657));
#81481=CARTESIAN_POINT('Ctrl Pts',(-0.11815117015547,0.101355676680991,
-0.16682461843477));
#81482=CARTESIAN_POINT('Ctrl Pts',(-0.123907203235406,0.0940905308038684,
-0.166120131438881));
#81483=CARTESIAN_POINT('Ctrl Pts',(-0.125814956920619,0.0915238935001316,
-0.165879952406257));
#81484=CARTESIAN_POINT('Ctrl Pts',(-0.128224288826043,0.0880645836709176,
-0.165569245734799));
#81485=CARTESIAN_POINT('Ctrl Pts',(-0.128797990164475,0.0872233742701828,
-0.165494670041611));
#81486=CARTESIAN_POINT('Ctrl Pts',(-0.129732545586649,0.0858237205618625,
-0.165372272970573));
#81487=CARTESIAN_POINT('Ctrl Pts',(-0.13009814506523,0.0852685000675042,
-0.165324152084376));
#81488=CARTESIAN_POINT('Ctrl Pts',(-0.130832673815881,0.0841372794266802,
-0.165227008930521));
#81489=CARTESIAN_POINT('Ctrl Pts',(-0.131201383551625,0.0835611592153828,
-0.165178000553216));
#81490=CARTESIAN_POINT('Ctrl Pts',(-0.132157477900669,0.0820453020307706,
-0.165050214847673));
#81491=CARTESIAN_POINT('Ctrl Pts',(-0.132738654331504,0.0811016669485627,
-0.164971826779628));
#81492=CARTESIAN_POINT('Ctrl Pts',(-0.135270554436817,0.0768905748567535,
-0.164626739381644));
#81493=CARTESIAN_POINT('Ctrl Pts',(-0.137111243809965,0.0735581110413254,
-0.164366137841692));
#81494=CARTESIAN_POINT('Ctrl Pts',(-0.142594652787796,0.0627080842823455,
-0.163545835545655));
#81495=CARTESIAN_POINT('Ctrl Pts',(-0.14575522831244,0.0549633442823664,
-0.163001376773668));
#81496=CARTESIAN_POINT('Ctrl Pts',(-0.150411519134649,0.0402739491853991,
-0.16198375661037));
#81497=CARTESIAN_POINT('Ctrl Pts',(-0.152083594010951,0.0334093009859926,
-0.161513883427001));
#81498=CARTESIAN_POINT('Ctrl Pts',(-0.153749516730865,0.0237568362296076,
-0.160842542147919));
#81499=CARTESIAN_POINT('Ctrl Pts',(-0.154143883005944,0.021046685002819,
-0.160652972335974));
#81500=CARTESIAN_POINT('Ctrl Pts',(-0.15462916250251,0.0169567259175699,
-0.160364502469057));
#81501=CARTESIAN_POINT('Ctrl Pts',(-0.154773563675264,0.0155837165186166,
-0.160267263016903));
#81502=CARTESIAN_POINT('Ctrl Pts',(-0.155002427330546,0.0130887562095317,
-0.160089748022903));
#81503=CARTESIAN_POINT('Ctrl Pts',(-0.155093030031646,0.0119674530359494,
-0.160009669716657));
#81504=CARTESIAN_POINT('Ctrl Pts',(-0.155263041862571,0.00953497045006591,
-0.159835257996851));
#81505=CARTESIAN_POINT('Ctrl Pts',(-0.155338019722236,0.00822357972594806,
-0.159740792791224));
#81506=CARTESIAN_POINT('Ctrl Pts',(-0.15549986499489,0.00458465720597244,
-0.159477375803979));
#81507=CARTESIAN_POINT('Ctrl Pts',(-0.155551073925404,0.0022559733692135,
-0.159307339306242));
#81508=CARTESIAN_POINT('Ctrl Pts',(-0.155546231361191,-0.00808099791623698,
-0.158545639796813));
#81509=CARTESIAN_POINT('Ctrl Pts',(-0.154924079204671,-0.0160756561186006,
-0.157937240778656));
#81510=CARTESIAN_POINT('Ctrl Pts',(-0.152324000699988,-0.0327357129707682,
-0.156636655028277));
#81511=CARTESIAN_POINT('Ctrl Pts',(-0.150213702579628,-0.0413530871017355,
-0.155944636559827));
#81512=CARTESIAN_POINT('Ctrl Pts',(-0.146383187404494,-0.052702095370091,
-0.155034449418541));
#81513=CARTESIAN_POINT('Ctrl Pts',(-0.145295929628231,-0.0556295287590152,
-0.154799915407875));
#81514=CARTESIAN_POINT('Ctrl Pts',(-0.143730082186628,-0.0594856849865002,
-0.154492999322737));
#81515=CARTESIAN_POINT('Ctrl Pts',(-0.143329297992639,-0.0604449810732597,
-0.154416819284242));
#81516=CARTESIAN_POINT('Ctrl Pts',(-0.142680896754708,-0.0619542394754681,
-0.154297316600963));
#81517=CARTESIAN_POINT('Ctrl Pts',(-0.142439656757601,-0.06250688205075,
-0.15425363362081));
#81518=CARTESIAN_POINT('Ctrl Pts',(-0.14192674836047,-0.0636634835104297,
-0.154162390320878));
#81519=CARTESIAN_POINT('Ctrl Pts',(-0.141654426030723,-0.0642671350459861,
-0.154114873846387));
#81520=CARTESIAN_POINT('Ctrl Pts',(-0.140958855831596,-0.0657830893378421,
-0.153995766082405));
#81521=CARTESIAN_POINT('Ctrl Pts',(-0.140530590315446,-0.0666930821503648,
-0.153924470699154));
#81522=CARTESIAN_POINT('Ctrl Pts',(-0.138753682158606,-0.0703755880718805,
-0.15363652308691));
#81523=CARTESIAN_POINT('Ctrl Pts',(-0.137331480573935,-0.0731120735731565,
-0.153423859740469));
#81524=CARTESIAN_POINT('Ctrl Pts',(-0.133047980982116,-0.0807873563138952,
-0.152825987949667));
#81525=CARTESIAN_POINT('Ctrl Pts',(-0.129994928632779,-0.0856136096135604,
-0.152448241417963));
#81526=CARTESIAN_POINT('Ctrl Pts',(-0.120109523062564,-0.099487927750899,
-0.151324800387112));
#81527=CARTESIAN_POINT('Ctrl Pts',(-0.112548242317941,-0.107967611537955,
-0.150584138550943));
#81528=CARTESIAN_POINT('Ctrl Pts',(-0.102427970050515,-0.11708794011791,
-0.149645511104979));
#81529=CARTESIAN_POINT('Ctrl Pts',(-0.100688527489477,-0.118587074619857,
-0.149485929661597));
#81530=CARTESIAN_POINT('Ctrl Pts',(-0.0979083465090845,-0.120877892989764,
-0.149233102559626));
#81531=CARTESIAN_POINT('Ctrl Pts',(-0.0968896782928011,-0.121695930027374,
-0.149140919895653));
#81532=CARTESIAN_POINT('Ctrl Pts',(-0.0949745517298871,-0.123194576095098,
-0.148968371894081));
#81533=CARTESIAN_POINT('Ctrl Pts',(-0.0940807706626771,-0.123878478863977,
-0.148888143909745));
#81534=CARTESIAN_POINT('Ctrl Pts',(-0.0920671148726055,-0.12538492488059,
-0.14870800729064));
#81535=CARTESIAN_POINT('Ctrl Pts',(-0.0909434940087749,-0.126202272937342,
-0.148607906154514));
#81536=CARTESIAN_POINT('Ctrl Pts',(-0.0875347503410679,-0.128612710226155,
-0.148305366956385));
#81537=CARTESIAN_POINT('Ctrl Pts',(-0.0852177466115496,-0.13015950053001,
-0.148101222246312));
#81538=CARTESIAN_POINT('Ctrl Pts',(-0.0775859401064273,-0.134963213971767,
-0.147433147069885));
#81539=CARTESIAN_POINT('Ctrl Pts',(-0.0721171409500961,-0.137962851490374,
-0.146960734050542));
#81540=CARTESIAN_POINT('Ctrl Pts',(-0.0573195635495639,-0.144958697470478,
-0.145702817273616));
#81541=CARTESIAN_POINT('Ctrl Pts',(-0.0477539703036574,-0.148385024339524,
-0.144908331901771));
#81542=CARTESIAN_POINT('Ctrl Pts',(-0.0350582461855507,-0.151576540388081,
-0.143915129893144));
#81543=CARTESIAN_POINT('Ctrl Pts',(-0.0321732767323222,-0.15221501657956,
-0.143693517212808));
#81544=CARTESIAN_POINT('Ctrl Pts',(-0.0282705475958293,-0.152962798246914,
-0.143400632601761));
#81545=CARTESIAN_POINT('Ctrl Pts',(-0.0272675433671392,-0.153144777042819,
-0.143325969967749));
#81546=CARTESIAN_POINT('Ctrl Pts',(-0.0256722250033197,-0.15341805096287,
-0.143208256255142));
#81547=CARTESIAN_POINT('Ctrl Pts',(-0.0250810693659445,-0.153515802085592,
-0.143164862627774));
#81548=CARTESIAN_POINT('Ctrl Pts',(-0.0238313213776839,-0.153715043599704,
-0.14307362265189));
#81549=CARTESIAN_POINT('Ctrl Pts',(-0.0231726129600604,-0.153815722700847,
-0.143025824853917));
#81550=CARTESIAN_POINT('Ctrl Pts',(-0.0214982998290823,-0.15406063027223,
-0.142905026755961));
#81551=CARTESIAN_POINT('Ctrl Pts',(-0.0204818549719584,-0.154199054670654,
-0.142832340131764));
#81552=CARTESIAN_POINT('Ctrl Pts',(-0.0162211543859929,-0.15473642265913,
-0.142530078814524));
#81553=CARTESIAN_POINT('Ctrl Pts',(-0.0129658583984935,-0.155043144152888,
-0.142305009129716));
#81554=CARTESIAN_POINT('Ctrl Pts',(-0.00340403136016302,-0.15564076473401,
-0.141654694293588));
#81555=CARTESIAN_POINT('Ctrl Pts',(0.00291356860509002,-0.155650755101249,
-0.141238549804585));
#81556=CARTESIAN_POINT('Ctrl Pts',(0.0195895207723907,-0.15466114369056,
-0.140138000042312));
#81557=CARTESIAN_POINT('Ctrl Pts',(0.0298753262041725,-0.153007359109028,
-0.139455320127346));
#81558=CARTESIAN_POINT('Ctrl Pts',(0.0419928269420551,-0.149789884614514,
-0.138592190486371));
#81559=CARTESIAN_POINT('Ctrl Pts',(0.0440550760486813,-0.149196369140589,
-0.138443260984368));
#81560=CARTESIAN_POINT('Ctrl Pts',(0.0474240356535321,-0.148150844650158,
-0.138196205313304));
#81561=CARTESIAN_POINT('Ctrl Pts',(0.048738209523348,-0.14772372403685,
-0.138098879799304));
#81562=CARTESIAN_POINT('Ctrl Pts',(0.0511116894266629,-0.146917199092269,
-0.137921274174827));
#81563=CARTESIAN_POINT('Ctrl Pts',(0.0521729122818032,-0.146543697538566,
-0.137841192287007));
#81564=CARTESIAN_POINT('Ctrl Pts',(0.0544632509303803,-0.145709572541708,
-0.137666849689987));
#81565=CARTESIAN_POINT('Ctrl Pts',(0.055690766025367,-0.145244840242195,
-0.137572458014198));
#81566=CARTESIAN_POINT('Ctrl Pts',(0.0591372624536412,-0.143889897789063,
-0.137304655600798));
#81567=CARTESIAN_POINT('Ctrl Pts',(0.0613417220724725,-0.142964018066949,
-0.137130073371118));
#81568=CARTESIAN_POINT('Ctrl Pts',(0.0710783574435325,-0.138607947421825,
-0.136343727067144));
#81569=CARTESIAN_POINT('Ctrl Pts',(0.0783499054799438,-0.134631161074682,
-0.135714064036659));
#81570=CARTESIAN_POINT('Ctrl Pts',(0.0931289925420109,-0.124944375660826,
-0.134349826740864));
#81571=CARTESIAN_POINT('Ctrl Pts',(0.100505516059808,-0.119091395922819,
-0.133615163624594));
#81572=CARTESIAN_POINT('Ctrl Pts',(0.10907910426226,-0.110921283305335,
-0.132721328145162));
#81573=CARTESIAN_POINT('Ctrl Pts',(0.110809459217712,-0.109192708096999,
-0.132538696024852));
#81574=CARTESIAN_POINT('Ctrl Pts',(0.113155733713252,-0.106735599745172,
-0.132288742941705));
#81575=CARTESIAN_POINT('Ctrl Pts',(0.113806708964276,-0.106041225199133,
-0.13221913552374));
#81576=CARTESIAN_POINT('Ctrl Pts',(0.11488837918105,-0.104866006860694,
-0.132103102618546));
#81577=CARTESIAN_POINT('Ctrl Pts',(0.115322521650834,-0.10438838599056,
-0.132056428871857));
#81578=CARTESIAN_POINT('Ctrl Pts',(0.116222930309442,-0.103385329676926,
-0.131959434366982));
#81579=CARTESIAN_POINT('Ctrl Pts',(0.11668862935952,-0.102859417420478,
-0.13190915381113));
#81580=CARTESIAN_POINT('Ctrl Pts',(0.117935853602077,-0.101431558885703,
-0.131774124317263));
#81581=CARTESIAN_POINT('Ctrl Pts',(0.118710607275242,-0.100523721833283,
-0.131689848399715));
#81582=CARTESIAN_POINT('Ctrl Pts',(0.123066776400221,-0.0952986612445279,
-0.131213086612784));
#81583=CARTESIAN_POINT('Ctrl Pts',(0.126423459789405,-0.0907986245009861,
-0.130834226990511));
#81584=CARTESIAN_POINT('Ctrl Pts',(0.135994531210639,-0.0764042139687098,
-0.129683017404976));
#81585=CARTESIAN_POINT('Ctrl Pts',(0.141343742329626,-0.0659853346916232,
-0.1289290866551));
#81586=CARTESIAN_POINT('Ctrl Pts',(0.146854097051682,-0.0514277188377062,
-0.127875503560243));
#81587=CARTESIAN_POINT('Ctrl Pts',(0.148094184488826,-0.0477393394530037,
-0.127608875861934));
#81588=CARTESIAN_POINT('Ctrl Pts',(0.149650266975529,-0.0424640243738569,
-0.127225611910502));
#81589=CARTESIAN_POINT('Ctrl Pts',(0.150081846495681,-0.0409125260293477,
-0.127112669171581));
#81590=CARTESIAN_POINT('Ctrl Pts',(0.150778348355001,-0.038249155273976,
-0.126918258672288));
#81591=CARTESIAN_POINT('Ctrl Pts',(0.151055251945639,-0.0371405296906429,
-0.126837180984591));
#81592=CARTESIAN_POINT('Ctrl Pts',(0.151597291910299,-0.0348639890248439,
-0.126670322018178));
#81593=CARTESIAN_POINT('Ctrl Pts',(0.151861203818948,-0.0336958643231532,
-0.126584507704465));
#81594=CARTESIAN_POINT('Ctrl Pts',(0.152495377574027,-0.0307299715899738,
-0.126366066943848));
#81595=CARTESIAN_POINT('Ctrl Pts',(0.152847345822969,-0.028928527061049,
-0.126232872464656));
#81596=CARTESIAN_POINT('Ctrl Pts',(0.154269106263817,-0.0208991588885878,
-0.12563665539049));
#81597=CARTESIAN_POINT('Ctrl Pts',(0.154990552413085,-0.0146164698083195,
-0.125163021815002));
#81598=CARTESIAN_POINT('Ctrl Pts',(0.155668420204074,-0.00194299723188557,
-0.124194568261939));
#81599=CARTESIAN_POINT('Ctrl Pts',(0.155617286804773,0.0044366409719101,
-0.123700498307034));
#81600=CARTESIAN_POINT('Ctrl Pts',(0.154669760544396,0.0180573654061419,
-0.122642587704769));
#81601=CARTESIAN_POINT('Ctrl Pts',(0.153655243252302,0.0252762739670338,
-0.122080011683065));
#81602=CARTESIAN_POINT('Ctrl Pts',(0.151804899131552,0.0339653125853173,
-0.121417491799563));
#81603=CARTESIAN_POINT('Ctrl Pts',(0.15144695827776,0.035527302384748,-0.121299003108598));
#81604=CARTESIAN_POINT('Ctrl Pts',(0.150877432083684,0.0378473448089441,
-0.121124190463759));
#81605=CARTESIAN_POINT('Ctrl Pts',(0.150684142213483,0.03860971869733,-0.121066937926192));
#81606=CARTESIAN_POINT('Ctrl Pts',(0.150324431550832,0.0399846295194425,
-0.120964071606457));
#81607=CARTESIAN_POINT('Ctrl Pts',(0.150160036703584,0.0405976444074333,
-0.120918351041281));
#81608=CARTESIAN_POINT('Ctrl Pts',(0.149777158106643,0.0419912172752532,
-0.120814732313206));
#81609=CARTESIAN_POINT('Ctrl Pts',(0.14955632047996,0.0427710942133087,
-0.120756967878569));
#81610=CARTESIAN_POINT('Ctrl Pts',(0.148844977583074,0.045210273877995,
-0.120576897182742));
#81611=CARTESIAN_POINT('Ctrl Pts',(0.148332857576188,0.0468632075740606,
-0.120455738753383));
#81612=CARTESIAN_POINT('Ctrl Pts',(0.147037498812961,0.0508099353442831,
-0.12016776329997));
#81613=CARTESIAN_POINT('Ctrl Pts',(0.146228010115644,0.0530946888306141,
-0.12000213419497));
#81614=CARTESIAN_POINT('Ctrl Pts',(0.142711754927331,0.0623277904326568,
-0.119333661571723));
#81615=CARTESIAN_POINT('Ctrl Pts',(0.139560330334423,0.0690965093559548,
-0.11884526679557));
#81616=CARTESIAN_POINT('Ctrl Pts',(0.131647368010437,0.0833221715997394,
-0.117772539797679));
#81617=CARTESIAN_POINT('Ctrl Pts',(0.126711976141903,0.0906513281441833,
-0.117188452647073));
#81618=CARTESIAN_POINT('Ctrl Pts',(0.119819814629659,0.0992156170903066,
-0.116431941971945));
#81619=CARTESIAN_POINT('Ctrl Pts',(0.118421847140731,0.100880087168698,
-0.11628113897298));
#81620=CARTESIAN_POINT('Ctrl Pts',(0.116073545200341,0.103559964708645,
-0.116031632949334));
#81621=CARTESIAN_POINT('Ctrl Pts',(0.115143627472956,0.104592920492552,
-0.115933759000465));
#81622=CARTESIAN_POINT('Ctrl Pts',(0.113435886689785,0.106439507297926,
-0.115755580728603));
#81623=CARTESIAN_POINT('Ctrl Pts',(0.112662828363345,0.107257429053053,
-0.115675481011064));
#81624=CARTESIAN_POINT('Ctrl Pts',(0.110973561566323,0.109006316795537,
-0.11550159106784));
#81625=CARTESIAN_POINT('Ctrl Pts',(0.110054372132267,0.109934268773431,
-0.115407675138143));
#81626=CARTESIAN_POINT('Ctrl Pts',(0.10744232692818,0.112505622375854,-0.115142666372704));
#81627=CARTESIAN_POINT('Ctrl Pts',(0.105723674699108,0.114122180874038,
-0.114970440914707));
#81628=CARTESIAN_POINT('Ctrl Pts',(0.103430043567632,0.11618327608146,-0.114743209866952));
#81629=CARTESIAN_POINT('Ctrl Pts',(0.102887773590145,0.11666376178256,-0.114689672288783));
#81630=CARTESIAN_POINT('Ctrl Pts',(0.102342241743611,0.11714037755997,-0.114635995609957));
#81631=CARTESIAN_POINT('Origin',(0.,0.,-1.10400562256037));
#81632=CARTESIAN_POINT('',(0.10234224283772,0.117140376604078,-0.0306875317892119));
#81633=CARTESIAN_POINT('',(0.102472688294207,0.117287771082297,-0.0445113451759945));
#81634=CARTESIAN_POINT('',(0.10234224283772,0.117140376604078,-1.10400562256037));
#81635=CARTESIAN_POINT('',(-0.155549938411928,0.00013841981592947,-0.0751943774352678));
#81636=CARTESIAN_POINT('Ctrl Pts',(-0.155549938411928,0.00013841981592947,
-0.0751943774352684));
#81637=CARTESIAN_POINT('Ctrl Pts',(-0.155558961220896,-0.0100010054528611,
-0.0744674884213844));
#81638=CARTESIAN_POINT('Ctrl Pts',(-0.15457225557722,-0.020170319397278,
-0.0737405994074998));
#81639=CARTESIAN_POINT('Ctrl Pts',(-0.152598751870448,-0.030156648148979,
-0.0730137103936159));
#81640=CARTESIAN_POINT('Ctrl Pts',(-0.150627608514691,-0.0401310330461434,
-0.0722876907539397));
#81641=CARTESIAN_POINT('Ctrl Pts',(-0.147672161675392,-0.0499219254392591,
-0.0715616711142636));
#81642=CARTESIAN_POINT('Ctrl Pts',(-0.143792804224831,-0.0593248004898402,
-0.0708356514745874));
#81643=CARTESIAN_POINT('Ctrl Pts',(-0.139904255190837,-0.0687499543099442,
-0.0701079116350643));
#81644=CARTESIAN_POINT('Ctrl Pts',(-0.135087793914332,-0.0777843672882017,
-0.0693801717955413));
#81645=CARTESIAN_POINT('Ctrl Pts',(-0.129452156882421,-0.0862435016594814,
-0.0686524319560182));
#81646=CARTESIAN_POINT('Ctrl Pts',(-0.123914476917127,-0.0945556017231172,
-0.0679373414868388));
#81647=CARTESIAN_POINT('Ctrl Pts',(-0.117586561399235,-0.102311666098563,
-0.0672222510176595));
#81648=CARTESIAN_POINT('Ctrl Pts',(-0.110609361986205,-0.109368055395553,
-0.0665071605484802));
#81649=CARTESIAN_POINT('Ctrl Pts',(-0.10341070889456,-0.116648411828215,
-0.0657693733774343));
#81650=CARTESIAN_POINT('Ctrl Pts',(-0.0954635778570838,-0.123241902787809,
-0.0650315862063881));
#81651=CARTESIAN_POINT('Ctrl Pts',(-0.0869230970916733,-0.128996812720282,
-0.064293799035342));
#81652=CARTESIAN_POINT('Ctrl Pts',(-0.078365523499258,-0.134763240468041,
-0.0635545352649303));
#81653=CARTESIAN_POINT('Ctrl Pts',(-0.0692129102355039,-0.13968709048397,
-0.0628152714945182));
#81654=CARTESIAN_POINT('Ctrl Pts',(-0.0596549654545681,-0.143656143609016,
-0.0620760077241065));
#81655=CARTESIAN_POINT('Ctrl Pts',(-0.0501377917152772,-0.147608266061835,
-0.0613398974092399));
#81656=CARTESIAN_POINT('Ctrl Pts',(-0.0402195952627188,-0.150613357985868,
-0.0606037870943737));
#81657=CARTESIAN_POINT('Ctrl Pts',(-0.0301093058995079,-0.152608100041413,
-0.0598676767795072));
#81658=CARTESIAN_POINT('Ctrl Pts',(-0.0199340486624365,-0.154615660142574,
-0.0591268362813229));
#81659=CARTESIAN_POINT('Ctrl Pts',(-0.00956514831970885,-0.155599647111316,
-0.0583859957831381));
#81660=CARTESIAN_POINT('Ctrl Pts',(0.000775890449174843,-0.155548064899602,
-0.0576451552849537));
#81661=CARTESIAN_POINT('Ctrl Pts',(0.0111169292180593,-0.155496482687888,
-0.0569043147867693));
#81662=CARTESIAN_POINT('Ctrl Pts',(0.021429166655461,-0.154409464200979,
-0.0561634742885849));
#81663=CARTESIAN_POINT('Ctrl Pts',(0.0314967375605351,-0.152327797932757,
-0.0554226337904005));
#81664=CARTESIAN_POINT('Ctrl Pts',(0.0415054151158392,-0.150258309011066,
-0.0546861270663702));
#81665=CARTESIAN_POINT('Ctrl Pts',(0.0513470946389434,-0.14719032789149,
-0.0539496203423399));
#81666=CARTESIAN_POINT('Ctrl Pts',(0.060810581508614,-0.14317079198141,
-0.0532131136183096));
#81667=CARTESIAN_POINT('Ctrl Pts',(0.0703136072509937,-0.139134462269967,
-0.0524735297361438));
#81668=CARTESIAN_POINT('Ctrl Pts',(0.0794343486427382,-0.134138822528049,
-0.0517339458539783));
#81669=CARTESIAN_POINT('Ctrl Pts',(0.0879745491710003,-0.128282037706607,
-0.0509943619718125));
#81670=CARTESIAN_POINT('Ctrl Pts',(0.0964599027186236,-0.122462866400519,
-0.050259527854331));
#81671=CARTESIAN_POINT('Ctrl Pts',(0.10437138151846,-0.115794117272148,
-0.04952469373685));
#81672=CARTESIAN_POINT('Ctrl Pts',(0.111542561775653,-0.108416140000115,
-0.0487898596193685));
#81673=CARTESIAN_POINT('Ctrl Pts',(0.118783270824285,-0.100966628918502,
-0.0480479008548607));
#81674=CARTESIAN_POINT('Ctrl Pts',(0.125268556296564,-0.0927947320807613,
-0.0473059420903526));
#81675=CARTESIAN_POINT('Ctrl Pts',(0.130867025676167,-0.0840810566695813,
-0.0465639833258447));
#81676=CARTESIAN_POINT('Ctrl Pts',(0.13646549505577,-0.0753673812584019,
-0.0458220245613368));
#81677=CARTESIAN_POINT('Ctrl Pts',(0.141176742647482,-0.0661128063666765,
-0.0450800657968286));
#81678=CARTESIAN_POINT('Ctrl Pts',(0.144917390905267,-0.0565221400268082,
-0.0443381070323208));
#81679=CARTESIAN_POINT('Ctrl Pts',(0.148642969898444,-0.0469701098480734,
-0.0435991372612117));
#81680=CARTESIAN_POINT('Ctrl Pts',(0.151433720977259,-0.03701323759064,
-0.0428601674901025));
#81681=CARTESIAN_POINT('Ctrl Pts',(0.153214174245866,-0.0268555266222315,
-0.0421211977189935));
#81682=CARTESIAN_POINT('Ctrl Pts',(0.154994623537292,-0.0166978383441483,
-0.0413822295985973));
#81683=CARTESIAN_POINT('Ctrl Pts',(0.155764497211888,-0.00634019488119242,
-0.0406432614782013));
#81684=CARTESIAN_POINT('Ctrl Pts',(0.155498581209574,0.00399921764967614,
-0.0399042933578051));
#81685=CARTESIAN_POINT('Ctrl Pts',(0.155233287886262,0.0143144190198078,
-0.0391670556332016));
#81686=CARTESIAN_POINT('Ctrl Pts',(0.153937050533157,0.0246105496841226,
-0.0384298179085981));
#81687=CARTESIAN_POINT('Ctrl Pts',(0.151636941721272,0.0346704543584231,
-0.0376925801839947));
#81688=CARTESIAN_POINT('Ctrl Pts',(0.149328734913697,0.0447657769504627,
-0.0369527468657023));
#81689=CARTESIAN_POINT('Ctrl Pts',(0.146009791770651,0.0546222990557376,
-0.0362129135474098));
#81690=CARTESIAN_POINT('Ctrl Pts',(0.141758457587672,0.0640339144701007,
-0.0354730802291174));
#81691=CARTESIAN_POINT('Ctrl Pts',(0.137507123404693,0.0734455298844644,
-0.034733246910825));
#81692=CARTESIAN_POINT('Ctrl Pts',(0.132323889645745,0.0824114459753015,
-0.0339934135925325));
#81693=CARTESIAN_POINT('Ctrl Pts',(0.126332605879763,0.0907517228025362,
-0.03325358027424));
#81694=CARTESIAN_POINT('Ctrl Pts',(0.120350725319235,0.0990789097245675,
-0.0325149081102118));
#81695=CARTESIAN_POINT('Ctrl Pts',(0.113520461596062,0.106842110718766,
-0.0317762359461835));
#81696=CARTESIAN_POINT('Ctrl Pts',(0.105972061558888,0.113867136035642,
-0.0310375637821552));
#81697=CARTESIAN_POINT('Ctrl Pts',(0.104779750257061,0.114976777421853,
-0.030920886451174));
#81698=CARTESIAN_POINT('Ctrl Pts',(0.103569608066442,0.116068062224272,
-0.030804209120193));
#81699=CARTESIAN_POINT('Ctrl Pts',(0.10234224283772,0.117140376604078,-0.0306875317892119));
#81700=CARTESIAN_POINT('Ctrl Pts',(0.10234224283772,0.117140376604078,-0.100698721018058));
#81701=CARTESIAN_POINT('Ctrl Pts',(0.099065544252337,0.120003135731656,
-0.100386060952946));
#81702=CARTESIAN_POINT('Ctrl Pts',(0.0956728992865777,0.122724582357694,
-0.100073400887833));
#81703=CARTESIAN_POINT('Ctrl Pts',(0.0921780765868749,0.125295669106096,
-0.099760740822721));
#81704=CARTESIAN_POINT('Ctrl Pts',(0.083933296768488,0.131361225489355,
-0.0990231316172315));
#81705=CARTESIAN_POINT('Ctrl Pts',(0.075056647698021,0.13663202138511,-0.0982855224117419));
#81706=CARTESIAN_POINT('Ctrl Pts',(0.0657249117760847,0.140982404831333,
-0.0975479132062524));
#81707=CARTESIAN_POINT('Ctrl Pts',(0.0563716805356272,0.145342809229569,
-0.0968086049444514));
#81708=CARTESIAN_POINT('Ctrl Pts',(0.0465620415849983,0.148778030941094,
-0.0960692966826506));
#81709=CARTESIAN_POINT('Ctrl Pts',(0.0365009764596717,0.151206749907173,
-0.0953299884208496));
#81710=CARTESIAN_POINT('Ctrl Pts',(0.0264859355025571,0.153624358740395,
-0.0945940621118913));
#81711=CARTESIAN_POINT('Ctrl Pts',(0.0162226691210491,0.15504443073102,
-0.093858135802933));
#81712=CARTESIAN_POINT('Ctrl Pts',(0.00592733703515371,0.155437026398705,
-0.0931222094939748));
#81713=CARTESIAN_POINT('Ctrl Pts',(-0.00443896342187721,0.155832328329269,
-0.0923812102557524));
#81714=CARTESIAN_POINT('Ctrl Pts',(-0.0148368252824632,0.155185885906542,
-0.0916402110175299));
#81715=CARTESIAN_POINT('Ctrl Pts',(-0.0250453720823497,0.153520460646966,
-0.0908992117793075));
#81716=CARTESIAN_POINT('Ctrl Pts',(-0.0352539188822363,0.15185503538739,
-0.0901582125410851));
#81717=CARTESIAN_POINT('Ctrl Pts',(-0.0452722405618459,0.14917090625426,
-0.0894172133028628));
#81718=CARTESIAN_POINT('Ctrl Pts',(-0.0548933067350833,0.145542184179323,
-0.0886762140646404));
#81719=CARTESIAN_POINT('Ctrl Pts',(-0.0644677683058369,0.141931039693687,
-0.0879388042388923));
#81720=CARTESIAN_POINT('Ctrl Pts',(-0.0737200321747962,0.137357610691785,
-0.0872013944131441));
#81721=CARTESIAN_POINT('Ctrl Pts',(-0.0824485118212944,0.13190165047661,
-0.086463984587396));
#81722=CARTESIAN_POINT('Ctrl Pts',(-0.091200052634537,0.126431275287309,
-0.0857246264806598));
#81723=CARTESIAN_POINT('Ctrl Pts',(-0.0994241707757214,0.120074063795145,
-0.0849852683739235));
#81724=CARTESIAN_POINT('Ctrl Pts',(-0.106940916035916,0.112957704373802,
-0.0842459102671873));
#81725=CARTESIAN_POINT('Ctrl Pts',(-0.114420758447958,0.105876282138971,
-0.0835101819788097));
#81726=CARTESIAN_POINT('Ctrl Pts',(-0.121199478655776,0.0980437895257948,
-0.0827744536904321));
#81727=CARTESIAN_POINT('Ctrl Pts',(-0.127134317940192,0.0896251510563975,
-0.0820387254020545));
#81728=CARTESIAN_POINT('Ctrl Pts',(-0.133113077763476,0.081144210792396,
-0.0812975523861389));
#81729=CARTESIAN_POINT('Ctrl Pts',(-0.138234853997668,0.0720691822704437,
-0.0805563793702231));
#81730=CARTESIAN_POINT('Ctrl Pts',(-0.142398385512891,0.0625979416859848,
-0.0798152063543074));
#81731=CARTESIAN_POINT('Ctrl Pts',(-0.146561917028115,0.0531267011015265,
-0.0790740333383918));
#81732=CARTESIAN_POINT('Ctrl Pts',(-0.149766941868116,0.0432601666174164,
-0.0783328603224763));
#81733=CARTESIAN_POINT('Ctrl Pts',(-0.151962914424122,0.0332125750240309,
-0.0775916873065607));
#81734=CARTESIAN_POINT('Ctrl Pts',(-0.154330524758453,0.0223796610941352,
-0.0767925840175835));
#81735=CARTESIAN_POINT('Ctrl Pts',(-0.155540019209143,0.0112851670771924,
-0.0759934807286063));
#81736=CARTESIAN_POINT('Ctrl Pts',(-0.155549938411874,0.000138419876762847,
-0.0751943774396291));
#81737=CARTESIAN_POINT('',(-0.155733678035791,-9.10003121109568E-5,-0.0890056225603696));
#81738=CARTESIAN_POINT('Ctrl Pts',(0.102342241743611,0.11714037755997,-0.114635995609957));
#81739=CARTESIAN_POINT('Ctrl Pts',(0.0968453600151427,0.121942847983995,
-0.11409513927507));
#81740=CARTESIAN_POINT('Ctrl Pts',(0.0910173447333404,0.126352381427472,
-0.11353950234708));
#81741=CARTESIAN_POINT('Ctrl Pts',(0.0774511378432751,0.135189422552379,
-0.112290605212437));
#81742=CARTESIAN_POINT('Ctrl Pts',(0.069598565891125,0.1393947807694,-0.111595784377499));
#81743=CARTESIAN_POINT('Ctrl Pts',(0.0586039155637544,0.144120933261064,
-0.110686783442491));
#81744=CARTESIAN_POINT('Ctrl Pts',(0.0557425926729581,0.145251605108168,
-0.11045580441431));
#81745=CARTESIAN_POINT('Ctrl Pts',(0.0518767736557376,0.146648124126632,
-0.11015273675136));
#81746=CARTESIAN_POINT('Ctrl Pts',(0.050900632440027,0.146989787829005,
-0.110076964342815));
#81747=CARTESIAN_POINT('Ctrl Pts',(0.0493510049672212,0.147514891328427,
-0.109957942021176));
#81748=CARTESIAN_POINT('Ctrl Pts',(0.0487797585361175,0.147704773264564,
-0.109914336590083));
#81749=CARTESIAN_POINT('Ctrl Pts',(0.047576719236147,0.148096922060416,
-0.109823091959806));
#81750=CARTESIAN_POINT('Ctrl Pts',(0.0469447086619598,0.148298472330081,
-0.109775497880124));
#81751=CARTESIAN_POINT('Ctrl Pts',(0.0453462199241087,0.148796992758305,
-0.109655935606263));
#81752=CARTESIAN_POINT('Ctrl Pts',(0.0443780774605145,0.149088601506892,
-0.109584267986357));
#81753=CARTESIAN_POINT('Ctrl Pts',(0.0404005469651865,0.150244471444413,
-0.109292611450648));
#81754=CARTESIAN_POINT('Ctrl Pts',(0.0373680168798433,0.151027282277312,
-0.109076741194422));
#81755=CARTESIAN_POINT('Ctrl Pts',(0.0286006284475955,0.153010179488705,
-0.108465651796799));
#81756=CARTESIAN_POINT('Ctrl Pts',(0.0228187282802862,0.15397865608585,
-0.108078290504308));
#81757=CARTESIAN_POINT('Ctrl Pts',(0.0059827903349026,0.15582925368744,
-0.106961695665347));
#81758=CARTESIAN_POINT('Ctrl Pts',(-0.00512656899842589,0.155859665710325,
-0.106236465954617));
#81759=CARTESIAN_POINT('Ctrl Pts',(-0.0184488146127189,0.154469452875764,
-0.105313868514814));
#81760=CARTESIAN_POINT('Ctrl Pts',(-0.0207474547415164,0.15417753660979,
-0.105152877653028));
#81761=CARTESIAN_POINT('Ctrl Pts',(-0.0243351354556274,0.153640236716811,
-0.104898308155404));
#81762=CARTESIAN_POINT('Ctrl Pts',(-0.0256291087018177,0.153429689944544,
-0.104805817141266));
#81763=CARTESIAN_POINT('Ctrl Pts',(-0.0280284508453781,0.153008086431379,
-0.104632980169495));
#81764=CARTESIAN_POINT('Ctrl Pts',(-0.0291344970364497,0.152801340083493,
-0.104552775240655));
#81765=CARTESIAN_POINT('Ctrl Pts',(-0.0315957180653166,0.15231358572355,
-0.104373064867778));
#81766=CARTESIAN_POINT('Ctrl Pts',(-0.0329495663908012,0.152026457046933,
-0.104273371318934));
#81767=CARTESIAN_POINT('Ctrl Pts',(-0.0369874899900583,0.151113610919677,
-0.103973416108908));
#81768=CARTESIAN_POINT('Ctrl Pts',(-0.0396588227989189,0.150434616424488,
-0.103771491193925));
#81769=CARTESIAN_POINT('Ctrl Pts',(-0.050852546957745,0.147270554916142,
-0.102910022147505));
#81770=CARTESIAN_POINT('Ctrl Pts',(-0.0591709003089992,0.144129657031934,
-0.102230545409286));
#81771=CARTESIAN_POINT('Ctrl Pts',(-0.0758443782874427,0.136146330023963,
-0.100799703513772));
#81772=CARTESIAN_POINT('Ctrl Pts',(-0.0841110990631629,0.131200403202779,
-0.100050059253136));
#81773=CARTESIAN_POINT('Ctrl Pts',(-0.093070702087738,0.124642950555568,
-0.099223382073601));
#81774=CARTESIAN_POINT('Ctrl Pts',(-0.0942599236657631,0.123746062276734,
-0.099113375727178));
#81775=CARTESIAN_POINT('Ctrl Pts',(-0.0960471084537074,0.122357484813098,
-0.0989478456297389));
#81776=CARTESIAN_POINT('Ctrl Pts',(-0.0966545488592804,0.121878215383102,
-0.0988915464626218));
#81777=CARTESIAN_POINT('Ctrl Pts',(-0.0977045129919885,0.121037008375313,
-0.0987942034440611));
#81778=CARTESIAN_POINT('Ctrl Pts',(-0.0981486413247851,0.12067714567441,
-0.0987530212801998));
#81779=CARTESIAN_POINT('Ctrl Pts',(-0.0986020514402913,0.120305603208518,
-0.0987109690894652));
#81780=CARTESIAN_POINT('Ctrl Pts',(-0.0986133015423969,0.120296381784774,
-0.098709925674646));
#81781=CARTESIAN_POINT('Ctrl Pts',(-0.0986343142312683,0.120279153287461,
-0.0987079767934577));
#81782=CARTESIAN_POINT('Ctrl Pts',(-0.0986440771352481,0.120271146604481,
-0.0987070712995619));
#81783=CARTESIAN_POINT('Ctrl Pts',(-0.0986623573757319,0.12025615102128,
-0.0987053758251081));
#81784=CARTESIAN_POINT('Ctrl Pts',(-0.0986708749438864,0.12024916240539,
-0.0987045858244758));
#81785=CARTESIAN_POINT('Ctrl Pts',(-0.0986868575231541,0.12023604594913,
-0.0987031034387955));
#81786=CARTESIAN_POINT('Ctrl Pts',(-0.0986943227053451,0.120229918319069,
-0.0987024110389428));
#81787=CARTESIAN_POINT('Ctrl Pts',(-0.0987083565367617,0.120218396770432,
-0.0987011093864393));
#81788=CARTESIAN_POINT('Ctrl Pts',(-0.0987149253142471,0.12021300300901,
-0.0987005001227003));
#81789=CARTESIAN_POINT('Ctrl Pts',(-0.0987272939401283,0.120202845172625,
-0.098699352909224));
#81790=CARTESIAN_POINT('Ctrl Pts',(-0.0987330938853791,0.120198081216613,
-0.0986988149511227));
#81791=CARTESIAN_POINT('Ctrl Pts',(-0.0987504054580136,0.120183859747638,
-0.0986972092567941));
#81792=CARTESIAN_POINT('Ctrl Pts',(-0.0987619160762045,0.120174400996715,
-0.098696141607642));
#81793=CARTESIAN_POINT('Ctrl Pts',(-0.0987846854587873,0.120155684972726,
-0.0986940296519114));
#81794=CARTESIAN_POINT('Ctrl Pts',(-0.098795944280803,0.120146427770956,
-0.0986929853403719));
#81795=CARTESIAN_POINT('Ctrl Pts',(-0.0988182315009227,0.120128097574941,
-0.0986909180728842));
#81796=CARTESIAN_POINT('Ctrl Pts',(-0.0988292599509602,0.120119024644269,
-0.0986898951124704));
#81797=CARTESIAN_POINT('Ctrl Pts',(-0.09885110625777,0.120101046989337,
-0.0986878687084864));
#81798=CARTESIAN_POINT('Ctrl Pts',(-0.0988619241610093,0.120092142322065,
-0.0986868652609278));
#81799=CARTESIAN_POINT('Ctrl Pts',(-0.0988833677845966,0.120074486320233,
-0.0986848761755496));
#81800=CARTESIAN_POINT('Ctrl Pts',(-0.0988939935463891,0.120065735036849,
-0.0986838905341799));
#81801=CARTESIAN_POINT('Ctrl Pts',(-0.0989150700336364,0.120048371932408,
-0.0986819354712143));
#81802=CARTESIAN_POINT('Ctrl Pts',(-0.0989255207964517,0.120039760156925,
-0.0986809660464215));
#81803=CARTESIAN_POINT('Ctrl Pts',(-0.0989462633091198,0.120022663089445,
-0.0986790419307446));
#81804=CARTESIAN_POINT('Ctrl Pts',(-0.0989565550921221,0.120014177838372,
-0.0986780872370303));
#81805=CARTESIAN_POINT('Ctrl Pts',(-0.0989769946672544,0.119997321635479,
-0.0986761911904458));
#81806=CARTESIAN_POINT('Ctrl Pts',(-0.098987142488969,0.119988950720136,
-0.0986752498350535));
#81807=CARTESIAN_POINT('Ctrl Pts',(-0.0990073082722792,0.119972311711489,
-0.0986733791546542));
#81808=CARTESIAN_POINT('Ctrl Pts',(-0.0990173262601682,0.119964043650623,
-0.0986724498274095));
#81809=CARTESIAN_POINT('Ctrl Pts',(-0.0990372457123638,0.119947599503267,
-0.0986706019664489));
#81810=CARTESIAN_POINT('Ctrl Pts',(-0.0990471472001404,0.119939423445343,
-0.0986696834307372));
#81811=CARTESIAN_POINT('Ctrl Pts',(-0.0990668462827558,0.119923153015172,
-0.0986678559813986));
#81812=CARTESIAN_POINT('Ctrl Pts',(-0.0990766438981405,0.119915058668179,
-0.0986669470660283));
#81813=CARTESIAN_POINT('Ctrl Pts',(-0.0990961472383411,0.119898941868049,
-0.0986651377441451));
#81814=CARTESIAN_POINT('Ctrl Pts',(-0.0991058529812392,0.119890919436886,
-0.0986642373360991));
#81815=CARTESIAN_POINT('Ctrl Pts',(-0.0991251840221976,0.119874937116027,
-0.0986624439672103));
#81816=CARTESIAN_POINT('Ctrl Pts',(-0.0991348093358464,0.11986697724541,
-0.0986615510050484));
#81817=CARTESIAN_POINT('Ctrl Pts',(-0.0991539904710281,0.119851111081601,
-0.0986597715119472));
#81818=CARTESIAN_POINT('Ctrl Pts',(-0.0991635463059423,0.119843204804664,
-0.0986588849798768));
#81819=CARTESIAN_POINT('Ctrl Pts',(-0.099182599002665,0.119827437204787,
-0.0986571173711519));
#81820=CARTESIAN_POINT('Ctrl Pts',(-0.0991920958754488,0.119819575895705,
-0.0986562362935733));
#81821=CARTESIAN_POINT('Ctrl Pts',(-0.0992110407855756,0.119803889906521,
-0.0986544786533435));
#81822=CARTESIAN_POINT('Ctrl Pts',(-0.0992204888319279,0.119796065237738,
-0.0986536020899347));
#81823=CARTESIAN_POINT('Ctrl Pts',(-0.0992393458956281,0.11978044446201,
-0.0986518525682251));
#81824=CARTESIAN_POINT('Ctrl Pts',(-0.0992487549198683,0.119772648364161,
-0.0986509796093476));
#81825=CARTESIAN_POINT('Ctrl Pts',(-0.0992675434581723,0.119757076885717,
-0.0986492364135049));
#81826=CARTESIAN_POINT('Ctrl Pts',(-0.0992769229777406,0.119749301511548,
-0.0986483661760762));
#81827=CARTESIAN_POINT('Ctrl Pts',(-0.0999553900851921,0.119186735686285,
-0.0985854170076944));
#81828=CARTESIAN_POINT('Ctrl Pts',(-0.100619837119209,0.118626331143525,
-0.0985237274904377));
#81829=CARTESIAN_POINT('Ctrl Pts',(-0.102105530527473,0.11735181038016,
-0.0983856043935393));
#81830=CARTESIAN_POINT('Ctrl Pts',(-0.102924058891223,0.116634579030526,
-0.098309376209202));
#81831=CARTESIAN_POINT('Ctrl Pts',(-0.105258513591226,0.114545309526885,
-0.0980913603341662));
#81832=CARTESIAN_POINT('Ctrl Pts',(-0.106755056684746,0.113151850869635,
-0.0979508393857119));
#81833=CARTESIAN_POINT('Ctrl Pts',(-0.112148857126832,0.107927278532898,
-0.0974395989850106));
#81834=CARTESIAN_POINT('Ctrl Pts',(-0.115871171224845,0.103920854332224,
-0.0970772306831424));
#81835=CARTESIAN_POINT('Ctrl Pts',(-0.12690615788372,0.0907117062908546,
-0.0959414475563277));
#81836=CARTESIAN_POINT('Ctrl Pts',(-0.133391034276816,0.0808738828897926,
-0.0951750182441215));
#81837=CARTESIAN_POINT('Ctrl Pts',(-0.139726588698447,0.0683912260705418,
-0.0942099975423691));
#81838=CARTESIAN_POINT('Ctrl Pts',(-0.140702539902558,0.0663601821256566,
-0.0940533298573491));
#81839=CARTESIAN_POINT('Ctrl Pts',(-0.142170248052984,0.0631276921755986,
-0.0938041055498973));
#81840=CARTESIAN_POINT('Ctrl Pts',(-0.142691694226751,0.0619400126611123,
-0.093712561729332));
#81841=CARTESIAN_POINT('Ctrl Pts',(-0.143637953927149,0.05970936804908,
-0.0935406000739668));
#81842=CARTESIAN_POINT('Ctrl Pts',(-0.144066415149209,0.058668035126323,
-0.093460311893836));
#81843=CARTESIAN_POINT('Ctrl Pts',(-0.145002677541301,0.0563204231500957,
-0.0932792333460877));
#81844=CARTESIAN_POINT('Ctrl Pts',(-0.145504199860699,0.0550117636832779,
-0.0931782408994444));
#81845=CARTESIAN_POINT('Ctrl Pts',(-0.146972063398045,0.0510209967130532,
-0.092870009362029));
#81846=CARTESIAN_POINT('Ctrl Pts',(-0.147882367790324,0.0483190734494026,
-0.0926609661109985));
#81847=CARTESIAN_POINT('Ctrl Pts',(-0.150977206614264,0.0382243320342762,
-0.0918781477971599));
#81848=CARTESIAN_POINT('Ctrl Pts',(-0.152685338588339,0.0306981094270853,
-0.0912902640206059));
#81849=CARTESIAN_POINT('Ctrl Pts',(-0.154978712495817,0.0154109329596322,
-0.0900962633168567));
#81850=CARTESIAN_POINT('Ctrl Pts',(-0.155554107791177,0.00766935171596105,
-0.0894917598193654));
#81851=CARTESIAN_POINT('Ctrl Pts',(-0.155549977927097,-8.28666372969583E-5,
-0.0889002981283004));
#81852=CARTESIAN_POINT('Ctrl Pts',(-0.155733678035791,-9.10003121109568E-5,
-0.0890056225603696));
#81853=CARTESIAN_POINT('Ctrl Pts',(-0.155771337450929,-0.00550761823091695,
-0.0886163681581111));
#81854=CARTESIAN_POINT('Ctrl Pts',(-0.153061777043569,-0.062301176855948,
-0.0845322715031591));
#81855=CARTESIAN_POINT('Ctrl Pts',(-0.0833593216436694,-0.163684077812068,
-0.0767533325955136));
#81856=CARTESIAN_POINT('Ctrl Pts',(0.0918939642601181,-0.159053435166454,
-0.0656688058374342));
#81857=CARTESIAN_POINT('Ctrl Pts',(0.180657312075961,-0.0140801128612938,
-0.0549214766975938));
#81858=CARTESIAN_POINT('Ctrl Pts',(0.137438874464206,0.0863139887816716,
-0.0478689898104475));
#81859=CARTESIAN_POINT('Ctrl Pts',(0.102472688294207,0.117287771082297,
-0.0445113451759945));
#81860=CARTESIAN_POINT('Origin',(0.,0.,-0.485));
#81861=CARTESIAN_POINT('',(-0.1956163961968,0.000134331411914747,-0.952013030787577));
#81862=CARTESIAN_POINT('',(0.0863231127633264,0.175648025443413,-0.974597867473044));
#81863=CARTESIAN_POINT('Ctrl Pts',(-0.1956163961968,0.000134331411914747,
-0.952013030787577));
#81864=CARTESIAN_POINT('Ctrl Pts',(-0.19566971989317,0.00745513469970677,
-0.952431787590014));
#81865=CARTESIAN_POINT('Ctrl Pts',(-0.191981342224257,0.0793125058488746,
-0.956545386645138));
#81866=CARTESIAN_POINT('Ctrl Pts',(-0.106281980654299,0.201804323958761,
-0.964073665540303));
#81867=CARTESIAN_POINT('Ctrl Pts',(0.03262926834607,0.201667302277058,-0.971183187633017));
#81868=CARTESIAN_POINT('Ctrl Pts',(0.0863231127633264,0.175648025443413,
-0.974597867473044));
#81869=CARTESIAN_POINT('',(-0.0861525859670517,0.175382131162755,-0.9746));
#81870=CARTESIAN_POINT('Origin',(0.,0.,-0.9746));
#81871=CARTESIAN_POINT('',(-0.195414161199284,0.000207025558219241,-0.962186969212424));
#81872=CARTESIAN_POINT('Ctrl Pts',(-0.0861525859670515,0.175382131162755,
-0.9746));
#81873=CARTESIAN_POINT('Ctrl Pts',(-0.144317765490378,0.146809775496019,
-0.970905157747306));
#81874=CARTESIAN_POINT('Ctrl Pts',(-0.191736685832022,0.0801530562864324,
-0.966767480818114));
#81875=CARTESIAN_POINT('Ctrl Pts',(-0.195639513638137,0.00794474237382261,
-0.962629803888923));
#81876=CARTESIAN_POINT('Ctrl Pts',(-0.195579810854541,0.000207201050681732,
-0.962186969212424));
#81877=CARTESIAN_POINT('',(-0.1953805473626,6.85612951323299E-5,-0.892186972544719));
#81878=CARTESIAN_POINT('Ctrl Pts',(-0.19539989034459,0.00020701043939857,
-0.962186969212424));
#81879=CARTESIAN_POINT('Ctrl Pts',(-0.195412469673056,-0.0116667839925565,
-0.961506776602131));
#81880=CARTESIAN_POINT('Ctrl Pts',(-0.194338478881212,-0.023590350489055,
-0.960826583991837));
#81881=CARTESIAN_POINT('Ctrl Pts',(-0.192177141769211,-0.0353426962952271,
-0.960146391381544));
#81882=CARTESIAN_POINT('Ctrl Pts',(-0.190018078336246,-0.0470826788924694,
-0.959466914318895));
#81883=CARTESIAN_POINT('Ctrl Pts',(-0.186774007411375,-0.0586508853449791,
-0.958787437256246));
#81884=CARTESIAN_POINT('Ctrl Pts',(-0.182496005115271,-0.0698309968206588,
-0.958107960193597));
#81885=CARTESIAN_POINT('Ctrl Pts',(-0.178221276950605,-0.081002551696338,
-0.957429003162742));
#81886=CARTESIAN_POINT('Ctrl Pts',(-0.172914506347834,-0.0917857398504531,
-0.956750046131888));
#81887=CARTESIAN_POINT('Ctrl Pts',(-0.1666757469373,-0.101982132664959,
-0.956071089101033));
#81888=CARTESIAN_POINT('Ctrl Pts',(-0.160422453067151,-0.112202280051459,
-0.95539055030161));
#81889=CARTESIAN_POINT('Ctrl Pts',(-0.153233342828904,-0.121832131556134,
-0.954710011502186));
#81890=CARTESIAN_POINT('Ctrl Pts',(-0.145252308775906,-0.130701670973515,
-0.954029472702763));
#81891=CARTESIAN_POINT('Ctrl Pts',(-0.139003391399146,-0.137646262190778,
-0.953496630629789));
#81892=CARTESIAN_POINT('Ctrl Pts',(-0.132269980151298,-0.14412527246669,
-0.952963788556815));
#81893=CARTESIAN_POINT('Ctrl Pts',(-0.125135862889114,-0.150073901192035,
-0.952430946483841));
#81894=CARTESIAN_POINT('Ctrl Pts',(-0.115793508275601,-0.157863820669655,
-0.951733172755742));
#81895=CARTESIAN_POINT('Ctrl Pts',(-0.105688809723304,-0.164804873099924,
-0.951035399027644));
#81896=CARTESIAN_POINT('Ctrl Pts',(-0.0950001891611107,-0.170751644382574,
-0.950337625299546));
#81897=CARTESIAN_POINT('Ctrl Pts',(-0.0843338282669652,-0.17668603117146,
-0.949641304725432));
#81898=CARTESIAN_POINT('Ctrl Pts',(-0.0730866783110694,-0.181629763867164,
-0.948944984151319));
#81899=CARTESIAN_POINT('Ctrl Pts',(-0.0614658534741819,-0.185480750636529,
-0.948248663577205));
#81900=CARTESIAN_POINT('Ctrl Pts',(-0.0498469122605606,-0.189331113198201,
-0.947552455869919));
#81901=CARTESIAN_POINT('Ctrl Pts',(-0.0378552285880504,-0.192088765254431,
-0.946856248162633));
#81902=CARTESIAN_POINT('Ctrl Pts',(-0.0257162504914437,-0.193700372897579,
-0.946160040455347));
#81903=CARTESIAN_POINT('Ctrl Pts',(-0.0135780569622602,-0.195311876379171,
-0.945463877745414));
#81904=CARTESIAN_POINT('Ctrl Pts',(-0.00129345549938047,-0.195777393556016,
-0.944767715035481));
#81905=CARTESIAN_POINT('Ctrl Pts',(0.0109063693168893,-0.195095389766964,
-0.944071552325549));
#81906=CARTESIAN_POINT('Ctrl Pts',(0.0231334414868171,-0.19441186277584,
-0.943373834790703));
#81907=CARTESIAN_POINT('Ctrl Pts',(0.0352744927484605,-0.192575810342531,
-0.942676117255857));
#81908=CARTESIAN_POINT('Ctrl Pts',(0.0471040609448881,-0.189637463183044,
-0.941978399721011));
#81909=CARTESIAN_POINT('Ctrl Pts',(0.0506757309876744,-0.188750295845185,
-0.941767739722594));
#81910=CARTESIAN_POINT('Ctrl Pts',(0.0542191050569545,-0.187762990553711,
-0.941557079724177));
#81911=CARTESIAN_POINT('Ctrl Pts',(0.0577282871149016,-0.186677810322436,
-0.941346419725759));
#81912=CARTESIAN_POINT('Ctrl Pts',(0.0693538915815736,-0.183082705840671,
-0.940648522102294));
#81913=CARTESIAN_POINT('Ctrl Pts',(0.0806815561660394,-0.17838535157395,
-0.939950624478829));
#81914=CARTESIAN_POINT('Ctrl Pts',(0.0914921904373815,-0.172656708786453,
-0.939252726855364));
#81915=CARTESIAN_POINT('Ctrl Pts',(0.102280936127439,-0.16693966493572,
-0.938556242283943));
#81916=CARTESIAN_POINT('Ctrl Pts',(0.112553933870211,-0.160195819692752,
-0.937859757712523));
#81917=CARTESIAN_POINT('Ctrl Pts',(0.122112927822495,-0.152543740804459,
-0.937163273141102));
#81918=CARTESIAN_POINT('Ctrl Pts',(0.131671149266465,-0.144892280317496,
-0.936466844855952));
#81919=CARTESIAN_POINT('Ctrl Pts',(0.140514775110156,-0.136333242083167,
-0.935770416570802));
#81920=CARTESIAN_POINT('Ctrl Pts',(0.148476551225366,-0.127027059070976,
-0.935073988285653));
#81921=CARTESIAN_POINT('Ctrl Pts',(0.156438191522455,-0.117721034810836,
-0.934377571880714));
#81922=CARTESIAN_POINT('Ctrl Pts',(0.163517466935723,-0.107668571558001,
-0.933681155475775));
#81923=CARTESIAN_POINT('Ctrl Pts',(0.169587527661876,-0.0970630231423506,
-0.932984739070836));
#81924=CARTESIAN_POINT('Ctrl Pts',(0.175671530092538,-0.0864331159222585,
-0.932286723137957));
#81925=CARTESIAN_POINT('Ctrl Pts',(0.180741314795697,-0.0752483757505814,
-0.931588707205077));
#81926=CARTESIAN_POINT('Ctrl Pts',(0.184716614286542,-0.0637254455183864,
-0.930890691272198));
#81927=CARTESIAN_POINT('Ctrl Pts',(0.18591031272142,-0.0602653530611877,
-0.930681091837359));
#81928=CARTESIAN_POINT('Ctrl Pts',(0.187005666383098,-0.0567748710197401,
-0.930471492402519));
#81929=CARTESIAN_POINT('Ctrl Pts',(0.188001393688077,-0.0532600785893206,
-0.93026189296768));
#81930=CARTESIAN_POINT('Ctrl Pts',(0.191306541060573,-0.0415933231351084,
-0.929566163305681));
#81931=CARTESIAN_POINT('Ctrl Pts',(0.19353343416577,-0.0295756893586034,
-0.928870433643683));
#81932=CARTESIAN_POINT('Ctrl Pts',(0.194621241094103,-0.0174279234273898,
-0.928174703981684));
#81933=CARTESIAN_POINT('Ctrl Pts',(0.195706742013875,-0.00530590917279384,
-0.927480449175669));
#81934=CARTESIAN_POINT('Ctrl Pts',(0.195657796133363,0.00694483124659212,
-0.926786194369654));
#81935=CARTESIAN_POINT('Ctrl Pts',(0.194464779426019,0.019094752231698,
-0.926091939563638));
#81936=CARTESIAN_POINT('Ctrl Pts',(0.193271955408107,0.0312427108290403,
-0.925397796889804));
#81937=CARTESIAN_POINT('Ctrl Pts',(0.190935466520171,0.0432890056340155,
-0.924703654215969));
#81938=CARTESIAN_POINT('Ctrl Pts',(0.187497697320824,0.0550070313631696,
-0.924009511542135));
#81939=CARTESIAN_POINT('Ctrl Pts',(0.184060158236639,0.0667242727187282,
-0.923315415332372));
#81940=CARTESIAN_POINT('Ctrl Pts',(0.179521757891869,0.0781124538651824,
-0.922621319122609));
#81941=CARTESIAN_POINT('Ctrl Pts',(0.173974552805762,0.0889607496373264,
-0.921927222912846));
#81942=CARTESIAN_POINT('Ctrl Pts',(0.168414633078311,0.099833910578108,
-0.921231535778603));
#81943=CARTESIAN_POINT('Ctrl Pts',(0.161841750388756,0.110163964756701,
-0.92053584864436));
#81944=CARTESIAN_POINT('Ctrl Pts',(0.154392924816104,0.11976637577688,-0.919840161510117));
#81945=CARTESIAN_POINT('Ctrl Pts',(0.152027375543106,0.122815846621144,
-0.919619229743278));
#81946=CARTESIAN_POINT('Ctrl Pts',(0.14957378835313,0.125792186122078,-0.919398297976439));
#81947=CARTESIAN_POINT('Ctrl Pts',(0.147037348322021,0.128690241271157,
-0.9191773662096));
#81948=CARTESIAN_POINT('Ctrl Pts',(0.13903647670072,0.137831780954669,-0.918480465560712));
#81949=CARTESIAN_POINT('Ctrl Pts',(0.130151875512212,0.146256274009908,
-0.917783564911824));
#81950=CARTESIAN_POINT('Ctrl Pts',(0.120536523779986,0.153792413450849,
-0.917086664262936));
#81951=CARTESIAN_POINT('Ctrl Pts',(0.110941208816254,0.161312848850427,
-0.916391215837259));
#81952=CARTESIAN_POINT('Ctrl Pts',(0.100618801895239,0.167948013162257,
-0.915695767411581));
#81953=CARTESIAN_POINT('Ctrl Pts',(0.0897574317888426,0.173564868100291,
-0.915000318985904));
#81954=CARTESIAN_POINT('Ctrl Pts',(0.0788975818574243,0.179180936894196,
-0.914304967896316));
#81955=CARTESIAN_POINT('Ctrl Pts',(0.0674996732154317,0.183778538112216,
-0.913609616806729));
#81956=CARTESIAN_POINT('Ctrl Pts',(0.0557775892654056,0.187269913589289,
-0.912914265717141));
#81957=CARTESIAN_POINT('Ctrl Pts',(0.0440561228898835,0.190761105124284,
-0.912218951261919));
#81958=CARTESIAN_POINT('Ctrl Pts',(0.0320113607683633,0.19314596284133,
-0.911523636806696));
#81959=CARTESIAN_POINT('Ctrl Pts',(0.0198709322294458,0.194387000728785,
-0.910828322351473));
#81960=CARTESIAN_POINT('Ctrl Pts',(0.00770286041451154,0.195630864410467,
-0.910131424692714));
#81961=CARTESIAN_POINT('Ctrl Pts',(-0.00456043690471319,0.195725684784602,
-0.909434527033955));
#81962=CARTESIAN_POINT('Ctrl Pts',(-0.0166889294022454,0.194686002669444,
-0.908737629375195));
#81963=CARTESIAN_POINT('Ctrl Pts',(-0.0204294737291825,0.194365354654989,
-0.908522699400637));
#81964=CARTESIAN_POINT('Ctrl Pts',(-0.0241572412903161,0.193937169211189,
-0.908307769426078));
#81965=CARTESIAN_POINT('Ctrl Pts',(-0.0278656665062796,0.193402855796291,
-0.90809283945152));
#81966=CARTESIAN_POINT('Ctrl Pts',(-0.039888809400841,0.191670549988924,
-0.907396011648354));
#81967=CARTESIAN_POINT('Ctrl Pts',(-0.0517917869311965,0.188806759265524,
-0.906699183845189));
#81968=CARTESIAN_POINT('Ctrl Pts',(-0.0633476521767701,0.184846517315558,
-0.906002356042024));
#81969=CARTESIAN_POINT('Ctrl Pts',(-0.0748794964147279,0.180894507462455,
-0.905306976724594));
#81970=CARTESIAN_POINT('Ctrl Pts',(-0.086064817578607,0.175850781673614,
-0.904611597407164));
#81971=CARTESIAN_POINT('Ctrl Pts',(-0.0966896311347117,0.169800692669475,
-0.903916218089734));
#81972=CARTESIAN_POINT('Ctrl Pts',(-0.107313058275478,0.163751393132007,
-0.903220929511266));
#81973=CARTESIAN_POINT('Ctrl Pts',(-0.117375341855184,0.15669638402423,
-0.902525640932798));
#81974=CARTESIAN_POINT('Ctrl Pts',(-0.126686456383126,0.148767273851093,
-0.90183035235433));
#81975=CARTESIAN_POINT('Ctrl Pts',(-0.135997130929772,0.140838538354927,
-0.901135096630573));
#81976=CARTESIAN_POINT('Ctrl Pts',(-0.144556058695458,0.13203637152894,
-0.900439840906815));
#81977=CARTESIAN_POINT('Ctrl Pts',(-0.152207903038364,0.122531278670648,
-0.899744585183057));
#81978=CARTESIAN_POINT('Ctrl Pts',(-0.15987724574609,0.11300444940803,-0.899047739536955));
#81979=CARTESIAN_POINT('Ctrl Pts',(-0.166634866901655,0.102772206786369,
-0.898350893890853));
#81980=CARTESIAN_POINT('Ctrl Pts',(-0.172367766296594,0.0920353907033747,
-0.89765404824475));
#81981=CARTESIAN_POINT('Ctrl Pts',(-0.174138573060907,0.0887189490152927,
-0.89743880306098));
#81982=CARTESIAN_POINT('Ctrl Pts',(-0.175811949310168,0.0853545311005462,
-0.89722355787721));
#81983=CARTESIAN_POINT('Ctrl Pts',(-0.17738549331188,0.0819484396587333,
-0.89700831269344));
#81984=CARTESIAN_POINT('Ctrl Pts',(-0.182914406178021,0.0699805615597355,
-0.8962520123519));
#81985=CARTESIAN_POINT('Ctrl Pts',(-0.187241060727249,0.0574235374384502,
-0.89549571201036));
#81986=CARTESIAN_POINT('Ctrl Pts',(-0.190259811913753,0.0445237461422927,
-0.89473941166882));
#81987=CARTESIAN_POINT('Ctrl Pts',(-0.193259450024786,0.0317056292437173,
-0.893987899805898));
#81988=CARTESIAN_POINT('Ctrl Pts',(-0.194967423098108,0.0185496467069044,
-0.893236387942975));
#81989=CARTESIAN_POINT('Ctrl Pts',(-0.195327639122108,0.00531727326583664,
-0.892484876080052));
#81990=CARTESIAN_POINT('Ctrl Pts',(-0.195375236304858,0.00356881218990247,
-0.892385574979892));
#81991=CARTESIAN_POINT('Ctrl Pts',(-0.195399373672046,0.00181903830544178,
-0.892286273879733));
#81992=CARTESIAN_POINT('Ctrl Pts',(-0.195399987967877,6.85722511850599E-5,
-0.892186972779573));
#81993=CARTESIAN_POINT('',(-0.195366936014536,-0.0001759764390597,-0.822186969212424));
#81994=CARTESIAN_POINT('Ctrl Pts',(-0.195104707912954,6.84058415591362E-5,
-0.892186969212424));
#81995=CARTESIAN_POINT('Ctrl Pts',(-0.19499122330115,-0.0366782010199141,
-0.890099241453403));
#81996=CARTESIAN_POINT('Ctrl Pts',(-0.167386274654172,-0.138618456874515,
-0.884316671441687));
#81997=CARTESIAN_POINT('Ctrl Pts',(-0.00315354223898925,-0.230724950314991,
-0.874839259177279));
#81998=CARTESIAN_POINT('Ctrl Pts',(0.191799192978493,-0.128288297037242,
-0.8637547324192));
#81999=CARTESIAN_POINT('Ctrl Pts',(0.212042795889746,0.0910094176328911,
-0.852670205661119));
#82000=CARTESIAN_POINT('Ctrl Pts',(0.03913571544926,0.227404907853978,-0.841585678903039));
#82001=CARTESIAN_POINT('Ctrl Pts',(-0.152045168436665,0.162551660997725,
-0.831424600086807));
#82002=CARTESIAN_POINT('Ctrl Pts',(-0.194931245944501,0.0484383113115352,
-0.824958363523269));
#82003=CARTESIAN_POINT('Ctrl Pts',(-0.195366936014536,-0.0001759764390597,
-0.822186969212424));
#82004=CARTESIAN_POINT('',(-0.195681094571072,7.47969092022707E-5,-0.752186969212423));
#82005=CARTESIAN_POINT('Ctrl Pts',(-0.195366936014536,-0.0001759764390597,
-0.822186969212424));
#82006=CARTESIAN_POINT('Ctrl Pts',(-0.195512110989054,-0.0163745966758234,
-0.821263521270576));
#82007=CARTESIAN_POINT('Ctrl Pts',(-0.186273967132678,-0.09722283275531,
-0.81664523107603));
#82008=CARTESIAN_POINT('Ctrl Pts',(-0.074157745877468,-0.218507032466107,
-0.808332098628802));
#82009=CARTESIAN_POINT('Ctrl Pts',(0.142885639710072,-0.181186120176718,
-0.797247571870717));
#82010=CARTESIAN_POINT('Ctrl Pts',(0.229774287535425,0.0211775855982428,
-0.78616304511264));
#82011=CARTESIAN_POINT('Ctrl Pts',(0.107361153908771,0.204250560881833,
-0.775078518354558));
#82012=CARTESIAN_POINT('Ctrl Pts',(-0.112847422116822,0.201271387892123,
-0.76399399159648));
#82013=CARTESIAN_POINT('Ctrl Pts',(-0.193675615340973,0.0730115495022533,
-0.756363475215766));
#82014=CARTESIAN_POINT('Ctrl Pts',(-0.195701748231673,0.00428175194181416,
-0.752427801087748));
#82015=CARTESIAN_POINT('Ctrl Pts',(-0.195681094571072,7.47969092022707E-5,
-0.752186969212423));
#82016=CARTESIAN_POINT('',(-0.19515607959856,0.000116101941455404,-0.682186969212424));
#82017=CARTESIAN_POINT('Ctrl Pts',(-0.195681094571072,7.47969092022707E-5,
-0.752186969212423));
#82018=CARTESIAN_POINT('Ctrl Pts',(-0.195384879803195,-0.060261345555979,
-0.748732958835055));
#82019=CARTESIAN_POINT('Ctrl Pts',(-0.133195868508463,-0.185668250759869,
-0.741584106204994));
#82020=CARTESIAN_POINT('Ctrl Pts',(0.0800418565502769,-0.216420915704385,
-0.730740411322238));
#82021=CARTESIAN_POINT('Ctrl Pts',(0.225105205951166,-0.0507184155460289,
-0.719655884564159));
#82022=CARTESIAN_POINT('Ctrl Pts',(0.165119859323233,0.161183570570169,
-0.708571357806077));
#82023=CARTESIAN_POINT('Ctrl Pts',(-0.0452734338024108,0.226263182214096,
-0.697486831048));
#82024=CARTESIAN_POINT('Ctrl Pts',(-0.179485015703818,0.114370598042359,
-0.688692034850112));
#82025=CARTESIAN_POINT('Ctrl Pts',(-0.195290790666625,0.0248312161815972,
-0.683592080904922));
#82026=CARTESIAN_POINT('Ctrl Pts',(-0.19515607959856,0.000116101941455404,
-0.682186969212424));
#82027=CARTESIAN_POINT('',(-0.195399931967772,-0.000163055175443911,-0.612186967161044));
#82028=CARTESIAN_POINT('Ctrl Pts',(-0.19515607959856,0.000116101941455404,
-0.682186969212424));
#82029=CARTESIAN_POINT('Ctrl Pts',(-0.194936558224572,-0.0401589542526584,
-0.679897238652229));
#82030=CARTESIAN_POINT('Ctrl Pts',(-0.163203532909971,-0.145741425442279,
-0.67391266583934));
#82031=CARTESIAN_POINT('Ctrl Pts',(0.00939477616280343,-0.230556825089081,
-0.664233250773757));
#82032=CARTESIAN_POINT('Ctrl Pts',(0.198490591378379,-0.117669862515987,
-0.653148724015678));
#82033=CARTESIAN_POINT('Ctrl Pts',(0.206781006218889,0.102402767916716,
-0.642064197257598));
#82034=CARTESIAN_POINT('Ctrl Pts',(0.0267142684199375,0.229196551618941,
-0.630979670499519));
#82035=CARTESIAN_POINT('Ctrl Pts',(-0.15693301120472,0.155538717273989,
-0.621020594484459));
#82036=CARTESIAN_POINT('Ctrl Pts',(-0.194907926478866,0.0449665939000981,
-0.614756360722095));
#82037=CARTESIAN_POINT('Ctrl Pts',(-0.19526695444957,-0.000162908179064867,
-0.612186969212424));
#82038=CARTESIAN_POINT('',(-0.195399999600512,1.24947932985652E-5,-0.542186969209066));
#82039=CARTESIAN_POINT('Ctrl Pts',(-0.195399931967772,-0.000163055175443911,
-0.612186967161044));
#82040=CARTESIAN_POINT('Ctrl Pts',(-0.195387649960393,-0.0148814067991219,
-0.611349560425973));
#82041=CARTESIAN_POINT('Ctrl Pts',(-0.193708372206648,-0.0295270808785863,
-0.610512153690901));
#82042=CARTESIAN_POINT('Ctrl Pts',(-0.19043429106854,-0.0437714608531942,
-0.60967474695583));
#82043=CARTESIAN_POINT('Ctrl Pts',(-0.189308103309253,-0.0486711092398252,
-0.609386703631673));
#82044=CARTESIAN_POINT('Ctrl Pts',(-0.187993644156325,-0.0535234622546284,
-0.609098660307515));
#82045=CARTESIAN_POINT('Ctrl Pts',(-0.186495138743599,-0.0583157202219598,
-0.608810616983358));
#82046=CARTESIAN_POINT('Ctrl Pts',(-0.182870726121707,-0.069906682868242,
-0.608113930904775));
#82047=CARTESIAN_POINT('Ctrl Pts',(-0.178148868935771,-0.0811991380356456,
-0.607417244826192));
#82048=CARTESIAN_POINT('Ctrl Pts',(-0.172400175377746,-0.0919746678695959,
-0.606720558747608));
#82049=CARTESIAN_POINT('Ctrl Pts',(-0.166663476446175,-0.102727714603012,
-0.606025326301783));
#82050=CARTESIAN_POINT('Ctrl Pts',(-0.159904536385181,-0.112965177748617,
-0.605330093855957));
#82051=CARTESIAN_POINT('Ctrl Pts',(-0.152241585329039,-0.122489426876367,
-0.604634861410131));
#82052=CARTESIAN_POINT('Ctrl Pts',(-0.144579692509108,-0.132012360726853,
-0.603939724974334));
#82053=CARTESIAN_POINT('Ctrl Pts',(-0.136014548859102,-0.140821566983641,
-0.603244588538537));
#82054=CARTESIAN_POINT('Ctrl Pts',(-0.126706245102679,-0.148750420006062,
-0.60254945210274));
#82055=CARTESIAN_POINT('Ctrl Pts',(-0.117398424234648,-0.156678861702082,
-0.601854351728648));
#82056=CARTESIAN_POINT('Ctrl Pts',(-0.107348203422377,-0.163726494047941,
-0.601159251354557));
#82057=CARTESIAN_POINT('Ctrl Pts',(-0.0967485603789931,-0.169767123037979,
-0.600464150980466));
#82058=CARTESIAN_POINT('Ctrl Pts',(-0.0861247016104804,-0.175821552323992,
-0.599767462594446));
#82059=CARTESIAN_POINT('Ctrl Pts',(-0.0749497067662055,-0.180864009385805,
-0.599070774208426));
#82060=CARTESIAN_POINT('Ctrl Pts',(-0.0634397670242631,-0.184814923531373,
-0.598374085822406));
#82061=CARTESIAN_POINT('Ctrl Pts',(-0.059871270488526,-0.186039849443893,
-0.59815808729003));
#82062=CARTESIAN_POINT('Ctrl Pts',(-0.0562706882353161,-0.187160216173435,
-0.597942088757653));
#82063=CARTESIAN_POINT('Ctrl Pts',(-0.0526446969434173,-0.188174641978498,
-0.597726090225277));
#82064=CARTESIAN_POINT('Ctrl Pts',(-0.0409493505614043,-0.191446591692103,
-0.597029404146688));
#82065=CARTESIAN_POINT('Ctrl Pts',(-0.0289067584796694,-0.19363553092092,
-0.5963327180681));
#82066=CARTESIAN_POINT('Ctrl Pts',(-0.0167385637002627,-0.194681741530253,
-0.595636031989512));
#82067=CARTESIAN_POINT('Ctrl Pts',(-0.00459575781131094,-0.195725769225272,
-0.594940799543681));
#82068=CARTESIAN_POINT('Ctrl Pts',(0.00767127380048421,-0.195631653110166,
-0.59424556709785));
#82069=CARTESIAN_POINT('Ctrl Pts',(0.0198323906566823,-0.194390936725046,
-0.593550334652019));
#82070=CARTESIAN_POINT('Ctrl Pts',(0.0319918280901456,-0.193150391680052,
-0.592855198216217));
#82071=CARTESIAN_POINT('Ctrl Pts',(0.04404450606983,-0.190763604270154,
-0.592160061780414));
#82072=CARTESIAN_POINT('Ctrl Pts',(0.0557634935802237,-0.187274111354795,
-0.591464925344612));
#82073=CARTESIAN_POINT('Ctrl Pts',(0.0674818731427938,-0.18378479946443,
-0.590769824970516));
#82074=CARTESIAN_POINT('Ctrl Pts',(0.0788657657328716,-0.179193171261107,
-0.590074724596419));
#82075=CARTESIAN_POINT('Ctrl Pts',(0.0897042429323871,-0.173592363887146,
-0.589379624222323));
#82076=CARTESIAN_POINT('Ctrl Pts',(0.100567481492599,-0.167978761024573,
-0.588682935836298));
#82077=CARTESIAN_POINT('Ctrl Pts',(0.11088207040143,-0.161351835747051,
-0.587986247450273));
#82078=CARTESIAN_POINT('Ctrl Pts',(0.12046354468802,-0.153849583688736,
-0.587289559064248));
#82079=CARTESIAN_POINT('Ctrl Pts',(0.123434147363716,-0.151523614910699,
-0.587073560531898));
#82080=CARTESIAN_POINT('Ctrl Pts',(0.126334525481837,-0.14911379729535,
-0.586857561999547));
#82081=CARTESIAN_POINT('Ctrl Pts',(0.129159884355811,-0.146624978339959,
-0.586641563467197));
#82082=CARTESIAN_POINT('Ctrl Pts',(0.138272854583456,-0.138597490840445,
-0.585944877388607));
#82083=CARTESIAN_POINT('Ctrl Pts',(0.146666564977586,-0.129689005850555,
-0.585248191310016));
#82084=CARTESIAN_POINT('Ctrl Pts',(0.154170232694714,-0.120052902300851,
-0.584551505231425));
#82085=CARTESIAN_POINT('Ctrl Pts',(0.161658244038721,-0.11043690444323,
-0.583856272785592));
#82086=CARTESIAN_POINT('Ctrl Pts',(0.168259308287332,-0.10009693958862,
-0.583161040339758));
#82087=CARTESIAN_POINT('Ctrl Pts',(0.173841009951574,-0.0892214282502628,
-0.582465807893925));
#82088=CARTESIAN_POINT('Ctrl Pts',(0.17942194079544,-0.0783474187954233,
-0.58177067145812));
#82089=CARTESIAN_POINT('Ctrl Pts',(0.183983349260585,-0.0669387662265575,
-0.581075535022315));
#82090=CARTESIAN_POINT('Ctrl Pts',(0.187438175868307,-0.055209512107621,
-0.58038039858651));
#82091=CARTESIAN_POINT('Ctrl Pts',(0.190892823249427,-0.0434808664691095,
-0.579685298212411));
#82092=CARTESIAN_POINT('Ctrl Pts',(0.193240781464953,-0.0314324992652491,
-0.578990197838312));
#82093=CARTESIAN_POINT('Ctrl Pts',(0.194445306428671,-0.0192920400129258,
-0.578295097464213));
#82094=CARTESIAN_POINT('Ctrl Pts',(0.195652583225192,-0.00712384491865252,
-0.577598409078185));
#82095=CARTESIAN_POINT('Ctrl Pts',(0.195711190497023,0.00513598575638776,
-0.576901720692157));
#82096=CARTESIAN_POINT('Ctrl Pts',(0.194636418920523,0.017257590497937,
-0.576205032306129));
#82097=CARTESIAN_POINT('Ctrl Pts',(0.194303200959987,0.0210157252483613,
-0.575989033773791));
#82098=CARTESIAN_POINT('Ctrl Pts',(0.193861415829799,0.0247606204490827,
-0.575773035241454));
#82099=CARTESIAN_POINT('Ctrl Pts',(0.193312518323342,0.0284856149571576,
-0.575557036709117));
#82100=CARTESIAN_POINT('Ctrl Pts',(0.191542093093218,0.0405002883371504,
-0.574860350630529));
#82101=CARTESIAN_POINT('Ctrl Pts',(0.188641077440746,0.0523914441757711,
-0.574163664551941));
#82102=CARTESIAN_POINT('Ctrl Pts',(0.184645115049052,0.063932319592851,
-0.573466978473353));
#82103=CARTESIAN_POINT('Ctrl Pts',(0.180657490217141,0.0754491150188532,
-0.572771746027523));
#82104=CARTESIAN_POINT('Ctrl Pts',(0.175579667013763,0.0866162379215019,
-0.572076513581693));
#82105=CARTESIAN_POINT('Ctrl Pts',(0.169497572422247,0.097220023364351,
-0.571381281135863));
#82106=CARTESIAN_POINT('Ctrl Pts',(0.163416317754239,0.107822344448413,
-0.570686144700061));
#82107=CARTESIAN_POINT('Ctrl Pts',(0.156331462364505,0.117860702119283,
-0.56999100826426));
#82108=CARTESIAN_POINT('Ctrl Pts',(0.148375120930957,0.12714552091491,-0.569295871828458));
#82109=CARTESIAN_POINT('Ctrl Pts',(0.140419192249829,0.136429858040481,
-0.568600771454362));
#82110=CARTESIAN_POINT('Ctrl Pts',(0.131592457158933,0.144960087093375,
-0.567905671080266));
#82111=CARTESIAN_POINT('Ctrl Pts',(0.122065826151406,0.15258143427683,-0.567210570706171));
#82112=CARTESIAN_POINT('Ctrl Pts',(0.112517430799842,0.16022019303233,-0.566513882320146));
#82113=CARTESIAN_POINT('Ctrl Pts',(0.102266670976131,0.166945429535853,
-0.565817193934121));
#82114=CARTESIAN_POINT('Ctrl Pts',(0.0915146647020496,0.172644797617743,
-0.565120505548097));
#82115=CARTESIAN_POINT('Ctrl Pts',(0.0881811548838333,0.174411807324983,
-0.564904507015744));
#82116=CARTESIAN_POINT('Ctrl Pts',(0.084799629294112,0.176080549022716,
-0.564688508483391));
#82117=CARTESIAN_POINT('Ctrl Pts',(0.0813764670325799,0.177648615568192,
-0.564472509951038));
#82118=CARTESIAN_POINT('Ctrl Pts',(0.0703353295471433,0.182706289435856,
-0.563775823872449));
#82119=CARTESIAN_POINT('Ctrl Pts',(0.0587821276928241,0.186748443058392,
-0.56307913779386));
#82120=CARTESIAN_POINT('Ctrl Pts',(0.046926463790817,0.18968148827993,-0.562382451715271));
#82121=CARTESIAN_POINT('Ctrl Pts',(0.0350955366848213,0.192608413714171,
-0.561687219269439));
#82122=CARTESIAN_POINT('Ctrl Pts',(0.0229642233891814,0.194430544371172,
-0.560991986823608));
#82123=CARTESIAN_POINT('Ctrl Pts',(0.0107585223315926,0.19510359862709,
-0.560296754377776));
#82124=CARTESIAN_POINT('Ctrl Pts',(-0.00144549314628636,0.195776559935737,
-0.559601617941973));
#82125=CARTESIAN_POINT('Ctrl Pts',(-0.0137230061700573,0.195300666488192,
-0.558906481506169));
#82126=CARTESIAN_POINT('Ctrl Pts',(-0.02584307137875,0.19368349351897,-0.558211345070366));
#82127=CARTESIAN_POINT('Ctrl Pts',(-0.0379625078328463,0.192066404444093,
-0.557516244696269));
#82128=CARTESIAN_POINT('Ctrl Pts',(-0.0499236489753525,0.189308295920255,
-0.556821144322172));
#82129=CARTESIAN_POINT('Ctrl Pts',(-0.0615036123781013,0.185468233572341,
-0.556126043948074));
#82130=CARTESIAN_POINT('Ctrl Pts',(-0.0731100311255822,0.18161939829746,
-0.555429355562048));
#82131=CARTESIAN_POINT('Ctrl Pts',(-0.0843327243602488,0.176684011833073,
-0.554732667176022));
#82132=CARTESIAN_POINT('Ctrl Pts',(-0.0949679454458698,0.170769579661573,
-0.554035978789996));
#82133=CARTESIAN_POINT('Ctrl Pts',(-0.0982652476425931,0.168935892328281,
-0.55381998025765));
#82134=CARTESIAN_POINT('Ctrl Pts',(-0.101506276568824,0.167008421014308,
-0.553603981725303));
#82135=CARTESIAN_POINT('Ctrl Pts',(-0.104685539550776,0.164991205247319,
-0.553387983192956));
#82136=CARTESIAN_POINT('Ctrl Pts',(-0.114939999317868,0.158484836305347,
-0.552691297114367));
#82137=CARTESIAN_POINT('Ctrl Pts',(-0.124621557139461,0.150995983446465,
-0.551994611035779));
#82138=CARTESIAN_POINT('Ctrl Pts',(-0.133537579149304,0.142649482841486,
-0.55129792495719));
#82139=CARTESIAN_POINT('Ctrl Pts',(-0.14243499791436,0.134320397177128,
-0.550602692511358));
#82140=CARTESIAN_POINT('Ctrl Pts',(-0.150569368421779,0.125137753829151,
-0.549907460065527));
#82141=CARTESIAN_POINT('Ctrl Pts',(-0.157780483132415,0.115266990689016,
-0.549212227619695));
#82142=CARTESIAN_POINT('Ctrl Pts',(-0.164990602004419,0.105397590678945,
-0.548517091183892));
#82143=CARTESIAN_POINT('Ctrl Pts',(-0.171277166213182,0.0948409382232021,
-0.547821954748089));
#82144=CARTESIAN_POINT('Ctrl Pts',(-0.176520768217102,0.0837948589595091,
-0.547126818312286));
#82145=CARTESIAN_POINT('Ctrl Pts',(-0.181764098197827,0.0727493527350705,
-0.546431717938189));
#82146=CARTESIAN_POINT('Ctrl Pts',(-0.185964222600671,0.0612152721448906,
-0.545736617564093));
#82147=CARTESIAN_POINT('Ctrl Pts',(-0.189049311026348,0.0494117192623678,
-0.545041517189996));
#82148=CARTESIAN_POINT('Ctrl Pts',(-0.192141447581195,0.037581200227212,
-0.54434482880397));
#82149=CARTESIAN_POINT('Ctrl Pts',(-0.194113304827838,0.0254808422989893,
-0.543648140417944));
#82150=CARTESIAN_POINT('Ctrl Pts',(-0.194944100655711,0.0133400756945423,
-0.542951452031918));
#82151=CARTESIAN_POINT('Ctrl Pts',(-0.195201677332887,0.00957600007519466,
-0.542735453499571));
#82152=CARTESIAN_POINT('Ctrl Pts',(-0.195349951110585,0.0058080524835065,
-0.542519454967224));
#82153=CARTESIAN_POINT('Ctrl Pts',(-0.195389319026348,0.00204303950528141,
-0.542303456434878));
#82154=CARTESIAN_POINT('Ctrl Pts',(-0.195396396017583,0.00136622023931689,
-0.542264627360726));
#82155=CARTESIAN_POINT('Ctrl Pts',(-0.195399956318106,0.000689364137931553,
-0.542225798286575));
#82156=CARTESIAN_POINT('Ctrl Pts',(-0.195399999600508,1.24948518317515E-5,
-0.542186969212424));
#82157=CARTESIAN_POINT('',(-0.19539994003323,0.000153084976888024,-0.472186969216991));
#82158=CARTESIAN_POINT('Ctrl Pts',(-0.195399999600512,1.24947932979144E-5,
-0.542186969209066));
#82159=CARTESIAN_POINT('Ctrl Pts',(-0.195400774759589,-0.0121098412592945,
-0.541491563027797));
#82160=CARTESIAN_POINT('Ctrl Pts',(-0.194269147082837,-0.0242755331708231,
-0.540796156846527));
#82161=CARTESIAN_POINT('Ctrl Pts',(-0.192006980379885,-0.0362557510665349,
-0.540100750665258));
#82162=CARTESIAN_POINT('Ctrl Pts',(-0.189749524678251,-0.0482110199510932,
-0.539406792679399));
#82163=CARTESIAN_POINT('Ctrl Pts',(-0.186366290974367,-0.0599807128695843,
-0.53871283469354));
#82164=CARTESIAN_POINT('Ctrl Pts',(-0.181910805132108,-0.0713415655574515,
-0.538018876707681));
#82165=CARTESIAN_POINT('Ctrl Pts',(-0.177455905552505,-0.0827009233592614,
-0.537325010034345));
#82166=CARTESIAN_POINT('Ctrl Pts',(-0.171929312599577,-0.0936507146707394,
-0.536631143361008));
#82167=CARTESIAN_POINT('Ctrl Pts',(-0.165433757398891,-0.10398476769645,
-0.535937276687672));
#82168=CARTESIAN_POINT('Ctrl Pts',(-0.158938385641453,-0.114318528874554,
-0.535243429610067));
#82169=CARTESIAN_POINT('Ctrl Pts',(-0.151474597899374,-0.124035857891667,
-0.534549582532462));
#82170=CARTESIAN_POINT('Ctrl Pts',(-0.143188554114146,-0.132959384665771,
-0.533855735454857));
#82171=CARTESIAN_POINT('Ctrl Pts',(-0.134883733044484,-0.141903133346097,
-0.533160316026892));
#82172=CARTESIAN_POINT('Ctrl Pts',(-0.125753584127312,-0.150048893232625,
-0.532464896598927));
#82173=CARTESIAN_POINT('Ctrl Pts',(-0.115980235201907,-0.157256939568689,
-0.531769477170962));
#82174=CARTESIAN_POINT('Ctrl Pts',(-0.113401123688238,-0.159159087485262,
-0.531585961339573));
#82175=CARTESIAN_POINT('Ctrl Pts',(-0.110777377410633,-0.160996168259883,
-0.531402445508185));
#82176=CARTESIAN_POINT('Ctrl Pts',(-0.108112652127949,-0.162766134222881,
-0.531218929676797));
#82177=CARTESIAN_POINT('Ctrl Pts',(-0.0979964839823108,-0.169485503536523,
-0.530522243598208));
#82178=CARTESIAN_POINT('Ctrl Pts',(-0.0872159900895472,-0.175281746321541,
-0.529825557519619));
#82179=CARTESIAN_POINT('Ctrl Pts',(-0.0759635920383071,-0.180029699451612,
-0.52912887144103));
#82180=CARTESIAN_POINT('Ctrl Pts',(-0.0647346720712546,-0.184767745996189,
-0.528433638995198));
#82181=CARTESIAN_POINT('Ctrl Pts',(-0.0530365717809753,-0.188461439541515,
-0.527738406549367));
#82182=CARTESIAN_POINT('Ctrl Pts',(-0.0410856054130471,-0.191031759212554,
-0.527043174103535));
#82183=CARTESIAN_POINT('Ctrl Pts',(-0.0291362894465465,-0.19360172392826,
-0.526348037667732));
#82184=CARTESIAN_POINT('Ctrl Pts',(-0.0169350213056709,-0.195048394718982,
-0.525652901231929));
#82185=CARTESIAN_POINT('Ctrl Pts',(-0.00471109725244599,-0.195343199427771,
-0.524957764796126));
#82186=CARTESIAN_POINT('Ctrl Pts',(0.00751219265827948,-0.195637988842929,
-0.524262664422029));
#82187=CARTESIAN_POINT('Ctrl Pts',(0.0197572607745834,-0.194781036751348,
-0.523567564047932));
#82188=CARTESIAN_POINT('Ctrl Pts',(0.0317947363763054,-0.192795888801502,
-0.522872463673835));
#82189=CARTESIAN_POINT('Ctrl Pts',(0.0438597125456626,-0.190806205623735,
-0.522175775287809));
#82190=CARTESIAN_POINT('Ctrl Pts',(0.0557152973938653,-0.187683387841771,
-0.521479086901783));
#82191=CARTESIAN_POINT('Ctrl Pts',(0.067143459072765,-0.183501814442648,
-0.520782398515756));
#82192=CARTESIAN_POINT('Ctrl Pts',(0.0706866014583335,-0.18220537584079,
-0.52056639998341));
#82193=CARTESIAN_POINT('Ctrl Pts',(0.0741888018429137,-0.180807517967788,
-0.520350401451063));
#82194=CARTESIAN_POINT('Ctrl Pts',(0.0776440042616577,-0.179311373320868,
-0.520134402918717));
#82195=CARTESIAN_POINT('Ctrl Pts',(0.0887884847249885,-0.174485677813866,
-0.519437716840128));
#82196=CARTESIAN_POINT('Ctrl Pts',(0.0995204703340839,-0.168600105294485,
-0.518741030761539));
#82197=CARTESIAN_POINT('Ctrl Pts',(0.109630200136307,-0.161747887831877,
-0.51804434468295));
#82198=CARTESIAN_POINT('Ctrl Pts',(0.11971883602714,-0.154909967493999,
-0.517349112237119));
#82199=CARTESIAN_POINT('Ctrl Pts',(0.129187034635739,-0.147109830474931,
-0.516653879791288));
#82200=CARTESIAN_POINT('Ctrl Pts',(0.137850725122369,-0.138485875031488,
-0.515958647345456));
#82201=CARTESIAN_POINT('Ctrl Pts',(0.146513219172936,-0.129863110536789,
-0.515263510909653));
#82202=CARTESIAN_POINT('Ctrl Pts',(0.154370774492035,-0.120417337671136,
-0.51456837447385));
#82203=CARTESIAN_POINT('Ctrl Pts',(0.161274563691475,-0.110325314892478,
-0.513873238038047));
#82204=CARTESIAN_POINT('Ctrl Pts',(0.16817799474192,-0.100233815659326,
-0.51317813766395));
#82205=CARTESIAN_POINT('Ctrl Pts',(0.174127286203008,-0.0894968705085294,
-0.512483037289853));
#82206=CARTESIAN_POINT('Ctrl Pts',(0.179017282850342,-0.0783196810570658,
-0.511787936915756));
#82207=CARTESIAN_POINT('Ctrl Pts',(0.183918451082812,-0.0671169564299077,
-0.51109124852973));
#82208=CARTESIAN_POINT('Ctrl Pts',(0.187755202693892,-0.0554728068230441,
-0.510394560143704));
#82209=CARTESIAN_POINT('Ctrl Pts',(0.190471192423205,-0.0436106048671915,
-0.509697871757678));
#82210=CARTESIAN_POINT('Ctrl Pts',(0.19131324721724,-0.0399328943379754,
-0.509481873225331));
#82211=CARTESIAN_POINT('Ctrl Pts',(0.192047943803405,-0.0362342952662712,
-0.509265874692984));
#82212=CARTESIAN_POINT('Ctrl Pts',(0.192674611726904,-0.0325215927636833,
-0.509049876160637));
#82213=CARTESIAN_POINT('Ctrl Pts',(0.194695879248751,-0.0205465662698088,
-0.508353190082048));
#82214=CARTESIAN_POINT('Ctrl Pts',(0.195603573544156,-0.00834035596272215,
-0.507656504003459));
#82215=CARTESIAN_POINT('Ctrl Pts',(0.195361665887142,0.00387033613536681,
-0.50695981792487));
#82216=CARTESIAN_POINT('Ctrl Pts',(0.195120262969501,0.0160555506725137,
-0.506264585479039));
#82217=CARTESIAN_POINT('Ctrl Pts',(0.193733962486938,0.0282443608433282,
-0.505569353033207));
#82218=CARTESIAN_POINT('Ctrl Pts',(0.19121860743086,0.0402070164548739,
-0.504874120587376));
#82219=CARTESIAN_POINT('Ctrl Pts',(0.188703599739626,0.052168020050737,
-0.504178984151573));
#82220=CARTESIAN_POINT('Ctrl Pts',(0.185059982402041,0.0639020668087616,
-0.50348384771577));
#82221=CARTESIAN_POINT('Ctrl Pts',(0.1803549640121,0.0751880772210209,-0.502788711279967));
#82222=CARTESIAN_POINT('Ctrl Pts',(0.175650189705162,0.086473502147082,
-0.50209361090587));
#82223=CARTESIAN_POINT('Ctrl Pts',(0.169884485307396,0.0973101396725234,
-0.501398510531773));
#82224=CARTESIAN_POINT('Ctrl Pts',(0.163172697153958,0.107498050696293,
-0.500703410157675));
#82225=CARTESIAN_POINT('Ctrl Pts',(0.156445575388213,0.117709236810736,
-0.50000672177165));
#82226=CARTESIAN_POINT('Ctrl Pts',(0.148768590520948,0.12726804355321,-0.499310033385624));
#82227=CARTESIAN_POINT('Ctrl Pts',(0.140298408868267,0.136005575139523,
-0.498613344999598));
#82228=CARTESIAN_POINT('Ctrl Pts',(0.137672346998442,0.138714525133288,
-0.498397346467251));
#82229=CARTESIAN_POINT('Ctrl Pts',(0.134970303478862,0.141344805533783,
-0.498181347934904));
#82230=CARTESIAN_POINT('Ctrl Pts',(0.132197604083141,0.143892159184151,
-0.497965349402556));
#82231=CARTESIAN_POINT('Ctrl Pts',(0.123254482812271,0.152108445684661,
-0.497268663323968));
#82232=CARTESIAN_POINT('Ctrl Pts',(0.113511065593818,0.159516637090257,
-0.496571977245379));
#82233=CARTESIAN_POINT('Ctrl Pts',(0.103137874553166,0.165963064663965,
-0.49587529116679));
#82234=CARTESIAN_POINT('Ctrl Pts',(0.092786327134741,0.172396041791944,
-0.495180058720958));
#82235=CARTESIAN_POINT('Ctrl Pts',(0.0818083109103004,0.177870718237551,
-0.494484826275126));
#82236=CARTESIAN_POINT('Ctrl Pts',(0.0704051512959251,0.182275271693661,
-0.493789593829295));
#82237=CARTESIAN_POINT('Ctrl Pts',(0.0590035664321041,0.186679216890899,
-0.493094457393492));
#82238=CARTESIAN_POINT('Ctrl Pts',(0.047177753357304,0.190012975391768,
-0.492399320957689));
#82239=CARTESIAN_POINT('Ctrl Pts',(0.0351497362308519,0.19221252831931,
-0.491704184521886));
#82240=CARTESIAN_POINT('Ctrl Pts',(0.0231223430838024,0.194411967140287,
-0.491009084147789));
#82241=CARTESIAN_POINT('Ctrl Pts',(0.0108936322782355,0.195477186410669,
-0.490313983773692));
#82242=CARTESIAN_POINT('Ctrl Pts',(-0.00130616200337565,0.195395634395503,
-0.489618883399595));
#82243=CARTESIAN_POINT('Ctrl Pts',(-0.0135338276825206,0.19531389606829,
-0.488922195013569));
#82244=CARTESIAN_POINT('Ctrl Pts',(-0.0257315711095326,0.194080227441351,
-0.488225506627542));
#82245=CARTESIAN_POINT('Ctrl Pts',(-0.0376724219922772,0.191734057019706,
-0.487528818241516));
#82246=CARTESIAN_POINT('Ctrl Pts',(-0.0413745165260365,0.191006659552094,
-0.48731281970917));
#82247=CARTESIAN_POINT('Ctrl Pts',(-0.045052004343916,0.190172694615065,
-0.487096821176823));
#82248=CARTESIAN_POINT('Ctrl Pts',(-0.0486984146996827,0.189234310857565,
-0.486880822644477));
#82249=CARTESIAN_POINT('Ctrl Pts',(-0.0604596211490331,0.186207628717083,
-0.486184136565888));
#82250=CARTESIAN_POINT('Ctrl Pts',(-0.0719788553954887,0.182069667701086,
-0.4854874504873));
#82251=CARTESIAN_POINT('Ctrl Pts',(-0.0830343733418138,0.176879769458614,
-0.484790764408711));
#82252=CARTESIAN_POINT('Ctrl Pts',(-0.0940668239935134,0.17170069991837,
-0.48409553196288));
#82253=CARTESIAN_POINT('Ctrl Pts',(-0.104636663244794,0.165474351019529,
-0.483400299517049));
#82254=CARTESIAN_POINT('Ctrl Pts',(-0.114540470901671,0.158308687460996,
-0.482705067071217));
#82255=CARTESIAN_POINT('Ctrl Pts',(-0.124442910865109,0.151144013464396,
-0.482009930635415));
#82256=CARTESIAN_POINT('Ctrl Pts',(-0.133678767441387,0.143040757703623,
-0.481314794199612));
#82257=CARTESIAN_POINT('Ctrl Pts',(-0.142073443071281,0.13415027683114,
-0.480619657763809));
#82258=CARTESIAN_POINT('Ctrl Pts',(-0.150467683209224,0.125260257171577,
-0.479924557389713));
#82259=CARTESIAN_POINT('Ctrl Pts',(-0.158020247992978,0.115583748232537,
-0.479229457015616));
#82260=CARTESIAN_POINT('Ctrl Pts',(-0.16459523608154,0.105307019040814,
-0.478534356641519));
#82261=CARTESIAN_POINT('Ctrl Pts',(-0.171185245251811,0.0950068118462686,
-0.477837668255493));
#82262=CARTESIAN_POINT('Ctrl Pts',(-0.176792803044107,0.0841044185953307,
-0.477140979869468));
#82263=CARTESIAN_POINT('Ctrl Pts',(-0.181327382796066,0.0728116765933106,
-0.476444291483442));
#82264=CARTESIAN_POINT('Ctrl Pts',(-0.18273326610184,0.0693105191927391,
-0.476228292951094));
#82265=CARTESIAN_POINT('Ctrl Pts',(-0.184036368623349,0.0657719689266645,
-0.476012294418746));
#82266=CARTESIAN_POINT('Ctrl Pts',(-0.185234968854937,0.0622026230420426,
-0.475796295886397));
#82267=CARTESIAN_POINT('Ctrl Pts',(-0.189780639450348,0.0486659406645715,
-0.474977125197729));
#82268=CARTESIAN_POINT('Ctrl Pts',(-0.192845581036781,0.0346083663153122,
-0.474157954509061));
#82269=CARTESIAN_POINT('Ctrl Pts',(-0.194339139427583,0.0203336884638898,
-0.473338783820393));
#82270=CARTESIAN_POINT('Ctrl Pts',(-0.195039157299054,0.0136432706891088,
-0.472954845619259));
#82271=CARTESIAN_POINT('Ctrl Pts',(-0.195394649920554,0.00690546343110999,
-0.472570907418125));
#82272=CARTESIAN_POINT('Ctrl Pts',(-0.19539994003323,0.000153084976888612,
-0.472186969216991));
#82273=CARTESIAN_POINT('',(-0.195399955328571,-0.000132127182848954,-0.402186969207341));
#82274=CARTESIAN_POINT('Ctrl Pts',(-0.195399940033293,0.000153084896563632,
-0.472186969212424));
#82275=CARTESIAN_POINT('Ctrl Pts',(-0.19540950022769,-0.0120496957420093,
-0.471493122787954));
#82276=CARTESIAN_POINT('Ctrl Pts',(-0.19427161528297,-0.0242672138561955,
-0.470799276363485));
#82277=CARTESIAN_POINT('Ctrl Pts',(-0.192004361224299,-0.0362696191164001,
-0.470105429939015));
#82278=CARTESIAN_POINT('Ctrl Pts',(-0.189737689439945,-0.0482689419287917,
-0.469411761707611));
#82279=CARTESIAN_POINT('Ctrl Pts',(-0.186342403735455,-0.0600524012197707,
-0.468718093476208));
#82280=CARTESIAN_POINT('Ctrl Pts',(-0.18188770489363,-0.0714004398342741,
-0.468024425244804));
#82281=CARTESIAN_POINT('Ctrl Pts',(-0.177421977072317,-0.0827765740147284,
-0.467329039623973));
#82282=CARTESIAN_POINT('Ctrl Pts',(-0.171891965994688,-0.0937143332632155,
-0.466633654003141));
#82283=CARTESIAN_POINT('Ctrl Pts',(-0.165414615592323,-0.104015214985328,
-0.46593826838231));
#82284=CARTESIAN_POINT('Ctrl Pts',(-0.161606433389355,-0.110071338556273,
-0.465529435297646));
#82285=CARTESIAN_POINT('Ctrl Pts',(-0.157471670309908,-0.115907817660625,
-0.465120602212981));
#82286=CARTESIAN_POINT('Ctrl Pts',(-0.153040690612817,-0.121489534597644,
-0.464711769128317));
#82287=CARTESIAN_POINT('Ctrl Pts',(-0.145489927268878,-0.131001251311659,
-0.464015083049728));
#82288=CARTESIAN_POINT('Ctrl Pts',(-0.137022523335021,-0.139839721180116,
-0.463318396971139));
#82289=CARTESIAN_POINT('Ctrl Pts',(-0.127782919780465,-0.147826538254737,
-0.462621710892551));
#82290=CARTESIAN_POINT('Ctrl Pts',(-0.118562594622314,-0.155796690867007,
-0.461926478446719));
#82291=CARTESIAN_POINT('Ctrl Pts',(-0.10857387499208,-0.162918095402392,
-0.461231246000888));
#82292=CARTESIAN_POINT('Ctrl Pts',(-0.0979981603981727,-0.169048870326228,
-0.460536013555057));
#82293=CARTESIAN_POINT('Ctrl Pts',(-0.0874239062865325,-0.175178798603914,
-0.459840877119254));
#82294=CARTESIAN_POINT('Ctrl Pts',(-0.0762635512230363,-0.180317891469279,
-0.459145740683451));
#82295=CARTESIAN_POINT('Ctrl Pts',(-0.0647264025934293,-0.184368253252325,
-0.458450604247648));
#82296=CARTESIAN_POINT('Ctrl Pts',(-0.0531898524783568,-0.188418404914094,
-0.457755503873551));
#82297=CARTESIAN_POINT('Ctrl Pts',(-0.0412773821397646,-0.191379673306578,
-0.457060403499454));
#82298=CARTESIAN_POINT('Ctrl Pts',(-0.0292144432181752,-0.193203717116033,
-0.456365303125357));
#82299=CARTESIAN_POINT('Ctrl Pts',(-0.0171239455559803,-0.195031928098224,
-0.455668614739331));
#82300=CARTESIAN_POINT('Ctrl Pts',(-0.00488316729722413,-0.195717661728824,
-0.454971926353305));
#82301=CARTESIAN_POINT('Ctrl Pts',(0.00727754878625668,-0.195264429130509,
-0.454275237967279));
#82302=CARTESIAN_POINT('Ctrl Pts',(0.0110478094637903,-0.195123910674896,
-0.454059239434932));
#82303=CARTESIAN_POINT('Ctrl Pts',(0.01481040213799,-0.194874289892408,
-0.453843240902584));
#82304=CARTESIAN_POINT('Ctrl Pts',(0.0185585999625431,-0.19451667889266,
-0.453627242370237));
#82305=CARTESIAN_POINT('Ctrl Pts',(0.0306481137929486,-0.193363233068902,
-0.452930556291648));
#82306=CARTESIAN_POINT('Ctrl Pts',(0.0426721119260769,-0.191074358260331,
-0.452233870213059));
#82307=CARTESIAN_POINT('Ctrl Pts',(0.0544023049230485,-0.187674050467985,
-0.45153718413447));
#82308=CARTESIAN_POINT('Ctrl Pts',(0.0661080229185633,-0.184280837404446,
-0.450841951688638));
#82309=CARTESIAN_POINT('Ctrl Pts',(0.0775202999573865,-0.179780964606533,
-0.450146719242806));
#82310=CARTESIAN_POINT('Ctrl Pts',(0.0884213549394379,-0.174249315610346,
-0.449451486796974));
#82311=CARTESIAN_POINT('Ctrl Pts',(0.0993209045104476,-0.168718430522376,
-0.448756350361171));
#82312=CARTESIAN_POINT('Ctrl Pts',(0.109708572580216,-0.162156407001039,
-0.448061213925368));
#82313=CARTESIAN_POINT('Ctrl Pts',(0.119388273052745,-0.154685488192924,
-0.447366077489565));
#82314=CARTESIAN_POINT('Ctrl Pts',(0.129067471369876,-0.14721495695488,
-0.446670977115468));
#82315=CARTESIAN_POINT('Ctrl Pts',(0.138038098868157,-0.138836180054443,
-0.445975876741371));
#82316=CARTESIAN_POINT('Ctrl Pts',(0.146136840781684,-0.129711926076012,
-0.445280776367273));
#82317=CARTESIAN_POINT('Ctrl Pts',(0.154254084913376,-0.120566827015775,
-0.444584087981247));
#82318=CARTESIAN_POINT('Ctrl Pts',(0.161494935443626,-0.110673548156325,
-0.443887399595221));
#82319=CARTESIAN_POINT('Ctrl Pts',(0.16773690428218,-0.100227196617639,
-0.443190711209195));
#82320=CARTESIAN_POINT('Ctrl Pts',(0.169672139797977,-0.0969884507938373,
-0.442974712676849));
#82321=CARTESIAN_POINT('Ctrl Pts',(0.171511692433523,-0.0936967247621157,
-0.442758714144502));
#82322=CARTESIAN_POINT('Ctrl Pts',(0.173252831848573,-0.0903582661213127,
-0.442542715612156));
#82323=CARTESIAN_POINT('Ctrl Pts',(0.178868738485392,-0.079590333424156,
-0.441846029533567));
#82324=CARTESIAN_POINT('Ctrl Pts',(0.183496651492235,-0.0682590536996094,
-0.441149343454978));
#82325=CARTESIAN_POINT('Ctrl Pts',(0.187032382179265,-0.0565689669019102,
-0.440452657376389));
#82326=CARTESIAN_POINT('Ctrl Pts',(0.19056073557815,-0.0449032714242446,
-0.439757424930557));
#82327=CARTESIAN_POINT('Ctrl Pts',(0.193001108433104,-0.0328810626946885,
-0.439062192484725));
#82328=CARTESIAN_POINT('Ctrl Pts',(0.19429771520829,-0.0207257777860888,
-0.438366960038894));
#82329=CARTESIAN_POINT('Ctrl Pts',(0.195594142925012,-0.00857217149484689,
-0.437671823603091));
#82330=CARTESIAN_POINT('Ctrl Pts',(0.195746980373878,0.003713610585935,
-0.436976687167288));
#82331=CARTESIAN_POINT('Ctrl Pts',(0.194751977890278,0.0159005379728084,
-0.436281550731485));
#82332=CARTESIAN_POINT('Ctrl Pts',(0.193757027024584,0.0280868331364667,
-0.435586450357388));
#82333=CARTESIAN_POINT('Ctrl Pts',(0.191614452601334,0.0401734139143807,
-0.434891349983291));
#82334=CARTESIAN_POINT('Ctrl Pts',(0.188371840413358,0.0519346679905087,
-0.434196249609194));
#82335=CARTESIAN_POINT('Ctrl Pts',(0.185121820220687,0.0637227915842889,
-0.433499561223168));
#82336=CARTESIAN_POINT('Ctrl Pts',(0.180767040576033,0.0751832792370354,
-0.432802872837142));
#82337=CARTESIAN_POINT('Ctrl Pts',(0.175404442670033,0.0861071512222719,
-0.432106184451116));
#82338=CARTESIAN_POINT('Ctrl Pts',(0.173741843866187,0.0894939456108076,
-0.431890185918769));
#82339=CARTESIAN_POINT('Ctrl Pts',(0.171982704995381,0.0928293383313204,
-0.431674187386423));
#82340=CARTESIAN_POINT('Ctrl Pts',(0.170130779294777,0.0961076372436237,
-0.431458188854077));
#82341=CARTESIAN_POINT('Ctrl Pts',(0.164157540309418,0.106681529523558,
-0.430761502775488));
#82342=CARTESIAN_POINT('Ctrl Pts',(0.157173794755142,0.116733533156061,
-0.430064816696899));
#82343=CARTESIAN_POINT('Ctrl Pts',(0.149294360337056,0.126064880008468,
-0.42936813061831));
#82344=CARTESIAN_POINT('Ctrl Pts',(0.141431366327829,0.135376757042442,
-0.428672898172479));
#82345=CARTESIAN_POINT('Ctrl Pts',(0.13267689542265,0.143970252348691,-0.427977665726647));
#82346=CARTESIAN_POINT('Ctrl Pts',(0.123187972784648,0.151676904508263,
-0.427282433280815));
#82347=CARTESIAN_POINT('Ctrl Pts',(0.113700360545405,0.159382492396599,
-0.426587296845013));
#82348=CARTESIAN_POINT('Ctrl Pts',(0.103479147494276,0.166200894290413,
-0.42589216040921));
#82349=CARTESIAN_POINT('Ctrl Pts',(0.0927157914244005,0.172002738410024,
-0.425197023973407));
#82350=CARTESIAN_POINT('Ctrl Pts',(0.0819529937268978,0.177804281546424,
-0.42450192359931));
#82351=CARTESIAN_POINT('Ctrl Pts',(0.0706488918858232,0.182588980244017,
-0.423806823225213));
#82352=CARTESIAN_POINT('Ctrl Pts',(0.0590186262771717,0.186273889078302,
-0.423111722851116));
#82353=CARTESIAN_POINT('Ctrl Pts',(0.0473617904044113,0.189967216379047,
-0.42241503446509));
#82354=CARTESIAN_POINT('Ctrl Pts',(0.0353781563987997,0.19255553610653,
-0.421718346079064));
#82355=CARTESIAN_POINT('Ctrl Pts',(0.0232957908446915,0.194006355898255,
-0.421021657693038));
#82356=CARTESIAN_POINT('Ctrl Pts',(0.0195498216577193,0.194456162371277,
-0.420805659160691));
#82357=CARTESIAN_POINT('Ctrl Pts',(0.0157943937200415,0.194797007162778,
-0.420589660628343));
#82358=CARTESIAN_POINT('Ctrl Pts',(0.0120363250164336,0.195028938570918,
-0.420373662095996));
#82359=CARTESIAN_POINT('Ctrl Pts',(-8.50265489191378E-5,0.195777014872558,
-0.419676976017407));
#82360=CARTESIAN_POINT('Ctrl Pts',(-0.01231892555592,0.19539335606406,-0.418980289938818));
#82361=CARTESIAN_POINT('Ctrl Pts',(-0.0244361355376008,0.193866024047506,
-0.418283603860229));
#82362=CARTESIAN_POINT('Ctrl Pts',(-0.0365280630084035,0.192341878803185,
-0.417588371414398));
#82363=CARTESIAN_POINT('Ctrl Pts',(-0.048502915982378,0.189678831927933,
-0.416893138968566));
#82364=CARTESIAN_POINT('Ctrl Pts',(-0.0601338930722158,0.185916849435384,
-0.416197906522735));
#82365=CARTESIAN_POINT('Ctrl Pts',(-0.0717632639504217,0.18215538646411,
-0.415502770086932));
#82366=CARTESIAN_POINT('Ctrl Pts',(-0.0830480080197834,0.177295514870008,
-0.414807633651129));
#82367=CARTESIAN_POINT('Ctrl Pts',(-0.0937753592425063,0.17142736654029,
-0.414112497215327));
#82368=CARTESIAN_POINT('Ctrl Pts',(-0.104502153960684,0.165559522633457,
-0.41341739684123));
#82369=CARTESIAN_POINT('Ctrl Pts',(-0.114670858589535,0.158683949476888,
-0.412722296467133));
#82370=CARTESIAN_POINT('Ctrl Pts',(-0.124094749885975,0.150935923658807,
-0.412027196093036));
#82371=CARTESIAN_POINT('Ctrl Pts',(-0.133540170809439,0.143170196861291,
-0.41133050770701));
#82372=CARTESIAN_POINT('Ctrl Pts',(-0.14223674759943,0.134528644042031,
-0.410633819320984));
#82373=CARTESIAN_POINT('Ctrl Pts',(-0.15003303449803,0.125184857547999,
-0.409937130934958));
#82374=CARTESIAN_POINT('Ctrl Pts',(-0.15245016468368,0.122287946662505,
-0.409721132402611));
#82375=CARTESIAN_POINT('Ctrl Pts',(-0.15478105631248,0.11932376745373,-0.409505133870263));
#82376=CARTESIAN_POINT('Ctrl Pts',(-0.15702203716539,0.116298064663308,
-0.409289135337916));
#82377=CARTESIAN_POINT('Ctrl Pts',(-0.164283431344131,0.106493955627549,
-0.40858924069876));
#82378=CARTESIAN_POINT('Ctrl Pts',(-0.170648781995794,0.0959725610274841,
-0.407889346059604));
#82379=CARTESIAN_POINT('Ctrl Pts',(-0.175981797535575,0.0849209452146396,
-0.407189451420448));
#82380=CARTESIAN_POINT('Ctrl Pts',(-0.18130290098295,0.0738940148481088,
-0.406491120101247));
#82381=CARTESIAN_POINT('Ctrl Pts',(-0.185595803747284,0.0623399493630731,
-0.405792788782047));
#82382=CARTESIAN_POINT('Ctrl Pts',(-0.188768944226097,0.0504722269744916,
-0.405094457462846));
#82383=CARTESIAN_POINT('Ctrl Pts',(-0.191939372373936,0.0386146488550512,
-0.40439672306196));
#82384=CARTESIAN_POINT('Ctrl Pts',(-0.193991676483236,0.026444767287892,
-0.403698988661075));
#82385=CARTESIAN_POINT('Ctrl Pts',(-0.194883961543337,0.0141916007967856,
-0.403001254260189));
#82386=CARTESIAN_POINT('Ctrl Pts',(-0.195231072794582,0.00942494926059903,
-0.402729825910934));
#82387=CARTESIAN_POINT('Ctrl Pts',(-0.195403186105232,0.00464579988061832,
-0.402458397561678));
#82388=CARTESIAN_POINT('Ctrl Pts',(-0.195399955328631,-0.000132127093388512,
-0.402186969212423));
#82389=CARTESIAN_POINT('',(-0.195399993177235,-5.16365805523595E-5,-0.332186969215685));
#82390=CARTESIAN_POINT('Ctrl Pts',(-0.195399955328571,-0.000132127182848178,
-0.402186969207341));
#82391=CARTESIAN_POINT('Ctrl Pts',(-0.195390495806332,-0.0141216044664258,
-0.401392243639799));
#82392=CARTESIAN_POINT('Ctrl Pts',(-0.193874546778018,-0.0280515508001564,
-0.400597518072257));
#82393=CARTESIAN_POINT('Ctrl Pts',(-0.190914403766276,-0.0416275201587533,
-0.399802792504715));
#82394=CARTESIAN_POINT('Ctrl Pts',(-0.188930132645979,-0.0507278926142205,
-0.399270064529755));
#82395=CARTESIAN_POINT('Ctrl Pts',(-0.186297990982151,-0.0596695466865476,
-0.398737336554796));
#82396=CARTESIAN_POINT('Ctrl Pts',(-0.183048772006924,-0.0683689042383835,
-0.398204608579836));
#82397=CARTESIAN_POINT('Ctrl Pts',(-0.178799538377885,-0.079745669837172,
-0.397507922501247));
#82398=CARTESIAN_POINT('Ctrl Pts',(-0.173470712728011,-0.0907647031971384,
-0.396811236422658));
#82399=CARTESIAN_POINT('Ctrl Pts',(-0.167144673837974,-0.101211748367456,
-0.396114550344069));
#82400=CARTESIAN_POINT('Ctrl Pts',(-0.160831834203152,-0.111636995819194,
-0.395419317898238));
#82401=CARTESIAN_POINT('Ctrl Pts',(-0.153526296825704,-0.121491844678251,
-0.394724085452406));
#82402=CARTESIAN_POINT('Ctrl Pts',(-0.145356861814906,-0.13058538479984,
-0.394028853006575));
#82403=CARTESIAN_POINT('Ctrl Pts',(-0.137188554984605,-0.139677669124106,
-0.393333716570772));
#82404=CARTESIAN_POINT('Ctrl Pts',(-0.128157137483981,-0.1480081732236,
-0.392638580134969));
#82405=CARTESIAN_POINT('Ctrl Pts',(-0.118431522417887,-0.155419221777043,
-0.391943443699166));
#82406=CARTESIAN_POINT('Ctrl Pts',(-0.108706411889108,-0.162829885866313,
-0.391248343325069));
#82407=CARTESIAN_POINT('Ctrl Pts',(-0.0982878876309854,-0.169320680297132,
-0.390553242950972));
#82408=CARTESIAN_POINT('Ctrl Pts',(-0.0873755028942675,-0.174776089594583,
-0.389858142576875));
#82409=CARTESIAN_POINT('Ctrl Pts',(-0.0764381879492221,-0.180243962207211,
-0.389161454190848));
#82410=CARTESIAN_POINT('Ctrl Pts',(-0.0650055713650576,-0.184671394988378,
-0.388464765804822));
#82411=CARTESIAN_POINT('Ctrl Pts',(-0.0532978506901253,-0.187990688896586,
-0.387768077418796));
#82412=CARTESIAN_POINT('Ctrl Pts',(-0.0496680349308383,-0.189019789749967,
-0.38755207888645));
#82413=CARTESIAN_POINT('Ctrl Pts',(-0.046011865622575,-0.189942741620966,
-0.387336080354103));
#82414=CARTESIAN_POINT('Ctrl Pts',(-0.0423360846919803,-0.190758527811874,
-0.387120081821756));
#82415=CARTESIAN_POINT('Ctrl Pts',(-0.0304801457906265,-0.193389781256677,
-0.386423395743169));
#82416=CARTESIAN_POINT('Ctrl Pts',(-0.0183363562956327,-0.194920746865561,
-0.385726709664581));
#82417=CARTESIAN_POINT('Ctrl Pts',(-0.00612927816464614,-0.195303845198143,
-0.385030023585993));
#82418=CARTESIAN_POINT('Ctrl Pts',(0.00605232994592505,-0.195686144197565,
-0.384334791140163));
#82419=CARTESIAN_POINT('Ctrl Pts',(0.0182961010228765,-0.194925228812739,
-0.383639558694332));
#82420=CARTESIAN_POINT('Ctrl Pts',(0.0303717752139235,-0.193025167453249,
-0.382944326248502));
#82421=CARTESIAN_POINT('Ctrl Pts',(0.0424457817816759,-0.191125368487935,
-0.3822491898127));
#82422=CARTESIAN_POINT('Ctrl Pts',(0.0543508674734123,-0.188086826848566,
-0.381554053376898));
#82423=CARTESIAN_POINT('Ctrl Pts',(0.0658628039446593,-0.183965352869901,
-0.380858916941096));
#82424=CARTESIAN_POINT('Ctrl Pts',(0.0773741432093051,-0.179844092701613,
-0.380163816567));
#82425=CARTESIAN_POINT('Ctrl Pts',(0.0884915590880914,-0.174640332115474,
-0.379468716192904));
#82426=CARTESIAN_POINT('Ctrl Pts',(0.0990094988516552,-0.168458538332564,
-0.378773615818808));
#82427=CARTESIAN_POINT('Ctrl Pts',(0.109551467682724,-0.162262621751516,
-0.378076927432783));
#82428=CARTESIAN_POINT('Ctrl Pts',(0.119490505659969,-0.155084710698945,
-0.377380239046758));
#82429=CARTESIAN_POINT('Ctrl Pts',(0.128649923243319,-0.14707262576526,
-0.376683550660733));
#82430=CARTESIAN_POINT('Ctrl Pts',(0.131489673115562,-0.144588590403863,
-0.376467552128381));
#82431=CARTESIAN_POINT('Ctrl Pts',(0.134254743571772,-0.142024648216559,
-0.376251553596028));
#82432=CARTESIAN_POINT('Ctrl Pts',(0.136940610567483,-0.139385900210189,
-0.376035555063675));
#82433=CARTESIAN_POINT('Ctrl Pts',(0.145603660841381,-0.130874828487042,
-0.375338868985085));
#82434=CARTESIAN_POINT('Ctrl Pts',(0.153500616710919,-0.121523167298244,
-0.374642182906494));
#82435=CARTESIAN_POINT('Ctrl Pts',(0.160469286891498,-0.111493353902975,
-0.373945496827903));
#82436=CARTESIAN_POINT('Ctrl Pts',(0.167423416969206,-0.101484467673832,
-0.37325026438207));
#82437=CARTESIAN_POINT('Ctrl Pts',(0.173452550890537,-0.0908009070984694,
-0.372555031936237));
#82438=CARTESIAN_POINT('Ctrl Pts',(0.178434713131651,-0.0796380132199777,
-0.371859799490404));
#82439=CARTESIAN_POINT('Ctrl Pts',(0.183416187347428,-0.0684766609118829,
-0.371164663054599));
#82440=CARTESIAN_POINT('Ctrl Pts',(0.187350579439717,-0.0568368860220045,
-0.370469526618794));
#82441=CARTESIAN_POINT('Ctrl Pts',(0.190162595785668,-0.044937146817044,
-0.369774390182989));
#82442=CARTESIAN_POINT('Ctrl Pts',(0.19297446625219,-0.0330380249367914,
-0.369079289808891));
#82443=CARTESIAN_POINT('Ctrl Pts',(0.194663901666248,-0.0208798232588043,
-0.368384189434792));
#82444=CARTESIAN_POINT('Ctrl Pts',(0.195206588133133,-0.00869183233969888,
-0.367689089060693));
#82445=CARTESIAN_POINT('Ctrl Pts',(0.195750514410289,0.00352400301121695,
-0.366992400674666));
#82446=CARTESIAN_POINT('Ctrl Pts',(0.19514248802952,0.0157688871230913,
-0.366295712288638));
#82447=CARTESIAN_POINT('Ctrl Pts',(0.193410274246544,0.0278141297882296,
-0.36559902390261));
#82448=CARTESIAN_POINT('Ctrl Pts',(0.192873225485115,0.0315485895402594,
-0.365383025370272));
#82449=CARTESIAN_POINT('Ctrl Pts',(0.192228489943372,0.0352639267049012,
-0.365167026837934));
#82450=CARTESIAN_POINT('Ctrl Pts',(0.191477882418444,0.0389535690861376,
-0.364951028305596));
#82451=CARTESIAN_POINT('Ctrl Pts',(0.189056857574245,0.050854216994026,
-0.364254342227008));
#82452=CARTESIAN_POINT('Ctrl Pts',(0.185513629958333,0.0625700616949622,
-0.363557656148419));
#82453=CARTESIAN_POINT('Ctrl Pts',(0.180896119262338,0.07387661359203,-0.362860970069831));
#82454=CARTESIAN_POINT('Ctrl Pts',(0.176288242984212,0.0851595744131221,
-0.362165737624));
#82455=CARTESIAN_POINT('Ctrl Pts',(0.170610791920237,0.0960341075904182,
-0.361470505178169));
#82456=CARTESIAN_POINT('Ctrl Pts',(0.163961182576747,0.106291535919068,
-0.360775272732339));
#82457=CARTESIAN_POINT('Ctrl Pts',(0.157312491529268,0.116547547720066,
-0.360080136296536));
#82458=CARTESIAN_POINT('Ctrl Pts',(0.149692345908798,0.12618586610788,-0.359384999860733));
#82459=CARTESIAN_POINT('Ctrl Pts',(0.141242971896812,0.135024378871952,
-0.358689863424931));
#82460=CARTESIAN_POINT('Ctrl Pts',(0.132794036214376,0.143862433119059,
-0.357994763050834));
#82461=CARTESIAN_POINT('Ctrl Pts',(0.123516581715587,0.151900150337455,
-0.357299662676738));
#82462=CARTESIAN_POINT('Ctrl Pts',(0.113589680906363,0.158992277773452,
-0.356604562302641));
#82463=CARTESIAN_POINT('Ctrl Pts',(0.103640101304996,0.166100607737013,
-0.355907873916616));
#82464=CARTESIAN_POINT('Ctrl Pts',(0.0930388627788211,0.172258580187678,
-0.35521118553059));
#82465=CARTESIAN_POINT('Ctrl Pts',(0.0819928939630575,0.177364949580132,
-0.354514497144565));
#82466=CARTESIAN_POINT('Ctrl Pts',(0.0785682451524217,0.178948108301491,
-0.354298498612215));
#82467=CARTESIAN_POINT('Ctrl Pts',(0.0751009942593462,0.180430533817913,
-0.354082500079865));
#82468=CARTESIAN_POINT('Ctrl Pts',(0.0715976418209153,0.181810169368173,
-0.353866501547515));
#82469=CARTESIAN_POINT('Ctrl Pts',(0.0602978573007469,0.186260074054694,
-0.353169815468932));
#82470=CARTESIAN_POINT('Ctrl Pts',(0.0485419779593049,0.189668120401466,
-0.352473129390349));
#82471=CARTESIAN_POINT('Ctrl Pts',(0.0365443843399179,0.191952254410352,
-0.351776443311766));
#82472=CARTESIAN_POINT('Ctrl Pts',(0.0245718236523404,0.194231622582629,
-0.351081210865941));
#82473=CARTESIAN_POINT('Ctrl Pts',(0.0123593869498785,0.19539149852171,
-0.350385978420115));
#82474=CARTESIAN_POINT('Ctrl Pts',(0.000135145916032145,0.19539995326402,
-0.34969074597429));
#82475=CARTESIAN_POINT('Ctrl Pts',(-0.012087406977776,0.19540840683875,
-0.348995609538493));
#82476=CARTESIAN_POINT('Ctrl Pts',(-0.0243208873540597,0.194265708933368,
-0.348300473102696));
#82477=CARTESIAN_POINT('Ctrl Pts',(-0.0363351032855113,0.191991979700276,
-0.347605336666898));
#82478=CARTESIAN_POINT('Ctrl Pts',(-0.0483486959535267,0.189718368421806,
-0.346910236292807));
#82479=CARTESIAN_POINT('Ctrl Pts',(-0.0601421920734194,0.186314031580679,
-0.346215135918716));
#82480=CARTESIAN_POINT('Ctrl Pts',(-0.0714962501735998,0.181850065194143,
-0.345520035544625));
#82481=CARTESIAN_POINT('Ctrl Pts',(-0.0828762475199363,0.177375900522385,
-0.344823347158605));
#82482=CARTESIAN_POINT('Ctrl Pts',(-0.0938140128905463,0.171837654257794,
-0.344126658772585));
#82483=CARTESIAN_POINT('Ctrl Pts',(-0.104111945898851,0.165353750248232,
-0.343429970386565));
#82484=CARTESIAN_POINT('Ctrl Pts',(-0.107304676624578,0.163343506101441,
-0.343213971854189));
#82485=CARTESIAN_POINT('Ctrl Pts',(-0.110436118429122,0.161242676171266,
-0.342997973321812));
#82486=CARTESIAN_POINT('Ctrl Pts',(-0.113501006385173,0.159055592638401,
-0.342781974789436));
#82487=CARTESIAN_POINT('Ctrl Pts',(-0.123318976184754,0.152049555098778,
-0.342090051594189));
#82488=CARTESIAN_POINT('Ctrl Pts',(-0.132522561191368,0.144104678485816,
-0.341398128398942));
#82489=CARTESIAN_POINT('Ctrl Pts',(-0.14092759677856,0.135353509249741,
-0.340706205203695));
#82490=CARTESIAN_POINT('Ctrl Pts',(-0.149551444308025,0.126374517023762,
-0.339996268871361));
#82491=CARTESIAN_POINT('Ctrl Pts',(-0.157333699405892,0.116547121797068,
-0.339286332539027));
#82492=CARTESIAN_POINT('Ctrl Pts',(-0.164112187289878,0.106058238637704,
-0.338576396206692));
#82493=CARTESIAN_POINT('Ctrl Pts',(-0.170703821381919,0.0958584889289168,
-0.337886029769297));
#82494=CARTESIAN_POINT('Ctrl Pts',(-0.176345925822205,0.0850341114372617,
-0.337195663331902));
#82495=CARTESIAN_POINT('Ctrl Pts',(-0.180932531280471,0.0737873913649312,
-0.336505296894507));
#82496=CARTESIAN_POINT('Ctrl Pts',(-0.18571416226884,0.0620624532370067,
-0.335785575614703));
#82497=CARTESIAN_POINT('Ctrl Pts',(-0.189347895449973,0.0498793191282996,
-0.3350658543349));
#82498=CARTESIAN_POINT('Ctrl Pts',(-0.191770197879697,0.0374880141536166,
-0.334346133055096));
#82499=CARTESIAN_POINT('Ctrl Pts',(-0.194192500309422,0.0250967091789336,
-0.333626411775292));
#82500=CARTESIAN_POINT('Ctrl Pts',(-0.195403309639771,0.0124983183140073,
-0.332906690495488));
#82501=CARTESIAN_POINT('Ctrl Pts',(-0.195399993177235,-5.16365805518149E-5,
-0.332186969215685));
#82502=CARTESIAN_POINT('',(-0.195399923138918,0.000173312737304163,-0.262186969217073));
#82503=CARTESIAN_POINT('Ctrl Pts',(-0.19539999317722,-5.16366374107664E-5,
-0.332186969212424));
#82504=CARTESIAN_POINT('Ctrl Pts',(-0.195399241274833,-0.0028969365771944,
-0.332023795485401));
#82505=CARTESIAN_POINT('Ctrl Pts',(-0.195336344993682,-0.00574133241449791,
-0.331860621758378));
#82506=CARTESIAN_POINT('Ctrl Pts',(-0.195211404501634,-0.00858298039724923,
-0.331697448031355));
#82507=CARTESIAN_POINT('Ctrl Pts',(-0.194677958933839,-0.0207156725035708,
-0.331000761952774));
#82508=CARTESIAN_POINT('Ctrl Pts',(-0.193007219482665,-0.0328410223409046,
-0.330304075874194));
#82509=CARTESIAN_POINT('Ctrl Pts',(-0.190211471622053,-0.0447298117967517,
-0.329607389795614));
#82510=CARTESIAN_POINT('Ctrl Pts',(-0.187421557078334,-0.0565937953402518,
-0.328912157349791));
#82511=CARTESIAN_POINT('Ctrl Pts',(-0.18351141975519,-0.0682213380092308,
-0.328216924903969));
#82512=CARTESIAN_POINT('Ctrl Pts',(-0.178544703623131,-0.0793911129039529,
-0.327521692458147));
#82513=CARTESIAN_POINT('Ctrl Pts',(-0.173578673383334,-0.0905593452780333,
-0.326826556022353));
#82514=CARTESIAN_POINT('Ctrl Pts',(-0.167556667527731,-0.101269118669381,
-0.32613141958656));
#82515=CARTESIAN_POINT('Ctrl Pts',(-0.160590737519437,-0.111318349893283,
-0.325436283150766));
#82516=CARTESIAN_POINT('Ctrl Pts',(-0.153625168883825,-0.121367059791584,
-0.324741182776679));
#82517=CARTESIAN_POINT('Ctrl Pts',(-0.145716294008896,-0.130754591856478,
-0.324046082402591));
#82518=CARTESIAN_POINT('Ctrl Pts',(-0.137018313282915,-0.139309518070751,
-0.323350982028503));
#82519=CARTESIAN_POINT('Ctrl Pts',(-0.128300461330176,-0.147883988692406,
-0.322654293642487));
#82520=CARTESIAN_POINT('Ctrl Pts',(-0.11879057371783,-0.155621489618999,
-0.32195760525647));
#82521=CARTESIAN_POINT('Ctrl Pts',(-0.108677235682741,-0.162389711633335,
-0.321260916870453));
#82522=CARTESIAN_POINT('Ctrl Pts',(-0.105541736057656,-0.164488104618403,
-0.321044918338061));
#82523=CARTESIAN_POINT('Ctrl Pts',(-0.102348430542222,-0.166493650443819,
-0.32082891980567));
#82524=CARTESIAN_POINT('Ctrl Pts',(-0.099103418872104,-0.168403302722543,
-0.320612921273278));
#82525=CARTESIAN_POINT('Ctrl Pts',(-0.0886368919457939,-0.174562734190601,
-0.319916235194723));
#82526=CARTESIAN_POINT('Ctrl Pts',(-0.0775572107272582,-0.179764286177824,
-0.319219549116168));
#82527=CARTESIAN_POINT('Ctrl Pts',(-0.0660633171180524,-0.183893442328321,
-0.318522863037613));
#82528=CARTESIAN_POINT('Ctrl Pts',(-0.0545934054725746,-0.18801398301078,
-0.317827630591816));
#82529=CARTESIAN_POINT('Ctrl Pts',(-0.0427117872134389,-0.19106620678016,
-0.317132398146018));
#82530=CARTESIAN_POINT('Ctrl Pts',(-0.0306387528817784,-0.192982970289736,
-0.316437165700221));
#82531=CARTESIAN_POINT('Ctrl Pts',(-0.0185673858088527,-0.194899469098607,
-0.315742029264451));
#82532=CARTESIAN_POINT('Ctrl Pts',(-0.00630551086825178,-0.195680637166155,
-0.315046892828682));
#82533=CARTESIAN_POINT('Ctrl Pts',(0.00591636139793886,-0.19531041105842,
-0.314351756392912));
#82534=CARTESIAN_POINT('Ctrl Pts',(0.0181375996280714,-0.194940204156965,
-0.313656656018849));
#82535=CARTESIAN_POINT('Ctrl Pts',(0.0303179655481477,-0.193418775190653,
-0.312961555644785));
#82536=CARTESIAN_POINT('Ctrl Pts',(0.0422297078280292,-0.190782105494093,
-0.312266455270722));
#82537=CARTESIAN_POINT('Ctrl Pts',(0.0541686634278107,-0.18813941211651,
-0.311569766884729));
#82538=CARTESIAN_POINT('Ctrl Pts',(0.0658369307298061,-0.184376644365591,
-0.310873078498736));
#82539=CARTESIAN_POINT('Ctrl Pts',(0.0770208442306797,-0.179579925253335,
-0.310176390112744));
#82540=CARTESIAN_POINT('Ctrl Pts',(0.0804882608728209,-0.178092769288098,
-0.309960391580227));
#82541=CARTESIAN_POINT('Ctrl Pts',(0.0839092820691905,-0.176506570005805,
-0.309744393047711));
#82542=CARTESIAN_POINT('Ctrl Pts',(0.0872780311207803,-0.174824784523477,
-0.309528394515195));
#82543=CARTESIAN_POINT('Ctrl Pts',(0.0981436631207327,-0.169400319277181,
-0.308831708436502));
#82544=CARTESIAN_POINT('Ctrl Pts',(0.108539786586155,-0.16293997130447,
-0.30813502235781));
#82545=CARTESIAN_POINT('Ctrl Pts',(0.118262019687355,-0.15554823913972,
-0.307438336279117));
#82546=CARTESIAN_POINT('Ctrl Pts',(0.127963967387505,-0.148171929795002,
-0.306743103833182));
#82547=CARTESIAN_POINT('Ctrl Pts',(0.136994081315752,-0.139868559100433,
-0.306047871387248));
#82548=CARTESIAN_POINT('Ctrl Pts',(0.145176087370112,-0.130786328245369,
-0.305352638941313));
#82549=CARTESIAN_POINT('Ctrl Pts',(0.153356963507925,-0.121705351625864,
-0.304657502505408));
#82550=CARTESIAN_POINT('Ctrl Pts',(0.160689345840531,-0.111846347112711,
-0.303962366069503));
#82551=CARTESIAN_POINT('Ctrl Pts',(0.167034237172029,-0.101393903230709,
-0.303267229633599));
#82552=CARTESIAN_POINT('Ctrl Pts',(0.173378799348559,-0.0909420015918515,
-0.302572129259401));
#82553=CARTESIAN_POINT('Ctrl Pts',(0.178735541318582,-0.0798974836952926,
-0.301877028885203));
#82554=CARTESIAN_POINT('Ctrl Pts',(0.183010619864622,-0.0684709647716965,
-0.301181928511005));
#82555=CARTESIAN_POINT('Ctrl Pts',(0.187295465166611,-0.057018341059503,
-0.300485240124881));
#82556=CARTESIAN_POINT('Ctrl Pts',(0.190493468620826,-0.0451828158518389,
-0.299788551738757));
#82557=CARTESIAN_POINT('Ctrl Pts',(0.192560512709603,-0.0331904947991887,
-0.299091863352634));
#82558=CARTESIAN_POINT('Ctrl Pts',(0.19320137094309,-0.029472442665253,
-0.298875864820794));
#82559=CARTESIAN_POINT('Ctrl Pts',(0.193733894081805,-0.0257393697745842,
-0.298659866288955));
#82560=CARTESIAN_POINT('Ctrl Pts',(0.194157781558028,-0.0219980876547268,
-0.298443867757116));
#82561=CARTESIAN_POINT('Ctrl Pts',(0.195524996885923,-0.00993087985273009,
-0.29774718167862));
#82562=CARTESIAN_POINT('Ctrl Pts',(0.195767716935638,0.0023066266717942,
-0.297050495600125));
#82563=CARTESIAN_POINT('Ctrl Pts',(0.194862291688264,0.014486106378107,
-0.296353809521629));
#82564=CARTESIAN_POINT('Ctrl Pts',(0.1939587556071,0.0266401736480271,-0.29565857707589));
#82565=CARTESIAN_POINT('Ctrl Pts',(0.191911819837225,0.0387355850229386,
-0.29496334463015));
#82566=CARTESIAN_POINT('Ctrl Pts',(0.188749795080135,0.050543791480331,
-0.29426811218441));
#82567=CARTESIAN_POINT('Ctrl Pts',(0.185588206991497,0.0623503672511719,
-0.293572975748696));
#82568=CARTESIAN_POINT('Ctrl Pts',(0.181312017803303,0.0738689612024969,
-0.292877839312982));
#82569=CARTESIAN_POINT('Ctrl Pts',(0.176000356436181,0.0848824748363132,
-0.292182702877267));
#82570=CARTESIAN_POINT('Ctrl Pts',(0.170688970622967,0.0958954171203168,
-0.291487602503257));
#82571=CARTESIAN_POINT('Ctrl Pts',(0.164342623729396,0.106402554748214,
-0.290792502129247));
#82572=CARTESIAN_POINT('Ctrl Pts',(0.157086862589102,0.116210488347277,
-0.290097401755237));
#82573=CARTESIAN_POINT('Ctrl Pts',(0.149814525087026,0.126040828948517,
-0.289400713369294));
#82574=CARTESIAN_POINT('Ctrl Pts',(0.141629198182814,0.135168112576547,
-0.288704024983351));
#82575=CARTESIAN_POINT('Ctrl Pts',(0.132696499062621,0.143432210944836,
-0.288007336597408));
#82576=CARTESIAN_POINT('Ctrl Pts',(0.129927040086767,0.145994379567717,
-0.287791338064617));
#82577=CARTESIAN_POINT('Ctrl Pts',(0.127085988979078,0.148473863955332,
-0.287575339531826));
#82578=CARTESIAN_POINT('Ctrl Pts',(0.124178895090764,0.150866702800973,
-0.287359340999035));
#82579=CARTESIAN_POINT('Ctrl Pts',(0.114802295099811,0.158584614076071,
-0.286662654920628));
#82580=CARTESIAN_POINT('Ctrl Pts',(0.104670517652445,0.165452114689179,
-0.285965968842221));
#82581=CARTESIAN_POINT('Ctrl Pts',(0.0939621873808109,0.17132503419703,
-0.285269282763813));
#82582=CARTESIAN_POINT('Ctrl Pts',(0.0832761999981347,0.177185699881446,
-0.284574050318166));
#82583=CARTESIAN_POINT('Ctrl Pts',(0.0720167716332992,0.182055422176276,
-0.283878817872519));
#82584=CARTESIAN_POINT('Ctrl Pts',(0.0603910095274079,0.185833489899589,
-0.283183585426872));
#82585=CARTESIAN_POINT('Ctrl Pts',(0.0487668529129842,0.189611035880289,
-0.282488448991254));
#82586=CARTESIAN_POINT('Ctrl Pts',(0.0367772798465013,0.192296913433613,
-0.281793312555636));
#82587=CARTESIAN_POINT('Ctrl Pts',(0.0246474667033551,0.193839269460827,
-0.281098176120018));
#82588=CARTESIAN_POINT('Ctrl Pts',(0.0125182828205135,0.195381545474984,
-0.280403075746107));
#82589=CARTESIAN_POINT('Ctrl Pts',(0.000249744703043385,0.195780334198186,
-0.279707975372196));
#82590=CARTESIAN_POINT('Ctrl Pts',(-0.0119275715780176,0.195035619916597,
-0.279012874998285));
#82591=CARTESIAN_POINT('Ctrl Pts',(-0.0241327079038838,0.194289204276169,
-0.278316186612442));
#82592=CARTESIAN_POINT('Ctrl Pts',(-0.0362453376655141,0.192394188927021,
-0.2776194982266));
#82593=CARTESIAN_POINT('Ctrl Pts',(-0.0480409699354846,0.189402284061354,
-0.276922809840757));
#82594=CARTESIAN_POINT('Ctrl Pts',(-0.0516980414771468,0.188474685617356,
-0.27670681130749));
#82595=CARTESIAN_POINT('Ctrl Pts',(-0.0553247487980788,0.187442015148976,
-0.276490812774223));
#82596=CARTESIAN_POINT('Ctrl Pts',(-0.058914747541078,0.18630676993113,
-0.276274814240956));
#82597=CARTESIAN_POINT('Ctrl Pts',(-0.0704940027847687,0.182645126826868,
-0.275578128161653));
#82598=CARTESIAN_POINT('Ctrl Pts',(-0.0817712252968662,0.177887004119356,
-0.27488144208235));
#82599=CARTESIAN_POINT('Ctrl Pts',(-0.0925282252597426,0.172103711552896,
-0.274184756003048));
#82600=CARTESIAN_POINT('Ctrl Pts',(-0.103262780784625,0.166332485803565,
-0.273489523556501));
#82601=CARTESIAN_POINT('Ctrl Pts',(-0.113478470266465,0.159540681102335,
-0.272794291109955));
#82602=CARTESIAN_POINT('Ctrl Pts',(-0.122978044244706,0.151847162086577,
-0.272099058663409));
#82603=CARTESIAN_POINT('Ctrl Pts',(-0.132476306353136,0.144154705528499,
-0.271403922226901));
#82604=CARTESIAN_POINT('Ctrl Pts',(-0.141257941827696,0.135561296467514,
-0.270708785790392));
#82605=CARTESIAN_POINT('Ctrl Pts',(-0.149156840362037,0.126227560275931,
-0.270013649353884));
#82606=CARTESIAN_POINT('Ctrl Pts',(-0.157055329123879,0.116894308292164,
-0.269318548979086));
#82607=CARTESIAN_POINT('Ctrl Pts',(-0.164070627274964,0.106821490801852,
-0.268623448604289));
#82608=CARTESIAN_POINT('Ctrl Pts',(-0.170077161622158,0.096202490064189,
-0.267928348229492));
#82609=CARTESIAN_POINT('Ctrl Pts',(-0.176097418373224,0.08555922937754,
-0.267231659842785));
#82610=CARTESIAN_POINT('Ctrl Pts',(-0.181103936970048,0.0743680875759282,
-0.266534971456079));
#82611=CARTESIAN_POINT('Ctrl Pts',(-0.185017841892093,0.0628455104330651,
-0.265838283069372));
#82612=CARTESIAN_POINT('Ctrl Pts',(-0.186231293589125,0.0592730959092883,
-0.26562228454054));
#82613=CARTESIAN_POINT('Ctrl Pts',(-0.187340083534537,0.0556689318504821,
-0.265406286011707));
#82614=CARTESIAN_POINT('Ctrl Pts',(-0.188342851450472,0.0520396993410366,
-0.265190287482875));
#82615=CARTESIAN_POINT('Ctrl Pts',(-0.192396085389066,0.0373701749729622,
-0.264317211516006));
#82616=CARTESIAN_POINT('Ctrl Pts',(-0.194736418589095,0.0222079032156958,
-0.263444135549137));
#82617=CARTESIAN_POINT('Ctrl Pts',(-0.195277763789369,0.00691049704604845,
-0.262571059582269));
#82618=CARTESIAN_POINT('Ctrl Pts',(-0.195357148052045,0.00466724577307081,
-0.262443029460537));
#82619=CARTESIAN_POINT('Ctrl Pts',(-0.195397929407478,0.00242112773447588,
-0.262314999338805));
#82620=CARTESIAN_POINT('Ctrl Pts',(-0.195399923138918,0.000173312737304944,
-0.262186969217073));
#82621=CARTESIAN_POINT('',(-0.195399980573749,-8.71308121574774E-5,-0.19218696920821));
#82622=CARTESIAN_POINT('Ctrl Pts',(-0.19539992313899,0.000173312655682386,
-0.262186969212424));
#82623=CARTESIAN_POINT('Ctrl Pts',(-0.195410653058069,-0.0119240460448848,
-0.2614979328331));
#82624=CARTESIAN_POINT('Ctrl Pts',(-0.194293610829215,-0.0240463379113419,
-0.260808896453775));
#82625=CARTESIAN_POINT('Ctrl Pts',(-0.192061369462662,-0.0359665172087442,
-0.260119860074451));
#82626=CARTESIAN_POINT('Ctrl Pts',(-0.189830801962487,-0.0478777580518912,
-0.259431340375287));
#82627=CARTESIAN_POINT('Ctrl Pts',(-0.186486850453256,-0.059586306886096,
-0.258742820676124));
#82628=CARTESIAN_POINT('Ctrl Pts',(-0.182093486969189,-0.0708739867892439,
-0.25805430097696));
#82629=CARTESIAN_POINT('Ctrl Pts',(-0.177689492763121,-0.0821889797493508,
-0.257364115250949));
#82630=CARTESIAN_POINT('Ctrl Pts',(-0.172231359849049,-0.093080239188824,
-0.256673929524939));
#82631=CARTESIAN_POINT('Ctrl Pts',(-0.165831481543612,-0.103349309281923,
-0.255983743798928));
#82632=CARTESIAN_POINT('Ctrl Pts',(-0.160026829896396,-0.112663294921408,
-0.255357749440884));
#82633=CARTESIAN_POINT('Ctrl Pts',(-0.153448374712411,-0.121465349160077,
-0.254731755082839));
#82634=CARTESIAN_POINT('Ctrl Pts',(-0.14620914768459,-0.129630417469612,
-0.254105760724795));
#82635=CARTESIAN_POINT('Ctrl Pts',(-0.138152415832565,-0.138717543162808,
-0.253409074647088));
#82636=CARTESIAN_POINT('Ctrl Pts',(-0.129217002484211,-0.147082581529689,
-0.252712388569381));
#82637=CARTESIAN_POINT('Ctrl Pts',(-0.119556834612108,-0.154555243513551,
-0.252015702491674));
#82638=CARTESIAN_POINT('Ctrl Pts',(-0.109916822642486,-0.162012313817412,
-0.251320470046744));
#82639=CARTESIAN_POINT('Ctrl Pts',(-0.0995556977450317,-0.168580115038724,
-0.250625237601813));
#82640=CARTESIAN_POINT('Ctrl Pts',(-0.0886623049952405,-0.174126837888164,
-0.249930005156882));
#82641=CARTESIAN_POINT('Ctrl Pts',(-0.0777704165985586,-0.179672794747617,
-0.249234868721993));
#82642=CARTESIAN_POINT('Ctrl Pts',(-0.0663471642281377,-0.184197516344812,
-0.248539732287103));
#82643=CARTESIAN_POINT('Ctrl Pts',(-0.0546068681200209,-0.18761463150331,
-0.247844595852214));
#82644=CARTESIAN_POINT('Ctrl Pts',(-0.0428671810652999,-0.191031569391526,
-0.247149495479039));
#82645=CARTESIAN_POINT('Ctrl Pts',(-0.0308113305979205,-0.193340796361407,
-0.246454395105865));
#82646=CARTESIAN_POINT('Ctrl Pts',(-0.0186670631411277,-0.194506300035976,
-0.24575929473269));
#82647=CARTESIAN_POINT('Ctrl Pts',(-0.00649505114212026,-0.19567446639613,
-0.245062606347582));
#82648=CARTESIAN_POINT('Ctrl Pts',(0.00576490455346149,-0.195693674682041,
-0.244365917962473));
#82649=CARTESIAN_POINT('Ctrl Pts',(0.0178829927575548,-0.194579954183449,
-0.243669229577365));
#82650=CARTESIAN_POINT('Ctrl Pts',(0.0216400373385423,-0.194234660644279,
-0.243453231040481));
#82651=CARTESIAN_POINT('Ctrl Pts',(0.0253834935417705,-0.193780843038646,
-0.243237232503598));
#82652=CARTESIAN_POINT('Ctrl Pts',(0.0291067049334456,-0.193219977559044,
-0.243021233966715));
#82653=CARTESIAN_POINT('Ctrl Pts',(0.041115626843582,-0.191410950609435,
-0.242324547883315));
#82654=CARTESIAN_POINT('Ctrl Pts',(0.0529973985326241,-0.188471736001752,
-0.241627861799915));
#82655=CARTESIAN_POINT('Ctrl Pts',(0.0645253728350063,-0.184438705971668,
-0.240931175716515));
#82656=CARTESIAN_POINT('Ctrl Pts',(0.0760292940647887,-0.180414090842725,
-0.240235943265861));
#82657=CARTESIAN_POINT('Ctrl Pts',(0.0871800410625355,-0.175300406681039,
-0.239540710815207));
#82658=CARTESIAN_POINT('Ctrl Pts',(0.0977642261316131,-0.169184266670654,
-0.238845478364553));
#82659=CARTESIAN_POINT('Ctrl Pts',(0.108346949547824,-0.16306897128586,
-0.238150341923984));
#82660=CARTESIAN_POINT('Ctrl Pts',(0.118362487240594,-0.155951892727064,
-0.237455205483415));
#82661=CARTESIAN_POINT('Ctrl Pts',(0.127621689294173,-0.147965754219352,
-0.236760069042845));
#82662=CARTESIAN_POINT('Ctrl Pts',(0.13688041100625,-0.139980030010166,
-0.23606496866401));
#82663=CARTESIAN_POINT('Ctrl Pts',(0.145382230068811,-0.131125927311856,
-0.235369868285175));
#82664=CARTESIAN_POINT('Ctrl Pts',(0.152972922727515,-0.121574853124327,
-0.23467476790634));
#82665=CARTESIAN_POINT('Ctrl Pts',(0.160580956924063,-0.112001958752276,
-0.233978079515703));
#82666=CARTESIAN_POINT('Ctrl Pts',(0.167273216425432,-0.101729639260994,
-0.233281391125066));
#82667=CARTESIAN_POINT('Ctrl Pts',(0.172938001961387,-0.0909593726759544,
-0.232584702734429));
#82668=CARTESIAN_POINT('Ctrl Pts',(0.174694289627061,-0.0876202018919485,
-0.232368704225831));
#82669=CARTESIAN_POINT('Ctrl Pts',(0.176352155506728,-0.0842333313931768,
-0.232152705717234));
#82670=CARTESIAN_POINT('Ctrl Pts',(0.177909212970956,-0.0808051479799098,
-0.231936707208636));
#82671=CARTESIAN_POINT('Ctrl Pts',(0.182931378426524,-0.0697478140606376,
-0.231240021136826));
#82672=CARTESIAN_POINT('Ctrl Pts',(0.186936383309858,-0.0581816819394014,
-0.230543335065016));
#82673=CARTESIAN_POINT('Ctrl Pts',(0.189831313534887,-0.0463166536099004,
-0.229846648993206));
#82674=CARTESIAN_POINT('Ctrl Pts',(0.192720203499534,-0.0344763816147428,
-0.22915141655411));
#82675=CARTESIAN_POINT('Ctrl Pts',(0.194503339078234,-0.0223392753961914,
-0.228456184115014));
#82676=CARTESIAN_POINT('Ctrl Pts',(0.195137165153437,-0.0101314745165962,
-0.227760951675918));
#82677=CARTESIAN_POINT('Ctrl Pts',(0.19577090369884,0.00207464049617775,
-0.227065815246685));
#82678=CARTESIAN_POINT('Ctrl Pts',(0.195255557244779,0.0143505606708363,
-0.226370678817453));
#82679=CARTESIAN_POINT('Ctrl Pts',(0.193599443161949,0.0264653661864563,
-0.225675542388221));
#82680=CARTESIAN_POINT('Ctrl Pts',(0.191943414993408,0.0385795432218813,
-0.224980442020606));
#82681=CARTESIAN_POINT('Ctrl Pts',(0.189146881990735,0.0505317589418535,
-0.224285341652991));
#82682=CARTESIAN_POINT('Ctrl Pts',(0.185269625737726,0.0620993218884295,
-0.223590241285376));
#82683=CARTESIAN_POINT('Ctrl Pts',(0.181383511583866,0.0736933118542674,
-0.222893552905585));
#82684=CARTESIAN_POINT('Ctrl Pts',(0.176412085024892,0.0849000865122645,
-0.222196864525794));
#82685=CARTESIAN_POINT('Ctrl Pts',(0.170463505756305,0.0955162457662059,
-0.221500176146003));
#82686=CARTESIAN_POINT('Ctrl Pts',(0.168619231294489,0.0988076386367702,
-0.221284177580853));
#82687=CARTESIAN_POINT('Ctrl Pts',(0.166681354149909,0.102042457122414,
-0.221068179015704));
#82688=CARTESIAN_POINT('Ctrl Pts',(0.164653931482825,0.105215221556813,
-0.220852180450555));
#82689=CARTESIAN_POINT('Ctrl Pts',(0.15811464202164,0.115448719172049,-0.22015549437535));
#82690=CARTESIAN_POINT('Ctrl Pts',(0.150594714827337,0.125106160460965,
-0.219458808300145));
#82691=CARTESIAN_POINT('Ctrl Pts',(0.142219604478747,0.133995313731148,
-0.218762122224941));
#82692=CARTESIAN_POINT('Ctrl Pts',(0.133861968766583,0.14286591981627,-0.218066889782627));
#82693=CARTESIAN_POINT('Ctrl Pts',(0.124653231947698,0.150970738568163,
-0.217371657340313));
#82694=CARTESIAN_POINT('Ctrl Pts',(0.114759345905742,0.158150094932903,
-0.216676424898));
#82695=CARTESIAN_POINT('Ctrl Pts',(0.104866826189024,0.16532845984335,-0.215981288465851));
#82696=CARTESIAN_POINT('Ctrl Pts',(0.0942900255519612,0.171581066289418,
-0.215286152033703));
#82697=CARTESIAN_POINT('Ctrl Pts',(0.0832271523410599,0.176789143086328,
-0.214591015601554));
#82698=CARTESIAN_POINT('Ctrl Pts',(0.0721648530419438,0.181996949702373,
-0.213895915231194));
#82699=CARTESIAN_POINT('Ctrl Pts',(0.0606173343890308,0.186159986037156,
-0.213200814860834));
#82700=CARTESIAN_POINT('Ctrl Pts',(0.0488039281591277,0.18920712617721,
-0.212505714490473));
#82701=CARTESIAN_POINT('Ctrl Pts',(0.0369635332665546,0.19226122775038,
-0.211809026108234));
#82702=CARTESIAN_POINT('Ctrl Pts',(0.0248569010483798,0.194194188646917,
-0.211112337725996));
#82703=CARTESIAN_POINT('Ctrl Pts',(0.0127135273208923,0.194985964169375,
-0.210415649343757));
#82704=CARTESIAN_POINT('Ctrl Pts',(0.00894864306373339,0.195231443166119,
-0.21019965079333));
#82705=CARTESIAN_POINT('Ctrl Pts',(0.00518023811354474,0.195367607366277,
-0.209983652242902));
#82706=CARTESIAN_POINT('Ctrl Pts',(0.00141511774680491,0.195394875679386,
-0.209767653692475));
#82707=CARTESIAN_POINT('Ctrl Pts',(-0.0107289779310962,0.195482827450142,
-0.20907096758229));
#82708=CARTESIAN_POINT('Ctrl Pts',(-0.0229239239752086,0.194434598883651,
-0.208374281472106));
#82709=CARTESIAN_POINT('Ctrl Pts',(-0.0349401738991443,0.192250732762966,
-0.207677595361922));
#82710=CARTESIAN_POINT('Ctrl Pts',(-0.0469313519681011,0.190071423269767,
-0.20698236288438));
#82711=CARTESIAN_POINT('Ctrl Pts',(-0.0587437084385229,0.186761261699367,
-0.206287130406837));
#82712=CARTESIAN_POINT('Ctrl Pts',(-0.0701529502464144,0.182372485785888,
-0.205591897929295));
#82713=CARTESIAN_POINT('Ctrl Pts',(-0.0815606164587637,0.177984315954381,
-0.204896761462093));
#82714=CARTESIAN_POINT('Ctrl Pts',(-0.0925644468468266,0.172518098822333,
-0.204201624994891));
#82715=CARTESIAN_POINT('Ctrl Pts',(-0.102956890375255,0.166075400719847,
-0.203506488527689));
#82716=CARTESIAN_POINT('Ctrl Pts',(-0.113348794770967,0.159633036847642,
-0.202811388122344));
#82717=CARTESIAN_POINT('Ctrl Pts',(-0.123128645861872,0.152214776589438,
-0.202116287716999));
#82718=CARTESIAN_POINT('Ctrl Pts',(-0.132117351332421,0.14396584830058,
-0.201421187311655));
#82719=CARTESIAN_POINT('Ctrl Pts',(-0.141126592202309,0.135698074691104,
-0.200724498895172));
#82720=CARTESIAN_POINT('Ctrl Pts',(-0.149340479210109,0.12659648382991,
-0.200027810478689));
#82721=CARTESIAN_POINT('Ctrl Pts',(-0.156617228512917,0.11684264518117,
-0.199331122062206));
#82722=CARTESIAN_POINT('Ctrl Pts',(-0.158873281569522,0.113818605657282,
-0.199115123686269));
#82723=CARTESIAN_POINT('Ctrl Pts',(-0.161039566480852,0.110732086044716,
-0.198899125310332));
#82724=CARTESIAN_POINT('Ctrl Pts',(-0.16311272879862,0.107589022227493,
-0.198683126934395));
#82725=CARTESIAN_POINT('Ctrl Pts',(-0.169922682695037,0.0972646402409293,
-0.19797361231066));
#82726=CARTESIAN_POINT('Ctrl Pts',(-0.175770941149539,0.0862577317658504,
-0.197264097686925));
#82727=CARTESIAN_POINT('Ctrl Pts',(-0.180529547933672,0.0747679230878049,
-0.196554583063191));
#82728=CARTESIAN_POINT('Ctrl Pts',(-0.185411701687211,0.0629798062902586,
-0.195826647421396));
#82729=CARTESIAN_POINT('Ctrl Pts',(-0.189146194866463,0.0506840503841172,
-0.195098711779602));
#82730=CARTESIAN_POINT('Ctrl Pts',(-0.191644763603409,0.038124068295415,
-0.194370776137807));
#82731=CARTESIAN_POINT('Ctrl Pts',(-0.194143332340355,0.0255640862067136,
-0.193642840496012));
#82732=CARTESIAN_POINT('Ctrl Pts',(-0.195405700671203,0.012740798323454,
-0.192914904854218));
#82733=CARTESIAN_POINT('Ctrl Pts',(-0.195399980573782,-8.71307379076436E-5,
-0.192186969212423));
#82734=CARTESIAN_POINT('',(-0.195399970103672,-0.000108090166289862,-0.122186969217338));
#82735=CARTESIAN_POINT('Ctrl Pts',(-0.195399980573749,-8.71308121576554E-5,
-0.19218696920821));
#82736=CARTESIAN_POINT('Ctrl Pts',(-0.195393971356559,-0.0135634303337909,
-0.191422241036227));
#82737=CARTESIAN_POINT('Ctrl Pts',(-0.193989563708496,-0.0269934619489129,
-0.190657512864245));
#82738=CARTESIAN_POINT('Ctrl Pts',(-0.191240294421705,-0.0401037378494752,
-0.189892784692262));
#82739=CARTESIAN_POINT('Ctrl Pts',(-0.188491025134915,-0.0532140137500375,
-0.18912805652028));
#82740=CARTESIAN_POINT('Ctrl Pts',(-0.184397210802687,-0.066004022077199,
-0.188363328348297));
#82741=CARTESIAN_POINT('Ctrl Pts',(-0.179060927217783,-0.0782198462278453,
-0.187598600176314));
#82742=CARTESIAN_POINT('Ctrl Pts',(-0.174199442314772,-0.089348760900636,
-0.186901914101849));
#82743=CARTESIAN_POINT('Ctrl Pts',(-0.168279411507396,-0.100061776817748,
-0.186205228027384));
#82744=CARTESIAN_POINT('Ctrl Pts',(-0.161394740466552,-0.110149433724075,
-0.185508541952918));
#82745=CARTESIAN_POINT('Ctrl Pts',(-0.15452443427393,-0.120216042760501,
-0.184813309512136));
#82746=CARTESIAN_POINT('Ctrl Pts',(-0.146693910245396,-0.129659125533717,
-0.184118077071353));
#82747=CARTESIAN_POINT('Ctrl Pts',(-0.138042157449026,-0.138295056913898,
-0.18342284463057));
#82748=CARTESIAN_POINT('Ctrl Pts',(-0.12939159945556,-0.146929795676105,
-0.182727708201054));
#82749=CARTESIAN_POINT('Ctrl Pts',(-0.119920624130205,-0.154756955044027,
-0.182032571771537));
#82750=CARTESIAN_POINT('Ctrl Pts',(-0.109806467286001,-0.161628276431348,
-0.18133743534202));
#82751=CARTESIAN_POINT('Ctrl Pts',(-0.0996928351460712,-0.168499241346869,
-0.180642334974932));
#82752=CARTESIAN_POINT('Ctrl Pts',(-0.088936826680016,-0.174413997399687,
-0.179947234607844));
#82753=CARTESIAN_POINT('Ctrl Pts',(-0.0777439803686978,-0.179268049346311,
-0.179252134240755));
#82754=CARTESIAN_POINT('Ctrl Pts',(-0.0665255631267537,-0.184133190753304,
-0.178555445862649));
#82755=CARTESIAN_POINT('Ctrl Pts',(-0.0548691438273311,-0.187932502481423,
-0.177858757484542));
#82756=CARTESIAN_POINT('Ctrl Pts',(-0.0429982750156473,-0.190610357393502,
-0.177162069106436));
#82757=CARTESIAN_POINT('Ctrl Pts',(-0.0393178768888787,-0.191440589144735,
-0.176946070543702));
#82758=CARTESIAN_POINT('Ctrl Pts',(-0.035616935330501,-0.192163396083465,
-0.176730071980969));
#82759=CARTESIAN_POINT('Ctrl Pts',(-0.0319022375746728,-0.192778129562793,
-0.176514073418235));
#82760=CARTESIAN_POINT('Ctrl Pts',(-0.0199207737687746,-0.194760903779428,
-0.17581738713805));
#82761=CARTESIAN_POINT('Ctrl Pts',(-0.007711706010355,-0.19562936689701,
-0.175120700857864));
#82762=CARTESIAN_POINT('Ctrl Pts',(0.0044981489421037,-0.195348218973439,
-0.174424014577679));
#82763=CARTESIAN_POINT('Ctrl Pts',(0.0166825281058876,-0.195067657663314,
-0.173728781929213));
#82764=CARTESIAN_POINT('Ctrl Pts',(0.0288668234303841,-0.193642192521187,
-0.173033549280747));
#82765=CARTESIAN_POINT('Ctrl Pts',(0.040821336716632,-0.191088404851439,
-0.172338316632281));
#82766=CARTESIAN_POINT('Ctrl Pts',(0.0527741990849647,-0.188534969859689,
-0.171643179995422));
#82767=CARTESIAN_POINT('Ctrl Pts',(0.0644964785721529,-0.184853659848699,
-0.170948043358563));
#82768=CARTESIAN_POINT('Ctrl Pts',(0.0757673127012417,-0.180112393593645,
-0.170252906721704));
#82769=CARTESIAN_POINT('Ctrl Pts',(0.0870375621198938,-0.175371373306888,
-0.169557806147274));
#82770=CARTESIAN_POINT('Ctrl Pts',(0.0978556166444629,-0.169570870150772,
-0.168862705572843));
#82771=CARTESIAN_POINT('Ctrl Pts',(0.10802190718798,-0.162826372456895,
-0.168167604998413));
#82772=CARTESIAN_POINT('Ctrl Pts',(0.118211423352824,-0.156066466473356,
-0.167470916416768));
#82773=CARTESIAN_POINT('Ctrl Pts',(0.127745510547746,-0.148358798376342,
-0.166774227835123));
#82774=CARTESIAN_POINT('Ctrl Pts',(0.136455777234141,-0.139860576501838,
-0.166077539253478));
#82775=CARTESIAN_POINT('Ctrl Pts',(0.139156260849229,-0.137225834104648,
-0.16586154172237));
#82776=CARTESIAN_POINT('Ctrl Pts',(0.141777831823451,-0.134515363975046,
-0.165645544191262));
#82777=CARTESIAN_POINT('Ctrl Pts',(0.144316250195574,-0.131734505462649,
-0.165429546660155));
#82778=CARTESIAN_POINT('Ctrl Pts',(0.152503749882229,-0.122765031222731,
-0.164732860984663));
#82779=CARTESIAN_POINT('Ctrl Pts',(0.159880587869742,-0.112997862757875,
-0.164036175309172));
#82780=CARTESIAN_POINT('Ctrl Pts',(0.166293644268259,-0.10260401491161,
-0.16333948963368));
#82781=CARTESIAN_POINT('Ctrl Pts',(0.172693319853186,-0.092231853782545,
-0.162644257589745));
#82782=CARTESIAN_POINT('Ctrl Pts',(0.178132687595168,-0.0812363071400706,
-0.16194902554581));
#82783=CARTESIAN_POINT('Ctrl Pts',(0.182500572794291,-0.0698190584994946,
-0.161253793501875));
#82784=CARTESIAN_POINT('Ctrl Pts',(0.186867854846755,-0.0584033864285969,
-0.160558657460208));
#82785=CARTESIAN_POINT('Ctrl Pts',(0.190163593566233,-0.0465669277301283,
-0.15986352141854));
#82786=CARTESIAN_POINT('Ctrl Pts',(0.192324483949466,-0.034531910945844,
-0.159168385376873));
#82787=CARTESIAN_POINT('Ctrl Pts',(0.194485262244566,-0.0224975184331854,
-0.158473285392796));
#82788=CARTESIAN_POINT('Ctrl Pts',(0.19551118106135,-0.010265454266999,
-0.157778185408719));
#82789=CARTESIAN_POINT('Ctrl Pts',(0.195390428658573,0.00193400843301484,
-0.157083085424642));
#82790=CARTESIAN_POINT('Ctrl Pts',(0.195269400384929,0.014161342018218,
-0.156386397415558));
#82791=CARTESIAN_POINT('Ctrl Pts',(0.193996545096175,0.0263550518336399,
-0.155689709406473));
#82792=CARTESIAN_POINT('Ctrl Pts',(0.191612020533415,0.0382882956933619,
-0.154993021397388));
#82793=CARTESIAN_POINT('Ctrl Pts',(0.190872724769203,0.0419880674535577,
-0.15477702089895));
#82794=CARTESIAN_POINT('Ctrl Pts',(0.190026939225289,0.0456628897167423,
-0.154561020400512));
#82795=CARTESIAN_POINT('Ctrl Pts',(0.189076833400025,0.0493062984964319,
-0.154345019902075));
#82796=CARTESIAN_POINT('Ctrl Pts',(0.186012370094469,0.0610577184073582,
-0.153648333718449));
#82797=CARTESIAN_POINT('Ctrl Pts',(0.181837411076989,0.0725635961155488,
-0.152951647534823));
#82798=CARTESIAN_POINT('Ctrl Pts',(0.176612010267933,0.0836023793269029,
-0.152254961351197));
#82799=CARTESIAN_POINT('Ctrl Pts',(0.171397512282338,0.0946181300649645,
-0.151559728806582));
#82800=CARTESIAN_POINT('Ctrl Pts',(0.165137226816864,0.105167906177253,
-0.150864496261968));
#82801=CARTESIAN_POINT('Ctrl Pts',(0.157939771708267,0.1150486354232,-0.150169263717353));
#82802=CARTESIAN_POINT('Ctrl Pts',(0.150743310659152,0.124928000015606,
-0.149474127193137));
#82803=CARTESIAN_POINT('Ctrl Pts',(0.142610414659424,0.134137768326967,
-0.148778990668921));
#82804=CARTESIAN_POINT('Ctrl Pts',(0.133693000655849,0.142503830038477,
-0.148083854144704));
#82805=CARTESIAN_POINT('Ctrl Pts',(0.124776049338251,0.150869457671292,
-0.14738875368811));
#82806=CARTESIAN_POINT('Ctrl Pts',(0.115075317446932,0.158390886677845,
-0.146693653231516));
#82807=CARTESIAN_POINT('Ctrl Pts',(0.104777509781274,0.164932814940008,
-0.145998552774923));
#82808=CARTESIAN_POINT('Ctrl Pts',(0.0944561761087307,0.171489688659917,
-0.14530186431643));
#82809=CARTESIAN_POINT('Ctrl Pts',(0.0835358165499775,0.177062180688005,
-0.144605175857937));
#82810=CARTESIAN_POINT('Ctrl Pts',(0.0722285582496733,0.181560445508303,
-0.143908487399444));
#82811=CARTESIAN_POINT('Ctrl Pts',(0.0687229078956497,0.182955066842756,
-0.143692489314294));
#82812=CARTESIAN_POINT('Ctrl Pts',(0.0651801953146029,0.184246788178321,
-0.143476491229144));
#82813=CARTESIAN_POINT('Ctrl Pts',(0.0616070232095414,0.18543390922714,
-0.143260493143995));
#82814=CARTESIAN_POINT('Ctrl Pts',(0.0500819964771528,0.189262888470214,
-0.142563805821834));
#82815=CARTESIAN_POINT('Ctrl Pts',(0.0381581932723761,0.192026748952457,
-0.141867118499673));
#82816=CARTESIAN_POINT('Ctrl Pts',(0.0260541390244445,0.193655213820065,
-0.141170431177512));
#82817=CARTESIAN_POINT('Ctrl Pts',(0.0139753396432458,0.195280280928346,
-0.140475197479493));
#82818=CARTESIAN_POINT('Ctrl Pts',(0.00171788443870832,0.195774465915562,
-0.139779963781474));
#82819=CARTESIAN_POINT('Ctrl Pts',(-0.0104887555978503,0.195118287215752,
-0.139084730083456));
#82820=CARTESIAN_POINT('Ctrl Pts',(-0.0226937098116175,0.194462199138832,
-0.138389592402098));
#82821=CARTESIAN_POINT('Ctrl Pts',(-0.0348469879742808,0.192656064389134,
-0.137694454720739));
#82822=CARTESIAN_POINT('Ctrl Pts',(-0.0467198318879055,0.189732488805597,
-0.136999317039381));
#82823=CARTESIAN_POINT('Ctrl Pts',(-0.0585920598278827,0.186809064899747,
-0.136304215422381));
#82824=CARTESIAN_POINT('Ctrl Pts',(-0.0701830392759854,0.182768550720884,
-0.135609113805381));
#82825=CARTESIAN_POINT('Ctrl Pts',(-0.0812776179338772,0.177693862648643,
-0.134914012188381));
#82826=CARTESIAN_POINT('Ctrl Pts',(-0.0923975425663838,0.172607581264116,
-0.13421732258607));
#82827=CARTESIAN_POINT('Ctrl Pts',(-0.103018034568636,0.166482832497714,
-0.133520632983759));
#82828=CARTESIAN_POINT('Ctrl Pts',(-0.112948223695707,0.159448608535742,
-0.132823943381448));
#82829=CARTESIAN_POINT('Ctrl Pts',(-0.116026846798592,0.157267811763085,
-0.132607951049604));
#82830=CARTESIAN_POINT('Ctrl Pts',(-0.119039350369695,0.154999900408411,
-0.132391958717759));
#82831=CARTESIAN_POINT('Ctrl Pts',(-0.121980713235812,0.152649486073431,
-0.132175966385915));
#82832=CARTESIAN_POINT('Ctrl Pts',(-0.131351103176399,0.145161699002201,
-0.131487872986465));
#82833=CARTESIAN_POINT('Ctrl Pts',(-0.140066232538382,0.136778248077627,
-0.130799779587016));
#82834=CARTESIAN_POINT('Ctrl Pts',(-0.147950444101791,0.127639437832054,
-0.130111686187566));
#82835=CARTESIAN_POINT('Ctrl Pts',(-0.155823820626387,0.118513186783163,
-0.129424538414528));
#82836=CARTESIAN_POINT('Ctrl Pts',(-0.162867891285451,0.108634248342843,
-0.12873739064149));
#82837=CARTESIAN_POINT('Ctrl Pts',(-0.168943071069768,0.0981804396889495,
-0.128050242868453));
#82838=CARTESIAN_POINT('Ctrl Pts',(-0.175012463749694,0.0877365891406759,
-0.12736374965973));
#82839=CARTESIAN_POINT('Ctrl Pts',(-0.180114328175564,0.076719721605862,
-0.126677256451007));
#82840=CARTESIAN_POINT('Ctrl Pts',(-0.18415346816745,0.0653349842113701,
-0.125990763242284));
#82841=CARTESIAN_POINT('Ctrl Pts',(-0.188200722658696,0.0539273752540016,
-0.12530289089129));
#82842=CARTESIAN_POINT('Ctrl Pts',(-0.191180699002706,0.042151276700291,
-0.124615018540296));
#82843=CARTESIAN_POINT('Ctrl Pts',(-0.19304760334189,0.0302288412604957,
-0.123927146189302));
#82844=CARTESIAN_POINT('Ctrl Pts',(-0.19462189927786,0.0201750633213751,
-0.123347087198647));
#82845=CARTESIAN_POINT('Ctrl Pts',(-0.195405571471215,0.0100177805586885,
-0.122767028207992));
#82846=CARTESIAN_POINT('Ctrl Pts',(-0.195399970103672,-0.000108090166289968,
-0.122186969217338));
#82847=CARTESIAN_POINT('',(-0.195399922633752,0.000173881349547679,-0.0521869692124231));
#82848=CARTESIAN_POINT('Ctrl Pts',(-0.195399970103625,-0.00010809025208222,
-0.122186969212423));
#82849=CARTESIAN_POINT('Ctrl Pts',(-0.195396443756117,-0.00648283898595459,
-0.121821792684227));
#82850=CARTESIAN_POINT('Ctrl Pts',(-0.195080985395644,-0.0128487550321653,
-0.12145661615603));
#82851=CARTESIAN_POINT('Ctrl Pts',(-0.194456030652044,-0.0191836425907903,
-0.121091439627833));
#82852=CARTESIAN_POINT('Ctrl Pts',(-0.193263735271741,-0.0312694091974816,
-0.120394751920406));
#82853=CARTESIAN_POINT('Ctrl Pts',(-0.19093622320459,-0.0432860108823252,
-0.119698064212978));
#82854=CARTESIAN_POINT('Ctrl Pts',(-0.18749822409405,-0.0550052357651287,
-0.119001376505551));
#82855=CARTESIAN_POINT('Ctrl Pts',(-0.184067398541676,-0.066700007895429,
-0.118306142472087));
#82856=CARTESIAN_POINT('Ctrl Pts',(-0.179530858135104,-0.0780977827826907,
-0.117610908438624));
#82857=CARTESIAN_POINT('Ctrl Pts',(-0.173964186021277,-0.0889810203467823,
-0.11691567440516));
#82858=CARTESIAN_POINT('Ctrl Pts',(-0.168398283310568,-0.0998627536733787,
-0.11622053646416));
#82859=CARTESIAN_POINT('Ctrl Pts',(-0.161802889014412,-0.110229292410544,
-0.115525398523159));
#82860=CARTESIAN_POINT('Ctrl Pts',(-0.154300875937143,-0.11988494352933,
-0.114830260582159));
#82861=CARTESIAN_POINT('Ctrl Pts',(-0.146799252541534,-0.129540093098714,
-0.114135158749134));
#82862=CARTESIAN_POINT('Ctrl Pts',(-0.138391662039633,-0.138483754014547,
-0.11344005691611));
#82863=CARTESIAN_POINT('Ctrl Pts',(-0.129241397230523,-0.14655313453455,
-0.112744955083086));
#82864=CARTESIAN_POINT('Ctrl Pts',(-0.120070229188774,-0.154640949071688,
-0.112048265331501));
#82865=CARTESIAN_POINT('Ctrl Pts',(-0.110153698806983,-0.161849966760308,
-0.111351575579916));
#82866=CARTESIAN_POINT('Ctrl Pts',(-0.0996873061692639,-0.168058326151118,
-0.110654885828331));
#82867=CARTESIAN_POINT('Ctrl Pts',(-0.096442466608256,-0.169983070507416,
-0.110438894842139));
#82868=CARTESIAN_POINT('Ctrl Pts',(-0.0931449582544428,-0.171811968871328,
-0.110222903855947));
#82869=CARTESIAN_POINT('Ctrl Pts',(-0.0898010367685515,-0.173542311253749,
-0.110006912869755));
#82870=CARTESIAN_POINT('Ctrl Pts',(-0.0790149934579321,-0.179123646807751,
-0.109310219439123));
#82871=CARTESIAN_POINT('Ctrl Pts',(-0.0676687750586451,-0.183715158419008,
-0.108613526008491));
#82872=CARTESIAN_POINT('Ctrl Pts',(-0.05596726049107,-0.187213316174691,
-0.10791683257786));
#82873=CARTESIAN_POINT('Ctrl Pts',(-0.0442901596874042,-0.190704175456567,
-0.107221592711963));
#82874=CARTESIAN_POINT('Ctrl Pts',(-0.0322600429270558,-0.193105889868855,
-0.106526352846067));
#82875=CARTESIAN_POINT('Ctrl Pts',(-0.0201005299208599,-0.194363393407557,
-0.105831112980171));
#82876=CARTESIAN_POINT('Ctrl Pts',(-0.00794269636402312,-0.195620723262205,
-0.105135969139514));
#82877=CARTESIAN_POINT('Ctrl Pts',(0.00434363363409507,-0.195734021012792,
-0.104440825298858));
#82878=CARTESIAN_POINT('Ctrl Pts',(0.016527413097827,-0.194699780729958,
-0.103745681458201));
#82879=CARTESIAN_POINT('Ctrl Pts',(0.0287105604776149,-0.193665594102615,
-0.103050573681005));
#82880=CARTESIAN_POINT('Ctrl Pts',(0.0407902983536555,-0.191484088585282,
-0.10235546590381));
#82881=CARTESIAN_POINT('Ctrl Pts',(0.052541164632059,-0.188203575999785,
-0.101660358126615));
#82882=CARTESIAN_POINT('Ctrl Pts',(0.0643188740718153,-0.184915569555829,
-0.100963662475829));
#82883=CARTESIAN_POINT('Ctrl Pts',(0.0757653876272328,-0.180523842190735,
-0.100266966825044));
#82884=CARTESIAN_POINT('Ctrl Pts',(0.0866720342857299,-0.175126007414014,
-0.0995702711742589));
#82885=CARTESIAN_POINT('Ctrl Pts',(0.0900528761425629,-0.173452786824697,
-0.0993543094867303));
#82886=CARTESIAN_POINT('Ctrl Pts',(0.0933820236128782,-0.171683224940323,
-0.0991383477992016));
#82887=CARTESIAN_POINT('Ctrl Pts',(0.0966537995815988,-0.169821091229682,
-0.098922386111673));
#82888=CARTESIAN_POINT('Ctrl Pts',(0.107208132624148,-0.163814084778215,
-0.0982257211821669));
#82889=CARTESIAN_POINT('Ctrl Pts',(0.117237377398798,-0.156798305440679,
-0.0975290562526608));
#82890=CARTESIAN_POINT('Ctrl Pts',(0.126543142295318,-0.148889197519588,
-0.0968323913231549));
#82891=CARTESIAN_POINT('Ctrl Pts',(0.135829490272315,-0.140996592327043,
-0.0961371800180442));
#82892=CARTESIAN_POINT('Ctrl Pts',(0.144394646745838,-0.13221486312393,
-0.0954419687129335));
#82893=CARTESIAN_POINT('Ctrl Pts',(0.152070661114356,-0.122701564897285,
-0.0947467574078229));
#82894=CARTESIAN_POINT('Ctrl Pts',(0.159745619057451,-0.113189575955592,
-0.0940516417824312));
#82895=CARTESIAN_POINT('Ctrl Pts',(0.166531093883671,-0.102946869348848,
-0.0933565261570396));
#82896=CARTESIAN_POINT('Ctrl Pts',(0.172298334522415,-0.0921653075772113,
-0.0926614105316478));
#82897=CARTESIAN_POINT('Ctrl Pts',(0.178065277385181,-0.0813843024825551,
-0.0919663307966842));
#82898=CARTESIAN_POINT('Ctrl Pts',(0.182813701569087,-0.0700652818063663,
-0.0912712510617206));
#82899=CARTESIAN_POINT('Ctrl Pts',(0.186461358328499,-0.0584236411933643,
-0.090576171326757));
#82900=CARTESIAN_POINT('Ctrl Pts',(0.190117351977106,-0.0467553930692292,
-0.0898795029547274));
#82901=CARTESIAN_POINT('Ctrl Pts',(0.192667356649156,-0.0347639068879149,
-0.0891828345826979));
#82902=CARTESIAN_POINT('Ctrl Pts',(0.194079618128655,-0.0226773417100732,
-0.0884861662106683));
#82903=CARTESIAN_POINT('Ctrl Pts',(0.194517693037703,-0.0189281628095307,
-0.088270063924977));
#82904=CARTESIAN_POINT('Ctrl Pts',(0.194846671950056,-0.01516986575135,
-0.0880539616392856));
#82905=CARTESIAN_POINT('Ctrl Pts',(0.195066625456177,-0.0114092783794373,
-0.0878378593535943));
#82906=CARTESIAN_POINT('Ctrl Pts',(0.195775744890149,0.000714672884618461,
-0.087141156067469));
#82907=CARTESIAN_POINT('Ctrl Pts',(0.195352724954443,0.0129475304762241,
-0.0864444527813439));
#82908=CARTESIAN_POINT('Ctrl Pts',(0.193786366364896,0.0250600121925408,
-0.0857477494952185));
#82909=CARTESIAN_POINT('Ctrl Pts',(0.192223276489041,0.0371472172990852,
-0.0850525001057845));
#82910=CARTESIAN_POINT('Ctrl Pts',(0.189521621688646,0.0491136765680657,
-0.0843572507163504));
#82911=CARTESIAN_POINT('Ctrl Pts',(0.185722098668139,0.0607327100194129,
-0.0836620013269164));
#82912=CARTESIAN_POINT('Ctrl Pts',(0.181923103784017,0.0723501284168967,
-0.0829668485776389));
#82913=CARTESIAN_POINT('Ctrl Pts',(0.177026772057464,0.0836193724441967,
-0.0822716958283615));
#82914=CARTESIAN_POINT('Ctrl Pts',(0.171123920650509,0.0943279586400468,
-0.081576543079084));
#82915=CARTESIAN_POINT('Ctrl Pts',(0.165221378424207,0.105035983939569,
-0.0808814267406471));
#82916=CARTESIAN_POINT('Ctrl Pts',(0.158312867207656,0.115182656519121,
-0.0801863104022101));
#82917=CARTESIAN_POINT('Ctrl Pts',(0.150534265355772,0.124581679848194,
-0.0794911940637732));
#82918=CARTESIAN_POINT('Ctrl Pts',(0.142737901980521,0.134002164742685,
-0.0787944905088514));
#82919=CARTESIAN_POINT('Ctrl Pts',(0.134068089445645,0.142670960403978,
-0.0780977869539296));
#82920=CARTESIAN_POINT('Ctrl Pts',(0.124698909072924,0.150437169861782,
-0.0774010833990079));
#82921=CARTESIAN_POINT('Ctrl Pts',(0.121795285730477,0.152844012954446,
-0.0771851664645099));
#82922=CARTESIAN_POINT('Ctrl Pts',(0.118824722122236,0.155164466597326,
-0.0769692495300118));
#82923=CARTESIAN_POINT('Ctrl Pts',(0.11579296795291,0.157394881024309,-0.0767533325955138));
#82924=CARTESIAN_POINT('Ctrl Pts',(0.106010014886606,0.164592047561869,
-0.0760566055132901));
#82925=CARTESIAN_POINT('Ctrl Pts',(0.0955191818643613,0.170898866630626,
-0.0753598784310665));
#82926=CARTESIAN_POINT('Ctrl Pts',(0.0845066983866875,0.176181094126985,
-0.0746631513488428));
#82927=CARTESIAN_POINT('Ctrl Pts',(0.0735171828830057,0.181452304847336,
-0.0739678773820345));
#82928=CARTESIAN_POINT('Ctrl Pts',(0.0620089255354657,0.185702724447798,
-0.0732726034152262));
#82929=CARTESIAN_POINT('Ctrl Pts',(0.050194229633594,0.188843054708109,
-0.072577329448418));
#82930=CARTESIAN_POINT('Ctrl Pts',(0.0383811633695494,0.191982951812882,
-0.0718821513829149));
#82931=CARTESIAN_POINT('Ctrl Pts',(0.0262625750398239,0.194012795377422,
-0.0711869733174118));
#82932=CARTESIAN_POINT('Ctrl Pts',(0.0140661510316737,0.194893056303076,
-0.0704917952519087));
#82933=CARTESIAN_POINT('Ctrl Pts',(0.0018703579051073,0.195773271695679,
-0.0697966531457195));
#82934=CARTESIAN_POINT('Ctrl Pts',(-0.0104023883744724,0.195503986493105,
-0.0691015110395303));
#82935=CARTESIAN_POINT('Ctrl Pts',(-0.0225218293580419,0.194097725907253,
-0.0684063689333411));
#82936=CARTESIAN_POINT('Ctrl Pts',(-0.0346689457229234,0.192688254051345,
-0.0677096394335682));
#82937=CARTESIAN_POINT('Ctrl Pts',(-0.0466611970798801,0.190136789244532,
-0.0670129099337952));
#82938=CARTESIAN_POINT('Ctrl Pts',(-0.0582772135502686,0.186507175145667,
-0.0663161804340223));
#82939=CARTESIAN_POINT('Ctrl Pts',(-0.0618749340328637,0.185383008610548,
-0.0661003889018261));
#82940=CARTESIAN_POINT('Ctrl Pts',(-0.0654366891829184,0.184155775180138,
-0.06588459736963));
#82941=CARTESIAN_POINT('Ctrl Pts',(-0.0689562978851465,0.182828304652138,
-0.0656688058374338));
#82942=CARTESIAN_POINT('Ctrl Pts',(-0.0803170025061345,0.178543453170741,
-0.0649722670842936));
#82943=CARTESIAN_POINT('Ctrl Pts',(-0.0913167663370378,0.173180569663799,
-0.0642757283311535));
#82944=CARTESIAN_POINT('Ctrl Pts',(-0.101741656481082,0.166822646353801,
-0.0635791895780133));
#82945=CARTESIAN_POINT('Ctrl Pts',(-0.112144788823725,0.160477992673583,
-0.0628841045717855));
#82946=CARTESIAN_POINT('Ctrl Pts',(-0.121974650517319,0.153142809387216,
-0.0621890195655576));
#82947=CARTESIAN_POINT('Ctrl Pts',(-0.131040793938003,0.144946439501279,
-0.0614939345593297));
#82948=CARTESIAN_POINT('Ctrl Pts',(-0.140105711886504,0.136751177520083,
-0.060798943507863));
#82949=CARTESIAN_POINT('Ctrl Pts',(-0.14840643765987,0.127695512494498,
-0.0601039524563963));
#82950=CARTESIAN_POINT('Ctrl Pts',(-0.155785882235974,0.11794879777242,
-0.0594089614049295));
#82951=CARTESIAN_POINT('Ctrl Pts',(-0.163164955042303,0.108202574081056,
-0.0587140053664863));
#82952=CARTESIAN_POINT('Ctrl Pts',(-0.169622332052514,0.0977660841308201,
-0.0580190493280431));
#82953=CARTESIAN_POINT('Ctrl Pts',(-0.175043182851466,0.0868391854938099,
-0.0573240932895998));
#82954=CARTESIAN_POINT('Ctrl Pts',(-0.180476453002008,0.0758872529643354,
-0.0566275450834874));
#82955=CARTESIAN_POINT('Ctrl Pts',(-0.184868126208397,0.0644434814927237,
-0.0559309968773751));
#82956=CARTESIAN_POINT('Ctrl Pts',(-0.188151256341738,0.0527282157580304,
-0.0552344486712627));
#82957=CARTESIAN_POINT('Ctrl Pts',(-0.189172765626258,0.0490831416267694,
-0.0550177254739597));
#82958=CARTESIAN_POINT('Ctrl Pts',(-0.190087330366273,0.045411874308117,
-0.0548010022766568));
#82959=CARTESIAN_POINT('Ctrl Pts',(-0.190893947145442,0.0417212289276486,
-0.0545842790793538));
#82960=CARTESIAN_POINT('Ctrl Pts',(-0.193868110175516,0.0281130554663777,
-0.0537851757903769));
#82961=CARTESIAN_POINT('Ctrl Pts',(-0.195387462253079,0.0141762883117028,
-0.0529860725014));
#82962=CARTESIAN_POINT('Ctrl Pts',(-0.195399922633752,0.000173881349547679,
-0.0521869692124231));
#82963=CARTESIAN_POINT('',(0.00542534466917562,0.195638851078239,1.80411241501588E-16));
#82964=CARTESIAN_POINT('Ctrl Pts',(-0.195432320986697,0.000173604797042496,
-0.0521869517874278));
#82965=CARTESIAN_POINT('Ctrl Pts',(-0.19496687862426,-0.0505761822068533,
-0.0492912186320431));
#82966=CARTESIAN_POINT('Ctrl Pts',(-0.148879977450944,-0.166826599982022,
-0.0427006432239653));
#82967=CARTESIAN_POINT('Ctrl Pts',(0.0467197021695734,-0.225989356129055,
-0.032415225563194));
#82968=CARTESIAN_POINT('Ctrl Pts',(0.214983941469384,-0.0838177601457405,
-0.021330698805113));
#82969=CARTESIAN_POINT('Ctrl Pts',(0.18806769685446,0.129051521723346,-0.0105256236173826));
#82970=CARTESIAN_POINT('Ctrl Pts',(0.0650705990701268,0.193654330577805,
-0.0034153906823444));
#82971=CARTESIAN_POINT('Ctrl Pts',(0.00542534466917562,0.195638851078239,
1.80411241501588E-16));
#82972=CARTESIAN_POINT('',(0.157947475570094,0.115038058750287,0.));
#82973=CARTESIAN_POINT('Origin',(0.,0.,0.));
#82974=CARTESIAN_POINT('',(-0.195399925034678,0.000171162035267742,-0.0420130307875766));
#82975=CARTESIAN_POINT('Ctrl Pts',(0.157947475570094,0.115038058750287,
0.));
#82976=CARTESIAN_POINT('Ctrl Pts',(0.196099648170939,0.0626550525062515,
-0.0036948422526933));
#82977=CARTESIAN_POINT('Ctrl Pts',(0.2155636754795,-0.0821381146635345,
-0.0110845267580803));
#82978=CARTESIAN_POINT('Ctrl Pts',(0.0481663642357293,-0.22581952090303,
-0.0221690535161595));
#82979=CARTESIAN_POINT('Ctrl Pts',(-0.148247008667004,-0.167596420983037,
-0.0324785467239276));
#82980=CARTESIAN_POINT('Ctrl Pts',(-0.19497457278765,-0.0509793119047676,
-0.039093197679001));
#82981=CARTESIAN_POINT('Ctrl Pts',(-0.195445212794411,0.000170774153815293,
-0.0420130063813814));
#82982=CARTESIAN_POINT('',(-0.195399966640887,-0.00011417854461868,-0.112013030792447));
#82983=CARTESIAN_POINT('Ctrl Pts',(-0.195399925034678,0.000171162035267742,
-0.0420130307875766));
#82984=CARTESIAN_POINT('Ctrl Pts',(-0.195388034908535,0.0137450235125697,
-0.0427880562024912));
#82985=CARTESIAN_POINT('Ctrl Pts',(-0.193960346547734,0.0272581797347334,
-0.0435630816174058));
#82986=CARTESIAN_POINT('Ctrl Pts',(-0.191162448998049,0.0404731774520893,
-0.0443381070323203));
#82987=CARTESIAN_POINT('Ctrl Pts',(-0.18865081136394,0.0523361156091008,
-0.0450338376532321));
#82988=CARTESIAN_POINT('Ctrl Pts',(-0.185021626603632,0.0640071061046373,
-0.0457295682741437));
#82989=CARTESIAN_POINT('Ctrl Pts',(-0.180323926183208,0.0752624849833763,
-0.0464252988950553));
#82990=CARTESIAN_POINT('Ctrl Pts',(-0.175636184117986,0.0864940043030182,
-0.0471195546810419));
#82991=CARTESIAN_POINT('Ctrl Pts',(-0.169884686431536,0.0973108296489234,
-0.0478138104670284));
#82992=CARTESIAN_POINT('Ctrl Pts',(-0.163167874027577,0.107505371425435,
-0.0485080662530149));
#82993=CARTESIAN_POINT('Ctrl Pts',(-0.15645214632649,0.117698266878054,
-0.0492022099231346));
#82994=CARTESIAN_POINT('Ctrl Pts',(-0.148771856484054,0.127268320790351,
-0.049896353593254));
#82995=CARTESIAN_POINT('Ctrl Pts',(-0.140270093219887,0.136034778450528,
-0.0505904972633736));
#82996=CARTESIAN_POINT('Ctrl Pts',(-0.131768898910346,0.144800649442212,
-0.0512845944800411));
#82997=CARTESIAN_POINT('Ctrl Pts',(-0.122446970559794,0.152762419409819,
-0.0519786916967088));
#82998=CARTESIAN_POINT('Ctrl Pts',(-0.112483994582994,0.159776440574488,
-0.0526727889133763));
#82999=CARTESIAN_POINT('Ctrl Pts',(-0.102498182728351,0.166806538394453,
-0.0533684770522029));
#83000=CARTESIAN_POINT('Ctrl Pts',(-0.0918691449919437,0.172884099581189,
-0.0540641651910295));
#83001=CARTESIAN_POINT('Ctrl Pts',(-0.0808041029838316,0.177909687597327,
-0.0547598533298561));
#83002=CARTESIAN_POINT('Ctrl Pts',(-0.0772902231149733,0.179505642908308,
-0.0549807801500376));
#83003=CARTESIAN_POINT('Ctrl Pts',(-0.0737325233941246,0.180995874483825,
-0.0552017069702189));
#83004=CARTESIAN_POINT('Ctrl Pts',(-0.0701379921819701,0.182378238977905,
-0.0554226337904004));
#83005=CARTESIAN_POINT('Ctrl Pts',(-0.0587992620769335,0.186738823705104,
-0.0561195340088575));
#83006=CARTESIAN_POINT('Ctrl Pts',(-0.0470127009258709,0.190053187710039,
-0.0568164342273145));
#83007=CARTESIAN_POINT('Ctrl Pts',(-0.0349934860263581,0.192241036034773,
-0.0575133344457717));
#83008=CARTESIAN_POINT('Ctrl Pts',(-0.0229993172646902,0.194424325230548,
-0.058208782434688));
#83009=CARTESIAN_POINT('Ctrl Pts',(-0.0107742956381948,0.195485530924792,
-0.0589042304236042));
#83010=CARTESIAN_POINT('Ctrl Pts',(0.00145313166310702,0.195394596671376,
-0.0595996784125205));
#83011=CARTESIAN_POINT('Ctrl Pts',(0.0136788475491207,0.195303675145598,
-0.0602950290628641));
#83012=CARTESIAN_POINT('Ctrl Pts',(0.0259060951035811,0.194060895136054,
-0.0609903797132079));
#83013=CARTESIAN_POINT('Ctrl Pts',(0.0379047371236277,0.191688264908389,
-0.0616857303635516));
#83014=CARTESIAN_POINT('Ctrl Pts',(0.0499027469665529,0.189315759688416,
-0.062381044377685));
#83015=CARTESIAN_POINT('Ctrl Pts',(0.0616713226686245,0.18581371845615,
-0.0630763583918182));
#83016=CARTESIAN_POINT('Ctrl Pts',(0.0729915885107183,0.181255035810545,
-0.0637716724059516));
#83017=CARTESIAN_POINT('Ctrl Pts',(0.0843376302544334,0.176685973182965,
-0.0644685696289843));
#83018=CARTESIAN_POINT('Ctrl Pts',(0.095232538151035,0.171055852766036,
-0.0651654668520171));
#83019=CARTESIAN_POINT('Ctrl Pts',(0.105479553706685,0.164484721934405,
-0.0658623640750498));
#83020=CARTESIAN_POINT('Ctrl Pts',(0.108639866435306,0.162458099812495,
-0.06607729623286));
#83021=CARTESIAN_POINT('Ctrl Pts',(0.111738766308828,0.160342278569007,
-0.06629222839067));
#83022=CARTESIAN_POINT('Ctrl Pts',(0.114771100586274,0.158141564650839,
-0.0665071605484802));
#83023=CARTESIAN_POINT('Ctrl Pts',(0.12460217738225,0.151006669366897,-0.0672039882581008));
#83024=CARTESIAN_POINT('Ctrl Pts',(0.133799720311098,0.142926611734703,
-0.0679008159677215));
#83025=CARTESIAN_POINT('Ctrl Pts',(0.14217924747587,0.134038134824367,-0.0685976436773421));
#83026=CARTESIAN_POINT('Ctrl Pts',(0.150541356185308,0.125168134319085,
-0.0692930228968395));
#83027=CARTESIAN_POINT('Ctrl Pts',(0.158088176868394,0.115493629854552,
-0.0699884021163368));
#83028=CARTESIAN_POINT('Ctrl Pts',(0.164670142831369,0.105189847703552,
-0.0706837813358341));
#83029=CARTESIAN_POINT('Ctrl Pts',(0.17125124987678,0.094887410150733,-0.0713790698114066));
#83030=CARTESIAN_POINT('Ctrl Pts',(0.176867244078257,0.0839565695938618,
-0.0720743582869791));
#83031=CARTESIAN_POINT('Ctrl Pts',(0.18141131068929,0.0726023164506069,
-0.0727696467625515));
#83032=CARTESIAN_POINT('Ctrl Pts',(0.185955162558449,0.0612485998825829,
-0.07346490238043));
#83033=CARTESIAN_POINT('Ctrl Pts',(0.189426887723643,0.0494723325132606,
-0.0741601579983084));
#83034=CARTESIAN_POINT('Ctrl Pts',(0.191768488377404,0.0374967580658035,
-0.0748554136161869));
#83035=CARTESIAN_POINT('Ctrl Pts',(0.194115443834778,0.0254937977149432,
-0.0755522591538872));
#83036=CARTESIAN_POINT('Ctrl Pts',(0.195327011951379,0.0132914905823344,
-0.0762491046915876));
#83037=CARTESIAN_POINT('Ctrl Pts',(0.195396789033291,0.00112019439362784,
-0.0769459502292879));
#83038=CARTESIAN_POINT('Ctrl Pts',(0.195418342183163,-0.00263934618474026,
-0.0771611959217122));
#83039=CARTESIAN_POINT('Ctrl Pts',(0.195331332677064,-0.00639593946438014,
-0.0773764416141365));
#83040=CARTESIAN_POINT('Ctrl Pts',(0.195136572149948,-0.0101428896064249,
-0.0775916873065607));
#83041=CARTESIAN_POINT('Ctrl Pts',(0.194506316991174,-0.0222682144433514,
-0.07828823352187));
#83042=CARTESIAN_POINT('Ctrl Pts',(0.192739361234437,-0.0343772940435297,
-0.0789847797371793));
#83043=CARTESIAN_POINT('Ctrl Pts',(0.189849733125944,-0.0462410946238046,
-0.0796813259524885));
#83044=CARTESIAN_POINT('Ctrl Pts',(0.186966149150865,-0.0580800801099577,
-0.0803764152265944));
#83045=CARTESIAN_POINT('Ctrl Pts',(0.182964686843806,-0.069673945306825,
-0.0810715045007004));
#83046=CARTESIAN_POINT('Ctrl Pts',(0.177910671093355,-0.080801937545532,
-0.0817665937748063));
#83047=CARTESIAN_POINT('Ctrl Pts',(0.172857372559139,-0.0919283506089666,
-0.0824615844086751));
#83048=CARTESIAN_POINT('Ctrl Pts',(0.166752137064087,-0.102588207318666,
-0.0831565750425438));
#83049=CARTESIAN_POINT('Ctrl Pts',(0.159708547162265,-0.112580371128001,
-0.0838515656764126));
#83050=CARTESIAN_POINT('Ctrl Pts',(0.15266533965571,-0.122571992464507,
-0.0845465185793612));
#83051=CARTESIAN_POINT('Ctrl Pts',(0.144684405290716,-0.131895292923133,
-0.0852414714823097));
#83052=CARTESIAN_POINT('Ctrl Pts',(0.135921235042931,-0.140380119192157,
-0.0859364243852583));
#83053=CARTESIAN_POINT('Ctrl Pts',(0.127138037481661,-0.148884336648475,
-0.0866329655307324));
#83054=CARTESIAN_POINT('Ctrl Pts',(0.11756970903862,-0.156545692955718,
-0.0873295066762065));
#83055=CARTESIAN_POINT('Ctrl Pts',(0.107405816032028,-0.163233423913407,
-0.0880260478216805));
#83056=CARTESIAN_POINT('Ctrl Pts',(0.104243418436957,-0.16531424710619,
-0.0882427699026672));
#83057=CARTESIAN_POINT('Ctrl Pts',(0.101023563147127,-0.167301141092061,
-0.088459491983654));
#83058=CARTESIAN_POINT('Ctrl Pts',(0.0977524379413281,-0.169191078005097,
-0.0886762140646408));
#83059=CARTESIAN_POINT('Ctrl Pts',(0.0872362900268904,-0.175266924961737,
-0.0893729411284476));
#83060=CARTESIAN_POINT('Ctrl Pts',(0.0761146347337262,-0.180379874266155,
-0.0900696681922544));
#83061=CARTESIAN_POINT('Ctrl Pts',(0.064587354304539,-0.184417010234794,
-0.0907663952560613));
#83062=CARTESIAN_POINT('Ctrl Pts',(0.0530841161000037,-0.188445726027442,
-0.0914616691697785));
#83063=CARTESIAN_POINT('Ctrl Pts',(0.04117772512102,-0.191402726279639,
-0.0921569430834958));
#83064=CARTESIAN_POINT('Ctrl Pts',(0.0290890283688226,-0.193222639534186,
-0.092852216997213));
#83065=CARTESIAN_POINT('Ctrl Pts',(0.0170019999063227,-0.195042301633244,
-0.0935473949602805));
#83066=CARTESIAN_POINT('Ctrl Pts',(0.00473357266567613,-0.195725013420667,
-0.094242572923348));
#83067=CARTESIAN_POINT('Ctrl Pts',(-0.00748559849745745,-0.195256564076947,
-0.0949377508864155));
#83068=CARTESIAN_POINT('Ctrl Pts',(-0.0197041370974415,-0.194788138983954,
-0.0956328928614478));
#83069=CARTESIAN_POINT('Ctrl Pts',(-0.0318725515042455,-0.193168731601081,
-0.0963280348364801));
#83070=CARTESIAN_POINT('Ctrl Pts',(-0.0437633637775224,-0.190436152006063,
-0.0970231768115124));
#83071=CARTESIAN_POINT('Ctrl Pts',(-0.0556813286728416,-0.18769733257652,
-0.0977199061404512));
#83072=CARTESIAN_POINT('Ctrl Pts',(-0.067319588594467,-0.183840525811168,
-0.09841663546939));
#83073=CARTESIAN_POINT('Ctrl Pts',(-0.0784651523874021,-0.178953569008337,
-0.0991133647983288));
#83074=CARTESIAN_POINT('Ctrl Pts',(-0.0819171724082724,-0.177439973730619,
-0.0993291568064593));
#83075=CARTESIAN_POINT('Ctrl Pts',(-0.0853220936137374,-0.175827899478522,
-0.0995449488145898));
#83076=CARTESIAN_POINT('Ctrl Pts',(-0.0886740841316249,-0.174120839658605,
-0.0997607408227204));
#83077=CARTESIAN_POINT('Ctrl Pts',(-0.0994962453262731,-0.168609464718409,
-0.100457442046678));
#83078=CARTESIAN_POINT('Ctrl Pts',(-0.109840577283525,-0.162065955095513,
-0.101154143270635));
#83079=CARTESIAN_POINT('Ctrl Pts',(-0.119503538064972,-0.154596456589256,
-0.101850844494592));
#83080=CARTESIAN_POINT('Ctrl Pts',(-0.129146346415747,-0.147142535974105,
-0.102546092724645));
#83081=CARTESIAN_POINT('Ctrl Pts',(-0.138109873678078,-0.138766931092801,
-0.103241340954697));
#83082=CARTESIAN_POINT('Ctrl Pts',(-0.146219037064314,-0.12961926245734,
-0.10393658918475));
#83083=CARTESIAN_POINT('Ctrl Pts',(-0.154327088704783,-0.120472847944085,
-0.104631742098031));
#83084=CARTESIAN_POINT('Ctrl Pts',(-0.161580395584372,-0.110555203472283,
-0.105326895011312));
#83085=CARTESIAN_POINT('Ctrl Pts',(-0.167841443444275,-0.100052035774102,
-0.106022047924593));
#83086=CARTESIAN_POINT('Ctrl Pts',(-0.174102170277236,-0.0895494066119433,
-0.106717165194828));
#83087=CARTESIAN_POINT('Ctrl Pts',(-0.179370314350734,-0.0784620792201427,
-0.107412282465063));
#83088=CARTESIAN_POINT('Ctrl Pts',(-0.183553723170007,-0.0670014231970367,
-0.108107399735299));
#83089=CARTESIAN_POINT('Ctrl Pts',(-0.187746690965306,-0.0555145798848333,
-0.108804105329699));
#83090=CARTESIAN_POINT('Ctrl Pts',(-0.190849737003367,-0.0436535486320951,
-0.1095008109241));
#83091=CARTESIAN_POINT('Ctrl Pts',(-0.19282055720892,-0.0316447897392526,
-0.1101975165185));
#83092=CARTESIAN_POINT('Ctrl Pts',(-0.193431336899323,-0.0279231382065417,
-0.110413433539267));
#83093=CARTESIAN_POINT('Ctrl Pts',(-0.193933747380923,-0.0241873459357263,
-0.110629350560034));
#83094=CARTESIAN_POINT('Ctrl Pts',(-0.194327542883033,-0.0204442186703937,
-0.110845267580801));
#83095=CARTESIAN_POINT('Ctrl Pts',(-0.195037475950106,-0.0136961227534052,
-0.111234521983059));
#83096=CARTESIAN_POINT('Ctrl Pts',(-0.195395995378517,-0.00691041122818272,
-0.111623776385318));
#83097=CARTESIAN_POINT('Ctrl Pts',(-0.195399966640838,-0.000114178629661407,
-0.112013030787576));
#83098=CARTESIAN_POINT('',(-0.195399983188327,-8.10555470994038E-5,-0.182013030783586));
#83099=CARTESIAN_POINT('Ctrl Pts',(-0.195399966640887,-0.000114178544617379,
-0.112013030792447));
#83100=CARTESIAN_POINT('Ctrl Pts',(-0.195406979528763,0.0118873587108309,
-0.11270041915692));
#83101=CARTESIAN_POINT('Ctrl Pts',(-0.194303978816564,0.0239328297705788,
-0.113387807521392));
#83102=CARTESIAN_POINT('Ctrl Pts',(-0.192092962998488,0.0357973960849315,
-0.114075195885865));
#83103=CARTESIAN_POINT('Ctrl Pts',(-0.18988411234439,0.0476503438792405,
-0.114761911116969));
#83104=CARTESIAN_POINT('Ctrl Pts',(-0.186569478115567,0.0593218440159743,
-0.115448626348073));
#83105=CARTESIAN_POINT('Ctrl Pts',(-0.182202859798727,0.0705923358528781,
-0.116135341579177));
#83106=CARTESIAN_POINT('Ctrl Pts',(-0.177839396744258,0.0818546837769824,
-0.116821560598666));
#83107=CARTESIAN_POINT('Ctrl Pts',(-0.172425776388526,0.0927157563474014,
-0.117507779618155));
#83108=CARTESIAN_POINT('Ctrl Pts',(-0.166064658076759,0.102974216859605,
-0.118193998637643));
#83109=CARTESIAN_POINT('Ctrl Pts',(-0.159688758125428,0.113256515454729,
-0.118881812257595));
#83110=CARTESIAN_POINT('Ctrl Pts',(-0.152361462661492,0.122932650620025,
-0.119569625877548));
#83111=CARTESIAN_POINT('Ctrl Pts',(-0.14422923316195,0.131829770164087,
-0.1202574394975));
#83112=CARTESIAN_POINT('Ctrl Pts',(-0.137638313286628,0.139040609705612,
-0.120814891111293));
#83113=CARTESIAN_POINT('Ctrl Pts',(-0.130519651799363,0.145740203779063,
-0.121372342725087));
#83114=CARTESIAN_POINT('Ctrl Pts',(-0.122967811914694,0.151855448479508,
-0.121929794338881));
#83115=CARTESIAN_POINT('Ctrl Pts',(-0.113529653954175,0.159498174799379,
-0.122626487656891));
#83116=CARTESIAN_POINT('Ctrl Pts',(-0.103343136437121,0.16628445122242,
-0.1233231809749));
#83117=CARTESIAN_POINT('Ctrl Pts',(-0.09258803740114,0.172071541314086,
-0.12401987429291));
#83118=CARTESIAN_POINT('Ctrl Pts',(-0.0818553769234864,0.177846557694655,
-0.124715114087006));
#83119=CARTESIAN_POINT('Ctrl Pts',(-0.0705572173752286,0.182626050012364,
-0.125410353881101));
#83120=CARTESIAN_POINT('Ctrl Pts',(-0.058901470050085,0.186310968077403,
-0.126105593675196));
#83121=CARTESIAN_POINT('Ctrl Pts',(-0.0472473315871257,0.189995377507074,
-0.126800737504187));
#83122=CARTESIAN_POINT('Ctrl Pts',(-0.0352365226550576,0.192585206048322,
-0.127495881333177));
#83123=CARTESIAN_POINT('Ctrl Pts',(-0.0230946316147195,0.194030404809608,
-0.128191025162168));
#83124=CARTESIAN_POINT('Ctrl Pts',(-0.0109533698761371,0.195475528667725,
-0.128886132962567));
#83125=CARTESIAN_POINT('Ctrl Pts',(0.00131808846455855,0.195776063967537,
-0.129581240762965));
#83126=CARTESIAN_POINT('Ctrl Pts',(0.01348917058184,0.194933840769154,-0.130276348563364));
#83127=CARTESIAN_POINT('Ctrl Pts',(0.0256880566690686,0.194089693571881,
-0.130973044288009));
#83128=CARTESIAN_POINT('Ctrl Pts',(0.0377852410819525,0.192097701857036,
-0.131669740012654));
#83129=CARTESIAN_POINT('Ctrl Pts',(0.0495566499006659,0.189011371220418,
-0.132366435737299));
#83130=CARTESIAN_POINT('Ctrl Pts',(0.0532055519806167,0.18805467024666,
-0.132582397523853));
#83131=CARTESIAN_POINT('Ctrl Pts',(0.0568232602525872,0.186993179440627,
-0.132798359310407));
#83132=CARTESIAN_POINT('Ctrl Pts',(0.0604034538302661,0.185829445366914,
-0.133014321096962));
#83133=CARTESIAN_POINT('Ctrl Pts',(0.0719530707618956,0.182075267703038,
-0.133711008539261));
#83134=CARTESIAN_POINT('Ctrl Pts',(0.0831918879570605,0.177227057516715,
-0.134407695981561));
#83135=CARTESIAN_POINT('Ctrl Pts',(0.0939022926886606,0.171357869465669,
-0.135104383423861));
#83136=CARTESIAN_POINT('Ctrl Pts',(0.104590351401938,0.165500926795354,
-0.135799617308547));
#83137=CARTESIAN_POINT('Ctrl Pts',(0.114751390751995,0.158627585957298,
-0.136494851193232));
#83138=CARTESIAN_POINT('Ctrl Pts',(0.124189118482288,0.15085828731161,-0.137190085077917));
#83139=CARTESIAN_POINT('Ctrl Pts',(0.133625544082522,0.143090060601624,
-0.137885223040686));
#83140=CARTESIAN_POINT('Ctrl Pts',(0.142338152868517,0.134426641736287,
-0.138580361003454));
#83141=CARTESIAN_POINT('Ctrl Pts',(0.150162125068484,0.125029981184182,
-0.139275498966222));
#83142=CARTESIAN_POINT('Ctrl Pts',(0.157985691976748,0.115633807391036,
-0.139970600919961));
#83143=CARTESIAN_POINT('Ctrl Pts',(0.164920174608912,0.105505157029631,
-0.140665702873699));
#83144=CARTESIAN_POINT('Ctrl Pts',(0.170841551236229,0.0948384118972837,
-0.141360804827437));
#83145=CARTESIAN_POINT('Ctrl Pts',(0.176776456107866,0.0841472970375365,
-0.142057494842474));
#83146=CARTESIAN_POINT('Ctrl Pts',(0.181693267050085,0.0729164293198139,
-0.142754184857511));
#83147=CARTESIAN_POINT('Ctrl Pts',(0.185514843110899,0.0613628795407983,
-0.143450874872548));
#83148=CARTESIAN_POINT('Ctrl Pts',(0.186699625431348,0.0577809957057574,
-0.143666865866713));
#83149=CARTESIAN_POINT('Ctrl Pts',(0.187779502715479,0.0541682031150062,
-0.143882856860877));
#83150=CARTESIAN_POINT('Ctrl Pts',(0.188753168329718,0.0505311927970559,
-0.144098847855041));
#83151=CARTESIAN_POINT('Ctrl Pts',(0.191893746382104,0.0387999427520509,
-0.144795531157671));
#83152=CARTESIAN_POINT('Ctrl Pts',(0.193947498709438,0.0267336131564428,
-0.145492214460302));
#83153=CARTESIAN_POINT('Ctrl Pts',(0.194857195170143,0.0145545006930803,
-0.146188897762932));
#83154=CARTESIAN_POINT('Ctrl Pts',(0.195764993449915,0.00240080127686617,
-0.146884127359828));
#83155=CARTESIAN_POINT('Ctrl Pts',(0.195533336034077,-0.00986435549050084,
-0.147579356956725));
#83156=CARTESIAN_POINT('Ctrl Pts',(0.194156346448908,-0.0220107504100111,
-0.148274586553622));
#83157=CARTESIAN_POINT('Ctrl Pts',(0.19277954714799,-0.034155466836306,
-0.148969720077719));
#83158=CARTESIAN_POINT('Ctrl Pts',(0.190257783232272,-0.0461805807952212,
-0.149664853601817));
#83159=CARTESIAN_POINT('Ctrl Pts',(0.186637132307281,-0.0578596650881648,
-0.150359987125914));
#83160=CARTESIAN_POINT('Ctrl Pts',(0.18301666941663,-0.0695381428413006,
-0.151055084549052));
#83161=CARTESIAN_POINT('Ctrl Pts',(0.178297717738639,-0.0808697988692114,
-0.151750181972189));
#83162=CARTESIAN_POINT('Ctrl Pts',(0.172575772659037,-0.091644763577285,
-0.152445279395327));
#83163=CARTESIAN_POINT('Ctrl Pts',(0.166840755320049,-0.102444344588305,
-0.153141964826333));
#83164=CARTESIAN_POINT('Ctrl Pts',(0.160098637886572,-0.112683953777672,
-0.15383865025734));
#83165=CARTESIAN_POINT('Ctrl Pts',(0.152489474724976,-0.122180686272835,
-0.154535335688346));
#83166=CARTESIAN_POINT('Ctrl Pts',(0.150130191900801,-0.125125225295825,
-0.154751348663271));
#83167=CARTESIAN_POINT('Ctrl Pts',(0.147687841662342,-0.127998594515703,
-0.154967361638196));
#83168=CARTESIAN_POINT('Ctrl Pts',(0.14516732599168,-0.130796052939014,
-0.155183374613122));
#83169=CARTESIAN_POINT('Ctrl Pts',(0.137038132673913,-0.139818444898807,
-0.155880061903247));
#83170=CARTESIAN_POINT('Ctrl Pts',(0.128036060866306,-0.148111738733537,
-0.156576749193372));
#83171=CARTESIAN_POINT('Ctrl Pts',(0.118316396013281,-0.155506882273514,
-0.157273436483497));
#83172=CARTESIAN_POINT('Ctrl Pts',(0.108617010874177,-0.162886596125568,
-0.157968670161883));
#83173=CARTESIAN_POINT('Ctrl Pts',(0.0982036492653511,-0.169371295979603,
-0.158663903840268));
#83174=CARTESIAN_POINT('Ctrl Pts',(0.0872662056366348,-0.174830687677491,
-0.159359137518654));
#83175=CARTESIAN_POINT('Ctrl Pts',(0.0763302722588966,-0.180289325538201,
-0.160054275198616));
#83176=CARTESIAN_POINT('Ctrl Pts',(0.0648711619465925,-0.184722505559066,
-0.160749412878579));
#83177=CARTESIAN_POINT('Ctrl Pts',(0.0531038798602043,-0.188045574113812,
-0.161444550558541));
#83178=CARTESIAN_POINT('Ctrl Pts',(0.0413372080917684,-0.191368470315385,
-0.162139652184723));
#83179=CARTESIAN_POINT('Ctrl Pts',(0.0292632456717851,-0.193581157594719,
-0.162834753810905));
#83180=CARTESIAN_POINT('Ctrl Pts',(0.0171100205517335,-0.194649446946862,
-0.163529855437087));
#83181=CARTESIAN_POINT('Ctrl Pts',(0.0049290306725261,-0.195720176869,-0.164226545063906));
#83182=CARTESIAN_POINT('Ctrl Pts',(-0.00733070674353389,-0.195641278068855,
-0.164923234690725));
#83183=CARTESIAN_POINT('Ctrl Pts',(-0.0194395154429373,-0.194430618060386,
-0.165619924317545));
#83184=CARTESIAN_POINT('Ctrl Pts',(-0.0231935688416982,-0.194055281193452,
-0.165835916668764));
#83185=CARTESIAN_POINT('Ctrl Pts',(-0.0269331667609787,-0.193571538690036,
-0.166051909019983));
#83186=CARTESIAN_POINT('Ctrl Pts',(-0.0306516653744782,-0.192980919807558,
-0.166267901371201));
#83187=CARTESIAN_POINT('Ctrl Pts',(-0.0426457312406904,-0.191075870884705,
-0.166964587522357));
#83188=CARTESIAN_POINT('Ctrl Pts',(-0.0545036084208412,-0.188041687468554,
-0.167661273673513));
#83189=CARTESIAN_POINT('Ctrl Pts',(-0.0659989479753539,-0.183916554084037,
-0.168357959824668));
#83190=CARTESIAN_POINT('Ctrl Pts',(-0.0774703026853929,-0.179800027725193,
-0.16905319235117));
#83191=CARTESIAN_POINT('Ctrl Pts',(-0.0885797808718527,-0.174597292625729,
-0.169748424877671));
#83192=CARTESIAN_POINT('Ctrl Pts',(-0.0991146946313072,-0.16839666655888,
-0.170443657404173));
#83193=CARTESIAN_POINT('Ctrl Pts',(-0.109648153704876,-0.162196896689189,
-0.171138793931318));
#83194=CARTESIAN_POINT('Ctrl Pts',(-0.119606429941285,-0.154999913465743,
-0.171833930458463));
#83195=CARTESIAN_POINT('Ctrl Pts',(-0.128801441376143,-0.146939949297079,
-0.172529066985608));
#83196=CARTESIAN_POINT('Ctrl Pts',(-0.13799597588318,-0.138880403183484,
-0.173224167457339));
#83197=CARTESIAN_POINT('Ctrl Pts',(-0.146426684035344,-0.129958562083755,
-0.173919267929069));
#83198=CARTESIAN_POINT('Ctrl Pts',(-0.153940718427832,-0.12034706149268,
-0.1746143684008));
#83199=CARTESIAN_POINT('Ctrl Pts',(-0.161471919307272,-0.110713602564596,
-0.175311056892035));
#83200=CARTESIAN_POINT('Ctrl Pts',(-0.168081778633305,-0.10038806776869,
-0.176007745383271));
#83201=CARTESIAN_POINT('Ctrl Pts',(-0.173660212725031,-0.0895728224200685,
-0.176704433874507));
#83202=CARTESIAN_POINT('Ctrl Pts',(-0.175389724688914,-0.086219713659579,
-0.176920431959431));
#83203=CARTESIAN_POINT('Ctrl Pts',(-0.177020436780129,-0.082819694360548,
-0.177136430044356));
#83204=CARTESIAN_POINT('Ctrl Pts',(-0.178550013560408,-0.0793791701744119,
-0.177352428129281));
#83205=CARTESIAN_POINT('Ctrl Pts',(-0.184050640726163,-0.0670064399874064,
-0.178129195238332));
#83206=CARTESIAN_POINT('Ctrl Pts',(-0.188273338435027,-0.0540322449477344,
-0.178905962347383));
#83207=CARTESIAN_POINT('Ctrl Pts',(-0.1911093419295,-0.0407232050221174,
-0.179682729456434));
#83208=CARTESIAN_POINT('Ctrl Pts',(-0.193945345423973,-0.0274141650965003,
-0.180459496565485));
#83209=CARTESIAN_POINT('Ctrl Pts',(-0.195394304400981,-0.0137708644685566,
-0.181236263674536));
#83210=CARTESIAN_POINT('Ctrl Pts',(-0.195399983188326,-8.10555470994277E-5,
-0.182013030783586));
#83211=CARTESIAN_POINT('',(-0.195399922115002,0.00017446332273763,-0.252013030791491));
#83212=CARTESIAN_POINT('Ctrl Pts',(-0.195399983188356,-8.105547677933E-5,
-0.182013030787576));
#83213=CARTESIAN_POINT('Ctrl Pts',(-0.19540516234588,0.0124043105133673,
-0.182721457157962));
#83214=CARTESIAN_POINT('Ctrl Pts',(-0.194209352567215,0.0248838378421996,
-0.183429883528347));
#83215=CARTESIAN_POINT('Ctrl Pts',(-0.191841856825415,0.0371195631679168,
-0.184138309898733));
#83216=CARTESIAN_POINT('Ctrl Pts',(-0.189447577492252,0.0494937118332676,
-0.184854750730171));
#83217=CARTESIAN_POINT('Ctrl Pts',(-0.185855101489844,0.0616176612605396,
-0.185571191561609));
#83218=CARTESIAN_POINT('Ctrl Pts',(-0.18114698418511,0.0732593346996781,
-0.186287632393047));
#83219=CARTESIAN_POINT('Ctrl Pts',(-0.176438866880377,0.0849010081388166,
-0.187004073224486));
#83220=CARTESIAN_POINT('Ctrl Pts',(-0.17061556133838,0.0960596672418057,
-0.187720514055924));
#83221=CARTESIAN_POINT('Ctrl Pts',(-0.163806866578169,0.10652920004319,
-0.188436954887362));
#83222=CARTESIAN_POINT('Ctrl Pts',(-0.157185909241894,0.116710054443329,
-0.189133641160719));
#83223=CARTESIAN_POINT('Ctrl Pts',(-0.149588953930905,0.126307024607797,
-0.189830327434076));
#83224=CARTESIAN_POINT('Ctrl Pts',(-0.141142989352494,0.135128888682775,
-0.190527013707433));
#83225=CARTESIAN_POINT('Ctrl Pts',(-0.132714647195745,0.143932346025504,
-0.191222246351763));
#83226=CARTESIAN_POINT('Ctrl Pts',(-0.123441357672301,0.15196323053721,
-0.191917478996092));
#83227=CARTESIAN_POINT('Ctrl Pts',(-0.113490345006027,0.15906319998797,
-0.192612711640422));
#83228=CARTESIAN_POINT('Ctrl Pts',(-0.103540706517675,0.166162188973566,
-0.193307848277101));
#83229=CARTESIAN_POINT('Ctrl Pts',(-0.0929142155251427,0.172329973771519,
-0.194002984913779));
#83230=CARTESIAN_POINT('Ctrl Pts',(-0.0818100244084474,0.177449372797678,
-0.194698121550458));
#83231=CARTESIAN_POINT('Ctrl Pts',(-0.0707064093203941,0.182568506255599,
-0.195393222127003));
#83232=CARTESIAN_POINT('Ctrl Pts',(-0.059125949223413,0.186639020139161,
-0.196088322703549));
#83233=CARTESIAN_POINT('Ctrl Pts',(-0.0472885380461972,0.189591545617027,
-0.196783423280094));
#83234=CARTESIAN_POINT('Ctrl Pts',(-0.0354240833959644,0.19255081636562,
-0.197480111867177));
#83235=CARTESIAN_POINT('Ctrl Pts',(-0.0233023698885466,0.194386851599335,
-0.19817680045426));
#83236=CARTESIAN_POINT('Ctrl Pts',(-0.0111530464764509,0.195081443387868,
-0.198873489041343));
#83237=CARTESIAN_POINT('Ctrl Pts',(-0.00738633642272806,0.195296790842567,
-0.199089486576042));
#83238=CARTESIAN_POINT('Ctrl Pts',(-0.00361698042405993,0.195402799863082,
-0.199305484110742));
#83239=CARTESIAN_POINT('Ctrl Pts',(0.000148219910908216,0.195399943784173,
-0.199521481645441));
#83240=CARTESIAN_POINT('Ctrl Pts',(0.0122926299414716,0.195390731686473,
-0.200218167716198));
#83241=CARTESIAN_POINT('Ctrl Pts',(0.0244787985054029,0.194244968897385,
-0.200914853786955));
#83242=CARTESIAN_POINT('Ctrl Pts',(0.036477190826623,0.191965034705277,
-0.201611539857711));
#83243=CARTESIAN_POINT('Ctrl Pts',(0.0484505485620488,0.1896898575845,-0.202306772296453));
#83244=CARTESIAN_POINT('Ctrl Pts',(0.0602360428669622,0.186285295386219,
-0.203002004735195));
#83245=CARTESIAN_POINT('Ctrl Pts',(0.0716098058136541,0.181805378664468,
-0.203697237173936));
#83246=CARTESIAN_POINT('Ctrl Pts',(0.0829819980891168,0.177326080601322,
-0.204392373603855));
#83247=CARTESIAN_POINT('Ctrl Pts',(0.0939417424025054,0.171772000804235,
-0.205087510033774));
#83248=CARTESIAN_POINT('Ctrl Pts',(0.104282306981401,0.165246362896848,
-0.205782646463693));
#83249=CARTESIAN_POINT('Ctrl Pts',(0.114622335131479,0.15872106351452,-0.206477746832601));
#83250=CARTESIAN_POINT('Ctrl Pts',(0.124342521798727,0.151224795917388,
-0.207172847201508));
#83251=CARTESIAN_POINT('Ctrl Pts',(0.133264942347688,0.142904216666505,
-0.207867947570416));
#83252=CARTESIAN_POINT('Ctrl Pts',(0.142207746888664,0.134564628378771,
-0.208564635952385));
#83253=CARTESIAN_POINT('Ctrl Pts',(0.150348552004181,0.12539761298159,-0.209261324334354));
#83254=CARTESIAN_POINT('Ctrl Pts',(0.157547031093136,0.115585868486327,
-0.209958012716324));
#83255=CARTESIAN_POINT('Ctrl Pts',(0.15977881961569,0.112543873298155,-0.210174011278723));
#83256=CARTESIAN_POINT('Ctrl Pts',(0.16192034282866,0.109440118121617,-0.210390009841122));
#83257=CARTESIAN_POINT('Ctrl Pts',(0.163968293874172,0.106280565504674,
-0.210606008403521));
#83258=CARTESIAN_POINT('Ctrl Pts',(0.170573795625582,0.0960896820894549,
-0.211302694432885));
#83259=CARTESIAN_POINT('Ctrl Pts',(0.176248779215107,0.085244866852711,
-0.21199938046225));
#83260=CARTESIAN_POINT('Ctrl Pts',(0.180870247225192,0.0739399328421249,
-0.212696066491614));
#83261=CARTESIAN_POINT('Ctrl Pts',(0.185482072550167,0.062658586557045,
-0.213391298886768));
#83262=CARTESIAN_POINT('Ctrl Pts',(0.189044349253176,0.0509198010178098,
-0.214086531281921));
#83263=CARTESIAN_POINT('Ctrl Pts',(0.191480487199185,0.0389407629863966,
-0.214781763677075));
#83264=CARTESIAN_POINT('Ctrl Pts',(0.193916288715316,0.0269633792563398,
-0.215476900060855));
#83265=CARTESIAN_POINT('Ctrl Pts',(0.195226041671566,0.0147466559843934,
-0.216172036444636));
#83266=CARTESIAN_POINT('Ctrl Pts',(0.195383747059877,0.00252019539758848,
-0.216867172828416));
#83267=CARTESIAN_POINT('Ctrl Pts',(0.19554144426669,-0.00970563090046064,
-0.217562273149659));
#83268=CARTESIAN_POINT('Ctrl Pts',(0.194547228318338,-0.021940318258623,
-0.218257373470902));
#83269=CARTESIAN_POINT('Ctrl Pts',(0.192427215569999,-0.0339547744503923,
-0.218952473792144));
#83270=CARTESIAN_POINT('Ctrl Pts',(0.190302359484847,-0.0459966786176576,
-0.219649162125053));
#83271=CARTESIAN_POINT('Ctrl Pts',(0.187046788337536,-0.0578164975414096,
-0.220345850457961));
#83272=CARTESIAN_POINT('Ctrl Pts',(0.18273732146997,-0.0691970472056503,
-0.221042538790869));
#83273=CARTESIAN_POINT('Ctrl Pts',(0.181401229582072,-0.0727254326309214,
-0.221258537581113));
#83274=CARTESIAN_POINT('Ctrl Pts',(0.179964183686421,-0.076211741199239,
-0.221474536371357));
#83275=CARTESIAN_POINT('Ctrl Pts',(0.178429384007929,-0.0796499524328228,
-0.221690535161602));
#83276=CARTESIAN_POINT('Ctrl Pts',(0.173479015467716,-0.0907396164221063,
-0.222387221270501));
#83277=CARTESIAN_POINT('Ctrl Pts',(0.16747346226795,-0.101404925766471,
-0.2230839073794));
#83278=CARTESIAN_POINT('Ctrl Pts',(0.160508302936004,-0.111437178215369,
-0.2237805934883));
#83279=CARTESIAN_POINT('Ctrl Pts',(0.153557676374664,-0.121448498418995,
-0.224475825965068));
#83280=CARTESIAN_POINT('Ctrl Pts',(0.145651851269864,-0.130828629795998,
-0.225171058441836));
#83281=CARTESIAN_POINT('Ctrl Pts',(0.136931281400909,-0.139395065098822,
-0.225866290918604));
#83282=CARTESIAN_POINT('Ctrl Pts',(0.128211915817396,-0.147960317401744,
-0.226561427385781));
#83283=CARTESIAN_POINT('Ctrl Pts',(0.11867862030011,-0.155711452131251,
-0.227256563852957));
#83284=CARTESIAN_POINT('Ctrl Pts',(0.108509811188828,-0.162501633455682,
-0.227951700320134));
#83285=CARTESIAN_POINT('Ctrl Pts',(0.0983415296023409,-0.169291462527557,
-0.228646800725888));
#83286=CARTESIAN_POINT('Ctrl Pts',(0.0875385425542467,-0.175119973763597,
-0.229341901131642));
#83287=CARTESIAN_POINT('Ctrl Pts',(0.076307218005659,-0.179884319717525,
-0.230037001537397));
#83288=CARTESIAN_POINT('Ctrl Pts',(0.0650502346092214,-0.184659550196018,
-0.230733689954919));
#83289=CARTESIAN_POINT('Ctrl Pts',(0.0533637905445501,-0.188365480666791,
-0.231430378372441));
#83290=CARTESIAN_POINT('Ctrl Pts',(0.0414718762791761,-0.190948274351681,
-0.232127066789963));
#83291=CARTESIAN_POINT('Ctrl Pts',(0.0377849566877756,-0.19174903295327,
-0.232343065166536));
#83292=CARTESIAN_POINT('Ctrl Pts',(0.0340783538329179,-0.192442206005216,
-0.232559063543108));
#83293=CARTESIAN_POINT('Ctrl Pts',(0.0303588599030374,-0.193027199185472,
-0.232775061919681));
#83294=CARTESIAN_POINT('Ctrl Pts',(0.0183619196136292,-0.19491404948972,
-0.233471747994509));
#83295=CARTESIAN_POINT('Ctrl Pts',(0.00614629785945884,-0.195684804064974,
-0.234168434069336));
#83296=CARTESIAN_POINT('Ctrl Pts',(-0.00606091356201013,-0.195305978727723,
-0.234865120144164));
#83297=CARTESIAN_POINT('Ctrl Pts',(-0.0182426546855573,-0.194927943808026,
-0.235560352586276));
#83298=CARTESIAN_POINT('Ctrl Pts',(-0.0304151521306216,-0.19340504300487,
-0.236255585028388));
#83299=CARTESIAN_POINT('Ctrl Pts',(-0.0423488478193519,-0.190755694773114,
-0.2369508174705));
#83300=CARTESIAN_POINT('Ctrl Pts',(-0.0542808954937715,-0.188106712409896,
-0.237645953902706));
#83301=CARTESIAN_POINT('Ctrl Pts',(-0.065973344173134,-0.184331736513773,
-0.238341090334911));
#83302=CARTESIAN_POINT('Ctrl Pts',(-0.0772058819424711,-0.179500450677666,
-0.239036226767116));
#83303=CARTESIAN_POINT('Ctrl Pts',(-0.0884378370006978,-0.174669415474497,
-0.239731327137682));
#83304=CARTESIAN_POINT('Ctrl Pts',(-0.0992091354226222,-0.168782549685527,
-0.240426427508248));
#83305=CARTESIAN_POINT('Ctrl Pts',(-0.109321138589207,-0.16195693457694,
-0.241121527878815));
#83306=CARTESIAN_POINT('Ctrl Pts',(-0.119456243431465,-0.155115725807641,
-0.241818216261475));
#83307=CARTESIAN_POINT('Ctrl Pts',(-0.128928357995219,-0.147332029574057,
-0.242514904644135));
#83308=CARTESIAN_POINT('Ctrl Pts',(-0.13757035400327,-0.138764396368143,
-0.243211593026795));
#83309=CARTESIAN_POINT('Ctrl Pts',(-0.140249684757291,-0.136108120767414,
-0.243427591577117));
#83310=CARTESIAN_POINT('Ctrl Pts',(-0.142849498779866,-0.133376750497312,
-0.243643590127439));
#83311=CARTESIAN_POINT('Ctrl Pts',(-0.145365598904999,-0.130575658738492,
-0.243859588677762));
#83312=CARTESIAN_POINT('Ctrl Pts',(-0.15340020980029,-0.121630989907819,
-0.244549332415879));
#83313=CARTESIAN_POINT('Ctrl Pts',(-0.160637251305879,-0.111907083313971,
-0.245239076153997));
#83314=CARTESIAN_POINT('Ctrl Pts',(-0.166925987723204,-0.101572016927069,
-0.245928819892114));
#83315=CARTESIAN_POINT('Ctrl Pts',(-0.173201884280739,-0.0912580518862106,
-0.246617155364358));
#83316=CARTESIAN_POINT('Ctrl Pts',(-0.178532788468517,-0.0803361179447198,
-0.247305490836601));
#83317=CARTESIAN_POINT('Ctrl Pts',(-0.182809932098231,-0.0690049905893792,
-0.247993826308844));
#83318=CARTESIAN_POINT('Ctrl Pts',(-0.187088666891204,-0.0576696478802656,
-0.248682417852478));
#83319=CARTESIAN_POINT('Ctrl Pts',(-0.190312494068741,-0.0459256273125695,
-0.249371009396111));
#83320=CARTESIAN_POINT('Ctrl Pts',(-0.19242059217681,-0.033992288924488,
-0.250059600939744));
#83321=CARTESIAN_POINT('Ctrl Pts',(-0.194414043788067,-0.0227079314525326,
-0.250710744222355));
#83322=CARTESIAN_POINT('Ctrl Pts',(-0.195410127008499,-0.0112550804263115,
-0.251361887504965));
#83323=CARTESIAN_POINT('Ctrl Pts',(-0.195399922115064,0.000174463254022285,
-0.252013030787576));
#83324=CARTESIAN_POINT('',(-0.195399991113071,-5.89322641794126E-5,-0.322013030791099));
#83325=CARTESIAN_POINT('Ctrl Pts',(-0.195399922115002,0.00017446332273629,
-0.252013030791491));
#83326=CARTESIAN_POINT('Ctrl Pts',(-0.19538611251111,0.0156412988881714,
-0.252894179362555));
#83327=CARTESIAN_POINT('Ctrl Pts',(-0.193531985236505,0.031025722314354,
-0.253775327933618));
#83328=CARTESIAN_POINT('Ctrl Pts',(-0.189918199616712,0.0459590845681982,
-0.254656476504681));
#83329=CARTESIAN_POINT('Ctrl Pts',(-0.18952497594356,0.0475840153681317,
-0.254752356148401));
#83330=CARTESIAN_POINT('Ctrl Pts',(-0.189110963346523,0.0492036272310654,
-0.254848235792121));
#83331=CARTESIAN_POINT('Ctrl Pts',(-0.188676298791606,0.0508174603291092,
-0.254944115435841));
#83332=CARTESIAN_POINT('Ctrl Pts',(-0.185517914649659,0.0625439855471211,
-0.255640801519016));
#83333=CARTESIAN_POINT('Ctrl Pts',(-0.181251035015882,0.0740160916859001,
-0.256337487602192));
#83334=CARTESIAN_POINT('Ctrl Pts',(-0.175937484489621,0.0850127140577487,
-0.257034173685368));
#83335=CARTESIAN_POINT('Ctrl Pts',(-0.17063502066475,0.0959863920220958,
-0.257729406135886));
#83336=CARTESIAN_POINT('Ctrl Pts',(-0.164290531131562,0.106485743283834,
-0.258424638586405));
#83337=CARTESIAN_POINT('Ctrl Pts',(-0.157014254994016,0.116308571174588,
-0.259119871036924));
#83338=CARTESIAN_POINT('Ctrl Pts',(-0.149738983692955,0.126130042556097,
-0.25981500747749));
#83339=CARTESIAN_POINT('Ctrl Pts',(-0.141532664824672,0.135274447027259,
-0.260510143918056));
#83340=CARTESIAN_POINT('Ctrl Pts',(-0.132548603495651,0.143568895347678,
-0.261205280358622));
#83341=CARTESIAN_POINT('Ctrl Pts',(-0.123565008233616,0.15186291337623,
-0.26190038073753));
#83342=CARTESIAN_POINT('Ctrl Pts',(-0.113804411841073,0.159306489128976,
-0.262595481116438));
#83343=CARTESIAN_POINT('Ctrl Pts',(-0.103454595656893,0.16576581866437,
-0.263290581495346));
#83344=CARTESIAN_POINT('Ctrl Pts',(-0.0930811344972744,0.172239905050078,
-0.263987269886165));
#83345=CARTESIAN_POINT('Ctrl Pts',(-0.0821165425315173,0.17772484879732,
-0.264683958276985));
#83346=CARTESIAN_POINT('Ctrl Pts',(-0.0707736589292538,0.182132504517359,
-0.265380646667805));
#83347=CARTESIAN_POINT('Ctrl Pts',(-0.067256956232909,0.183499036635534,
-0.265596645176511));
#83348=CARTESIAN_POINT('Ctrl Pts',(-0.0637040156330268,0.184762375124595,
-0.265812643685216));
#83349=CARTESIAN_POINT('Ctrl Pts',(-0.0601214532647579,0.185920872570385,
-0.266028642193922));
#83350=CARTESIAN_POINT('Ctrl Pts',(-0.048566182168939,0.189657514301592,
-0.266725328271599));
#83351=CARTESIAN_POINT('Ctrl Pts',(-0.0366206693845789,0.192325885138425,
-0.267422014349276));
#83352=CARTESIAN_POINT('Ctrl Pts',(-0.024503994786874,0.193857458560368,
-0.268118700426954));
#83353=CARTESIAN_POINT('Ctrl Pts',(-0.012412601583059,0.19538583636039,
-0.26881393287187));
#83354=CARTESIAN_POINT('Ctrl Pts',(-0.000151605633977037,0.195781942874476,
-0.269509165316787));
#83355=CARTESIAN_POINT('Ctrl Pts',(0.0120493742582722,0.195028132791103,
-0.270204397761704));
#83356=CARTESIAN_POINT('Ctrl Pts',(0.0242486692229536,0.194274426807188,
-0.270899534196601));
#83357=CARTESIAN_POINT('Ctrl Pts',(0.0363870898065443,0.192371128093905,
-0.271594670631498));
#83358=CARTESIAN_POINT('Ctrl Pts',(0.0482361466365246,0.189352671377141,
-0.272289807066396));
#83359=CARTESIAN_POINT('Ctrl Pts',(0.0600845887711323,0.186334371249329,
-0.272984907439592));
#83360=CARTESIAN_POINT('Ctrl Pts',(0.0716428557342279,0.182201270174255,
-0.273680007812788));
#83361=CARTESIAN_POINT('Ctrl Pts',(0.0826964661184239,0.177038002958473,
-0.274375108185984));
#83362=CARTESIAN_POINT('Ctrl Pts',(0.0937753293525448,0.171862939849079,
-0.275071796571132));
#83363=CARTESIAN_POINT('Ctrl Pts',(0.104346469879209,0.16565344143362,-0.27576848495628));
#83364=CARTESIAN_POINT('Ctrl Pts',(0.114220056217435,0.158540022573753,
-0.276465173341428));
#83365=CARTESIAN_POINT('Ctrl Pts',(0.117281224234673,0.156334606065393,
-0.276681171878286));
#83366=CARTESIAN_POINT('Ctrl Pts',(0.120275574076283,0.154042601749538,
-0.276897170415144));
#83367=CARTESIAN_POINT('Ctrl Pts',(0.123198121195366,0.151668661673834,
-0.277113168952002));
#83368=CARTESIAN_POINT('Ctrl Pts',(0.132624564167303,0.144011707027558,
-0.277809855029848));
#83369=CARTESIAN_POINT('Ctrl Pts',(0.141367523257338,0.135445719343915,
-0.278506541107693));
#83370=CARTESIAN_POINT('Ctrl Pts',(0.149250223522671,0.12611713118539,-0.279203227185539));
#83371=CARTESIAN_POINT('Ctrl Pts',(0.157116476564654,0.116808007089663,
-0.279898459630601));
#83372=CARTESIAN_POINT('Ctrl Pts',(0.164125417987913,0.106740054854432,
-0.280593692075663));
#83373=CARTESIAN_POINT('Ctrl Pts',(0.170137209426213,0.096096253666108,
-0.281288924520725));
#83374=CARTESIAN_POINT('Ctrl Pts',(0.176148170649486,0.0854539223630562,
-0.281984060955733));
#83375=CARTESIAN_POINT('Ctrl Pts',(0.18116178612565,0.0742366383704422,
-0.28267919739074));
#83376=CARTESIAN_POINT('Ctrl Pts',(0.185082513551193,0.0626547937317849,
-0.283374333825748));
#83377=CARTESIAN_POINT('Ctrl Pts',(0.189003037580431,0.0510735499266331,
-0.284069434199034));
#83378=CARTESIAN_POINT('Ctrl Pts',(0.191830531175522,0.0391286204697831,
-0.28476453457232));
#83379=CARTESIAN_POINT('Ctrl Pts',(0.193519184317751,0.0270459849329323,
-0.285459634945605));
#83380=CARTESIAN_POINT('Ctrl Pts',(0.195211695321984,0.0149357456571146,
-0.286156323330811));
#83381=CARTESIAN_POINT('Ctrl Pts',(0.195760115543239,0.00268804718140895,
-0.286853011716017));
#83382=CARTESIAN_POINT('Ctrl Pts',(0.195170538988722,-0.00946682158127442,
-0.287549700101223));
#83383=CARTESIAN_POINT('Ctrl Pts',(0.194987748984599,-0.0132352694515691,
-0.287765698637509));
#83384=CARTESIAN_POINT('Ctrl Pts',(0.194695949500409,-0.0169948263072403,
-0.287981697173795));
#83385=CARTESIAN_POINT('Ctrl Pts',(0.194296328011977,-0.020738778195985,
-0.288197695710081));
#83386=CARTESIAN_POINT('Ctrl Pts',(0.193007380722087,-0.0328145968898343,
-0.288894381789347));
#83387=CARTESIAN_POINT('Ctrl Pts',(0.190583810546708,-0.0448121710990928,
-0.289591067868612));
#83388=CARTESIAN_POINT('Ctrl Pts',(0.187052172057487,-0.0565034948350653,
-0.290287753947877));
#83389=CARTESIAN_POINT('Ctrl Pts',(0.18352790231797,-0.0681704246704228,
-0.290982986394401));
#83390=CARTESIAN_POINT('Ctrl Pts',(0.178900333129847,-0.0795315217171349,
-0.291678218840924));
#83391=CARTESIAN_POINT('Ctrl Pts',(0.173246785557543,-0.0903698583266489,
-0.292373451287448));
#83392=CARTESIAN_POINT('Ctrl Pts',(0.167594018727271,-0.101206698186584,
-0.293068587723955));
#83393=CARTESIAN_POINT('Ctrl Pts',(0.160915918632716,-0.111520125358314,
-0.293763724160463));
#83394=CARTESIAN_POINT('Ctrl Pts',(0.153336919679044,-0.121115436932467,
-0.29445886059697));
#83395=CARTESIAN_POINT('Ctrl Pts',(0.14575831390225,-0.130710250729187,
-0.295153960971779));
#83396=CARTESIAN_POINT('Ctrl Pts',(0.137279465614492,-0.139586353029643,
-0.295849061346588));
#83397=CARTESIAN_POINT('Ctrl Pts',(0.128064964606821,-0.147582264653493,
-0.296544161721397));
#83398=CARTESIAN_POINT('Ctrl Pts',(0.118829412340891,-0.15559644357152,
-0.297240850108134));
#83399=CARTESIAN_POINT('Ctrl Pts',(0.108855555357494,-0.162725893770916,
-0.297937538494871));
#83400=CARTESIAN_POINT('Ctrl Pts',(0.0983398621120382,-0.168850322829971,
-0.298634226881607));
#83401=CARTESIAN_POINT('Ctrl Pts',(0.09507961791375,-0.170749116741274,
-0.298850225410459));
#83402=CARTESIAN_POINT('Ctrl Pts',(0.0917674698458486,-0.172551639662424,
-0.299066223939311));
#83403=CARTESIAN_POINT('Ctrl Pts',(0.0884096957325332,-0.174255231486693,
-0.299282222468162));
#83404=CARTESIAN_POINT('Ctrl Pts',(0.0775794623433502,-0.179750031444668,
-0.299978908546569));
#83405=CARTESIAN_POINT('Ctrl Pts',(0.066196996889879,-0.184250582423813,
-0.300675594624976));
#83406=CARTESIAN_POINT('Ctrl Pts',(0.0544679948553741,-0.187654996033772,
-0.301372280703383));
#83407=CARTESIAN_POINT('Ctrl Pts',(0.0427634653374316,-0.191052306348138,
-0.302067513149031));
#83408=CARTESIAN_POINT('Ctrl Pts',(0.0307146457960079,-0.193357706528318,
-0.302762745594679));
#83409=CARTESIAN_POINT('Ctrl Pts',(0.0185455848429963,-0.194517920210019,
-0.303457978040326));
#83410=CARTESIAN_POINT('Ctrl Pts',(0.00637820440977671,-0.195677973668835,
-0.304153114475946));
#83411=CARTESIAN_POINT('Ctrl Pts',(-0.00590851907373053,-0.195693026527156,
-0.304848250911565));
#83412=CARTESIAN_POINT('Ctrl Pts',(-0.0180835219950757,-0.194561420205172,
-0.305543387347185));
#83413=CARTESIAN_POINT('Ctrl Pts',(-0.0302578933118102,-0.193429872587714,
-0.306238487721098));
#83414=CARTESIAN_POINT('Ctrl Pts',(-0.0423196868550718,-0.191151891791996,
-0.306933588095011));
#83415=CARTESIAN_POINT('Ctrl Pts',(-0.0540438381313047,-0.187777590675877,
-0.307628688468925));
#83416=CARTESIAN_POINT('Ctrl Pts',(-0.0657947741609637,-0.184395580701245,
-0.30832537685477));
#83417=CARTESIAN_POINT('Ctrl Pts',(-0.0772057058796961,-0.179912554912077,
-0.309022065240616));
#83418=CARTESIAN_POINT('Ctrl Pts',(-0.0880687538179938,-0.174427791939661,
-0.309718753626461));
#83419=CARTESIAN_POINT('Ctrl Pts',(-0.0914366905729014,-0.17272731755055,
-0.309934752159721));
#83420=CARTESIAN_POINT('Ctrl Pts',(-0.0947521462737708,-0.170930885591786,
-0.310150750692981));
#83421=CARTESIAN_POINT('Ctrl Pts',(-0.0980094712277496,-0.169042312897265,
-0.310366749226242));
#83422=CARTESIAN_POINT('Ctrl Pts',(-0.108515713628368,-0.162950871975601,
-0.311063435304748));
#83423=CARTESIAN_POINT('Ctrl Pts',(-0.118488768195282,-0.155854840580449,
-0.311760121383255));
#83424=CARTESIAN_POINT('Ctrl Pts',(-0.127731166881062,-0.147871258218771,
-0.312456807461761));
#83425=CARTESIAN_POINT('Ctrl Pts',(-0.136954281338361,-0.139904333570267,
-0.313152039907507));
#83426=CARTESIAN_POINT('Ctrl Pts',(-0.145449062057614,-0.131054044145402,
-0.313847272353253));
#83427=CARTESIAN_POINT('Ctrl Pts',(-0.153048819121446,-0.12147929439016,
-0.314542504798999));
#83428=CARTESIAN_POINT('Ctrl Pts',(-0.160647526675976,-0.111905866886252,
-0.315237641234713));
#83429=CARTESIAN_POINT('Ctrl Pts',(-0.167350877291185,-0.101608833764162,
-0.315932777670427));
#83430=CARTESIAN_POINT('Ctrl Pts',(-0.173031654364707,-0.0907810915764546,
-0.316627914106141));
#83431=CARTESIAN_POINT('Ctrl Pts',(-0.178712136735613,-0.0799539111013252,
-0.317323014480146));
#83432=CARTESIAN_POINT('Ctrl Pts',(-0.183369768325558,-0.0685968635977168,
-0.318018114854152));
#83433=CARTESIAN_POINT('Ctrl Pts',(-0.186924021548781,-0.056926006078336,
-0.318713215228158));
#83434=CARTESIAN_POINT('Ctrl Pts',(-0.190486394745354,-0.0452284855594271,
-0.319409903614091));
#83435=CARTESIAN_POINT('Ctrl Pts',(-0.192940165079464,-0.0332165792117047,
-0.320106592000024));
#83436=CARTESIAN_POINT('Ctrl Pts',(-0.194255399811661,-0.0211187036536718,
-0.320803280385958));
#83437=CARTESIAN_POINT('Ctrl Pts',(-0.194663170025953,-0.0173679257978144,
-0.321019278918746));
#83438=CARTESIAN_POINT('Ctrl Pts',(-0.194961879337744,-0.0136089117019791,
-0.321235277451534));
#83439=CARTESIAN_POINT('Ctrl Pts',(-0.19515165250027,-0.0098484783806397,
-0.321451275984323));
#83440=CARTESIAN_POINT('Ctrl Pts',(-0.195316169027614,-0.00658851568041518,
-0.321638527585407));
#83441=CARTESIAN_POINT('Ctrl Pts',(-0.19539900625428,-0.00332439645530177,
-0.321825779186492));
#83442=CARTESIAN_POINT('Ctrl Pts',(-0.195399991113052,-5.89323256041572E-5,
-0.322013030787577));
#83443=CARTESIAN_POINT('',(-0.195399958457515,-0.000127415860640841,-0.392013030782495));
#83444=CARTESIAN_POINT('Ctrl Pts',(-0.195399991113071,-5.89322641801936E-5,
-0.322013030791099));
#83445=CARTESIAN_POINT('Ctrl Pts',(-0.195403626754625,0.0119956584972156,
-0.322704277526881));
#83446=CARTESIAN_POINT('Ctrl Pts',(-0.194287443259356,0.0240951078562085,
-0.323395524262662));
#83447=CARTESIAN_POINT('Ctrl Pts',(-0.192052701434784,0.0360127737282426,
-0.324086770998444));
#83448=CARTESIAN_POINT('Ctrl Pts',(-0.189776451431471,0.0481517987746372,
-0.324790856977107));
#83449=CARTESIAN_POINT('Ctrl Pts',(-0.186339582668901,0.0601012590536241,
-0.32549494295577));
#83450=CARTESIAN_POINT('Ctrl Pts',(-0.181798927369129,0.0716261824156088,
-0.326199028934434));
#83451=CARTESIAN_POINT('Ctrl Pts',(-0.177350367924567,0.0829173514837377,
-0.326888834287049));
#83452=CARTESIAN_POINT('Ctrl Pts',(-0.171842810096671,0.0938002223460869,
-0.327578639639665));
#83453=CARTESIAN_POINT('Ctrl Pts',(-0.165379301193847,0.104071354063618,
-0.328268444992281));
#83454=CARTESIAN_POINT('Ctrl Pts',(-0.158715077074959,0.114661441390694,
-0.328979671283968));
#83455=CARTESIAN_POINT('Ctrl Pts',(-0.151034936542069,0.124600231003395,
-0.329690897575655));
#83456=CARTESIAN_POINT('Ctrl Pts',(-0.14249967734951,0.133697426883562,
-0.330402123867342));
#83457=CARTESIAN_POINT('Ctrl Pts',(-0.133964418156952,0.142794622763729,
-0.331113350159029));
#83458=CARTESIAN_POINT('Ctrl Pts',(-0.124574843318938,0.151049580247938,
-0.331824576450716));
#83459=CARTESIAN_POINT('Ctrl Pts',(-0.114529878220969,0.15831635100232,
-0.332535802742403));
#83460=CARTESIAN_POINT('Ctrl Pts',(-0.104690271017,0.165434560888274,-0.333232488820959));
#83461=CARTESIAN_POINT('Ctrl Pts',(-0.0941499836913328,0.171656925557161,
-0.333929174899515));
#83462=CARTESIAN_POINT('Ctrl Pts',(-0.0830962830901262,0.176850693344995,
-0.334625860978071));
#83463=CARTESIAN_POINT('Ctrl Pts',(-0.0720656459916771,0.182033624356801,
-0.335321093423868));
#83464=CARTESIAN_POINT('Ctrl Pts',(-0.0605244745726656,0.186191783164639,
-0.336016325869666));
#83465=CARTESIAN_POINT('Ctrl Pts',(-0.048685752938174,0.189237568840976,
-0.336711558315464));
#83466=CARTESIAN_POINT('Ctrl Pts',(-0.0368486662043658,0.192282933901199,
-0.337406694751233));
#83467=CARTESIAN_POINT('Ctrl Pts',(-0.0247149456230209,0.194215969199016,
-0.338101831187002));
#83468=CARTESIAN_POINT('Ctrl Pts',(-0.0125125627019548,0.194998963521937,
-0.338796967622772));
#83469=CARTESIAN_POINT('Ctrl Pts',(-0.000310812805895387,0.195781917225334,
-0.339492067996835));
#83470=CARTESIAN_POINT('Ctrl Pts',(0.0119587174464459,0.195414919359468,
-0.340187168370898));
#83471=CARTESIAN_POINT('Ctrl Pts',(0.0240658997042646,0.193912331921991,
-0.340882268744961));
#83472=CARTESIAN_POINT('Ctrl Pts',(0.0362007417801083,0.19240631170435,
-0.341578957130953));
#83473=CARTESIAN_POINT('Ctrl Pts',(0.0481716358262746,0.189759695239158,
-0.342275645516946));
#83474=CARTESIAN_POINT('Ctrl Pts',(0.0597577521874501,0.186038090329651,
-0.342972333902938));
#83475=CARTESIAN_POINT('Ctrl Pts',(0.0633498662256263,0.18488425855175,
-0.343188332435453));
#83476=CARTESIAN_POINT('Ctrl Pts',(0.0669051233157821,0.183627452595414,
-0.343404330967968));
#83477=CARTESIAN_POINT('Ctrl Pts',(0.0704173471656434,0.182270560481262,
-0.343620329500482));
#83478=CARTESIAN_POINT('Ctrl Pts',(0.0817457457087745,0.177894012941515,
-0.344317015579063));
#83479=CARTESIAN_POINT('Ctrl Pts',(0.0927043277675154,0.172441952940687,
-0.345013701657644));
#83480=CARTESIAN_POINT('Ctrl Pts',(0.10307977467419,0.165999156784359,-0.345710387736224));
#83481=CARTESIAN_POINT('Ctrl Pts',(0.113433573251774,0.159569803496826,
-0.346405620182047));
#83482=CARTESIAN_POINT('Ctrl Pts',(0.12320587681191,0.152154211441365,-0.34710085262787));
#83483=CARTESIAN_POINT('Ctrl Pts',(0.132207231602128,0.143883313529059,
-0.347796085073693));
#83484=CARTESIAN_POINT('Ctrl Pts',(0.141207343325602,0.135613557809052,
-0.348491221509487));
#83485=CARTESIAN_POINT('Ctrl Pts',(0.149436043646649,0.126489288433088,
-0.349186357945281));
#83486=CARTESIAN_POINT('Ctrl Pts',(0.156737561380853,0.116681176084163,
-0.349881494381075));
#83487=CARTESIAN_POINT('Ctrl Pts',(0.164038700333029,0.106873572552284,
-0.350576594755162));
#83488=CARTESIAN_POINT('Ctrl Pts',(0.170412251402083,0.0963829144782153,
-0.35127169512925));
#83489=CARTESIAN_POINT('Ctrl Pts',(0.175744944203048,0.0854100379760329,
-0.351966795503338));
#83490=CARTESIAN_POINT('Ctrl Pts',(0.181089819963621,0.0744120930672893,
-0.352663483889354));
#83491=CARTESIAN_POINT('Ctrl Pts',(0.185388766914424,0.0629305453448282,
-0.353360172275371));
#83492=CARTESIAN_POINT('Ctrl Pts',(0.188576559606052,0.0511863377000667,
-0.354056860661387));
#83493=CARTESIAN_POINT('Ctrl Pts',(0.189564890338673,0.0475452096630725,
-0.354272859193779));
#83494=CARTESIAN_POINT('Ctrl Pts',(0.190446783230149,0.0438789201081062,
-0.35448885772617));
#83495=CARTESIAN_POINT('Ctrl Pts',(0.191221297251884,0.0401942219393102,
-0.354704856258562));
#83496=CARTESIAN_POINT('Ctrl Pts',(0.193719430598673,0.0283095211979321,
-0.355401542337165));
#83497=CARTESIAN_POINT('Ctrl Pts',(0.195114117287976,0.0161493267899574,
-0.356098228415768));
#83498=CARTESIAN_POINT('Ctrl Pts',(0.195360299149651,0.00393872011683205,
-0.35679491449437));
#83499=CARTESIAN_POINT('Ctrl Pts',(0.195605967353843,-0.00824640917358917,
-0.357490146940215));
#83500=CARTESIAN_POINT('Ctrl Pts',(0.194707795953346,-0.0204808773087043,
-0.35818537938606));
#83501=CARTESIAN_POINT('Ctrl Pts',(0.192672435277541,-0.0325344845390488,
-0.358880611831906));
#83502=CARTESIAN_POINT('Ctrl Pts',(0.190637355680441,-0.0445864271935094,
-0.359575748267723));
#83503=CARTESIAN_POINT('Ctrl Pts',(0.187465499323653,-0.0564566895275863,
-0.360270884703541));
#83504=CARTESIAN_POINT('Ctrl Pts',(0.183215187569739,-0.0679216831636653,
-0.360966021139358));
#83505=CARTESIAN_POINT('Ctrl Pts',(0.17896509630994,-0.0793860820284035,
-0.36166112151347));
#83506=CARTESIAN_POINT('Ctrl Pts',(0.17363699022893,-0.0904444429220991,
-0.362356221887581));
#83507=CARTESIAN_POINT('Ctrl Pts',(0.167337635084274,-0.10089239755503,
-0.363051322261693));
#83508=CARTESIAN_POINT('Ctrl Pts',(0.161023888563226,-0.111364221368887,
-0.363748010647733));
#83509=CARTESIAN_POINT('Ctrl Pts',(0.153734970694931,-0.121222139978164,
-0.364444699033774));
#83510=CARTESIAN_POINT('Ctrl Pts',(0.145620674203163,-0.130291132640009,
-0.365141387419814));
#83511=CARTESIAN_POINT('Ctrl Pts',(0.143104949572476,-0.133102847523494,
-0.36535738595209));
#83512=CARTESIAN_POINT('Ctrl Pts',(0.140510160609027,-0.135838991597314,
-0.365573384484366));
#83513=CARTESIAN_POINT('Ctrl Pts',(0.137841458732347,-0.138495098305097,
-0.365789383016642));
#83514=CARTESIAN_POINT('Ctrl Pts',(0.129233773181065,-0.147062159141318,
-0.366486069095226));
#83515=CARTESIAN_POINT('Ctrl Pts',(0.119794142142335,-0.154853747223658,
-0.367182755173809));
#83516=CARTESIAN_POINT('Ctrl Pts',(0.109686811503521,-0.161709503067046,
-0.367879441252392));
#83517=CARTESIAN_POINT('Ctrl Pts',(0.0996005697702513,-0.168550954402887,
-0.368574673698218));
#83518=CARTESIAN_POINT('Ctrl Pts',(0.088850069189045,-0.174459901826862,
-0.369269906144044));
#83519=CARTESIAN_POINT('Ctrl Pts',(0.0776320063753439,-0.17931656807484,
-0.36996513858987));
#83520=CARTESIAN_POINT('Ctrl Pts',(0.0664154927507509,-0.18417256362819,
-0.370660275025667));
#83521=CARTESIAN_POINT('Ctrl Pts',(0.054732328796273,-0.187976177782212,
-0.371355411461464));
#83522=CARTESIAN_POINT('Ctrl Pts',(0.0428018033980549,-0.190654571479087,
-0.372050547897261));
#83523=CARTESIAN_POINT('Ctrl Pts',(0.0308718969216478,-0.193332826228496,
-0.372745648271352));
#83524=CARTESIAN_POINT('Ctrl Pts',(0.0186955141282983,-0.194885811137499,
-0.373440748645443));
#83525=CARTESIAN_POINT('Ctrl Pts',(0.00650220381703275,-0.195291785146026,
-0.374135849019534));
#83526=CARTESIAN_POINT('Ctrl Pts',(-0.00571896307862414,-0.195698686634372,
-0.374832537405554));
#83527=CARTESIAN_POINT('Ctrl Pts',(-0.0179562587032461,-0.19495338214258,
-0.375529225791574));
#83528=CARTESIAN_POINT('Ctrl Pts',(-0.0299813185939873,-0.193086199753804,
-0.376225914177595));
#83529=CARTESIAN_POINT('Ctrl Pts',(-0.0337095209585613,-0.192507305855547,
-0.376441912709971));
#83530=CARTESIAN_POINT('Ctrl Pts',(-0.0374173943191617,-0.191820946392533,
-0.376657911242346));
#83531=CARTESIAN_POINT('Ctrl Pts',(-0.0410983872444957,-0.19102900974957,
-0.376873909774722));
#83532=CARTESIAN_POINT('Ctrl Pts',(-0.0529711370185562,-0.188474681124243,
-0.377570595853311));
#83533=CARTESIAN_POINT('Ctrl Pts',(-0.0646465106214749,-0.184800292708903,
-0.378267281931899));
#83534=CARTESIAN_POINT('Ctrl Pts',(-0.0759005699525302,-0.180056278648874,
-0.378963968010487));
#83535=CARTESIAN_POINT('Ctrl Pts',(-0.0871311477331368,-0.175322162955489,
-0.379659200456318));
#83536=CARTESIAN_POINT('Ctrl Pts',(-0.0979413291472134,-0.169523119913525,
-0.380354432902149));
#83537=CARTESIAN_POINT('Ctrl Pts',(-0.108123542558037,-0.162758900047587,
-0.38104966534798));
#83538=CARTESIAN_POINT('Ctrl Pts',(-0.118304349828217,-0.155995614305113,
-0.381744801783782));
#83539=CARTESIAN_POINT('Ctrl Pts',(-0.127856608459109,-0.148267862001208,
-0.382439938219584));
#83540=CARTESIAN_POINT('Ctrl Pts',(-0.136599812641646,-0.13971990261329,
-0.383135074655386));
#83541=CARTESIAN_POINT('Ctrl Pts',(-0.145342563251557,-0.131172386669253,
-0.383830175029483));
#83542=CARTESIAN_POINT('Ctrl Pts',(-0.153275735998863,-0.121805379131019,
-0.384525275403579));
#83543=CARTESIAN_POINT('Ctrl Pts',(-0.160256095414963,-0.111799570134908,
-0.385220375777675));
#83544=CARTESIAN_POINT('Ctrl Pts',(-0.16725240201572,-0.101770902074644,
-0.3859170641637));
#83545=CARTESIAN_POINT('Ctrl Pts',(-0.173291103041914,-0.0911012735474523,
-0.386613752549726));
#83546=CARTESIAN_POINT('Ctrl Pts',(-0.178273279849769,-0.0799987355625439,
-0.387310440935751));
#83547=CARTESIAN_POINT('Ctrl Pts',(-0.179817934389725,-0.0765565482687536,
-0.387526439468101));
#83548=CARTESIAN_POINT('Ctrl Pts',(-0.181261384311482,-0.0730728912117539,
-0.387742438000452));
#83549=CARTESIAN_POINT('Ctrl Pts',(-0.182601645881345,-0.0695542875847618,
-0.387958436532803));
#83550=CARTESIAN_POINT('Ctrl Pts',(-0.187506976567928,-0.056676268298449,
-0.388748986864783));
#83551=CARTESIAN_POINT('Ctrl Pts',(-0.191054998852211,-0.0432541867438378,
-0.389539537196764));
#83552=CARTESIAN_POINT('Ctrl Pts',(-0.193150344420641,-0.0295652574855622,
-0.390330087528744));
#83553=CARTESIAN_POINT('Ctrl Pts',(-0.194637219047094,-0.0198514795369075,
-0.390891068613328));
#83554=CARTESIAN_POINT('Ctrl Pts',(-0.195393518260447,-0.010003849086555,
-0.391452049697911));
#83555=CARTESIAN_POINT('Ctrl Pts',(-0.195399958457515,-0.000127415860641863,
-0.392013030782495));
#83556=CARTESIAN_POINT('',(-0.195399937376808,0.000156438931572747,-0.462013030791968));
#83557=CARTESIAN_POINT('Ctrl Pts',(-0.195399958457573,-0.000127415771186929,
-0.392013030787576));
#83558=CARTESIAN_POINT('Ctrl Pts',(-0.195407982922204,0.0121785965931462,
-0.392712011887839));
#83559=CARTESIAN_POINT('Ctrl Pts',(-0.194249139815125,0.0244910033759845,
-0.393410992988102));
#83560=CARTESIAN_POINT('Ctrl Pts',(-0.191946026930775,0.0365770795101272,
-0.394109974088365));
#83561=CARTESIAN_POINT('Ctrl Pts',(-0.189642503287119,0.0486653111913485,
-0.394809079851642));
#83562=CARTESIAN_POINT('Ctrl Pts',(-0.1861945007376,0.0605262928072483,
-0.395508185614918));
#83563=CARTESIAN_POINT('Ctrl Pts',(-0.181675493516228,0.0719386895601725,
-0.396207291378194));
#83564=CARTESIAN_POINT('Ctrl Pts',(-0.177144780405295,0.0833806486150532,
-0.396908208082337));
#83565=CARTESIAN_POINT('Ctrl Pts',(-0.171537904050401,0.0943709278614005,
-0.397609124786481));
#83566=CARTESIAN_POINT('Ctrl Pts',(-0.164975564812825,0.104710185821101,
-0.398310041490624));
#83567=CARTESIAN_POINT('Ctrl Pts',(-0.162688235729128,0.108313974741315,
-0.398554348757377));
#83568=CARTESIAN_POINT('Ctrl Pts',(-0.160285211847533,0.111838934565166,
-0.39879865602413));
#83569=CARTESIAN_POINT('Ctrl Pts',(-0.157772770271872,0.115277547513551,
-0.399042963290883));
#83570=CARTESIAN_POINT('Ctrl Pts',(-0.150608091577316,0.125083370331001,
-0.39973964936947));
#83571=CARTESIAN_POINT('Ctrl Pts',(-0.142500603725442,0.134253109679862,
-0.400436335448058));
#83572=CARTESIAN_POINT('Ctrl Pts',(-0.133587503863308,0.142602730729712,
-0.401133021526646));
#83573=CARTESIAN_POINT('Ctrl Pts',(-0.12469300114891,0.150934930328147,
-0.401828253972477));
#83574=CARTESIAN_POINT('Ctrl Pts',(-0.114996804596432,0.158449761984512,
-0.402523486418308));
#83575=CARTESIAN_POINT('Ctrl Pts',(-0.10467449976499,0.164998209381039,
-0.403218718864138));
#83576=CARTESIAN_POINT('Ctrl Pts',(-0.0943536204205046,0.171545752451788,
-0.40391385529994));
#83577=CARTESIAN_POINT('Ctrl Pts',(-0.0834075178718574,0.177126669904706,
-0.404608991735742));
#83578=CARTESIAN_POINT('Ctrl Pts',(-0.0720414207893906,0.181634781059812,
-0.405304128171544));
#83579=CARTESIAN_POINT('Ctrl Pts',(-0.0606759133477934,0.186142658346902,
-0.40599922854564));
#83580=CARTESIAN_POINT('Ctrl Pts',(-0.0488912779366786,0.189577542375047,
-0.406694328919736));
#83581=CARTESIAN_POINT('Ctrl Pts',(-0.0369108546065943,0.191882122179767,
-0.407389429293832));
#83582=CARTESIAN_POINT('Ctrl Pts',(-0.0249030610493165,0.194191966979812,
-0.408086117679857));
#83583=CARTESIAN_POINT('Ctrl Pts',(-0.0126994575272143,0.195366251471346,
-0.408782806065882));
#83584=CARTESIAN_POINT('Ctrl Pts',(-0.000530343157295054,0.195399280285613,
-0.409479494451907));
#83585=CARTESIAN_POINT('Ctrl Pts',(0.00324252129208505,0.195409520409534,
-0.409695492984259));
#83586=CARTESIAN_POINT('Ctrl Pts',(0.00701208320713229,0.195310438946965,
-0.409911491516611));
#83587=CARTESIAN_POINT('Ctrl Pts',(0.0107715766774621,0.19510287833828,
-0.410127490048963));
#83588=CARTESIAN_POINT('Ctrl Pts',(0.022897523714242,0.194433408111054,
-0.410824176127552));
#83589=CARTESIAN_POINT('Ctrl Pts',(0.0350033751244801,0.192626797852022,
-0.411520862206141));
#83590=CARTESIAN_POINT('Ctrl Pts',(0.046860064980641,0.189697902755961,
-0.41221754828473));
#83591=CARTESIAN_POINT('Ctrl Pts',(0.0586920159001438,0.186775118787975,
-0.412912780730562));
#83592=CARTESIAN_POINT('Ctrl Pts',(0.0702749784319402,0.182734833971876,
-0.413608013176394));
#83593=CARTESIAN_POINT('Ctrl Pts',(0.0813883533085182,0.177643170276056,
-0.414303245622225));
#83594=CARTESIAN_POINT('Ctrl Pts',(0.0925001934531584,0.172552209727478,
-0.414998382058028));
#83595=CARTESIAN_POINT('Ctrl Pts',(0.103141761541885,0.166410481205699,
-0.415693518493831));
#83596=CARTESIAN_POINT('Ctrl Pts',(0.113112243662521,0.159332295325306,
-0.416388654929634));
#83597=CARTESIAN_POINT('Ctrl Pts',(0.123082208542832,0.152254476641114,
-0.417083755303731));
#83598=CARTESIAN_POINT('Ctrl Pts',(0.132380458758455,0.144240825601304,
-0.417778855677828));
#83599=CARTESIAN_POINT('Ctrl Pts',(0.140837306302754,0.135447455322661,
-0.418473956051925));
#83600=CARTESIAN_POINT('Ctrl Pts',(0.149313474185928,0.126633995892269,
-0.419170644437951));
#83601=CARTESIAN_POINT('Ctrl Pts',(0.156943842972338,0.11703793653566,-0.419867332823977));
#83602=CARTESIAN_POINT('Ctrl Pts',(0.163598226593451,0.106849334370776,
-0.420564021210002));
#83603=CARTESIAN_POINT('Ctrl Pts',(0.165661325569498,0.103690500151024,
-0.420780019742349));
#83604=CARTESIAN_POINT('Ctrl Pts',(0.16763093497854,0.10047490488067,-0.420996018274696));
#83605=CARTESIAN_POINT('Ctrl Pts',(0.169504077028634,0.0972086820745506,
-0.421212016807043));
#83606=CARTESIAN_POINT('Ctrl Pts',(0.175545747661026,0.086673740314212,
-0.421908702885632));
#83607=CARTESIAN_POINT('Ctrl Pts',(0.180622723021697,0.0755364246510001,
-0.422605388964221));
#83608=CARTESIAN_POINT('Ctrl Pts',(0.184622724926109,0.0639969486839681,
-0.42330207504281));
#83609=CARTESIAN_POINT('Ctrl Pts',(0.188614380842308,0.0524815497880715,
-0.423997307488642));
#83610=CARTESIAN_POINT('Ctrl Pts',(0.191533170069643,0.0405664504660143,
-0.424692539934473));
#83611=CARTESIAN_POINT('Ctrl Pts',(0.193314423861388,0.028472680364513,
-0.425387772380304));
#83612=CARTESIAN_POINT('Ctrl Pts',(0.195095431666012,0.016380580385307,
-0.426082908816108));
#83613=CARTESIAN_POINT('Ctrl Pts',(0.195739043730156,0.00411071632195411,
-0.426778045251911));
#83614=CARTESIAN_POINT('Ctrl Pts',(0.195231782616843,-0.00810623563990015,
-0.427473181687714));
#83615=CARTESIAN_POINT('Ctrl Pts',(0.194724547818799,-0.0203225538209459,
-0.428168282061811));
#83616=CARTESIAN_POINT('Ctrl Pts',(0.193066621695153,-0.0324850922496084,
-0.428863382435908));
#83617=CARTESIAN_POINT('Ctrl Pts',(0.190296537362577,-0.0443665174181312,
-0.429558482810005));
#83618=CARTESIAN_POINT('Ctrl Pts',(0.187520124552663,-0.0562750866447022,
-0.430255171196031));
#83619=CARTESIAN_POINT('Ctrl Pts',(0.18362674334812,-0.0679004238780226,
-0.430951859582057));
#83620=CARTESIAN_POINT('Ctrl Pts',(0.178704907429044,-0.0790298428492471,
-0.431648547968084));
#83621=CARTESIAN_POINT('Ctrl Pts',(0.177178960741411,-0.082480364218438,
-0.43186454650043));
#83622=CARTESIAN_POINT('Ctrl Pts',(0.175554497251728,-0.0858833823696525,
-0.432080545032776));
#83623=CARTESIAN_POINT('Ctrl Pts',(0.173835039761986,-0.089233059742164,
-0.432296543565122));
#83624=CARTESIAN_POINT('Ctrl Pts',(0.168289066449964,-0.10003717756576,
-0.432993229643711));
#83625=CARTESIAN_POINT('Ctrl Pts',(0.161712540702625,-0.11036019980197,
-0.4336899157223));
#83626=CARTESIAN_POINT('Ctrl Pts',(0.15421224645812,-0.119998929338307,
-0.434386601800889));
#83627=CARTESIAN_POINT('Ctrl Pts',(0.146727601547996,-0.129617547703455,
-0.43508183424672));
#83628=CARTESIAN_POINT('Ctrl Pts',(0.138323487648071,-0.138553978308862,
-0.435777066692552));
#83629=CARTESIAN_POINT('Ctrl Pts',(0.129150073398274,-0.14663362009178,
-0.436472299138383));
#83630=CARTESIAN_POINT('Ctrl Pts',(0.119977925976243,-0.154712146094437,
-0.437167435574186));
#83631=CARTESIAN_POINT('Ctrl Pts',(0.110037314746755,-0.161933506700741,
-0.437862572009989));
#83632=CARTESIAN_POINT('Ctrl Pts',(0.0995143753671538,-0.168160783464175,
-0.438557708445792));
#83633=CARTESIAN_POINT('Ctrl Pts',(0.0889919818877899,-0.174387737174161,
-0.439252808819889));
#83634=CARTESIAN_POINT('Ctrl Pts',(0.07788808700947,-0.179620287087094,
-0.439947909193986));
#83635=CARTESIAN_POINT('Ctrl Pts',(0.0664143450939421,-0.183766957763747,
-0.440643009568083));
#83636=CARTESIAN_POINT('Ctrl Pts',(0.0549143905050947,-0.187923101838409,
-0.441339697954108));
#83637=CARTESIAN_POINT('Ctrl Pts',(0.0430437465390059,-0.190988178480599,
-0.442036386340134));
#83638=CARTESIAN_POINT('Ctrl Pts',(0.0310289993702008,-0.192920608536476,
-0.44273307472616));
#83639=CARTESIAN_POINT('Ctrl Pts',(0.027303994321965,-0.193519731565231,
-0.442949073258508));
#83640=CARTESIAN_POINT('Ctrl Pts',(0.0235651843507864,-0.194010357865431,
-0.443165071790856));
#83641=CARTESIAN_POINT('Ctrl Pts',(0.0198193839265638,-0.194392263273957,
-0.443381070323204));
#83642=CARTESIAN_POINT('Ctrl Pts',(0.00773760272017369,-0.195624068780068,
-0.444077756401793));
#83643=CARTESIAN_POINT('Ctrl Pts',(-0.00450185620683019,-0.195729539956344,
-0.444774442480382));
#83644=CARTESIAN_POINT('Ctrl Pts',(-0.0166704164553885,-0.194687588754918,
-0.445471128558971));
#83645=CARTESIAN_POINT('Ctrl Pts',(-0.0288135870509505,-0.193647811580566,
-0.446166361004803));
#83646=CARTESIAN_POINT('Ctrl Pts',(-0.0408852831489385,-0.191465364393067,
-0.446861593450635));
#83647=CARTESIAN_POINT('Ctrl Pts',(-0.0526572875794893,-0.188171119103785,
-0.447556825896467));
#83648=CARTESIAN_POINT('Ctrl Pts',(-0.0644276663228442,-0.18487732874233,
-0.44825196233227));
#83649=CARTESIAN_POINT('Ctrl Pts',(-0.0758975820168812,-0.180472236848403,
-0.448947098768073));
#83650=CARTESIAN_POINT('Ctrl Pts',(-0.0868508371809369,-0.175037401948756,
-0.449642235203876));
#83651=CARTESIAN_POINT('Ctrl Pts',(-0.0978035241211859,-0.169602848992926,
-0.450337335577973));
#83652=CARTESIAN_POINT('Ctrl Pts',(-0.108238831969957,-0.163139072220679,
-0.45103243595207));
#83653=CARTESIAN_POINT('Ctrl Pts',(-0.117964781420494,-0.155773779386696,
-0.451727536326167));
#83654=CARTESIAN_POINT('Ctrl Pts',(-0.127712950573862,-0.148391659957133,
-0.452424224712193));
#83655=CARTESIAN_POINT('Ctrl Pts',(-0.136747868534464,-0.140104492742853,
-0.453120913098219));
#83656=CARTESIAN_POINT('Ctrl Pts',(-0.144911274345799,-0.13107968022343,
-0.453817601484244));
#83657=CARTESIAN_POINT('Ctrl Pts',(-0.147442224638013,-0.1282816627769,
-0.454033600016591));
#83658=CARTESIAN_POINT('Ctrl Pts',(-0.149889693047452,-0.125412984936567,
-0.454249598548937));
#83659=CARTESIAN_POINT('Ctrl Pts',(-0.152249780747947,-0.122479240127468,
-0.454465597081283));
#83660=CARTESIAN_POINT('Ctrl Pts',(-0.159839932411845,-0.113044180557622,
-0.455160258393802));
#83661=CARTESIAN_POINT('Ctrl Pts',(-0.166577789997525,-0.102865895547722,
-0.455854919706322));
#83662=CARTESIAN_POINT('Ctrl Pts',(-0.172320935541128,-0.092123043665689,
-0.456549581018841));
#83663=CARTESIAN_POINT('Ctrl Pts',(-0.178051864918719,-0.0814030427563561,
-0.457242764726823));
#83664=CARTESIAN_POINT('Ctrl Pts',(-0.182791800687757,-0.0701215888384119,
-0.457935948434805));
#83665=CARTESIAN_POINT('Ctrl Pts',(-0.186441932507934,-0.0584856033798669,
-0.458629132142786));
#83666=CARTESIAN_POINT('Ctrl Pts',(-0.190090870931465,-0.0468534222622858,
-0.459322089217005));
#83667=CARTESIAN_POINT('Ctrl Pts',(-0.192650406516594,-0.034867764431544,
-0.460015046291223));
#83668=CARTESIAN_POINT('Ctrl Pts',(-0.194070739924089,-0.0227531954968199,
-0.460708003365442));
#83669=CARTESIAN_POINT('Ctrl Pts',(-0.194962365160494,-0.0151481815378657,
-0.461143012506153));
#83670=CARTESIAN_POINT('Ctrl Pts',(-0.195406061327982,-0.00749268174718338,
-0.461578021646865));
#83671=CARTESIAN_POINT('Ctrl Pts',(-0.19539993737687,0.00015643885435388,
-0.462013030787577));
#83672=CARTESIAN_POINT('',(-0.195399999942242,4.75099905391278E-6,-0.532013030784479));
#83673=CARTESIAN_POINT('Ctrl Pts',(-0.195399937376808,0.000156438931571927,
-0.462013030791968));
#83674=CARTESIAN_POINT('Ctrl Pts',(-0.195388329591929,0.0146551344658182,
-0.462837578529473));
#83675=CARTESIAN_POINT('Ctrl Pts',(-0.193758956620724,0.0290846302221516,
-0.463662126266977));
#83676=CARTESIAN_POINT('Ctrl Pts',(-0.190581249380799,0.0431271073045003,
-0.464486674004482));
#83677=CARTESIAN_POINT('Ctrl Pts',(-0.189215113705894,0.0491641420146828,
-0.464841157282775));
#83678=CARTESIAN_POINT('Ctrl Pts',(-0.187563420811457,0.0551299029508943,
-0.465195640561069));
#83679=CARTESIAN_POINT('Ctrl Pts',(-0.185634374162934,0.0610003207297784,
-0.465550123839363));
#83680=CARTESIAN_POINT('Ctrl Pts',(-0.181843109448154,0.0725377855200353,
-0.466246809917952));
#83681=CARTESIAN_POINT('Ctrl Pts',(-0.176958821129432,0.0837609404514446,
-0.466943495996541));
#83682=CARTESIAN_POINT('Ctrl Pts',(-0.171055261286761,0.0944524091070096,
-0.46764018207513));
#83683=CARTESIAN_POINT('Ctrl Pts',(-0.165164019198436,0.105121570055359,
-0.468335414520962));
#83684=CARTESIAN_POINT('Ctrl Pts',(-0.158258080992425,0.115260452632001,
-0.469030646966793));
#83685=CARTESIAN_POINT('Ctrl Pts',(-0.150458515822565,0.124673152749383,
-0.469725879412625));
#83686=CARTESIAN_POINT('Ctrl Pts',(-0.142660027755015,0.134084552994167,
-0.470421015848428));
#83687=CARTESIAN_POINT('Ctrl Pts',(-0.133968680219217,0.14276926822463,
-0.471116152284231));
#83688=CARTESIAN_POINT('Ctrl Pts',(-0.124546951277911,0.150562999861777,
-0.471811288720034));
#83689=CARTESIAN_POINT('Ctrl Pts',(-0.11512571110917,0.158356327182241,
-0.472506389094131));
#83690=CARTESIAN_POINT('Ctrl Pts',(-0.104974856198617,0.165258225808353,
-0.473201489468229));
#83691=CARTESIAN_POINT('Ctrl Pts',(-0.0942891648455739,0.171145299066975,
-0.473896589842326));
#83692=CARTESIAN_POINT('Ctrl Pts',(-0.0835790611832178,0.177045821811324,
-0.474593278228352));
#83693=CARTESIAN_POINT('Ctrl Pts',(-0.0723324791007605,0.181926526110376,
-0.475289966614378));
#83694=CARTESIAN_POINT('Ctrl Pts',(-0.0607667352856288,0.185710968665629,
-0.475986655000404));
#83695=CARTESIAN_POINT('Ctrl Pts',(-0.0571809374746232,0.186884282379595,
-0.47620265353275));
#83696=CARTESIAN_POINT('Ctrl Pts',(-0.0535645658198097,0.187952584874734,
-0.476418652065097));
#83697=CARTESIAN_POINT('Ctrl Pts',(-0.0499243162402038,0.188914590881562,
-0.476634650597444));
#83698=CARTESIAN_POINT('Ctrl Pts',(-0.0381829808841359,0.192017464707577,
-0.477331336676032));
#83699=CARTESIAN_POINT('Ctrl Pts',(-0.0261100611714576,0.194032430862605,
-0.478028022754621));
#83700=CARTESIAN_POINT('Ctrl Pts',(-0.0139280386221067,0.194902975195714,
-0.47872470883321));
#83701=CARTESIAN_POINT('Ctrl Pts',(-0.00177143381479845,0.195771703141503,
-0.479419941279041));
#83702=CARTESIAN_POINT('Ctrl Pts',(0.0104929631452944,0.195500613463922,
-0.480115173724872));
#83703=CARTESIAN_POINT('Ctrl Pts',(0.0226349137272716,0.194084570949262,
-0.480810406170703));
#83704=CARTESIAN_POINT('Ctrl Pts',(0.0347751875333354,0.192668723986869,
-0.481505542606506));
#83705=CARTESIAN_POINT('Ctrl Pts',(0.0467921755147186,0.19010829424219,
-0.482200679042309));
#83706=CARTESIAN_POINT('Ctrl Pts',(0.0584595984062355,0.186450088104516,
-0.482895815478112));
#83707=CARTESIAN_POINT('Ctrl Pts',(0.0701264160249562,0.182792071744197,
-0.483590915852209));
#83708=CARTESIAN_POINT('Ctrl Pts',(0.08144287774861,0.178036679634478,-0.484286016226306));
#83709=CARTESIAN_POINT('Ctrl Pts',(0.092199420855013,0.172280082406528,
-0.484981116600402));
#83710=CARTESIAN_POINT('Ctrl Pts',(0.10298053813718,0.16651033377569,-0.485677804986428));
#83711=CARTESIAN_POINT('Ctrl Pts',(0.113198443100993,0.15973528387605,-0.486374493372454));
#83712=CARTESIAN_POINT('Ctrl Pts',(0.122670680915762,0.152095575358599,
-0.48707118175848));
#83713=CARTESIAN_POINT('Ctrl Pts',(0.125607416344511,0.149726990119582,
-0.487287180290827));
#83714=CARTESIAN_POINT('Ctrl Pts',(0.128472724790555,0.147275577939621,
-0.487503178823175));
#83715=CARTESIAN_POINT('Ctrl Pts',(0.131261882003931,0.144746254987084,
-0.487719177355523));
#83716=CARTESIAN_POINT('Ctrl Pts',(0.140258086656035,0.136588125067709,
-0.488415863434112));
#83717=CARTESIAN_POINT('Ctrl Pts',(0.14852239569127,0.127559466520344,-0.489112549512701));
#83718=CARTESIAN_POINT('Ctrl Pts',(0.155886256925708,0.117816106291509,
-0.48980923559129));
#83719=CARTESIAN_POINT('Ctrl Pts',(0.163234753492699,0.108093075545396,
-0.490504468037121));
#83720=CARTESIAN_POINT('Ctrl Pts',(0.169685950201453,0.0976589496388772,
-0.491199700482953));
#83721=CARTESIAN_POINT('Ctrl Pts',(0.175110163793777,0.08670403990655,-0.491894932928784));
#83722=CARTESIAN_POINT('Ctrl Pts',(0.180533628314472,0.0757506430224801,
-0.492590069364587));
#83723=CARTESIAN_POINT('Ctrl Pts',(0.184929962974441,0.0642773678937392,
-0.49328520580039));
#83724=CARTESIAN_POINT('Ctrl Pts',(0.188215205454289,0.0524994898622816,
-0.493980342236193));
#83725=CARTESIAN_POINT('Ctrl Pts',(0.191500277505078,0.0407222228337199,
-0.49467544261029));
#83726=CARTESIAN_POINT('Ctrl Pts',(0.193674162774775,0.0286412343437673,
-0.495370542984387));
#83727=CARTESIAN_POINT('Ctrl Pts',(0.194703405140545,0.0164846603445962,
-0.496065643358484));
#83728=CARTESIAN_POINT('Ctrl Pts',(0.195734998892123,0.00430031368805828,
-0.49676233174451));
#83729=CARTESIAN_POINT('Ctrl Pts',(0.195616720597611,-0.00795908651086126,
-0.497459020130536));
#83730=CARTESIAN_POINT('Ctrl Pts',(0.194367175683108,-0.0200639232696899,
-0.498155708516562));
#83731=CARTESIAN_POINT('Ctrl Pts',(0.193979771682914,-0.0238168593407548,
-0.498371707048909));
#83732=CARTESIAN_POINT('Ctrl Pts',(0.193484002827447,-0.0275549908805594,
-0.498587705581256));
#83733=CARTESIAN_POINT('Ctrl Pts',(0.19288141986272,-0.0312716784285904,
-0.498803704113604));
#83734=CARTESIAN_POINT('Ctrl Pts',(0.190937836458897,-0.0432595583694434,
-0.499500390192193));
#83735=CARTESIAN_POINT('Ctrl Pts',(0.187865562364591,-0.0551076219616193,
-0.500197076270781));
#83736=CARTESIAN_POINT('Ctrl Pts',(0.183703509188537,-0.0665896441784849,
-0.50089376234937));
#83737=CARTESIAN_POINT('Ctrl Pts',(0.179550140120032,-0.0780477092012426,
-0.501588994795202));
#83738=CARTESIAN_POINT('Ctrl Pts',(0.174311731072823,-0.0891404091909756,
-0.502284227241033));
#83739=CARTESIAN_POINT('Ctrl Pts',(0.16807728275083,-0.0996553411669321,
-0.502979459686865));
#83740=CARTESIAN_POINT('Ctrl Pts',(0.161843695392049,-0.110168821054565,
-0.503674596122668));
#83741=CARTESIAN_POINT('Ctrl Pts',(0.154614748386074,-0.12010391671626,
-0.504369732558471));
#83742=CARTESIAN_POINT('Ctrl Pts',(0.146525277771686,-0.12927297851419,
-0.505064868994274));
#83743=CARTESIAN_POINT('Ctrl Pts',(0.138436226816083,-0.138441564647208,
-0.505759969368371));
#83744=CARTESIAN_POINT('Ctrl Pts',(0.129487340027504,-0.14684355758373,
-0.506455069742468));
#83745=CARTESIAN_POINT('Ctrl Pts',(0.119851743118805,-0.154326665457995,
-0.507150170116565));
#83746=CARTESIAN_POINT('Ctrl Pts',(0.110194132924826,-0.16182686908564,
-0.507846858502591));
#83747=CARTESIAN_POINT('Ctrl Pts',(0.0998474112615499,-0.168403512136232,
-0.508543546888617));
#83748=CARTESIAN_POINT('Ctrl Pts',(0.0890142960991703,-0.173947161776125,
-0.509240235274643));
#83749=CARTESIAN_POINT('Ctrl Pts',(0.0856556395997188,-0.175665893148829,
-0.50945623380699));
#83750=CARTESIAN_POINT('Ctrl Pts',(0.0822503900941689,-0.177285673989513,
-0.509672232339337));
#83751=CARTESIAN_POINT('Ctrl Pts',(0.0788049607474615,-0.178804189440827,
-0.509888230871684));
#83752=CARTESIAN_POINT('Ctrl Pts',(0.0676920025503313,-0.183702040197298,
-0.510584916950272));
#83753=CARTESIAN_POINT('Ctrl Pts',(0.0560816847625869,-0.187577088566324,
-0.511281603028861));
#83754=CARTESIAN_POINT('Ctrl Pts',(0.0441849381383652,-0.190338780183411,
-0.51197828910745));
#83755=CARTESIAN_POINT('Ctrl Pts',(0.0323130140290933,-0.193094709541822,
-0.512673521553281));
#83756=CARTESIAN_POINT('Ctrl Pts',(0.0201566744902528,-0.194741625272648,
-0.513368753999112));
#83757=CARTESIAN_POINT('Ctrl Pts',(0.00794253330288551,-0.19523851096731,
-0.514063986444944));
#83758=CARTESIAN_POINT('Ctrl Pts',(-0.0042699211392091,-0.195735328043182,
-0.514759122880747));
#83759=CARTESIAN_POINT('Ctrl Pts',(-0.0165392903042251,-0.195082349548358,
-0.51545425931655));
#83760=CARTESIAN_POINT('Ctrl Pts',(-0.0286347621607715,-0.193290481907403,
-0.516149395752352));
#83761=CARTESIAN_POINT('Ctrl Pts',(-0.0407296065385554,-0.191498707223457,
-0.516844496126449));
#83762=CARTESIAN_POINT('Ctrl Pts',(-0.0526497099517824,-0.188568315666333,
-0.517539596500546));
#83763=CARTESIAN_POINT('Ctrl Pts',(-0.0641730653434497,-0.184561582363246,
-0.518234696874643));
#83764=CARTESIAN_POINT('Ctrl Pts',(-0.0757227467543576,-0.180545695360178,
-0.518931385260669));
#83765=CARTESIAN_POINT('Ctrl Pts',(-0.0868730663070533,-0.175448906482376,
-0.519628073646694));
#83766=CARTESIAN_POINT('Ctrl Pts',(-0.0974218496138087,-0.169381649589985,
-0.52032476203272));
#83767=CARTESIAN_POINT('Ctrl Pts',(-0.100692352980909,-0.16750058108013,
-0.520540760565068));
#83768=CARTESIAN_POINT('Ctrl Pts',(-0.103905235860399,-0.165526550236975,
-0.520756759097416));
#83769=CARTESIAN_POINT('Ctrl Pts',(-0.10705506443072,-0.163463675413635,
-0.520972757629764));
#83770=CARTESIAN_POINT('Ctrl Pts',(-0.117207367848539,-0.156814764004024,
-0.521668948736437));
#83771=CARTESIAN_POINT('Ctrl Pts',(-0.1267737660995,-0.149192930854621,
-0.522365139843109));
#83772=CARTESIAN_POINT('Ctrl Pts',(-0.135563601880418,-0.140725512417641,
-0.523061330949781));
#83773=CARTESIAN_POINT('Ctrl Pts',(-0.144335100214774,-0.132275758796816,
-0.523756069655347));
#83774=CARTESIAN_POINT('Ctrl Pts',(-0.152332575326338,-0.122984469850852,
-0.524450808360913));
#83775=CARTESIAN_POINT('Ctrl Pts',(-0.159398358528159,-0.113019128020563,
-0.525145547066479));
#83776=CARTESIAN_POINT('Ctrl Pts',(-0.16646317386283,-0.103055151237392,
-0.525840190607114));
#83777=CARTESIAN_POINT('Ctrl Pts',(-0.172596007680861,-0.0924179925879917,
-0.526534834147748));
#83778=CARTESIAN_POINT('Ctrl Pts',(-0.17768045116012,-0.081306932518306,
-0.527229477688383));
#83779=CARTESIAN_POINT('Ctrl Pts',(-0.18276467250458,-0.0701963578809189,
-0.527924090880662));
#83780=CARTESIAN_POINT('Ctrl Pts',(-0.186800254976389,-0.0586127313267355,
-0.52861870407294));
#83781=CARTESIAN_POINT('Ctrl Pts',(-0.189718671700916,-0.0467759084149099,
-0.529313317265219));
#83782=CARTESIAN_POINT('Ctrl Pts',(-0.192643733322442,-0.034912134427736,
-0.530009512011316));
#83783=CARTESIAN_POINT('Ctrl Pts',(-0.194446406647556,-0.0227948792513746,
-0.530705706757414));
#83784=CARTESIAN_POINT('Ctrl Pts',(-0.195109359192541,-0.010653541921629,
-0.531401901503512));
#83785=CARTESIAN_POINT('Ctrl Pts',(-0.195303342133092,-0.00710093120272025,
-0.531605611263834));
#83786=CARTESIAN_POINT('Ctrl Pts',(-0.195400086282404,-0.00354626374671888,
-0.531809321024156));
#83787=CARTESIAN_POINT('Ctrl Pts',(-0.195399999942242,4.75099905375869E-6,
-0.532013030784479));
#83788=CARTESIAN_POINT('',(-0.195399934316705,-0.000160215565585998,-0.602013030783437));
#83789=CARTESIAN_POINT('Ctrl Pts',(-0.19539999994224,4.75105306059038E-6,
-0.532013030787577));
#83790=CARTESIAN_POINT('Ctrl Pts',(-0.195399704441082,0.0121580412039381,
-0.532710224125548));
#83791=CARTESIAN_POINT('Ctrl Pts',(-0.194261233336228,0.0243536335351822,
-0.533407417463518));
#83792=CARTESIAN_POINT('Ctrl Pts',(-0.19198694281045,0.0363617077472572,
-0.534104610801489));
#83793=CARTESIAN_POINT('Ctrl Pts',(-0.189717397132364,0.0483447295385626,
-0.534800349586419));
#83794=CARTESIAN_POINT('Ctrl Pts',(-0.186316824434827,0.0601401463011918,
-0.535496088371348));
#83795=CARTESIAN_POINT('Ctrl Pts',(-0.181839233487673,0.0715237943947003,
-0.536191827156278));
#83796=CARTESIAN_POINT('Ctrl Pts',(-0.177362265235332,0.0829058593738311,
-0.536887469185399));
#83797=CARTESIAN_POINT('Ctrl Pts',(-0.171808852972938,0.0938754410502758,
-0.537583111214521));
#83798=CARTESIAN_POINT('Ctrl Pts',(-0.165282210432941,0.104225481118587,
-0.538278753243642));
#83799=CARTESIAN_POINT('Ctrl Pts',(-0.158755959389981,0.114574900345479,
-0.538974353545062));
#83800=CARTESIAN_POINT('Ctrl Pts',(-0.151257082255755,0.124304126911855,
-0.539669953846481));
#83801=CARTESIAN_POINT('Ctrl Pts',(-0.1429322553959,0.133234869187616,-0.540365554147901));
#83802=CARTESIAN_POINT('Ctrl Pts',(-0.134588349521748,0.142186079127443,
-0.541062748640806));
#83803=CARTESIAN_POINT('Ctrl Pts',(-0.12541535689199,0.150334556288951,
-0.541759943133711));
#83804=CARTESIAN_POINT('Ctrl Pts',(-0.115596060566579,0.157539553069976,
-0.542457137626616));
#83805=CARTESIAN_POINT('Ctrl Pts',(-0.112381743643222,0.159898086952496,
-0.542685362133052));
#83806=CARTESIAN_POINT('Ctrl Pts',(-0.109098407206999,0.162155865510001,
-0.542913586639488));
#83807=CARTESIAN_POINT('Ctrl Pts',(-0.105753080990153,0.164308995070538,
-0.543141811145924));
#83808=CARTESIAN_POINT('Ctrl Pts',(-0.0955410216455612,0.170881713371695,
-0.543838497224512));
#83809=CARTESIAN_POINT('Ctrl Pts',(-0.0846780241638187,0.17652181662486,
-0.544535183303101));
#83810=CARTESIAN_POINT('Ctrl Pts',(-0.0733582959045753,0.181106930905409,
-0.54523186938169));
#83811=CARTESIAN_POINT('Ctrl Pts',(-0.062062186213738,0.185682478363081,
-0.545927101827521));
#83812=CARTESIAN_POINT('Ctrl Pts',(-0.050312012500802,0.1892070123924,-0.546622334273352));
#83813=CARTESIAN_POINT('Ctrl Pts',(-0.0383252065753447,0.191604641230209,
-0.547317566719184));
#83814=CARTESIAN_POINT('Ctrl Pts',(-0.0263400560006732,0.194001938960899,
-0.548012703154987));
#83815=CARTESIAN_POINT('Ctrl Pts',(-0.0141191858681597,0.195272424626458,
-0.548707839590789));
#83816=CARTESIAN_POINT('Ctrl Pts',(-0.00189228080062207,0.195390837229824,
-0.549402976026592));
#83817=CARTESIAN_POINT('Ctrl Pts',(0.0103339899697718,0.195509243690281,
-0.550098076400689));
#83818=CARTESIAN_POINT('Ctrl Pts',(0.0225654198570891,0.194475714313942,
-0.550793176774786));
#83819=CARTESIAN_POINT('Ctrl Pts',(0.0345730017209927,0.192317101558858,
-0.551488277148883));
#83820=CARTESIAN_POINT('Ctrl Pts',(0.0466080158579125,0.190153557281749,
-0.552184965534909));
#83821=CARTESIAN_POINT('Ctrl Pts',(0.0584173120980081,0.186860017346395,
-0.552881653920935));
#83822=CARTESIAN_POINT('Ctrl Pts',(0.0697839543939136,0.182513998666262,
-0.55357834230696));
#83823=CARTESIAN_POINT('Ctrl Pts',(0.0733080235514968,0.181166576095002,
-0.553794340839308));
#83824=CARTESIAN_POINT('Ctrl Pts',(0.0767896917366288,0.179718335501842,
-0.554010339371656));
#83825=CARTESIAN_POINT('Ctrl Pts',(0.0802229488090808,0.178172496430778,
-0.554226337904004));
#83826=CARTESIAN_POINT('Ctrl Pts',(0.0912966463041234,0.173186515513026,
-0.554923023982593));
#83827=CARTESIAN_POINT('Ctrl Pts',(0.101942600437265,0.167146719192801,
-0.555619710061182));
#83828=CARTESIAN_POINT('Ctrl Pts',(0.111952417199804,0.160149356174544,
-0.556316396139771));
#83829=CARTESIAN_POINT('Ctrl Pts',(0.121941348519114,0.15316659312665,-0.557011628585602));
#83830=CARTESIAN_POINT('Ctrl Pts',(0.131296024692209,0.145230664944981,
-0.557706861031433));
#83831=CARTESIAN_POINT('Ctrl Pts',(0.139834390787362,0.136482611174931,
-0.558402093477264));
#83832=CARTESIAN_POINT('Ctrl Pts',(0.14837157775347,0.127735765491319,-0.559097229913067));
#83833=CARTESIAN_POINT('Ctrl Pts',(0.156092035764051,0.11817761040108,-0.55979236634887));
#83834=CARTESIAN_POINT('Ctrl Pts',(0.16284950311487,0.107987033181026,-0.560487502784673));
#83835=CARTESIAN_POINT('Ctrl Pts',(0.169606619907455,0.0977969846192045,
-0.56118260315877));
#83836=CARTESIAN_POINT('Ctrl Pts',(0.175400384209146,0.0869753232275042,
-0.561877703532867));
#83837=CARTESIAN_POINT('Ctrl Pts',(0.18012861229942,0.0757287463984798,
-0.562572803906964));
#83838=CARTESIAN_POINT('Ctrl Pts',(0.184867642401734,0.0644564758727907,
-0.56326949229299));
#83839=CARTESIAN_POINT('Ctrl Pts',(0.188535997983766,0.0527581832488236,
-0.563966180679016));
#83840=CARTESIAN_POINT('Ctrl Pts',(0.191080562372172,0.0408580308328046,
-0.564662869065041));
#83841=CARTESIAN_POINT('Ctrl Pts',(0.191869469126445,0.0371685542918895,
-0.564878867597389));
#83842=CARTESIAN_POINT('Ctrl Pts',(0.192550727476237,0.0334597402998151,
-0.565094866129736));
#83843=CARTESIAN_POINT('Ctrl Pts',(0.193123764929154,0.0297383829350012,
-0.565310864662084));
#83844=CARTESIAN_POINT('Ctrl Pts',(0.194972051635638,0.017735440871715,
-0.566007550740673));
#83845=CARTESIAN_POINT('Ctrl Pts',(0.19570354560059,0.00551740520414245,
-0.566704236819262));
#83846=CARTESIAN_POINT('Ctrl Pts',(0.195285492605467,-0.00668852583458686,
-0.567400922897851));
#83847=CARTESIAN_POINT('Ctrl Pts',(0.194868311876272,-0.0188689892463043,
-0.568096155343683));
#83848=CARTESIAN_POINT('Ctrl Pts',(0.193306300869942,-0.0310365298369193,
-0.568791387789514));
#83849=CARTESIAN_POINT('Ctrl Pts',(0.190618615664043,-0.0429616499022531,
-0.569486620235346));
#83850=CARTESIAN_POINT('Ctrl Pts',(0.187931301621392,-0.0548851231354774,
-0.570181756671149));
#83851=CARTESIAN_POINT('Ctrl Pts',(0.184118769834951,-0.0665653800675682,
-0.570876893106952));
#83852=CARTESIAN_POINT('Ctrl Pts',(0.179251411541754,-0.0777823338573007,
-0.571572029542756));
#83853=CARTESIAN_POINT('Ctrl Pts',(0.174384305753297,-0.0889987057432954,
-0.572267129916853));
#83854=CARTESIAN_POINT('Ctrl Pts',(0.168462855206484,-0.0997510303050761,
-0.57296223029095));
#83855=CARTESIAN_POINT('Ctrl Pts',(0.161604778916721,-0.109841046204403,
-0.573657330665048));
#83856=CARTESIAN_POINT('Ctrl Pts',(0.154731034807801,-0.119954113545231,
-0.574354019051074));
#83857=CARTESIAN_POINT('Ctrl Pts',(0.146916938705459,-0.129401165206762,
-0.5750507074371));
#83858=CARTESIAN_POINT('Ctrl Pts',(0.138321577373936,-0.138015583296909,
-0.575747395823126));
#83859=CARTESIAN_POINT('Ctrl Pts',(0.13565670528789,-0.140686363665592,
-0.575963394355472));
#83860=CARTESIAN_POINT('Ctrl Pts',(0.132916994470893,-0.143277386399193,
-0.576179392887818));
#83861=CARTESIAN_POINT('Ctrl Pts',(0.130107831562634,-0.145784471621875,
-0.576395391420164));
#83862=CARTESIAN_POINT('Ctrl Pts',(0.121047100133513,-0.153870875513176,
-0.577092077498753));
#83863=CARTESIAN_POINT('Ctrl Pts',(0.111197814895793,-0.161137722098923,
-0.577788763577342));
#83864=CARTESIAN_POINT('Ctrl Pts',(0.100732697291677,-0.167433818854923,
-0.578485449655931));
#83865=CARTESIAN_POINT('Ctrl Pts',(0.0902894151142026,-0.173716778829853,
-0.579180682101762));
#83866=CARTESIAN_POINT('Ctrl Pts',(0.0792335552777163,-0.179032499447423,
-0.579875914547594));
#83867=CARTESIAN_POINT('Ctrl Pts',(0.0677680355670711,-0.183272074674185,
-0.580571146993425));
#83868=CARTESIAN_POINT('Ctrl Pts',(0.0563040992187653,-0.187511064425198,
-0.581266283429228));
#83869=CARTESIAN_POINT('Ctrl Pts',(0.0444314189991363,-0.19067385828896,
-0.581961419865031));
#83870=CARTESIAN_POINT('Ctrl Pts',(0.0323729195949517,-0.192699647319083,
-0.582656556300834));
#83871=CARTESIAN_POINT('Ctrl Pts',(0.0203150457515041,-0.194725331257018,
-0.583351656674931));
#83872=CARTESIAN_POINT('Ctrl Pts',(0.00807223922603621,-0.195614009173991,
-0.584046757049028));
#83873=CARTESIAN_POINT('Ctrl Pts',(-0.00412510867143945,-0.195356452359396,
-0.584741857423125));
#83874=CARTESIAN_POINT('Ctrl Pts',(-0.0163503223774861,-0.195098307135831,
-0.58543854580915));
#83875=CARTESIAN_POINT('Ctrl Pts',(-0.0285289974000453,-0.193688783213689,
-0.586135234195176));
#83876=CARTESIAN_POINT('Ctrl Pts',(-0.0404347559278585,-0.191170579622113,
-0.586831922581202));
#83877=CARTESIAN_POINT('Ctrl Pts',(-0.0441259705656679,-0.190389845665809,
-0.58704792111355));
#83878=CARTESIAN_POINT('Ctrl Pts',(-0.0477910435399655,-0.189502910346834,
-0.587263919645897));
#83879=CARTESIAN_POINT('Ctrl Pts',(-0.051423535777776,-0.188512015447588,
-0.587479918178244));
#83880=CARTESIAN_POINT('Ctrl Pts',(-0.0631398504450944,-0.185315962797851,
-0.588176604256832));
#83881=CARTESIAN_POINT('Ctrl Pts',(-0.0745981850498335,-0.181012238006438,
-0.58887329033542));
#83882=CARTESIAN_POINT('Ctrl Pts',(-0.0855776747297964,-0.175663375772644,
-0.589569976414008));
#83883=CARTESIAN_POINT('Ctrl Pts',(-0.0965342557478107,-0.170325673918822,
-0.590265208859839));
#83884=CARTESIAN_POINT('Ctrl Pts',(-0.107013163827437,-0.163947476064685,
-0.590960441305669));
#83885=CARTESIAN_POINT('Ctrl Pts',(-0.116812557614591,-0.156639670529332,
-0.5916556737515));
#83886=CARTESIAN_POINT('Ctrl Pts',(-0.126610598127626,-0.149332874185397,
-0.592350810187302));
#83887=CARTESIAN_POINT('Ctrl Pts',(-0.135728583186761,-0.141097210940505,
-0.593045946623104));
#83888=CARTESIAN_POINT('Ctrl Pts',(-0.143994117112832,-0.132086540710611,
-0.593741083058906));
#83889=CARTESIAN_POINT('Ctrl Pts',(-0.152259222246454,-0.123076337928724,
-0.594436183433003));
#83890=CARTESIAN_POINT('Ctrl Pts',(-0.159671392506933,-0.113291871050581,
-0.595131283807099));
#83891=CARTESIAN_POINT('Ctrl Pts',(-0.166097428106162,-0.102921350440607,
-0.595826384181195));
#83892=CARTESIAN_POINT('Ctrl Pts',(-0.172538144493329,-0.0925271375538757,
-0.59652307256722));
#83893=CARTESIAN_POINT('Ctrl Pts',(-0.177987823682078,-0.0815449756659985,
-0.597219760953245));
#83894=CARTESIAN_POINT('Ctrl Pts',(-0.182359004728149,-0.0701879861127176,
-0.59791644933927));
#83895=CARTESIAN_POINT('Ctrl Pts',(-0.183714228540592,-0.0666669096535048,
-0.598132447871621));
#83896=CARTESIAN_POINT('Ctrl Pts',(-0.184966142778584,-0.0631099270968684,
-0.598348446403973));
#83897=CARTESIAN_POINT('Ctrl Pts',(-0.186113121297839,-0.0595236598402349,
-0.598564444936324));
#83898=CARTESIAN_POINT('Ctrl Pts',(-0.190528317054616,-0.0457186306192422,
-0.599395912821293));
#83899=CARTESIAN_POINT('Ctrl Pts',(-0.193410026225108,-0.0314006634720892,
-0.600227380706261));
#83900=CARTESIAN_POINT('Ctrl Pts',(-0.194669066429944,-0.0168853361024844,
-0.601058848591229));
#83901=CARTESIAN_POINT('Ctrl Pts',(-0.195150686050878,-0.0113327997826631,
-0.601376909321965));
#83902=CARTESIAN_POINT('Ctrl Pts',(-0.19539534973394,-0.00575160219395176,
-0.601694970052701));
#83903=CARTESIAN_POINT('Ctrl Pts',(-0.195399934316705,-0.000160215565585217,
-0.602013030783437));
#83904=CARTESIAN_POINT('',(-0.19539996230052,0.000121379385344387,-0.672013030792617));
#83905=CARTESIAN_POINT('Ctrl Pts',(-0.195399934316764,-0.000160215492812403,
-0.602013030787577));
#83906=CARTESIAN_POINT('Ctrl Pts',(-0.195409913750772,0.0120107719400208,
-0.602705365876152));
#83907=CARTESIAN_POINT('Ctrl Pts',(-0.194278398116146,0.0241993431608203,
-0.603397700964727));
#83908=CARTESIAN_POINT('Ctrl Pts',(-0.19202192620965,0.0361765097091413,
-0.604090036053301));
#83909=CARTESIAN_POINT('Ctrl Pts',(-0.189766351259512,0.0481489152871848,
-0.604782095935986));
#83910=CARTESIAN_POINT('Ctrl Pts',(-0.186386880787103,0.0599092164680677,
-0.605474155818671));
#83911=CARTESIAN_POINT('Ctrl Pts',(-0.181951258354798,0.0712383294519561,
-0.606166215701356));
#83912=CARTESIAN_POINT('Ctrl Pts',(-0.177504766240249,0.082595204911151,
-0.606859971506346));
#83913=CARTESIAN_POINT('Ctrl Pts',(-0.171997315619093,0.0935179720006077,
-0.607553727311336));
#83914=CARTESIAN_POINT('Ctrl Pts',(-0.165544577333922,0.103808250709339,
-0.608247483116325));
#83915=CARTESIAN_POINT('Ctrl Pts',(-0.161199417774438,0.110737541953609,
-0.608714645975685));
#83916=CARTESIAN_POINT('Ctrl Pts',(-0.156426621585289,0.117380524878914,
-0.609181808835044));
#83917=CARTESIAN_POINT('Ctrl Pts',(-0.151271963941549,0.123684893682562,
-0.609648971694404));
#83918=CARTESIAN_POINT('Ctrl Pts',(-0.143584755619367,0.133086681285734,
-0.610345657772992));
#83919=CARTESIAN_POINT('Ctrl Pts',(-0.134990715424245,0.141802067227806,
-0.611042343851581));
#83920=CARTESIAN_POINT('Ctrl Pts',(-0.125636843254467,0.149654748060502,
-0.611739029930169));
#83921=CARTESIAN_POINT('Ctrl Pts',(-0.116302487902111,0.157491044305586,
-0.612434262376));
#83922=CARTESIAN_POINT('Ctrl Pts',(-0.106212063419679,0.164467594754932,
-0.613129494821831));
#83923=CARTESIAN_POINT('Ctrl Pts',(-0.0955489974396641,0.17044514979393,
-0.613824727267662));
#83924=CARTESIAN_POINT('Ctrl Pts',(-0.0848874040049419,0.176421879346097,
-0.614519863703464));
#83925=CARTESIAN_POINT('Ctrl Pts',(-0.0736540659606052,0.181399420606974,
-0.615215000139267));
#83926=CARTESIAN_POINT('Ctrl Pts',(-0.0620596813029653,0.18528290789108,
-0.615910136575069));
#83927=CARTESIAN_POINT('Ctrl Pts',(-0.050465898129107,0.189166193710883,
-0.616605236949166));
#83928=CARTESIAN_POINT('Ctrl Pts',(-0.0385119437893241,0.191955285982993,
-0.617300337323262));
#83929=CARTESIAN_POINT('Ctrl Pts',(-0.0264239439058242,0.193605101142666,
-0.617995437697359));
#83930=CARTESIAN_POINT('Ctrl Pts',(-0.0143083280279611,0.195258685435908,
-0.618692126083384));
#83931=CARTESIAN_POINT('Ctrl Pts',(-0.00205893035789418,0.195767743107061,
-0.61938881446941));
#83932=CARTESIAN_POINT('Ctrl Pts',(0.0100939809641747,0.195139108197959,
-0.620085502855435));
#83933=CARTESIAN_POINT('Ctrl Pts',(0.0138618218841569,0.194944208698451,
-0.620301501387785));
#83934=CARTESIAN_POINT('Ctrl Pts',(0.0176204215183335,0.194640328858322,
-0.620517499920135));
#83935=CARTESIAN_POINT('Ctrl Pts',(0.0213630697655697,0.194228677723428,
-0.620733498452485));
#83936=CARTESIAN_POINT('Ctrl Pts',(0.0334346838757103,0.192900929743878,
-0.621430184531068));
#83937=CARTESIAN_POINT('Ctrl Pts',(0.0454244076356298,0.190438816189816,
-0.622126870609651));
#83938=CARTESIAN_POINT('Ctrl Pts',(0.0571043215712217,0.186869624224727,
-0.622823556688234));
#83939=CARTESIAN_POINT('Ctrl Pts',(0.0687598654124098,0.183307879364608,
-0.623518789134059));
#83940=CARTESIAN_POINT('Ctrl Pts',(0.0801060324371824,0.178643823591831,
-0.624214021579884));
#83941=CARTESIAN_POINT('Ctrl Pts',(0.0909261445995594,0.172955474698721,
-0.62490925402571));
#83942=CARTESIAN_POINT('Ctrl Pts',(0.101744762528922,0.167267911353726,
-0.625604390461507));
#83943=CARTESIAN_POINT('Ctrl Pts',(0.112036675421449,0.160556702101101,
-0.626299526897304));
#83944=CARTESIAN_POINT('Ctrl Pts',(0.12160758126088,0.15294690640833,-0.626994663333101));
#83945=CARTESIAN_POINT('Ctrl Pts',(0.131177990588873,0.145337505490166,
-0.627689763707192));
#83946=CARTESIAN_POINT('Ctrl Pts',(0.14002679907744,0.136830176391645,-0.628384864081283));
#83947=CARTESIAN_POINT('Ctrl Pts',(0.147993057312752,0.127590026989669,
-0.629079964455375));
#83948=CARTESIAN_POINT('Ctrl Pts',(0.155977515096758,0.118328767733604,
-0.629776652841395));
#83949=CARTESIAN_POINT('Ctrl Pts',(0.16307487608635,0.108332050773861,-0.630473341227415));
#83950=CARTESIAN_POINT('Ctrl Pts',(0.169165479860222,0.0977967301276523,
-0.631170029613435));
#83951=CARTESIAN_POINT('Ctrl Pts',(0.171053786745825,0.0945304006705272,
-0.631386028145812));
#83952=CARTESIAN_POINT('Ctrl Pts',(0.172845656334852,0.0912124769904705,
-0.631602026678188));
#83953=CARTESIAN_POINT('Ctrl Pts',(0.174538448708856,0.0878492454282104,
-0.631818025210564));
#83954=CARTESIAN_POINT('Ctrl Pts',(0.179998415811227,0.0770014096453982,
-0.632514711289167));
#83955=CARTESIAN_POINT('Ctrl Pts',(0.184462364392482,0.0656045398091443,
-0.633211397367771));
#83956=CARTESIAN_POINT('Ctrl Pts',(0.187829067619882,0.053864657773402,
-0.633908083446374));
#83957=CARTESIAN_POINT('Ctrl Pts',(0.191188746234265,0.0421492709552665,
-0.63460331589222));
#83958=CARTESIAN_POINT('Ctrl Pts',(0.19345541392759,0.0300931048987756,
-0.635298548338066));
#83959=CARTESIAN_POINT('Ctrl Pts',(0.19457651462254,0.017920378270127,-0.635993780783911));
#83960=CARTESIAN_POINT('Ctrl Pts',(0.19569746049602,0.00574933266749327,
-0.636688917219729));
#83961=CARTESIAN_POINT('Ctrl Pts',(0.195673028155159,-0.00653737574804703,
-0.637384053655546));
#83962=CARTESIAN_POINT('Ctrl Pts',(0.194502301584276,-0.018708679227013,
-0.638079190091363));
#83963=CARTESIAN_POINT('Ctrl Pts',(0.193331635747367,-0.0308793512932791,
-0.638774290465474));
#83964=CARTESIAN_POINT('Ctrl Pts',(0.191014904436083,-0.0429337619423767,
-0.639469390839585));
#83965=CARTESIAN_POINT('Ctrl Pts',(0.187602943526061,-0.0546470088875656,
-0.640164491213696));
#83966=CARTESIAN_POINT('Ctrl Pts',(0.184183187720758,-0.0663870156743068,
-0.640861179599736));
#83967=CARTESIAN_POINT('Ctrl Pts',(0.179663514437599,-0.0777834816358084,
-0.641557867985775));
#83968=CARTESIAN_POINT('Ctrl Pts',(0.174143869845266,-0.0886288474217898,
-0.642254556371815));
#83969=CARTESIAN_POINT('Ctrl Pts',(0.172432580903867,-0.0919913020553304,
-0.642470554904092));
#83970=CARTESIAN_POINT('Ctrl Pts',(0.170625503544467,-0.0953009675331104,
-0.642686553436368));
#83971=CARTESIAN_POINT('Ctrl Pts',(0.168726472737284,-0.0985522064574634,
-0.642902551968645));
#83972=CARTESIAN_POINT('Ctrl Pts',(0.162601299977015,-0.109038818902745,
-0.643599238047224));
#83973=CARTESIAN_POINT('Ctrl Pts',(0.155473255404872,-0.118989017874075,
-0.644295924125804));
#83974=CARTESIAN_POINT('Ctrl Pts',(0.147460012514969,-0.128205712466665,
-0.644992610204383));
#83975=CARTESIAN_POINT('Ctrl Pts',(0.139463489224775,-0.137403176462311,
-0.645687842650206));
#83976=CARTESIAN_POINT('Ctrl Pts',(0.130585946322826,-0.145869471663221,
-0.646383075096028));
#83977=CARTESIAN_POINT('Ctrl Pts',(0.120986823116204,-0.153438419674632,
-0.64707830754185));
#83978=CARTESIAN_POINT('Ctrl Pts',(0.111389025526781,-0.161006322431444,
-0.647773443977645));
#83979=CARTESIAN_POINT('Ctrl Pts',(0.101070503411513,-0.167676547463309,
-0.648468580413439));
#83980=CARTESIAN_POINT('Ctrl Pts',(0.0902245611554579,-0.173322498725079,
-0.649163716849233));
#83981=CARTESIAN_POINT('Ctrl Pts',(0.0793791815561055,-0.178968157090921,
-0.649858817223322));
#83982=CARTESIAN_POINT('Ctrl Pts',(0.0680072247396998,-0.183589267154824,
-0.650553917597411));
#83983=CARTESIAN_POINT('Ctrl Pts',(0.0563250053900924,-0.187105996076572,
-0.6512490179715));
#83984=CARTESIAN_POINT('Ctrl Pts',(0.0446160970839333,-0.190630759244432,
-0.651945706357518));
#83985=CARTESIAN_POINT('Ctrl Pts',(0.032596367224158,-0.193045914950913,
-0.652642394743536));
#83986=CARTESIAN_POINT('Ctrl Pts',(0.0204943274429066,-0.194322264660185,
-0.653339083129553));
#83987=CARTESIAN_POINT('Ctrl Pts',(0.0167422585349957,-0.194717979113809,
-0.653555081661944));
#83988=CARTESIAN_POINT('Ctrl Pts',(0.0129823039122766,-0.195004606760184,
-0.653771080194334));
#83989=CARTESIAN_POINT('Ctrl Pts',(0.00922128015307064,-0.195182294259337,
-0.653987078726724));
#83990=CARTESIAN_POINT('Ctrl Pts',(-0.0029096027059849,-0.195755411148715,
-0.65468376480528));
#83991=CARTESIAN_POINT('Ctrl Pts',(-0.0151366931140761,-0.195195286936917,
-0.655380450883835));
#83992=CARTESIAN_POINT('Ctrl Pts',(-0.0272306062261563,-0.193493292091886,
-0.656077136962391));
#83993=CARTESIAN_POINT('Ctrl Pts',(-0.039299285436176,-0.191794848452394,
-0.656772369408188));
#83994=CARTESIAN_POINT('Ctrl Pts',(-0.0512344707610213,-0.188959310821571,
-0.657467601853986));
#83995=CARTESIAN_POINT('Ctrl Pts',(-0.0628099610316357,-0.18502991324433,
-0.658162834299783));
#83996=CARTESIAN_POINT('Ctrl Pts',(-0.0743838527532299,-0.181101058308006,
-0.658857970735553));
#83997=CARTESIAN_POINT('Ctrl Pts',(-0.0855973061772885,-0.176078881198892,
-0.659553107171322));
#83998=CARTESIAN_POINT('Ctrl Pts',(-0.0962388777946769,-0.170056574118207,
-0.660248243607091));
#83999=CARTESIAN_POINT('Ctrl Pts',(-0.106879897357519,-0.164034579457729,
-0.660943343981155));
#84000=CARTESIAN_POINT('Ctrl Pts',(-0.11694834584246,-0.157013012314087,
-0.661638444355218));
#84001=CARTESIAN_POINT('Ctrl Pts',(-0.126259471152442,-0.149129829156697,
-0.662333544729281));
#84002=CARTESIAN_POINT('Ctrl Pts',(-0.135591868466614,-0.141228636242208,
-0.663030233115274));
#84003=CARTESIAN_POINT('Ctrl Pts',(-0.144162863554939,-0.132462512459477,
-0.663726921501266));
#84004=CARTESIAN_POINT('Ctrl Pts',(-0.151823530936729,-0.123007217080561,
-0.664423609887259));
#84005=CARTESIAN_POINT('Ctrl Pts',(-0.154198614181723,-0.120075734415706,
-0.664639608419774));
#84006=CARTESIAN_POINT('Ctrl Pts',(-0.156486497327773,-0.117078234641055,
-0.664855606952289));
#84007=CARTESIAN_POINT('Ctrl Pts',(-0.158683591420661,-0.114020514881493,
-0.665071605484804));
#84008=CARTESIAN_POINT('Ctrl Pts',(-0.165825731652837,-0.104080720594039,
-0.665773756482416));
#84009=CARTESIAN_POINT('Ctrl Pts',(-0.172055164421404,-0.0934329165091907,
-0.666475907480027));
#84010=CARTESIAN_POINT('Ctrl Pts',(-0.177237810842229,-0.0822673593100837,
-0.667178058477638));
#84011=CARTESIAN_POINT('Ctrl Pts',(-0.182408615182921,-0.0711273148340792,
-0.667878605096386));
#84012=CARTESIAN_POINT('Ctrl Pts',(-0.186536952766617,-0.0594726009180445,
-0.668579151715133));
#84013=CARTESIAN_POINT('Ctrl Pts',(-0.189533861475579,-0.0475192103696621,
-0.66927969833388));
#84014=CARTESIAN_POINT('Ctrl Pts',(-0.192527619210319,-0.0355783877134433,
-0.669979508392207));
#84015=CARTESIAN_POINT('Ctrl Pts',(-0.194392063214706,-0.0233403297780268,
-0.670679318450535));
#84016=CARTESIAN_POINT('Ctrl Pts',(-0.195088109560349,-0.011035828386175,
-0.671379128508862));
#84017=CARTESIAN_POINT('Ctrl Pts',(-0.195298273903919,-0.00732060529198014,
-0.671590429268434));
#84018=CARTESIAN_POINT('Ctrl Pts',(-0.195402273579095,-0.0035993848560569,
-0.671801730028005));
#84019=CARTESIAN_POINT('Ctrl Pts',(-0.195399962300576,0.000121379296588555,
-0.672013030787577));
#84020=CARTESIAN_POINT('',(-0.195399988273324,6.76962695950741E-5,-0.742013030783604));
#84021=CARTESIAN_POINT('Ctrl Pts',(-0.19539996230052,0.000121379385344218,
-0.672013030792617));
#84022=CARTESIAN_POINT('Ctrl Pts',(-0.195391368601875,0.0139557581525191,
-0.672798679821104));
#84023=CARTESIAN_POINT('Ctrl Pts',(-0.193909385686024,0.0277341230872606,
-0.673584328849591));
#84024=CARTESIAN_POINT('Ctrl Pts',(-0.191013872295133,0.0411686845893673,
-0.674369977878078));
#84025=CARTESIAN_POINT('Ctrl Pts',(-0.188819578705173,0.0513497365163667,
-0.674965362666347));
#84026=CARTESIAN_POINT('Ctrl Pts',(-0.185814593619475,0.061333606866596,
-0.675560747454616));
#84027=CARTESIAN_POINT('Ctrl Pts',(-0.182043323198772,0.0710027357131215,
-0.676156132242885));
#84028=CARTESIAN_POINT('Ctrl Pts',(-0.177630392851685,0.0823170111049079,
-0.676852818321381));
#84029=CARTESIAN_POINT('Ctrl Pts',(-0.172143144054868,0.0932580156109927,
-0.677549504399877));
#84030=CARTESIAN_POINT('Ctrl Pts',(-0.165667038205755,0.103612704105882,
-0.678246190478373));
#84031=CARTESIAN_POINT('Ctrl Pts',(-0.159204444725966,0.113945787584046,
-0.678941422924112));
#84032=CARTESIAN_POINT('Ctrl Pts',(-0.151757486287423,0.12369420963015,
-0.679636655369852));
#84033=CARTESIAN_POINT('Ctrl Pts',(-0.143457703961445,0.132668938241437,
-0.680331887815592));
#84034=CARTESIAN_POINT('Ctrl Pts',(-0.135159067816597,0.141642427463043,
-0.681027024251306));
#84035=CARTESIAN_POINT('Ctrl Pts',(-0.126008401467838,0.149841763165552,
-0.681722160687021));
#84036=CARTESIAN_POINT('Ctrl Pts',(-0.116176875309522,0.157111723443274,
-0.682417297122735));
#84037=CARTESIAN_POINT('Ctrl Pts',(-0.106345859182866,0.1643813065761,-0.683112397496745));
#84038=CARTESIAN_POINT('Ctrl Pts',(-0.095834772975827,0.170721111523679,
-0.683807497870755));
#84039=CARTESIAN_POINT('Ctrl Pts',(-0.0848448157757491,0.176018513901178,
-0.684502598244765));
#84040=CARTESIAN_POINT('Ctrl Pts',(-0.0738297511468309,0.181328018614547,
-0.685199286630709));
#84041=CARTESIAN_POINT('Ctrl Pts',(-0.0623344474413148,0.185590045793406,
-0.685895975016652));
#84042=CARTESIAN_POINT('Ctrl Pts',(-0.0505800560208747,0.18874008035636,
-0.686592663402595));
#84043=CARTESIAN_POINT('Ctrl Pts',(-0.0469357706389397,0.189716704708889,
-0.686808661935385));
#84044=CARTESIAN_POINT('Ctrl Pts',(-0.0432666659218911,0.190586810909412,
-0.687024660468175));
#84045=CARTESIAN_POINT('Ctrl Pts',(-0.0395794977631675,0.191349479635601,
-0.687240659000965));
#84046=CARTESIAN_POINT('Ctrl Pts',(-0.0276868302910744,0.193809406918948,
-0.687937345079373));
#84047=CARTESIAN_POINT('Ctrl Pts',(-0.0155222166564679,0.195165007905675,
-0.688634031157782));
#84048=CARTESIAN_POINT('Ctrl Pts',(-0.00331088189918468,0.195371947989085,
-0.68933071723619));
#84049=CARTESIAN_POINT('Ctrl Pts',(0.00887497395619728,0.195578456292825,
-0.690025949681839));
#84050=CARTESIAN_POINT('Ctrl Pts',(0.0211064925116929,0.194640972341691,
-0.690721182127487));
#84051=CARTESIAN_POINT('Ctrl Pts',(0.0331534965784134,0.192566886210026,
-0.691416414573135));
#84052=CARTESIAN_POINT('Ctrl Pts',(0.0451988369811046,0.190493086504967,
-0.692111551008754));
#84053=CARTESIAN_POINT('Ctrl Pts',(0.0570588448093164,0.18728309976618,
-0.692806687444373));
#84054=CARTESIAN_POINT('Ctrl Pts',(0.068510120264012,0.182995965587798,
-0.693501823879992));
#84055=CARTESIAN_POINT('Ctrl Pts',(0.0799608016590144,0.178709053813778,
-0.694196924253904));
#84056=CARTESIAN_POINT('Ctrl Pts',(0.0910019828272812,0.173345437645973,
-0.694892024627817));
#84057=CARTESIAN_POINT('Ctrl Pts',(0.101429639641313,0.167012539056903,
-0.695587125001729));
#84058=CARTESIAN_POINT('Ctrl Pts',(0.111881119264334,0.160665172458755,
-0.696283813387573));
#84059=CARTESIAN_POINT('Ctrl Pts',(0.121715563002558,0.153344612420341,
-0.696980501773416));
#84060=CARTESIAN_POINT('Ctrl Pts',(0.130758432397035,0.145201213345723,
-0.69767719015926));
#84061=CARTESIAN_POINT('Ctrl Pts',(0.133562048138837,0.142676465852265,
-0.697893188692521));
#84062=CARTESIAN_POINT('Ctrl Pts',(0.136289839376129,0.140072897291044,
-0.698109187225783));
#84063=CARTESIAN_POINT('Ctrl Pts',(0.138937356130358,0.137395673408976,
-0.698325185759044));
#84064=CARTESIAN_POINT('Ctrl Pts',(0.147476710724727,0.128760500837933,
-0.699021871838344));
#84065=CARTESIAN_POINT('Ctrl Pts',(0.15523792299337,0.119295879165266,-0.699718557917643));
#84066=CARTESIAN_POINT('Ctrl Pts',(0.162061162106512,0.109166568768497,
-0.700415243996942));
#84067=CARTESIAN_POINT('Ctrl Pts',(0.168870164558155,0.0990583931379199,
-0.701110476443485));
#84068=CARTESIAN_POINT('Ctrl Pts',(0.174744533221545,0.0882889588215705,
-0.701805708890027));
#84069=CARTESIAN_POINT('Ctrl Pts',(0.179565123563313,0.0770553463407453,
-0.70250094133657));
#84070=CARTESIAN_POINT('Ctrl Pts',(0.184385048192392,0.0658232851965483,
-0.703196077773075));
#84071=CARTESIAN_POINT('Ctrl Pts',(0.188151097207593,0.0541279581078693,
-0.70389121420958));
#84072=CARTESIAN_POINT('Ctrl Pts',(0.19079113664295,0.0421888869074672,
-0.704586350646084));
#84073=CARTESIAN_POINT('Ctrl Pts',(0.193431039120533,0.0302504350722879,
-0.705281451020878));
#84074=CARTESIAN_POINT('Ctrl Pts',(0.194944885479764,0.0180691244063143,
-0.705976551395672));
#84075=CARTESIAN_POINT('Ctrl Pts',(0.19531167246024,0.00587457239158232,
-0.706671651770466));
#84076=CARTESIAN_POINT('Ctrl Pts',(0.19567929739465,-0.00634783904393062,
-0.707368340157169));
#84077=CARTESIAN_POINT('Ctrl Pts',(0.194894670464553,-0.0185826763482537,
-0.708065028543872));
#84078=CARTESIAN_POINT('Ctrl Pts',(0.192988853477866,-0.0306016737009374,
-0.708761716930575));
#84079=CARTESIAN_POINT('Ctrl Pts',(0.192397981470756,-0.0343279963955332,
-0.708977715459425));
#84080=CARTESIAN_POINT('Ctrl Pts',(0.191699709787446,-0.0380336448360147,
-0.709193713988275));
#84081=CARTESIAN_POINT('Ctrl Pts',(0.190895947856836,-0.0417120736938359,
-0.709409712517125));
#84082=CARTESIAN_POINT('Ctrl Pts',(0.188303477667904,-0.0535765534518853,
-0.710106398594895));
#84083=CARTESIAN_POINT('Ctrl Pts',(0.184591587771128,-0.0652400585887095,
-0.710803084672665));
#84084=CARTESIAN_POINT('Ctrl Pts',(0.179811431707822,-0.0764788142375607,
-0.711499770750434));
#84085=CARTESIAN_POINT('Ctrl Pts',(0.175041249421265,-0.0876941202671337,
-0.712195003195454));
#84086=CARTESIAN_POINT('Ctrl Pts',(0.169207496290184,-0.0984856098079502,
-0.712890235640474));
#84087=CARTESIAN_POINT('Ctrl Pts',(0.162410589384586,-0.108646032857861,
-0.713585468085493));
#84088=CARTESIAN_POINT('Ctrl Pts',(0.155614621116236,-0.118805052776662,
-0.714280604520508));
#84089=CARTESIAN_POINT('Ctrl Pts',(0.147856211198137,-0.128332427854005,
-0.714975740955522));
#84090=CARTESIAN_POINT('Ctrl Pts',(0.139280198443431,-0.137048116811427,
-0.715670877390536));
#84091=CARTESIAN_POINT('Ctrl Pts',(0.130704630587781,-0.14576335362379,
-0.716365977763857));
#84092=CARTESIAN_POINT('Ctrl Pts',(0.121312177063685,-0.153666383203982,
-0.717061078137178));
#84093=CARTESIAN_POINT('Ctrl Pts',(0.111283987381547,-0.16061455149663,
-0.717756178510498));
#84094=CARTESIAN_POINT('Ctrl Pts',(0.101232887504312,-0.167578593431102,
-0.71845286689578));
#84095=CARTESIAN_POINT('Ctrl Pts',(0.0905439078716308,-0.173582974921055,
-0.719149555281062));
#84096=CARTESIAN_POINT('Ctrl Pts',(0.0794254163071088,-0.178529446435154,
-0.719846243666344));
#84097=CARTESIAN_POINT('Ctrl Pts',(0.0759782827616286,-0.180063031075576,
-0.720062242202631));
#84098=CARTESIAN_POINT('Ctrl Pts',(0.0724900049008866,-0.181495278347787,
-0.720278240738918));
#84099=CARTESIAN_POINT('Ctrl Pts',(0.0689671122597918,-0.182824225491441,
-0.720494239275204));
#84100=CARTESIAN_POINT('Ctrl Pts',(0.0576043025921026,-0.187110638672362,
-0.721190925352916));
#84101=CARTESIAN_POINT('Ctrl Pts',(0.045800477050706,-0.19034872162001,
-0.721887611430628));
#84102=CARTESIAN_POINT('Ctrl Pts',(0.033771177704092,-0.192459521864933,
-0.72258429750834));
#84103=CARTESIAN_POINT('Ctrl Pts',(0.021766977443515,-0.194565917933401,
-0.723279529953276));
#84104=CARTESIAN_POINT('Ctrl Pts',(0.00953907767813231,-0.19554947746548,
-0.723974762398212));
#84105=CARTESIAN_POINT('Ctrl Pts',(-0.00268401299032918,-0.195381565338872,
-0.724669994843147));
#84106=CARTESIAN_POINT('Ctrl Pts',(-0.0149054156773831,-0.195213676400551,
-0.725365131278042));
#84107=CARTESIAN_POINT('Ctrl Pts',(-0.0271211364012227,-0.193894598142963,
-0.726060267712936));
#84108=CARTESIAN_POINT('Ctrl Pts',(-0.0391012974787524,-0.191447769732317,
-0.72675540414783));
#84109=CARTESIAN_POINT('Ctrl Pts',(-0.0510808370593697,-0.189001068256216,
-0.72745050452101));
#84110=CARTESIAN_POINT('Ctrl Pts',(-0.0628239893884408,-0.185426934365536,
-0.72814560489419));
#84111=CARTESIAN_POINT('Ctrl Pts',(-0.0741124615666403,-0.180799621240016,
-0.72884070526737));
#84112=CARTESIAN_POINT('Ctrl Pts',(-0.0854267231548624,-0.176161736650651,
-0.729537393652484));
#84113=CARTESIAN_POINT('Ctrl Pts',(-0.0962834466948086,-0.170466261552371,
-0.730234082037597));
#84114=CARTESIAN_POINT('Ctrl Pts',(-0.106486760934479,-0.163834458358683,
-0.730930770422711));
#84115=CARTESIAN_POINT('Ctrl Pts',(-0.10965015649836,-0.161778360084078,
-0.731146768959569));
#84116=CARTESIAN_POINT('Ctrl Pts',(-0.112750962585627,-0.159632569700436,
-0.731362767496427));
#84117=CARTESIAN_POINT('Ctrl Pts',(-0.115783977319435,-0.157401494897896,
-0.731578766033286));
#84118=CARTESIAN_POINT('Ctrl Pts',(-0.125482540042977,-0.150267266807228,
-0.732269456828343));
#84119=CARTESIAN_POINT('Ctrl Pts',(-0.134556120011492,-0.1422059751907,
-0.7329601476234));
#84120=CARTESIAN_POINT('Ctrl Pts',(-0.142822838970763,-0.133352152844758,
-0.733650838418457));
#84121=CARTESIAN_POINT('Ctrl Pts',(-0.15116326841965,-0.124419385081255,
-0.734347687782219));
#84122=CARTESIAN_POINT('Ctrl Pts',(-0.158681612033931,-0.114680408755922,
-0.735044537145981));
#84123=CARTESIAN_POINT('Ctrl Pts',(-0.165226227850539,-0.104314206272596,
-0.735741386509744));
#84124=CARTESIAN_POINT('Ctrl Pts',(-0.17169835600434,-0.0940628190528786,
-0.736430517623402));
#84125=CARTESIAN_POINT('Ctrl Pts',(-0.177217764800105,-0.0831988186608179,
-0.73711964873706));
#84126=CARTESIAN_POINT('Ctrl Pts',(-0.181680927325022,-0.0719249653897735,
-0.737808779850718));
#84127=CARTESIAN_POINT('Ctrl Pts',(-0.186219070801908,-0.0604617118345347,
-0.738509488339532));
#84128=CARTESIAN_POINT('Ctrl Pts',(-0.189664727549586,-0.0485755602974442,
-0.739210196828347));
#84129=CARTESIAN_POINT('Ctrl Pts',(-0.191961028025369,-0.0364982700883675,
-0.739910905317161));
#84130=CARTESIAN_POINT('Ctrl Pts',(-0.194257328501152,-0.0244209798792907,
-0.740611613805975));
#84131=CARTESIAN_POINT('Ctrl Pts',(-0.195404222307629,-0.012153512645485,
-0.74131232229479));
#84132=CARTESIAN_POINT('Ctrl Pts',(-0.195399988273324,6.76962695950502E-5,
-0.742013030783604));
#84133=CARTESIAN_POINT('',(-0.195399921197426,-0.00017548800484569,-0.812013030784603));
#84134=CARTESIAN_POINT('Ctrl Pts',(-0.1953999882733,6.76963388894689E-5,
-0.742013030787577));
#84135=CARTESIAN_POINT('Ctrl Pts',(-0.195398678534898,0.00384814994386311,
-0.742229784788839));
#84136=CARTESIAN_POINT('Ctrl Pts',(-0.195287664303936,0.00762655792512721,
-0.742446538790102));
#84137=CARTESIAN_POINT('Ctrl Pts',(-0.195067254895793,0.0113985116317773,
-0.742663292791365));
#84138=CARTESIAN_POINT('Ctrl Pts',(-0.194358819693395,0.0235222445074034,
-0.743359978863201));
#84139=CARTESIAN_POINT('Ctrl Pts',(-0.192513314931336,0.0356222275051059,
-0.744056664935038));
#84140=CARTESIAN_POINT('Ctrl Pts',(-0.189546331861466,0.0474694436228498,
-0.744753351006874));
#84141=CARTESIAN_POINT('Ctrl Pts',(-0.186585539389951,0.0592919405713621,
-0.745448583445996));
#84142=CARTESIAN_POINT('Ctrl Pts',(-0.182508052018168,0.0708618591793415,
-0.746143815885119));
#84143=CARTESIAN_POINT('Ctrl Pts',(-0.1773807002981,0.0819588138137424,
-0.746839048324241));
#84144=CARTESIAN_POINT('Ctrl Pts',(-0.172254056652507,0.0930542359864036,
-0.747534184753499));
#84145=CARTESIAN_POINT('Ctrl Pts',(-0.166078161760922,0.103676011751318,
-0.748229321182757));
#84146=CARTESIAN_POINT('Ctrl Pts',(-0.158967970989733,0.113623695589465,
-0.748924457612014));
#84147=CARTESIAN_POINT('Ctrl Pts',(-0.151858149074166,0.123570863371261,
-0.749619557979654));
#84148=CARTESIAN_POINT('Ctrl Pts',(-0.143814658298944,0.13284331254129,
-0.750314658347294));
#84149=CARTESIAN_POINT('Ctrl Pts',(-0.134994156289213,0.141271857663738,
-0.751009758714934));
#84150=CARTESIAN_POINT('Ctrl Pts',(-0.126153503139833,0.149719658469096,
-0.751706447094748));
#84151=CARTESIAN_POINT('Ctrl Pts',(-0.11653297221146,0.157319149566077,
-0.752403135474563));
#84152=CARTESIAN_POINT('Ctrl Pts',(-0.106323038009839,0.163940756337033,
-0.753099823854378));
#84153=CARTESIAN_POINT('Ctrl Pts',(-0.103157589582081,0.165993693635985,
-0.7533158224194));
#84154=CARTESIAN_POINT('Ctrl Pts',(-0.0999356808215271,0.167952959412892,
-0.753531820984422));
#84155=CARTESIAN_POINT('Ctrl Pts',(-0.0966634547837876,0.169815595600824,
-0.753747819549444));
#84156=CARTESIAN_POINT('Ctrl Pts',(-0.0861091517251182,0.17582337947295,
-0.75444450562467));
#84157=CARTESIAN_POINT('Ctrl Pts',(-0.0749555780612429,0.180864537255721,
-0.755141191699895));
#84158=CARTESIAN_POINT('Ctrl Pts',(-0.0634033071758778,0.184827434757834,
-0.75583787777512));
#84159=CARTESIAN_POINT('Ctrl Pts',(-0.0518751400605106,0.188782063689129,
-0.756533110217455));
#84160=CARTESIAN_POINT('Ctrl Pts',(-0.0399507223910989,0.19166254699148,
-0.75722834265979));
#84161=CARTESIAN_POINT('Ctrl Pts',(-0.0278512904924889,0.193404926560579,
-0.757923575102125));
#84162=CARTESIAN_POINT('Ctrl Pts',(-0.0157535295004372,0.195147065510658,
-0.758618711534295));
#84163=CARTESIAN_POINT('Ctrl Pts',(-0.00348166052095019,0.195751243336099,
-0.759313847966465));
#84164=CARTESIAN_POINT('Ctrl Pts',(0.0087335981420215,0.195204723978427,
-0.760008984398636));
#84165=CARTESIAN_POINT('Ctrl Pts',(0.0209482231105826,0.194658232972693,
-0.760704084769018));
#84166=CARTESIAN_POINT('Ctrl Pts',(0.0331053707006321,0.192961229423343,
-0.7613991851394));
#84167=CARTESIAN_POINT('Ctrl Pts',(0.0449778324117177,0.190152976814836,
-0.762094285509782));
#84168=CARTESIAN_POINT('Ctrl Pts',(0.0568774177024041,0.187338308530707,
-0.762790973892043));
#84169=CARTESIAN_POINT('Ctrl Pts',(0.0684901829337995,0.183407587835583,
-0.763487662274304));
#84170=CARTESIAN_POINT('Ctrl Pts',(0.0796037273880817,0.178450011448372,
-0.764184350656565));
#84171=CARTESIAN_POINT('Ctrl Pts',(0.0830493273897015,0.176912983790087,
-0.764400349206885));
#84172=CARTESIAN_POINT('Ctrl Pts',(0.0864471078133341,0.175277592480136,
-0.764616347757206));
#84173=CARTESIAN_POINT('Ctrl Pts',(0.0897912424479248,0.173547379063062,
-0.764832346307526));
#84174=CARTESIAN_POINT('Ctrl Pts',(0.100577482201028,0.167966713575625,
-0.765529032417583));
#84175=CARTESIAN_POINT('Ctrl Pts',(0.110879316957741,0.161357046962324,
-0.766225718527639));
#84176=CARTESIAN_POINT('Ctrl Pts',(0.120493893810033,0.153825815630851,
-0.766922404637696));
#84177=CARTESIAN_POINT('Ctrl Pts',(0.130088409888116,0.14631029818191,-0.767617637115111));
#84178=CARTESIAN_POINT('Ctrl Pts',(0.138997786808178,0.137877508735213,
-0.768312869592525));
#84179=CARTESIAN_POINT('Ctrl Pts',(0.147047906989292,0.128678176277365,
-0.76900810206994));
#84180=CARTESIAN_POINT('Ctrl Pts',(0.155096915463461,0.119480114230585,
-0.769703238537015));
#84181=CARTESIAN_POINT('Ctrl Pts',(0.162286293315973,0.109516346921563,
-0.77039837500409));
#84182=CARTESIAN_POINT('Ctrl Pts',(0.168479720973745,0.0989734490689751,
-0.771093511471166));
#84183=CARTESIAN_POINT('Ctrl Pts',(0.174672827332737,0.0884310981542712,
-0.771788611876384));
#84184=CARTESIAN_POINT('Ctrl Pts',(0.179869666201818,0.0773104444712772,
-0.772483712281603));
#84185=CARTESIAN_POINT('Ctrl Pts',(0.183979442788537,0.065823435273613,
-0.773178812686822));
#84186=CARTESIAN_POINT('Ctrl Pts',(0.188098608480714,0.0543101831066573,
-0.773875501103182));
#84187=CARTESIAN_POINT('Ctrl Pts',(0.191125521016396,0.0424297497631005,
-0.774572189519542));
#84188=CARTESIAN_POINT('Ctrl Pts',(0.19301932961613,0.0304088538840238,
-0.775268877935902));
#84189=CARTESIAN_POINT('Ctrl Pts',(0.193606478151208,0.0266819453639537,
-0.77548487631247));
#84190=CARTESIAN_POINT('Ctrl Pts',(0.194085086310145,0.0229415806826977,
-0.775700874689037));
#84191=CARTESIAN_POINT('Ctrl Pts',(0.194454951830309,0.0191945749802449,
-0.775916873065605));
#84192=CARTESIAN_POINT('Ctrl Pts',(0.195647924404063,0.00710889844909368,
-0.776613559091126));
#84193=CARTESIAN_POINT('Ctrl Pts',(0.195714061909135,-0.00513083536851569,
-0.777310245116648));
#84194=CARTESIAN_POINT('Ctrl Pts',(0.194633010957284,-0.0172959835135673,
-0.778006931142169));
#84195=CARTESIAN_POINT('Ctrl Pts',(0.193554215613781,-0.0294357491272439,
-0.778702163535175));
#84196=CARTESIAN_POINT('Ctrl Pts',(0.191332986002734,-0.0415003685242515,
-0.779397395928181));
#84197=CARTESIAN_POINT('Ctrl Pts',(0.188000927272401,-0.053261724950639,
-0.780092628321187));
#84198=CARTESIAN_POINT('Ctrl Pts',(0.184669328686416,-0.0650214571794575,
-0.780787764705304));
#84199=CARTESIAN_POINT('Ctrl Pts',(0.180227400023203,-0.0764771566544016,
-0.781482901089421));
#84200=CARTESIAN_POINT('Ctrl Pts',(0.17475739415817,-0.0874128891356764,
-0.782178037473538));
#84201=CARTESIAN_POINT('Ctrl Pts',(0.169287672056742,-0.0983480543117332,
-0.782873137796559));
#84202=CARTESIAN_POINT('Ctrl Pts',(0.162790394247606,-0.108762535603792,
-0.78356823811958));
#84203=CARTESIAN_POINT('Ctrl Pts',(0.155393884766881,-0.118464765128949,
-0.784263338442601));
#84204=CARTESIAN_POINT('Ctrl Pts',(0.147980477353117,-0.128189160193849,
-0.784960026779367));
#84205=CARTESIAN_POINT('Ctrl Pts',(0.139664319068716,-0.13719739936423,
-0.785656715116132));
#84206=CARTESIAN_POINT('Ctrl Pts',(0.13061332010973,-0.1453317604996,-0.786353403452897));
#84207=CARTESIAN_POINT('Ctrl Pts',(0.127807180373147,-0.147853709084183,
-0.78656940224316));
#84208=CARTESIAN_POINT('Ctrl Pts',(0.124930648719368,-0.150291948941695,
-0.786785401033423));
#84209=CARTESIAN_POINT('Ctrl Pts',(0.121989331094927,-0.152642599227779,
-0.787001399823686));
#84210=CARTESIAN_POINT('Ctrl Pts',(0.112502356527963,-0.160224425581584,
-0.787698085898216));
#84211=CARTESIAN_POINT('Ctrl Pts',(0.102272552464107,-0.166945034456582,
-0.788394771972746));
#84212=CARTESIAN_POINT('Ctrl Pts',(0.0914806049602737,-0.172662847526914,
-0.789091458047276));
#84213=CARTESIAN_POINT('Ctrl Pts',(0.0807111748267906,-0.178368730395172,
-0.789786690488127));
#84214=CARTESIAN_POINT('Ctrl Pts',(0.06938266028967,-0.183075499694555,
-0.790481922928977));
#84215=CARTESIAN_POINT('Ctrl Pts',(0.0577036000417347,-0.18668544276998,
-0.791177155369828));
#84216=CARTESIAN_POINT('Ctrl Pts',(0.0460261526663467,-0.19029488731402,
-0.791872291799416));
#84217=CARTESIAN_POINT('Ctrl Pts',(0.0339990769748144,-0.192807505017742,
-0.792567428229004));
#84218=CARTESIAN_POINT('Ctrl Pts',(0.0218482740129643,-0.194174696916602,
-0.793262564658592));
#84219=CARTESIAN_POINT('Ctrl Pts',(0.00969810141288971,-0.195541817888009,
-0.793957665025755));
#84220=CARTESIAN_POINT('Ctrl Pts',(-0.00257491320132761,-0.195763560068986,
-0.794652765392917));
#84221=CARTESIAN_POINT('Ctrl Pts',(-0.0147402175345476,-0.19484323438866,
-0.795347865760079));
#84222=CARTESIAN_POINT('Ctrl Pts',(-0.0269333144546391,-0.193920806152515,
-0.796044554138261));
#84223=CARTESIAN_POINT('Ctrl Pts',(-0.0390173429669599,-0.191851232420075,
-0.796741242516443));
#84224=CARTESIAN_POINT('Ctrl Pts',(-0.0507685815630807,-0.188689456849271,
-0.797437930894624));
#84225=CARTESIAN_POINT('Ctrl Pts',(-0.0544118899954307,-0.18770919221554,
-0.797653929457005));
#84226=CARTESIAN_POINT('Ctrl Pts',(-0.058023321427186,-0.186624304545733,
-0.797869928019385));
#84227=CARTESIAN_POINT('Ctrl Pts',(-0.0615965681883146,-0.185437382389372,
-0.798085926581765));
#84228=CARTESIAN_POINT('Ctrl Pts',(-0.073121793005532,-0.181609058848606,
-0.798782612861233));
#84229=CARTESIAN_POINT('Ctrl Pts',(-0.0843291966479146,-0.176688726846239,
-0.7994792991407));
#84230=CARTESIAN_POINT('Ctrl Pts',(-0.0950016407521072,-0.17075083676049,
-0.800175985420167));
#84231=CARTESIAN_POINT('Ctrl Pts',(-0.105651816866004,-0.164825336046615,
-0.800871218067911));
#84232=CARTESIAN_POINT('Ctrl Pts',(-0.115768456042509,-0.157886848105303,
-0.801566450715655));
#84233=CARTESIAN_POINT('Ctrl Pts',(-0.125156044212862,-0.150057071132913,
-0.8022616833634));
#84234=CARTESIAN_POINT('Ctrl Pts',(-0.13454233595766,-0.142228375452412,
-0.802956819999543));
#84235=CARTESIAN_POINT('Ctrl Pts',(-0.143199076614239,-0.133509159851367,
-0.803651956635686));
#84236=CARTESIAN_POINT('Ctrl Pts',(-0.150962490541431,-0.124062429645434,
-0.80434709327183));
#84237=CARTESIAN_POINT('Ctrl Pts',(-0.158725501716818,-0.114616189518696,
-0.805042193845547));
#84238=CARTESIAN_POINT('Ctrl Pts',(-0.165594743530101,-0.104443202878264,
-0.805737294419265));
#84239=CARTESIAN_POINT('Ctrl Pts',(-0.171447445837107,-0.093738643663818,
-0.806432394992983));
#84240=CARTESIAN_POINT('Ctrl Pts',(-0.177313519063283,-0.0830096291142981,
-0.807129083573933));
#84241=CARTESIAN_POINT('Ctrl Pts',(-0.182158054466896,-0.0717474160740974,
-0.807825772154882));
#84242=CARTESIAN_POINT('Ctrl Pts',(-0.185905307464628,-0.0601695658658265,
-0.808522460735831));
#84243=CARTESIAN_POINT('Ctrl Pts',(-0.187067085382959,-0.0565800322202864,
-0.808738458270502));
#84244=CARTESIAN_POINT('Ctrl Pts',(-0.188123755338865,-0.0529602626463094,
-0.808954455805174));
#84245=CARTESIAN_POINT('Ctrl Pts',(-0.189074053603399,-0.0493169570632572,
-0.809170453339845));
#84246=CARTESIAN_POINT('Ctrl Pts',(-0.192997021238052,-0.03427686868377,
-0.810062122165628));
#84247=CARTESIAN_POINT('Ctrl Pts',(-0.195125884706412,-0.0187503439611592,
-0.810953790991411));
#84248=CARTESIAN_POINT('Ctrl Pts',(-0.195375169370054,-0.00311499496350872,
-0.811845459817194));
#84249=CARTESIAN_POINT('Ctrl Pts',(-0.195390785359249,-0.00213554665955173,
-0.81190131680633));
#84250=CARTESIAN_POINT('Ctrl Pts',(-0.195399040891236,-0.00115567898833329,
-0.811957173795467));
#84251=CARTESIAN_POINT('Ctrl Pts',(-0.195399921197426,-0.00017548800484569,
-0.812013030784603));
#84252=CARTESIAN_POINT('',(-0.195379220633989,7.37186862735708E-5,-0.882013034935241));
#84253=CARTESIAN_POINT('Ctrl Pts',(-0.195399921197473,-0.000175487952656256,
-0.812013030787577));
#84254=CARTESIAN_POINT('Ctrl Pts',(-0.19541076648611,0.0119003754503791,
-0.812701183792726));
#84255=CARTESIAN_POINT('Ctrl Pts',(-0.19429783114136,0.0240036113255929,
-0.813389336797875));
#84256=CARTESIAN_POINT('Ctrl Pts',(-0.192072370349911,0.0359077226814327,
-0.814077489803025));
#84257=CARTESIAN_POINT('Ctrl Pts',(-0.18984883478061,0.0478015359188242,
-0.814765047494425));
#84258=CARTESIAN_POINT('Ctrl Pts',(-0.186514832957703,0.059495682482877,
-0.815452605185825));
#84259=CARTESIAN_POINT('Ctrl Pts',(-0.182133079421123,0.070772179425102,
-0.816140162877225));
#84260=CARTESIAN_POINT('Ctrl Pts',(-0.177740715773814,0.0820759816185671,
-0.816829385441645));
#84261=CARTESIAN_POINT('Ctrl Pts',(-0.172295871312637,0.0929592772620382,
-0.817518608006064));
#84262=CARTESIAN_POINT('Ctrl Pts',(-0.16590985247905,0.103223451067962,
-0.818207830570483));
#84263=CARTESIAN_POINT('Ctrl Pts',(-0.159587204270127,0.113385770005823,
-0.818890213746297));
#84264=CARTESIAN_POINT('Ctrl Pts',(-0.152342595762826,0.122940581824888,
-0.819572596922112));
#84265=CARTESIAN_POINT('Ctrl Pts',(-0.144323676122428,0.131726369837283,
-0.820254980097926));
#84266=CARTESIAN_POINT('Ctrl Pts',(-0.136136676912347,0.140696311268674,
-0.820951666281588));
#84267=CARTESIAN_POINT('Ctrl Pts',(-0.127081505453031,0.14893156321025,
-0.821648352465251));
#84268=CARTESIAN_POINT('Ctrl Pts',(-0.117314529548643,0.156264075067754,
-0.822345038648913));
#84269=CARTESIAN_POINT('Ctrl Pts',(-0.107567932485336,0.16358128760484,
-0.823040271193582));
#84270=CARTESIAN_POINT('Ctrl Pts',(-0.0971131273755955,0.169998919590237,
-0.823735503738251));
#84271=CARTESIAN_POINT('Ctrl Pts',(-0.0861408413320165,0.175387899966367,
-0.82443073628292));
#84272=CARTESIAN_POINT('Ctrl Pts',(-0.0751700706993675,0.180776136056418,
-0.825125872807216));
#84273=CARTESIAN_POINT('Ctrl Pts',(-0.0636827251959411,0.185135576734265,
-0.825821009331513));
#84274=CARTESIAN_POINT('Ctrl Pts',(-0.0518943488922855,0.188382951864137,
-0.826516145855809));
#84275=CARTESIAN_POINT('Ctrl Pts',(-0.0401065842361512,0.191630158501852,
-0.827211246312497));
#84276=CARTESIAN_POINT('Ctrl Pts',(-0.0280186705253376,0.193765207842195,
-0.827906346769186));
#84277=CARTESIAN_POINT('Ctrl Pts',(-0.0158588500843532,0.194755377009216,
-0.828601447225874));
#84278=CARTESIAN_POINT('Ctrl Pts',(-0.0036712497476722,0.195747808281696,
-0.829298135684481));
#84279=CARTESIAN_POINT('Ctrl Pts',(0.00858770854901134,0.195590132007127,
-0.829994824143088));
#84280=CARTESIAN_POINT('Ctrl Pts',(0.0206884687465203,0.194301691348594,
-0.830691512601694));
#84281=CARTESIAN_POINT('Ctrl Pts',(0.0244401327717179,0.193902229133962,
-0.830907510686465));
#84282=CARTESIAN_POINT('Ctrl Pts',(0.0281766441647945,0.193394450641261,
-0.831123508771235));
#84283=CARTESIAN_POINT('Ctrl Pts',(0.0318913685240223,0.192779927932513,
-0.831339506856005));
#84284=CARTESIAN_POINT('Ctrl Pts',(0.0438729625033843,0.190797826200248,
-0.8320361941743));
#84285=CARTESIAN_POINT('Ctrl Pts',(0.0557111120044502,0.18768748499762,
-0.832732881492595));
#84286=CARTESIAN_POINT('Ctrl Pts',(0.0671797176113246,0.18348854335261,
-0.83342956881089));
#84287=CARTESIAN_POINT('Ctrl Pts',(0.0786243942018095,0.179298362715423,
-0.83412480250502));
#84288=CARTESIAN_POINT('Ctrl Pts',(0.0897002184680624,0.174024318521112,
-0.834820036199149));
#84289=CARTESIAN_POINT('Ctrl Pts',(0.100195074047842,0.167756094186016,
-0.835515269893279));
#84290=CARTESIAN_POINT('Ctrl Pts',(0.110688480214663,0.161488735536542,
-0.836210407570773));
#84291=CARTESIAN_POINT('Ctrl Pts',(0.120600303685354,0.154227878369273,
-0.836905545248266));
#84292=CARTESIAN_POINT('Ctrl Pts',(0.129743328677118,0.146108961613521,
-0.83760068292576));
#84293=CARTESIAN_POINT('Ctrl Pts',(0.138885879320792,0.137990466074233,
-0.838295784538906));
#84294=CARTESIAN_POINT('Ctrl Pts',(0.147259074374735,0.129014600520134,
-0.838990886152053));
#84295=CARTESIAN_POINT('Ctrl Pts',(0.154711178707542,0.119354979715649,
-0.839685987765199));
#84296=CARTESIAN_POINT('Ctrl Pts',(0.162180307648888,0.10967329114943,-0.840382677363742));
#84297=CARTESIAN_POINT('Ctrl Pts',(0.168723662724559,0.0993054610685011,
-0.841079366962286));
#84298=CARTESIAN_POINT('Ctrl Pts',(0.174232462703801,0.0884545586172281,
-0.841776056560829));
#84299=CARTESIAN_POINT('Ctrl Pts',(0.175940337576147,0.0850904895443564,
-0.841992048911915));
#84300=CARTESIAN_POINT('Ctrl Pts',(0.177549118335746,0.0816801484068674,
-0.842208041263));
#84301=CARTESIAN_POINT('Ctrl Pts',(0.179056510935435,0.078229955206612,
-0.842424033614086));
#84302=CARTESIAN_POINT('Ctrl Pts',(0.183918604355241,0.067101360267584,
-0.843120716740406));
#84303=CARTESIAN_POINT('Ctrl Pts',(0.18775631155332,0.055478697225224,-0.843817399866725));
#84304=CARTESIAN_POINT('Ctrl Pts',(0.190479756283891,0.0435731849424565,
-0.844514082993045));
#84305=CARTESIAN_POINT('Ctrl Pts',(0.193197518552431,0.0316925134874612,
-0.845209312491403));
#84306=CARTESIAN_POINT('Ctrl Pts',(0.194805367887041,0.0195309922381451,
-0.84590454198976));
#84307=CARTESIAN_POINT('Ctrl Pts',(0.195263016082719,0.00731536398820651,
-0.846599771488118));
#84308=CARTESIAN_POINT('Ctrl Pts',(0.195720601111664,-0.00489857820389136,
-0.847294905027666));
#84309=CARTESIAN_POINT('Ctrl Pts',(0.195028222143748,-0.01716574122849,
-0.847990038567214));
#84310=CARTESIAN_POINT('Ctrl Pts',(0.19319752702589,-0.0292553508110982,
-0.848685172106763));
#84311=CARTESIAN_POINT('Ctrl Pts',(0.191366926808907,-0.0413443336839361,
-0.849380269611484));
#84312=CARTESIAN_POINT('Ctrl Pts',(0.188398285339225,-0.0532549203161764,
-0.850075367116206));
#84313=CARTESIAN_POINT('Ctrl Pts',(0.184354590604969,-0.0647653064755681,
-0.850770464620928));
#84314=CARTESIAN_POINT('Ctrl Pts',(0.180301657159965,-0.0763019906458915,
-0.851467150228909));
#84315=CARTESIAN_POINT('Ctrl Pts',(0.175169118484121,-0.0874358457666871,
-0.852163835836891));
#84316=CARTESIAN_POINT('Ctrl Pts',(0.169068057282984,-0.0979650550275846,
-0.852860521444872));
#84317=CARTESIAN_POINT('Ctrl Pts',(0.167176374190521,-0.101229721038824,
-0.853076534420637));
#84318=CARTESIAN_POINT('Ctrl Pts',(0.165191901970452,-0.104436460480499,
-0.853292547396402));
#84319=CARTESIAN_POINT('Ctrl Pts',(0.163118777296953,-0.107579851706289,
-0.853508560372167));
#84320=CARTESIAN_POINT('Ctrl Pts',(0.156432510105898,-0.117717955743309,
-0.854205248078005));
#84321=CARTESIAN_POINT('Ctrl Pts',(0.148774015022097,-0.127265912653565,
-0.854901935783844));
#84322=CARTESIAN_POINT('Ctrl Pts',(0.140271507458899,-0.136033320165348,
-0.855598623489683));
#84323=CARTESIAN_POINT('Ctrl Pts',(0.13178674080447,-0.144782434041324,
-0.856293857521656));
#84324=CARTESIAN_POINT('Ctrl Pts',(0.122462007313727,-0.152753557937461,
-0.85698909155363));
#84325=CARTESIAN_POINT('Ctrl Pts',(0.112465545786131,-0.159789427093997,
-0.857684325585604));
#84326=CARTESIAN_POINT('Ctrl Pts',(0.102470465927083,-0.166824323782515,
-0.858379463525276));
#84327=CARTESIAN_POINT('Ctrl Pts',(0.0918045306694918,-0.17292368243484,
-0.859074601464948));
#84328=CARTESIAN_POINT('Ctrl Pts',(0.0806676418023429,-0.177971603257511,
-0.859769739404621));
#84329=CARTESIAN_POINT('Ctrl Pts',(0.0695313314239663,-0.183019261873604,
-0.860464841236409));
#84330=CARTESIAN_POINT('Ctrl Pts',(0.0579249240961688,-0.187015254500705,
-0.861159943068197));
#84331=CARTESIAN_POINT('Ctrl Pts',(0.0460687555565446,-0.18989162635954,
-0.861855044899985));
#84332=CARTESIAN_POINT('Ctrl Pts',(0.034185502306362,-0.192774569118494,
-0.862551734650489));
#84333=CARTESIAN_POINT('Ctrl Pts',(0.0220522138573652,-0.194532642413946,
-0.863248424400992));
#84334=CARTESIAN_POINT('Ctrl Pts',(0.00989865210069558,-0.195149113978489,
-0.863945114151496));
#84335=CARTESIAN_POINT('Ctrl Pts',(0.00613074842564256,-0.195340235356742,
-0.864161105144413));
#84336=CARTESIAN_POINT('Ctrl Pts',(0.00236090170122731,-0.195422010120875,
-0.864377096137329));
#84337=CARTESIAN_POINT('Ctrl Pts',(-0.00140409027209528,-0.195394955233004,
-0.864593087130246));
#84338=CARTESIAN_POINT('Ctrl Pts',(-0.0135483239942191,-0.195307687880524,
-0.865289780541132));
#84339=CARTESIAN_POINT('Ctrl Pts',(-0.0257270041931643,-0.194083600023529,
-0.865986473952018));
#84340=CARTESIAN_POINT('Ctrl Pts',(-0.0377106119642735,-0.191726549401172,
-0.866683167362904));
#84341=CARTESIAN_POINT('Ctrl Pts',(-0.0496692174156106,-0.189374416474262,
-0.867378407208905));
#84342=CARTESIAN_POINT('Ctrl Pts',(-0.0614326940351443,-0.185894107403963,
-0.868073647054907));
#84343=CARTESIAN_POINT('Ctrl Pts',(-0.0727775223520668,-0.181341093633777,
-0.868768886900908));
#84344=CARTESIAN_POINT('Ctrl Pts',(-0.0841207837437583,-0.176788708716841,
-0.869464030721759));
#84345=CARTESIAN_POINT('Ctrl Pts',(-0.0950446839703465,-0.17116419653728,
-0.870159174542609));
#84346=CARTESIAN_POINT('Ctrl Pts',(-0.105343155999477,-0.16457211028625,
-0.870854318363459));
#84347=CARTESIAN_POINT('Ctrl Pts',(-0.115641093753242,-0.157980366026662,
-0.87154942612088));
#84348=CARTESIAN_POINT('Ctrl Pts',(-0.125312945390698,-0.150421641829479,
-0.872244533878301));
#84349=CARTESIAN_POINT('Ctrl Pts',(-0.134181729704214,-0.142043737678171,
-0.872939641635722));
#84350=CARTESIAN_POINT('Ctrl Pts',(-0.143070773483751,-0.133646695406184,
-0.873636337267139));
#84351=CARTESIAN_POINT('Ctrl Pts',(-0.151152496979953,-0.124427385289625,
-0.874333032898556));
#84352=CARTESIAN_POINT('Ctrl Pts',(-0.158287747857834,-0.114569406379255,
-0.875029728529974));
#84353=CARTESIAN_POINT('Ctrl Pts',(-0.160499533685813,-0.111513629025431,
-0.875245690316091));
#84354=CARTESIAN_POINT('Ctrl Pts',(-0.162620689753645,-0.10839669430786,
-0.875461652102209));
#84355=CARTESIAN_POINT('Ctrl Pts',(-0.164647949236151,-0.105224582737732,
-0.875677613888326));
#84356=CARTESIAN_POINT('Ctrl Pts',(-0.171337062502713,-0.0947579336630299,
-0.876390197975886));
#84357=CARTESIAN_POINT('Ctrl Pts',(-0.177045708979376,-0.0836179136310407,
-0.877102782063446));
#84358=CARTESIAN_POINT('Ctrl Pts',(-0.181648137368076,-0.0720077370197724,
-0.877815366151006));
#84359=CARTESIAN_POINT('Ctrl Pts',(-0.186238975491459,-0.060426798240347,
-0.878526155742718));
#84360=CARTESIAN_POINT('Ctrl Pts',(-0.189728752788956,-0.0483787787415931,
-0.87923694533443));
#84361=CARTESIAN_POINT('Ctrl Pts',(-0.19203819111273,-0.0360900700214141,
-0.879947734926141));
#84362=CARTESIAN_POINT('Ctrl Pts',(-0.194274986862109,-0.024187898334174,
-0.880636166879953));
#84363=CARTESIAN_POINT('Ctrl Pts',(-0.195404560012147,-0.0120607127809722,
-0.881324598833765));
#84364=CARTESIAN_POINT('Ctrl Pts',(-0.195399986118627,7.3653515014446E-5,
-0.882013030787577));
#84365=CARTESIAN_POINT('Ctrl Pts',(-0.195109753188566,7.45643940919532E-5,
-0.882013088758234));
#84366=CARTESIAN_POINT('Ctrl Pts',(-0.195204102274039,0.0279355699642562,
-0.883596106054292));
#84367=CARTESIAN_POINT('Ctrl Pts',(-0.176621603793911,0.120705073777376,
-0.888873965603043));
#84368=CARTESIAN_POINT('Ctrl Pts',(-0.03438531833784,0.228170121929786,
-0.897846667404486));
#84369=CARTESIAN_POINT('Ctrl Pts',(0.172650552859722,0.153093766216358,
-0.908931194162567));
#84370=CARTESIAN_POINT('Ctrl Pts',(0.222416746898179,-0.0614474453631151,
-0.920015720920646));
#84371=CARTESIAN_POINT('Ctrl Pts',(0.0695869939549012,-0.219994184582197,
-0.931100247678726));
#84372=CARTESIAN_POINT('Ctrl Pts',(-0.138468335956508,-0.179768882909404,
-0.94176601763437));
#84373=CARTESIAN_POINT('Ctrl Pts',(-0.195199225693986,-0.0571389522596028,
-0.94873694533732));
#84374=CARTESIAN_POINT('Ctrl Pts',(-0.1956163961968,0.000134331411914747,
-0.952013030787577));
#84375=CARTESIAN_POINT('Origin',(0.,0.,-1.10400562256037));
#84376=CARTESIAN_POINT('',(-0.155549940342626,0.000136232908569803,-0.0190056209657492));
#84377=CARTESIAN_POINT('Ctrl Pts',(0.102472688294207,0.117287771082297,
-0.0445113451759945));
#84378=CARTESIAN_POINT('Ctrl Pts',(0.0989611449419164,0.120398369956428,
-0.0441741475577544));
#84379=CARTESIAN_POINT('Ctrl Pts',(0.055236448550028,0.15556450473979,-0.0401421076868207));
#84380=CARTESIAN_POINT('Ctrl Pts',(-0.065934354559954,0.171464947984463,
-0.0324152255631935));
#84381=CARTESIAN_POINT('Ctrl Pts',(-0.149738893304472,0.0731738720390481,
-0.0242505156428922));
#84382=CARTESIAN_POINT('Ctrl Pts',(-0.155685419418353,0.0109444862887444,
-0.0197806479752842));
#84383=CARTESIAN_POINT('Ctrl Pts',(-0.155585995199752,0.000136286723707784,
-0.0190056225603694));
#84384=CARTESIAN_POINT('',(0.0210111597547384,-0.154124409701257,-3.03070625262691E-7));
#84385=CARTESIAN_POINT('Ctrl Pts',(-0.155549940342626,0.000136232908569803,
-0.0190056209657492));
#84386=CARTESIAN_POINT('Ctrl Pts',(-0.155558853686153,-0.0100409707379475,
-0.0182756668891895));
#84387=CARTESIAN_POINT('Ctrl Pts',(-0.154564581067856,-0.0202492057705681,
-0.01754571281263));
#84388=CARTESIAN_POINT('Ctrl Pts',(-0.152575659837309,-0.0302732641981308,
-0.0168157587360704));
#84389=CARTESIAN_POINT('Ctrl Pts',(-0.150595804610828,-0.0402516304418793,
-0.0160891319740994));
#84390=CARTESIAN_POINT('Ctrl Pts',(-0.147630507612318,-0.0500465508032369,
-0.0153625052121281));
#84391=CARTESIAN_POINT('Ctrl Pts',(-0.143739789739225,-0.0594531357097622,
-0.014635878450157));
#84392=CARTESIAN_POINT('Ctrl Pts',(-0.13982234774238,-0.0689243315049017,
-0.0139042607163031));
#84393=CARTESIAN_POINT('Ctrl Pts',(-0.134967074703252,-0.0780009252912488,
-0.0131726429824491));
#84394=CARTESIAN_POINT('Ctrl Pts',(-0.129283997512143,-0.0864953784157288,
-0.0124410252485951));
#84395=CARTESIAN_POINT('Ctrl Pts',(-0.123600920321035,-0.0949898315402083,
-0.0117094075147413));
#84396=CARTESIAN_POINT('Ctrl Pts',(-0.117090687318054,-0.102901409291159,
-0.0109777897808876));
#84397=CARTESIAN_POINT('Ctrl Pts',(-0.109904308625208,-0.110076543575891,
-0.0102461720470337));
#84398=CARTESIAN_POINT('Ctrl Pts',(-0.102729446060097,-0.117240179751983,
-0.0095157267261066));
#84399=CARTESIAN_POINT('Ctrl Pts',(-0.0948223501874392,-0.123727993173485,
-0.00878528140517938));
#84400=CARTESIAN_POINT('Ctrl Pts',(-0.0863355949095739,-0.129390755278768,
-0.00805483608425228));
#84401=CARTESIAN_POINT('Ctrl Pts',(-0.0778602724806752,-0.135045888849732,
-0.00732537477556061));
#84402=CARTESIAN_POINT('Ctrl Pts',(-0.068807567315153,-0.139877575646078,
-0.00659591346686866));
#84403=CARTESIAN_POINT('Ctrl Pts',(-0.0593625781028027,-0.143777212453812,
-0.00586645215817705));
#84404=CARTESIAN_POINT('Ctrl Pts',(-0.0499260002920378,-0.147673376371267,
-0.00513764048410867));
#84405=CARTESIAN_POINT('Ctrl Pts',(-0.0400987007419705,-0.150638763861192,
-0.00440882881004057));
#84406=CARTESIAN_POINT('Ctrl Pts',(-0.0300864858397496,-0.152612600625946,
-0.0036800171359721));
#84407=CARTESIAN_POINT('Ctrl Pts',(-0.0200527190266847,-0.154590686196223,
-0.00294963664977016));
#84408=CARTESIAN_POINT('Ctrl Pts',(-0.00983418001629753,-0.155572803316964,
-0.00221925616356821));
#84409=CARTESIAN_POINT('Ctrl Pts',(0.000354303184596075,-0.15554959649338,
-0.00148887567736633));
#84410=CARTESIAN_POINT('Ctrl Pts',(0.00727594529835836,-0.155533830718998,
-0.000992684808452523));
#84411=CARTESIAN_POINT('Ctrl Pts',(0.0141835652280306,-0.155055188152375,
-0.000496493939539067));
#84412=CARTESIAN_POINT('Ctrl Pts',(0.0210111597547384,-0.154124409701257,
-3.03070625262691E-7));
#84413=CARTESIAN_POINT('',(-0.138946909435068,-0.0699253806456778,0.));
#84414=CARTESIAN_POINT('Origin',(0.,0.,0.));
#84415=CARTESIAN_POINT('',(-0.155549948455572,0.000126631232131687,-0.00519437743962925));
#84416=CARTESIAN_POINT('Ctrl Pts',(-0.155549936615206,0.000140424376441733,
-0.0050017268448989));
#84417=CARTESIAN_POINT('Ctrl Pts',(-0.155550517862743,-0.000503431197937891,
-0.00495542424155714));
#84418=CARTESIAN_POINT('Ctrl Pts',(-0.155547101522606,-0.0011472927388459,
-0.0049092353714434));
#84419=CARTESIAN_POINT('Ctrl Pts',(-0.155531454351363,-0.00250608036372759,
-0.00481199043401684));
#84420=CARTESIAN_POINT('Ctrl Pts',(-0.155518291643096,-0.00322098180988224,
-0.00476096163639329));
#84421=CARTESIAN_POINT('Ctrl Pts',(-0.155465720677275,-0.0052980293137128,
-0.00461307543001361));
#84422=CARTESIAN_POINT('Ctrl Pts',(-0.155413341233105,-0.0066598027843363,
-0.00451658109682896));
#84423=CARTESIAN_POINT('Ctrl Pts',(-0.155226329145725,-0.0102817887289338,
-0.00426101493953919));
#84424=CARTESIAN_POINT('Ctrl Pts',(-0.15506023115533,-0.0125400927092421,
-0.00410279931249361));
#84425=CARTESIAN_POINT('Ctrl Pts',(-0.154165829117664,-0.0219015287112345,
-0.00345034722190772));
#84426=CARTESIAN_POINT('Ctrl Pts',(-0.152998200286724,-0.028954161007669,
-0.00296738723038534));
#84427=CARTESIAN_POINT('Ctrl Pts',(-0.149139281806736,-0.0452219429515892,
-0.00184186572284642));
#84428=CARTESIAN_POINT('Ctrl Pts',(-0.146072590171909,-0.0543167899376314,
-0.00120369172680408));
#84429=CARTESIAN_POINT('Ctrl Pts',(-0.141566225103923,-0.0644761159143157,
-0.00042849118234209));
#84430=CARTESIAN_POINT('Ctrl Pts',(-0.140922145946666,-0.0658719518483347,
-0.000320527592429761));
#84431=CARTESIAN_POINT('Ctrl Pts',(-0.140029455127714,-0.067733539564464,
-0.000174304757339283));
#84432=CARTESIAN_POINT('Ctrl Pts',(-0.139798985468618,-0.0682079491771672,
-0.000136843834668115));
#84433=CARTESIAN_POINT('Ctrl Pts',(-0.139361561421611,-0.06909683287829,
-6.62681200140033E-5));
#84434=CARTESIAN_POINT('Ctrl Pts',(-0.139155158822226,-0.0695115736921777,
-3.31792881770164E-5));
#84435=CARTESIAN_POINT('Ctrl Pts',(-0.138946909435068,-0.0699253806456779,
1.65503461629912E-16));
#84436=CARTESIAN_POINT('Ctrl Pts',(0.10234224283772,0.117140376604078,-0.0306875317892119));
#84437=CARTESIAN_POINT('Ctrl Pts',(0.094583506915784,0.123918965326908,
-0.0299499611150766));
#84438=CARTESIAN_POINT('Ctrl Pts',(0.0861337948976529,0.12993622197685,
-0.0292123904409415));
#84439=CARTESIAN_POINT('Ctrl Pts',(0.0771670433343891,0.135059431077687,
-0.0284748197668061));
#84440=CARTESIAN_POINT('Ctrl Pts',(0.0682074047892692,0.140178576111506,
-0.0277378341823267));
#84441=CARTESIAN_POINT('Ctrl Pts',(0.0587323383981438,0.144404615767851,
-0.0270008485978476));
#84442=CARTESIAN_POINT('Ctrl Pts',(0.048942195600838,0.147649801861599,
-0.0262638630133682));
#84443=CARTESIAN_POINT('Ctrl Pts',(0.0391279920756871,0.150902963481447,
-0.0255250661775169));
#84444=CARTESIAN_POINT('Ctrl Pts',(0.0289980539335844,0.153170184543577,
-0.0247862693416651));
#84445=CARTESIAN_POINT('Ctrl Pts',(0.0187684845020169,0.154413556689487,
-0.0240474725058137));
#84446=CARTESIAN_POINT('Ctrl Pts',(0.0100987950178107,0.155467330310212,
-0.0234213328425959));
#84447=CARTESIAN_POINT('Ctrl Pts',(0.00135808684489701,0.155786583508046,
-0.0227951931793781));
#84448=CARTESIAN_POINT('Ctrl Pts',(-0.0073214427802927,0.155377601267412,
-0.0221690535161603));
#84449=CARTESIAN_POINT('Ctrl Pts',(-0.0174343336593535,0.154901078581321,
-0.0214395114369677));
#84450=CARTESIAN_POINT('Ctrl Pts',(-0.0275428404924019,0.15343092992204,
-0.0207099693577752));
#84451=CARTESIAN_POINT('Ctrl Pts',(-0.0374342961525748,0.150978395711311,
-0.0199804272785826));
#84452=CARTESIAN_POINT('Ctrl Pts',(-0.0474855104765481,0.148486250183311,
-0.0192391022352074));
#84453=CARTESIAN_POINT('Ctrl Pts',(-0.0573115842108452,0.144979686726725,
-0.0184977771918322));
#84454=CARTESIAN_POINT('Ctrl Pts',(-0.0666968112862147,0.140525221452418,
-0.017756452148457));
#84455=CARTESIAN_POINT('Ctrl Pts',(-0.075913181054113,0.136150900111379,
-0.0170284648911343));
#84456=CARTESIAN_POINT('Ctrl Pts',(-0.084703590970681,0.130863005220033,
-0.016300477633812));
#84457=CARTESIAN_POINT('Ctrl Pts',(-0.0928847001194851,0.124772733334304,
-0.0155724903764893));
#84458=CARTESIAN_POINT('Ctrl Pts',(-0.101290644007637,0.118515087481662,
-0.0148244964400879));
#84459=CARTESIAN_POINT('Ctrl Pts',(-0.109052378371382,0.111410830305483,
-0.0140765025036864));
#84460=CARTESIAN_POINT('Ctrl Pts',(-0.116007279635627,0.103624869464532,
-0.013328508567285));
#84461=CARTESIAN_POINT('Ctrl Pts',(-0.122962180899872,0.0958389086235821,
-0.0125805146308835));
#84462=CARTESIAN_POINT('Ctrl Pts',(-0.129109668280135,0.0873721506017285,
-0.011832520694482));
#84463=CARTESIAN_POINT('Ctrl Pts',(-0.13433441540455,0.0784223650364991,
-0.0110845267580806));
#84464=CARTESIAN_POINT('Ctrl Pts',(-0.139898640305477,0.0688910674417676,
-0.0102879319396981));
#84465=CARTESIAN_POINT('Ctrl Pts',(-0.144456639849757,0.058745004040905,
-0.00949133712131538));
#84466=CARTESIAN_POINT('Ctrl Pts',(-0.147892118257631,0.0482050190049829,
-0.00869474230293288));
#84467=CARTESIAN_POINT('Ctrl Pts',(-0.151308474758384,0.0377236996310117,
-0.00790258133926343));
#84468=CARTESIAN_POINT('Ctrl Pts',(-0.153614448655364,0.0268534505681371,
-0.00711042037559407));
#84469=CARTESIAN_POINT('Ctrl Pts',(-0.154742021800765,0.0158337989443936,
-0.00631825941192465));
#84470=CARTESIAN_POINT('Ctrl Pts',(-0.155275271644623,0.0106224053140157,
-0.00594363208782615));
#84471=CARTESIAN_POINT('Ctrl Pts',(-0.155545673493413,0.00537786453568078,
-0.00556900476372773));
#84472=CARTESIAN_POINT('Ctrl Pts',(-0.155549948455572,0.000126631232131687,
-0.00519437743962925));
#84473=CARTESIAN_POINT('Ctrl Pts',(-0.0684858909661362,0.139417771125461,
-0.997734010353788));
#84474=CARTESIAN_POINT('Ctrl Pts',(-0.114723552878964,0.116704544205191,
-0.994039168101094));
#84475=CARTESIAN_POINT('Ctrl Pts',(-0.182045051175031,0.0220707951371245,
-0.986649483595708));
#84476=CARTESIAN_POINT('Ctrl Pts',(-0.117521741175058,-0.140994311004445,
-0.975564956837627));
#84477=CARTESIAN_POINT('Ctrl Pts',(0.0542023734324004,-0.175183216767612,
-0.964480430079548));
#84478=CARTESIAN_POINT('Ctrl Pts',(0.17647635671274,-0.0500200511658903,
-0.953395903321467));
#84479=CARTESIAN_POINT('Ctrl Pts',(0.138038040413487,0.120822126492967,
-0.942311376563387));
#84480=CARTESIAN_POINT('Ctrl Pts',(-0.0261604923186076,0.181546629858235,
-0.931226849805308));
#84481=CARTESIAN_POINT('Ctrl Pts',(-0.166518288973121,0.0769318273169837,
-0.920142323047226));
#84482=CARTESIAN_POINT('Ctrl Pts',(-0.155200137290489,-0.097777006996296,
-0.909057796289148));
#84483=CARTESIAN_POINT('Ctrl Pts',(-0.00250686787299496,-0.183411833934768,
-0.897973269531066));
#84484=CARTESIAN_POINT('Ctrl Pts',(0.152468303420884,-0.101981132945721,
-0.886888742772987));
#84485=CARTESIAN_POINT('Ctrl Pts',(0.168560695380791,0.0723467668780286,
-0.875804216014907));
#84486=CARTESIAN_POINT('Ctrl Pts',(0.0311104340172021,0.180772608850168,
-0.864719689256827));
#84487=CARTESIAN_POINT('Ctrl Pts',(-0.134678138991185,0.124533056899584,
-0.853635162498746));
#84488=CARTESIAN_POINT('Ctrl Pts',(-0.17778829995743,-0.0451442083670213,
-0.842550635740667));
#84489=CARTESIAN_POINT('Ctrl Pts',(-0.0589507469967352,-0.173699357167665,
-0.831466108982587));
#84490=CARTESIAN_POINT('Ctrl Pts',(0.113585102895841,-0.144031577598204,
-0.820381582224506));
#84491=CARTESIAN_POINT('Ctrl Pts',(0.182656116776244,0.0168348494932255,
-0.809297055466426));
#84492=CARTESIAN_POINT('Ctrl Pts',(0.0853453694751092,0.162366358308449,
-0.798212528708347));
#84493=CARTESIAN_POINT('Ctrl Pts',(-0.0897066078766045,0.159998103029135,
-0.787128001950266));
#84494=CARTESIAN_POINT('Ctrl Pts',(-0.183044693750403,0.0118873098484331,
-0.776043475192187));
#84495=CARTESIAN_POINT('Ctrl Pts',(-0.109647071009597,-0.147051649214227,
-0.764958948434105));
#84496=CARTESIAN_POINT('Ctrl Pts',(0.0636282451524521,-0.172041025459065,
-0.753874421676027));
#84497=CARTESIAN_POINT('Ctrl Pts',(0.178944490378705,-0.0403179525962051,
-0.742789894917946));
#84498=CARTESIAN_POINT('Ctrl Pts',(0.131259910019175,0.128130807864812,
-0.731705368159865));
#84499=CARTESIAN_POINT('Ctrl Pts',(-0.0359895343390016,0.179865008726402,
-0.720620841401787));
#84500=CARTESIAN_POINT('Ctrl Pts',(-0.170456053776628,0.0677598823930454,
-0.709536314643705));
#84501=CARTESIAN_POINT('Ctrl Pts',(-0.149653878410367,-0.106067830204563,
-0.698451787885626));
#84502=CARTESIAN_POINT('Ctrl Pts',(0.00746825656729185,-0.183278184947211,
-0.687367261127545));
#84503=CARTESIAN_POINT('Ctrl Pts',(0.157787544579823,-0.0935401448930603,
-0.676282734369466));
#84504=CARTESIAN_POINT('Ctrl Pts',(0.164377903307406,0.0814037642567962,
-0.665198207611385));
#84505=CARTESIAN_POINT('Ctrl Pts',(0.0212361643438886,0.182196853034596,
-0.654113680853305));
#84506=CARTESIAN_POINT('Ctrl Pts',(-0.14124963103096,0.117026534020937,
-0.643029154095226));
#84507=CARTESIAN_POINT('Ctrl Pts',(-0.175070909294838,-0.0547434438998959,
-0.631944627337146));
#84508=CARTESIAN_POINT('Ctrl Pts',(-0.0494198134360999,-0.176647530329169,
-0.620860100579064));
#84509=CARTESIAN_POINT('Ctrl Pts',(0.121247870324878,-0.137643095987666,
-0.609775573820986));
#84510=CARTESIAN_POINT('Ctrl Pts',(0.1814706731176,0.0267406568662764,-0.598691047062905));
#84511=CARTESIAN_POINT('Ctrl Pts',(0.0763915465817655,0.166766302178392,
-0.587606520304825));
#84512=CARTESIAN_POINT('Ctrl Pts',(-0.0982727631543477,0.154884253406886,
-0.576521993546745));
#84513=CARTESIAN_POINT('Ctrl Pts',(-0.183420254162722,0.00191788797457964,
-0.565437466788665));
#84514=CARTESIAN_POINT('Ctrl Pts',(-0.101489939318737,-0.152795484712349,
-0.554352940030585));
#84515=CARTESIAN_POINT('Ctrl Pts',(0.0728877252188209,-0.168327203516921,
-0.543268413272505));
#84516=CARTESIAN_POINT('Ctrl Pts',(0.180871843096437,-0.0305294006868705,
-0.532183886514424));
#84517=CARTESIAN_POINT('Ctrl Pts',(0.124099506879204,0.135077682552448,
-0.521099359756346));
#84518=CARTESIAN_POINT('Ctrl Pts',(-0.0457152706506643,0.177642286521926,
-0.510014832998264));
#84519=CARTESIAN_POINT('Ctrl Pts',(-0.173887934286807,0.0583922446979787,
-0.498930306240185));
#84520=CARTESIAN_POINT('Ctrl Pts',(-0.143665797646062,-0.114047387160434,
-0.487845779482104));
#84521=CARTESIAN_POINT('Ctrl Pts',(0.0174217461783371,-0.182601069798343,
-0.476761252724024));
#84522=CARTESIAN_POINT('Ctrl Pts',(0.162639793262148,-0.0848231429448783,
-0.465676725965944));
#84523=CARTESIAN_POINT('Ctrl Pts',(0.159708989901038,0.0902203218581661,
-0.454592199207864));
#84524=CARTESIAN_POINT('Ctrl Pts',(0.0112990096116807,0.183081949719785,
-0.443507672449784));
#84525=CARTESIAN_POINT('Ctrl Pts',(-0.147403256787751,0.109173933792666,
-0.432423145691704));
#84526=CARTESIAN_POINT('Ctrl Pts',(-0.171835658433079,-0.0641807948086411,
-0.421338618933623));
#84527=CARTESIAN_POINT('Ctrl Pts',(-0.039742681192371,-0.179073133727677,
-0.410254092175544));
#84528=CARTESIAN_POINT('Ctrl Pts',(0.128551968555153,-0.130847465821811,
-0.399169565417463));
#84529=CARTESIAN_POINT('Ctrl Pts',(0.179748422455937,0.0365673700994489,
-0.388085038659384));
#84530=CARTESIAN_POINT('Ctrl Pts',(0.0672117479383925,0.17067292951877,
-0.377000511901303));
#84531=CARTESIAN_POINT('Ctrl Pts',(-0.106548216364339,0.149312241698129,
-0.365915985143223));
#84532=CARTESIAN_POINT('Ctrl Pts',(-0.183253238240171,-0.00805720831474408,
-0.354831458385143));
#84533=CARTESIAN_POINT('Ctrl Pts',(-0.0930325893378739,-0.158087334258128,
-0.343746931627063));
#84534=CARTESIAN_POINT('Ctrl Pts',(0.0819315954977009,-0.164115452015086,
-0.332662404868983));
#84535=CARTESIAN_POINT('Ctrl Pts',(0.182264157622932,-0.0206505393912029,
-0.321577878110903));
#84536=CARTESIAN_POINT('Ctrl Pts',(0.116572004105514,0.14162498293918,-0.310493351352823));
#84537=CARTESIAN_POINT('Ctrl Pts',(-0.0553057762937551,0.17489407947702,
-0.299408824594743));
#84538=CARTESIAN_POINT('Ctrl Pts',(-0.176805435700639,0.0488518765015995,
-0.288324297836663));
#84539=CARTESIAN_POINT('Ctrl Pts',(-0.137252738105612,-0.121689579786436,
-0.277239771078583));
#84540=CARTESIAN_POINT('Ctrl Pts',(0.0273237004269018,-0.181383801088499,
-0.266155244320502));
#84541=CARTESIAN_POINT('Ctrl Pts',(0.167010936000477,-0.075855225229966,
-0.255070717562423));
#84542=CARTESIAN_POINT('Ctrl Pts',(0.154567640328825,0.098769998407238,
-0.243986190804342));
#84543=CARTESIAN_POINT('Ctrl Pts',(0.00132843101394552,0.183425469847153,
-0.232901664046263));
#84544=CARTESIAN_POINT('Ctrl Pts',(-0.153120847597592,0.100998386504967,
-0.221817137288183));
#84545=CARTESIAN_POINT('Ctrl Pts',(-0.168092100005951,-0.0734282941735533,
-0.210732610530102));
#84546=CARTESIAN_POINT('Ctrl Pts',(-0.0299479845542862,-0.180969015641703,
-0.199648083772023));
#84547=CARTESIAN_POINT('Ctrl Pts',(0.135475793855047,-0.123664782507313,
-0.188563557013942));
#84548=CARTESIAN_POINT('Ctrl Pts',(0.177494461442691,0.0462859276935804,
-0.177479030255862));
#84549=CARTESIAN_POINT('Ctrl Pts',(0.0578331208192682,0.174074660385242,
-0.166394503497782));
#84550=CARTESIAN_POINT('Ctrl Pts',(-0.114508471537225,0.14329860116919,
-0.155309976739702));
#84551=CARTESIAN_POINT('Ctrl Pts',(-0.182544172064818,-0.0180085709609084,
-0.144225449981622));
#84552=CARTESIAN_POINT('Ctrl Pts',(-0.084299977295163,-0.162911353328334,
-0.133140923223542));
#84553=CARTESIAN_POINT('Ctrl Pts',(0.0907329858453492,-0.15941859359732,
-0.122056396465462));
#84554=CARTESIAN_POINT('Ctrl Pts',(0.183117539039973,-0.0107098982665486,
-0.110971869707382));
#84555=CARTESIAN_POINT('Ctrl Pts',(0.108699242850674,0.14775202136532,-0.0998873429493014));
#84556=CARTESIAN_POINT('Ctrl Pts',(-0.0647318703529614,0.1716310306231,
-0.0888028161912215));
#84557=CARTESIAN_POINT('Ctrl Pts',(-0.179201472288944,0.0391622132462028,
-0.0777182894331414));
#84558=CARTESIAN_POINT('Ctrl Pts',(-0.130430729224305,-0.128962688577941,
-0.0666337626750612));
#84559=CARTESIAN_POINT('Ctrl Pts',(0.0371392267897813,-0.179647334199356,
-0.0555492359169813));
#84560=CARTESIAN_POINT('Ctrl Pts',(0.170898721259193,-0.0666298511870843,
-0.0444647091589011));
#84561=CARTESIAN_POINT('Ctrl Pts',(0.14894861527182,0.106964324573014,-0.0333801824008211));
#84562=CARTESIAN_POINT('Ctrl Pts',(-0.00860614795259104,0.183348546767771,
-0.0222956556427411));
#84563=CARTESIAN_POINT('Ctrl Pts',(-0.158470039306694,0.0922754967336385,
-0.0112111288846609));
#84564=CARTESIAN_POINT('Ctrl Pts',(-0.161908972733501,-0.0238102660988092,
-0.00382144437927415));
#84565=CARTESIAN_POINT('Ctrl Pts',(-0.138751033761026,-0.0698268057214688,
-0.000126602126580784));
#84566=CARTESIAN_POINT('Ctrl Pts',(-0.0744116356088496,0.151480899730365,
-0.989974424426066));
#84567=CARTESIAN_POINT('Ctrl Pts',(-0.124650013194736,0.126802409880127,
-0.986279582173373));
#84568=CARTESIAN_POINT('Ctrl Pts',(-0.197796507007979,0.0239804716296012,
-0.978889897667986));
#84569=CARTESIAN_POINT('Ctrl Pts',(-0.127690314852737,-0.153193849789752,
-0.967805370909905));
#84570=CARTESIAN_POINT('Ctrl Pts',(0.0588922361100749,-0.190340952085206,
-0.956720844151826));
#84571=CARTESIAN_POINT('Ctrl Pts',(0.191745981019349,-0.0543480382307185,
-0.945636317393745));
#84572=CARTESIAN_POINT('Ctrl Pts',(0.149981787759574,0.131276266151323,
-0.934551790635665));
#84573=CARTESIAN_POINT('Ctrl Pts',(-0.0284240300344901,0.197254959765447,
-0.923467263877585));
#84574=CARTESIAN_POINT('Ctrl Pts',(-0.180926291042983,0.083588356963409,
-0.912382737119506));
#84575=CARTESIAN_POINT('Ctrl Pts',(-0.16862883580231,-0.106237166705329,
-0.901298210361425));
#84576=CARTESIAN_POINT('Ctrl Pts',(-0.0027237747228427,-0.199281550704414,
-0.890213683603345));
#84577=CARTESIAN_POINT('Ctrl Pts',(0.165660629890387,-0.1108050548322,-0.879129156845265));
#84578=CARTESIAN_POINT('Ctrl Pts',(0.183145416752364,0.0786065739740197,
-0.868044630087185));
#84579=CARTESIAN_POINT('Ctrl Pts',(0.0338022656501029,0.196413966556576,
-0.856960103329105));
#84580=CARTESIAN_POINT('Ctrl Pts',(-0.146331170723112,0.135308284969968,
-0.845875576571024));
#84581=CARTESIAN_POINT('Ctrl Pts',(-0.193171440209355,-0.0490503129252965,
-0.834791049812945));
#84582=CARTESIAN_POINT('Ctrl Pts',(-0.0640514628999968,-0.188728701469957,
-0.823706523054863));
#84583=CARTESIAN_POINT('Ctrl Pts',(0.123413058778169,-0.156493916005342,
-0.812621996296785));
#84584=CARTESIAN_POINT('Ctrl Pts',(0.198460445086451,0.0182914855650937,
-0.801537469538704));
#84585=CARTESIAN_POINT('Ctrl Pts',(0.0927298812163344,0.176415114400109,
-0.790452942780624));
#84586=CARTESIAN_POINT('Ctrl Pts',(-0.0974684759569022,0.173841945731542,
-0.779368416022544));
#84587=CARTESIAN_POINT('Ctrl Pts',(-0.198882643699906,0.0129158598410958,
-0.768283889264463));
#84588=CARTESIAN_POINT('Ctrl Pts',(-0.119134288514671,-0.159775299447008,
-0.757199362506384));
#84589=CARTESIAN_POINT('Ctrl Pts',(0.069133681783536,-0.186926882539398,
-0.746114835748302));
#84590=CARTESIAN_POINT('Ctrl Pts',(0.194427670056241,-0.0438064651676544,
-0.735030308990224));
#84591=CARTESIAN_POINT('Ctrl Pts',(0.142617179343217,0.139217331491218,
-0.723945782232142));
#84592=CARTESIAN_POINT('Ctrl Pts',(-0.039103530335761,0.195427836293314,
-0.712861255474064));
#84593=CARTESIAN_POINT('Ctrl Pts',(-0.185204771114401,0.073622809112947,
-0.701776728715982));
#84594=CARTESIAN_POINT('Ctrl Pts',(-0.162602686635556,-0.115245353746014,
-0.690692201957904));
#84595=CARTESIAN_POINT('Ctrl Pts',(0.008114447785945,-0.199136337732496,
-0.679607675199823));
#84596=CARTESIAN_POINT('Ctrl Pts',(0.171440118617931,-0.101633709927542,
-0.668523148441744));
#84597=CARTESIAN_POINT('Ctrl Pts',(0.178600708416069,0.0884472284380528,
-0.657438621683664));
#84598=CARTESIAN_POINT('Ctrl Pts',(0.0230736243713112,0.197961443529929,
-0.646354094925584));
#84599=CARTESIAN_POINT('Ctrl Pts',(-0.153471261392474,0.127152259878442,
-0.635269568167503));
#84600=CARTESIAN_POINT('Ctrl Pts',(-0.19021892720355,-0.0594801227228939,
-0.624185041409425));
#84601=CARTESIAN_POINT('Ctrl Pts',(-0.0536958649057056,-0.191931965440254,
-0.613100514651342));
#84602=CARTESIAN_POINT('Ctrl Pts',(0.131738847486486,-0.149552670750429,
-0.602015987893264));
#84603=CARTESIAN_POINT('Ctrl Pts',(0.197172430864581,0.0290543933444405,
-0.590931461135182));
#84604=CARTESIAN_POINT('Ctrl Pts',(0.0830013284144861,0.18119576360144,
-0.579846934377105));
#84605=CARTESIAN_POINT('Ctrl Pts',(-0.106775818186142,0.16828562005218,
-0.56876240761902));
#84606=CARTESIAN_POINT('Ctrl Pts',(-0.199290699492951,0.00208383331354575,
-0.557677880860944));
#84607=CARTESIAN_POINT('Ctrl Pts',(-0.11027136065565,-0.166016120557078,
-0.546593354102861));
#84608=CARTESIAN_POINT('Ctrl Pts',(0.0791943387583679,-0.182891721994993,
-0.535508827344784));
#84609=CARTESIAN_POINT('Ctrl Pts',(0.196521787050244,-0.0331709583860329,
-0.524424300586703));
#84610=CARTESIAN_POINT('Ctrl Pts',(0.134837222015547,0.14676528480809,-0.513339773828623));
#84611=CARTESIAN_POINT('Ctrl Pts',(-0.0496707863974368,0.193012792955104,
-0.502255247070543));
#84612=CARTESIAN_POINT('Ctrl Pts',(-0.188933595232391,0.0634446361659716,
-0.491170720312461));
#84613=CARTESIAN_POINT('Ctrl Pts',(-0.156096486927209,-0.123915342208513,
-0.480086193554382));
#84614=CARTESIAN_POINT('Ctrl Pts',(0.0189291635109664,-0.198400635166434,
-0.469001666796301));
#84615=CARTESIAN_POINT('Ctrl Pts',(0.176712208324863,-0.092162469013257,
-0.457917140038222));
#84616=CARTESIAN_POINT('Ctrl Pts',(0.173527817077681,0.0980266390626729,
-0.446832613280141));
#84617=CARTESIAN_POINT('Ctrl Pts',(0.0122766569012164,0.19892312324363,
-0.435748086522061));
#84618=CARTESIAN_POINT('Ctrl Pts',(-0.160157329880857,0.118620213079824,
-0.424663559763982));
#84619=CARTESIAN_POINT('Ctrl Pts',(-0.186703746122714,-0.0697340408223409,
-0.4135790330059));
#84620=CARTESIAN_POINT('Ctrl Pts',(-0.0431814183810181,-0.194567444276481,
-0.402494506247822));
#84621=CARTESIAN_POINT('Ctrl Pts',(0.13967493312829,-0.142169048394049,
-0.391409979489741));
#84622=CARTESIAN_POINT('Ctrl Pts',(0.195301162390815,0.0397313633600757,
-0.380325452731661));
#84623=CARTESIAN_POINT('Ctrl Pts',(0.0730272473011798,0.185440412039401,
-0.369240925973581));
#84624=CARTESIAN_POINT('Ctrl Pts',(-0.115767305338796,0.162231489792192,
-0.358156399215501));
#84625=CARTESIAN_POINT('Ctrl Pts',(-0.199109232510563,-0.00875435860851541,
-0.347071872457421));
#84626=CARTESIAN_POINT('Ctrl Pts',(-0.101082238106252,-0.171765847610963,
-0.335987345699341));
#84627=CARTESIAN_POINT('Ctrl Pts',(0.0890207302996347,-0.178315548514465,
-0.32490281894126));
#84628=CARTESIAN_POINT('Ctrl Pts',(0.198034571650647,-0.0224373281945668,
-0.313818292183181));
#84629=CARTESIAN_POINT('Ctrl Pts',(0.126658401742661,0.153879090640594,
-0.302733765425101));
#84630=CARTESIAN_POINT('Ctrl Pts',(-0.0600911109511644,0.190026797178187,
-0.29164923866702));
#84631=CARTESIAN_POINT('Ctrl Pts',(-0.192103533580739,0.0530787872036758,
-0.280564711908941));
#84632=CARTESIAN_POINT('Ctrl Pts',(-0.149128537135947,-0.132218775878082,
-0.26948018515086));
#84633=CARTESIAN_POINT('Ctrl Pts',(0.0296878847740664,-0.19707804222945,
-0.258395658392781));
#84634=CARTESIAN_POINT('Ctrl Pts',(0.181461564375435,-0.0824186018348015,
-0.2473111316347));
#84635=CARTESIAN_POINT('Ctrl Pts',(0.167941612014008,0.10731607674054,-0.23622660487662));
#84636=CARTESIAN_POINT('Ctrl Pts',(0.00144337356420142,0.1992963664647,
-0.22514207811854));
#84637=CARTESIAN_POINT('Ctrl Pts',(-0.166369635479871,0.109737276213662,
-0.21405755136046));
#84638=CARTESIAN_POINT('Ctrl Pts',(-0.182636276142689,-0.0797816804650109,
-0.20297302460238));
#84639=CARTESIAN_POINT('Ctrl Pts',(-0.0325392351977291,-0.196627367454142,
-0.1918884978443));
#84640=CARTESIAN_POINT('Ctrl Pts',(0.147197842708159,-0.134364883098799,
-0.18080397108622));
#84641=CARTESIAN_POINT('Ctrl Pts',(0.19285217730457,0.0502908195653797,
-0.16971944432814));
#84642=CARTESIAN_POINT('Ctrl Pts',(0.0628371340697605,0.189136477814472,
-0.158634917570059));
#84643=CARTESIAN_POINT('Ctrl Pts',(-0.124416321930711,0.155697518759482,
-0.147550390811979));
#84644=CARTESIAN_POINT('Ctrl Pts',(-0.198338814354084,-0.0195667633329289,
-0.136465864053899));
#84645=CARTESIAN_POINT('Ctrl Pts',(-0.0915940364333415,-0.177007265137383,
-0.125381337295819));
#84646=CARTESIAN_POINT('Ctrl Pts',(0.0985836613232566,-0.173212294221374,
-0.114296810537739));
#84647=CARTESIAN_POINT('Ctrl Pts',(0.198961791931268,-0.0116365726717701,
-0.103212283779659));
#84648=CARTESIAN_POINT('Ctrl Pts',(0.11810444948379,0.160536271328406,-0.0921277570215794));
#84649=CARTESIAN_POINT('Ctrl Pts',(-0.0703327982016847,0.18648141288273,
-0.0810432302634995));
#84650=CARTESIAN_POINT('Ctrl Pts',(-0.194706887337247,0.0425507254210006,
-0.0699587035054193));
#84651=CARTESIAN_POINT('Ctrl Pts',(-0.141716253644635,-0.140121190718603,
-0.0588741767473393));
#84652=CARTESIAN_POINT('Ctrl Pts',(0.0403526999749784,-0.195191327468512,
-0.0477896499892592));
#84653=CARTESIAN_POINT('Ctrl Pts',(0.185685740419814,-0.0723950019085964,
-0.0367051232311792));
#84654=CARTESIAN_POINT('Ctrl Pts',(0.161836400573806,0.116219417328008,
-0.025620596473099));
#84655=CARTESIAN_POINT('Ctrl Pts',(-0.00935079527198692,0.199212787612586,
-0.0145360697150191));
#84656=CARTESIAN_POINT('Ctrl Pts',(-0.172181666230212,0.10025963803208,
-0.00345154295693894));
#84657=CARTESIAN_POINT('Ctrl Pts',(-0.175918153518743,-0.0258704503905826,
0.00393814154844779));
#84658=CARTESIAN_POINT('Ctrl Pts',(-0.150756472886978,-0.0758685730706938,
0.00763298380114117));
#84659=CARTESIAN_POINT('Ctrl Pts',(-0.0803373802515631,0.163544028335269,
-0.982214838498344));
#84660=CARTESIAN_POINT('Ctrl Pts',(-0.134576473510508,0.136900275555064,
-0.97851999624565));
#84661=CARTESIAN_POINT('Ctrl Pts',(-0.213547962840926,0.0258901481220782,
-0.971130311740263));
#84662=CARTESIAN_POINT('Ctrl Pts',(-0.137858888530416,-0.16539338857506,
-0.960045784982185));
#84663=CARTESIAN_POINT('Ctrl Pts',(0.0635820987877494,-0.205498687402797,
-0.948961258224102));
#84664=CARTESIAN_POINT('Ctrl Pts',(0.207015605325956,-0.0586760252955468,
-0.937876731466025));
#84665=CARTESIAN_POINT('Ctrl Pts',(0.161925535105659,0.141730405809681,
-0.926792204707942));
#84666=CARTESIAN_POINT('Ctrl Pts',(-0.0306875677503726,0.212963289672657,
-0.915707677949864));
#84667=CARTESIAN_POINT('Ctrl Pts',(-0.195334293112845,0.0902448866098343,
-0.904623151191783));
#84668=CARTESIAN_POINT('Ctrl Pts',(-0.182057534314132,-0.114697326414361,
-0.893538624433703));
#84669=CARTESIAN_POINT('Ctrl Pts',(-0.00294068157269068,-0.215151267474059,
-0.882454097675622));
#84670=CARTESIAN_POINT('Ctrl Pts',(0.178852956359889,-0.11962897671868,
-0.871369570917544));
#84671=CARTESIAN_POINT('Ctrl Pts',(0.197730138123937,0.0848663810700111,
-0.860285044159461));
#84672=CARTESIAN_POINT('Ctrl Pts',(0.036494097283004,0.212055324262984,
-0.849200517401385));
#84673=CARTESIAN_POINT('Ctrl Pts',(-0.15798420245504,0.146083513040354,
-0.838115990643301));
#84674=CARTESIAN_POINT('Ctrl Pts',(-0.208554580461279,-0.052956417483572,
-0.827031463885224));
#84675=CARTESIAN_POINT('Ctrl Pts',(-0.0691521788032584,-0.203758045772247,
-0.815946937127142));
#84676=CARTESIAN_POINT('Ctrl Pts',(0.133241014660498,-0.16895625441248,
-0.804862410369063));
#84677=CARTESIAN_POINT('Ctrl Pts',(0.214264773396658,0.0197481216369616,
-0.793777883610981));
#84678=CARTESIAN_POINT('Ctrl Pts',(0.10011439295756,0.19046387049177,-0.782693356852903));
#84679=CARTESIAN_POINT('Ctrl Pts',(-0.1052303440372,0.187685788433949,-0.771608830094822));
#84680=CARTESIAN_POINT('Ctrl Pts',(-0.214720593649408,0.0139444098337588,
-0.760524303336743));
#84681=CARTESIAN_POINT('Ctrl Pts',(-0.128621506019745,-0.172498949679788,
-0.749439776578661));
#84682=CARTESIAN_POINT('Ctrl Pts',(0.0746391184146198,-0.201812739619732,
-0.738355249820582));
#84683=CARTESIAN_POINT('Ctrl Pts',(0.209910849733778,-0.0472949777391037,
-0.727270723062502));
#84684=CARTESIAN_POINT('Ctrl Pts',(0.153974448667259,0.150303855117625,
-0.716186196304421));
#84685=CARTESIAN_POINT('Ctrl Pts',(-0.0422175263325201,0.210990663860225,
-0.705101669546343));
#84686=CARTESIAN_POINT('Ctrl Pts',(-0.199953488452174,0.079485735832849,
-0.69401714278826));
#84687=CARTESIAN_POINT('Ctrl Pts',(-0.175551494860746,-0.124422877287465,
-0.682932616030183));
#84688=CARTESIAN_POINT('Ctrl Pts',(0.00876063900459808,-0.214994490517782,
-0.671848089272101));
#84689=CARTESIAN_POINT('Ctrl Pts',(0.185092692656038,-0.109727274962025,
-0.660763562514022));
#84690=CARTESIAN_POINT('Ctrl Pts',(0.192823513524732,0.0954906926193094,
-0.649679035755941));
#84691=CARTESIAN_POINT('Ctrl Pts',(0.0249110843987339,0.213726034025263,
-0.638594508997861));
#84692=CARTESIAN_POINT('Ctrl Pts',(-0.165692891753988,0.137277985735947,
-0.627509982239781));
#84693=CARTESIAN_POINT('Ctrl Pts',(-0.20536694511226,-0.0642168015458922,
-0.616425455481702));
#84694=CARTESIAN_POINT('Ctrl Pts',(-0.0579719163753115,-0.207216400551339,
-0.60534092872362));
#84695=CARTESIAN_POINT('Ctrl Pts',(0.142229824648094,-0.161462245513192,
-0.594256401965542));
#84696=CARTESIAN_POINT('Ctrl Pts',(0.212874188611563,0.0313681298226046,
-0.58317187520746));
#84697=CARTESIAN_POINT('Ctrl Pts',(0.0896111102472069,0.195625225024487,
-0.572087348449381));
#84698=CARTESIAN_POINT('Ctrl Pts',(-0.115278873217937,0.181686986697472,
-0.561002821691301));
#84699=CARTESIAN_POINT('Ctrl Pts',(-0.21516114482318,0.00224977865251208,
-0.549918294933221));
#84700=CARTESIAN_POINT('Ctrl Pts',(-0.119052781992563,-0.179236756401807,
-0.53883376817514));
#84701=CARTESIAN_POINT('Ctrl Pts',(0.0855009522979151,-0.197456240473065,
-0.527749241417061));
#84702=CARTESIAN_POINT('Ctrl Pts',(0.212171731004051,-0.0358125160851952,
-0.51666471465898));
#84703=CARTESIAN_POINT('Ctrl Pts',(0.14557493715189,0.15845288706373,-0.505580187900901));
#84704=CARTESIAN_POINT('Ctrl Pts',(-0.05362630214421,0.208383299388281,
-0.49449566114282));
#84705=CARTESIAN_POINT('Ctrl Pts',(-0.203979256177974,0.0684970276339647,
-0.483411134384741));
#84706=CARTESIAN_POINT('Ctrl Pts',(-0.168527176208356,-0.133783297256591,
-0.47232660762666));
#84707=CARTESIAN_POINT('Ctrl Pts',(0.0204365808435957,-0.214200200534527,
-0.46124208086858));
#84708=CARTESIAN_POINT('Ctrl Pts',(0.190784623387578,-0.0995017950816356,
-0.4501575541105));
#84709=CARTESIAN_POINT('Ctrl Pts',(0.187346644254324,0.10583295626718,-0.43907302735242));
#84710=CARTESIAN_POINT('Ctrl Pts',(0.0132543041907522,0.214764296767476,
-0.427988500594339));
#84711=CARTESIAN_POINT('Ctrl Pts',(-0.172911402973964,0.128066492366983,
-0.416903973836261));
#84712=CARTESIAN_POINT('Ctrl Pts',(-0.201571833812347,-0.0752872868360405,
-0.405819447078179));
#84713=CARTESIAN_POINT('Ctrl Pts',(-0.0466201555696652,-0.210061754825286,
-0.3947349203201));
#84714=CARTESIAN_POINT('Ctrl Pts',(0.150797897701427,-0.153490630966287,
-0.383650393562019));
#84715=CARTESIAN_POINT('Ctrl Pts',(0.210853902325691,0.0428953566207025,
-0.372565866803939));
#84716=CARTESIAN_POINT('Ctrl Pts',(0.0788427466639674,0.200207894560031,
-0.361481340045859));
#84717=CARTESIAN_POINT('Ctrl Pts',(-0.124986394313251,0.175150737886255,
-0.350396813287779));
#84718=CARTESIAN_POINT('Ctrl Pts',(-0.214965226780956,-0.00945150890228677,
-0.3393122865297));
#84719=CARTESIAN_POINT('Ctrl Pts',(-0.109131886874631,-0.185444360963798,
-0.328227759771619));
#84720=CARTESIAN_POINT('Ctrl Pts',(0.0961098651015682,-0.192515645013844,
-0.317143233013539));
#84721=CARTESIAN_POINT('Ctrl Pts',(0.213804985678363,-0.0242241169979305,
-0.306058706255459));
#84722=CARTESIAN_POINT('Ctrl Pts',(0.13674479937981,0.166133198342007,-0.294974179497379));
#84723=CARTESIAN_POINT('Ctrl Pts',(-0.0648764456085735,0.205159514879355,
-0.283889652739298));
#84724=CARTESIAN_POINT('Ctrl Pts',(-0.20740163146084,0.0573056979057522,
-0.272805125981219));
#84725=CARTESIAN_POINT('Ctrl Pts',(-0.161004336166281,-0.142747971969729,
-0.261720599223138));
#84726=CARTESIAN_POINT('Ctrl Pts',(0.0320520691212311,-0.2127722833704,
-0.250636072465059));
#84727=CARTESIAN_POINT('Ctrl Pts',(0.195912192750394,-0.0889819784396372,
-0.239551545706979));
#84728=CARTESIAN_POINT('Ctrl Pts',(0.181315583699191,0.11586215507384,-0.228467018948898));
#84729=CARTESIAN_POINT('Ctrl Pts',(0.0015583161144573,0.215167263082248,
-0.217382492190819));
#84730=CARTESIAN_POINT('Ctrl Pts',(-0.179618423362151,0.118476165922355,
-0.206297965432738));
#84731=CARTESIAN_POINT('Ctrl Pts',(-0.197180452279427,-0.0861350667564684,
-0.195213438674658));
#84732=CARTESIAN_POINT('Ctrl Pts',(-0.0351304858411718,-0.212285719266582,
-0.184128911916578));
#84733=CARTESIAN_POINT('Ctrl Pts',(0.158919891561272,-0.145064983690286,
-0.173044385158498));
#84734=CARTESIAN_POINT('Ctrl Pts',(0.20820989316645,0.054295711437179,-0.161959858400418));
#84735=CARTESIAN_POINT('Ctrl Pts',(0.0678411473202531,0.204198295243703,
-0.150875331642338));
#84736=CARTESIAN_POINT('Ctrl Pts',(-0.134324172324197,0.168096436349775,
-0.139790804884258));
#84737=CARTESIAN_POINT('Ctrl Pts',(-0.214133456643352,-0.0211249557049494,
-0.128706278126178));
#84738=CARTESIAN_POINT('Ctrl Pts',(-0.0988880955715197,-0.191103176946429,
-0.117621751368098));
#84739=CARTESIAN_POINT('Ctrl Pts',(0.106434336801163,-0.187005994845427,
-0.106537224610018));
#84740=CARTESIAN_POINT('Ctrl Pts',(0.214806044822565,-0.0125632470769915,
-0.0954526978519376));
#84741=CARTESIAN_POINT('Ctrl Pts',(0.127509656116906,0.173320521291492,
-0.0843681710938575));
#84742=CARTESIAN_POINT('Ctrl Pts',(-0.075933726050408,0.20133179514236,
-0.0732836443357776));
#84743=CARTESIAN_POINT('Ctrl Pts',(-0.21021230238555,0.045939237595798,
-0.0621991175776973));
#84744=CARTESIAN_POINT('Ctrl Pts',(-0.153001778064964,-0.151279692859263,
-0.0511145908196174));
#84745=CARTESIAN_POINT('Ctrl Pts',(0.0435661731601757,-0.210735320737669,
-0.0400300640615372));
#84746=CARTESIAN_POINT('Ctrl Pts',(0.200472759580433,-0.0781601526301082,
-0.0289455373034573));
#84747=CARTESIAN_POINT('Ctrl Pts',(0.174724185875792,0.125474510083003,
-0.0178610105453771));
#84748=CARTESIAN_POINT('Ctrl Pts',(-0.0100954425913831,0.215077028457403,
-0.00677648378729714));
#84749=CARTESIAN_POINT('Ctrl Pts',(-0.185893293153729,0.10824377933052,
0.00430804297078301));
#84750=CARTESIAN_POINT('Ctrl Pts',(-0.189927334303986,-0.0279306346823561,
0.0116977274761698));
#84751=CARTESIAN_POINT('Ctrl Pts',(-0.16276191201293,-0.081910340419919,
0.0153925697288631));
#84752=CARTESIAN_POINT('Ctrl Pts',(-0.0862631248942766,0.175607156940174,
-0.974455252570622));
#84753=CARTESIAN_POINT('Ctrl Pts',(-0.14450293382628,0.146998141230001,
-0.970760410317929));
#84754=CARTESIAN_POINT('Ctrl Pts',(-0.229299418673872,0.0277998246145549,
-0.963370725812542));
#84755=CARTESIAN_POINT('Ctrl Pts',(-0.148027462208095,-0.177592927360367,
-0.952286199054462));
#84756=CARTESIAN_POINT('Ctrl Pts',(0.0682719614654239,-0.22065642272039,
-0.941201672296381));
#84757=CARTESIAN_POINT('Ctrl Pts',(0.222285229632565,-0.0630040123603747,
-0.930117145538302));
#84758=CARTESIAN_POINT('Ctrl Pts',(0.173869282451744,0.152184545468037,
-0.919032618780222));
#84759=CARTESIAN_POINT('Ctrl Pts',(-0.0329511054662551,0.228671619579868,
-0.907948092022141));
#84760=CARTESIAN_POINT('Ctrl Pts',(-0.209742295182707,0.0969014162562596,
-0.896863565264062));
#84761=CARTESIAN_POINT('Ctrl Pts',(-0.195486232825953,-0.123157486123393,
-0.885779038505981));
#84762=CARTESIAN_POINT('Ctrl Pts',(-0.00315758842253853,-0.231020984243704,
-0.874694511747901));
#84763=CARTESIAN_POINT('Ctrl Pts',(0.192045282829392,-0.128452898605159,
-0.863609984989822));
#84764=CARTESIAN_POINT('Ctrl Pts',(0.212314859495509,0.0911261881660022,
-0.852525458231741));
#84765=CARTESIAN_POINT('Ctrl Pts',(0.0391859289159049,0.227696681969392,
-0.841440931473661));
#84766=CARTESIAN_POINT('Ctrl Pts',(-0.169637234186967,0.156858741110739,
-0.830356404715581));
#84767=CARTESIAN_POINT('Ctrl Pts',(-0.223937720713203,-0.0568625220418472,
-0.819271877957501));
#84768=CARTESIAN_POINT('Ctrl Pts',(-0.0742528947065199,-0.218787390074539,
-0.808187351199421));
#84769=CARTESIAN_POINT('Ctrl Pts',(0.143068970542826,-0.181418592819617,
-0.79710282444134));
#84770=CARTESIAN_POINT('Ctrl Pts',(0.230069101706865,0.0212047577088296,
-0.786018297683261));
#84771=CARTESIAN_POINT('Ctrl Pts',(0.107498904698785,0.204512626583431,
-0.77493377092518));
#84772=CARTESIAN_POINT('Ctrl Pts',(-0.112992212117498,0.201529631136357,
-0.763849244167102));
#84773=CARTESIAN_POINT('Ctrl Pts',(-0.230558543598911,0.0149729598264217,
-0.752764717409019));
#84774=CARTESIAN_POINT('Ctrl Pts',(-0.13810872352482,-0.18522259991257,
-0.741680190650942));
#84775=CARTESIAN_POINT('Ctrl Pts',(0.0801445550457034,-0.216698596700065,
-0.73059566389286));
#84776=CARTESIAN_POINT('Ctrl Pts',(0.225394029411315,-0.050783490310553,
-0.719511137134781));
#84777=CARTESIAN_POINT('Ctrl Pts',(0.165331717991301,0.161390378744031,
-0.708426610376699));
#84778=CARTESIAN_POINT('Ctrl Pts',(-0.0453315223292791,0.226553491427137,
-0.697342083618621));
#84779=CARTESIAN_POINT('Ctrl Pts',(-0.214702205789946,0.0853486625527506,
-0.686257556860539));
#84780=CARTESIAN_POINT('Ctrl Pts',(-0.188500303085936,-0.133600400828916,
-0.675173030102461));
#84781=CARTESIAN_POINT('Ctrl Pts',(0.00940683022325126,-0.230852643303067,
-0.664088503344379));
#84782=CARTESIAN_POINT('Ctrl Pts',(0.198745266694145,-0.117820839996506,
-0.6530039765863));
#84783=CARTESIAN_POINT('Ctrl Pts',(0.207046318633396,0.102534156800566,
-0.641919449828219));
#84784=CARTESIAN_POINT('Ctrl Pts',(0.0267485444261562,0.229490624520597,
-0.630834923070141));
#84785=CARTESIAN_POINT('Ctrl Pts',(-0.177914522115502,0.147403711593452,
-0.619750396312058));
#84786=CARTESIAN_POINT('Ctrl Pts',(-0.220514963020972,-0.0689534803688902,
-0.608665869553981));
#84787=CARTESIAN_POINT('Ctrl Pts',(-0.0622479678449172,-0.222500835662425,
-0.597581342795898));
#84788=CARTESIAN_POINT('Ctrl Pts',(0.152720801809701,-0.173371820275954,
-0.58649681603782));
#84789=CARTESIAN_POINT('Ctrl Pts',(0.228575946358543,0.0336818663007685,
-0.575412289279738));
#84790=CARTESIAN_POINT('Ctrl Pts',(0.0962208920799274,0.210054686447534,
-0.56432776252166));
#84791=CARTESIAN_POINT('Ctrl Pts',(-0.123781928249732,0.195088353342765,
-0.553243235763578));
#84792=CARTESIAN_POINT('Ctrl Pts',(-0.23103159015341,0.00241572399147842,
-0.5421587090055));
#84793=CARTESIAN_POINT('Ctrl Pts',(-0.127834203329475,-0.192457392246536,
-0.531074182247418));
#84794=CARTESIAN_POINT('Ctrl Pts',(0.0918075658374621,-0.212020758951138,
-0.519989655489339));
#84795=CARTESIAN_POINT('Ctrl Pts',(0.227821674957858,-0.0384540737843577,
-0.508905128731259));
#84796=CARTESIAN_POINT('Ctrl Pts',(0.156312652288233,0.170140489319371,
-0.497820601973179));
#84797=CARTESIAN_POINT('Ctrl Pts',(-0.0575818178909828,0.223753805821459,
-0.486736075215099));
#84798=CARTESIAN_POINT('Ctrl Pts',(-0.219024917123558,0.0735494191019577,
-0.475651548457019));
#84799=CARTESIAN_POINT('Ctrl Pts',(-0.180957865489502,-0.14365125230467,
-0.464567021698939));
#84800=CARTESIAN_POINT('Ctrl Pts',(0.0219439981762253,-0.229999765902618,
-0.453482494940859));
#84801=CARTESIAN_POINT('Ctrl Pts',(0.204857038450294,-0.106841121150014,
-0.442397968182778));
#84802=CARTESIAN_POINT('Ctrl Pts',(0.201165471430968,0.113639273471686,
-0.431313441424699));
#84803=CARTESIAN_POINT('Ctrl Pts',(0.014231951480288,0.230605470291321,
-0.420228914666617));
#84804=CARTESIAN_POINT('Ctrl Pts',(-0.185665476067071,0.137512771654142,
-0.409144387908539));
#84805=CARTESIAN_POINT('Ctrl Pts',(-0.21643992150198,-0.0808405328497407,
-0.398059861150457));
#84806=CARTESIAN_POINT('Ctrl Pts',(-0.0500588927583125,-0.225556065374089,
-0.386975334392379));
#84807=CARTESIAN_POINT('Ctrl Pts',(0.161920862274563,-0.164812213538526,
-0.375890807634297));
#84808=CARTESIAN_POINT('Ctrl Pts',(0.226406642260568,0.0460593498813293,
-0.364806280876218));
#84809=CARTESIAN_POINT('Ctrl Pts',(0.0846582460267547,0.214975377080661,
-0.353721754118138));
#84810=CARTESIAN_POINT('Ctrl Pts',(-0.134205483287707,0.188069985980317,
-0.342637227360058));
#84811=CARTESIAN_POINT('Ctrl Pts',(-0.230821221051348,-0.0101486591960582,
-0.331552700601978));
#84812=CARTESIAN_POINT('Ctrl Pts',(-0.117181535643009,-0.199122874316633,
-0.320468173843897));
#84813=CARTESIAN_POINT('Ctrl Pts',(0.103198999903502,-0.206715741513223,
-0.309383647085818));
#84814=CARTESIAN_POINT('Ctrl Pts',(0.229575399706078,-0.0260109058012938,
-0.298299120327737));
#84815=CARTESIAN_POINT('Ctrl Pts',(0.146831197016957,0.178387306043421,
-0.287214593569658));
#84816=CARTESIAN_POINT('Ctrl Pts',(-0.0696617802659827,0.220292232580522,
-0.276130066811577));
#84817=CARTESIAN_POINT('Ctrl Pts',(-0.22269972934094,0.0615326086078283,
-0.265045540053497));
#84818=CARTESIAN_POINT('Ctrl Pts',(-0.172880135196616,-0.153277168061375,
-0.253961013295417));
#84819=CARTESIAN_POINT('Ctrl Pts',(0.0344162534683956,-0.228466524511351,
-0.242876486537337));
#84820=CARTESIAN_POINT('Ctrl Pts',(0.210362821125352,-0.0955453550444726,
-0.231791959779257));
#84821=CARTESIAN_POINT('Ctrl Pts',(0.194689555384374,0.124408233407141,
-0.220707433021177));
#84822=CARTESIAN_POINT('Ctrl Pts',(0.0016732586647134,0.231038159699794,
-0.209622906263097));
#84823=CARTESIAN_POINT('Ctrl Pts',(-0.192867211244431,0.127215055631049,
-0.198538379505017));
#84824=CARTESIAN_POINT('Ctrl Pts',(-0.211724628416165,-0.0924884530479261,
-0.187453852746937));
#84825=CARTESIAN_POINT('Ctrl Pts',(-0.0377217364846146,-0.22794407107902,
-0.176369325988857));
#84826=CARTESIAN_POINT('Ctrl Pts',(0.170641940414384,-0.155765084281773,
-0.165284799230776));
#84827=CARTESIAN_POINT('Ctrl Pts',(0.223567609028329,0.0583006033089783,
-0.154200272472697));
#84828=CARTESIAN_POINT('Ctrl Pts',(0.0728451605707456,0.219260112672934,
-0.143115745714616));
#84829=CARTESIAN_POINT('Ctrl Pts',(-0.144232022717683,0.180495353940067,
-0.132031218956536));
#84830=CARTESIAN_POINT('Ctrl Pts',(-0.229928098932619,-0.0226831480769699,
-0.120946692198456));
#84831=CARTESIAN_POINT('Ctrl Pts',(-0.106182154709698,-0.205199088755477,
-0.109862165440376));
#84832=CARTESIAN_POINT('Ctrl Pts',(0.114285012279071,-0.200799695469481,
-0.0987776386822957));
#84833=CARTESIAN_POINT('Ctrl Pts',(0.230650297713861,-0.0134899214822133,
-0.0876931119242156));
#84834=CARTESIAN_POINT('Ctrl Pts',(0.136914862750022,0.186104771254577,
-0.0766085851661355));
#84835=CARTESIAN_POINT('Ctrl Pts',(-0.0815346538991313,0.216182177401989,
-0.0655240584080556));
#84836=CARTESIAN_POINT('Ctrl Pts',(-0.225717717433852,0.0493277497705959,
-0.0544395316499754));
#84837=CARTESIAN_POINT('Ctrl Pts',(-0.164287302485293,-0.162438194999925,
-0.0433550048918953));
#84838=CARTESIAN_POINT('Ctrl Pts',(0.0467796463453727,-0.226279314006825,
-0.0322704781338153));
#84839=CARTESIAN_POINT('Ctrl Pts',(0.215259778741053,-0.0839253033516204,
-0.0211859513757352));
#84840=CARTESIAN_POINT('Ctrl Pts',(0.187611971177778,0.134729602837997,
-0.0101014246176551));
#84841=CARTESIAN_POINT('Ctrl Pts',(-0.0108400899107792,0.230941269302219,
0.000983102140424831));
#84842=CARTESIAN_POINT('Ctrl Pts',(-0.199604920077247,0.116227920628962,
0.012067628898505));
#84843=CARTESIAN_POINT('Ctrl Pts',(-0.203936515089227,-0.0299908189741295,
0.0194573134038917));
#84844=CARTESIAN_POINT('Ctrl Pts',(-0.174767351138882,-0.087952107769144,
0.0231521556565851));
#84845=CARTESIAN_POINT('Ctrl Pts',(0.00540516581313481,0.195637521218248,
-4.85722573273506E-16));
#84846=CARTESIAN_POINT('Ctrl Pts',(0.000530987028742651,0.195316024296212,
-6.89315582075481E-16));
#84847=CARTESIAN_POINT('Ctrl Pts',(-0.00432231600472944,0.194799753536188,
-6.5733328270164E-16));
#84848=CARTESIAN_POINT('Ctrl Pts',(-0.00914525981218943,0.194083130228181,
-7.73686670285656E-16));
#84849=CARTESIAN_POINT('Ctrl Pts',(-0.0182975460219355,0.192723226011732,
-6.37220818447363E-16));
#84850=CARTESIAN_POINT('Ctrl Pts',(-0.0273404118900563,0.190642703413875,
-4.3456410221573E-16));
#84851=CARTESIAN_POINT('Ctrl Pts',(-0.0362103123303198,0.187887905371836,
-5.72458747072346E-16));
#84852=CARTESIAN_POINT('Ctrl Pts',(-0.0426952759989041,0.185873816787954,
-6.73276311825183E-16));
#84853=CARTESIAN_POINT('Ctrl Pts',(-0.0490889890704407,0.183497301278578,
-5.53257083171345E-16));
#84854=CARTESIAN_POINT('Ctrl Pts',(-0.0553333559413038,0.180788923207186,
-5.62050406216485E-16));
#84855=CARTESIAN_POINT('Ctrl Pts',(-0.0654069179123671,0.176419702931141,
-5.76236005246569E-16));
#84856=CARTESIAN_POINT('Ctrl Pts',(-0.0751114695691119,0.171183241386391,
-3.41160100153046E-16));
#84857=CARTESIAN_POINT('Ctrl Pts',(-0.0843298237574837,0.165151495399874,
-4.68375338513738E-16));
#84858=CARTESIAN_POINT('Ctrl Pts',(-0.0881916390397545,0.162624635577229,
-5.21669206551349E-16));
#84859=CARTESIAN_POINT('Ctrl Pts',(-0.0919679137130864,0.159957413059854,
-6.04042371500311E-16));
#84860=CARTESIAN_POINT('Ctrl Pts',(-0.0956347997707068,0.157166413867924,
-4.8919202022546E-16));
#84861=CARTESIAN_POINT('Ctrl Pts',(-0.104794954097449,0.150194290130738,
-2.02287293537293E-16));
#84862=CARTESIAN_POINT('Ctrl Pts',(-0.113294139529456,0.142440339385748,
-3.10624878440371E-16));
#84863=CARTESIAN_POINT('Ctrl Pts',(-0.120997002971,0.133986645954499,-1.07552855510562E-16));
#84864=CARTESIAN_POINT('Ctrl Pts',(-0.125172453318786,0.12940419717484,
2.52531933996346E-18));
#84865=CARTESIAN_POINT('Ctrl Pts',(-0.129113156531883,0.124615891131193,
-1.51055882874737E-16));
#84866=CARTESIAN_POINT('Ctrl Pts',(-0.132792406759928,0.119633076898729,
9.8879238130678E-17));
#84867=CARTESIAN_POINT('Ctrl Pts',(-0.135556286113385,0.115889950847057,
2.86632306781755E-16));
#84868=CARTESIAN_POINT('Ctrl Pts',(-0.138174807679848,0.112032992900381,
-3.37097310003989E-16));
#84869=CARTESIAN_POINT('Ctrl Pts',(-0.140624206910481,0.108085595299114,
-4.63171168085807E-16));
#84870=CARTESIAN_POINT('Ctrl Pts',(-0.140929371379385,0.107593798993523,
-4.78878391907511E-16));
#84871=CARTESIAN_POINT('Ctrl Pts',(-0.141231895824984,0.107100637144526,
-4.76751570490669E-16));
#84872=CARTESIAN_POINT('Ctrl Pts',(-0.141531732093613,0.106606173963904,
-4.82253126321552E-16));
#84873=CARTESIAN_POINT('Ctrl Pts',(-0.14512786301753,0.100675756197219,
-5.17611903429286E-16));
#84874=CARTESIAN_POINT('Ctrl Pts',(-0.148344736494633,0.094547001960059,
-1.53978557988108E-16));
#84875=CARTESIAN_POINT('Ctrl Pts',(-0.151148162339273,0.0882379718247826,
-1.64798730217797E-16));
#84876=CARTESIAN_POINT('Ctrl Pts',(-0.154328174579003,0.0810814447172957,
1.1508442599124E-16));
#84877=CARTESIAN_POINT('Ctrl Pts',(-0.1569763429285,0.0736927501953974,
9.29594947834426E-17));
#84878=CARTESIAN_POINT('Ctrl Pts',(-0.159093979189513,0.0661295205528138,
-5.3776427755281E-17));
#84879=CARTESIAN_POINT('Ctrl Pts',(-0.160234456452329,0.0620562566029943,
2.41628073730984E-16));
#84880=CARTESIAN_POINT('Ctrl Pts',(-0.161220877544346,0.057932365739095,
2.60879163199896E-17));
#84881=CARTESIAN_POINT('Ctrl Pts',(-0.162052257864859,0.0537670724081219,
8.84708972748172E-17));
#84882=CARTESIAN_POINT('Ctrl Pts',(-0.162804807434059,0.0499967285300273,
1.44938778802232E-16));
#84883=CARTESIAN_POINT('Ctrl Pts',(-0.163429545394715,0.0461947404422942,
-9.50192087901827E-17));
#84884=CARTESIAN_POINT('Ctrl Pts',(-0.163924812172196,0.0423819372460028,
-2.67147415300428E-16));
#84885=CARTESIAN_POINT('Ctrl Pts',(-0.165187320646542,0.0326625363792493,
-7.05927743950919E-16));
#84886=CARTESIAN_POINT('Ctrl Pts',(-0.165615374754996,0.0228510577214756,
2.09168582709701E-16));
#84887=CARTESIAN_POINT('Ctrl Pts',(-0.165212654472542,0.0130612428985379,
1.92554305833426E-16));
#84888=CARTESIAN_POINT('Ctrl Pts',(-0.164960053646113,0.00692071454025313,
1.82133226358855E-16));
#84889=CARTESIAN_POINT('Ctrl Pts',(-0.164380026075269,0.000788975702457714,
-7.40388912887612E-17));
#84890=CARTESIAN_POINT('Ctrl Pts',(-0.163468309056199,-0.00530325479555159,
-1.56125112837913E-17));
#84891=CARTESIAN_POINT('Ctrl Pts',(-0.16264648558514,-0.0107948030606855,
3.70531398039655E-17));
#84892=CARTESIAN_POINT('Ctrl Pts',(-0.161552824018776,-0.0162603049141666,
-7.32136910689234E-17));
#84893=CARTESIAN_POINT('Ctrl Pts',(-0.160193793940068,-0.021636056037818,
-1.15792792021452E-16));
#84894=CARTESIAN_POINT('Ctrl Pts',(-0.157557295101067,-0.0320649360297449,
-1.98395636495481E-16));
#84895=CARTESIAN_POINT('Ctrl Pts',(-0.153922696083113,-0.042186526932804,
6.12453783703427E-16));
#84896=CARTESIAN_POINT('Ctrl Pts',(-0.149273689660746,-0.0518329037170428,
1.85398571495021E-16));
#84897=CARTESIAN_POINT('Ctrl Pts',(-0.146262157372015,-0.0580816314054429,
-9.1239153600102E-17));
#84898=CARTESIAN_POINT('Ctrl Pts',(-0.14282411654673,-0.064130517147505,
8.59534368207069E-17));
#84899=CARTESIAN_POINT('Ctrl Pts',(-0.138946909435068,-0.0699253806456778,
-1.51788304147971E-18));
#84900=CARTESIAN_POINT('Ctrl Pts',(-0.0905532414578939,-0.126782311156848,
-0.9746));
#84901=CARTESIAN_POINT('Ctrl Pts',(-0.0940297960121039,-0.124924866292241,
-0.9746));
#84902=CARTESIAN_POINT('Ctrl Pts',(-0.0974241536190665,-0.122930444609242,
-0.9746));
#84903=CARTESIAN_POINT('Ctrl Pts',(-0.100727224830823,-0.120800921794934,
-0.9746));
#84904=CARTESIAN_POINT('Ctrl Pts',(-0.10828471896806,-0.115928530268235,
-0.9746));
#84905=CARTESIAN_POINT('Ctrl Pts',(-0.115365087206815,-0.110350660277646,
-0.9746));
#84906=CARTESIAN_POINT('Ctrl Pts',(-0.12193959644215,-0.104174135776912,
-0.9746));
#84907=CARTESIAN_POINT('Ctrl Pts',(-0.125553172842108,-0.10077930547541,
-0.9746));
#84908=CARTESIAN_POINT('Ctrl Pts',(-0.129009586137417,-0.0972064788121822,
-0.9746));
#84909=CARTESIAN_POINT('Ctrl Pts',(-0.132294618133166,-0.0934837784148553,
-0.9746));
#84910=CARTESIAN_POINT('Ctrl Pts',(-0.137791783897699,-0.0872542192500508,
-0.9746));
#84911=CARTESIAN_POINT('Ctrl Pts',(-0.142817433677964,-0.0805988103873133,
-0.9746));
#84912=CARTESIAN_POINT('Ctrl Pts',(-0.147349142107892,-0.0735898319648689,
-0.9746));
#84913=CARTESIAN_POINT('Ctrl Pts',(-0.15016186090448,-0.0692395332511452,
-0.9746));
#84914=CARTESIAN_POINT('Ctrl Pts',(-0.152782767435203,-0.0647533954404122,
-0.9746));
#84915=CARTESIAN_POINT('Ctrl Pts',(-0.155194586759511,-0.0601701145151422,
-0.9746));
#84916=CARTESIAN_POINT('Ctrl Pts',(-0.160644212994169,-0.0498139623276951,
-0.9746));
#84917=CARTESIAN_POINT('Ctrl Pts',(-0.165043005663089,-0.0389449931280598,
-0.9746));
#84918=CARTESIAN_POINT('Ctrl Pts',(-0.168323366438074,-0.027755975176349,
-0.9746));
#84919=CARTESIAN_POINT('Ctrl Pts',(-0.169980006434906,-0.0221053239414555,
-0.9746));
#84920=CARTESIAN_POINT('Ctrl Pts',(-0.171350852496603,-0.0163723993947195,
-0.9746));
#84921=CARTESIAN_POINT('Ctrl Pts',(-0.172423067159833,-0.0105792113265366,
-0.9746));
#84922=CARTESIAN_POINT('Ctrl Pts',(-0.173278550653338,-0.00595702424305383,
-0.9746));
#84923=CARTESIAN_POINT('Ctrl Pts',(-0.173942658225041,-0.00129956377914802,
-0.9746));
#84924=CARTESIAN_POINT('Ctrl Pts',(-0.174407751945051,0.00335988535112334,
-0.9746));
#84925=CARTESIAN_POINT('Ctrl Pts',(-0.174995692542755,0.00925005154507497,
-0.9746));
#84926=CARTESIAN_POINT('Ctrl Pts',(-0.175267577699845,0.0151526234854924,
-0.9746));
#84927=CARTESIAN_POINT('Ctrl Pts',(-0.175214225529177,0.0210443329477897,
-0.9746));
#84928=CARTESIAN_POINT('Ctrl Pts',(-0.175144700049102,0.0287220698364688,
-0.9746));
#84929=CARTESIAN_POINT('Ctrl Pts',(-0.174523326685391,0.0363814112077174,
-0.9746));
#84930=CARTESIAN_POINT('Ctrl Pts',(-0.173385196589427,0.0439834824917145,
-0.9746));
#84931=CARTESIAN_POINT('Ctrl Pts',(-0.172591342738426,0.0492859813763208,
-0.9746));
#84932=CARTESIAN_POINT('Ctrl Pts',(-0.171545526366501,0.0545620014471183,
-0.9746));
#84933=CARTESIAN_POINT('Ctrl Pts',(-0.170257892847336,0.0597943370226613,
-0.9746));
#84934=CARTESIAN_POINT('Ctrl Pts',(-0.16917772877666,0.0641836145696469,
-0.9746));
#84935=CARTESIAN_POINT('Ctrl Pts',(-0.167929193511731,0.0685340110951642,
-0.9746));
#84936=CARTESIAN_POINT('Ctrl Pts',(-0.166522756084503,0.0728284761344198,
-0.9746));
#84937=CARTESIAN_POINT('Ctrl Pts',(-0.163087091801193,0.0833190531523973,
-0.9746));
#84938=CARTESIAN_POINT('Ctrl Pts',(-0.158706981261738,0.0934946544278663,
-0.9746));
#84939=CARTESIAN_POINT('Ctrl Pts',(-0.153475389427475,0.103246175515399,
-0.9746));
#84940=CARTESIAN_POINT('Ctrl Pts',(-0.150477503861082,0.108834139034881,
-0.9746));
#84941=CARTESIAN_POINT('Ctrl Pts',(-0.147199377055609,0.114282853508606,
-0.9746));
#84942=CARTESIAN_POINT('Ctrl Pts',(-0.143653574449483,0.119570985860742,
-0.9746));
#84943=CARTESIAN_POINT('Ctrl Pts',(-0.140594184743723,0.124133692665932,
-0.9746));
#84944=CARTESIAN_POINT('Ctrl Pts',(-0.137333362290461,0.128578228872186,
-0.9746));
#84945=CARTESIAN_POINT('Ctrl Pts',(-0.133900829694537,0.132864190726999,
-0.9746));
#84946=CARTESIAN_POINT('Ctrl Pts',(-0.125893219189598,0.142862730351392,
-0.9746));
#84947=CARTESIAN_POINT('Ctrl Pts',(-0.11693274942408,0.152034765661666,
-0.9746));
#84948=CARTESIAN_POINT('Ctrl Pts',(-0.107134319818378,0.160216555670847,
-0.9746));
#84949=CARTESIAN_POINT('Ctrl Pts',(-0.100515704826846,0.165743167606786,
-0.974600000000001));
#84950=CARTESIAN_POINT('Ctrl Pts',(-0.0935136574613262,0.170817815415233,
-0.9746));
#84951=CARTESIAN_POINT('Ctrl Pts',(-0.0861525859670518,0.175382131162754,
-0.9746));
#84952=CARTESIAN_POINT('Origin',(-2.59090492670967E-17,0.,-0.9746));
#84953=CARTESIAN_POINT('',(-0.1954,-2.39295984553393E-17,-0.9746));
#84954=CARTESIAN_POINT('Origin',(0.,0.,-0.9746));
#84955=CARTESIAN_POINT('',(0.089187861459517,0.173858233536057,-0.9746));
#84956=CARTESIAN_POINT('Origin',(0.,0.,-0.9746));
#84957=CARTESIAN_POINT('Ctrl Pts',(0.0891878614595168,0.173858233536056,
-0.9746));
#84958=CARTESIAN_POINT('Ctrl Pts',(0.0923684083710216,0.171824919272554,
-0.9746));
#84959=CARTESIAN_POINT('Ctrl Pts',(0.0954821720660944,0.169694318827644,
-0.9746));
#84960=CARTESIAN_POINT('Ctrl Pts',(0.0985240274780785,0.167466145207355,
-0.9746));
#84961=CARTESIAN_POINT('Ctrl Pts',(0.105746831175391,0.162175406995579,
-0.9746));
#84962=CARTESIAN_POINT('Ctrl Pts',(0.112564936659085,0.156334970325733,
-0.9746));
#84963=CARTESIAN_POINT('Ctrl Pts',(0.118945973249969,0.150010093026968,
-0.9746));
#84964=CARTESIAN_POINT('Ctrl Pts',(0.123811088224797,0.145187795768224,
-0.9746));
#84965=CARTESIAN_POINT('Ctrl Pts',(0.128424432090268,0.140079378982527,
-0.9746));
#84966=CARTESIAN_POINT('Ctrl Pts',(0.132746242480251,0.1347416062205,-0.9746));
#84967=CARTESIAN_POINT('Ctrl Pts',(0.137683220397198,0.128644053603919,
-0.974600000000001));
#84968=CARTESIAN_POINT('Ctrl Pts',(0.142247212696115,0.12224100971048,-0.9746));
#84969=CARTESIAN_POINT('Ctrl Pts',(0.146414335551708,0.115576031346523,
-0.9746));
#84970=CARTESIAN_POINT('Ctrl Pts',(0.148827550732419,0.11171628745982,-0.9746));
#84971=CARTESIAN_POINT('Ctrl Pts',(0.151107538509771,0.107768645316273,
-0.9746));
#84972=CARTESIAN_POINT('Ctrl Pts',(0.153248499385483,0.103741352735909,
-0.9746));
#84973=CARTESIAN_POINT('Ctrl Pts',(0.155301440138075,0.0998796319755569,
-0.9746));
#84974=CARTESIAN_POINT('Ctrl Pts',(0.157222955525038,0.0959510427103076,
-0.9746));
#84975=CARTESIAN_POINT('Ctrl Pts',(0.159005757143888,0.0919709142949633,
-0.9746));
#84976=CARTESIAN_POINT('Ctrl Pts',(0.163158600449716,0.0826996361722365,
-0.9746));
#84977=CARTESIAN_POINT('Ctrl Pts',(0.166567079218136,0.0731365417482814,
-0.9746));
#84978=CARTESIAN_POINT('Ctrl Pts',(0.169173701012897,0.0633765445475195,
-0.9746));
#84979=CARTESIAN_POINT('Ctrl Pts',(0.170831815402072,0.0571680520729268,
-0.9746));
#84980=CARTESIAN_POINT('Ctrl Pts',(0.1721649817233,0.0508798122827543,-0.9746));
#84981=CARTESIAN_POINT('Ctrl Pts',(0.17315298703667,0.0445368070399667,
-0.9746));
#84982=CARTESIAN_POINT('Ctrl Pts',(0.174093136343655,0.0385010378973178,
-0.9746));
#84983=CARTESIAN_POINT('Ctrl Pts',(0.174720282450967,0.0324079620925687,
-0.9746));
#84984=CARTESIAN_POINT('Ctrl Pts',(0.175013450792712,0.0263260434350132,
-0.9746));
#84985=CARTESIAN_POINT('Ctrl Pts',(0.175314120252881,0.0200885104576577,
-0.9746));
#84986=CARTESIAN_POINT('Ctrl Pts',(0.175265697707793,0.0138545067086832,
-0.9746));
#84987=CARTESIAN_POINT('Ctrl Pts',(0.174851965608991,0.00764741813027898,
-0.9746));
#84988=CARTESIAN_POINT('Ctrl Pts',(0.17433114008016,-0.000166358467454291,
-0.9746));
#84989=CARTESIAN_POINT('Ctrl Pts',(0.173231574277968,-0.00793775250040705,
-0.9746));
#84990=CARTESIAN_POINT('Ctrl Pts',(0.171581280878545,-0.0156163834798823,
-0.9746));
#84991=CARTESIAN_POINT('Ctrl Pts',(0.170692439127582,-0.0197520649333607,
-0.9746));
#84992=CARTESIAN_POINT('Ctrl Pts',(0.169643681680851,-0.0238607579522018,
-0.9746));
#84993=CARTESIAN_POINT('Ctrl Pts',(0.168438435903388,-0.027933840546177,
-0.9746));
#84994=CARTESIAN_POINT('Ctrl Pts',(0.167347408280003,-0.0316209272014028,
-0.9746));
#84995=CARTESIAN_POINT('Ctrl Pts',(0.166128520428818,-0.0352764519303832,
-0.9746));
#84996=CARTESIAN_POINT('Ctrl Pts',(0.164790010901572,-0.0388812084305513,
-0.9746));
#84997=CARTESIAN_POINT('Ctrl Pts',(0.16137835252225,-0.04806918764839,-0.9746));
#84998=CARTESIAN_POINT('Ctrl Pts',(0.157185477598737,-0.0569498321473851,
-0.9746));
#84999=CARTESIAN_POINT('Ctrl Pts',(0.152267636060245,-0.0654242188104072,
-0.9746));
#85000=CARTESIAN_POINT('Ctrl Pts',(0.149183032157992,-0.0707395844978447,
-0.9746));
#85001=CARTESIAN_POINT('Ctrl Pts',(0.145812828254551,-0.0758946172057797,
-0.9746));
#85002=CARTESIAN_POINT('Ctrl Pts',(0.142167564876524,-0.0808601523014113,
-0.9746));
#85003=CARTESIAN_POINT('Ctrl Pts',(0.138881773074575,-0.0853360194247216,
-0.9746));
#85004=CARTESIAN_POINT('Ctrl Pts',(0.135367611992976,-0.0896621905227919,
-0.9746));
#85005=CARTESIAN_POINT('Ctrl Pts',(0.131660485192568,-0.0937853191898041,
-0.9746));
#85006=CARTESIAN_POINT('Ctrl Pts',(0.124468401335915,-0.101784475604323,
-0.9746));
#85007=CARTESIAN_POINT('Ctrl Pts',(0.116536365050231,-0.10904667878116,
-0.9746));
#85008=CARTESIAN_POINT('Ctrl Pts',(0.107928190692747,-0.115415747498982,
-0.9746));
#85009=CARTESIAN_POINT('Ctrl Pts',(0.102351941465377,-0.119541536898908,
-0.9746));
#85010=CARTESIAN_POINT('Ctrl Pts',(0.0964914220373157,-0.123291767245807,
-0.9746));
#85011=CARTESIAN_POINT('Ctrl Pts',(0.0903606778650203,-0.126612599672284,
-0.9746));
#85012=CARTESIAN_POINT('Ctrl Pts',(0.113597585008592,-0.159278481118232,
-0.997748074722608));
#85013=CARTESIAN_POINT('Ctrl Pts',(0.16644003092961,-0.121593162196469,
-0.994052057794214));
#85014=CARTESIAN_POINT('Ctrl Pts',(0.230765385058606,0.00981445541203181,
-0.986661198613126));
#85015=CARTESIAN_POINT('Ctrl Pts',(0.117189675071622,0.199275529823258,
-0.975575497179346));
#85016=CARTESIAN_POINT('Ctrl Pts',(-0.103218031716069,0.206613681168277,
-0.964490970421265));
#85017=CARTESIAN_POINT('Ctrl Pts',(-0.229553900654321,0.0260392872026454,
-0.953406443663186));
#85018=CARTESIAN_POINT('Ctrl Pts',(-0.146815211474769,-0.1784061830235,
-0.942321916905106));
#85019=CARTESIAN_POINT('Ctrl Pts',(0.0696715872818821,-0.220261620189527,
-0.931237390147025));
#85020=CARTESIAN_POINT('Ctrl Pts',(0.222687127489829,-0.0615221438598078,
-0.920152863388945));
#85021=CARTESIAN_POINT('Ctrl Pts',(0.172860435250692,0.153279874428372,
-0.909068336630866));
#85022=CARTESIAN_POINT('Ctrl Pts',(-0.034427118799567,0.228447496603342,
-0.897983809872785));
#85023=CARTESIAN_POINT('Ctrl Pts',(-0.210353898174444,0.0955279693800359,
-0.886899283114706));
#85024=CARTESIAN_POINT('Ctrl Pts',(-0.194669526643631,-0.124411313377869,
-0.875814756356625));
#85025=CARTESIAN_POINT('Ctrl Pts',(-0.0016600774612449,-0.231022463164353,
-0.864730229598545));
#85026=CARTESIAN_POINT('Ctrl Pts',(0.192861385988943,-0.127195753155124,
-0.853645702840465));
#85027=CARTESIAN_POINT('Ctrl Pts',(0.211705181679844,0.0924942334409426,
-0.842561176082385));
#85028=CARTESIAN_POINT('Ctrl Pts',(0.0377063431658909,0.227930832056205,
-0.831476649324304));
#85029=CARTESIAN_POINT('Ctrl Pts',(-0.170639242107946,0.155744994213846,
-0.820392122566225));
#85030=CARTESIAN_POINT('Ctrl Pts',(-0.223549277689542,-0.0583092770165013,
-0.809307595808144));
#85031=CARTESIAN_POINT('Ctrl Pts',(-0.0728279089482567,-0.219249498669582,
-0.798223069050065));
#85032=CARTESIAN_POINT('Ctrl Pts',(0.144232516508625,-0.18047501610888,
-0.787138542291984));
#85033=CARTESIAN_POINT('Ctrl Pts',(0.229911311338269,0.0226944598360864,
-0.776054015533904));
#85034=CARTESIAN_POINT('Ctrl Pts',(0.106163520338706,0.205191510592405,
-0.764969488775825));
#85035=CARTESIAN_POINT('Ctrl Pts',(-0.114288792391887,0.200779285496967,
-0.753884962017745));
#85036=CARTESIAN_POINT('Ctrl Pts',(-0.230635259730438,0.0134768834665719,
-0.742800435259663));
#85037=CARTESIAN_POINT('Ctrl Pts',(-0.136895696235943,-0.186101632754491,
-0.731715908501585));
#85038=CARTESIAN_POINT('Ctrl Pts',(0.0815423780626619,-0.216159871416477,
-0.720631381743503));
#85039=CARTESIAN_POINT('Ctrl Pts',(0.225703368478632,-0.0493177337732571,
-0.709546854985425));
#85040=CARTESIAN_POINT('Ctrl Pts',(0.164270795880326,0.162448007136189,
-0.698462328227344));
#85041=CARTESIAN_POINT('Ctrl Pts',(-0.0467963100731284,0.226239595948386,
-0.687377801469264));
#85042=CARTESIAN_POINT('Ctrl Pts',(-0.215236581581508,0.0839491712670712,
-0.676293274711184));
#85043=CARTESIAN_POINT('Ctrl Pts',(-0.187617503186297,-0.134810689135161,
-0.665208747953103));
#85044=CARTESIAN_POINT('Ctrl Pts',(0.0109026619765615,-0.230771275010779,
-0.654124221195024));
#85045=CARTESIAN_POINT('Ctrl Pts',(0.199491574731264,-0.116521933638534,
-0.643039694436944));
#85046=CARTESIAN_POINT('Ctrl Pts',(0.206363289762344,0.103867425336797,
-0.631955167678864));
#85047=CARTESIAN_POINT('Ctrl Pts',(0.0252583507465755,0.229643778764786,
-0.620870640920783));
#85048=CARTESIAN_POINT('Ctrl Pts',(-0.178854460771993,0.1462372431006,-0.609786114162703));
#85049=CARTESIAN_POINT('Ctrl Pts',(-0.220048455014294,-0.0703770335659106,
-0.598701587404623));
#85050=CARTESIAN_POINT('Ctrl Pts',(-0.0607999560716834,-0.222884756655582,
-0.587617060646543));
#85051=CARTESIAN_POINT('Ctrl Pts',(0.153831321085638,-0.17236639481282,
-0.576532533888463));
#85052=CARTESIAN_POINT('Ctrl Pts',(0.228337399334668,0.0351607945417151,
-0.565448007130383));
#85053=CARTESIAN_POINT('Ctrl Pts',(0.0948505716256339,0.210659959342106,
-0.554363480372303));
#85054=CARTESIAN_POINT('Ctrl Pts',(-0.125035795018697,0.194268626833483,
-0.543278953614223));
#85055=CARTESIAN_POINT('Ctrl Pts',(-0.23102685397145,0.000917688279968637,
-0.532194426856142));
#85056=CARTESIAN_POINT('Ctrl Pts',(-0.126575178392383,-0.193269174010399,
-0.521109900098063));
#85057=CARTESIAN_POINT('Ctrl Pts',(0.0931740316803935,-0.211406833447139,
-0.510025373339982));
#85058=CARTESIAN_POINT('Ctrl Pts',(0.228050865762629,-0.0369736667459479,
-0.498940846581903));
#85059=CARTESIAN_POINT('Ctrl Pts',(0.155195797780493,0.171138872729142,
-0.487856319823823));
#85060=CARTESIAN_POINT('Ctrl Pts',(-0.0590273731357318,0.223360736541632,
-0.476771793065742));
#85061=CARTESIAN_POINT('Ctrl Pts',(-0.219482414497422,0.0721229445745739,
-0.465687266307662));
#85062=CARTESIAN_POINT('Ctrl Pts',(-0.18001056989549,-0.14481175412799,
-0.454602739549582));
#85063=CARTESIAN_POINT('Ctrl Pts',(0.0234331936510666,-0.229837192036099,
-0.443518212791502));
#85064=CARTESIAN_POINT('Ctrl Pts',(0.205531623241974,-0.105503560391314,
-0.432433686033422));
#85065=CARTESIAN_POINT('Ctrl Pts',(0.200410965162878,0.11493343486647,-0.421349159275342));
#85066=CARTESIAN_POINT('Ctrl Pts',(0.0127356351310226,0.230677378616861,
-0.410264632517262));
#85067=CARTESIAN_POINT('Ctrl Pts',(-0.18654060551751,0.136296925500451,
-0.399180105759182));
#85068=CARTESIAN_POINT('Ctrl Pts',(-0.215896707223304,-0.0822366172567873,
-0.388095579001102));
#85069=CARTESIAN_POINT('Ctrl Pts',(-0.0485921495146213,-0.225860692492862,
-0.377011052243022));
#85070=CARTESIAN_POINT('Ctrl Pts',(0.162975075692969,-0.163747898033848,
-0.365926525484941));
#85071=CARTESIAN_POINT('Ctrl Pts',(0.226088041147545,0.0475231212957209,
-0.354841998726862));
#85072=CARTESIAN_POINT('Ctrl Pts',(0.0832570446511227,0.215505252660433,
-0.343757471968781));
#85073=CARTESIAN_POINT('Ctrl Pts',(-0.135412928329534,0.187183301200128,
-0.332672945210701));
#85074=CARTESIAN_POINT('Ctrl Pts',(-0.230735046119166,-0.0116442217304382,
-0.321588418452622));
#85075=CARTESIAN_POINT('Ctrl Pts',(-0.115880237623372,-0.199865004289646,
-0.310503891694541));
#85076=CARTESIAN_POINT('Ctrl Pts',(0.104530066545176,-0.206028431508216,
-0.299419364936461));
#85077=CARTESIAN_POINT('Ctrl Pts',(0.229723764209575,-0.0245202276603256,
-0.288334838178381));
#85078=CARTESIAN_POINT('Ctrl Pts',(0.145661713927447,0.179323491284942,
-0.277250311420301));
#85079=CARTESIAN_POINT('Ctrl Pts',(-0.0710838269339852,0.219821152099225,
-0.266165784662221));
#85080=CARTESIAN_POINT('Ctrl Pts',(-0.2230789949398,0.0600833707072694,
-0.255081257904141));
#85081=CARTESIAN_POINT('Ctrl Pts',(-0.171871146156301,-0.154384450868564,
-0.243996731146061));
#85082=CARTESIAN_POINT('Ctrl Pts',(0.0358944075470365,-0.228223225322811,
-0.232912204387981));
#85083=CARTESIAN_POINT('Ctrl Pts',(0.210963687025698,-0.0941730977777479,
-0.2218276776299));
#85084=CARTESIAN_POINT('Ctrl Pts',(0.193865803917006,0.125659461758854,
-0.21074315087182));
#85085=CARTESIAN_POINT('Ctrl Pts',(0.000175245362767064,0.23102860489061,
-0.199658624113741));
#85086=CARTESIAN_POINT('Ctrl Pts',(-0.193674941721658,0.125953436994848,
-0.18857409735566));
#85087=CARTESIAN_POINT('Ctrl Pts',(-0.211106316733187,-0.0938529552288718,
-0.17748957059758));
#85088=CARTESIAN_POINT('Ctrl Pts',(-0.0362405967794985,-0.228168472103057,
-0.1664050438395));
#85089=CARTESIAN_POINT('Ctrl Pts',(0.171636722311097,-0.154645086324223,
-0.15532051708142));
#85090=CARTESIAN_POINT('Ctrl Pts',(0.223169909972479,0.0597450007042502,
-0.14423599032334));
#85091=CARTESIAN_POINT('Ctrl Pts',(0.0714171971037106,0.219712808687961,
-0.13315146356526));
#85092=CARTESIAN_POINT('Ctrl Pts',(-0.145389424622739,0.179544742913656,
-0.12206693680718));
#85093=CARTESIAN_POINT('Ctrl Pts',(-0.229760834740975,-0.0241725925417204,
-0.1109824100491));
#85094=CARTESIAN_POINT('Ctrl Pts',(-0.10484225286162,-0.205867887802041,
-0.0998978832910191));
#85095=CARTESIAN_POINT('Ctrl Pts',(0.115576399225017,-0.20004385999579,
-0.0888133565329394));
#85096=CARTESIAN_POINT('Ctrl Pts',(0.230718050422665,-0.0119879999976286,
-0.0777288297748591));
#85097=CARTESIAN_POINT('Ctrl Pts',(0.135694965983318,0.186965739133346,
-0.0666443030167789));
#85098=CARTESIAN_POINT('Ctrl Pts',(-0.0829266138056062,0.215654003403905,
-0.055559776258699));
#85099=CARTESIAN_POINT('Ctrl Pts',(-0.22602215760672,0.0478228193903156,
-0.0444752495006188));
#85100=CARTESIAN_POINT('Ctrl Pts',(-0.163210881612501,-0.163417818613872,
-0.0333907227425388));
#85101=CARTESIAN_POINT('Ctrl Pts',(0.0482249176056553,-0.226094038071907,
-0.0223061959844587));
#85102=CARTESIAN_POINT('Ctrl Pts',(0.215825725144946,-0.0822379657419614,
-0.0112216692263785));
#85103=CARTESIAN_POINT('Ctrl Pts',(0.196338036420179,0.0627312190287936,
-0.00383198472099195));
#85104=CARTESIAN_POINT('Ctrl Pts',(0.158139484186755,0.115177904597422,
-0.000137142468298633));
#85105=CARTESIAN_POINT('Ctrl Pts',(0.105785576840747,-0.148325037034332,
-0.989980505168611));
#85106=CARTESIAN_POINT('Ctrl Pts',(0.154994093227852,-0.113231305065781,
-0.986284488240217));
#85107=CARTESIAN_POINT('Ctrl Pts',(0.214895848106765,0.00913952375890018,
-0.978893629059131));
#85108=CARTESIAN_POINT('Ctrl Pts',(0.109130641961213,0.185571523118247,
-0.967807927625349));
#85109=CARTESIAN_POINT('Ctrl Pts',(-0.0961198164963202,0.192405036109906,
-0.956723400867269));
#85110=CARTESIAN_POINT('Ctrl Pts',(-0.213767676442455,0.0242485878290922,
-0.945638874109188));
#85111=CARTESIAN_POINT('Ctrl Pts',(-0.136718855719335,-0.16613734333938,
-0.93455434735111));
#85112=CARTESIAN_POINT('Ctrl Pts',(0.064880332178426,-0.205114418109014,
-0.923469820593028));
#85113=CARTESIAN_POINT('Ctrl Pts',(0.207373125359477,-0.0572913189677125,
-0.91238529383495));
#85114=CARTESIAN_POINT('Ctrl Pts',(0.16097297186867,0.142738949364604,-0.901300767076867));
#85115=CARTESIAN_POINT('Ctrl Pts',(-0.0320595954650073,0.212737358845976,
-0.89021624031879));
#85116=CARTESIAN_POINT('Ctrl Pts',(-0.195888041611099,0.0889585931296678,
-0.879131713560708));
#85117=CARTESIAN_POINT('Ctrl Pts',(-0.181282270813716,-0.115855654415518,
-0.868047186802629));
#85118=CARTESIAN_POINT('Ctrl Pts',(-0.00154591536276689,-0.215135247172401,
-0.856962660044548));
#85119=CARTESIAN_POINT('Ctrl Pts',(0.179598474435907,-0.118448610665361,
-0.845878133286468));
#85120=CARTESIAN_POINT('Ctrl Pts',(0.19714639851264,0.086133484600512,-0.834793606528389));
#85121=CARTESIAN_POINT('Ctrl Pts',(0.0351133103935012,0.212256224875146,
-0.823709079770307));
#85122=CARTESIAN_POINT('Ctrl Pts',(-0.158904528266968,0.145034544983717,
-0.812624553012229));
#85123=CARTESIAN_POINT('Ctrl Pts',(-0.208175986231854,-0.0542993982124802,
-0.801540026254147));
#85124=CARTESIAN_POINT('Ctrl Pts',(-0.0678195963198858,-0.204171899315044,
-0.790455499496069));
#85125=CARTESIAN_POINT('Ctrl Pts',(0.134313770463549,-0.168063904553753,
-0.779370972737988));
#85126=CARTESIAN_POINT('Ctrl Pts',(0.214100508301226,0.0211337813622365,
-0.768286445979907));
#85127=CARTESIAN_POINT('Ctrl Pts',(0.098862746401033,0.191080666980729,
-0.757201919221828));
#85128=CARTESIAN_POINT('Ctrl Pts',(-0.106429250487093,0.186971866808289,
-0.746117392463747));
#85129=CARTESIAN_POINT('Ctrl Pts',(-0.21477467138544,0.0125500897877264,
-0.735032865705668));
#85130=CARTESIAN_POINT('Ctrl Pts',(-0.127481497007524,-0.173303583614474,
-0.723948338947588));
#85131=CARTESIAN_POINT('Ctrl Pts',(0.0759347788922858,-0.201294743069443,
-0.712863812189507));
#85132=CARTESIAN_POINT('Ctrl Pts',(0.21018194205102,-0.045926195660653,
-0.701779285431428));
#85133=CARTESIAN_POINT('Ctrl Pts',(0.152974034606232,0.151276597475482,
-0.690694758673347));
#85134=CARTESIAN_POINT('Ctrl Pts',(-0.0435781680986445,0.210681293619115,
-0.679610231915267));
#85135=CARTESIAN_POINT('Ctrl Pts',(-0.200434947081913,0.0781760589991238,
-0.668525705157188));
#85136=CARTESIAN_POINT('Ctrl Pts',(-0.174715208941123,-0.125539874050871,
-0.657441178399106));
#85137=CARTESIAN_POINT('Ctrl Pts',(0.0101528952944126,-0.214901333011996,
-0.646356651641028));
#85138=CARTESIAN_POINT('Ctrl Pts',(0.18577271080384,-0.108508820531872,
-0.635272124882946));
#85139=CARTESIAN_POINT('Ctrl Pts',(0.192171863905492,0.0967245518765679,
-0.624187598124867));
#85140=CARTESIAN_POINT('Ctrl Pts',(0.0235213557010934,0.213851373712605,
-0.613103071366787));
#85141=CARTESIAN_POINT('Ctrl Pts',(-0.166554793412863,0.136180633732903,
-0.602018544608706));
#85142=CARTESIAN_POINT('Ctrl Pts',(-0.204915912119448,-0.065537265528554,
-0.590934017850627));
#85143=CARTESIAN_POINT('Ctrl Pts',(-0.056618795412319,-0.207557163737565,
-0.579849491092546));
#85144=CARTESIAN_POINT('Ctrl Pts',(0.143252473509781,-0.160512906166578,
-0.568764964334467));
#85145=CARTESIAN_POINT('Ctrl Pts',(0.212634832871727,0.0327428169577119,
-0.557680437576386));
#85146=CARTESIAN_POINT('Ctrl Pts',(0.0883277794359205,0.196173055215632,
-0.546595910818307));
#85147=CARTESIAN_POINT('Ctrl Pts',(-0.116437190991286,0.180908940538528,
-0.535511384060226));
#85148=CARTESIAN_POINT('Ctrl Pts',(-0.215139336027473,0.000854579646644794,
-0.524426857302147));
#85149=CARTESIAN_POINT('Ctrl Pts',(-0.117870712295035,-0.179978219226038,
-0.513342330544065));
#85150=CARTESIAN_POINT('Ctrl Pts',(0.0867665337000174,-0.196868567431163,
-0.502257803785986));
#85151=CARTESIAN_POINT('Ctrl Pts',(0.21236800396687,-0.0344310195004734,
-0.491173277027906));
#85152=CARTESIAN_POINT('Ctrl Pts',(0.144523116316493,0.159369799720287,
-0.480088750269826));
#85153=CARTESIAN_POINT('Ctrl Pts',(-0.0549681114795289,0.208000410896443,
-0.469004223511746));
#85154=CARTESIAN_POINT('Ctrl Pts',(-0.204388797721832,0.0671631117395441,
-0.457919696753665));
#85155=CARTESIAN_POINT('Ctrl Pts',(-0.167631397906793,-0.134853174410277,
-0.446835169995586));
#85156=CARTESIAN_POINT('Ctrl Pts',(0.0218217130884572,-0.214031486119685,
-0.435750643237505));
#85157=CARTESIAN_POINT('Ctrl Pts',(0.191397390376061,-0.0982481713313137,
-0.424666116479425));
#85158=CARTESIAN_POINT('Ctrl Pts',(0.186628875546626,0.107029561453428,
-0.413581589721345));
#85159=CARTESIAN_POINT('Ctrl Pts',(0.0118598164623526,0.214813893792287,
-0.402497062963266));
#85160=CARTESIAN_POINT('Ctrl Pts',(-0.173712368598325,0.126923903220257,
-0.391412536205185));
#85161=CARTESIAN_POINT('Ctrl Pts',(-0.201049676451375,-0.0765812758544393,
-0.380328009447106));
#85162=CARTESIAN_POINT('Ctrl Pts',(-0.0452505092071028,-0.210328447028174,
-0.369243482689025));
#85163=CARTESIAN_POINT('Ctrl Pts',(0.151767419981167,-0.152487095994691,
-0.358158955930945));
#85164=CARTESIAN_POINT('Ctrl Pts',(0.210540161111511,0.0442549971388958,
-0.347074429172865));
#85165=CARTESIAN_POINT('Ctrl Pts',(0.0775315293349641,0.200685141881938,
-0.335989902414785));
#85166=CARTESIAN_POINT('Ctrl Pts',(-0.126100697774086,0.174310866651902,
-0.324905375656704));
#85167=CARTESIAN_POINT('Ctrl Pts',(-0.214867595550083,-0.0108434586221435,
-0.313820848898625));
#85168=CARTESIAN_POINT('Ctrl Pts',(-0.10791125339948,-0.186120459932837,
-0.302736322140544));
#85169=CARTESIAN_POINT('Ctrl Pts',(0.0973416238192642,-0.191860033565348,
-0.291651795382465));
#85170=CARTESIAN_POINT('Ctrl Pts',(0.213925858627184,-0.0228339927043137,
-0.280567268624384));
#85171=CARTESIAN_POINT('Ctrl Pts',(0.135644683205733,0.166991569101047,
-0.269482741866305));
#85172=CARTESIAN_POINT('Ctrl Pts',(-0.0661954533249173,0.204704240630249,
-0.258398215108224));
#85173=CARTESIAN_POINT('Ctrl Pts',(-0.207738044422124,0.0559514890067786,
-0.247313688350144));
#85174=CARTESIAN_POINT('Ctrl Pts',(-0.160051715333997,-0.143767565033517,
-0.236229161592064));
#85175=CARTESIAN_POINT('Ctrl Pts',(0.0334259800279473,-0.212528510508417,
-0.225144634833984));
#85176=CARTESIAN_POINT('Ctrl Pts',(0.196455895807788,-0.0876968948815729,
-0.214060108075904));
#85177=CARTESIAN_POINT('Ctrl Pts',(0.180533819407379,0.117017968706402,
-0.202975581317824));
#85178=CARTESIAN_POINT('Ctrl Pts',(0.000163193889970841,0.215140966537429,
-0.191891054559744));
#85179=CARTESIAN_POINT('Ctrl Pts',(-0.180356082640966,0.117291727518387,
-0.180806527801664));
#85180=CARTESIAN_POINT('Ctrl Pts',(-0.196588716993028,-0.0873987682602953,
-0.169722001043584));
#85181=CARTESIAN_POINT('Ctrl Pts',(-0.033748362124794,-0.21247752262047,
-0.158637474285504));
#85182=CARTESIAN_POINT('Ctrl Pts',(0.159833412614901,-0.144010276813171,
-0.147552947527423));
#85183=CARTESIAN_POINT('Ctrl Pts',(0.207822707306238,0.0556363884176943,
-0.136468420769343));
#85184=CARTESIAN_POINT('Ctrl Pts',(0.0665058979149409,0.204603347902146,
-0.125383894011263));
#85185=CARTESIAN_POINT('Ctrl Pts',(-0.135391119002199,0.167197605445644,
-0.114299367253183));
#85186=CARTESIAN_POINT('Ctrl Pts',(-0.21396037985004,-0.0225102641536699,
-0.103214840495103));
#85187=CARTESIAN_POINT('Ctrl Pts',(-0.0976323413513673,-0.191710530311696,
-0.0921303137370228));
#85188=CARTESIAN_POINT('Ctrl Pts',(0.107628309706322,-0.186287015885978,
-0.0810457869789431));
#85189=CARTESIAN_POINT('Ctrl Pts',(0.214851768633005,-0.0111635955537256,
-0.0699612602208629));
#85190=CARTESIAN_POINT('Ctrl Pts',(0.126363339941118,0.174108266141238,
-0.0588767334627826));
#85191=CARTESIAN_POINT('Ctrl Pts',(-0.0772238219343526,0.200823663164785,
-0.0477922067047027));
#85192=CARTESIAN_POINT('Ctrl Pts',(-0.210478808325096,0.0445340852534203,
-0.0367076799466226));
#85193=CARTESIAN_POINT('Ctrl Pts',(-0.151987009730526,-0.152179715852388,
-0.0256231531885425));
#85194=CARTESIAN_POINT('Ctrl Pts',(0.0449085315205072,-0.210545745632544,
-0.0145386264304624));
#85195=CARTESIAN_POINT('Ctrl Pts',(0.200983575749465,-0.0765825316054464,
-0.00345409967238224));
#85196=CARTESIAN_POINT('Ctrl Pts',(0.182836038608719,0.0584172470777646,
0.00393558483300434));
#85197=CARTESIAN_POINT('Ctrl Pts',(0.147264367941702,0.107257219211354,
0.00763042708569767));
#85198=CARTESIAN_POINT('Ctrl Pts',(0.0979735686729031,-0.137371592950432,
-0.982212935614615));
#85199=CARTESIAN_POINT('Ctrl Pts',(0.143548155526095,-0.104869447935093,
-0.978516918686221));
#85200=CARTESIAN_POINT('Ctrl Pts',(0.199026311154924,0.00846459210576822,
-0.971126059505134));
#85201=CARTESIAN_POINT('Ctrl Pts',(0.101071608850804,0.171867516413235,
-0.960040358071353));
#85202=CARTESIAN_POINT('Ctrl Pts',(-0.0890216012765712,0.178196391051536,
-0.948955831313273));
#85203=CARTESIAN_POINT('Ctrl Pts',(-0.197981452230588,0.0224578884555389,
-0.937871304555193));
#85204=CARTESIAN_POINT('Ctrl Pts',(-0.126622499963902,-0.153868503655261,
-0.926786777797113));
#85205=CARTESIAN_POINT('Ctrl Pts',(0.0600890770749705,-0.189967216028501,
-0.915702251039033));
#85206=CARTESIAN_POINT('Ctrl Pts',(0.192059123229125,-0.0530604940756169,
-0.904617724280951));
#85207=CARTESIAN_POINT('Ctrl Pts',(0.149085508486649,0.132198024300836,
-0.893533197522875));
#85208=CARTESIAN_POINT('Ctrl Pts',(-0.0296920721304479,0.197027221088611,
-0.882448670764791));
#85209=CARTESIAN_POINT('Ctrl Pts',(-0.181422185047754,0.0823892168792999,
-0.871364144006712));
#85210=CARTESIAN_POINT('Ctrl Pts',(-0.1678950149838,-0.107299995453168,
-0.860279617248632));
#85211=CARTESIAN_POINT('Ctrl Pts',(-0.00143175326428869,-0.19924803118045,
-0.849195090490551));
#85212=CARTESIAN_POINT('Ctrl Pts',(0.16633556288287,-0.109701468175598,
-0.838110563732473));
#85213=CARTESIAN_POINT('Ctrl Pts',(0.182587615345437,0.0797727357600818,
-0.827026036974391));
#85214=CARTESIAN_POINT('Ctrl Pts',(0.0325202776211112,0.196581617694085,
-0.815941510216311));
#85215=CARTESIAN_POINT('Ctrl Pts',(-0.147169814425989,0.13432409575359,
-0.804856983458232));
#85216=CARTESIAN_POINT('Ctrl Pts',(-0.192802694774166,-0.0502895194084593,
-0.793772456700151));
#85217=CARTESIAN_POINT('Ctrl Pts',(-0.062811283691515,-0.189094299960506,
-0.782687929942072));
#85218=CARTESIAN_POINT('Ctrl Pts',(0.124395024418474,-0.155652792998626,
-0.771603403183991));
#85219=CARTESIAN_POINT('Ctrl Pts',(0.198289705264184,0.0195731028883869,
-0.760518876425912));
#85220=CARTESIAN_POINT('Ctrl Pts',(0.0915619724633603,0.176969823369053,
-0.749434349667831));
#85221=CARTESIAN_POINT('Ctrl Pts',(-0.0985697085822984,0.17316444811961,
-0.738349822909751));
#85222=CARTESIAN_POINT('Ctrl Pts',(-0.198914083040442,0.011623296108881,
-0.727265296151671));
#85223=CARTESIAN_POINT('Ctrl Pts',(-0.118067297779106,-0.160505534474456,
-0.716180769393592));
#85224=CARTESIAN_POINT('Ctrl Pts',(0.0703271797219096,-0.186429614722409,
-0.705096242635511));
#85225=CARTESIAN_POINT('Ctrl Pts',(0.194660515623409,-0.0425346575480492,
-0.694011715877431));
#85226=CARTESIAN_POINT('Ctrl Pts',(0.141677273332138,0.140105187814775,
-0.682927189119351));
#85227=CARTESIAN_POINT('Ctrl Pts',(-0.0403600261241604,0.195122991289844,
-0.67184266236127));
#85228=CARTESIAN_POINT('Ctrl Pts',(-0.185633312582319,0.0724029467311765,
-0.660758135603191));
#85229=CARTESIAN_POINT('Ctrl Pts',(-0.161812914695948,-0.116269058966581,
-0.64967360884511));
#85230=CARTESIAN_POINT('Ctrl Pts',(0.00940312861226361,-0.199031391013213,
-0.638589082087031));
#85231=CARTESIAN_POINT('Ctrl Pts',(0.172053846876416,-0.100495707425211,
-0.62750455532895));
#85232=CARTESIAN_POINT('Ctrl Pts',(0.17798043804864,0.089581678416339,-0.616420028570871));
#85233=CARTESIAN_POINT('Ctrl Pts',(0.0217843606556112,0.198058968660423,
-0.60533550181279));
#85234=CARTESIAN_POINT('Ctrl Pts',(-0.154255126053732,0.126124024365207,
-0.59425097505471));
#85235=CARTESIAN_POINT('Ctrl Pts',(-0.189783369224603,-0.0606974974911975,
-0.58316644829663));
#85236=CARTESIAN_POINT('Ctrl Pts',(-0.0524376347529544,-0.192229570819549,
-0.57208192153855));
#85237=CARTESIAN_POINT('Ctrl Pts',(0.132673625933925,-0.148659417520336,
-0.56099739478047));
#85238=CARTESIAN_POINT('Ctrl Pts',(0.196932266408787,0.0303248393737088,
-0.54991286802239));
#85239=CARTESIAN_POINT('Ctrl Pts',(0.0818049872462071,0.181686151089158,
-0.53882834126431));
#85240=CARTESIAN_POINT('Ctrl Pts',(-0.107838586963876,0.167549254243574,
-0.52774381450623));
#85241=CARTESIAN_POINT('Ctrl Pts',(-0.199251818083495,0.000791471013320985,
-0.51665928774815));
#85242=CARTESIAN_POINT('Ctrl Pts',(-0.109166246197688,-0.166687264441677,
-0.50557476099007));
#85243=CARTESIAN_POINT('Ctrl Pts',(0.0803590357196412,-0.182330301415187,
-0.494490234231989));
#85244=CARTESIAN_POINT('Ctrl Pts',(0.196685142171111,-0.0318883722549989,
-0.48340570747391));
#85245=CARTESIAN_POINT('Ctrl Pts',(0.133850434852491,0.147600726711432,
-0.472321180715829));
#85246=CARTESIAN_POINT('Ctrl Pts',(-0.0509088498233257,0.192640085251252,
-0.461236653957749));
#85247=CARTESIAN_POINT('Ctrl Pts',(-0.189295180946243,0.0622032789045141,
-0.450152127199669));
#85248=CARTESIAN_POINT('Ctrl Pts',(-0.155252225918095,-0.124894594692565,
-0.439067600441589));
#85249=CARTESIAN_POINT('Ctrl Pts',(0.020210232525848,-0.198225780203272,
-0.427983073683509));
#85250=CARTESIAN_POINT('Ctrl Pts',(0.17726315751015,-0.0909927822713134,
-0.416898546925429));
#85251=CARTESIAN_POINT('Ctrl Pts',(0.172846785930375,0.0991256880403857,
-0.405814020167349));
#85252=CARTESIAN_POINT('Ctrl Pts',(0.0109839977936825,0.198950408967714,
-0.394729493409269));
#85253=CARTESIAN_POINT('Ctrl Pts',(-0.16088413167914,0.117550880940063,
-0.383644966651188));
#85254=CARTESIAN_POINT('Ctrl Pts',(-0.186202645679447,-0.0709259344520911,
-0.372560439893108));
#85255=CARTESIAN_POINT('Ctrl Pts',(-0.0419088688995842,-0.194796201563484,
-0.361475913135029));
#85256=CARTESIAN_POINT('Ctrl Pts',(0.140559764269364,-0.141226293955535,
-0.350391386376948));
#85257=CARTESIAN_POINT('Ctrl Pts',(0.194992281075478,0.0409868729820711,
-0.339306859618868));
#85258=CARTESIAN_POINT('Ctrl Pts',(0.0718060140188057,0.185865031103444,
-0.328222332860789));
#85259=CARTESIAN_POINT('Ctrl Pts',(-0.116788467218639,0.161438432103676,
-0.317137806102708));
#85260=CARTESIAN_POINT('Ctrl Pts',(-0.199000144981,-0.0100426955138486,
-0.306053279344628));
#85261=CARTESIAN_POINT('Ctrl Pts',(-0.0999422691755887,-0.172375915576028,
-0.294968752586547));
#85262=CARTESIAN_POINT('Ctrl Pts',(0.0901531810933522,-0.177691635622479,
-0.283884225828468));
#85263=CARTESIAN_POINT('Ctrl Pts',(0.198127953044795,-0.0211477577483022,
-0.272799699070387));
#85264=CARTESIAN_POINT('Ctrl Pts',(0.125627652484019,0.154659646917152,
-0.261715172312308));
#85265=CARTESIAN_POINT('Ctrl Pts',(-0.0613070797158493,0.189587329161274,
-0.250630645554227));
#85266=CARTESIAN_POINT('Ctrl Pts',(-0.192397093904447,0.0518196073062874,
-0.239546118796148));
#85267=CARTESIAN_POINT('Ctrl Pts',(-0.148232284511692,-0.133150679198468,
-0.228461592038067));
#85268=CARTESIAN_POINT('Ctrl Pts',(0.030957552508858,-0.196833795694023,
-0.217377065279988));
#85269=CARTESIAN_POINT('Ctrl Pts',(0.181948104589878,-0.0812206919853976,
-0.206292538521907));
#85270=CARTESIAN_POINT('Ctrl Pts',(0.167201834897751,0.10837647565395,-0.195208011763827));
#85271=CARTESIAN_POINT('Ctrl Pts',(0.00015114241717486,0.199253328184248,
-0.184123485005747));
#85272=CARTESIAN_POINT('Ctrl Pts',(-0.167037223560273,0.108630018041926,
-0.173038958247667));
#85273=CARTESIAN_POINT('Ctrl Pts',(-0.18207111725287,-0.0809445812917186,
-0.161954431489587));
#85274=CARTESIAN_POINT('Ctrl Pts',(-0.0312561274700897,-0.196786573137883,
-0.150869904731507));
#85275=CARTESIAN_POINT('Ctrl Pts',(0.148030102918704,-0.133375467302118,
-0.139785377973427));
#85276=CARTESIAN_POINT('Ctrl Pts',(0.192475504639999,0.0515277761311382,
-0.128700851215347));
#85277=CARTESIAN_POINT('Ctrl Pts',(0.0615945987261712,0.189493887116332,
-0.117616324457267));
#85278=CARTESIAN_POINT('Ctrl Pts',(-0.125392813381662,0.154850467977633,
-0.106531797699187));
#85279=CARTESIAN_POINT('Ctrl Pts',(-0.198159924959106,-0.0208479357656191,
-0.0954472709411068));
#85280=CARTESIAN_POINT('Ctrl Pts',(-0.0904224298411148,-0.177553172821352,
-0.0843627441830265));
#85281=CARTESIAN_POINT('Ctrl Pts',(0.0996802201876276,-0.172530171776165,
-0.0732782174249468));
#85282=CARTESIAN_POINT('Ctrl Pts',(0.198985486843346,-0.0103391911098226,
-0.0621936906668666));
#85283=CARTESIAN_POINT('Ctrl Pts',(0.117031713898918,0.161250793149128,
-0.0511091639087864));
#85284=CARTESIAN_POINT('Ctrl Pts',(-0.0715210300630994,0.185993322925665,
-0.0400246371507064));
#85285=CARTESIAN_POINT('Ctrl Pts',(-0.194935459043471,0.0412453511165247,
-0.0289401103926264));
#85286=CARTESIAN_POINT('Ctrl Pts',(-0.140763137848552,-0.140941613090905,
-0.0178555836345462));
#85287=CARTESIAN_POINT('Ctrl Pts',(0.0415921454353594,-0.194997453193184,
-0.00677105687646613));
#85288=CARTESIAN_POINT('Ctrl Pts',(0.186141426353985,-0.0709270974689309,
0.00431346988161405));
#85289=CARTESIAN_POINT('Ctrl Pts',(0.16933404079726,0.0541032751267355,
0.0117031543870006));
#85290=CARTESIAN_POINT('Ctrl Pts',(0.136389251696648,0.0993365338252848,
0.0153979966396939));
#85291=CARTESIAN_POINT('Ctrl Pts',(0.0901615605050589,-0.126418148866534,
-0.974445366060619));
#85292=CARTESIAN_POINT('Ctrl Pts',(0.132102217824338,-0.0965075908044056,
-0.970749349132225));
#85293=CARTESIAN_POINT('Ctrl Pts',(0.183156774203084,0.00778966045263656,
-0.963358489951137));
#85294=CARTESIAN_POINT('Ctrl Pts',(0.0930125757403958,0.158163509708224,
-0.952272788517358));
#85295=CARTESIAN_POINT('Ctrl Pts',(-0.0819233860568225,0.163987745993166,
-0.941188261759276));
#85296=CARTESIAN_POINT('Ctrl Pts',(-0.182195228018721,0.0206671890819858,
-0.930103735001198));
#85297=CARTESIAN_POINT('Ctrl Pts',(-0.116526144208468,-0.141599663971141,
-0.919019208243116));
#85298=CARTESIAN_POINT('Ctrl Pts',(0.0552978219715147,-0.174820013947988,
-0.907934681485038));
#85299=CARTESIAN_POINT('Ctrl Pts',(0.176745121098773,-0.0488296691835216,
-0.896850154726956));
#85300=CARTESIAN_POINT('Ctrl Pts',(0.137198045104627,0.121657099237068,
-0.885765627968878));
#85301=CARTESIAN_POINT('Ctrl Pts',(-0.027324548795888,0.181317083331244,
-0.874681101210796));
#85302=CARTESIAN_POINT('Ctrl Pts',(-0.166956328484408,0.0758198406289321,
-0.863596574452717));
#85303=CARTESIAN_POINT('Ctrl Pts',(-0.154507759153884,-0.0987443364908174,
-0.852512047694636));
#85304=CARTESIAN_POINT('Ctrl Pts',(-0.00131759116581058,-0.183360815188498,
-0.841427520936557));
#85305=CARTESIAN_POINT('Ctrl Pts',(0.153072651329834,-0.100954325685835,
-0.830342994178476));
#85306=CARTESIAN_POINT('Ctrl Pts',(0.168028832178233,0.0734119869196514,
-0.819258467420397));
#85307=CARTESIAN_POINT('Ctrl Pts',(0.0299272448487212,0.180907010513025,
-0.808173940662315));
#85308=CARTESIAN_POINT('Ctrl Pts',(-0.13543510058501,0.123613646523463,
-0.797089413904237));
#85309=CARTESIAN_POINT('Ctrl Pts',(-0.177429403316478,-0.0462796406044383,
-0.786004887146155));
#85310=CARTESIAN_POINT('Ctrl Pts',(-0.0578029710631441,-0.174016700605967,
-0.774920360388076));
#85311=CARTESIAN_POINT('Ctrl Pts',(0.114476278373398,-0.1432416814435,-0.763835833629995));
#85312=CARTESIAN_POINT('Ctrl Pts',(0.182478902227141,0.0180124244145374,
-0.752751306871914));
#85313=CARTESIAN_POINT('Ctrl Pts',(0.0842611985256882,0.162858979757378,
-0.741666780113836));
#85314=CARTESIAN_POINT('Ctrl Pts',(-0.0907101666775044,0.15935702943093,
-0.730582253355755));
#85315=CARTESIAN_POINT('Ctrl Pts',(-0.183053494695443,0.0106965024300354,
-0.719497726597676));
#85316=CARTESIAN_POINT('Ctrl Pts',(-0.108653098550686,-0.147707485334438,
-0.708413199839595));
#85317=CARTESIAN_POINT('Ctrl Pts',(0.0647195805515337,-0.171564486375374,
-0.697328673081514));
#85318=CARTESIAN_POINT('Ctrl Pts',(0.179139089195798,-0.0391431194354451,
-0.686244146323435));
#85319=CARTESIAN_POINT('Ctrl Pts',(0.130380512058046,0.128933778154068,
-0.675159619565355));
#85320=CARTESIAN_POINT('Ctrl Pts',(-0.0371418841496764,0.179564688960573,
-0.664075092807276));
#85321=CARTESIAN_POINT('Ctrl Pts',(-0.170831678082726,0.0666298344632292,
-0.652990566049193));
#85322=CARTESIAN_POINT('Ctrl Pts',(-0.148910620450773,-0.106998243882291,
-0.641906039291115));
#85323=CARTESIAN_POINT('Ctrl Pts',(0.00865336193011468,-0.18316144901443,
-0.630821512533036));
#85324=CARTESIAN_POINT('Ctrl Pts',(0.158334982948992,-0.0924825943185493,
-0.619736985774954));
#85325=CARTESIAN_POINT('Ctrl Pts',(0.163789012191789,0.08243880495611,-0.608652459016875));
#85326=CARTESIAN_POINT('Ctrl Pts',(0.0200473656101289,0.182266563608242,
-0.597567932258793));
#85327=CARTESIAN_POINT('Ctrl Pts',(-0.141955458694602,0.11606741499751,
-0.586483405500715));
#85328=CARTESIAN_POINT('Ctrl Pts',(-0.174650826329757,-0.0558577294538408,
-0.575398878742634));
#85329=CARTESIAN_POINT('Ctrl Pts',(-0.0482564740935901,-0.176901977901532,
-0.564314351984555));
#85330=CARTESIAN_POINT('Ctrl Pts',(0.122094778358068,-0.136805928874095,
-0.553229825226472));
#85331=CARTESIAN_POINT('Ctrl Pts',(0.181229699945847,0.0279068617897054,
-0.542145298468395));
#85332=CARTESIAN_POINT('Ctrl Pts',(0.0752821950564939,0.167199246962685,
-0.531060771710313));
#85333=CARTESIAN_POINT('Ctrl Pts',(-0.0992399829364661,0.154189567948618,
-0.519976244952235));
#85334=CARTESIAN_POINT('Ctrl Pts',(-0.183364300139518,0.000728362379997262,
-0.508891718194153));
#85335=CARTESIAN_POINT('Ctrl Pts',(-0.10046178010034,-0.153396309657315,
-0.497807191436073));
#85336=CARTESIAN_POINT('Ctrl Pts',(0.0739515377392648,-0.167792035399211,
-0.486722664677994));
#85337=CARTESIAN_POINT('Ctrl Pts',(0.181002280375352,-0.0293457250095247,
-0.475638137919914));
#85338=CARTESIAN_POINT('Ctrl Pts',(0.12317775338849,0.135831653702577,-0.464553611161834));
#85339=CARTESIAN_POINT('Ctrl Pts',(-0.0468495881671225,0.177279759606062,
-0.453469084403753));
#85340=CARTESIAN_POINT('Ctrl Pts',(-0.174201564170652,0.0572434460694844,
-0.442384557645674));
#85341=CARTESIAN_POINT('Ctrl Pts',(-0.142873053929396,-0.114936014974851,
-0.431300030887593));
#85342=CARTESIAN_POINT('Ctrl Pts',(0.0185987519632387,-0.182420074286859,
-0.420215504129514));
#85343=CARTESIAN_POINT('Ctrl Pts',(0.163128924644238,-0.0837373932113132,
-0.409130977371433));
#85344=CARTESIAN_POINT('Ctrl Pts',(0.159064696314123,0.0912218146273431,
-0.398046450613352));
#85345=CARTESIAN_POINT('Ctrl Pts',(0.0101081791250124,0.183086924143141,
-0.386961923855273));
#85346=CARTESIAN_POINT('Ctrl Pts',(-0.148055894759956,0.108177858659869,
-0.375877397097193));
#85347=CARTESIAN_POINT('Ctrl Pts',(-0.171355614907519,-0.0652705930497431,
-0.364792870339113));
#85348=CARTESIAN_POINT('Ctrl Pts',(-0.0385672285920655,-0.179263956098795,
-0.353708343581032));
#85349=CARTESIAN_POINT('Ctrl Pts',(0.129352108557561,-0.129965491916379,
-0.342623816822953));
#85350=CARTESIAN_POINT('Ctrl Pts',(0.179444401039445,0.0377187488252464,
-0.331539290064872));
#85351=CARTESIAN_POINT('Ctrl Pts',(0.066080498702647,0.17104492032495,-0.320454763306793));
#85352=CARTESIAN_POINT('Ctrl Pts',(-0.107476236663192,0.148565997555451,
-0.309370236548711));
#85353=CARTESIAN_POINT('Ctrl Pts',(-0.183132694411917,-0.009241932405554,
-0.298285709790633));
#85354=CARTESIAN_POINT('Ctrl Pts',(-0.0919732849516963,-0.158631371219217,
-0.287201183032551));
#85355=CARTESIAN_POINT('Ctrl Pts',(0.0829647383674402,-0.163523237679612,
-0.276116656274472));
#85356=CARTESIAN_POINT('Ctrl Pts',(0.182330047462404,-0.0194615227922904,
-0.265032129516391));
#85357=CARTESIAN_POINT('Ctrl Pts',(0.115610621762305,0.142327724733257,
-0.253947602758312));
#85358=CARTESIAN_POINT('Ctrl Pts',(-0.0564187061067814,0.174470417692299,
-0.242863076000231));
#85359=CARTESIAN_POINT('Ctrl Pts',(-0.177056143386771,0.0476877256057966,
-0.231778549242151));
#85360=CARTESIAN_POINT('Ctrl Pts',(-0.136412853689387,-0.12253379336342,
-0.220694022484071));
#85361=CARTESIAN_POINT('Ctrl Pts',(0.0284891249897688,-0.181139080879629,
-0.209609495725991));
#85362=CARTESIAN_POINT('Ctrl Pts',(0.167440313371968,-0.0747444890892225,
-0.198524968967911));
#85363=CARTESIAN_POINT('Ctrl Pts',(0.153869850388125,0.0997349826014979,
-0.187440442209831));
#85364=CARTESIAN_POINT('Ctrl Pts',(0.000139090944378808,0.183365689831066,
-0.176355915451751));
#85365=CARTESIAN_POINT('Ctrl Pts',(-0.153718364479581,0.0999683085654659,
-0.165271388693671));
#85366=CARTESIAN_POINT('Ctrl Pts',(-0.167553517512711,-0.0744903943231421,
-0.15418686193559));
#85367=CARTESIAN_POINT('Ctrl Pts',(-0.0287638928153855,-0.181095623655295,
-0.143102335177511));
#85368=CARTESIAN_POINT('Ctrl Pts',(0.136226793222509,-0.122740657791065,
-0.13201780841943));
#85369=CARTESIAN_POINT('Ctrl Pts',(0.177128301973759,0.0474191638445822,
-0.12093328166135));
#85370=CARTESIAN_POINT('Ctrl Pts',(0.0566832995374016,0.174384426330519,
-0.10984875490327));
#85371=CARTESIAN_POINT('Ctrl Pts',(-0.115394507761123,0.142503330509622,
-0.0987642281451906));
#85372=CARTESIAN_POINT('Ctrl Pts',(-0.18235947006817,-0.0191856073775684,
-0.0876797013871106));
#85373=CARTESIAN_POINT('Ctrl Pts',(-0.0832125183308621,-0.163395815331006,
-0.0765951746290301));
#85374=CARTESIAN_POINT('Ctrl Pts',(0.0917321306689327,-0.158773327666352,
-0.0655106478709507));
#85375=CARTESIAN_POINT('Ctrl Pts',(0.183119205053686,-0.00951478666591987,
-0.05442612111287));
#85376=CARTESIAN_POINT('Ctrl Pts',(0.107700087856717,0.148393320157019,
-0.0433415943547902));
#85377=CARTESIAN_POINT('Ctrl Pts',(-0.065818238191846,0.171162982686544,
-0.03225706759671));
#85378=CARTESIAN_POINT('Ctrl Pts',(-0.179392109761845,0.0379566169796293,
-0.0211725408386302));
#85379=CARTESIAN_POINT('Ctrl Pts',(-0.129539265966577,-0.129703510329422,
-0.0100880140805498));
#85380=CARTESIAN_POINT('Ctrl Pts',(0.0382757593502112,-0.179449160753822,
0.000996512677530166));
#85381=CARTESIAN_POINT('Ctrl Pts',(0.171299276958504,-0.0652716633324161,
0.0120810394356104));
#85382=CARTESIAN_POINT('Ctrl Pts',(0.1558320429858,0.0497893031757065,0.019470723940997));
#85383=CARTESIAN_POINT('Ctrl Pts',(0.125514135451595,0.0914158484392161,
0.0231655661936903));
#85384=CARTESIAN_POINT('Ctrl Pts',(0.0210491062034705,-0.154371551634071,
-1.92554305833426E-15));
#85385=CARTESIAN_POINT('Ctrl Pts',(0.0249906761485533,-0.154347944482943,
-2.08179767172651E-15));
#85386=CARTESIAN_POINT('Ctrl Pts',(0.0289233405816073,-0.154164839339631,
-1.82232685243181E-15));
#85387=CARTESIAN_POINT('Ctrl Pts',(0.0328381830330719,-0.153819660683202,
-1.9671764217577E-15));
#85388=CARTESIAN_POINT('Ctrl Pts',(0.0417954224626671,-0.15302988487231,
-2.40177476828239E-15));
#85389=CARTESIAN_POINT('Ctrl Pts',(0.0506592073437473,-0.151393578924998,
-2.68040904842411E-15));
#85390=CARTESIAN_POINT('Ctrl Pts',(0.0593543406709811,-0.148991873564261,
-2.49106291150269E-15));
#85391=CARTESIAN_POINT('Ctrl Pts',(0.0641334869885079,-0.147671813146716,
-2.21133230102988E-15));
#85392=CARTESIAN_POINT('Ctrl Pts',(0.0688565095039308,-0.14612102978709,
-2.56627996653982E-15));
#85393=CARTESIAN_POINT('Ctrl Pts',(0.0734977242378156,-0.144357781793704,
-2.47024622979097E-15));
#85394=CARTESIAN_POINT('Ctrl Pts',(0.0812645483498012,-0.14140708077777,
-2.30953891825472E-15));
#85395=CARTESIAN_POINT('Ctrl Pts',(0.0888125783363352,-0.137859846860542,
-1.52387926237079E-15));
#85396=CARTESIAN_POINT('Ctrl Pts',(0.0960882881071144,-0.133769590071901,
-2.19615992058664E-15));
#85397=CARTESIAN_POINT('Ctrl Pts',(0.100603799299556,-0.131231061063605,
-2.61339630470243E-15));
#85398=CARTESIAN_POINT('Ctrl Pts',(0.105012894248953,-0.128482986224302,
-2.24724647575841E-15));
#85399=CARTESIAN_POINT('Ctrl Pts',(0.109282262285862,-0.125551551600707,
-2.11289319373975E-15));
#85400=CARTESIAN_POINT('Ctrl Pts',(0.118929558089528,-0.118927522775262,
-1.80930122354136E-15));
#85401=CARTESIAN_POINT('Ctrl Pts',(0.127886007007196,-0.111360115256469,
-1.91826500988144E-15));
#85402=CARTESIAN_POINT('Ctrl Pts',(0.136001978678605,-0.102988394911393,
-1.38604405730547E-15));
#85403=CARTESIAN_POINT('Ctrl Pts',(0.14010066837913,-0.0987605482230019,
-1.11726434428458E-15));
#85404=CARTESIAN_POINT('Ctrl Pts',(0.14398482089894,-0.0943267422381278,
-9.21274069104527E-16));
#85405=CARTESIAN_POINT('Ctrl Pts',(0.147632822555182,-0.0897004696527729,
-5.95010152260045E-16));
#85406=CARTESIAN_POINT('Ctrl Pts',(0.150543464665863,-0.0860092915582159,
-3.34692974514596E-16));
#85407=CARTESIAN_POINT('Ctrl Pts',(0.153301209336262,-0.082197730922776,
-8.41928195914956E-17));
#85408=CARTESIAN_POINT('Ctrl Pts',(0.155883789306881,-0.0782916799561493,
-1.09287578986539E-16));
#85409=CARTESIAN_POINT('Ctrl Pts',(0.159148499358082,-0.0733539339826171,
-1.41010551425541E-16));
#85410=CARTESIAN_POINT('Ctrl Pts',(0.162139340594116,-0.0682579463034665,
3.42436685437861E-16));
#85411=CARTESIAN_POINT('Ctrl Pts',(0.164837347197669,-0.063020026556347,
5.91540705308091E-16));
#85412=CARTESIAN_POINT('Ctrl Pts',(0.168353236127199,-0.0561942671129082,
8.97277816030434E-16));
#85413=CARTESIAN_POINT('Ctrl Pts',(0.171372272563736,-0.0491276521825463,
1.12084903965696E-15));
#85414=CARTESIAN_POINT('Ctrl Pts',(0.173907391890521,-0.0418709293396242,
1.60461921527855E-15));
#85415=CARTESIAN_POINT('Ctrl Pts',(0.175675656440153,-0.0368093112871495,
1.40713357097467E-15));
#85416=CARTESIAN_POINT('Ctrl Pts',(0.177208643735401,-0.0316537207737417,
1.59324788500904E-15));
#85417=CARTESIAN_POINT('Ctrl Pts',(0.178507313524868,-0.0264241089443225,
1.66533453693773E-15));
#85418=CARTESIAN_POINT('Ctrl Pts',(0.179596733069877,-0.0220371266752443,
1.72580611191571E-15));
#85419=CARTESIAN_POINT('Ctrl Pts',(0.180519059980037,-0.0176060950243616,
1.88764134780047E-15));
#85420=CARTESIAN_POINT('Ctrl Pts',(0.181275612730176,-0.0131509784388465,
1.85268467234323E-15));
#85421=CARTESIAN_POINT('Ctrl Pts',(0.183123733832993,-0.00226793693819612,
1.76729185659452E-15));
#85422=CARTESIAN_POINT('Ctrl Pts',(0.183989435438147,0.00877647129111679,
1.46112760885068E-15));
#85423=CARTESIAN_POINT('Ctrl Pts',(0.183904136655522,0.0198423917610982,
1.51875040321769E-15));
#85424=CARTESIAN_POINT('Ctrl Pts',(0.18385525744904,0.0261835539079751,
1.5517702937391E-15));
#85425=CARTESIAN_POINT('Ctrl Pts',(0.183493534385419,0.0325320838244838,
7.45918507883439E-16));
#85426=CARTESIAN_POINT('Ctrl Pts',(0.182820145325716,0.0388632508128488,
7.19042880792387E-16));
#85427=CARTESIAN_POINT('Ctrl Pts',(0.182239131666724,0.0443259093526593,
6.95854047815544E-16));
#85428=CARTESIAN_POINT('Ctrl Pts',(0.181424826261944,0.0497778655432242,
9.96295625820296E-16));
#85429=CARTESIAN_POINT('Ctrl Pts',(0.180384702012361,0.055169520382088,
9.51062145704284E-16));
#85430=CARTESIAN_POINT('Ctrl Pts',(0.177958241768075,0.0677474754895241,
8.45538943782813E-16));
#85431=CARTESIAN_POINT('Ctrl Pts',(0.174303572517529,0.080038108209797,
4.0076412894154E-16));
#85432=CARTESIAN_POINT('Ctrl Pts',(0.169446063228336,0.0918430005340087,
-2.68231617472914E-16));
#85433=CARTESIAN_POINT('Ctrl Pts',(0.166164925312101,0.0998169389242502,
-7.20123148436007E-16));
#85434=CARTESIAN_POINT('Ctrl Pts',(0.162333929398081,0.107569631004673,
-1.26651752900455E-16));
#85435=CARTESIAN_POINT('Ctrl Pts',(0.157947475570094,0.115038058750287,
1.30104260698261E-18));
#85436=CARTESIAN_POINT('Ctrl Pts',(0.089187861459517,0.173858233536057,
-0.9746));
#85437=CARTESIAN_POINT('Ctrl Pts',(0.0882329452274535,0.174454830838509,
-0.9746));
#85438=CARTESIAN_POINT('Ctrl Pts',(0.08727802899539,0.175051428140961,-0.9746));
#85439=CARTESIAN_POINT('Ctrl Pts',(0.0863231127633264,0.175648025443413,
-0.9746));
#85440=CARTESIAN_POINT('Origin',(0.,0.,0.232200846792815));
#85441=CARTESIAN_POINT('',(0.125,-0.0422728431058792,0.201303634366138));
#85442=CARTESIAN_POINT('',(0.125,0.0422728431058792,0.201303634366138));
#85443=CARTESIAN_POINT('Ctrl Pts',(0.125,-0.0422728431058792,0.201303634366138));
#85444=CARTESIAN_POINT('Ctrl Pts',(0.125,2.15105711021124E-16,0.193484871477951));
#85445=CARTESIAN_POINT('Ctrl Pts',(0.125,0.0422728431058792,0.201303634366138));
#85446=CARTESIAN_POINT('Origin',(0.,0.,0.201303634366138));
#85447=CARTESIAN_POINT('Origin',(0.,0.,0.232200846792815));
#85448=CARTESIAN_POINT('',(0.0258906439801145,-0.129389597025995,0.201303634366138));
#85449=CARTESIAN_POINT('',(0.0991093560198853,-0.0871167539201152,0.201303634366137));
#85450=CARTESIAN_POINT('Ctrl Pts',(0.0258906439801145,-0.129389597025995,
0.201303634366138));
#85451=CARTESIAN_POINT('Ctrl Pts',(0.0625000000000001,-0.108253175473055,
0.19348487147795));
#85452=CARTESIAN_POINT('Ctrl Pts',(0.0991093560198853,-0.0871167539201152,
0.201303634366138));
#85453=CARTESIAN_POINT('Origin',(0.,0.,0.201303634366138));
#85454=CARTESIAN_POINT('Origin',(0.,0.,0.232200846792815));
#85455=CARTESIAN_POINT('',(0.0991093560198853,0.0871167539201153,0.201303634366138));
#85456=CARTESIAN_POINT('',(0.0258906439801146,0.129389597025995,0.201303634366138));
#85457=CARTESIAN_POINT('Ctrl Pts',(0.0991093560198853,0.0871167539201153,
0.201303634366138));
#85458=CARTESIAN_POINT('Ctrl Pts',(0.0624999999999998,0.108253175473055,
0.193484871477951));
#85459=CARTESIAN_POINT('Ctrl Pts',(0.0258906439801146,0.129389597025995,
0.201303634366138));
#85460=CARTESIAN_POINT('Origin',(0.,0.,0.201303634366138));
#85461=CARTESIAN_POINT('Origin',(0.,0.,0.232200846792815));
#85462=CARTESIAN_POINT('',(-0.0258906439801146,0.129389597025995,0.201303634366138));
#85463=CARTESIAN_POINT('',(-0.0991093560198852,0.0871167539201153,0.201303634366138));
#85464=CARTESIAN_POINT('Ctrl Pts',(-0.0258906439801146,0.129389597025995,
0.201303634366138));
#85465=CARTESIAN_POINT('Ctrl Pts',(-0.0625000000000002,0.108253175473055,
0.19348487147795));
#85466=CARTESIAN_POINT('Ctrl Pts',(-0.0991093560198852,0.0871167539201153,
0.201303634366137));
#85467=CARTESIAN_POINT('Origin',(0.,0.,0.201303634366138));
#85468=CARTESIAN_POINT('Origin',(0.,0.,0.232200846792815));
#85469=CARTESIAN_POINT('',(-0.125,0.0422728431058793,0.201303634366137));
#85470=CARTESIAN_POINT('',(-0.125,-0.0422728431058794,0.201303634366138));
#85471=CARTESIAN_POINT('Ctrl Pts',(-0.125,0.0422728431058793,0.201303634366137));
#85472=CARTESIAN_POINT('Ctrl Pts',(-0.125,-2.98372437868011E-16,0.19348487147795));
#85473=CARTESIAN_POINT('Ctrl Pts',(-0.125,-0.0422728431058794,0.201303634366137));
#85474=CARTESIAN_POINT('',(-0.131954512102672,-1.61597670879588E-17,0.201303634366138));
#85475=CARTESIAN_POINT('Origin',(0.,0.,0.201303634366138));
#85476=CARTESIAN_POINT('Origin',(0.,0.,0.201303634366138));
#85477=CARTESIAN_POINT('Origin',(0.,0.,0.232200846792815));
#85478=CARTESIAN_POINT('',(-0.0991093560198854,-0.0871167539201152,0.201303634366138));
#85479=CARTESIAN_POINT('',(-0.0258906439801146,-0.129389597025995,0.201303634366138));
#85480=CARTESIAN_POINT('Ctrl Pts',(-0.0991093560198854,-0.0871167539201152,
0.201303634366138));
#85481=CARTESIAN_POINT('Ctrl Pts',(-0.0624999999999998,-0.108253175473055,
0.19348487147795));
#85482=CARTESIAN_POINT('Ctrl Pts',(-0.0258906439801146,-0.129389597025995,
0.201303634366138));
#85483=CARTESIAN_POINT('Origin',(0.,0.,0.201303634366138));
#85484=CARTESIAN_POINT('Origin',(5.55111512312578E-17,0.,-0.255));
#85485=CARTESIAN_POINT('',(-0.38,-4.65365783675994E-17,0.03));
#85486=CARTESIAN_POINT('Origin',(5.55111512312578E-17,0.,-0.255));
#85487=CARTESIAN_POINT('Origin',(0.,0.,0.03));
#85488=CARTESIAN_POINT('',(-0.125,0.0721687836487032,0.197539132746182));
#85489=CARTESIAN_POINT('Origin',(-0.125,-2.40370335797946E-17,-0.255));
#85490=CARTESIAN_POINT('Origin',(-0.0625,0.108253175473055,-0.255));
#85491=CARTESIAN_POINT('',(8.83812698937422E-18,0.144337567297406,0.197539132746182));
#85492=CARTESIAN_POINT('Origin',(-0.0625,0.108253175473055,-0.255));
#85493=CARTESIAN_POINT('Origin',(0.0625000000000001,0.108253175473055,-0.255));
#85494=CARTESIAN_POINT('',(0.125,0.0721687836487032,0.197539132746182));
#85495=CARTESIAN_POINT('Origin',(0.0625000000000001,0.108253175473055,-0.255));
#85496=CARTESIAN_POINT('Origin',(0.125,-4.80740671595891E-17,-0.255));
#85497=CARTESIAN_POINT('',(0.125,-0.0721687836487033,0.197539132746182));
#85498=CARTESIAN_POINT('Origin',(0.125,-4.80740671595891E-17,-0.255));
#85499=CARTESIAN_POINT('Origin',(0.0625,-0.108253175473055,-0.255));
#85500=CARTESIAN_POINT('',(-2.65143809681227E-17,-0.144337567297406,0.197539132746182));
#85501=CARTESIAN_POINT('Origin',(0.0625,-0.108253175473055,-0.255));
#85502=CARTESIAN_POINT('Origin',(-0.0625,-0.108253175473055,-0.255));
#85503=CARTESIAN_POINT('',(-0.125,-0.0721687836487032,0.197539132746182));
#85504=CARTESIAN_POINT('Origin',(-0.0625,-0.108253175473055,-0.255));
#85505=CARTESIAN_POINT('Origin',(-0.125,-2.40370335797946E-17,-0.255));
#85506=CARTESIAN_POINT('Origin',(0.,0.,0.033697287084562));
#85507=CARTESIAN_POINT('',(0.,0.,-0.00360542583087612));
#85508=CARTESIAN_POINT('',(-0.120858028271594,1.48008397474068E-17,0.07));
#85509=CARTESIAN_POINT('',(-0.06125,-7.50096164477754E-18,0.033697287084562));
#85510=CARTESIAN_POINT('Origin',(0.,0.,0.07));
#85511=CARTESIAN_POINT('Origin',(-2.77555756156289E-17,-0.144337567297406,
0.22));
#85512=CARTESIAN_POINT('',(-2.77555756156289E-17,-0.144337567297406,0.07));
#85513=CARTESIAN_POINT('',(-2.65143809681227E-17,-0.144337567297406,0.22));
#85514=CARTESIAN_POINT('',(-0.125,-0.0721687836487032,0.07));
#85515=CARTESIAN_POINT('',(-0.125,-0.0721687836487032,0.07));
#85516=CARTESIAN_POINT('',(-0.125,-0.0721687836487032,0.22));
#85517=CARTESIAN_POINT('Origin',(-0.125,-0.0721687836487032,0.22));
#85518=CARTESIAN_POINT('',(-0.125,0.0721687836487032,0.07));
#85519=CARTESIAN_POINT('',(-0.125,0.0721687836487032,0.07));
#85520=CARTESIAN_POINT('',(-0.125,0.0721687836487032,0.22));
#85521=CARTESIAN_POINT('Origin',(-0.125,0.0721687836487032,0.22));
#85522=CARTESIAN_POINT('',(1.38777878078145E-17,0.144337567297406,0.07));
#85523=CARTESIAN_POINT('',(8.83812698937423E-18,0.144337567297406,0.07));
#85524=CARTESIAN_POINT('',(8.83812698937423E-18,0.144337567297406,0.22));
#85525=CARTESIAN_POINT('Origin',(0.,0.144337567297406,0.22));
#85526=CARTESIAN_POINT('',(0.125,0.0721687836487032,0.07));
#85527=CARTESIAN_POINT('',(0.125,0.0721687836487032,0.07));
#85528=CARTESIAN_POINT('',(0.125,0.0721687836487032,0.22));
#85529=CARTESIAN_POINT('Origin',(0.125,-0.0721687836487033,0.22));
#85530=CARTESIAN_POINT('',(0.125,-0.0721687836487033,0.07));
#85531=CARTESIAN_POINT('',(0.125,-0.0721687836487033,0.22));
#85532=CARTESIAN_POINT('',(-2.65143809681227E-17,-0.144337567297406,0.07));
#85533=CARTESIAN_POINT('Origin',(0.125,0.0721687836487032,0.22));
#85534=CARTESIAN_POINT('',(0.125,-0.0721687836487033,0.07));
#85535=CARTESIAN_POINT('Origin',(0.,0.,0.07));
#85536=CARTESIAN_POINT('Origin',(0.17,0.,-1.));
#85537=CARTESIAN_POINT('',(-0.17,-2.0818995585505E-17,-1.));
#85538=CARTESIAN_POINT('Origin',(0.,0.,-1.));
#85539=CARTESIAN_POINT('Origin',(0.,0.,-0.985));
#85540=CARTESIAN_POINT('',(-0.185,-2.2655965784226E-17,-0.985));
#85541=CARTESIAN_POINT('Origin',(0.38,0.,0.));
#85542=CARTESIAN_POINT('',(-0.38,-4.65365783675994E-17,0.));
#85543=CARTESIAN_POINT('Origin',(0.,0.,0.));
#85544=CARTESIAN_POINT('Origin',(0.,0.,0.015));
#85545=CARTESIAN_POINT('',(-0.38,-4.65365783675994E-17,0.015));
#85546=CARTESIAN_POINT('',(0.,0.,0.));
#85547=CARTESIAN_POINT('Origin',(0.,0.21,-1.085));
#85548=CARTESIAN_POINT('',(0.,0.21,-0.265461026520961));
#85549=CARTESIAN_POINT('',(0.07,0.21,-0.265461026520961));
#85550=CARTESIAN_POINT('',(0.,0.21,-0.265461026520961));
#85551=CARTESIAN_POINT('',(0.,0.21,-0.500206207478476));
#85552=CARTESIAN_POINT('',(0.,0.21,-0.5425));
#85553=CARTESIAN_POINT('',(0.07,0.21,-0.500206207478476));
#85554=CARTESIAN_POINT('',(0.,0.21,-0.500206207478476));
#85555=CARTESIAN_POINT('',(0.07,0.21,-0.5425));
#85556=CARTESIAN_POINT('Origin',(0.,0.21,-1.085));
#85557=CARTESIAN_POINT('',(0.07,0.21,-0.167559714847562));
#85558=CARTESIAN_POINT('',(0.,0.21,-0.167559714847562));
#85559=CARTESIAN_POINT('',(0.,0.21,-0.167559714847562));
#85560=CARTESIAN_POINT('',(0.07,0.21,-0.141680910152439));
#85561=CARTESIAN_POINT('',(0.07,0.21,-0.5425));
#85562=CARTESIAN_POINT('',(0.,0.21,-0.141680910152439));
#85563=CARTESIAN_POINT('',(0.,0.21,-0.141680910152439));
#85564=CARTESIAN_POINT('',(0.,0.21,-0.5425));
#85565=CARTESIAN_POINT('Origin',(0.,-0.21,-0.075));
#85566=CARTESIAN_POINT('',(0.07,-0.21,-0.265461026520961));
#85567=CARTESIAN_POINT('',(0.,-0.21,-0.265461026520961));
#85568=CARTESIAN_POINT('',(0.,-0.21,-0.265461026520961));
#85569=CARTESIAN_POINT('',(0.07,-0.21,-0.500206207478476));
#85570=CARTESIAN_POINT('',(0.07,-0.21,-0.0375));
#85571=CARTESIAN_POINT('',(0.,-0.21,-0.500206207478476));
#85572=CARTESIAN_POINT('',(0.,-0.21,-0.500206207478476));
#85573=CARTESIAN_POINT('',(0.,-0.21,-0.0375));
#85574=CARTESIAN_POINT('Origin',(0.,-0.21,-0.075));
#85575=CARTESIAN_POINT('',(0.07,-0.21,-0.141680910152439));
#85576=CARTESIAN_POINT('',(0.,-0.21,-0.141680910152439));
#85577=CARTESIAN_POINT('',(0.,-0.21,-0.141680910152439));
#85578=CARTESIAN_POINT('',(0.07,-0.21,-0.167559714847561));
#85579=CARTESIAN_POINT('',(0.07,-0.21,-0.0375));
#85580=CARTESIAN_POINT('',(0.,-0.21,-0.167559714847561));
#85581=CARTESIAN_POINT('',(0.,-0.21,-0.167559714847561));
#85582=CARTESIAN_POINT('',(0.,-0.21,-0.0375));
#85583=CARTESIAN_POINT('Origin',(0.,0.267810237132177,-0.1546203125));
#85584=CARTESIAN_POINT('',(0.07,0.31628195418898,-0.120562357541491));
#85585=CARTESIAN_POINT('Origin',(0.07,0.267810237132177,-0.1546203125));
#85586=CARTESIAN_POINT('',(0.,0.31628195418898,-0.120562357541491));
#85587=CARTESIAN_POINT('',(0.,0.31628195418898,-0.120562357541491));
#85588=CARTESIAN_POINT('Origin',(0.,0.267810237132177,-0.1546203125));
#85589=CARTESIAN_POINT('Origin',(0.,0.267810237132177,-0.1546203125));
#85590=CARTESIAN_POINT('',(0.,0.262551041465563,-0.213627028315498));
#85591=CARTESIAN_POINT('Origin',(0.,0.267810237132177,-0.1546203125));
#85592=CARTESIAN_POINT('',(0.07,0.262551041465563,-0.213627028315498));
#85593=CARTESIAN_POINT('',(0.,0.262551041465563,-0.213627028315498));
#85594=CARTESIAN_POINT('Origin',(0.07,0.267810237132177,-0.1546203125));
#85595=CARTESIAN_POINT('Origin',(0.,-0.267810237132177,-0.1546203125));
#85596=CARTESIAN_POINT('',(0.07,-0.262551041465564,-0.213627028315498));
#85597=CARTESIAN_POINT('Origin',(0.07,-0.267810237132177,-0.1546203125));
#85598=CARTESIAN_POINT('',(0.,-0.262551041465564,-0.213627028315498));
#85599=CARTESIAN_POINT('',(0.,-0.262551041465564,-0.213627028315498));
#85600=CARTESIAN_POINT('Origin',(0.,-0.267810237132177,-0.1546203125));
#85601=CARTESIAN_POINT('Origin',(0.,-0.267810237132177,-0.1546203125));
#85602=CARTESIAN_POINT('',(0.,-0.31628195418898,-0.120562357541491));
#85603=CARTESIAN_POINT('Origin',(0.,-0.267810237132177,-0.1546203125));
#85604=CARTESIAN_POINT('',(0.07,-0.31628195418898,-0.120562357541491));
#85605=CARTESIAN_POINT('',(0.,-0.31628195418898,-0.120562357541491));
#85606=CARTESIAN_POINT('Origin',(0.07,-0.267810237132177,-0.1546203125));
#85607=CARTESIAN_POINT('Origin',(0.,0.,0.));
#85608=CARTESIAN_POINT('Origin',(0.,0.,0.));
#85609=CARTESIAN_POINT('Origin',(0.07,0.,0.));
#85610=CARTESIAN_POINT('Origin',(0.,0.,0.));
#85611=CARTESIAN_POINT('',(0.,0.0537309127234168,0.334189385856988));
#85612=CARTESIAN_POINT('Origin',(0.,0.,0.));
#85613=CARTESIAN_POINT('',(0.,-0.0537309127234167,0.334189385856988));
#85614=CARTESIAN_POINT('Origin',(0.,1.89355270786289E-17,0.309240625));
#85615=CARTESIAN_POINT('Origin',(0.,0.,0.));
#85616=CARTESIAN_POINT('Origin',(0.,0.,0.));
#85617=CARTESIAN_POINT('Origin',(0.,0.,0.));
#85618=CARTESIAN_POINT('Origin',(0.,0.,0.));
#85619=CARTESIAN_POINT('Origin',(0.07,0.,0.));
#85620=CARTESIAN_POINT('Origin',(0.,0.,0.));
#85621=CARTESIAN_POINT('',(0.07,0.0537309127234168,0.334189385856988));
#85622=CARTESIAN_POINT('Origin',(0.07,0.,0.));
#85623=CARTESIAN_POINT('',(0.,0.0537309127234168,0.334189385856988));
#85624=CARTESIAN_POINT('Origin',(0.,1.89355270786289E-17,0.309240625));
#85625=CARTESIAN_POINT('',(0.07,-0.0537309127234167,0.334189385856988));
#85626=CARTESIAN_POINT('Origin',(0.07,1.89355270786289E-17,0.309240625));
#85627=CARTESIAN_POINT('',(0.,-0.0537309127234167,0.334189385856988));
#85628=CARTESIAN_POINT('Origin',(0.,0.,0.));
#85629=CARTESIAN_POINT('Origin',(0.07,0.,0.));
#85630=CARTESIAN_POINT('Origin',(0.,0.,0.));
#85631=CARTESIAN_POINT('Origin',(0.07,0.,0.));
#85632=CARTESIAN_POINT('Origin',(0.07,0.,0.));
#85633=CARTESIAN_POINT('',(0.,0.,0.));
#85634=CARTESIAN_POINT('Origin',(0.,0.1344,-0.69));
#85635=CARTESIAN_POINT('',(0.,0.1344,-0.169045678460734));
#85636=CARTESIAN_POINT('',(0.06,0.1344,-0.169045678460734));
#85637=CARTESIAN_POINT('',(0.,0.1344,-0.169045678460734));
#85638=CARTESIAN_POINT('',(0.,0.1344,-0.31774461443115));
#85639=CARTESIAN_POINT('',(0.,0.1344,-0.345));
#85640=CARTESIAN_POINT('',(0.06,0.1344,-0.31774461443115));
#85641=CARTESIAN_POINT('',(0.,0.1344,-0.31774461443115));
#85642=CARTESIAN_POINT('',(0.06,0.1344,-0.345));
#85643=CARTESIAN_POINT('Origin',(0.,0.1344,-0.69));
#85644=CARTESIAN_POINT('',(0.06,0.1344,-0.11308850359562));
#85645=CARTESIAN_POINT('',(0.,0.1344,-0.11308850359562));
#85646=CARTESIAN_POINT('',(0.,0.1344,-0.11308850359562));
#85647=CARTESIAN_POINT('',(0.06,0.1344,-0.0898927464043797));
#85648=CARTESIAN_POINT('',(0.06,0.1344,-0.345));
#85649=CARTESIAN_POINT('',(0.,0.1344,-0.0898927464043797));
#85650=CARTESIAN_POINT('',(0.,0.1344,-0.0898927464043797));
#85651=CARTESIAN_POINT('',(0.,0.1344,-0.345));
#85652=CARTESIAN_POINT('Origin',(0.,-0.1344,-0.048));
#85653=CARTESIAN_POINT('',(0.06,-0.1344,-0.169045678460734));
#85654=CARTESIAN_POINT('',(0.,-0.1344,-0.169045678460734));
#85655=CARTESIAN_POINT('',(0.,-0.1344,-0.169045678460734));
#85656=CARTESIAN_POINT('',(0.06,-0.1344,-0.31774461443115));
#85657=CARTESIAN_POINT('',(0.06,-0.1344,-0.024));
#85658=CARTESIAN_POINT('',(0.,-0.1344,-0.31774461443115));
#85659=CARTESIAN_POINT('',(0.,-0.1344,-0.31774461443115));
#85660=CARTESIAN_POINT('',(0.,-0.1344,-0.024));
#85661=CARTESIAN_POINT('Origin',(0.,-0.1344,-0.048));
#85662=CARTESIAN_POINT('',(0.06,-0.1344,-0.0898927464043798));
#85663=CARTESIAN_POINT('',(0.,-0.1344,-0.0898927464043798));
#85664=CARTESIAN_POINT('',(0.,-0.1344,-0.0898927464043798));
#85665=CARTESIAN_POINT('',(0.06,-0.1344,-0.11308850359562));
#85666=CARTESIAN_POINT('',(0.06,-0.1344,-0.024));
#85667=CARTESIAN_POINT('',(0.,-0.1344,-0.11308850359562));
#85668=CARTESIAN_POINT('',(0.,-0.1344,-0.11308850359562));
#85669=CARTESIAN_POINT('',(0.,-0.1344,-0.024));
#85670=CARTESIAN_POINT('Origin',(0.,0.17578691899192,-0.101490625));
#85671=CARTESIAN_POINT('',(0.06,0.204478107495771,-0.0694874446299335));
#85672=CARTESIAN_POINT('Origin',(0.06,0.17578691899192,-0.101490625));
#85673=CARTESIAN_POINT('',(0.,0.204478107495771,-0.0694874446299335));
#85674=CARTESIAN_POINT('',(0.,0.204478107495771,-0.0694874446299335));
#85675=CARTESIAN_POINT('Origin',(0.,0.17578691899192,-0.101490625));
#85676=CARTESIAN_POINT('Origin',(0.,0.17578691899192,-0.101490625));
#85677=CARTESIAN_POINT('',(0.,0.162416946041472,-0.142339513294136));
#85678=CARTESIAN_POINT('Origin',(0.,0.17578691899192,-0.101490625));
#85679=CARTESIAN_POINT('',(0.06,0.162416946041472,-0.142339513294136));
#85680=CARTESIAN_POINT('',(0.,0.162416946041472,-0.142339513294136));
#85681=CARTESIAN_POINT('Origin',(0.06,0.17578691899192,-0.101490625));
#85682=CARTESIAN_POINT('Origin',(0.,-0.17578691899192,-0.101490625));
#85683=CARTESIAN_POINT('',(0.06,-0.162416946041472,-0.142339513294136));
#85684=CARTESIAN_POINT('Origin',(0.06,-0.17578691899192,-0.101490625));
#85685=CARTESIAN_POINT('',(0.,-0.162416946041472,-0.142339513294136));
#85686=CARTESIAN_POINT('',(0.,-0.162416946041472,-0.142339513294136));
#85687=CARTESIAN_POINT('Origin',(0.,-0.17578691899192,-0.101490625));
#85688=CARTESIAN_POINT('Origin',(0.,-0.17578691899192,-0.101490625));
#85689=CARTESIAN_POINT('',(0.,-0.204478107495771,-0.0694874446299334));
#85690=CARTESIAN_POINT('Origin',(0.,-0.17578691899192,-0.101490625));
#85691=CARTESIAN_POINT('',(0.06,-0.204478107495771,-0.0694874446299334));
#85692=CARTESIAN_POINT('',(0.,-0.204478107495771,-0.0694874446299334));
#85693=CARTESIAN_POINT('Origin',(0.06,-0.17578691899192,-0.101490625));
#85694=CARTESIAN_POINT('Origin',(0.,0.,0.));
#85695=CARTESIAN_POINT('Origin',(0.,0.,0.));
#85696=CARTESIAN_POINT('Origin',(0.06,0.,0.));
#85697=CARTESIAN_POINT('Origin',(0.,0.,0.));
#85698=CARTESIAN_POINT('',(0.,0.0420611614542984,0.211826957924069));
#85699=CARTESIAN_POINT('Origin',(0.,0.,0.));
#85700=CARTESIAN_POINT('',(0.,-0.0420611614542984,0.211826957924069));
#85701=CARTESIAN_POINT('Origin',(0.,1.24290169049714E-17,0.20298125));
#85702=CARTESIAN_POINT('Origin',(0.,0.,0.));
#85703=CARTESIAN_POINT('Origin',(0.,0.,0.));
#85704=CARTESIAN_POINT('Origin',(0.,0.,0.));
#85705=CARTESIAN_POINT('Origin',(0.,0.,0.));
#85706=CARTESIAN_POINT('Origin',(0.06,0.,0.));
#85707=CARTESIAN_POINT('Origin',(0.,0.,0.));
#85708=CARTESIAN_POINT('',(0.06,0.0420611614542984,0.211826957924069));
#85709=CARTESIAN_POINT('Origin',(0.06,0.,0.));
#85710=CARTESIAN_POINT('',(0.,0.0420611614542984,0.211826957924069));
#85711=CARTESIAN_POINT('Origin',(0.,1.24290169049714E-17,0.20298125));
#85712=CARTESIAN_POINT('',(0.06,-0.0420611614542984,0.211826957924069));
#85713=CARTESIAN_POINT('Origin',(0.06,1.24290169049714E-17,0.20298125));
#85714=CARTESIAN_POINT('',(0.,-0.0420611614542984,0.211826957924069));
#85715=CARTESIAN_POINT('Origin',(0.,0.,0.));
#85716=CARTESIAN_POINT('Origin',(0.06,0.,0.));
#85717=CARTESIAN_POINT('Origin',(0.,0.,0.));
#85718=CARTESIAN_POINT('Origin',(0.06,0.,0.));
#85719=CARTESIAN_POINT('Origin',(0.06,0.,0.));
#85720=CARTESIAN_POINT('',(0.,0.,0.));
#85721=CARTESIAN_POINT('',(0.,0.,0.));
#85722=CARTESIAN_POINT('',(0.,0.,0.));
#85723=CARTESIAN_POINT('',(0.,0.,0.));
#85724=CARTESIAN_POINT('',(0.,0.,0.));
#85725=CARTESIAN_POINT('',(0.,0.,0.));
#85726=CARTESIAN_POINT('',(0.,0.,0.));
#85727=CARTESIAN_POINT('',(0.,2.1,7.4));
#85728=CARTESIAN_POINT('',(1.65,2.1,7.4));
#85729=CARTESIAN_POINT('',(0.,2.1,8.8));
#85730=CARTESIAN_POINT('',(1.75,2.1,8.8));
#85731=CARTESIAN_POINT('',(0.,2.1,12.72));
#85732=CARTESIAN_POINT('',(0.,0.,0.));
#85733=CARTESIAN_POINT('',(0.,0.,0.));
#85734=CARTESIAN_POINT('',(3.,0.,10.7));
#85735=CARTESIAN_POINT('',(3.55,3.85,2.5));
#85736=CARTESIAN_POINT('',(2.6,2.1,7.4));
#85737=CARTESIAN_POINT('',(2.6,2.1,8.8));
#85738=CARTESIAN_POINT('',(-1.65,2.1,7.4));
#85739=CARTESIAN_POINT('',(-1.75,2.1,8.8));
#85740=CARTESIAN_POINT('',(0.,2.1,7.4));
#85741=CARTESIAN_POINT('',(0.,2.1,8.8));
#85742=CARTESIAN_POINT('',(-3.,0.,10.7));
#85743=CARTESIAN_POINT('',(5.,-0.4,12.1));
#85744=CARTESIAN_POINT('',(-5.,-0.4,12.1));
#85745=CARTESIAN_POINT('',(-3.55,3.85,2.5));
#85746=CARTESIAN_POINT('',(3.55,3.85,10.));
#85747=CARTESIAN_POINT('',(-3.55,3.85,10.));
#85748=CARTESIAN_POINT('',(-2.67,2.1,7.4));
#85749=CARTESIAN_POINT('',(-2.66,2.1,8.8));
#85750=UNCERTAINTY_MEASURE_WITH_UNIT(LENGTH_MEASURE(0.001),#85790,
'DISTANCE_ACCURACY_VALUE',
'Maximum model space distance between geometric entities at asserted c
onnectivities');
#85751=UNCERTAINTY_MEASURE_WITH_UNIT(LENGTH_MEASURE(0.001),#85790,
'DISTANCE_ACCURACY_VALUE',
'Maximum model space distance between geometric entities at asserted c
onnectivities');
#85752=UNCERTAINTY_MEASURE_WITH_UNIT(LENGTH_MEASURE(0.001),#85790,
'DISTANCE_ACCURACY_VALUE',
'Maximum model space distance between geometric entities at asserted c
onnectivities');
#85753=UNCERTAINTY_MEASURE_WITH_UNIT(LENGTH_MEASURE(0.001),#85790,
'DISTANCE_ACCURACY_VALUE',
'Maximum model space distance between geometric entities at asserted c
onnectivities');
#85754=UNCERTAINTY_MEASURE_WITH_UNIT(LENGTH_MEASURE(0.001),#85790,
'DISTANCE_ACCURACY_VALUE',
'Maximum model space distance between geometric entities at asserted c
onnectivities');
#85755=UNCERTAINTY_MEASURE_WITH_UNIT(LENGTH_MEASURE(0.001),#85790,
'DISTANCE_ACCURACY_VALUE',
'Maximum model space distance between geometric entities at asserted c
onnectivities');
#85756=UNCERTAINTY_MEASURE_WITH_UNIT(LENGTH_MEASURE(0.001),#85790,
'DISTANCE_ACCURACY_VALUE',
'Maximum model space distance between geometric entities at asserted c
onnectivities');
#85757=UNCERTAINTY_MEASURE_WITH_UNIT(LENGTH_MEASURE(0.001),#85790,
'DISTANCE_ACCURACY_VALUE',
'Maximum model space distance between geometric entities at asserted c
onnectivities');
#85758=UNCERTAINTY_MEASURE_WITH_UNIT(LENGTH_MEASURE(0.001),#85790,
'DISTANCE_ACCURACY_VALUE',
'Maximum model space distance between geometric entities at asserted c
onnectivities');
#85759=UNCERTAINTY_MEASURE_WITH_UNIT(LENGTH_MEASURE(0.001),#85790,
'DISTANCE_ACCURACY_VALUE',
'Maximum model space distance between geometric entities at asserted c
onnectivities');
#85760=UNCERTAINTY_MEASURE_WITH_UNIT(LENGTH_MEASURE(0.001),#85790,
'DISTANCE_ACCURACY_VALUE',
'Maximum model space distance between geometric entities at asserted c
onnectivities');
#85761=UNCERTAINTY_MEASURE_WITH_UNIT(LENGTH_MEASURE(0.001),#85790,
'DISTANCE_ACCURACY_VALUE',
'Maximum model space distance between geometric entities at asserted c
onnectivities');
#85762=UNCERTAINTY_MEASURE_WITH_UNIT(LENGTH_MEASURE(0.001),#85790,
'DISTANCE_ACCURACY_VALUE',
'Maximum model space distance between geometric entities at asserted c
onnectivities');
#85763=UNCERTAINTY_MEASURE_WITH_UNIT(LENGTH_MEASURE(0.001),#85790,
'DISTANCE_ACCURACY_VALUE',
'Maximum model space distance between geometric entities at asserted c
onnectivities');
#85764=UNCERTAINTY_MEASURE_WITH_UNIT(LENGTH_MEASURE(0.001),#85790,
'DISTANCE_ACCURACY_VALUE',
'Maximum model space distance between geometric entities at asserted c
onnectivities');
#85765=UNCERTAINTY_MEASURE_WITH_UNIT(LENGTH_MEASURE(0.001),#85790,
'DISTANCE_ACCURACY_VALUE',
'Maximum model space distance between geometric entities at asserted c
onnectivities');
#85766=UNCERTAINTY_MEASURE_WITH_UNIT(LENGTH_MEASURE(0.001),#85790,
'DISTANCE_ACCURACY_VALUE',
'Maximum model space distance between geometric entities at asserted c
onnectivities');
#85767=UNCERTAINTY_MEASURE_WITH_UNIT(LENGTH_MEASURE(0.001),#85790,
'DISTANCE_ACCURACY_VALUE',
'Maximum model space distance between geometric entities at asserted c
onnectivities');
#85768=UNCERTAINTY_MEASURE_WITH_UNIT(LENGTH_MEASURE(0.001),#85790,
'DISTANCE_ACCURACY_VALUE',
'Maximum model space distance between geometric entities at asserted c
onnectivities');
#85769=UNCERTAINTY_MEASURE_WITH_UNIT(LENGTH_MEASURE(0.001),#85790,
'DISTANCE_ACCURACY_VALUE',
'Maximum model space distance between geometric entities at asserted c
onnectivities');
#85770=(
GEOMETRIC_REPRESENTATION_CONTEXT(3)
GLOBAL_UNCERTAINTY_ASSIGNED_CONTEXT((#85750))
GLOBAL_UNIT_ASSIGNED_CONTEXT((#85790,#85792,#85793))
REPRESENTATION_CONTEXT('','3D')
);
#85771=(
GEOMETRIC_REPRESENTATION_CONTEXT(3)
GLOBAL_UNCERTAINTY_ASSIGNED_CONTEXT((#85751))
GLOBAL_UNIT_ASSIGNED_CONTEXT((#85790,#85792,#85793))
REPRESENTATION_CONTEXT('','3D')
);
#85772=(
GEOMETRIC_REPRESENTATION_CONTEXT(3)
GLOBAL_UNCERTAINTY_ASSIGNED_CONTEXT((#85752))
GLOBAL_UNIT_ASSIGNED_CONTEXT((#85790,#85792,#85793))
REPRESENTATION_CONTEXT('','3D')
);
#85773=(
GEOMETRIC_REPRESENTATION_CONTEXT(3)
GLOBAL_UNCERTAINTY_ASSIGNED_CONTEXT((#85753))
GLOBAL_UNIT_ASSIGNED_CONTEXT((#85790,#85792,#85793))
REPRESENTATION_CONTEXT('','3D')
);
#85774=(
GEOMETRIC_REPRESENTATION_CONTEXT(3)
GLOBAL_UNCERTAINTY_ASSIGNED_CONTEXT((#85754))
GLOBAL_UNIT_ASSIGNED_CONTEXT((#85790,#85792,#85793))
REPRESENTATION_CONTEXT('','3D')
);
#85775=(
GEOMETRIC_REPRESENTATION_CONTEXT(3)
GLOBAL_UNCERTAINTY_ASSIGNED_CONTEXT((#85755))
GLOBAL_UNIT_ASSIGNED_CONTEXT((#85790,#85792,#85793))
REPRESENTATION_CONTEXT('','3D')
);
#85776=(
GEOMETRIC_REPRESENTATION_CONTEXT(3)
GLOBAL_UNCERTAINTY_ASSIGNED_CONTEXT((#85756))
GLOBAL_UNIT_ASSIGNED_CONTEXT((#85790,#85792,#85793))
REPRESENTATION_CONTEXT('','3D')
);
#85777=(
GEOMETRIC_REPRESENTATION_CONTEXT(3)
GLOBAL_UNCERTAINTY_ASSIGNED_CONTEXT((#85757))
GLOBAL_UNIT_ASSIGNED_CONTEXT((#85790,#85792,#85793))
REPRESENTATION_CONTEXT('','3D')
);
#85778=(
GEOMETRIC_REPRESENTATION_CONTEXT(3)
GLOBAL_UNCERTAINTY_ASSIGNED_CONTEXT((#85758))
GLOBAL_UNIT_ASSIGNED_CONTEXT((#85790,#85792,#85793))
REPRESENTATION_CONTEXT('','3D')
);
#85779=(
GEOMETRIC_REPRESENTATION_CONTEXT(3)
GLOBAL_UNCERTAINTY_ASSIGNED_CONTEXT((#85759))
GLOBAL_UNIT_ASSIGNED_CONTEXT((#85790,#85792,#85793))
REPRESENTATION_CONTEXT('','3D')
);
#85780=(
GEOMETRIC_REPRESENTATION_CONTEXT(3)
GLOBAL_UNCERTAINTY_ASSIGNED_CONTEXT((#85760))
GLOBAL_UNIT_ASSIGNED_CONTEXT((#85790,#85792,#85793))
REPRESENTATION_CONTEXT('','3D')
);
#85781=(
GEOMETRIC_REPRESENTATION_CONTEXT(3)
GLOBAL_UNCERTAINTY_ASSIGNED_CONTEXT((#85761))
GLOBAL_UNIT_ASSIGNED_CONTEXT((#85790,#85792,#85793))
REPRESENTATION_CONTEXT('','3D')
);
#85782=(
GEOMETRIC_REPRESENTATION_CONTEXT(3)
GLOBAL_UNCERTAINTY_ASSIGNED_CONTEXT((#85762))
GLOBAL_UNIT_ASSIGNED_CONTEXT((#85790,#85792,#85793))
REPRESENTATION_CONTEXT('','3D')
);
#85783=(
GEOMETRIC_REPRESENTATION_CONTEXT(3)
GLOBAL_UNCERTAINTY_ASSIGNED_CONTEXT((#85763))
GLOBAL_UNIT_ASSIGNED_CONTEXT((#85790,#85792,#85793))
REPRESENTATION_CONTEXT('','3D')
);
#85784=(
GEOMETRIC_REPRESENTATION_CONTEXT(3)
GLOBAL_UNCERTAINTY_ASSIGNED_CONTEXT((#85764))
GLOBAL_UNIT_ASSIGNED_CONTEXT((#85790,#85792,#85793))
REPRESENTATION_CONTEXT('','3D')
);
#85785=(
GEOMETRIC_REPRESENTATION_CONTEXT(3)
GLOBAL_UNCERTAINTY_ASSIGNED_CONTEXT((#85765))
GLOBAL_UNIT_ASSIGNED_CONTEXT((#85790,#85792,#85793))
REPRESENTATION_CONTEXT('','3D')
);
#85786=(
GEOMETRIC_REPRESENTATION_CONTEXT(3)
GLOBAL_UNCERTAINTY_ASSIGNED_CONTEXT((#85766))
GLOBAL_UNIT_ASSIGNED_CONTEXT((#85790,#85792,#85793))
REPRESENTATION_CONTEXT('','3D')
);
#85787=(
GEOMETRIC_REPRESENTATION_CONTEXT(3)
GLOBAL_UNCERTAINTY_ASSIGNED_CONTEXT((#85767))
GLOBAL_UNIT_ASSIGNED_CONTEXT((#85790,#85792,#85793))
REPRESENTATION_CONTEXT('','3D')
);
#85788=(
GEOMETRIC_REPRESENTATION_CONTEXT(3)
GLOBAL_UNCERTAINTY_ASSIGNED_CONTEXT((#85768))
GLOBAL_UNIT_ASSIGNED_CONTEXT((#85790,#85792,#85793))
REPRESENTATION_CONTEXT('','3D')
);
#85789=(
GEOMETRIC_REPRESENTATION_CONTEXT(3)
GLOBAL_UNCERTAINTY_ASSIGNED_CONTEXT((#85769))
GLOBAL_UNIT_ASSIGNED_CONTEXT((#85790,#85792,#85793))
REPRESENTATION_CONTEXT('','3D')
);
#85790=(
LENGTH_UNIT()
NAMED_UNIT(*)
SI_UNIT(.CENTI.,.METRE.)
);
#85791=(
LENGTH_UNIT()
NAMED_UNIT(*)
SI_UNIT($,.METRE.)
);
#85792=(
NAMED_UNIT(*)
PLANE_ANGLE_UNIT()
SI_UNIT($,.RADIAN.)
);
#85793=(
NAMED_UNIT(*)
SI_UNIT($,.STERADIAN.)
SOLID_ANGLE_UNIT()
);
#85794=SHAPE_DEFINITION_REPRESENTATION(#85813,#85862);
#85795=SHAPE_DEFINITION_REPRESENTATION(#85814,#85863);
#85796=SHAPE_DEFINITION_REPRESENTATION(#85815,#85864);
#85797=SHAPE_DEFINITION_REPRESENTATION(#85816,#85865);
#85798=SHAPE_DEFINITION_REPRESENTATION(#85817,#85866);
#85799=SHAPE_DEFINITION_REPRESENTATION(#85818,#85867);
#85800=SHAPE_DEFINITION_REPRESENTATION(#85819,#85868);
#85801=SHAPE_DEFINITION_REPRESENTATION(#85820,#85869);
#85802=SHAPE_DEFINITION_REPRESENTATION(#85821,#85870);
#85803=SHAPE_DEFINITION_REPRESENTATION(#85822,#85871);
#85804=SHAPE_DEFINITION_REPRESENTATION(#85823,#85872);
#85805=SHAPE_DEFINITION_REPRESENTATION(#85824,#85873);
#85806=SHAPE_DEFINITION_REPRESENTATION(#85825,#85874);
#85807=SHAPE_DEFINITION_REPRESENTATION(#85826,#85875);
#85808=SHAPE_DEFINITION_REPRESENTATION(#85827,#85876);
#85809=SHAPE_DEFINITION_REPRESENTATION(#85828,#85877);
#85810=SHAPE_DEFINITION_REPRESENTATION(#85829,#85878);
#85811=SHAPE_DEFINITION_REPRESENTATION(#85830,#85879);
#85812=SHAPE_DEFINITION_REPRESENTATION(#85831,#85880);
#85813=PRODUCT_DEFINITION_SHAPE('',$,#85882);
#85814=PRODUCT_DEFINITION_SHAPE('',$,#85883);
#85815=PRODUCT_DEFINITION_SHAPE('',$,#85884);
#85816=PRODUCT_DEFINITION_SHAPE('',$,#85885);
#85817=PRODUCT_DEFINITION_SHAPE('',$,#85886);
#85818=PRODUCT_DEFINITION_SHAPE('',$,#85887);
#85819=PRODUCT_DEFINITION_SHAPE('',$,#85888);
#85820=PRODUCT_DEFINITION_SHAPE('',$,#85889);
#85821=PRODUCT_DEFINITION_SHAPE('',$,#85890);
#85822=PRODUCT_DEFINITION_SHAPE('',$,#85891);
#85823=PRODUCT_DEFINITION_SHAPE('',$,#85892);
#85824=PRODUCT_DEFINITION_SHAPE('',$,#85893);
#85825=PRODUCT_DEFINITION_SHAPE('',$,#85894);
#85826=PRODUCT_DEFINITION_SHAPE('',$,#85895);
#85827=PRODUCT_DEFINITION_SHAPE('',$,#85896);
#85828=PRODUCT_DEFINITION_SHAPE('',$,#85897);
#85829=PRODUCT_DEFINITION_SHAPE('',$,#85898);
#85830=PRODUCT_DEFINITION_SHAPE('',$,#85899);
#85831=PRODUCT_DEFINITION_SHAPE('',$,#85900);
#85832=PRODUCT_DEFINITION_SHAPE($,$,#101);
#85833=PRODUCT_DEFINITION_SHAPE($,$,#102);
#85834=PRODUCT_DEFINITION_SHAPE($,$,#103);
#85835=PRODUCT_DEFINITION_SHAPE($,$,#104);
#85836=PRODUCT_DEFINITION_SHAPE($,$,#105);
#85837=PRODUCT_DEFINITION_SHAPE($,$,#106);
#85838=PRODUCT_DEFINITION_SHAPE($,$,#107);
#85839=PRODUCT_DEFINITION_SHAPE($,$,#108);
#85840=PRODUCT_DEFINITION_SHAPE($,$,#109);
#85841=PRODUCT_DEFINITION_SHAPE($,$,#110);
#85842=PRODUCT_DEFINITION_SHAPE($,$,#111);
#85843=PRODUCT_DEFINITION_SHAPE($,$,#112);
#85844=PRODUCT_DEFINITION_SHAPE($,$,#113);
#85845=PRODUCT_DEFINITION_SHAPE($,$,#114);
#85846=PRODUCT_DEFINITION_SHAPE($,$,#115);
#85847=PRODUCT_DEFINITION_SHAPE($,$,#116);
#85848=PRODUCT_DEFINITION_SHAPE($,$,#117);
#85849=PRODUCT_DEFINITION_SHAPE($,$,#118);
#85850=PRODUCT_DEFINITION_SHAPE($,$,#119);
#85851=PRODUCT_DEFINITION_SHAPE($,$,#120);
#85852=PRODUCT_DEFINITION_SHAPE($,$,#121);
#85853=PRODUCT_DEFINITION_SHAPE($,$,#122);
#85854=PRODUCT_DEFINITION_SHAPE($,$,#123);
#85855=PRODUCT_DEFINITION_SHAPE($,$,#124);
#85856=PRODUCT_DEFINITION_SHAPE($,$,#125);
#85857=PRODUCT_DEFINITION_SHAPE($,$,#126);
#85858=PRODUCT_DEFINITION_SHAPE($,$,#127);
#85859=PRODUCT_DEFINITION_SHAPE($,$,#128);
#85860=PRODUCT_DEFINITION_SHAPE($,$,#129);
#85861=PRODUCT_DEFINITION_SHAPE($,$,#130);
#85862=SHAPE_REPRESENTATION('',(#10098,#10929,#10930,#10931,#10932,#10933,
#10934,#10935,#10936,#10937,#10938,#10939,#10940,#10941,#10942,#10943,#10944,
#10945,#10946,#10947,#10948,#10949,#10950,#10951,#10952,#10953,#10954,#10955,
#10956,#10957,#10958),#85770);
#85863=SHAPE_REPRESENTATION('',(#10099),#85771);
#85864=SHAPE_REPRESENTATION('',(#10303),#85772);
#85865=SHAPE_REPRESENTATION('',(#10376),#85773);
#85866=SHAPE_REPRESENTATION('',(#10453),#85774);
#85867=SHAPE_REPRESENTATION('',(#10480),#85775);
#85868=SHAPE_REPRESENTATION('',(#10504),#85776);
#85869=SHAPE_REPRESENTATION('',(#10562),#85777);
#85870=SHAPE_REPRESENTATION('',(#10565),#85778);
#85871=SHAPE_REPRESENTATION('',(#10598),#85779);
#85872=SHAPE_REPRESENTATION('',(#10679),#85780);
#85873=SHAPE_REPRESENTATION('',(#10691),#85781);
#85874=SHAPE_REPRESENTATION('',(#10724),#85782);
#85875=SHAPE_REPRESENTATION('',(#10741),#85783);
#85876=SHAPE_REPRESENTATION('',(#10759),#85784);
#85877=SHAPE_REPRESENTATION('',(#10777),#85785);
#85878=SHAPE_REPRESENTATION('',(#10788),#85786);
#85879=SHAPE_REPRESENTATION('',(#10855),#85787);
#85880=SHAPE_REPRESENTATION('',(#10892),#85788);
#85881=PRODUCT_DEFINITION_CONTEXT('part definition',#85940,'design');
#85882=PRODUCT_DEFINITION('MAS-602',
'MAS-602',#85901,#85881);
#85883=PRODUCT_DEFINITION('Clutch Release Fork Lever',
'Clutch Release Fork Lever',#85902,#85881);
#85884=PRODUCT_DEFINITION('Lever Actuator Housing',
'Lever Actuator Housing',#85903,#85881);
#85885=PRODUCT_DEFINITION('Actuator Front Cover Plate',
'Actuator Front Cover Plate',#85904,#85881);
#85886=PRODUCT_DEFINITION('Fork Pivot Mounting Bracket',
'Fork Pivot Mounting Bracket',#85905,#85881);
#85887=PRODUCT_DEFINITION('Actuator Spindle M8x1.25',
'Actuator Spindle M8x1.25',#85906,#85881);
#85888=PRODUCT_DEFINITION('Roller Carriage Spindle Nut',
'Roller Carriage Spindle Nut',#85907,#85881);
#85889=PRODUCT_DEFINITION('Preload Compression Spring d2.2',
'Preload Compression Spring d2.2',#85908,#85881);
#85890=PRODUCT_DEFINITION('Deep Groove Ball Bearing 608-2RS',
'Deep Groove Ball Bearing 608-2RS',#85909,#85881);
#85891=PRODUCT_DEFINITION('Spindle Bearing Cap','Spindle Bearing Cap',#85910,
#85881);
#85892=PRODUCT_DEFINITION('Cap Retaining Clamp Band',
'Cap Retaining Clamp Band',#85911,#85881);
#85893=PRODUCT_DEFINITION('Main Roller Needle Bearing 6x20x9',
'Main Roller Needle Bearing 6x20x9',#85912,#85881);
#85894=PRODUCT_DEFINITION('Guide Roller 4x7x8','Guide Roller 4x7x8',#85913,
#85881);
#85895=PRODUCT_DEFINITION('Main Roller Stub Axle 6x22',
'Main Roller Stub Axle 6x22',#85914,#85881);
#85896=PRODUCT_DEFINITION('Guide Roller Stub Axle 4x22',
'Guide Roller Stub Axle 4x22',#85915,#85881);
#85897=PRODUCT_DEFINITION('ISO 8734 Dowel 6x16','ISO 8734 Dowel 6x16',#85916,
#85881);
#85898=PRODUCT_DEFINITION('ISO 7380 M4x10 Button Head',
'ISO 7380 M4x10 Button Head',#85917,#85881);
#85899=PRODUCT_DEFINITION('DIN 6799 E-Ring 5','DIN 6799 E-Ring 5',#85918,
#85881);
#85900=PRODUCT_DEFINITION('DIN 6799 E-Ring 3.2','DIN 6799 E-Ring 3.2',#85919,
#85881);
#85901=PRODUCT_DEFINITION_FORMATION('',$,#85942);
#85902=PRODUCT_DEFINITION_FORMATION('',$,#85943);
#85903=PRODUCT_DEFINITION_FORMATION('',$,#85944);
#85904=PRODUCT_DEFINITION_FORMATION('',$,#85945);
#85905=PRODUCT_DEFINITION_FORMATION('',$,#85946);
#85906=PRODUCT_DEFINITION_FORMATION('',$,#85947);
#85907=PRODUCT_DEFINITION_FORMATION('',$,#85948);
#85908=PRODUCT_DEFINITION_FORMATION('',$,#85949);
#85909=PRODUCT_DEFINITION_FORMATION('',$,#85950);
#85910=PRODUCT_DEFINITION_FORMATION('',$,#85951);
#85911=PRODUCT_DEFINITION_FORMATION('',$,#85952);
#85912=PRODUCT_DEFINITION_FORMATION('',$,#85953);
#85913=PRODUCT_DEFINITION_FORMATION('',$,#85954);
#85914=PRODUCT_DEFINITION_FORMATION('',$,#85955);
#85915=PRODUCT_DEFINITION_FORMATION('',$,#85956);
#85916=PRODUCT_DEFINITION_FORMATION('',$,#85957);
#85917=PRODUCT_DEFINITION_FORMATION('',$,#85958);
#85918=PRODUCT_DEFINITION_FORMATION('',$,#85959);
#85919=PRODUCT_DEFINITION_FORMATION('',$,#85960);
#85920=PRODUCT_RELATED_PRODUCT_CATEGORY(
'MAS-602','MAS-602',(#85942));
#85921=PRODUCT_RELATED_PRODUCT_CATEGORY('Clutch Release Fork Lever',
'Clutch Release Fork Lever',(#85943));
#85922=PRODUCT_RELATED_PRODUCT_CATEGORY('Lever Actuator Housing',
'Lever Actuator Housing',(#85944));
#85923=PRODUCT_RELATED_PRODUCT_CATEGORY('Actuator Front Cover Plate',
'Actuator Front Cover Plate',(#85945));
#85924=PRODUCT_RELATED_PRODUCT_CATEGORY('Fork Pivot Mounting Bracket',
'Fork Pivot Mounting Bracket',(#85946));
#85925=PRODUCT_RELATED_PRODUCT_CATEGORY('Actuator Spindle M8x1.25',
'Actuator Spindle M8x1.25',(#85947));
#85926=PRODUCT_RELATED_PRODUCT_CATEGORY('Roller Carriage Spindle Nut',
'Roller Carriage Spindle Nut',(#85948));
#85927=PRODUCT_RELATED_PRODUCT_CATEGORY(
'Preload Compression Spring d2.2','Preload Compression Spring d2.2',(#85949));
#85928=PRODUCT_RELATED_PRODUCT_CATEGORY(
'Deep Groove Ball Bearing 608-2RS','Deep Groove Ball Bearing 608-2RS',(#85950));
#85929=PRODUCT_RELATED_PRODUCT_CATEGORY('Spindle Bearing Cap',
'Spindle Bearing Cap',(#85951));
#85930=PRODUCT_RELATED_PRODUCT_CATEGORY('Cap Retaining Clamp Band',
'Cap Retaining Clamp Band',(#85952));
#85931=PRODUCT_RELATED_PRODUCT_CATEGORY(
'Main Roller Needle Bearing 6x20x9','Main Roller Needle Bearing 6x20x9',
(#85953));
#85932=PRODUCT_RELATED_PRODUCT_CATEGORY('Guide Roller 4x7x8',
'Guide Roller 4x7x8',(#85954));
#85933=PRODUCT_RELATED_PRODUCT_CATEGORY('Main Roller Stub Axle 6x22',
'Main Roller Stub Axle 6x22',(#85955));
#85934=PRODUCT_RELATED_PRODUCT_CATEGORY('Guide Roller Stub Axle 4x22',
'Guide Roller Stub Axle 4x22',(#85956));
#85935=PRODUCT_RELATED_PRODUCT_CATEGORY('ISO 8734 Dowel 6x16',
'ISO 8734 Dowel 6x16',(#85957));
#85936=PRODUCT_RELATED_PRODUCT_CATEGORY('ISO 7380 M4x10 Button Head',
'ISO 7380 M4x10 Button Head',(#85958));
#85937=PRODUCT_RELATED_PRODUCT_CATEGORY('DIN 6799 E-Ring 5',
'DIN 6799 E-Ring 5',(#85959));
#85938=PRODUCT_RELATED_PRODUCT_CATEGORY('DIN 6799 E-Ring 3.2',
'DIN 6799 E-Ring 3.2',(#85960));
#85939=APPLICATION_PROTOCOL_DEFINITION('international standard',
'automotive_design',2009,#85940);
#85940=APPLICATION_CONTEXT(
'Core Data for Automotive Mechanical Design Process');
#85941=PRODUCT_CONTEXT('part definition',#85940,'mechanical');
#85942=PRODUCT('MAS-602',
'MAS-602',$,(#85941));
#85943=PRODUCT('Clutch Release Fork Lever','Clutch Release Fork Lever',
$,(#85941));
#85944=PRODUCT('Lever Actuator Housing','Lever Actuator Housing',$,(#85941));
#85945=PRODUCT('Actuator Front Cover Plate',
'Actuator Front Cover Plate',$,(#85941));
#85946=PRODUCT('Fork Pivot Mounting Bracket',
'Fork Pivot Mounting Bracket',$,(#85941));
#85947=PRODUCT('Actuator Spindle M8x1.25','Actuator Spindle M8x1.25',$,
(#85941));
#85948=PRODUCT('Roller Carriage Spindle Nut',
'Roller Carriage Spindle Nut',$,(#85941));
#85949=PRODUCT('Preload Compression Spring d2.2',
'Preload Compression Spring d2.2',$,(#85941));
#85950=PRODUCT('Deep Groove Ball Bearing 608-2RS',
'Deep Groove Ball Bearing 608-2RS',$,(#85941));
#85951=PRODUCT('Spindle Bearing Cap','Spindle Bearing Cap',$,(#85941));
#85952=PRODUCT('Cap Retaining Clamp Band','Cap Retaining Clamp Band',$,
(#85941));
#85953=PRODUCT('Main Roller Needle Bearing 6x20x9',
'Main Roller Needle Bearing 6x20x9',$,(#85941));
#85954=PRODUCT('Guide Roller 4x7x8','Guide Roller 4x7x8',$,(#85941));
#85955=PRODUCT('Main Roller Stub Axle 6x22',
'Main Roller Stub Axle 6x22',$,(#85941));
#85956=PRODUCT('Guide Roller Stub Axle 4x22',
'Guide Roller Stub Axle 4x22',$,(#85941));
#85957=PRODUCT('ISO 8734 Dowel 6x16','ISO 8734 Dowel 6x16',$,(#85941));
#85958=PRODUCT('ISO 7380 M4x10 Button Head',
'ISO 7380 M4x10 Button Head',$,(#85941));
#85959=PRODUCT('DIN 6799 E-Ring 5','DIN 6799 E-Ring 5',$,(#85941));
#85960=PRODUCT('DIN 6799 E-Ring 3.2','DIN 6799 E-Ring 3.2',$,(#85941));
#85961=PRESENTATION_STYLE_ASSIGNMENT((#85979));
#85962=PRESENTATION_STYLE_ASSIGNMENT((#85980));
#85963=PRESENTATION_STYLE_ASSIGNMENT((#85981));
#85964=PRESENTATION_STYLE_ASSIGNMENT((#85982));
#85965=PRESENTATION_STYLE_ASSIGNMENT((#85983));
#85966=PRESENTATION_STYLE_ASSIGNMENT((#85984));
#85967=PRESENTATION_STYLE_ASSIGNMENT((#85985));
#85968=PRESENTATION_STYLE_ASSIGNMENT((#85986));
#85969=PRESENTATION_STYLE_ASSIGNMENT((#85987));
#85970=PRESENTATION_STYLE_ASSIGNMENT((#85988));
#85971=PRESENTATION_STYLE_ASSIGNMENT((#85989));
#85972=PRESENTATION_STYLE_ASSIGNMENT((#85990));
#85973=PRESENTATION_STYLE_ASSIGNMENT((#85991));
#85974=PRESENTATION_STYLE_ASSIGNMENT((#85992));
#85975=PRESENTATION_STYLE_ASSIGNMENT((#85993));
#85976=PRESENTATION_STYLE_ASSIGNMENT((#85994));
#85977=PRESENTATION_STYLE_ASSIGNMENT((#85995));
#85978=PRESENTATION_STYLE_ASSIGNMENT((#85996));
#85979=SURFACE_STYLE_USAGE(.BOTH.,#85997);
#85980=SURFACE_STYLE_USAGE(.BOTH.,#85998);
#85981=SURFACE_STYLE_USAGE(.BOTH.,#85999);
#85982=SURFACE_STYLE_USAGE(.BOTH.,#86000);
#85983=SURFACE_STYLE_USAGE(.BOTH.,#86001);
#85984=SURFACE_STYLE_USAGE(.BOTH.,#86002);
#85985=SURFACE_STYLE_USAGE(.BOTH.,#86003);
#85986=SURFACE_STYLE_USAGE(.BOTH.,#86004);
#85987=SURFACE_STYLE_USAGE(.BOTH.,#86005);
#85988=SURFACE_STYLE_USAGE(.BOTH.,#86006);
#85989=SURFACE_STYLE_USAGE(.BOTH.,#86007);
#85990=SURFACE_STYLE_USAGE(.BOTH.,#86008);
#85991=SURFACE_STYLE_USAGE(.BOTH.,#86009);
#85992=SURFACE_STYLE_USAGE(.BOTH.,#86010);
#85993=SURFACE_STYLE_USAGE(.BOTH.,#86011);
#85994=SURFACE_STYLE_USAGE(.BOTH.,#86012);
#85995=SURFACE_STYLE_USAGE(.BOTH.,#86013);
#85996=SURFACE_STYLE_USAGE(.BOTH.,#86014);
#85997=SURFACE_SIDE_STYLE('',(#86015));
#85998=SURFACE_SIDE_STYLE('',(#86016));
#85999=SURFACE_SIDE_STYLE('',(#86017));
#86000=SURFACE_SIDE_STYLE('',(#86018));
#86001=SURFACE_SIDE_STYLE('',(#86019));
#86002=SURFACE_SIDE_STYLE('',(#86020));
#86003=SURFACE_SIDE_STYLE('',(#86021));
#86004=SURFACE_SIDE_STYLE('',(#86022));
#86005=SURFACE_SIDE_STYLE('',(#86023));
#86006=SURFACE_SIDE_STYLE('',(#86024));
#86007=SURFACE_SIDE_STYLE('',(#86025));
#86008=SURFACE_SIDE_STYLE('',(#86026));
#86009=SURFACE_SIDE_STYLE('',(#86027));
#86010=SURFACE_SIDE_STYLE('',(#86028));
#86011=SURFACE_SIDE_STYLE('',(#86029));
#86012=SURFACE_SIDE_STYLE('',(#86030));
#86013=SURFACE_SIDE_STYLE('',(#86031));
#86014=SURFACE_SIDE_STYLE('',(#86032));
#86015=SURFACE_STYLE_FILL_AREA(#86033);
#86016=SURFACE_STYLE_FILL_AREA(#86034);
#86017=SURFACE_STYLE_FILL_AREA(#86035);
#86018=SURFACE_STYLE_FILL_AREA(#86036);
#86019=SURFACE_STYLE_FILL_AREA(#86037);
#86020=SURFACE_STYLE_FILL_AREA(#86038);
#86021=SURFACE_STYLE_FILL_AREA(#86039);
#86022=SURFACE_STYLE_FILL_AREA(#86040);
#86023=SURFACE_STYLE_FILL_AREA(#86041);
#86024=SURFACE_STYLE_FILL_AREA(#86042);
#86025=SURFACE_STYLE_FILL_AREA(#86043);
#86026=SURFACE_STYLE_FILL_AREA(#86044);
#86027=SURFACE_STYLE_FILL_AREA(#86045);
#86028=SURFACE_STYLE_FILL_AREA(#86046);
#86029=SURFACE_STYLE_FILL_AREA(#86047);
#86030=SURFACE_STYLE_FILL_AREA(#86048);
#86031=SURFACE_STYLE_FILL_AREA(#86049);
#86032=SURFACE_STYLE_FILL_AREA(#86050);
#86033=FILL_AREA_STYLE('Steel - Satin',(#86051));
#86034=FILL_AREA_STYLE('Opaque(112,115,119)',(#86052));
#86035=FILL_AREA_STYLE('Opaque(176,180,186)',(#86053));
#86036=FILL_AREA_STYLE('Opaque(84,86,90)',(#86054));
#86037=FILL_AREA_STYLE('Opaque(150,153,157)',(#86055));
#86038=FILL_AREA_STYLE('Opaque(212,215,220)',(#86056));
#86039=FILL_AREA_STYLE('Opaque(200,203,207)',(#86057));
#86040=FILL_AREA_STYLE('Opaque(38,38,41)',(#86058));
#86041=FILL_AREA_STYLE('Opaque(218,221,226)',(#86059));
#86042=FILL_AREA_STYLE('Opaque(30,30,33)',(#86060));
#86043=FILL_AREA_STYLE('Opaque(205,208,212)',(#86061));
#86044=FILL_AREA_STYLE('Opaque(206,209,214)',(#86062));
#86045=FILL_AREA_STYLE('Opaque(208,211,216)',(#86063));
#86046=FILL_AREA_STYLE('Opaque(216,219,224)',(#86064));
#86047=FILL_AREA_STYLE('Opaque(214,217,222)',(#86065));
#86048=FILL_AREA_STYLE('Opaque(210,213,218)',(#86066));
#86049=FILL_AREA_STYLE('Opaque(200,204,209)',(#86067));
#86050=FILL_AREA_STYLE('Opaque(198,202,207)',(#86068));
#86051=FILL_AREA_STYLE_COLOUR('Steel - Satin',#86069);
#86052=FILL_AREA_STYLE_COLOUR('Opaque(112,115,119)',#86070);
#86053=FILL_AREA_STYLE_COLOUR('Opaque(176,180,186)',#86071);
#86054=FILL_AREA_STYLE_COLOUR('Opaque(84,86,90)',#86072);
#86055=FILL_AREA_STYLE_COLOUR('Opaque(150,153,157)',#86073);
#86056=FILL_AREA_STYLE_COLOUR('Opaque(212,215,220)',#86074);
#86057=FILL_AREA_STYLE_COLOUR('Opaque(200,203,207)',#86075);
#86058=FILL_AREA_STYLE_COLOUR('Opaque(38,38,41)',#86076);
#86059=FILL_AREA_STYLE_COLOUR('Opaque(218,221,226)',#86077);
#86060=FILL_AREA_STYLE_COLOUR('Opaque(30,30,33)',#86078);
#86061=FILL_AREA_STYLE_COLOUR('Opaque(205,208,212)',#86079);
#86062=FILL_AREA_STYLE_COLOUR('Opaque(206,209,214)',#86080);
#86063=FILL_AREA_STYLE_COLOUR('Opaque(208,211,216)',#86081);
#86064=FILL_AREA_STYLE_COLOUR('Opaque(216,219,224)',#86082);
#86065=FILL_AREA_STYLE_COLOUR('Opaque(214,217,222)',#86083);
#86066=FILL_AREA_STYLE_COLOUR('Opaque(210,213,218)',#86084);
#86067=FILL_AREA_STYLE_COLOUR('Opaque(200,204,209)',#86085);
#86068=FILL_AREA_STYLE_COLOUR('Opaque(198,202,207)',#86086);
#86069=COLOUR_RGB('Steel - Satin', 0.66274510, 0.83137255, 0.94901961);
#86070=COLOUR_RGB('Opaque(112,115,119)', 0.66274510, 0.83137255, 0.94901961);
#86071=COLOUR_RGB('Opaque(176,180,186)', 0.31764706, 0.68627451, 0.89019608);
#86072=COLOUR_RGB('Opaque(84,86,90)', 0.40784314, 0.44705882, 0.49803922);
#86073=COLOUR_RGB('Opaque(150,153,157)', 0.72549020, 0.75294118, 0.79215686);
#86074=COLOUR_RGB('Opaque(212,215,220)', 0.08235294, 0.09019608, 0.10196078);
#86075=COLOUR_RGB('Opaque(200,203,207)', 0.09019608, 0.27058824, 0.51372549);
#86076=COLOUR_RGB('Opaque(38,38,41)', 0.66274510, 0.83137255, 0.94901961);
#86077=COLOUR_RGB('Opaque(218,221,226)', 0.31764706, 0.68627451, 0.89019608);
#86078=COLOUR_RGB('Opaque(30,30,33)', 0.40784314, 0.44705882, 0.49803922);
#86079=COLOUR_RGB('Opaque(205,208,212)', 0.72549020, 0.75294118, 0.79215686);
#86080=COLOUR_RGB('Opaque(206,209,214)', 0.08235294, 0.09019608, 0.10196078);
#86081=COLOUR_RGB('Opaque(208,211,216)', 0.09019608, 0.27058824, 0.51372549);
#86082=COLOUR_RGB('Opaque(216,219,224)', 0.66274510, 0.83137255, 0.94901961);
#86083=COLOUR_RGB('Opaque(214,217,222)', 0.31764706, 0.68627451, 0.89019608);
#86084=COLOUR_RGB('Opaque(210,213,218)', 0.40784314, 0.44705882, 0.49803922);
#86085=COLOUR_RGB('Opaque(200,204,209)', 0.72549020, 0.75294118, 0.79215686);
#86086=COLOUR_RGB('Opaque(198,202,207)', 0.08235294, 0.09019608, 0.10196078);
ENDSEC;
END-ISO-10303-21;
